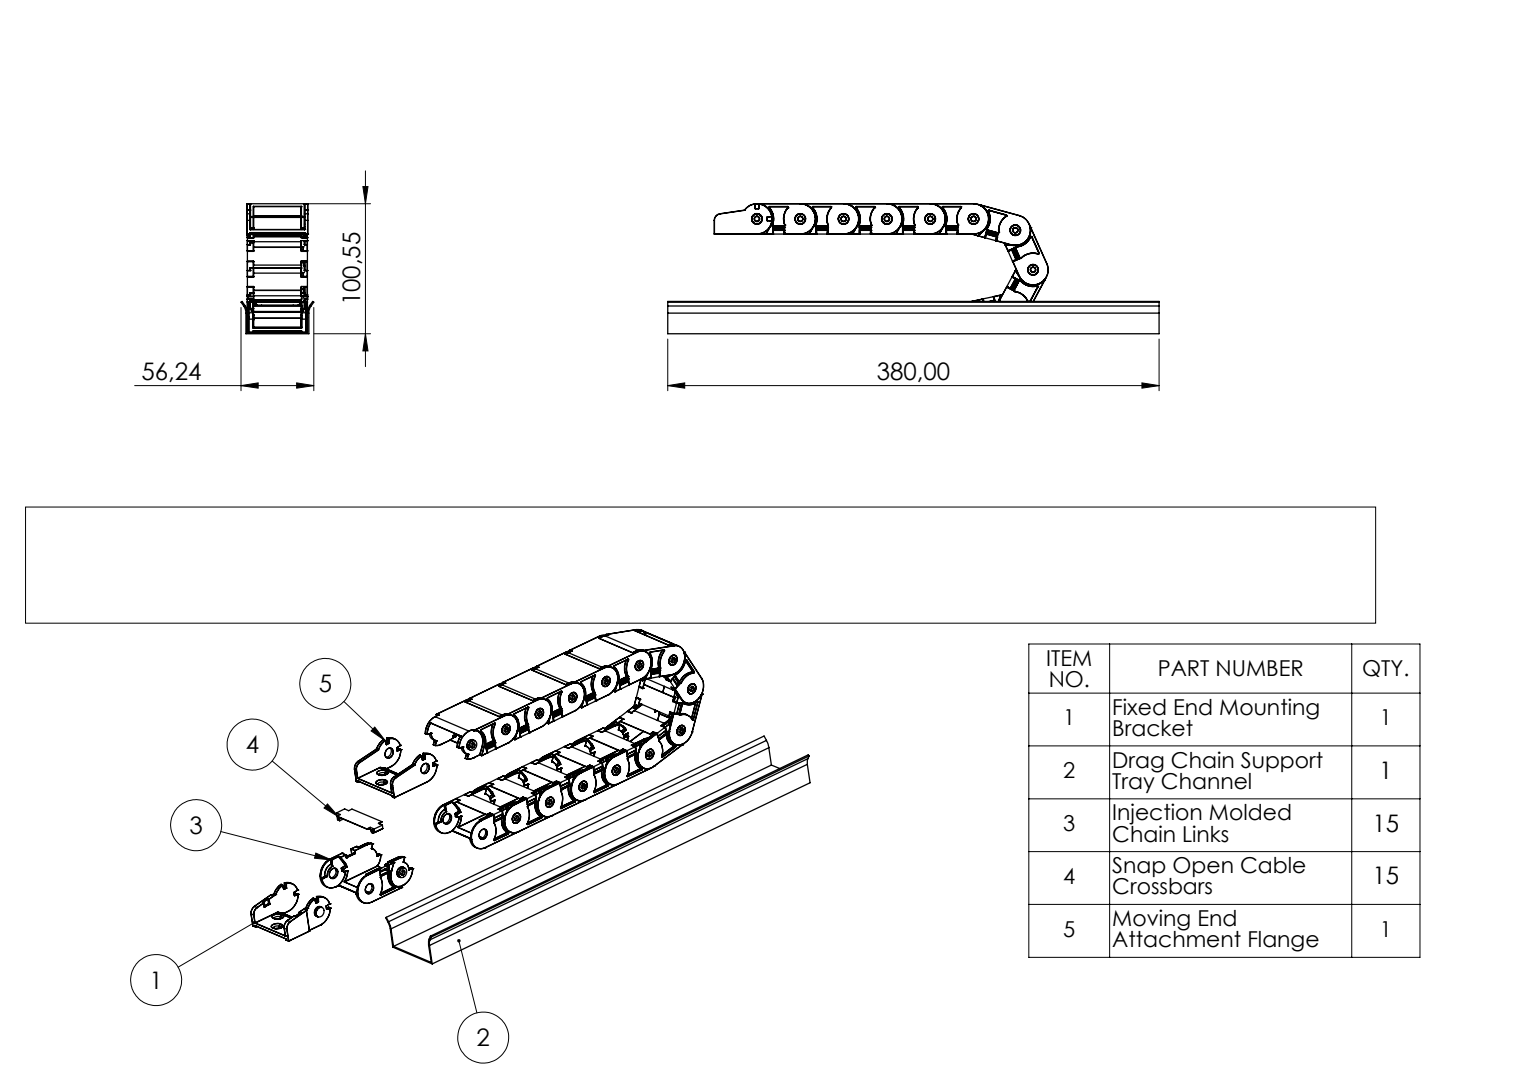
ISO-10303-21;
HEADER;
FILE_DESCRIPTION (('STEP AP214'),
    '1' );
FILE_NAME ('MAS-200',
    '2026-10-08T22:59:04',
    ( '' ),
    ( '' ),
    'SwSTEP 2.0',
    'SolidWorks 2020',
    '' );
FILE_SCHEMA (( 'AUTOMOTIVE_DESIGN' ));
ENDSEC;

DATA;
#1 = CARTESIAN_POINT ( 'NONE',  ( -16.92989143108098204, 9.949999999999981526, -12.88248387475667656 ) ) ;
#2 = ADVANCED_FACE ( 'NONE', ( #179969 ), #178383, .T. ) ;
#4 = DIRECTION ( 'NONE',  ( 0.000000000000000000, 0.000000000000000000, -1.000000000000000000 ) ) ;
#3 = CARTESIAN_POINT ( 'NONE',  ( -23.15000000000000213, 3.470628026992396808, -231.7731008717366876 ) ) ;
#5 = DIRECTION ( 'NONE',  ( 1.000000000000000000, -7.304098846218133681E-16, 0.000000000000000000 ) ) ;
#8 = ORIENTED_EDGE ( 'NONE', *, *, #143500, .T. ) ;
#7 = EDGE_CURVE ( 'NONE', #162791, #50451, #132568, .T. ) ;
#6 = CARTESIAN_POINT ( 'NONE',  ( 20.11144452914042802, 66.06638914889212799, -128.6328140305745933 ) ) ;
#10 = DIRECTION ( 'NONE',  ( 0.000000000000000000, 0.3427706569149662763, -0.9394191166662954062 ) ) ;
#9 = CARTESIAN_POINT ( 'NONE',  ( -18.59999999999999787, 68.22930980752001062, -227.7331931781284879 ) ) ;
#11 = ORIENTED_EDGE ( 'NONE', *, *, #97972, .T. ) ;
#13 = ORIENTED_EDGE ( 'NONE', *, *, #236887, .F. ) ;
#12 = CARTESIAN_POINT ( 'NONE',  ( 20.94999999999999929, 11.65000000001115943, -67.00000000000000000 ) ) ;
#14 = ORIENTED_EDGE ( 'NONE', *, *, #107088, .T. ) ;
#15 = DIRECTION ( 'NONE',  ( 0.000000000000000000, 0.000000000000000000, -1.000000000000000000 ) ) ;
#16 = CARTESIAN_POINT ( 'NONE',  ( -22.47071067811865319, 0.09909245471376178227, -25.77992525550193648 ) ) ;
#17 = CARTESIAN_POINT ( 'NONE',  ( -21.05000000000000071, 11.65000000001115232, -167.5999999999999659 ) ) ;
#18 = CARTESIAN_POINT ( 'NONE',  ( -17.29838795460356593, 22.07107181154411890, -229.9709893146081754 ) ) ;
#19 = ORIENTED_EDGE ( 'NONE', *, *, #38836, .T. ) ;
#20 = LINE ( 'NONE', #198225, #75570 ) ;
#21 = CARTESIAN_POINT ( 'NONE',  ( 20.97462148592267539, 8.874737576461731337, -112.7546443317310434 ) ) ;
#22 = CARTESIAN_POINT ( 'NONE',  ( 21.05000000000000071, 11.75000000001116263, -93.48519422934610645 ) ) ;
#23 = EDGE_CURVE ( 'NONE', #151382, #73251, #20149, .T. ) ;
#24 = ORIENTED_EDGE ( 'NONE', *, *, #246973, .F. ) ;
#25 = ADVANCED_FACE ( 'NONE', ( #203377 ), #234826, .T. ) ;
#26 = TOROIDAL_SURFACE ( 'NONE', #183386, 0.4000000000000009104, 0.1000000000000000056 ) ;
#27 = DIRECTION ( 'NONE',  ( -1.000000000000000000, -2.952720810173289112E-16, 0.000000000000000000 ) ) ;
#28 = CIRCLE ( 'NONE', #245740, 0.1000000000000032113 ) ;
#29 = DIRECTION ( 'NONE',  ( -1.020425574104004196E-15, -6.982962677686266711E-15, 1.000000000000000000 ) ) ;
#30 = EDGE_CURVE ( 'NONE', #21530, #216178, #199211, .T. ) ;
#31 = ORIENTED_EDGE ( 'NONE', *, *, #146192, .F. ) ;
#32 = ORIENTED_EDGE ( 'NONE', *, *, #162707, .T. ) ;
#33 = CARTESIAN_POINT ( 'NONE',  ( 18.39999999999999503, 64.52683809664910086, -56.87310748452440379 ) ) ;
#34 = AXIS2_PLACEMENT_3D ( 'NONE', #189135, #91325, #191735 ) ;
#35 = ORIENTED_EDGE ( 'NONE', *, *, #78924, .T. ) ;
#36 = CARTESIAN_POINT ( 'NONE',  ( -17.29838795458766043, 10.37154985795013218, -11.39525871738185714 ) ) ;
#37 = ORIENTED_EDGE ( 'NONE', *, *, #109345, .T. ) ;
#38 = PLANE ( 'NONE',  #96833 ) ;
#39 = LINE ( 'NONE', #62597, #48246 ) ;
#40 = LINE ( 'NONE', #161717, #239034 ) ;
#41 = ADVANCED_FACE ( 'NONE', ( #121306 ), #43023, .F. ) ;
#42 = CARTESIAN_POINT ( 'NONE',  ( -20.94999999999999929, 0.000000000000000000, -7.900000000000000355 ) ) ;
#43 = TOROIDAL_SURFACE ( 'NONE', #87521, 0.2000000000000000111, 0.1000000000000000056 ) ;
#44 = EDGE_CURVE ( 'NONE', #241330, #245837, #16247, .T. ) ;
#45 = AXIS2_PLACEMENT_3D ( 'NONE', #144433, #222696, #243559 ) ;
#46 = DIRECTION ( 'NONE',  ( 4.408576920032446739E-17, 0.1350103645451945777, -0.9908441862701590219 ) ) ;
#47 = DIRECTION ( 'NONE',  ( -0.000000000000000000, 6.982962677686266711E-15, -1.000000000000000000 ) ) ;
#48 = CARTESIAN_POINT ( 'NONE',  ( 21.05000000000000071, 5.850000000011156942, -56.86750277572208034 ) ) ;
#49 = ORIENTED_EDGE ( 'NONE', *, *, #170481, .T. ) ;
#51 = LINE ( 'NONE', #18341, #77316 ) ;
#50 = DIRECTION ( 'NONE',  ( -0.000000000000000000, -0.000000000000000000, 1.000000000000000000 ) ) ;
#52 = VERTEX_POINT ( 'NONE', #84661 ) ;
#55 = ORIENTED_EDGE ( 'NONE', *, *, #79678, .T. ) ;
#54 = CARTESIAN_POINT ( 'NONE',  ( -21.05000000000000071, 56.01362831242966678, -232.7091905853083347 ) ) ;
#53 = CARTESIAN_POINT ( 'NONE',  ( 21.05000000000000071, 76.00000000001172396, -71.52310748452431710 ) ) ;
#56 = COLOUR_RGB ( '', 0.40784314, 0.44705882, 0.49803922) ;
#57 = ORIENTED_EDGE ( 'NONE', *, *, #255744, .F. ) ;
#58 = DIRECTION ( 'NONE',  ( 1.000000000000000000, 0.000000000000000000, 0.000000000000000000 ) ) ;
#59 = CARTESIAN_POINT ( 'NONE',  ( 21.05000000000000071, -0.08559286335111461475, -60.58633726513042461 ) ) ;
#60 = FACE_OUTER_BOUND ( 'NONE', #199534, .T. ) ;
#61 = CARTESIAN_POINT ( 'NONE',  ( -18.39418127959864790, 64.51609439831406689, -145.7731074845244450 ) ) ;
#62 = VERTEX_POINT ( 'NONE', #243781 ) ;
#63 = LINE ( 'NONE', #3928, #147005 ) ;
#64 = DIRECTION ( 'NONE',  ( 0.000000000000000000, 0.000000000000000000, 1.000000000000000000 ) ) ;
#66 = LINE ( 'NONE', #97860, #134130 ) ;
#65 = DIRECTION ( 'NONE',  ( -1.000000000000000000, 0.000000000000000000, 0.000000000000000000 ) ) ;
#68 = ORIENTED_EDGE ( 'NONE', *, *, #6404, .T. ) ;
#67 = CARTESIAN_POINT ( 'NONE',  ( -23.15000000000000213, 0.000000000000000000, -4.149999999999999467 ) ) ;
#69 = AXIS2_PLACEMENT_3D ( 'NONE', #162469, #21667, #98580 ) ;
#70 = VECTOR ( 'NONE', #89864, 1000.000000000000000 ) ;
#71 = ORIENTED_EDGE ( 'NONE', *, *, #179559, .T. ) ;
#72 = B_SPLINE_CURVE_WITH_KNOTS ( 'NONE', 3,
 ( #139012, #19102, #60787, #178213, #62093, #257652, #41274, #180758, #218573, #162488, #79052, #22993, #39989, #157373, #119506, #236866, #137752, #173434, #141618, #102458, #199035, #795, #182040, #58212, #240730, #42515, #122066, #201587, #20411, #3376 ),
 .UNSPECIFIED., .F., .F.,
 ( 4, 2, 2, 2, 2, 2, 2, 2, 2, 2, 2, 2, 2, 2, 4 ),
 ( 0.000000000000000000, 0.0003422764154113359459, 0.0006845528308226718917, 0.001026829246234007729, 0.001369105661645343783, 0.002053658492468013290, 0.002738211323290682796, 0.003080487738702016899, 0.003422764154113351869, 0.003765040569524686406, 0.004107316984936021376, 0.004449593400347355912, 0.004791869815758691316, 0.005134146231170024985, 0.005476422646581360389 ),
 .UNSPECIFIED. ) ;
#73 = CARTESIAN_POINT ( 'NONE',  ( 33.30000000000001137, 3.332938107839120701, 33.00000000000000000 ) ) ;
#74 = ORIENTED_EDGE ( 'NONE', *, *, #168378, .T. ) ;
#75 = CARTESIAN_POINT ( 'NONE',  ( 20.94999999999999574, 65.57661458509869590, -62.03105556065429482 ) ) ;
#76 = ORIENTED_EDGE ( 'NONE', *, *, #212684, .T. ) ;
#77 = LINE ( 'NONE', #43075, #147484 ) ;
#78 = CARTESIAN_POINT ( 'NONE',  ( 22.59999999999999432, 75.89914163091330579, -114.7726746080137161 ) ) ;
#79 = CARTESIAN_POINT ( 'NONE',  ( -20.54999999999999716, 87.75000000001259082, -191.1731074845242517 ) ) ;
#80 = ORIENTED_EDGE ( 'NONE', *, *, #1653, .T. ) ;
#81 = DIRECTION ( 'NONE',  ( 1.000000000000000000, -7.049440681616511973E-16, 1.911869773728122111E-16 ) ) ;
#82 = VECTOR ( 'NONE', #56443, 999.9999999999998863 ) ;
#83 = AXIS2_PLACEMENT_3D ( 'NONE', #206420, #107313, #246821 ) ;
#84 = EDGE_CURVE ( 'NONE', #177357, #123054, #144663, .T. ) ;
#85 = CIRCLE ( 'NONE', #249894, 12.87500000000000000 ) ;
#86 = AXIS2_PLACEMENT_3D ( 'NONE', #170578, #248783, #191400 ) ;
#87 = CARTESIAN_POINT ( 'NONE',  ( -18.59999999999999787, 61.54970422893871529, -212.2965875311496688 ) ) ;
#88 = ORIENTED_EDGE ( 'NONE', *, *, #100506, .F. ) ;
#89 = CIRCLE ( 'NONE', #91688, 0.2000000000000000944 ) ;
#90 = ORIENTED_EDGE ( 'NONE', *, *, #88866, .F. ) ;
#91 = EDGE_LOOP ( 'NONE', ( #74556, #125437, #66569, #237966 ) ) ;
#92 = CARTESIAN_POINT ( 'NONE',  ( -20.90000000000000213, 6.336640076952988920, 12.03401928653448572 ) ) ;
#94 = EDGE_CURVE ( 'NONE', #19242, #16854, #137031, .T. ) ;
#93 = EDGE_LOOP ( 'NONE', ( #41790, #120721, #253364, #8024, #101724, #76712, #208119, #163090, #81602, #93473, #199890, #120447, #37635, #170547, #25122, #143467, #230838, #110010, #37319, #108527, #200762, #188074, #74749, #27804, #95098, #214920, #223956 ) ) ;
#96 = EDGE_LOOP ( 'NONE', ( #150504, #184348, #87694, #206446 ) ) ;
#95 = CARTESIAN_POINT ( 'NONE',  ( -18.50000000000000000, 76.00000000001244871, -170.0231074845243597 ) ) ;
#97 = ORIENTED_EDGE ( 'NONE', *, *, #227198, .T. ) ;
#98 = ADVANCED_FACE ( 'NONE', ( #186389 ), #170715, .F. ) ;
#100 = EDGE_CURVE ( 'NONE', #48831, #76480, #107799, .T. ) ;
#99 = AXIS2_PLACEMENT_3D ( 'NONE', #76575, #156148, #56984 ) ;
#103 = ORIENTED_EDGE ( 'NONE', *, *, #206571, .T. ) ;
#102 = ORIENTED_EDGE ( 'NONE', *, *, #34870, .F. ) ;
#101 = CARTESIAN_POINT ( 'NONE',  ( -20.54999999999999716, 23.49882452903949925, -253.1653563615082305 ) ) ;
#104 = VECTOR ( 'NONE', #151138, 1000.000000000000000 ) ;
#105 = ORIENTED_EDGE ( 'NONE', *, *, #252643, .T. ) ;
#106 = CARTESIAN_POINT ( 'NONE',  ( 23.14999999999999858, 76.00000000001170974, -69.52310748452431710 ) ) ;
#107 = CARTESIAN_POINT ( 'NONE',  ( -23.15000000000000213, 85.60000000001221565, -146.4170766071767389 ) ) ;
#108 = CARTESIAN_POINT ( 'NONE',  ( -16.82055514392371620, 14.15329893112338588, -219.2288882764422624 ) ) ;
#109 = VERTEX_POINT ( 'NONE', #88531 ) ;
#110 = EDGE_CURVE ( 'NONE', #147343, #202762, #12898, .T. ) ;
#111 = CARTESIAN_POINT ( 'NONE',  ( -20.94999999999999929, 87.48912529308798014, -105.9231074845242091 ) ) ;
#113 = VERTEX_POINT ( 'NONE', #246350 ) ;
#112 = CARTESIAN_POINT ( 'NONE',  ( 21.07928932188134397, 6.328516656404459262, -167.4011048543455615 ) ) ;
#114 = DIRECTION ( 'NONE',  ( 0.000000000000000000, -0.4088369013363280513, 0.9126074666063769270 ) ) ;
#115 = ORIENTED_EDGE ( 'NONE', *, *, #108700, .T. ) ;
#116 = EDGE_LOOP ( 'NONE', ( #122907, #87226, #174706, #3134 ) ) ;
#117 = CARTESIAN_POINT ( 'NONE',  ( -20.94999999999999929, 14.80545736607782814, -235.9842437978701639 ) ) ;
#118 = CARTESIAN_POINT ( 'NONE',  ( 22.88900146558018989, 64.28838232313110268, -213.4537907441674918 ) ) ;
#119 = ORIENTED_EDGE ( 'NONE', *, *, #90031, .T. ) ;
#120 = ORIENTED_EDGE ( 'NONE', *, *, #167346, .T. ) ;
#122 = TOROIDAL_SURFACE ( 'NONE', #25285, 11.65000000000000036, 0.1000000000000000056 ) ;
#121 = DIRECTION ( 'NONE',  ( 1.000000000000000000, 0.000000000000000000, -0.000000000000000000 ) ) ;
#123 = CARTESIAN_POINT ( 'NONE',  ( -23.15000000000000213, 54.26389919992384137, -237.1169412515656632 ) ) ;
#125 = VERTEX_POINT ( 'NONE', #228076 ) ;
#124 = ORIENTED_EDGE ( 'NONE', *, *, #248251, .T. ) ;
#126 = VERTEX_POINT ( 'NONE', #92393 ) ;
#127 = DIRECTION ( 'NONE',  ( 0.000000000000000000, -0.9126074666065964180, -0.4088369013358383874 ) ) ;
#129 = ORIENTED_EDGE ( 'NONE', *, *, #240704, .T. ) ;
#128 = EDGE_CURVE ( 'NONE', #174631, #91171, #224322, .T. ) ;
#130 = ORIENTED_EDGE ( 'NONE', *, *, #78727, .F. ) ;
#131 = DIRECTION ( 'NONE',  ( -0.000000000000000000, -6.982962677686266711E-15, 1.000000000000000000 ) ) ;
#132 = AXIS2_PLACEMENT_3D ( 'NONE', #200037, #1808, #61804 ) ;
#133 = VERTEX_POINT ( 'NONE', #245061 ) ;
#134 = CARTESIAN_POINT ( 'NONE',  ( -16.93909480342660245, 12.44555890197899295, -211.1852061227702109 ) ) ;
#136 = DIRECTION ( 'NONE',  ( 0.000000000000000000, -0.2128009952263678062, 0.9770955615653298398 ) ) ;
#135 = DIRECTION ( 'NONE',  ( 0.000000000000000000, -1.000000000000000000, 0.000000000000000000 ) ) ;
#137 = ORIENTED_EDGE ( 'NONE', *, *, #203695, .F. ) ;
#140 = EDGE_CURVE ( 'NONE', #198947, #93557, #66106, .T. ) ;
#139 = ORIENTED_EDGE ( 'NONE', *, *, #116118, .F. ) ;
#138 = ORIENTED_EDGE ( 'NONE', *, *, #133333, .T. ) ;
#141 = LINE ( 'NONE', #80958, #244386 ) ;
#142 = CARTESIAN_POINT ( 'NONE',  ( 20.12500000000000355, 10.24195072709382970, -175.3602037270860592 ) ) ;
#144 = ORIENTED_EDGE ( 'NONE', *, *, #165937, .T. ) ;
#143 = AXIS2_PLACEMENT_3D ( 'NONE', #77919, #25665, #21818 ) ;
#145 = VECTOR ( 'NONE', #17658, 1000.000000000000000 ) ;
#146 = LINE ( 'NONE', #4012, #142490 ) ;
#147 = ORIENTED_EDGE ( 'NONE', *, *, #183774, .F. ) ;
#148 = ORIENTED_EDGE ( 'NONE', *, *, #102799, .T. ) ;
#149 = AXIS2_PLACEMENT_3D ( 'NONE', #44529, #5360, #61520 ) ;
#150 = DIRECTION ( 'NONE',  ( 0.000000000000000000, 0.8660254037844309360, -0.5000000000000134337 ) ) ;
#151 = ORIENTED_EDGE ( 'NONE', *, *, #31189, .T. ) ;
#152 = DIRECTION ( 'NONE',  ( 1.000000000000000000, 0.000000000000000000, 0.000000000000000000 ) ) ;
#153 = CARTESIAN_POINT ( 'NONE',  ( 18.59999999999999432, 77.13501884592184865, -61.80613060109197932 ) ) ;
#154 = ORIENTED_EDGE ( 'NONE', *, *, #235914, .T. ) ;
#155 = CIRCLE ( 'NONE', #224998, 12.77499999999999503 ) ;
#156 = DIRECTION ( 'NONE',  ( -1.000000000000000000, 0.000000000000000000, 0.000000000000000000 ) ) ;
#158 = AXIS2_PLACEMENT_3D ( 'NONE', #230625, #35020, #51950 ) ;
#157 = CARTESIAN_POINT ( 'NONE',  ( -21.05000000000000071, 0.4879293624014888198, -209.1697915983179428 ) ) ;
#160 = CARTESIAN_POINT ( 'NONE',  ( -16.82055514392394713, 9.950000000011193890, -121.3232019254582497 ) ) ;
#159 = DIRECTION ( 'NONE',  ( -1.000000000000000000, 0.000000000000000000, 0.000000000000000000 ) ) ;
#161 = CARTESIAN_POINT ( 'NONE',  ( 21.15000000000003055, 74.83745509109094485, -44.02310748452479316 ) ) ;
#162 = EDGE_CURVE ( 'NONE', #138584, #10632, #99412, .T. ) ;
#163 = CARTESIAN_POINT ( 'NONE',  ( 21.07928932188134397, 1.148907358139439339E-11, -201.0000000000015064 ) ) ;
#164 = DIRECTION ( 'NONE',  ( 2.952720810173289605E-16, -0.4721928772777346794, -0.8814952561688429444 ) ) ;
#165 = DIRECTION ( 'NONE',  ( -0.000000000000000000, 1.000000000000000000, 0.000000000000000000 ) ) ;
#166 = DIRECTION ( 'NONE',  ( -2.952720810173289112E-16, 1.000000000000000000, 0.000000000000000000 ) ) ;
#167 = CARTESIAN_POINT ( 'NONE',  ( -18.39999999999999858, 11.47316190337362762, -176.8259460668079441 ) ) ;
#168 = VERTEX_POINT ( 'NONE', #130234 ) ;
#169 = VECTOR ( 'NONE', #156157, 1000.000000000000000 ) ;
#170 = VECTOR ( 'NONE', #232496, 1000.000000000000000 ) ;
#171 = CIRCLE ( 'NONE', #95836, 0.9750000000000036415 ) ;
#172 = AXIS2_PLACEMENT_3D ( 'NONE', #68198, #90308, #107312 ) ;
#173 = AXIS2_PLACEMENT_3D ( 'NONE', #207427, #126590, #204823 ) ;
#174 = EDGE_CURVE ( 'NONE', #29202, #220627, #141140, .T. ) ;
#176 = VERTEX_POINT ( 'NONE', #31196 ) ;
#175 = ORIENTED_EDGE ( 'NONE', *, *, #85520, .F. ) ;
#177 = EDGE_LOOP ( 'NONE', ( #39245, #107994, #42022, #72538 ) ) ;
#179 = ORIENTED_EDGE ( 'NONE', *, *, #45901, .T. ) ;
#178 = EDGE_CURVE ( 'NONE', #224075, #38015, #66431, .T. ) ;
#180 = CARTESIAN_POINT ( 'NONE',  ( 21.14999999999999858, 76.10000000001194564, -103.0231074845243171 ) ) ;
#181 = LINE ( 'NONE', #1467, #236049 ) ;
#182 = EDGE_CURVE ( 'NONE', #9569, #208902, #126394, .T. ) ;
#183 = ADVANCED_FACE ( 'NONE', ( #7745 ), #109386, .T. ) ;
#185 = DIRECTION ( 'NONE',  ( -1.000000000000000000, 0.000000000000000000, 0.000000000000000000 ) ) ;
#184 = DIRECTION ( 'NONE',  ( -1.000000000000000000, 2.952720810173289112E-16, 2.061873921506763405E-30 ) ) ;
#186 = DIRECTION ( 'NONE',  ( -0.000000000000000000, 0.1350103645451876666, 0.9908441862701600211 ) ) ;
#187 = EDGE_LOOP ( 'NONE', ( #19437, #210011, #114046, #182505, #122843 ) ) ;
#188 = FACE_OUTER_BOUND ( 'NONE', #64548, .T. ) ;
#189 = CIRCLE ( 'NONE', #183374, 0.1000000000000015044 ) ;
#190 = CARTESIAN_POINT ( 'NONE',  ( 18.39999999999999503, 70.35000000001159037, -56.87310748452436115 ) ) ;
#191 = CARTESIAN_POINT ( 'NONE',  ( 18.49999999999999289, 69.55000000001277272, -215.2731074845244166 ) ) ;
#192 = EDGE_CURVE ( 'NONE', #72719, #31733, #199411, .T. ) ;
#193 = CARTESIAN_POINT ( 'NONE',  ( -18.40000000000000213, 11.47316190337364183, -91.25000000000005684 ) ) ;
#194 = ORIENTED_EDGE ( 'NONE', *, *, #188174, .T. ) ;
#195 = EDGE_CURVE ( 'NONE', #225539, #67597, #120326, .T. ) ;
#197 = EDGE_CURVE ( 'NONE', #86923, #12856, #126876, .T. ) ;
#196 = EDGE_CURVE ( 'NONE', #151569, #28788, #226776, .T. ) ;
#198 = DIRECTION ( 'NONE',  ( 1.000000000000000000, 0.000000000000000000, 0.000000000000000000 ) ) ;
#199 = CARTESIAN_POINT ( 'NONE',  ( -22.50000000000000000, 1.619487989037824871, -230.7814958294534335 ) ) ;
#200 = VERTEX_POINT ( 'NONE', #187678 ) ;
#201 = DIRECTION ( 'NONE',  ( 1.000000000000000000, 1.832422279913646096E-16, 3.990820347355631841E-17 ) ) ;
#202 = CARTESIAN_POINT ( 'NONE',  ( 20.99999999999999645, 9.749999999999982236, -9.250000000000001776 ) ) ;
#203 = FACE_OUTER_BOUND ( 'NONE', #140613, .T. ) ;
#204 = DIRECTION ( 'NONE',  ( -1.000000000000000000, -0.000000000000000000, -0.000000000000000000 ) ) ;
#205 = VERTEX_POINT ( 'NONE', #188945 ) ;
#206 = DIRECTION ( 'NONE',  ( 2.694716079187273439E-16, 1.000000000000000000, 6.467318590049456648E-15 ) ) ;
#207 = CARTESIAN_POINT ( 'NONE',  ( -16.81744102076748959, 66.05000000001182059, -82.17310748452439384 ) ) ;
#208 = CIRCLE ( 'NONE', #96054, 11.75000000000000000 ) ;
#209 = DIRECTION ( 'NONE',  ( -0.7071067811865474617, -0.7071067811865474617, -2.044391222244499837E-16 ) ) ;
#210 = EDGE_CURVE ( 'NONE', #252512, #147282, #169419, .T. ) ;
#212 = DIRECTION ( 'NONE',  ( -0.7070776581708964059, -0.3339045366652730884, -0.6233369439636241571 ) ) ;
#211 = CARTESIAN_POINT ( 'NONE',  ( -23.15000000000000213, 74.00000000001254818, -183.2477294072864709 ) ) ;
#213 = CARTESIAN_POINT ( 'NONE',  ( 18.49999999999998934, 6.550000000011156231, -177.5170271704400022 ) ) ;
#214 = AXIS2_PLACEMENT_3D ( 'NONE', #162739, #3632, #83138 ) ;
#215 = DIRECTION ( 'NONE',  ( -1.000000000000000000, 0.000000000000000000, 0.000000000000000000 ) ) ;
#216 = FACE_OUTER_BOUND ( 'NONE', #240838, .T. ) ;
#217 = CARTESIAN_POINT ( 'NONE',  ( 22.49806830649814060, 75.92253568368651884, -114.6729971393633889 ) ) ;
#218 = EDGE_CURVE ( 'NONE', #140485, #55100, #47742, .T. ) ;
#219 = ADVANCED_FACE ( 'NONE', ( #251471 ), #75440, .T. ) ;
#221 = VERTEX_POINT ( 'NONE', #213632 ) ;
#220 = CIRCLE ( 'NONE', #212623, 0.1000000000000024342 ) ;
#222 = ORIENTED_EDGE ( 'NONE', *, *, #184474, .T. ) ;
#223 = EDGE_CURVE ( 'NONE', #25855, #57391, #222711, .T. ) ;
#224 = AXIS2_PLACEMENT_3D ( 'NONE', #149688, #207076, #227918 ) ;
#225 = ORIENTED_EDGE ( 'NONE', *, *, #31957, .F. ) ;
#226 = LINE ( 'NONE', #155042, #92913 ) ;
#227 = EDGE_CURVE ( 'NONE', #173426, #116632, #172895, .T. ) ;
#228 = DIRECTION ( 'NONE',  ( -1.073024830501117725E-15, 6.982962677686266711E-15, -1.000000000000000000 ) ) ;
#229 = AXIS2_PLACEMENT_3D ( 'NONE', #181398, #200936, #217905 ) ;
#230 = DIRECTION ( 'NONE',  ( 0.000000000000000000, 0.000000000000000000, -1.000000000000000000 ) ) ;
#231 = CARTESIAN_POINT ( 'NONE',  ( 22.47007471830798764, 65.21035539001043446, -243.3066537799435878 ) ) ;
#232 = AXIS2_PLACEMENT_3D ( 'NONE', #173463, #54731, #134253 ) ;
#233 = ORIENTED_EDGE ( 'NONE', *, *, #144291, .F. ) ;
#234 = CIRCLE ( 'NONE', #162756, 0.09999999999998898659 ) ;
#235 = DIRECTION ( 'NONE',  ( 1.000000000000000000, 0.000000000000000000, 0.000000000000000000 ) ) ;
#236 = CARTESIAN_POINT ( 'NONE',  ( 21.00000000000000000, 51.97441255244040548, -232.0063394385699667 ) ) ;
#238 = CARTESIAN_POINT ( 'NONE',  ( 21.97500000000000497, 9.750000000011153745, -112.7500000000000284 ) ) ;
#237 = AXIS2_PLACEMENT_3D ( 'NONE', #83814, #157333, #257616 ) ;
#239 = CARTESIAN_POINT ( 'NONE',  ( -20.64999999999999858, 85.50000000001188027, -93.12913836187179584 ) ) ;
#241 = ORIENTED_EDGE ( 'NONE', *, *, #154688, .T. ) ;
#240 = LINE ( 'NONE', #240155, #250850 ) ;
#243 = DIRECTION ( 'NONE',  ( 0.000000000000000000, -0.9770955615653290627, -0.2128009952263723858 ) ) ;
#242 = DIRECTION ( 'NONE',  ( 0.000000000000000000, 0.1568667991644863147, -0.9876197685951252359 ) ) ;
#244 = DIRECTION ( 'NONE',  ( -1.000000000000000000, 0.000000000000000000, 0.000000000000000000 ) ) ;
#245 = DIRECTION ( 'NONE',  ( -1.000000000000000000, 0.000000000000000000, 0.000000000000000000 ) ) ;
#246 = CARTESIAN_POINT ( 'NONE',  ( 22.39999999999999503, -0.09999999998884338825, -55.35042919245524473 ) ) ;
#247 = VERTEX_POINT ( 'NONE', #134084 ) ;
#248 =( NAMED_UNIT ( * ) SI_UNIT ( $, .STERADIAN. ) SOLID_ANGLE_UNIT ( ) );
#249 = LINE ( 'NONE', #242710, #54314 ) ;
#250 = DIRECTION ( 'NONE',  ( 2.557131231893037478E-16, 0.8660254037844420383, -0.4999999999999942824 ) ) ;
#251 = CIRCLE ( 'NONE', #17030, 0.09999999999998898659 ) ;
#252 = ORIENTED_EDGE ( 'NONE', *, *, #113172, .F. ) ;
#253 = CYLINDRICAL_SURFACE ( 'NONE', #33673, 0.1000000000000000472 ) ;
#254 = CARTESIAN_POINT ( 'NONE',  ( -23.15000000000000213, 2.000000000011154189, -113.7246219227621395 ) ) ;
#255 = ORIENTED_EDGE ( 'NONE', *, *, #208280, .F. ) ;
#256 = CARTESIAN_POINT ( 'NONE',  ( 18.49999999999999289, 55.04793976901535757, -229.8170162380219210 ) ) ;
#257 = CARTESIAN_POINT ( 'NONE',  ( -21.05000000000000071, 0.000000000000000000, -33.50000000000000000 ) ) ;
#258 = DIRECTION ( 'NONE',  ( 0.000000000000000000, -0.2818822000686205809, 0.9594490217226104845 ) ) ;
#259 = ORIENTED_EDGE ( 'NONE', *, *, #102586, .T. ) ;
#260 = VERTEX_POINT ( 'NONE', #174569 ) ;
#261 = CARTESIAN_POINT ( 'NONE',  ( -22.39999999999999858, 11.65000000001115588, -100.5000000000000284 ) ) ;
#262 = CYLINDRICAL_SURFACE ( 'NONE', #140052, 0.09999999999999939493 ) ;
#263 = VECTOR ( 'NONE', #242147, 1000.000000000000000 ) ;
#264 = ADVANCED_FACE ( 'NONE', ( #17990 ), #237050, .T. ) ;
#265 = DIRECTION ( 'NONE',  ( 1.000000000000000000, 1.836970198721029934E-16, 0.000000000000000000 ) ) ;
#267 = DIRECTION ( 'NONE',  ( 0.000000000000000000, -1.000000000000000000, 0.000000000000000000 ) ) ;
#266 = AXIS2_PLACEMENT_3D ( 'NONE', #27213, #123720, #224080 ) ;
#270 = CARTESIAN_POINT ( 'NONE',  ( -21.59142135623730852, 7.850000000011158718, -112.7500000000000284 ) ) ;
#269 = TOROIDAL_SURFACE ( 'NONE', #212681, 0.2000000000000000111, 0.1000000000000000056 ) ;
#268 = CARTESIAN_POINT ( 'NONE',  ( 21.72449340488910252, 43.99894805634765760, -234.9941606142489832 ) ) ;
#271 = DIRECTION ( 'NONE',  ( 3.265361837132813093E-16, 1.000000000000000000, 6.982962677686266711E-15 ) ) ;
#272 = EDGE_CURVE ( 'NONE', #20238, #178566, #58379, .T. ) ;
#273 = DIRECTION ( 'NONE',  ( 1.000000000000000000, 0.000000000000000000, 0.000000000000000000 ) ) ;
#274 = FACE_OUTER_BOUND ( 'NONE', #244850, .T. ) ;
#275 = EDGE_LOOP ( 'NONE', ( #125788, #98661, #200671, #130469 ) ) ;
#276 = CARTESIAN_POINT ( 'NONE',  ( 23.25000000000000000, 85.60000000001159037, -59.62913836187181005 ) ) ;
#278 = VERTEX_POINT ( 'NONE', #173282 ) ;
#277 = DIRECTION ( 'NONE',  ( 1.000000000000000000, 0.000000000000000000, 0.000000000000000000 ) ) ;
#279 = VECTOR ( 'NONE', #178302, 1000.000000000000227 ) ;
#280 = DIRECTION ( 'NONE',  ( 1.000000000000000000, 0.000000000000000000, -0.000000000000000000 ) ) ;
#281 = DIRECTION ( 'NONE',  ( 1.000000000000000000, 0.000000000000000000, 0.000000000000000000 ) ) ;
#283 = DIRECTION ( 'NONE',  ( 1.000000000000000000, -0.000000000000000000, -0.000000000000000000 ) ) ;
#282 = DIRECTION ( 'NONE',  ( 0.000000000000000000, 1.776356839400155604E-15, 1.000000000000000000 ) ) ;
#284 = EDGE_CURVE ( 'NONE', #234077, #216189, #164488, .T. ) ;
#285 = EDGE_CURVE ( 'NONE', #102466, #142934, #55807, .T. ) ;
#286 = VERTEX_POINT ( 'NONE', #33766 ) ;
#287 = CARTESIAN_POINT ( 'NONE',  ( -18.50000000000000000, -1.637172712959223952, -112.0821533654720383 ) ) ;
#288 = FACE_OUTER_BOUND ( 'NONE', #250177, .T. ) ;
#289 = DIRECTION ( 'NONE',  ( 0.000000000000000000, -6.982962677686266711E-15, 1.000000000000000000 ) ) ;
#290 = DIRECTION ( 'NONE',  ( 1.000000000000000000, 0.000000000000000000, 0.000000000000000000 ) ) ;
#291 = CYLINDRICAL_SURFACE ( 'NONE', #124370, 0.1000000000000028644 ) ;
#292 = ORIENTED_EDGE ( 'NONE', *, *, #254482, .F. ) ;
#293 = DIRECTION ( 'NONE',  ( 0.000000000000000000, -1.000000000000000000, 0.000000000000000000 ) ) ;
#295 = VERTEX_POINT ( 'NONE', #252749 ) ;
#294 = AXIS2_PLACEMENT_3D ( 'NONE', #120251, #5368, #35877 ) ;
#296 = CARTESIAN_POINT ( 'NONE',  ( 22.50927854361892244, 76.10085807354055021, -215.2726746105512348 ) ) ;
#297 = VERTEX_POINT ( 'NONE', #114542 ) ;
#298 = DIRECTION ( 'NONE',  ( 0.000000000000000000, -0.9910827722268049644, -0.1332476588733589040 ) ) ;
#299 = ORIENTED_EDGE ( 'NONE', *, *, #10132, .F. ) ;
#300 = EDGE_CURVE ( 'NONE', #67768, #134738, #175812, .T. ) ;
#301 = CARTESIAN_POINT ( 'NONE',  ( -21.59780538579341425, 6.847090529954407145, -167.4010213304019885 ) ) ;
#302 = ADVANCED_FACE ( 'NONE', ( #14182 ), #214528, .T. ) ;
#303 = DIRECTION ( 'NONE',  ( 0.7071067811865462405, 0.6909108974501247946, 0.1504730267678065503 ) ) ;
#304 = ORIENTED_EDGE ( 'NONE', *, *, #196870, .F. ) ;
#305 = AXIS2_PLACEMENT_3D ( 'NONE', #200096, #237928, #219641 ) ;
#306 = CARTESIAN_POINT ( 'NONE',  ( -16.81931177881022421, 9.936996059515065483, -87.77321787861730229 ) ) ;
#307 = FACE_OUTER_BOUND ( 'NONE', #226701, .T. ) ;
#308 = CARTESIAN_POINT ( 'NONE',  ( -23.25000000000000000, 76.00000000001264766, -199.4731074845243484 ) ) ;
#309 = AXIS2_PLACEMENT_3D ( 'NONE', #21762, #240801, #38751 ) ;
#310 = CARTESIAN_POINT ( 'NONE',  ( -18.50000000000000000, 9.350000000000001421, -21.35000000000000142 ) ) ;
#311 = CARTESIAN_POINT ( 'NONE',  ( 23.14999999999998437, 76.00000000001165290, -69.52310748452431710 ) ) ;
#312 = ADVANCED_FACE ( 'NONE', ( #35040 ), #74164, .F. ) ;
#313 = LINE ( 'NONE', #160718, #74675 ) ;
#315 = DIRECTION ( 'NONE',  ( -0.000000000000000000, 1.000000000000000000, -0.000000000000000000 ) ) ;
#314 = AXIS2_PLACEMENT_3D ( 'NONE', #40816, #102008, #159455 ) ;
#317 = ORIENTED_EDGE ( 'NONE', *, *, #114958, .T. ) ;
#316 = EDGE_CURVE ( 'NONE', #120394, #176327, #185325, .T. ) ;
#318 = DIRECTION ( 'NONE',  ( 0.000000000000000000, 0.6728971962616412394, -0.7397360091703134577 ) ) ;
#319 = VERTEX_POINT ( 'NONE', #153722 ) ;
#321 = ORIENTED_EDGE ( 'NONE', *, *, #151126, .F. ) ;
#320 = CARTESIAN_POINT ( 'NONE',  ( 20.94999999999999929, 1.115600667400684642E-11, -134.0000000000000284 ) ) ;
#322 = EDGE_LOOP ( 'NONE', ( #244833, #202567, #58686, #132622 ) ) ;
#323 = DIRECTION ( 'NONE',  ( -0.000000000000000000, -6.982962677686266711E-15, 1.000000000000000000 ) ) ;
#324 = DIRECTION ( 'NONE',  ( 0.000000000000000000, 0.2128009952263601456, -0.9770955615653316162 ) ) ;
#325 = CARTESIAN_POINT ( 'NONE',  ( -18.50000000000000000, -7.631834139421013852, -210.1304494778855769 ) ) ;
#326 = CARTESIAN_POINT ( 'NONE',  ( 21.05000000000000071, 60.06860817181090795, -221.2964476536733684 ) ) ;
#327 = DIRECTION ( 'NONE',  ( -1.000000000000000000, -0.000000000000000000, -0.000000000000000000 ) ) ;
#328 = CIRCLE ( 'NONE', #17110, 0.09999999999998898659 ) ;
#329 = ORIENTED_EDGE ( 'NONE', *, *, #220458, .F. ) ;
#330 = CARTESIAN_POINT ( 'NONE',  ( -20.54999999999999716, -8.999999999988844479, -191.1060308773475356 ) ) ;
#331 = EDGE_CURVE ( 'NONE', #102761, #231063, #231938, .T. ) ;
#334 = ORIENTED_EDGE ( 'NONE', *, *, #211457, .T. ) ;
#333 = B_SPLINE_CURVE_WITH_KNOTS ( 'NONE', 3,
 ( #148170, #229008, #126030, #184720, #50334, #66064, #49068, #145593, #90750, #205561, #47767, #209424, #226401 ),
 .UNSPECIFIED., .F., .F.,
 ( 4, 3, 3, 3, 4 ),
 ( -3.224855718292275407E-06, 0.000000000000000000, 6.199515528651840239E-06, 4.034952380126954614E-05, 7.452715123699161213E-05 ),
 .UNSPECIFIED. ) ;
#332 = CYLINDRICAL_SURFACE ( 'NONE', #17646, 0.1000000000000075273 ) ;
#335 = EDGE_CURVE ( 'NONE', #34147, #83134, #97503, .T. ) ;
#336 = CARTESIAN_POINT ( 'NONE',  ( -20.94999027547553894, 10.29326151434211489, -38.95928225104149334 ) ) ;
#337 = CARTESIAN_POINT ( 'NONE',  ( -23.25000000000000355, 7.488999128699433072, -208.8358083214519070 ) ) ;
#339 = ADVANCED_FACE ( 'NONE', ( #38863 ), #118398, .T. ) ;
#338 = CIRCLE ( 'NONE', #33524, 0.5000000000000004441 ) ;
#340 = ORIENTED_EDGE ( 'NONE', *, *, #133488, .F. ) ;
#341 = AXIS2_PLACEMENT_3D ( 'NONE', #63201, #44950, #142741 ) ;
#342 = EDGE_CURVE ( 'NONE', #84120, #176836, #119484, .T. ) ;
#343 = AXIS2_PLACEMENT_3D ( 'NONE', #231284, #38216, #12243 ) ;
#344 = DIRECTION ( 'NONE',  ( 1.000000000000000000, 0.000000000000000000, 0.000000000000000000 ) ) ;
#345 = ORIENTED_EDGE ( 'NONE', *, *, #216352, .F. ) ;
#346 = DIRECTION ( 'NONE',  ( 0.000000000000000000, -7.272083257015735086E-15, 1.000000000000000000 ) ) ;
#347 = DIRECTION ( 'NONE',  ( 0.000000000000000000, -1.000000000000000000, 0.000000000000000000 ) ) ;
#348 = CARTESIAN_POINT ( 'NONE',  ( 20.95000000000000284, 64.36312671090941251, -176.8448666978491985 ) ) ;
#349 = CIRCLE ( 'NONE', #121198, 0.1000000000000000472 ) ;
#350 = EDGE_CURVE ( 'NONE', #79629, #237280, #201885, .T. ) ;
#351 = AXIS2_PLACEMENT_3D ( 'NONE', #154646, #254933, #132486 ) ;
#352 = CARTESIAN_POINT ( 'NONE',  ( -18.59999999999999787, 10.63601275468165142, -265.6051570720007931 ) ) ;
#353 = ADVANCED_FACE ( 'NONE', ( #239625 ), #221311, .T. ) ;
#354 = CIRCLE ( 'NONE', #158793, 0.09999999999999939493 ) ;
#355 = CIRCLE ( 'NONE', #133630, 0.6000000000000033085 ) ;
#356 = EDGE_LOOP ( 'NONE', ( #15486, #102274, #95283, #141475 ) ) ;
#358 =( LENGTH_UNIT ( ) NAMED_UNIT ( * ) SI_UNIT ( .MILLI., .METRE. ) );
#357 = AXIS2_PLACEMENT_3D ( 'NONE', #213494, #19149, #34902 ) ;
#359 = AXIS2_PLACEMENT_3D ( 'NONE', #100272, #179854, #1176 ) ;
#360 = VERTEX_POINT ( 'NONE', #59665 ) ;
#361 = DIRECTION ( 'NONE',  ( 0.000000000000000000, 0.6728971962617102953, 0.7397360091702507301 ) ) ;
#363 = ADVANCED_FACE ( 'NONE', ( #179658 ), #56124, .T. ) ;
#362 = CARTESIAN_POINT ( 'NONE',  ( -16.92570016628983609, 9.958788957751020021, -79.62065067003905483 ) ) ;
#365 = VERTEX_POINT ( 'NONE', #103924 ) ;
#364 = CARTESIAN_POINT ( 'NONE',  ( 20.94999999999999929, 85.00000000001179501, -79.41707660717668205 ) ) ;
#366 = DIRECTION ( 'NONE',  ( 0.000000000000000000, 0.000000000000000000, -1.000000000000000000 ) ) ;
#367 = FACE_OUTER_BOUND ( 'NONE', #189454, .T. ) ;
#368 = CARTESIAN_POINT ( 'NONE',  ( -23.15000000000000213, 71.75000000001151079, -48.27310748452435263 ) ) ;
#369 = CARTESIAN_POINT ( 'NONE',  ( -20.54999999999999361, 15.92646454033039305, -219.3818586450342707 ) ) ;
#370 = DIRECTION ( 'NONE',  ( 1.836970198721029934E-16, -1.000000000000000000, -0.000000000000000000 ) ) ;
#371 = DIRECTION ( 'NONE',  ( 0.000000000000000000, -0.8814952561688430555, 0.4721928772777346239 ) ) ;
#372 = TOROIDAL_SURFACE ( 'NONE', #246093, 0.9750000000000019762, 0.1000000000000000056 ) ;
#374 = VERTEX_POINT ( 'NONE', #183498 ) ;
#373 = CARTESIAN_POINT ( 'NONE',  ( 20.94999999999999574, 67.23127455305841238, -235.8551265064783991 ) ) ;
#375 = CARTESIAN_POINT ( 'NONE',  ( -23.15000000000000213, 54.09940989982483472, -238.8890605415484174 ) ) ;
#376 = ORIENTED_EDGE ( 'NONE', *, *, #193695, .T. ) ;
#377 = EDGE_LOOP ( 'NONE', ( #153054, #45410, #48839 ) ) ;
#378 = FACE_OUTER_BOUND ( 'NONE', #36021, .T. ) ;
#379 = CARTESIAN_POINT ( 'NONE',  ( 22.47007471830797343, 68.27928934808548433, -103.0231074845243455 ) ) ;
#380 = ORIENTED_EDGE ( 'NONE', *, *, #23400, .F. ) ;
#381 = CARTESIAN_POINT ( 'NONE',  ( -18.59999999999999787, 77.83585931145570669, -125.0186683157258045 ) ) ;
#382 = AXIS2_PLACEMENT_3D ( 'NONE', #149587, #227805, #71331 ) ;
#383 = ORIENTED_EDGE ( 'NONE', *, *, #120416, .F. ) ;
#384 = CIRCLE ( 'NONE', #179491, 0.1000000000000124678 ) ;
#386 = ADVANCED_FACE ( 'NONE', ( #20587 ), #193882, .T. ) ;
#385 = CARTESIAN_POINT ( 'NONE',  ( 23.24999999999999289, 11.65000000001116298, -155.3500000000000227 ) ) ;
#387 = DIRECTION ( 'NONE',  ( 0.000000000000000000, 0.9770955615653551529, 0.2128009952262517601 ) ) ;
#389 = EDGE_LOOP ( 'NONE', ( #34523, #210444, #11516, #231770, #22823, #35860, #120111, #57918, #85074, #11479, #66670, #27843 ) ) ;
#388 = AXIS2_PLACEMENT_3D ( 'NONE', #182068, #137780, #103776 ) ;
#390 = CARTESIAN_POINT ( 'NONE',  ( -18.41431012584568805, 64.51252797080333323, -45.24987147142272903 ) ) ;
#391 = ORIENTED_EDGE ( 'NONE', *, *, #246071, .F. ) ;
#392 = CARTESIAN_POINT ( 'NONE',  ( -22.39999999999999858, 76.00000000001243450, -177.8138870828977360 ) ) ;
#393 = EDGE_CURVE ( 'NONE', #139006, #141665, #163936, .T. ) ;
#395 = ORIENTED_EDGE ( 'NONE', *, *, #245882, .T. ) ;
#394 = CYLINDRICAL_SURFACE ( 'NONE', #26043, 0.09999999999999939493 ) ;
#396 = DIRECTION ( 'NONE',  ( 0.000000000000000000, 1.000000000000000000, 6.982962677686266711E-15 ) ) ;
#397 = ORIENTED_EDGE ( 'NONE', *, *, #191069, .F. ) ;
#398 = EDGE_CURVE ( 'NONE', #14558, #190027, #2320, .T. ) ;
#399 = CARTESIAN_POINT ( 'NONE',  ( 21.05000000000000071, -11.74999999998883560, -97.40000000000004832 ) ) ;
#400 = EDGE_CURVE ( 'NONE', #236903, #41196, #35696, .T. ) ;
#401 = VERTEX_POINT ( 'NONE', #80504 ) ;
#403 = ORIENTED_EDGE ( 'NONE', *, *, #146611, .T. ) ;
#402 = EDGE_LOOP ( 'NONE', ( #242482, #239735, #248991, #84795 ) ) ;
#404 = CARTESIAN_POINT ( 'NONE',  ( -20.94999999999999929, 43.24695311518262031, -245.0026972281755491 ) ) ;
#405 = ORIENTED_EDGE ( 'NONE', *, *, #194450, .F. ) ;
#406 = DIRECTION ( 'NONE',  ( 0.000000000000000000, 0.000000000000000000, -1.000000000000000000 ) ) ;
#407 = VECTOR ( 'NONE', #248788, 1000.000000000000000 ) ;
#408 = ORIENTED_EDGE ( 'NONE', *, *, #58975, .F. ) ;
#409 = AXIS2_PLACEMENT_3D ( 'NONE', #159903, #62072, #196433 ) ;
#410 = CIRCLE ( 'NONE', #104453, 0.09999999999999939493 ) ;
#411 = VERTEX_POINT ( 'NONE', #140497 ) ;
#412 = EDGE_CURVE ( 'NONE', #54594, #188452, #201762, .T. ) ;
#413 = CYLINDRICAL_SURFACE ( 'NONE', #45294, 1.749999999999998002 ) ;
#414 = CARTESIAN_POINT ( 'NONE',  ( -21.05000000000000071, 56.46250644710310951, -240.6794019422471251 ) ) ;
#416 = VERTEX_POINT ( 'NONE', #243460 ) ;
#415 = CARTESIAN_POINT ( 'NONE',  ( -20.94999999999999929, -11.48912529306489994, -130.9000000000000341 ) ) ;
#417 = CARTESIAN_POINT ( 'NONE',  ( -23.15000000000000213, 11.65000000001115588, -88.75000000000004263 ) ) ;
#418 = ORIENTED_EDGE ( 'NONE', *, *, #6305, .F. ) ;
#419 = CARTESIAN_POINT ( 'NONE',  ( -18.40000000000000213, 64.52683809664901560, -45.34905355133235361 ) ) ;
#420 = CARTESIAN_POINT ( 'NONE',  ( -20.64999999999999858, 1.115625160336667635E-11, -169.5000000000000284 ) ) ;
#421 = CARTESIAN_POINT ( 'NONE',  ( -12.25000000000000178, 66.15000000001155911, -52.77310748452439526 ) ) ;
#422 = ORIENTED_EDGE ( 'NONE', *, *, #103927, .F. ) ;
#423 = CARTESIAN_POINT ( 'NONE',  ( 23.50000000000005684, 64.35000000001120668, -36.02310748452479316 ) ) ;
#424 = CARTESIAN_POINT ( 'NONE',  ( 23.14999999999999858, 5.000000000011153745, -146.4052660189131245 ) ) ;
#425 = CARTESIAN_POINT ( 'NONE',  ( 21.05000000000000071, 65.27628289530457550, -128.8581939154367717 ) ) ;
#426 = AXIS2_PLACEMENT_3D ( 'NONE', #170438, #150818, #257245 ) ;
#427 = EDGE_LOOP ( 'NONE', ( #38646, #216992, #230740, #125875 ) ) ;
#428 = CARTESIAN_POINT ( 'NONE',  ( 13.99999999999999822, 47.91805600923871822, -233.7139610577891631 ) ) ;
#429 = VERTEX_POINT ( 'NONE', #64820 ) ;
#430 = EDGE_LOOP ( 'NONE', ( #122674, #216629, #10019, #127244 ) ) ;
#431 = CARTESIAN_POINT ( 'NONE',  ( -18.59999999999999787, 64.25000000001244871, -170.0231074845244166 ) ) ;
#432 = ORIENTED_EDGE ( 'NONE', *, *, #190307, .F. ) ;
#433 = VERTEX_POINT ( 'NONE', #45265 ) ;
#434 = CARTESIAN_POINT ( 'NONE',  ( -16.84421487269769102, 9.950000000011138823, -79.66950212244499596 ) ) ;
#435 = EDGE_CURVE ( 'NONE', #50141, #155954, #166590, .T. ) ;
#436 = CARTESIAN_POINT ( 'NONE',  ( -16.93211319090181988, 9.999986781168624717, -188.4225054992730293 ) ) ;
#437 = ORIENTED_EDGE ( 'NONE', *, *, #217472, .F. ) ;
#438 = ADVANCED_FACE ( 'NONE', ( #220054 ), #102639, .T. ) ;
#439 = ORIENTED_EDGE ( 'NONE', *, *, #203304, .T. ) ;
#440 = CARTESIAN_POINT ( 'NONE',  ( -23.15000000000000213, 11.75000000000000355, -26.65839931010294350 ) ) ;
#441 = LINE ( 'NONE', #175283, #227247 ) ;
#442 = VERTEX_POINT ( 'NONE', #204323 ) ;
#443 = AXIS2_PLACEMENT_3D ( 'NONE', #84004, #106171, #207893 ) ;
#444 = AXIS2_PLACEMENT_3D ( 'NONE', #191508, #53247, #36272 ) ;
#446 = EDGE_CURVE ( 'NONE', #92780, #16498, #242176, .T. ) ;
#445 = EDGE_LOOP ( 'NONE', ( #60488, #4015, #173917, #89051 ) ) ;
#447 = B_SPLINE_CURVE_WITH_KNOTS ( 'NONE', 3,
 ( #104583, #22530, #181601, #82451, #44648, #185439, #202431, #102011 ),
 .UNSPECIFIED., .F., .F.,
 ( 4, 2, 2, 4 ),
 ( 0.000000000000000000, 0.0002114466876441559802, 0.0003171700314662930322, 0.0004228933752884300843 ),
 .UNSPECIFIED. ) ;
#448 = ORIENTED_EDGE ( 'NONE', *, *, #174825, .F. ) ;
#449 = VECTOR ( 'NONE', #150397, 1000.000000000000000 ) ;
#450 = CARTESIAN_POINT ( 'NONE',  ( 21.05000000000000071, 69.74218538953655866, -203.6208977758331855 ) ) ;
#451 = DIRECTION ( 'NONE',  ( 0.000000000000000000, 0.9126074666063545004, 0.4088369013363783999 ) ) ;
#452 = DIRECTION ( 'NONE',  ( 1.000000000000000000, 0.000000000000000000, 0.000000000000000000 ) ) ;
#453 = DIRECTION ( 'NONE',  ( 1.000000000000000000, 0.000000000000000000, -0.000000000000000000 ) ) ;
#454 = DIRECTION ( 'NONE',  ( 0.000000000000000000, 0.000000000000000000, -1.000000000000000000 ) ) ;
#455 = AXIS2_PLACEMENT_3D ( 'NONE', #75670, #54785, #56055 ) ;
#456 = SPHERICAL_SURFACE ( 'NONE', #94402, 0.1000000000000000056 ) ;
#458 = EDGE_CURVE ( 'NONE', #4905, #253894, #120982, .T. ) ;
#457 = DIRECTION ( 'NONE',  ( 1.000000000000000000, 0.000000000000000000, 0.000000000000000000 ) ) ;
#460 = CARTESIAN_POINT ( 'NONE',  ( 21.09813707148777340, 6.385062105747659977, -100.4686485004705219 ) ) ;
#459 = CARTESIAN_POINT ( 'NONE',  ( -16.77779411440718249, 66.05389855290464141, -149.1861649015289402 ) ) ;
#461 = FACE_OUTER_BOUND ( 'NONE', #189351, .T. ) ;
#462 = CARTESIAN_POINT ( 'NONE',  ( -16.77180007708461318, 22.96538637364528412, -230.9282705005597620 ) ) ;
#463 = DIRECTION ( 'NONE',  ( -1.000000000000000000, 0.000000000000000000, -0.000000000000000000 ) ) ;
#464 = CARTESIAN_POINT ( 'NONE',  ( -15.55912972643740488, 29.51733789627897409, -236.0932609367895907 ) ) ;
#465 = ORIENTED_EDGE ( 'NONE', *, *, #48822, .T. ) ;
#466 = EDGE_CURVE ( 'NONE', #193723, #152968, #120794, .T. ) ;
#468 = ORIENTED_EDGE ( 'NONE', *, *, #8297, .T. ) ;
#467 = CARTESIAN_POINT ( 'NONE',  ( -12.25000000000000178, 47.91805600923872532, -233.7139610577891631 ) ) ;
#469 = CARTESIAN_POINT ( 'NONE',  ( 18.59999999999999076, 64.75617845954087670, -200.4736850529726269 ) ) ;
#470 = DIRECTION ( 'NONE',  ( 0.000000000000000000, 0.9998779222360096863, -0.01562500000001061998 ) ) ;
#471 = ADVANCED_FACE ( 'NONE', ( #161377 ), #240905, .T. ) ;
#472 = EDGE_CURVE ( 'NONE', #99142, #37547, #63531, .T. ) ;
#473 = DIRECTION ( 'NONE',  ( -1.000000000000000000, -0.000000000000000000, -0.000000000000000000 ) ) ;
#474 = EDGE_LOOP ( 'NONE', ( #173375, #214797, #80010, #38035 ) ) ;
#475 = AXIS2_PLACEMENT_3D ( 'NONE', #177956, #81371, #38431 ) ;
#476 =( LENGTH_UNIT ( ) NAMED_UNIT ( * ) SI_UNIT ( .MILLI., .METRE. ) );
#477 = CARTESIAN_POINT ( 'NONE',  ( -20.94999999999999929, 44.43513953521873106, -247.3415577889845736 ) ) ;
#478 = VECTOR ( 'NONE', #249908, 1000.000000000000000 ) ;
#479 = CARTESIAN_POINT ( 'NONE',  ( -17.11825945287481687, 9.950000000011138823, -54.25000000000000711 ) ) ;
#480 = ORIENTED_EDGE ( 'NONE', *, *, #233587, .T. ) ;
#481 = EDGE_CURVE ( 'NONE', #3545, #139104, #71272, .T. ) ;
#482 = CARTESIAN_POINT ( 'NONE',  ( -18.52643265882458579, 10.31973158071402530, -206.5505334713354273 ) ) ;
#483 = CYLINDRICAL_SURFACE ( 'NONE', #100617, 0.1000000000000055844 ) ;
#485 = ADVANCED_FACE ( 'NONE', ( #188619 ), #68687, .F. ) ;
#484 = CIRCLE ( 'NONE', #104535, 0.09999999999998898659 ) ;
#486 = DIRECTION ( 'NONE',  ( 1.000000000000000000, -7.304098846218134667E-16, -5.100424963727256530E-30 ) ) ;
#487 = AXIS2_PLACEMENT_3D ( 'NONE', #75647, #218977, #256772 ) ;
#488 = CARTESIAN_POINT ( 'NONE',  ( -20.94999999999999929, 69.15387683765929694, -99.28538121767448388 ) ) ;
#490 = ORIENTED_EDGE ( 'NONE', *, *, #191260, .T. ) ;
#489 = CARTESIAN_POINT ( 'NONE',  ( -20.94999999999999929, 67.49462292596868451, -195.5612049585272700 ) ) ;
#491 = ADVANCED_FACE ( 'NONE', ( #30869 ), #107802, .F. ) ;
#493 = VERTEX_POINT ( 'NONE', #148215 ) ;
#492 = DIRECTION ( 'NONE',  ( 0.000000000000000000, -1.000000000000000000, -2.891205793294679805E-16 ) ) ;
#495 = VECTOR ( 'NONE', #96044, 1000.000000000000000 ) ;
#494 = DIRECTION ( 'NONE',  ( 0.000000000000000000, -1.000000000000000000, -2.891205793294679805E-16 ) ) ;
#496 = FACE_OUTER_BOUND ( 'NONE', #17360, .T. ) ;
#497 = CARTESIAN_POINT ( 'NONE',  ( -22.10000000000000142, -11.65000000000000036, 12.09999999999999609 ) ) ;
#498 = EDGE_CURVE ( 'NONE', #61807, #44661, #190075, .T. ) ;
#500 = DIRECTION ( 'NONE',  ( 1.000000000000000000, 0.000000000000000000, 0.000000000000000000 ) ) ;
#499 = CARTESIAN_POINT ( 'NONE',  ( -16.94132844910802049, 63.05686860792959436, -213.0719227120540609 ) ) ;
#501 = DIRECTION ( 'NONE',  ( 0.000000000000000000, -1.000000000000000000, -6.982962677686266711E-15 ) ) ;
#502 = CARTESIAN_POINT ( 'NONE',  ( 22.39999999999999503, 11.75000000001115552, -67.00000000000004263 ) ) ;
#504 = DIRECTION ( 'NONE',  ( 0.000000000000000000, 1.000000000000000000, 0.000000000000000000 ) ) ;
#503 = AXIS2_PLACEMENT_3D ( 'NONE', #254332, #51308, #249556 ) ;
#505 = CARTESIAN_POINT ( 'NONE',  ( -18.40000000000000213, 85.50000000001242029, -163.4229180933022860 ) ) ;
#506 = CARTESIAN_POINT ( 'NONE',  ( 21.14999999999999858, 10.21728496540352360, -227.9671432372868765 ) ) ;
#507 = EDGE_CURVE ( 'NONE', #246385, #131339, #94376, .T. ) ;
#509 = EDGE_CURVE ( 'NONE', #239043, #160419, #536, .T. ) ;
#508 = AXIS2_PLACEMENT_3D ( 'NONE', #214942, #57126, #117135 ) ;
#510 = ORIENTED_EDGE ( 'NONE', *, *, #73936, .T. ) ;
#511 = CARTESIAN_POINT ( 'NONE',  ( -23.25000000000000000, 2.000000000011154189, -53.77537807723790309 ) ) ;
#512 = EDGE_LOOP ( 'NONE', ( #80460, #76518, #125761, #137091, #11787, #28045, #59353 ) ) ;
#513 = CIRCLE ( 'NONE', #221269, 0.09999999999999939493 ) ;
#514 = VERTEX_POINT ( 'NONE', #110365 ) ;
#515 = EDGE_CURVE ( 'NONE', #206460, #129055, #226257, .T. ) ;
#516 = CARTESIAN_POINT ( 'NONE',  ( 20.97438252431638972, 67.07457649393589350, -94.55073679551357202 ) ) ;
#517 = CARTESIAN_POINT ( 'NONE',  ( 21.05000000000000071, 78.89331866122350334, -228.7665898296168052 ) ) ;
#518 = ORIENTED_EDGE ( 'NONE', *, *, #173023, .F. ) ;
#519 = CIRCLE ( 'NONE', #54870, 0.1000000000000028644 ) ;
#520 = ADVANCED_FACE ( 'NONE', ( #209471 ), #170403, .T. ) ;
#521 = EDGE_CURVE ( 'NONE', #72122, #174796, #227746, .T. ) ;
#522 = EDGE_LOOP ( 'NONE', ( #79861, #184621, #166928, #70389 ) ) ;
#523 = FILL_AREA_STYLE_COLOUR ( '', #40236 ) ;
#524 = EDGE_CURVE ( 'NONE', #89812, #126094, #5508, .T. ) ;
#526 = ORIENTED_EDGE ( 'NONE', *, *, #181331, .T. ) ;
#525 = VECTOR ( 'NONE', #181803, 1000.000000000000000 ) ;
#527 = AXIS2_PLACEMENT_3D ( 'NONE', #46875, #130268, #126427 ) ;
#528 = VECTOR ( 'NONE', #86821, 1000.000000000000000 ) ;
#529 = EDGE_LOOP ( 'NONE', ( #16011, #85095, #85187, #255666 ) ) ;
#530 = AXIS2_PLACEMENT_3D ( 'NONE', #16682, #154923, #256492 ) ;
#531 = CARTESIAN_POINT ( 'NONE',  ( -21.05000000000000071, 40.27305497204160645, -251.4871534980821082 ) ) ;
#532 = LINE ( 'NONE', #140035, #145210 ) ;
#533 = DIRECTION ( 'NONE',  ( 1.000000000000000000, 0.000000000000000000, 0.000000000000000000 ) ) ;
#534 = LINE ( 'NONE', #56632, #244821 ) ;
#536 = CIRCLE ( 'NONE', #105450, 0.09999999999998898659 ) ;
#535 = CARTESIAN_POINT ( 'NONE',  ( -23.25000000000000000, 71.75000000001186606, -90.87310748452432563 ) ) ;
#537 = DIRECTION ( 'NONE',  ( 1.000000000000000000, 0.000000000000000000, -0.000000000000000000 ) ) ;
#538 = DIRECTION ( 'NONE',  ( 1.000000000000000000, 0.000000000000000000, 0.000000000000000000 ) ) ;
#540 = ORIENTED_EDGE ( 'NONE', *, *, #177845, .T. ) ;
#539 = FACE_OUTER_BOUND ( 'NONE', #95996, .T. ) ;
#542 = DIRECTION ( 'NONE',  ( 0.000000000000000000, 0.000000000000000000, 1.000000000000000000 ) ) ;
#541 = CARTESIAN_POINT ( 'NONE',  ( -16.97683809663753962, 66.05000000001226113, -149.7946366524138284 ) ) ;
#543 = EDGE_CURVE ( 'NONE', #117026, #131456, #76254, .T. ) ;
#544 = CARTESIAN_POINT ( 'NONE',  ( -20.64999999999999858, 67.23127455305841238, -235.8551265064783991 ) ) ;
#545 = ORIENTED_EDGE ( 'NONE', *, *, #247092, .F. ) ;
#546 = DIRECTION ( 'NONE',  ( 1.000000000000000000, 0.000000000000000000, 0.000000000000000000 ) ) ;
#547 = FACE_OUTER_BOUND ( 'NONE', #29913, .T. ) ;
#548 = ORIENTED_EDGE ( 'NONE', *, *, #24283, .F. ) ;
#550 = CARTESIAN_POINT ( 'NONE',  ( -20.94999999999999929, 74.25000000001156764, -57.85359592662268824 ) ) ;
#549 = DIRECTION ( 'NONE',  ( 0.000000000000000000, 0.000000000000000000, 1.000000000000000000 ) ) ;
#551 = CARTESIAN_POINT ( 'NONE',  ( 18.39999999999999503, 64.25000000001253397, -179.2731074845244450 ) ) ;
#552 = DIRECTION ( 'NONE',  ( 0.000000000000000000, 0.000000000000000000, -1.000000000000000000 ) ) ;
#553 = ORIENTED_EDGE ( 'NONE', *, *, #95844, .F. ) ;
#554 = FACE_OUTER_BOUND ( 'NONE', #175787, .T. ) ;
#555 = CARTESIAN_POINT ( 'NONE',  ( -18.33682934331559267, -0.6949736787240441416, -242.5041756961801980 ) ) ;
#556 = DIRECTION ( 'NONE',  ( 0.000000000000000000, 6.982962677686267499E-15, -1.000000000000000000 ) ) ;
#557 = CARTESIAN_POINT ( 'NONE',  ( 16.87683809663750267, 9.950000000011138823, -146.6500000000000341 ) ) ;
#558 = ORIENTED_EDGE ( 'NONE', *, *, #48980, .F. ) ;
#559 = CARTESIAN_POINT ( 'NONE',  ( -21.14999999999999858, 64.35000000001262777, -196.7392418215462726 ) ) ;
#560 = CARTESIAN_POINT ( 'NONE',  ( -17.73285935860190676, 10.85798180380700728, -123.7585618097890148 ) ) ;
#561 = EDGE_CURVE ( 'NONE', #167581, #177661, #248601, .T. ) ;
#562 = CARTESIAN_POINT ( 'NONE',  ( -23.25000000000000000, 76.00000000001165290, -61.62310748452430431 ) ) ;
#563 = DIRECTION ( 'NONE',  ( 1.000000000000000000, -7.049440681616512959E-16, 1.911869773728117674E-16 ) ) ;
#564 = DIRECTION ( 'NONE',  ( 0.000000000000000000, 0.9550021345545507412, -0.2965989261549202838 ) ) ;
#565 = EDGE_CURVE ( 'NONE', #186188, #257228, #38296, .T. ) ;
#566 = DIRECTION ( 'NONE',  ( 0.000000000000000000, 0.000000000000000000, -1.000000000000000000 ) ) ;
#567 = AXIS2_PLACEMENT_3D ( 'NONE', #191071, #17524, #234014 ) ;
#569 = ORIENTED_EDGE ( 'NONE', *, *, #82426, .T. ) ;
#568 = CARTESIAN_POINT ( 'NONE',  ( 18.39999999999999503, 32.67104411594546320, -237.4063322638886859 ) ) ;
#570 = CARTESIAN_POINT ( 'NONE',  ( -23.25000000000000000, 23.68770167995059595, -252.8127582590406348 ) ) ;
#571 = CARTESIAN_POINT ( 'NONE',  ( -21.05000000000000071, 1.115649653272650466E-11, -171.5000000000000284 ) ) ;
#572 = DIRECTION ( 'NONE',  ( 0.000000000000000000, -1.000000000000000000, 0.000000000000000000 ) ) ;
#573 = CARTESIAN_POINT ( 'NONE',  ( 21.05000000000000071, 10.68429367439853905, -175.0266739386375150 ) ) ;
#575 = ORIENTED_EDGE ( 'NONE', *, *, #24922, .T. ) ;
#574 = CARTESIAN_POINT ( 'NONE',  ( 20.94999999999999574, 44.06250559941687328, -258.7395785465160429 ) ) ;
#576 = DIRECTION ( 'NONE',  ( 0.000000000000000000, 1.000000000000000000, 0.000000000000000000 ) ) ;
#577 = DIRECTION ( 'NONE',  ( 0.000000000000000000, -7.172728831056617961E-15, 1.000000000000000000 ) ) ;
#578 = ORIENTED_EDGE ( 'NONE', *, *, #68615, .F. ) ;
#579 = DIRECTION ( 'NONE',  ( 1.000000000000000000, 0.000000000000000000, 0.000000000000000000 ) ) ;
#580 = CARTESIAN_POINT ( 'NONE',  ( 21.04999999999999716, 76.01454569058392963, -176.5201252709579194 ) ) ;
#581 = LINE ( 'NONE', #39765, #75360 ) ;
#582 = ADVANCED_FACE ( 'NONE', ( #208207 ), #150784, .T. ) ;
#584 = CIRCLE ( 'NONE', #183777, 0.1000000000000033362 ) ;
#583 = CARTESIAN_POINT ( 'NONE',  ( 22.39999999999999858, 59.68594599439719417, -233.9123800762197902 ) ) ;
#586 = AXIS2_PLACEMENT_3D ( 'NONE', #112751, #253528, #74936 ) ;
#585 = DIRECTION ( 'NONE',  ( 0.000000000000000000, 0.000000000000000000, -1.000000000000000000 ) ) ;
#587 = ORIENTED_EDGE ( 'NONE', *, *, #178313, .F. ) ;
#588 = VERTEX_POINT ( 'NONE', #129920 ) ;
#589 = AXIS2_PLACEMENT_3D ( 'NONE', #105465, #182495, #185039 ) ;
#590 = CARTESIAN_POINT ( 'NONE',  ( -18.40000000000000213, 23.63051550414076729, -229.7170656735756324 ) ) ;
#591 = DIRECTION ( 'NONE',  ( 0.000000000000000000, -0.000000000000000000, 1.000000000000000000 ) ) ;
#592 =( BOUNDED_SURFACE ( )  B_SPLINE_SURFACE ( 3, 2, ( 
 ( #139194, #218736, #199202 ),
 ( #179650, #4506, #84001 ),
 ( #64499, #144017, #44937 ),
 ( #124484, #145299, #244407 ),
 ( #65778, #224842, #130882 ),
 ( #30529, #129613, #87880 ) ),
 .UNSPECIFIED., .F., .F., .F. ) 
 B_SPLINE_SURFACE_WITH_KNOTS ( ( 4, 2, 4 ),
 ( 3, 3 ),
 ( 0.0001342700090130149982, 0.0002909192928057525150, 0.0004475685765984900046 ),
 ( 0.000000000000000000, 1.000000000000000000 ),
 .UNSPECIFIED. ) 
 GEOMETRIC_REPRESENTATION_ITEM ( )  RATIONAL_B_SPLINE_SURFACE ( (
 ( 1.000000000000000000, 0.7250110520819876836, 1.000000000000000000),
 ( 1.000000000000000000, 0.7257599279122789460, 1.000000000000000000),
 ( 1.000000000000000000, 0.7137594617299418687, 1.000000000000000000),
 ( 1.000000000000000000, 0.6959270178795029516, 1.000000000000000000),
 ( 1.000000000000000000, 0.6919879549349066128, 1.000000000000000000),
 ( 1.000000000000000000, 0.7071067811865494601, 1.000000000000000000) ) ) 
 REPRESENTATION_ITEM ( '' )  SURFACE ( )  );
#593 = DIRECTION ( 'NONE',  ( 1.000000000000000000, 0.000000000000000000, 0.000000000000000000 ) ) ;
#594 = DIRECTION ( 'NONE',  ( -1.000000000000000000, 0.000000000000000000, 0.000000000000000000 ) ) ;
#595 = ORIENTED_EDGE ( 'NONE', *, *, #102002, .T. ) ;
#596 = CARTESIAN_POINT ( 'NONE',  ( -21.14999999999999858, -1.427715776309795404, -194.9144328397408401 ) ) ;
#597 = AXIS2_PLACEMENT_3D ( 'NONE', #30263, #69391, #11991 ) ;
#598 = DIRECTION ( 'NONE',  ( -0.7071067811865474617, -0.7071067811865474617, -0.000000000000000000 ) ) ;
#599 = CARTESIAN_POINT ( 'NONE',  ( 20.94999999999999929, 67.22371710471975348, -148.7731074845244166 ) ) ;
#600 = ORIENTED_EDGE ( 'NONE', *, *, #38576, .F. ) ;
#601 = CARTESIAN_POINT ( 'NONE',  ( -16.87331047859649757, 66.05000000001153637, -48.67310748452439384 ) ) ;
#602 = ORIENTED_EDGE ( 'NONE', *, *, #47162, .T. ) ;
#603 = VERTEX_POINT ( 'NONE', #169105 ) ;
#604 = SPHERICAL_SURFACE ( 'NONE', #217070, 0.1000000000000000056 ) ;
#605 = DIRECTION ( 'NONE',  ( 1.000000000000000000, -0.000000000000000000, 0.000000000000000000 ) ) ;
#606 = DIRECTION ( 'NONE',  ( -0.000000000000000000, 0.4721928772777331806, 0.8814952561688438326 ) ) ;
#607 = EDGE_LOOP ( 'NONE', ( #13906, #218176, #236632, #54115 ) ) ;
#608 = DIRECTION ( 'NONE',  ( -1.000000000000000000, 0.000000000000000000, 0.000000000000000000 ) ) ;
#609 = LINE ( 'NONE', #234103, #72056 ) ;
#610 = EDGE_CURVE ( 'NONE', #44096, #9432, #54358, .T. ) ;
#611 = VERTEX_POINT ( 'NONE', #153398 ) ;
#612 = CARTESIAN_POINT ( 'NONE',  ( 22.48660254037843842, 11.75000000001115730, -100.4500000000000313 ) ) ;
#614 = ORIENTED_EDGE ( 'NONE', *, *, #241541, .T. ) ;
#613 = DIRECTION ( 'NONE',  ( 0.000000000000000000, -6.982962677686266711E-15, 1.000000000000000000 ) ) ;
#615 = CIRCLE ( 'NONE', #146367, 2.000000000000005773 ) ;
#616 = VECTOR ( 'NONE', #164742, 1000.000000000000000 ) ;
#618 = ADVANCED_FACE ( 'NONE', ( #152096 ), #136321, .T. ) ;
#617 = DIRECTION ( 'NONE',  ( 2.557131231893037478E-16, 0.8660254037844420383, -0.4999999999999942824 ) ) ;
#619 = DIRECTION ( 'NONE',  ( -2.578261006436899437E-14, -0.1350103645451973811, 0.9908441862701586889 ) ) ;
#620 = CIRCLE ( 'NONE', #221208, 0.2000000000000057288 ) ;
#621 = ORIENTED_EDGE ( 'NONE', *, *, #77674, .T. ) ;
#622 = CARTESIAN_POINT ( 'NONE',  ( -21.05000000000000071, 76.25610579210490414, -203.5580039261966760 ) ) ;
#624 = EDGE_CURVE ( 'NONE', #224260, #121586, #254952, .T. ) ;
#623 = CARTESIAN_POINT ( 'NONE',  ( 21.06490991615909181, 10.72489134759826790, -79.20371135353316561 ) ) ;
#625 = DIRECTION ( 'NONE',  ( 0.000000000000000000, -6.467318590049456648E-15, 1.000000000000000000 ) ) ;
#626 = ORIENTED_EDGE ( 'NONE', *, *, #237164, .T. ) ;
#627 = CARTESIAN_POINT ( 'NONE',  ( 18.49999999999999645, 1.637172712981537659, -45.08215336547201701 ) ) ;
#629 = EDGE_CURVE ( 'NONE', #170828, #113349, #13847, .T. ) ;
#628 = CARTESIAN_POINT ( 'NONE',  ( 20.94999999999999574, 69.65000000001187175, -93.17928539484123007 ) ) ;
#630 = CARTESIAN_POINT ( 'NONE',  ( -18.59999999999999787, 1.115600667400684642E-11, -67.00000000000004263 ) ) ;
#631 = ORIENTED_EDGE ( 'NONE', *, *, #65245, .T. ) ;
#632 = EDGE_CURVE ( 'NONE', #13934, #143709, #236723, .T. ) ;
#633 = VERTEX_POINT ( 'NONE', #171670 ) ;
#634 = ORIENTED_EDGE ( 'NONE', *, *, #116099, .T. ) ;
#635 = ORIENTED_EDGE ( 'NONE', *, *, #34729, .F. ) ;
#636 = DIRECTION ( 'NONE',  ( 1.000000000000000000, 0.000000000000000000, 0.000000000000000000 ) ) ;
#638 = EDGE_CURVE ( 'NONE', #245148, #85564, #76363, .T. ) ;
#637 = CARTESIAN_POINT ( 'NONE',  ( 21.12400222705963060, 8.778511907088196509, -45.75000000000000000 ) ) ;
#639 = VECTOR ( 'NONE', #154118, 1000.000000000000114 ) ;
#641 = EDGE_LOOP ( 'NONE', ( #78881, #244574, #237015, #68225, #250908, #111414, #247052, #30325, #136634, #124686, #247417, #184716 ) ) ;
#640 = CARTESIAN_POINT ( 'NONE',  ( 18.52928932188133970, 10.27928932189250411, -158.6500000000000057 ) ) ;
#642 = FACE_OUTER_BOUND ( 'NONE', #91854, .T. ) ;
#643 = DIRECTION ( 'NONE',  ( -1.000000000000000000, 0.000000000000000000, 0.000000000000000000 ) ) ;
#644 = CARTESIAN_POINT ( 'NONE',  ( 23.15000000000000213, 85.00000000001149658, -45.91707660717670336 ) ) ;
#645 = CARTESIAN_POINT ( 'NONE',  ( 20.94999999999999574, 77.83534155023670564, -158.3679561919613548 ) ) ;
#646 = FACE_OUTER_BOUND ( 'NONE', #203716, .T. ) ;
#647 = CIRCLE ( 'NONE', #158927, 11.80000000000001670 ) ;
#648 = DIRECTION ( 'NONE',  ( 0.000000000000000000, 0.2128009952263604232, -0.9770955615653316162 ) ) ;
#650 = ORIENTED_EDGE ( 'NONE', *, *, #214860, .F. ) ;
#649 = DIRECTION ( 'NONE',  ( 0.000000000000000000, -0.6728971962616965286, 0.7397360091702632756 ) ) ;
#652 = ORIENTED_EDGE ( 'NONE', *, *, #252109, .F. ) ;
#651 = DIRECTION ( 'NONE',  ( 1.000000000000000000, 0.000000000000000000, 0.000000000000000000 ) ) ;
#653 = CARTESIAN_POINT ( 'NONE',  ( -16.85718274719388177, 60.89144504857533491, -221.1185173850411445 ) ) ;
#654 = VERTEX_POINT ( 'NONE', #97177 ) ;
#655 = ORIENTED_EDGE ( 'NONE', *, *, #91877, .T. ) ;
#656 = CARTESIAN_POINT ( 'NONE',  ( -21.44999999999999929, 68.75000000001151079, -48.27310748452437394 ) ) ;
#657 = DIRECTION ( 'NONE',  ( 1.000000000000000000, 0.000000000000000000, 0.000000000000000000 ) ) ;
#658 = CIRCLE ( 'NONE', #225521, 0.1000000000000013933 ) ;
#659 = DIRECTION ( 'NONE',  ( 0.000000000000000000, -0.9876197685951263461, 0.1568667991644794590 ) ) ;
#660 = CIRCLE ( 'NONE', #167314, 0.1000000000000002554 ) ;
#661 = DIRECTION ( 'NONE',  ( 0.000000000000000000, 0.000000000000000000, 1.000000000000000000 ) ) ;
#662 = CARTESIAN_POINT ( 'NONE',  ( -18.40000000000000213, 64.25000000001199396, -112.2731074845243739 ) ) ;
#663 = DIRECTION ( 'NONE',  ( 0.000000000000000000, 0.000000000000000000, -1.000000000000000000 ) ) ;
#664 = AXIS2_PLACEMENT_3D ( 'NONE', #248100, #70784, #68187 ) ;
#665 = FACE_OUTER_BOUND ( 'NONE', #166817, .T. ) ;
#666 = ORIENTED_EDGE ( 'NONE', *, *, #40911, .T. ) ;
#667 = EDGE_LOOP ( 'NONE', ( #215294, #148642, #179262, #17609, #245790 ) ) ;
#668 = SURFACE_STYLE_USAGE ( .BOTH. , #22864 ) ;
#669 = AXIS2_PLACEMENT_3D ( 'NONE', #62579, #85950, #142101 ) ;
#670 = VERTEX_POINT ( 'NONE', #54237 ) ;
#671 = DIRECTION ( 'NONE',  ( 0.000000000000000000, 6.982962677686266711E-15, -1.000000000000000000 ) ) ;
#672 = CARTESIAN_POINT ( 'NONE',  ( -23.15000000000000213, -8.999999999988846255, -176.8939691226524076 ) ) ;
#674 = ADVANCED_FACE ( 'NONE', ( #35989 ), #104880, .F. ) ;
#673 = CARTESIAN_POINT ( 'NONE',  ( 21.46681500597178882, 76.00000000001243450, -176.8806186439590249 ) ) ;
#676 =( BOUNDED_SURFACE ( )  B_SPLINE_SURFACE ( 3, 2, ( 
 ( #42500, #144156, #123339 ),
 ( #141606, #122052, #161182 ),
 ( #201576, #238130, #24253 ),
 ( #39977, #239438, #103734 ),
 ( #45076, #120792, #243261 ),
 ( #223694, #59464, #119492 ) ),
 .UNSPECIFIED., .F., .F., .F. ) 
 B_SPLINE_SURFACE_WITH_KNOTS ( ( 4, 2, 4 ),
 ( 3, 3 ),
 ( 4.712388980384689674, 5.497787143782137953, 6.283185307179586232 ),
 ( 0.000000000000000000, 1.000000000000000000 ),
 .UNSPECIFIED. ) 
 GEOMETRIC_REPRESENTATION_ITEM ( )  RATIONAL_B_SPLINE_SURFACE ( (
 ( 1.000000000000000000, 0.7071067811865536790, 1.000000000000000000),
 ( 1.000000000000000000, 0.7727932973495903468, 1.000000000000000000),
 ( 1.000000000000000000, 0.8282379607643433062, 1.000000000000000000),
 ( 1.000000000000000000, 0.9038128468045532049, 1.000000000000000000),
 ( 1.000000000000000000, 0.9240297172239071433, 1.000000000000000000),
 ( 1.000000000000000000, 0.9238795325112914014, 1.000000000000000000) ) ) 
 REPRESENTATION_ITEM ( '' )  SURFACE ( )  );
#675 = AXIS2_PLACEMENT_3D ( 'NONE', #77860, #154878, #178290 ) ;
#677 = CARTESIAN_POINT ( 'NONE',  ( -21.05000000000000426, 57.84918772656043018, -226.1321410194968280 ) ) ;
#678 = ORIENTED_EDGE ( 'NONE', *, *, #100875, .T. ) ;
#679 = CARTESIAN_POINT ( 'NONE',  ( -23.25000000000000000, -1.835859311432481045, -212.6044391687984785 ) ) ;
#680 = EDGE_LOOP ( 'NONE', ( #34192, #227915, #87333 ) ) ;
#682 = ADVANCED_FACE ( 'NONE', ( #93369 ), #256227, .F. ) ;
#681 = DIRECTION ( 'NONE',  ( 1.000000000000000000, -0.000000000000000000, -0.000000000000000000 ) ) ;
#683 = ORIENTED_EDGE ( 'NONE', *, *, #92102, .F. ) ;
#684 = DIRECTION ( 'NONE',  ( -1.000000000000000000, 0.000000000000000000, 0.000000000000000000 ) ) ;
#685 = EDGE_CURVE ( 'NONE', #12588, #160946, #231620, .T. ) ;
#686 = CARTESIAN_POINT ( 'NONE',  ( -16.89268316805466341, 9.951721813253341153, -113.1442475214544885 ) ) ;
#687 = EDGE_CURVE ( 'NONE', #34471, #187182, #9630, .T. ) ;
#688 = ORIENTED_EDGE ( 'NONE', *, *, #183122, .T. ) ;
#689 = CYLINDRICAL_SURFACE ( 'NONE', #44570, 11.80000000000000426 ) ;
#691 = VERTEX_POINT ( 'NONE', #157234 ) ;
#690 = DIRECTION ( 'NONE',  ( 1.000000000000000000, 0.000000000000000000, -0.000000000000000000 ) ) ;
#692 = VECTOR ( 'NONE', #235400, 1000.000000000000114 ) ;
#693 = LINE ( 'NONE', #254979, #156291 ) ;
#695 = VERTEX_POINT ( 'NONE', #253718 ) ;
#694 = TOROIDAL_SURFACE ( 'NONE', #134002, 0.2000000000000000111, 0.1000000000000000056 ) ;
#696 = VECTOR ( 'NONE', #239567, 1000.000000000000227 ) ;
#697 = AXIS2_PLACEMENT_3D ( 'NONE', #238510, #41624, #258027 ) ;
#698 = DIRECTION ( 'NONE',  ( -1.000000000000000000, 0.000000000000000000, 0.000000000000000000 ) ) ;
#699 = EDGE_LOOP ( 'NONE', ( #15772, #45586, #89651 ) ) ;
#700 = EDGE_CURVE ( 'NONE', #10156, #141625, #51297, .T. ) ;
#701 = CARTESIAN_POINT ( 'NONE',  ( 16.87683809663750267, 22.97806745954241592, -230.9350634111226270 ) ) ;
#702 = CARTESIAN_POINT ( 'NONE',  ( 20.04142135623731136, 64.25000000001250555, -178.8731074845244393 ) ) ;
#703 = CARTESIAN_POINT ( 'NONE',  ( -20.54999999999999716, 1.115625160336667635E-11, -69.00000000000000000 ) ) ;
#704 = CARTESIAN_POINT ( 'NONE',  ( -16.86733706339143524, 9.965990529650820662, -121.4031153019987386 ) ) ;
#705 = EDGE_CURVE ( 'NONE', #15348, #228584, #142870, .T. ) ;
#706 = CARTESIAN_POINT ( 'NONE',  ( -23.15000000000000213, 1.115600667400684642E-11, -167.5000000000000284 ) ) ;
#707 = ORIENTED_EDGE ( 'NONE', *, *, #23388, .F. ) ;
#708 = DIRECTION ( 'NONE',  ( 0.000000000000000000, 1.000000000000000000, -0.000000000000000000 ) ) ;
#709 = CARTESIAN_POINT ( 'NONE',  ( 18.69999999999999929, -11.65000000000000036, -15.00000000000000000 ) ) ;
#710 = DIRECTION ( 'NONE',  ( 1.000000000000000000, 0.000000000000000000, 0.000000000000000000 ) ) ;
#711 = EDGE_LOOP ( 'NONE', ( #221584, #172126, #200683, #173138 ) ) ;
#713 = CARTESIAN_POINT ( 'NONE',  ( -21.14999999999999858, 76.00000000001200817, -109.5637644362255543 ) ) ;
#712 = CIRCLE ( 'NONE', #213125, 0.8750000000000007772 ) ;
#714 = EDGE_LOOP ( 'NONE', ( #126745, #183780, #201751, #236755 ) ) ;
#715 = CARTESIAN_POINT ( 'NONE',  ( -16.87683809663752399, 21.23804903844422043, -146.6500000000000341 ) ) ;
#716 = ORIENTED_EDGE ( 'NONE', *, *, #78279, .T. ) ;
#717 = CARTESIAN_POINT ( 'NONE',  ( 20.94999999999999929, 77.36242903720570041, -162.1342262366031548 ) ) ;
#718 = FACE_OUTER_BOUND ( 'NONE', #166984, .T. ) ;
#719 = EDGE_CURVE ( 'NONE', #17064, #33613, #92090, .T. ) ;
#720 = ORIENTED_EDGE ( 'NONE', *, *, #92942, .T. ) ;
#722 = EDGE_LOOP ( 'NONE', ( #109350, #213225, #212878, #122895 ) ) ;
#721 = LINE ( 'NONE', #159848, #119717 ) ;
#723 = ADVANCED_FACE ( 'NONE', ( #191226 ), #255273, .F. ) ;
#724 = CARTESIAN_POINT ( 'NONE',  ( -18.52186455168981638, 8.844482643606943029, -245.4073368711099477 ) ) ;
#725 = EDGE_LOOP ( 'NONE', ( #93746, #200882, #21273 ) ) ;
#726 = EDGE_CURVE ( 'NONE', #253511, #179129, #72550, .T. ) ;
#727 = DIRECTION ( 'NONE',  ( 0.000000000000000000, 0.9770955615653316162, 0.2128009952263604232 ) ) ;
#728 = DIRECTION ( 'NONE',  ( 0.000000000000000000, 0.9908441862701600211, -0.1350103645451876666 ) ) ;
#729 = VERTEX_POINT ( 'NONE', #162357 ) ;
#730 = ORIENTED_EDGE ( 'NONE', *, *, #103764, .F. ) ;
#731 = FACE_BOUND ( 'NONE', #81297, .T. ) ;
#732 = CARTESIAN_POINT ( 'NONE',  ( -18.40000000000000213, 70.35000000001187459, -90.37310748452433984 ) ) ;
#733 = EDGE_LOOP ( 'NONE', ( #232923, #215789, #253052, #35694 ) ) ;
#734 = DIRECTION ( 'NONE',  ( 0.000000000000000000, -0.9998779222360097974, 0.01562500000000363945 ) ) ;
#735 = ORIENTED_EDGE ( 'NONE', *, *, #173041, .F. ) ;
#736 = ORIENTED_EDGE ( 'NONE', *, *, #51566, .T. ) ;
#737 = AXIS2_PLACEMENT_3D ( 'NONE', #87488, #126631, #168379 ) ;
#738 = FACE_OUTER_BOUND ( 'NONE', #224116, .T. ) ;
#740 = ORIENTED_EDGE ( 'NONE', *, *, #146274, .F. ) ;
#739 = CARTESIAN_POINT ( 'NONE',  ( 21.10000000000000142, 6.223900101154156594, 12.09999999999999964 ) ) ;
#741 = CYLINDRICAL_SURFACE ( 'NONE', #86628, 0.1999999999999987899 ) ;
#742 = DIRECTION ( 'NONE',  ( -1.000000000000000000, -0.000000000000000000, 0.000000000000000000 ) ) ;
#744 = ADVANCED_FACE ( 'NONE', ( #222276 ), #93020, .T. ) ;
#743 = CARTESIAN_POINT ( 'NONE',  ( -16.80469485234341320, 63.08282825821666506, -213.1683133085603856 ) ) ;
#746 = CARTESIAN_POINT ( 'NONE',  ( 20.94999999999999574, -11.64999999998883595, -36.60000000000000853 ) ) ;
#745 = FACE_OUTER_BOUND ( 'NONE', #98219, .T. ) ;
#747 = CYLINDRICAL_SURFACE ( 'NONE', #257067, 0.5000000000000004441 ) ;
#748 = DIRECTION ( 'NONE',  ( 1.000000000000000000, 0.000000000000000000, 0.000000000000000000 ) ) ;
#749 = VECTOR ( 'NONE', #230866, 1000.000000000000000 ) ;
#750 = CARTESIAN_POINT ( 'NONE',  ( 18.41356215285961895, -9.499999999988869348, -40.53206939669960462 ) ) ;
#751 = CIRCLE ( 'NONE', #108925, 0.09999999999998898659 ) ;
#752 = DIRECTION ( 'NONE',  ( 0.000000000000000000, 0.000000000000000000, 1.000000000000000000 ) ) ;
#753 = AXIS2_PLACEMENT_3D ( 'NONE', #237667, #179014, #176429 ) ;
#754 = EDGE_LOOP ( 'NONE', ( #252584, #112082, #982, #102048 ) ) ;
#755 = EDGE_LOOP ( 'NONE', ( #182777, #183423, #9876, #121194 ) ) ;
#756 = ORIENTED_EDGE ( 'NONE', *, *, #206141, .F. ) ;
#757 = EDGE_CURVE ( 'NONE', #213598, #47066, #138218, .T. ) ;
#758 = DIRECTION ( 'NONE',  ( 0.000000000000000000, 0.000000000000000000, -1.000000000000000000 ) ) ;
#759 = ORIENTED_EDGE ( 'NONE', *, *, #133909, .T. ) ;
#760 = LINE ( 'NONE', #80294, #188466 ) ;
#761 = DIRECTION ( 'NONE',  ( 1.224646799147353207E-16, -1.000000000000000000, -6.982962677686266711E-15 ) ) ;
#762 = EDGE_CURVE ( 'NONE', #110751, #214790, #59667, .T. ) ;
#763 = ORIENTED_EDGE ( 'NONE', *, *, #124966, .T. ) ;
#764 = CIRCLE ( 'NONE', #146531, 0.09999999999999949207 ) ;
#766 = EDGE_CURVE ( 'NONE', #120723, #201736, #30504, .T. ) ;
#765 = CARTESIAN_POINT ( 'NONE',  ( -18.39999999999999858, 64.52683809664941350, -93.69716141771641560 ) ) ;
#768 = ORIENTED_EDGE ( 'NONE', *, *, #108329, .T. ) ;
#767 = ORIENTED_EDGE ( 'NONE', *, *, #253164, .T. ) ;
#769 = ORIENTED_EDGE ( 'NONE', *, *, #44737, .T. ) ;
#770 = ORIENTED_EDGE ( 'NONE', *, *, #240435, .F. ) ;
#771 = EDGE_CURVE ( 'NONE', #146335, #61093, #246950, .T. ) ;
#772 = CARTESIAN_POINT ( 'NONE',  ( 18.59999999999999076, 62.49201502323811752, -208.8221019049098857 ) ) ;
#773 = CARTESIAN_POINT ( 'NONE',  ( 20.94999999999999929, 71.00000000001151079, -48.42837350343745584 ) ) ;
#776 = ADVANCED_FACE ( 'NONE', ( #218436 ), #241868, .T. ) ;
#775 = ORIENTED_EDGE ( 'NONE', *, *, #51382, .T. ) ;
#774 = CARTESIAN_POINT ( 'NONE',  ( 20.12500000000000000, 66.25000000001223555, -148.7731074845244450 ) ) ;
#777 = DIRECTION ( 'NONE',  ( 0.000000000000000000, -6.982962677686266711E-15, 1.000000000000000000 ) ) ;
#778 = DIRECTION ( 'NONE',  ( -2.342056488767301376E-15, 0.1350103645451974088, -0.9908441862701587999 ) ) ;
#780 = ORIENTED_EDGE ( 'NONE', *, *, #246088, .F. ) ;
#779 = CARTESIAN_POINT ( 'NONE',  ( 20.95520789717937404, 10.57693059939611224, -141.5802329738748710 ) ) ;
#781 = CARTESIAN_POINT ( 'NONE',  ( 21.05000000000003979, 77.26165318615413469, -44.00978271863746016 ) ) ;
#782 = VERTEX_POINT ( 'NONE', #38545 ) ;
#783 = LINE ( 'NONE', #80319, #8482 ) ;
#785 = VERTEX_POINT ( 'NONE', #120670 ) ;
#784 = CARTESIAN_POINT ( 'NONE',  ( 21.15000000000005187, 82.72707916847673459, -26.51159310135756897 ) ) ;
#786 = DIRECTION ( 'NONE',  ( 0.000000000000000000, 0.9424537609900496271, 0.3343365196859450217 ) ) ;
#787 = CARTESIAN_POINT ( 'NONE',  ( -14.56336952470179824, 27.81851053932208728, -234.0989799278904115 ) ) ;
#788 = VECTOR ( 'NONE', #158193, 1000.000000000000000 ) ;
#789 = CIRCLE ( 'NONE', #92397, 0.09999999999999939493 ) ;
#790 = CARTESIAN_POINT ( 'NONE',  ( 20.85000000106584750, 11.75000000001115907, -60.15550465647353207 ) ) ;
#791 = TOROIDAL_SURFACE ( 'NONE', #108965, 0.4000000000000003553, 0.1000000000000000056 ) ;
#792 = ORIENTED_EDGE ( 'NONE', *, *, #7077, .F. ) ;
#794 = CARTESIAN_POINT ( 'NONE',  ( -18.59999999999999787, 9.350000000011156942, -45.65000000000000568 ) ) ;
#793 = CARTESIAN_POINT ( 'NONE',  ( -16.80070461187922959, 9.950000000011137047, -46.14696382916198303 ) ) ;
#795 = CARTESIAN_POINT ( 'NONE',  ( -15.31895204843005054, 66.60346600605788581, -85.11716770535106491 ) ) ;
#796 = CARTESIAN_POINT ( 'NONE',  ( 18.48413544395647534, 85.66430403364030610, -163.3400024914861888 ) ) ;
#797 = EDGE_CURVE ( 'NONE', #139213, #218531, #126331, .T. ) ;
#798 = CARTESIAN_POINT ( 'NONE',  ( 20.94999999999999929, 67.12338541492522381, -161.6380270056797599 ) ) ;
#799 = CARTESIAN_POINT ( 'NONE',  ( 23.14999999999999858, 71.18691588786234092, -91.08158972800052311 ) ) ;
#800 = ADVANCED_FACE ( 'NONE', ( #141486 ), #137617, .F. ) ;
#801 = ORIENTED_EDGE ( 'NONE', *, *, #154892, .F. ) ;
#802 = ORIENTED_EDGE ( 'NONE', *, *, #150859, .T. ) ;
#803 = EDGE_LOOP ( 'NONE', ( #185870, #252756, #109743, #49629 ) ) ;
#804 = DIRECTION ( 'NONE',  ( -3.265361837132812600E-16, 0.4721928772777346239, 0.8814952561688430555 ) ) ;
#805 = ORIENTED_EDGE ( 'NONE', *, *, #207373, .F. ) ;
#806 = FACE_OUTER_BOUND ( 'NONE', #236236, .T. ) ;
#807 = ORIENTED_EDGE ( 'NONE', *, *, #217651, .F. ) ;
#808 = EDGE_CURVE ( 'NONE', #17724, #122594, #59345, .T. ) ;
#809 = DIRECTION ( 'NONE',  ( -1.000000000000000000, -2.885090398161910739E-16, -6.283419270304611573E-17 ) ) ;
#810 = LINE ( 'NONE', #257668, #225073 ) ;
#811 = AXIS2_PLACEMENT_3D ( 'NONE', #209395, #174172, #150714 ) ;
#812 = EDGE_CURVE ( 'NONE', #61221, #186482, #97065, .T. ) ;
#813 = ORIENTED_EDGE ( 'NONE', *, *, #63724, .F. ) ;
#814 = DIRECTION ( 'NONE',  ( 0.000000000000000000, 0.000000000000000000, -1.000000000000000000 ) ) ;
#815 = EDGE_CURVE ( 'NONE', #144454, #50955, #20274, .T. ) ;
#816 = VERTEX_POINT ( 'NONE', #22856 ) ;
#817 = ORIENTED_EDGE ( 'NONE', *, *, #80729, .T. ) ;
#818 = ORIENTED_EDGE ( 'NONE', *, *, #85034, .T. ) ;
#819 = ADVANCED_FACE ( 'NONE', ( #178071 ), #102324, .T. ) ;
#820 = DIRECTION ( 'NONE',  ( 1.000000000000000000, 0.000000000000000000, 0.000000000000000000 ) ) ;
#821 = CARTESIAN_POINT ( 'NONE',  ( 22.42196299218230493, 75.99755832602546946, -215.1727191871738398 ) ) ;
#822 = FACE_OUTER_BOUND ( 'NONE', #16958, .T. ) ;
#823 = CARTESIAN_POINT ( 'NONE',  ( -22.59080734064478335, 11.75000000001115907, -167.4692502919029380 ) ) ;
#824 = CARTESIAN_POINT ( 'NONE',  ( 21.30000000000002558, 76.00000000001237765, -170.0231074845243597 ) ) ;
#825 = CARTESIAN_POINT ( 'NONE',  ( -21.00000000000000000, 7.800000000000000711, -1.212568896937008089 ) ) ;
#826 = AXIS2_PLACEMENT_3D ( 'NONE', #121089, #76785, #174665 ) ;
#828 = FACE_OUTER_BOUND ( 'NONE', #254581, .T. ) ;
#827 = FACE_OUTER_BOUND ( 'NONE', #190311, .T. ) ;
#829 = FACE_OUTER_BOUND ( 'NONE', #191459, .T. ) ;
#831 = ORIENTED_EDGE ( 'NONE', *, *, #64309, .T. ) ;
#830 = CARTESIAN_POINT ( 'NONE',  ( 22.37643362114956247, 68.37421000605357335, -103.1221888582057460 ) ) ;
#832 = DIRECTION ( 'NONE',  ( 1.000000000000000000, -7.304098846218134667E-16, -5.100424963727256530E-30 ) ) ;
#833 = EDGE_LOOP ( 'NONE', ( #155225, #94012, #29102, #142462, #244770 ) ) ;
#834 = CARTESIAN_POINT ( 'NONE',  ( -18.40000000000000213, -9.519327731081286714, -140.9729763765593304 ) ) ;
#835 = EDGE_CURVE ( 'NONE', #115342, #123667, #138878, .T. ) ;
#836 = ORIENTED_EDGE ( 'NONE', *, *, #101044, .T. ) ;
#837 = ORIENTED_EDGE ( 'NONE', *, *, #33805, .F. ) ;
#838 = DIRECTION ( 'NONE',  ( 1.000000000000000000, 0.000000000000000000, 0.000000000000000000 ) ) ;
#839 = CIRCLE ( 'NONE', #250650, 2.000000000000001776 ) ;
#840 = FACE_OUTER_BOUND ( 'NONE', #86890, .T. ) ;
#841 = CARTESIAN_POINT ( 'NONE',  ( 23.14999999999999858, 76.00000000001169553, -67.52310748452430289 ) ) ;
#842 = ORIENTED_EDGE ( 'NONE', *, *, #95761, .F. ) ;
#843 = CIRCLE ( 'NONE', #192410, 2.000000000000003109 ) ;
#844 = AXIS2_PLACEMENT_3D ( 'NONE', #116240, #210200, #54935 ) ;
#845 = AXIS2_PLACEMENT_3D ( 'NONE', #148975, #12035, #206367 ) ;
#846 = DIRECTION ( 'NONE',  ( 0.000000000000000000, 0.000000000000000000, 1.000000000000000000 ) ) ;
#847 = TOROIDAL_SURFACE ( 'NONE', #100785, 4.099999999999999645, 0.1000000000000000056 ) ;
#848 = ORIENTED_EDGE ( 'NONE', *, *, #73889, .F. ) ;
#849 = EDGE_LOOP ( 'NONE', ( #140911, #103088, #131923, #146660 ) ) ;
#850 = CARTESIAN_POINT ( 'NONE',  ( -16.89797118371581419, 9.976380722644179855, -12.56270663244076857 ) ) ;
#851 = EDGE_LOOP ( 'NONE', ( #102145, #160499, #222247 ) ) ;
#852 = CARTESIAN_POINT ( 'NONE',  ( 21.30000000000002558, 76.00000000001213607, -136.5231074845242745 ) ) ;
#853 = DIRECTION ( 'NONE',  ( -1.000000000000000000, 0.000000000000000000, -0.000000000000000000 ) ) ;
#854 = ORIENTED_EDGE ( 'NONE', *, *, #85923, .F. ) ;
#855 = CARTESIAN_POINT ( 'NONE',  ( 21.05000000000000071, 69.74218538953603286, -136.6208977758331287 ) ) ;
#856 = DIRECTION ( 'NONE',  ( 2.465190328815662439E-32, -0.9126074666063770380, -0.4088369013363282178 ) ) ;
#857 = CARTESIAN_POINT ( 'NONE',  ( 18.59999999999999076, 10.99842653345846699, -220.2504445088529792 ) ) ;
#858 = ORIENTED_EDGE ( 'NONE', *, *, #21750, .T. ) ;
#859 = AXIS2_PLACEMENT_3D ( 'NONE', #123694, #27188, #143234 ) ;
#860 = CARTESIAN_POINT ( 'NONE',  ( -21.05000000000000071, 74.14897176987119565, -124.8691942151018139 ) ) ;
#861 = DIRECTION ( 'NONE',  ( 0.000000000000000000, 0.3738317757009942399, -0.9274965247785252886 ) ) ;
#862 = AXIS2_PLACEMENT_3D ( 'NONE', #221308, #2266, #162654 ) ;
#863 = CARTESIAN_POINT ( 'NONE',  ( 21.05000000000000071, 70.50000000001205080, -124.1178414656112352 ) ) ;
#864 = CIRCLE ( 'NONE', #179979, 6.258578643762696458 ) ;
#865 = ORIENTED_EDGE ( 'NONE', *, *, #57052, .T. ) ;
#866 = AXIS2_PLACEMENT_3D ( 'NONE', #49325, #89726, #93591 ) ;
#869 = ORIENTED_EDGE ( 'NONE', *, *, #89409, .F. ) ;
#868 = EDGE_CURVE ( 'NONE', #145080, #106770, #13915, .T. ) ;
#867 = CARTESIAN_POINT ( 'NONE',  ( -18.50000000000000000, 16.56538529403860238, -240.6448716151659823 ) ) ;
#870 = FACE_OUTER_BOUND ( 'NONE', #12758, .T. ) ;
#871 = AXIS2_PLACEMENT_3D ( 'NONE', #98806, #217487, #221333 ) ;
#872 = CARTESIAN_POINT ( 'NONE',  ( 23.15000000000000213, -12.41227409413852811, -97.50000000000004263 ) ) ;
#873 = CARTESIAN_POINT ( 'NONE',  ( -18.59999999999999787, 7.021664781900089913, -37.13356540189729316 ) ) ;
#874 = DIRECTION ( 'NONE',  ( 0.000000000000000000, -1.000000000000000000, 0.000000000000000000 ) ) ;
#875 = CARTESIAN_POINT ( 'NONE',  ( -16.88219499860498374, 66.04979357458446998, -123.8737977944170581 ) ) ;
#876 = EDGE_LOOP ( 'NONE', ( #135196, #248914, #189669, #154039 ) ) ;
#877 = FACE_OUTER_BOUND ( 'NONE', #241147, .T. ) ;
#878 = DIRECTION ( 'NONE',  ( 0.000000000000000000, 0.000000000000000000, -1.000000000000000000 ) ) ;
#879 = CARTESIAN_POINT ( 'NONE',  ( -18.59999999999999787, 77.44184265367995579, -241.6694879557322508 ) ) ;
#880 = FACE_OUTER_BOUND ( 'NONE', #179454, .T. ) ;
#881 = EDGE_CURVE ( 'NONE', #38302, #220817, #47206, .T. ) ;
#882 = AXIS2_PLACEMENT_3D ( 'NONE', #20233, #158478, #21524 ) ;
#883 = AXIS2_PLACEMENT_3D ( 'NONE', #48065, #246277, #168062 ) ;
#884 = CARTESIAN_POINT ( 'NONE',  ( 20.22516295850462598, 66.10063570456274817, -61.61304177243275149 ) ) ;
#885 = AXIS2_PLACEMENT_3D ( 'NONE', #13789, #95876, #252376 ) ;
#886 = CIRCLE ( 'NONE', #254924, 0.09999999999998898659 ) ;
#887 = ORIENTED_EDGE ( 'NONE', *, *, #95778, .T. ) ;
#888 = ORIENTED_EDGE ( 'NONE', *, *, #177250, .T. ) ;
#889 = FACE_OUTER_BOUND ( 'NONE', #237114, .T. ) ;
#890 = DIRECTION ( 'NONE',  ( -1.476360405086644309E-16, -1.000000000000000000, -0.000000000000000000 ) ) ;
#891 = DIRECTION ( 'NONE',  ( 0.000000000000000000, -1.000000000000000000, -6.860497997771532351E-15 ) ) ;
#892 = ORIENTED_EDGE ( 'NONE', *, *, #60521, .F. ) ;
#893 = LINE ( 'NONE', #202972, #43304 ) ;
#894 = FACE_OUTER_BOUND ( 'NONE', #91992, .T. ) ;
#895 = CARTESIAN_POINT ( 'NONE',  ( 18.54999999999999716, 9.950000000011153034, -46.14999999999994884 ) ) ;
#896 = CARTESIAN_POINT ( 'NONE',  ( 23.24999999999999289, 57.93055674131822741, -245.5071546967800771 ) ) ;
#897 = AXIS2_PLACEMENT_3D ( 'NONE', #252922, #212543, #254198 ) ;
#898 = ORIENTED_EDGE ( 'NONE', *, *, #17139, .F. ) ;
#899 = CARTESIAN_POINT ( 'NONE',  ( -23.49999999999994316, 74.83745509109094485, -44.02310748452479316 ) ) ;
#900 = ORIENTED_EDGE ( 'NONE', *, *, #233229, .T. ) ;
#901 = DIRECTION ( 'NONE',  ( 1.000000000000000000, -2.952720810173289112E-16, -2.061873921506763405E-30 ) ) ;
#902 = FACE_OUTER_BOUND ( 'NONE', #56191, .T. ) ;
#903 = CARTESIAN_POINT ( 'NONE',  ( 20.94999999999999929, 1.115600667400684642E-11, -134.0000000000000284 ) ) ;
#904 = CARTESIAN_POINT ( 'NONE',  ( 18.54148534481893762, 65.67467670974396299, -63.95317318268842399 ) ) ;
#905 = CARTESIAN_POINT ( 'NONE',  ( -23.15000000000000213, 1.925233644870972816, -79.73024353312617052 ) ) ;
#906 = CARTESIAN_POINT ( 'NONE',  ( -20.85000000000000142, -1.835859311432481045, -212.5044391687984842 ) ) ;
#907 = LINE ( 'NONE', #247242, #149676 ) ;
#908 = CARTESIAN_POINT ( 'NONE',  ( -23.15000000000000213, 84.66355140188136374, -146.0472086025916099 ) ) ;
#909 = CARTESIAN_POINT ( 'NONE',  ( -23.15000000000000213, 4.250000000011156409, -88.25000000000005684 ) ) ;
#910 = DIRECTION ( 'NONE',  ( 0.000000000000000000, 0.000000000000000000, -1.000000000000000000 ) ) ;
#912 = EDGE_CURVE ( 'NONE', #150586, #28814, #180624, .T. ) ;
#911 = CARTESIAN_POINT ( 'NONE',  ( -23.39999999999994529, 84.00000000001119815, -37.18565239344504647 ) ) ;
#913 = LINE ( 'NONE', #177050, #202210 ) ;
#914 = B_SPLINE_CURVE_WITH_KNOTS ( 'NONE', 3,
 ( #31194, #50679, #228074, #166844 ),
 .UNSPECIFIED., .F., .F.,
 ( 4, 4 ),
 ( 0.000000000000000000, 0.0001048066582182268164 ),
 .UNSPECIFIED. ) ;
#915 = DIRECTION ( 'NONE',  ( 2.952720810173289112E-16, 1.000000000000000000, 6.467318590049456648E-15 ) ) ;
#916 = DIRECTION ( 'NONE',  ( -0.000000000000000000, 0.5474227397873200340, -0.8368562265788217491 ) ) ;
#917 = ORIENTED_EDGE ( 'NONE', *, *, #4878, .T. ) ;
#918 = DIRECTION ( 'NONE',  ( -1.000000000000000000, 7.304098846218134667E-16, 5.100424963727256530E-30 ) ) ;
#920 = EDGE_CURVE ( 'NONE', #170466, #191384, #225694, .T. ) ;
#919 = CARTESIAN_POINT ( 'NONE',  ( -23.25000000000000000, 76.00000000001172396, -71.62310748452431142 ) ) ;
#921 = CARTESIAN_POINT ( 'NONE',  ( 23.25000000000000000, -8.999999999988842703, -191.1060308773475072 ) ) ;
#922 = APPLICATION_CONTEXT ( 'automotive_design' ) ;
#923 = ORIENTED_EDGE ( 'NONE', *, *, #9294, .F. ) ;
#925 = ADVANCED_FACE ( 'NONE', ( #171064 ), #228436, .T. ) ;
#924 = CARTESIAN_POINT ( 'NONE',  ( -22.49510344025093644, 0.06712767820541534758, -55.35002989488578606 ) ) ;
#926 = CARTESIAN_POINT ( 'NONE',  ( 21.14999999999999503, 1.115600667400684642E-11, -134.0000000000000000 ) ) ;
#927 = EDGE_LOOP ( 'NONE', ( #85776, #236101, #50558, #161418 ) ) ;
#928 = CARTESIAN_POINT ( 'NONE',  ( -16.87304349924914604, 9.961745077968330975, -188.3890666750451999 ) ) ;
#929 = CARTESIAN_POINT ( 'NONE',  ( 22.59999999999999432, 31.76322370622491320, -238.8696546380523671 ) ) ;
#930 = VECTOR ( 'NONE', #157455, 1000.000000000000000 ) ;
#931 = ADVANCED_FACE ( 'NONE', ( #208858 ), #144935, .T. ) ;
#932 = VERTEX_POINT ( 'NONE', #64520 ) ;
#933 = CIRCLE ( 'NONE', #167593, 0.1000000000000028644 ) ;
#934 = ORIENTED_EDGE ( 'NONE', *, *, #121343, .F. ) ;
#935 = DIRECTION ( 'NONE',  ( -0.000000000000000000, 1.000000000000000000, 6.982962677686267499E-15 ) ) ;
#936 = VERTEX_POINT ( 'NONE', #30232 ) ;
#937 = B_SPLINE_CURVE_WITH_KNOTS ( 'NONE', 3,
 ( #16436, #256229, #95929, #254954, #76368, #56786, #112952, #37281, #77643, #73851 ),
 .UNSPECIFIED., .F., .F.,
 ( 4, 2, 2, 2, 4 ),
 ( 5.329075035707888194E-16, 9.930191194499807640E-05, 0.0001986038238894632403, 0.0003972076477784337650, 0.0007944152955563318257 ),
 .UNSPECIFIED. ) ;
#938 = EDGE_CURVE ( 'NONE', #254106, #142564, #184202, .T. ) ;
#939 = CARTESIAN_POINT ( 'NONE',  ( 21.05000000000000071, -0.08559286336224566916, 6.413662734869540749 ) ) ;
#940 = CARTESIAN_POINT ( 'NONE',  ( 21.05000000000000071, -8.999999999988842703, -57.10603087734755690 ) ) ;
#942 = CARTESIAN_POINT ( 'NONE',  ( 21.13498764882293557, 34.00176438950338564, -243.6238902785767095 ) ) ;
#941 = UNCERTAINTY_MEASURE_WITH_UNIT (LENGTH_MEASURE( 1.000000000000000082E-05 ), #199056, 'distance_accuracy_value', 'NONE');
#943 = CARTESIAN_POINT ( 'NONE',  ( 23.14999999999999503, 64.35000000001173248, -81.27310748452440237 ) ) ;
#944 = CARTESIAN_POINT ( 'NONE',  ( -20.94999999999999929, 76.25610579210490414, -203.5580039261966760 ) ) ;
#945 = CARTESIAN_POINT ( 'NONE',  ( 20.94999999999999574, 1.115600667400684642E-11, -100.5000000000000284 ) ) ;
#946 = CIRCLE ( 'NONE', #104987, 0.1999999999999987899 ) ;
#947 = DIRECTION ( 'NONE',  ( -1.000000000000000000, 6.938893903907270030E-14, 0.000000000000000000 ) ) ;
#949 = DIRECTION ( 'NONE',  ( 1.000000000000000000, 0.000000000000000000, 0.000000000000000000 ) ) ;
#948 = AXIS2_PLACEMENT_3D ( 'NONE', #31250, #130291, #251525 ) ;
#951 = ORIENTED_EDGE ( 'NONE', *, *, #5769, .F. ) ;
#950 = CARTESIAN_POINT ( 'NONE',  ( 18.44206774312969443, 86.89455662089525845, -199.6122089586171739 ) ) ;
#952 = VERTEX_POINT ( 'NONE', #168495 ) ;
#954 = DIRECTION ( 'NONE',  ( -1.000000000000000000, 0.000000000000000000, 0.000000000000000000 ) ) ;
#953 = CARTESIAN_POINT ( 'NONE',  ( 22.40000000000010516, -9.465541304798784944E-13, 11.75043289245892808 ) ) ;
#956 = ORIENTED_EDGE ( 'NONE', *, *, #204565, .T. ) ;
#955 = CARTESIAN_POINT ( 'NONE',  ( -16.84793658983402764, 60.96125253478340511, -220.9609974078819903 ) ) ;
#957 = EDGE_LOOP ( 'NONE', ( #50520, #79684, #17049, #193542 ) ) ;
#958 = CARTESIAN_POINT ( 'NONE',  ( -16.94052228080552425, 66.01372026691339556, -149.1327319818550450 ) ) ;
#959 = CARTESIAN_POINT ( 'NONE',  ( 13.40000000000000036, -11.65000000000000036, 17.70000000000000284 ) ) ;
#960 = CARTESIAN_POINT ( 'NONE',  ( -20.85000000000000142, 7.021664781900089913, -37.33356540189728889 ) ) ;
#961 = FACE_OUTER_BOUND ( 'NONE', #150516, .T. ) ;
#962 = DIRECTION ( 'NONE',  ( 1.000000000000000000, -0.000000000000000000, -0.000000000000000000 ) ) ;
#963 = DIRECTION ( 'NONE',  ( 0.000000000000000000, -1.734723475976997999E-14, 1.000000000000000000 ) ) ;
#964 = CARTESIAN_POINT ( 'NONE',  ( 18.59999999999999076, 69.45000000001252261, -182.2731074845244166 ) ) ;
#965 = EDGE_CURVE ( 'NONE', #227768, #157652, #25810, .T. ) ;
#966 = AXIS2_PLACEMENT_3D ( 'NONE', #7756, #245072, #225483 ) ;
#967 = VECTOR ( 'NONE', #117987, 1000.000000000000114 ) ;
#969 = VECTOR ( 'NONE', #242743, 1000.000000000000000 ) ;
#968 = CARTESIAN_POINT ( 'NONE',  ( -21.05000000000000071, 87.65000000001192859, -106.1231074845242262 ) ) ;
#970 = EDGE_LOOP ( 'NONE', ( #120414, #176231, #21740, #124725 ) ) ;
#971 = VERTEX_POINT ( 'NONE', #210151 ) ;
#972 = DIRECTION ( 'NONE',  ( 6.938893903907991995E-14, 0.000000000000000000, 1.000000000000000000 ) ) ;
#973 = VERTEX_POINT ( 'NONE', #10661 ) ;
#974 = LINE ( 'NONE', #144343, #138543 ) ;
#975 = VERTEX_POINT ( 'NONE', #144040 ) ;
#976 = CARTESIAN_POINT ( 'NONE',  ( -16.97683809663753962, 14.02673956256705523, -218.6477791648082700 ) ) ;
#977 = ADVANCED_FACE ( 'NONE', ( #13240 ), #152767, .T. ) ;
#978 = CARTESIAN_POINT ( 'NONE',  ( -15.69373346032659100, 48.53477651487867206, -233.9781183031096816 ) ) ;
#979 = CARTESIAN_POINT ( 'NONE',  ( -20.54999999999999716, 50.16665896658852120, -238.7333021241242079 ) ) ;
#980 = CARTESIAN_POINT ( 'NONE',  ( 18.52928932188133970, 65.72071067813013201, -44.87310748452439668 ) ) ;
#981 = CARTESIAN_POINT ( 'NONE',  ( 20.94999999999999929, 1.115600667400684642E-11, -100.5000000000000426 ) ) ;
#982 = ORIENTED_EDGE ( 'NONE', *, *, #230832, .F. ) ;
#984 = ADVANCED_FACE ( 'NONE', ( #247971 ), #13226, .T. ) ;
#983 = CARTESIAN_POINT ( 'NONE',  ( -23.25000000000000000, 2.000000000011154189, -87.87537807723795424 ) ) ;
#985 = ORIENTED_EDGE ( 'NONE', *, *, #144619, .F. ) ;
#986 = CARTESIAN_POINT ( 'NONE',  ( 21.05000000000000071, 0.09779029131994770863, -27.24218538952387547 ) ) ;
#987 = SPHERICAL_SURFACE ( 'NONE', #235532, 0.1000000000000000056 ) ;
#988 = CARTESIAN_POINT ( 'NONE',  ( -1.739115166359751170E-14, 11.65000000001114699, -146.2500000000000284 ) ) ;
#989 = CARTESIAN_POINT ( 'NONE',  ( -20.65000000000000568, 68.75000000001153921, -48.67310748452437252 ) ) ;
#990 = EDGE_CURVE ( 'NONE', #220874, #195448, #229707, .T. ) ;
#991 = VERTEX_POINT ( 'NONE', #173638 ) ;
#992 = CIRCLE ( 'NONE', #105215, 12.97499999999999964 ) ;
#993 = CARTESIAN_POINT ( 'NONE',  ( -18.52309608778508476, 85.64247632006660638, -29.30851114335468921 ) ) ;
#994 = VERTEX_POINT ( 'NONE', #31540 ) ;
#997 = VERTEX_POINT ( 'NONE', #190596 ) ;
#996 = DIRECTION ( 'NONE',  ( -1.000000000000000000, 2.952720810173289112E-16, 2.061873921506763405E-30 ) ) ;
#995 = CARTESIAN_POINT ( 'NONE',  ( -22.59999999999999787, 64.25043287652329127, -203.6239658536231616 ) ) ;
#998 = VECTOR ( 'NONE', #226913, 1000.000000000000000 ) ;
#999 = CARTESIAN_POINT ( 'NONE',  ( -20.94999999999999929, 1.115600667400684642E-11, -100.5000000000000426 ) ) ;
#1000 = CARTESIAN_POINT ( 'NONE',  ( -23.15000000000000213, 1.115651490242849210E-11, -96.35000000000003695 ) ) ;
#1001 = ORIENTED_EDGE ( 'NONE', *, *, #105577, .T. ) ;
#1002 = CARTESIAN_POINT ( 'NONE',  ( -20.85000000000000142, 7.120270961708750512, -137.6595630418393625 ) ) ;
#1003 = AXIS2_PLACEMENT_3D ( 'NONE', #134817, #155729, #193549 ) ;
#1005 = EDGE_CURVE ( 'NONE', #205753, #123238, #843, .T. ) ;
#1004 = CARTESIAN_POINT ( 'NONE',  ( 21.05000000000000071, 1.115650877919449575E-11, -196.8999999999999773 ) ) ;
#1006 = DIRECTION ( 'NONE',  ( 1.000000000000000000, 0.000000000000000000, 0.000000000000000000 ) ) ;
#1007 = ORIENTED_EDGE ( 'NONE', *, *, #156845, .F. ) ;
#1008 = AXIS2_PLACEMENT_3D ( 'NONE', #183384, #165097, #242056 ) ;
#1009 = EDGE_CURVE ( 'NONE', #228001, #178016, #16977, .T. ) ;
#1010 = EDGE_CURVE ( 'NONE', #27613, #234902, #105062, .T. ) ;
#1011 = CYLINDRICAL_SURFACE ( 'NONE', #164253, 0.1000000000000001443 ) ;
#1012 = AXIS2_PLACEMENT_3D ( 'NONE', #50416, #71315, #248640 ) ;
#1013 = ORIENTED_EDGE ( 'NONE', *, *, #141561, .F. ) ;
#1014 = VECTOR ( 'NONE', #215002, 1000.000000000000000 ) ;
#1015 = CIRCLE ( 'NONE', #130218, 0.09999999999999907574 ) ;
#1016 = FACE_OUTER_BOUND ( 'NONE', #23267, .T. ) ;
#1017 = CARTESIAN_POINT ( 'NONE',  ( 21.07016717456946608, 61.13071397353302672, -234.2006012892922797 ) ) ;
#1018 = CARTESIAN_POINT ( 'NONE',  ( -18.40000000000000213, 67.17743825834537574, -78.77310748452437394 ) ) ;
#1019 = ORIENTED_EDGE ( 'NONE', *, *, #12800, .T. ) ;
#1020 = DIRECTION ( 'NONE',  ( 0.000000000000000000, 0.000000000000000000, -1.000000000000000000 ) ) ;
#1022 = ORIENTED_EDGE ( 'NONE', *, *, #256802, .T. ) ;
#1021 = AXIS2_PLACEMENT_3D ( 'NONE', #24358, #201685, #107719 ) ;
#1023 = DIRECTION ( 'NONE',  ( 0.000000000000000000, 0.000000000000000000, 1.000000000000000000 ) ) ;
#1024 = AXIS2_PLACEMENT_3D ( 'NONE', #181277, #82122, #221642 ) ;
#1025 = EDGE_CURVE ( 'NONE', #149860, #28751, #199594, .T. ) ;
#1026 = DIRECTION ( 'NONE',  ( -1.000000000000000000, -9.012599976027990443E-15, -6.882867235861669241E-14 ) ) ;
#1027 = DIRECTION ( 'NONE',  ( 0.000000000000000000, 0.9654727137038715545, 0.2605042016806676242 ) ) ;
#1028 = VERTEX_POINT ( 'NONE', #117468 ) ;
#1029 = EDGE_CURVE ( 'NONE', #88325, #70494, #117580, .T. ) ;
#1030 = CARTESIAN_POINT ( 'NONE',  ( 21.10642757222115407, 22.98234816118409185, -230.0602600960314419 ) ) ;
#1031 = EDGE_CURVE ( 'NONE', #108484, #237026, #66, .T. ) ;
#1032 = VECTOR ( 'NONE', #248459, 999.9999999999998863 ) ;
#1033 = CARTESIAN_POINT ( 'NONE',  ( 21.05000000000000071, 1.115600667400684642E-11, -200.9999999999999432 ) ) ;
#1034 = TOROIDAL_SURFACE ( 'NONE', #80138, 7.800000000000000711, 0.1000000000000000056 ) ;
#1035 = CARTESIAN_POINT ( 'NONE',  ( -20.54999999999999716, 76.00000000001244871, -170.0231074845243597 ) ) ;
#1036 = ORIENTED_EDGE ( 'NONE', *, *, #252988, .T. ) ;
#1037 = TOROIDAL_SURFACE ( 'NONE', #71828, 0.2000000000000000111, 0.1000000000000000056 ) ;
#1038 = VECTOR ( 'NONE', #250333, 1000.000000000000000 ) ;
#1039 = CARTESIAN_POINT ( 'NONE',  ( -20.85000000000000142, 77.25000000001239187, -162.2226267301092548 ) ) ;
#1040 = LINE ( 'NONE', #115896, #206521 ) ;
#1041 = ORIENTED_EDGE ( 'NONE', *, *, #205494, .F. ) ;
#1042 = CARTESIAN_POINT ( 'NONE',  ( 19.99999999999998934, 64.25000000001151079, -48.17310748452440805 ) ) ;
#1043 = ORIENTED_EDGE ( 'NONE', *, *, #128497, .F. ) ;
#1044 = ORIENTED_EDGE ( 'NONE', *, *, #191598, .F. ) ;
#1045 = TOROIDAL_SURFACE ( 'NONE', #30150, 11.65000000000000036, 0.1000000000000000056 ) ;
#1046 = DIRECTION ( 'NONE',  ( -1.000000000000000000, 2.952720810173289112E-16, 2.061873921506763405E-30 ) ) ;
#1047 = ORIENTED_EDGE ( 'NONE', *, *, #175147, .T. ) ;
#1049 = ORIENTED_EDGE ( 'NONE', *, *, #19953, .F. ) ;
#1048 = FACE_OUTER_BOUND ( 'NONE', #196732, .T. ) ;
#1050 = ADVANCED_FACE ( 'NONE', ( #118760 ), #42562, .F. ) ;
#1051 = ADVANCED_FACE ( 'NONE', ( #15824 ), #217817, .T. ) ;
#1052 = CIRCLE ( 'NONE', #79612, 0.09999999999999935330 ) ;
#1055 = ORIENTED_EDGE ( 'NONE', *, *, #23889, .F. ) ;
#1054 = ORIENTED_EDGE ( 'NONE', *, *, #171013, .T. ) ;
#1053 = CARTESIAN_POINT ( 'NONE',  ( -16.94107738177414291, 14.24304960796391306, -219.3391119284832484 ) ) ;
#1056 = B_SPLINE_CURVE_WITH_KNOTS ( 'NONE', 3,
 ( #24582, #242312, #4960, #182362, #88352, #44128 ),
 .UNSPECIFIED., .F., .F.,
 ( 4, 2, 4 ),
 ( 0.000000000000000000, 0.0002113392456166024729, 0.0004226784912332049457 ),
 .UNSPECIFIED. ) ;
#1057 = CARTESIAN_POINT ( 'NONE',  ( 21.05000000000000071, 65.52661458509899717, -95.44445302027585853 ) ) ;
#1058 = PLANE ( 'NONE',  #110612 ) ;
#1060 = EDGE_CURVE ( 'NONE', #31696, #10002, #250840, .T. ) ;
#1059 = CARTESIAN_POINT ( 'NONE',  ( -21.65000000000000213, 68.29142135624935861, -124.2731074845243597 ) ) ;
#1061 = LINE ( 'NONE', #25789, #119140 ) ;
#1062 = CARTESIAN_POINT ( 'NONE',  ( 23.14999999999998437, 0.8618440306782493288, -204.9572370243411115 ) ) ;
#1063 = AXIS2_PLACEMENT_3D ( 'NONE', #82994, #24366, #21792 ) ;
#1064 = CARTESIAN_POINT ( 'NONE',  ( -23.49999999999994316, 83.80000000001119531, -34.86056257560453986 ) ) ;
#1065 = AXIS2_PLACEMENT_3D ( 'NONE', #149817, #229347, #50668 ) ;
#1066 = DIRECTION ( 'NONE',  ( -1.000000000000000000, -0.000000000000000000, -0.000000000000000000 ) ) ;
#1069 = DIRECTION ( 'NONE',  ( 1.000000000000000000, 0.000000000000000000, 0.000000000000000000 ) ) ;
#1068 = CARTESIAN_POINT ( 'NONE',  ( 18.59999999999999076, 68.92903212821357783, -166.2765432626560766 ) ) ;
#1067 = VECTOR ( 'NONE', #103802, 1000.000000000000000 ) ;
#1070 = ORIENTED_EDGE ( 'NONE', *, *, #6774, .F. ) ;
#1071 = ORIENTED_EDGE ( 'NONE', *, *, #163341, .T. ) ;
#1072 = CARTESIAN_POINT ( 'NONE',  ( 18.79999999999999716, 6.841561409100513025, 9.675512259591560138 ) ) ;
#1074 = VERTEX_POINT ( 'NONE', #134427 ) ;
#1073 = CARTESIAN_POINT ( 'NONE',  ( -23.15000000000000213, 1.115600667400684642E-11, -65.00000000000000000 ) ) ;
#1075 = CARTESIAN_POINT ( 'NONE',  ( 22.39999999999999503, 0.1000000000111554016, -126.2092204016266379 ) ) ;
#1076 = ORIENTED_EDGE ( 'NONE', *, *, #254807, .T. ) ;
#1077 = DIRECTION ( 'NONE',  ( -0.000000000000000000, -0.1350103645451876666, 0.9908441862701600211 ) ) ;
#1078 = EDGE_LOOP ( 'NONE', ( #153899, #117454, #241349, #25597 ) ) ;
#1079 = CARTESIAN_POINT ( 'NONE',  ( 23.14999999999999503, 11.65000000001116298, -179.7499999999999716 ) ) ;
#1080 = ADVANCED_FACE ( 'NONE', ( #36672 ), #154068, .F. ) ;
#1081 = ORIENTED_EDGE ( 'NONE', *, *, #230083, .T. ) ;
#1082 = CARTESIAN_POINT ( 'NONE',  ( -16.92563707711778775, 66.03100930561501514, -82.14234918500042681 ) ) ;
#1084 = EDGE_CURVE ( 'NONE', #166202, #45065, #38658, .T. ) ;
#1083 = CYLINDRICAL_SURFACE ( 'NONE', #136111, 0.09999999999999438505 ) ;
#1085 = AXIS2_PLACEMENT_3D ( 'NONE', #149356, #48937, #73678 ) ;
#1087 = EDGE_LOOP ( 'NONE', ( #140736, #240001, #225855, #36280 ) ) ;
#1086 = ORIENTED_EDGE ( 'NONE', *, *, #86462, .F. ) ;
#1088 = ORIENTED_EDGE ( 'NONE', *, *, #35954, .T. ) ;
#1089 = CARTESIAN_POINT ( 'NONE',  ( -20.54999999999999716, 1.115625160336667635E-11, -136.0000000000000284 ) ) ;
#1090 = ORIENTED_EDGE ( 'NONE', *, *, #72256, .T. ) ;
#1091 = VERTEX_POINT ( 'NONE', #138280 ) ;
#1092 = CARTESIAN_POINT ( 'NONE',  ( 20.94999999999999929, -8.730841121484166578, -90.90192528101570701 ) ) ;
#1093 = CIRCLE ( 'NONE', #167741, 0.1000000000000028644 ) ;
#1096 = EDGE_CURVE ( 'NONE', #181952, #210604, #195739, .T. ) ;
#1095 = VERTEX_POINT ( 'NONE', #78315 ) ;
#1094 = FACE_OUTER_BOUND ( 'NONE', #108621, .T. ) ;
#1098 = CARTESIAN_POINT ( 'NONE',  ( 23.14999999999999858, 5.500000000011153745, -146.4052660189131245 ) ) ;
#1097 = DIRECTION ( 'NONE',  ( -1.000000000000000000, 0.000000000000000000, -0.000000000000000000 ) ) ;
#1099 = DIRECTION ( 'NONE',  ( 0.000000000000000000, 0.000000000000000000, -1.000000000000000000 ) ) ;
#1100 = FACE_OUTER_BOUND ( 'NONE', #4489, .T. ) ;
#1101 = DIRECTION ( 'NONE',  ( 0.000000000000000000, -0.9910827722268055195, 0.1332476588733540468 ) ) ;
#1102 = EDGE_LOOP ( 'NONE', ( #9288, #170503 ) ) ;
#1103 = EDGE_CURVE ( 'NONE', #196419, #152244, #238187, .T. ) ;
#1104 = VERTEX_POINT ( 'NONE', #27388 ) ;
#1105 = FACE_OUTER_BOUND ( 'NONE', #33158, .T. ) ;
#1106 = CARTESIAN_POINT ( 'NONE',  ( 20.94999999999999929, -9.399999999988844834, -57.10603087734755690 ) ) ;
#1107 = DIRECTION ( 'NONE',  ( -0.000000000000000000, 0.000000000000000000, 1.000000000000000000 ) ) ;
#1108 = EDGE_CURVE ( 'NONE', #224475, #57327, #209152, .T. ) ;
#1109 = ORIENTED_EDGE ( 'NONE', *, *, #21363, .F. ) ;
#1110 = FACE_OUTER_BOUND ( 'NONE', #233161, .T. ) ;
#1111 = EDGE_CURVE ( 'NONE', #101652, #9861, #66472, .T. ) ;
#1112 = CIRCLE ( 'NONE', #151177, 0.2000000000000057288 ) ;
#1113 = CARTESIAN_POINT ( 'NONE',  ( -23.25000000000000000, 61.54970422893871529, -212.2965875311496688 ) ) ;
#1114 = CARTESIAN_POINT ( 'NONE',  ( -15.52965525596988527, 12.53792204840291369, -214.5112614470118615 ) ) ;
#1116 = ADVANCED_FACE ( 'NONE', ( #84706 ), #204865, .T. ) ;
#1115 = ADVANCED_FACE ( 'NONE', ( #182586 ), #85999, .T. ) ;
#1117 = ORIENTED_EDGE ( 'NONE', *, *, #211260, .F. ) ;
#1118 = ORIENTED_EDGE ( 'NONE', *, *, #258057, .F. ) ;
#1119 = DIRECTION ( 'NONE',  ( 1.000000000000000000, -0.000000000000000000, -0.000000000000000000 ) ) ;
#1120 = DIRECTION ( 'NONE',  ( 0.000000000000000000, 1.000000000000000000, 6.982962677686266711E-15 ) ) ;
#1121 = EDGE_LOOP ( 'NONE', ( #113054, #182674, #33801, #198627 ) ) ;
#1122 = SPHERICAL_SURFACE ( 'NONE', #193152, 0.1000000000000000056 ) ;
#1123 = ORIENTED_EDGE ( 'NONE', *, *, #146803, .T. ) ;
#1124 = CARTESIAN_POINT ( 'NONE',  ( 21.05000000000000071, 72.06688615501691686, -225.0895073929160048 ) ) ;
#1125 = DIRECTION ( 'NONE',  ( 0.000000000000000000, 6.982962677686266711E-15, -1.000000000000000000 ) ) ;
#1127 = CARTESIAN_POINT ( 'NONE',  ( -20.94999999999999929, 76.00000000001237765, -170.0231074845243597 ) ) ;
#1126 = CARTESIAN_POINT ( 'NONE',  ( -22.39999999999999858, 10.80758397488570743, -226.8651660546161111 ) ) ;
#1128 = CARTESIAN_POINT ( 'NONE',  ( -18.39999999999999858, 85.60000000001241460, -163.4229180933022576 ) ) ;
#1129 = FACE_OUTER_BOUND ( 'NONE', #213578, .T. ) ;
#1130 = VERTEX_POINT ( 'NONE', #101710 ) ;
#1131 = AXIS2_PLACEMENT_3D ( 'NONE', #155849, #153298, #136228 ) ;
#1132 = CARTESIAN_POINT ( 'NONE',  ( -23.15000000000000213, 61.88149656937975607, -248.1136133839584090 ) ) ;
#1133 = EDGE_CURVE ( 'NONE', #226006, #125569, #21733, .T. ) ;
#1134 = EDGE_CURVE ( 'NONE', #176594, #123224, #5180, .T. ) ;
#1135 = CIRCLE ( 'NONE', #230280, 0.1000000000000028644 ) ;
#1137 = ORIENTED_EDGE ( 'NONE', *, *, #13931, .T. ) ;
#1136 = EDGE_LOOP ( 'NONE', ( #176857, #128273, #32056, #181394 ) ) ;
#1138 = ORIENTED_EDGE ( 'NONE', *, *, #55559, .F. ) ;
#1139 = VERTEX_POINT ( 'NONE', #3933 ) ;
#1140 = AXIS2_PLACEMENT_3D ( 'NONE', #231171, #127229, #167657 ) ;
#1141 = EDGE_CURVE ( 'NONE', #118769, #81824, #59092, .T. ) ;
#1142 = CARTESIAN_POINT ( 'NONE',  ( -16.94445028196808778, 66.00793639031455484, -157.4157773061059800 ) ) ;
#1143 = CARTESIAN_POINT ( 'NONE',  ( -22.57848426163147693, 76.00426432929484122, -81.27316579141465525 ) ) ;
#1144 = LINE ( 'NONE', #173765, #92456 ) ;
#1145 = DIRECTION ( 'NONE',  ( -1.000000000000000000, -3.265361837132813093E-16, 0.000000000000000000 ) ) ;
#1146 = FACE_OUTER_BOUND ( 'NONE', #164575, .T. ) ;
#1148 = DIRECTION ( 'NONE',  ( 0.000000000000000000, -0.1335171055202864221, 0.9910465087640865089 ) ) ;
#1147 = CARTESIAN_POINT ( 'NONE',  ( 20.96937028524355640, 10.62446937162667737, -7.491426101169610163 ) ) ;
#1149 = EDGE_CURVE ( 'NONE', #115956, #185096, #224248, .T. ) ;
#1150 = ORIENTED_EDGE ( 'NONE', *, *, #62827, .T. ) ;
#1151 = CARTESIAN_POINT ( 'NONE',  ( -16.83199318825828072, 66.06935387203033372, -48.79552229631519111 ) ) ;
#1152 = EDGE_LOOP ( 'NONE', ( #213535, #112196, #56971, #205951 ) ) ;
#1153 = CARTESIAN_POINT ( 'NONE',  ( -23.24999999999999645, 85.60000000001137721, -29.32291809330221355 ) ) ;
#1154 = ADVANCED_FACE ( 'NONE', ( #82149 ), #61338, .F. ) ;
#1155 = VERTEX_POINT ( 'NONE', #161747 ) ;
#1156 = ORIENTED_EDGE ( 'NONE', *, *, #29802, .T. ) ;
#1157 = CARTESIAN_POINT ( 'NONE',  ( 23.14999999999999858, 0.000000000000000000, -33.50000000000000000 ) ) ;
#1159 = CIRCLE ( 'NONE', #221721, 0.09999999999998898659 ) ;
#1158 = LINE ( 'NONE', #121168, #231032 ) ;
#1160 = CARTESIAN_POINT ( 'NONE',  ( 20.94999999999999929, 0.000000000000000000, -12.87500000000000000 ) ) ;
#1161 = AXIS2_PLACEMENT_3D ( 'NONE', #77695, #114274, #157280 ) ;
#1162 = DIRECTION ( 'NONE',  ( 0.000000000000000000, 0.2128009952264768301, -0.9770955615653060811 ) ) ;
#1163 = DIRECTION ( 'NONE',  ( 1.000000000000000000, 0.000000000000000000, 0.000000000000000000 ) ) ;
#1164 = ORIENTED_EDGE ( 'NONE', *, *, #177190, .F. ) ;
#1165 = ORIENTED_EDGE ( 'NONE', *, *, #245877, .T. ) ;
#1166 = AXIS2_PLACEMENT_3D ( 'NONE', #61305, #43035, #117434 ) ;
#1167 = DIRECTION ( 'NONE',  ( -0.000000000000000000, 0.000000000000000000, 1.000000000000000000 ) ) ;
#1169 = EDGE_CURVE ( 'NONE', #149634, #78058, #175861, .T. ) ;
#1168 = ORIENTED_EDGE ( 'NONE', *, *, #66721, .F. ) ;
#1170 = FACE_OUTER_BOUND ( 'NONE', #239611, .T. ) ;
#1171 = DIRECTION ( 'NONE',  ( 0.000000000000000000, 0.000000000000000000, -1.000000000000000000 ) ) ;
#1172 = ADVANCED_FACE ( 'NONE', ( #241277 ), #63904, .F. ) ;
#1173 = DIRECTION ( 'NONE',  ( 1.000000000000000000, 0.000000000000000000, 0.000000000000000000 ) ) ;
#1174 = CARTESIAN_POINT ( 'NONE',  ( -22.47071067811865319, 75.90090754530959316, -144.2431822290223522 ) ) ;
#1175 = CARTESIAN_POINT ( 'NONE',  ( -23.25000000000000000, -11.75000000000000000, 3.469446951953614189E-15 ) ) ;
#1176 = DIRECTION ( 'NONE',  ( -3.265361837132813093E-16, 1.000000000000000000, 0.000000000000000000 ) ) ;
#1177 = CIRCLE ( 'NONE', #121826, 0.6000000000000081934 ) ;
#1180 = DIRECTION ( 'NONE',  ( 0.000000000000000000, 0.000000000000000000, 1.000000000000000000 ) ) ;
#1179 = AXIS2_PLACEMENT_3D ( 'NONE', #169114, #67404, #208218 ) ;
#1178 = CARTESIAN_POINT ( 'NONE',  ( -16.94333152882355975, 30.26242836586778040, -234.7913307026829841 ) ) ;
#1182 = DIRECTION ( 'NONE',  ( -1.000000000000000000, -0.000000000000000000, -0.000000000000000000 ) ) ;
#1181 = VECTOR ( 'NONE', #107103, 1000.000000000000000 ) ;
#1183 = AXIS2_PLACEMENT_3D ( 'NONE', #208111, #209369, #67292 ) ;
#1185 = EDGE_CURVE ( 'NONE', #42318, #28415, #156424, .T. ) ;
#1184 = CARTESIAN_POINT ( 'NONE',  ( -21.05000000000000071, 6.350981563072554792, -199.7191680003453769 ) ) ;
#1186 = CARTESIAN_POINT ( 'NONE',  ( -23.15000000000000213, 0.000000000000000000, 0.000000000000000000 ) ) ;
#1187 = ORIENTED_EDGE ( 'NONE', *, *, #165921, .F. ) ;
#1189 = ADVANCED_FACE ( 'NONE', ( #122614 ), #9245, .F. ) ;
#1188 = CARTESIAN_POINT ( 'NONE',  ( -16.87665923198281348, 30.20632856012693424, -234.8070450048000737 ) ) ;
#1190 = ORIENTED_EDGE ( 'NONE', *, *, #142213, .T. ) ;
#1191 = CARTESIAN_POINT ( 'NONE',  ( -18.59999999999999787, 7.250000000011155521, -155.3500000000000227 ) ) ;
#1192 = CARTESIAN_POINT ( 'NONE',  ( 13.40000000000005898, 67.72071067812984779, -17.05239680640613997 ) ) ;
#1193 = ORIENTED_EDGE ( 'NONE', *, *, #64693, .T. ) ;
#1194 = DIRECTION ( 'NONE',  ( 0.000000000000000000, 0.000000000000000000, 1.000000000000000000 ) ) ;
#1195 = LINE ( 'NONE', #182443, #193762 ) ;
#1197 = AXIS2_PLACEMENT_3D ( 'NONE', #36958, #101994, #116467 ) ;
#1196 = CARTESIAN_POINT ( 'NONE',  ( -18.50000000000000000, 51.33926024308902925, -230.0993571250899379 ) ) ;
#1198 = ADVANCED_FACE ( 'NONE', ( #80877 ), #126440, .F. ) ;
#1199 = CARTESIAN_POINT ( 'NONE',  ( -20.94999999999994600, 65.25000000001119815, -51.02310748452479316 ) ) ;
#1200 = CARTESIAN_POINT ( 'NONE',  ( -20.85000000000000142, 6.846123162363745074, -171.2377262668498759 ) ) ;
#1201 = FACE_OUTER_BOUND ( 'NONE', #201757, .T. ) ;
#1202 = ORIENTED_EDGE ( 'NONE', *, *, #70596, .F. ) ;
#1203 = LINE ( 'NONE', #44221, #137456 ) ;
#1205 = ORIENTED_EDGE ( 'NONE', *, *, #153700, .T. ) ;
#1204 = DIRECTION ( 'NONE',  ( 0.000000000000000000, 0.4999999999999689138, 0.8660254037844565822 ) ) ;
#1206 = VECTOR ( 'NONE', #217210, 1000.000000000000000 ) ;
#1207 = DIRECTION ( 'NONE',  ( 1.000000000000000000, 0.000000000000000000, 0.000000000000000000 ) ) ;
#1208 = CIRCLE ( 'NONE', #117918, 0.1999999999999987899 ) ;
#1209 = LINE ( 'NONE', #44225, #82841 ) ;
#1210 = CARTESIAN_POINT ( 'NONE',  ( 20.99999999999997868, 76.00000000001237765, -170.0231074845243597 ) ) ;
#1211 = ORIENTED_EDGE ( 'NONE', *, *, #25154, .T. ) ;
#1212 = CARTESIAN_POINT ( 'NONE',  ( -22.49510344025093644, 75.93287232181796753, -148.1730775896385808 ) ) ;
#1213 = AXIS2_PLACEMENT_3D ( 'NONE', #17555, #99643, #159659 ) ;
#1214 = APPLICATION_PROTOCOL_DEFINITION ( 'draft international standard', 'automotive_design', 1998, #139160 ) ;
#1216 = CIRCLE ( 'NONE', #126111, 0.09999999999999939493 ) ;
#1215 = FACE_OUTER_BOUND ( 'NONE', #255672, .T. ) ;
#1217 = EDGE_LOOP ( 'NONE', ( #94303, #5481, #138383, #26896, #232197 ) ) ;
#1218 = AXIS2_PLACEMENT_3D ( 'NONE', #140597, #156355, #178481 ) ;
#1219 = DIRECTION ( 'NONE',  ( 1.000000000000000000, -0.000000000000000000, -0.000000000000000000 ) ) ;
#1220 = FACE_OUTER_BOUND ( 'NONE', #156586, .T. ) ;
#1221 = AXIS2_PLACEMENT_3D ( 'NONE', #83190, #118526, #58505 ) ;
#1222 = VECTOR ( 'NONE', #70005, 1000.000000000000000 ) ;
#1223 = CARTESIAN_POINT ( 'NONE',  ( -18.59999999999999787, 64.25000000001190870, -96.00830171387039513 ) ) ;
#1224 = VERTEX_POINT ( 'NONE', #31242 ) ;
#1225 = ORIENTED_EDGE ( 'NONE', *, *, #153604, .F. ) ;
#1226 = CARTESIAN_POINT ( 'NONE',  ( -23.25000000000000000, 76.00000000001244871, -170.0231074845243597 ) ) ;
#1228 = AXIS2_PLACEMENT_3D ( 'NONE', #234016, #55344, #254814 ) ;
#1227 = CARTESIAN_POINT ( 'NONE',  ( -23.25000000000000000, -1.835859311432481045, -212.5044391687984842 ) ) ;
#1230 = CIRCLE ( 'NONE', #21927, 11.80000000000000426 ) ;
#1229 = FACE_OUTER_BOUND ( 'NONE', #124610, .T. ) ;
#1231 = CYLINDRICAL_SURFACE ( 'NONE', #44591, 0.09999999999998898659 ) ;
#1232 = CARTESIAN_POINT ( 'NONE',  ( 21.05000000000000071, 85.50000000001251976, -179.9170766071767389 ) ) ;
#1233 = ADVANCED_FACE ( 'NONE', ( #109429 ), #132875, .F. ) ;
#1234 = CARTESIAN_POINT ( 'NONE',  ( -18.59999999999999787, -11.75000000000000000, 29.89999999999999858 ) ) ;
#1236 = CARTESIAN_POINT ( 'NONE',  ( -18.59999999999999787, 11.75000000000000000, 30.09999999999999787 ) ) ;
#1235 = CARTESIAN_POINT ( 'NONE',  ( 20.95035502843362707, 65.52236167323542304, -95.44680777578801667 ) ) ;
#1237 = CIRCLE ( 'NONE', #88726, 0.5000000000000004441 ) ;
#1238 = CARTESIAN_POINT ( 'NONE',  ( -20.94999999999999929, 76.00000000001195133, -103.0231074845243171 ) ) ;
#1239 = FACE_OUTER_BOUND ( 'NONE', #129427, .T. ) ;
#1240 = DIRECTION ( 'NONE',  ( 1.000000000000000000, 0.000000000000000000, 0.000000000000000000 ) ) ;
#1241 = CARTESIAN_POINT ( 'NONE',  ( -16.88495309932523369, 9.954627058484017965, -146.6345486738119348 ) ) ;
#1242 = ORIENTED_EDGE ( 'NONE', *, *, #189634, .F. ) ;
#1243 = ORIENTED_EDGE ( 'NONE', *, *, #90316, .T. ) ;
#1244 = AXIS2_PLACEMENT_3D ( 'NONE', #170789, #254105, #134165 ) ;
#1245 = CARTESIAN_POINT ( 'NONE',  ( -18.41431012584568805, 64.51252797080402956, -145.7498714714227788 ) ) ;
#1247 = CARTESIAN_POINT ( 'NONE',  ( 21.05000000000000071, 67.22371710472012296, -191.3731074845244109 ) ) ;
#1246 = CARTESIAN_POINT ( 'NONE',  ( -21.05000000000000071, 69.58624026620167058, -102.9374944237203948 ) ) ;
#1248 = AXIS2_PLACEMENT_3D ( 'NONE', #185662, #63124, #162264 ) ;
#1249 = VECTOR ( 'NONE', #185443, 1000.000000000000000 ) ;
#1250 = CIRCLE ( 'NONE', #209554, 0.2000000000000057288 ) ;
#1251 = DIRECTION ( 'NONE',  ( -0.7071067811864931718, -0.2890913453341744099, 0.6453109281989217738 ) ) ;
#1253 = ADVANCED_FACE ( 'NONE', ( #12943 ), #10365, .F. ) ;
#1252 = DIRECTION ( 'NONE',  ( 0.000000000000000000, -0.4721928772777346239, -0.8814952561688430555 ) ) ;
#1254 = FACE_BOUND ( 'NONE', #25184, .T. ) ;
#1255 = VERTEX_POINT ( 'NONE', #130282 ) ;
#1256 = CARTESIAN_POINT ( 'NONE',  ( 21.14999999999999503, 76.10000000001203091, -114.6726782920691079 ) ) ;
#1257 = ORIENTED_EDGE ( 'NONE', *, *, #10705, .T. ) ;
#1258 = EDGE_CURVE ( 'NONE', #252901, #127123, #130020, .T. ) ;
#1259 = CARTESIAN_POINT ( 'NONE',  ( -12.33960340485503515, 9.360749169915104417, -17.31457014060726962 ) ) ;
#1260 = ORIENTED_EDGE ( 'NONE', *, *, #116402, .F. ) ;
#1262 = EDGE_CURVE ( 'NONE', #252143, #114575, #242463, .T. ) ;
#1261 = CIRCLE ( 'NONE', #80352, 0.09999999999999883982 ) ;
#1263 = AXIS2_PLACEMENT_3D ( 'NONE', #235738, #57082, #136631 ) ;
#1264 = CIRCLE ( 'NONE', #80355, 11.75000000000001066 ) ;
#1265 = VECTOR ( 'NONE', #67470, 1000.000000000000000 ) ;
#1266 = CARTESIAN_POINT ( 'NONE',  ( 18.44206774312972996, 85.49102735755145943, -29.39687997982606404 ) ) ;
#1267 = EDGE_CURVE ( 'NONE', #34286, #18345, #17600, .T. ) ;
#1268 = EDGE_CURVE ( 'NONE', #177395, #152802, #103725, .T. ) ;
#1269 = ORIENTED_EDGE ( 'NONE', *, *, #30961, .F. ) ;
#1270 = CARTESIAN_POINT ( 'NONE',  ( -17.01764560440403784, 66.05000000001263061, -190.7731074853133180 ) ) ;
#1271 = ORIENTED_EDGE ( 'NONE', *, *, #247386, .F. ) ;
#1272 = EDGE_CURVE ( 'NONE', #91651, #218145, #55012, .T. ) ;
#1273 = DIRECTION ( 'NONE',  ( 0.000000000000000000, -1.000000000000000000, -6.789366196018718420E-15 ) ) ;
#1274 = CARTESIAN_POINT ( 'NONE',  ( -23.15000000000000213, 7.128833340094563376, -233.7327013124401276 ) ) ;
#1275 = DIRECTION ( 'NONE',  ( 1.000000000000000000, 0.000000000000000000, 0.000000000000000000 ) ) ;
#1276 = CARTESIAN_POINT ( 'NONE',  ( 21.05000000000000071, 61.95000000001175522, -75.03680255528533394 ) ) ;
#1277 = DIRECTION ( 'NONE',  ( 1.000000000000000000, 0.000000000000000000, 0.000000000000000000 ) ) ;
#1279 = DIRECTION ( 'NONE',  ( -0.000000000000000000, 1.000000000000000000, -0.000000000000000000 ) ) ;
#1278 = PLANE ( 'NONE',  #112418 ) ;
#1280 = EDGE_CURVE ( 'NONE', #250524, #245594, #200785, .T. ) ;
#1281 = CARTESIAN_POINT ( 'NONE',  ( 16.87683809663749557, 9.950000000011131718, -54.35000000000000142 ) ) ;
#1283 = EDGE_LOOP ( 'NONE', ( #201603, #71956, #89397 ) ) ;
#1282 = CARTESIAN_POINT ( 'NONE',  ( 20.74625933824082580, 67.11708647892778856, -127.9679364604012477 ) ) ;
#1285 = CARTESIAN_POINT ( 'NONE',  ( -16.81453563122427752, 66.06089979457505024, -115.7348488238790338 ) ) ;
#1284 = CARTESIAN_POINT ( 'NONE',  ( -18.47140463609786210, 37.97412965213577962, -261.2273517166002534 ) ) ;
#1286 = VERTEX_POINT ( 'NONE', #149882 ) ;
#1288 = EDGE_LOOP ( 'NONE', ( #222345, #60721, #222413, #103347 ) ) ;
#1287 = DIRECTION ( 'NONE',  ( -1.000000000000000000, 0.000000000000000000, 0.000000000000000000 ) ) ;
#1289 = VERTEX_POINT ( 'NONE', #29937 ) ;
#1290 = FACE_OUTER_BOUND ( 'NONE', #252660, .T. ) ;
#1291 = DIRECTION ( 'NONE',  ( 0.000000000000000000, 0.000000000000000000, -1.000000000000000000 ) ) ;
#1292 = CYLINDRICAL_SURFACE ( 'NONE', #68375, 12.87499999999999822 ) ;
#1293 = CIRCLE ( 'NONE', #172041, 0.1000000000000053346 ) ;
#1294 = VERTEX_POINT ( 'NONE', #91167 ) ;
#1295 = DIRECTION ( 'NONE',  ( 0.000000000000000000, 7.086529944415894657E-15, -1.000000000000000000 ) ) ;
#1296 = LINE ( 'NONE', #62581, #184822 ) ;
#1297 = DIRECTION ( 'NONE',  ( 0.000000000000000000, -6.982962677686266711E-15, 1.000000000000000000 ) ) ;
#1298 = EDGE_LOOP ( 'NONE', ( #189655, #86851, #167928, #233536 ) ) ;
#1300 = ADVANCED_FACE ( 'NONE', ( #170762 ), #69060, .F. ) ;
#1299 = CARTESIAN_POINT ( 'NONE',  ( -18.54148534481894472, 46.44433919924418319, -243.0795225066946159 ) ) ;
#1301 = B_SPLINE_CURVE_WITH_KNOTS ( 'NONE', 3,
 ( #78150, #179853, #222794, #162864, #237246, #44192, #98978, #200690, #58583, #161581, #61170, #42898, #178584 ),
 .UNSPECIFIED., .F., .F.,
 ( 4, 3, 3, 3, 4 ),
 ( 1.084445006577768341E-16, 1.946463881814499081E-05, 3.922356109944648083E-05, 4.215060953239448225E-05, 4.415117091092920593E-05 ),
 .UNSPECIFIED. ) ;
#1302 = CARTESIAN_POINT ( 'NONE',  ( 21.07971444708685738, 69.67020791838558580, -136.6109309208422644 ) ) ;
#1303 = EDGE_LOOP ( 'NONE', ( #252309, #196137, #144068, #151074 ) ) ;
#1304 = ORIENTED_EDGE ( 'NONE', *, *, #48349, .T. ) ;
#1305 = CARTESIAN_POINT ( 'NONE',  ( -23.25000000000000000, 68.76258920191057200, -222.5680764032308048 ) ) ;
#1306 = AXIS2_PLACEMENT_3D ( 'NONE', #80522, #239639, #121000 ) ;
#1307 = CIRCLE ( 'NONE', #167950, 0.09999999999998898659 ) ;
#1308 = ORIENTED_EDGE ( 'NONE', *, *, #192763, .F. ) ;
#1309 = CARTESIAN_POINT ( 'NONE',  ( 18.49999999999999289, 65.50857864377491069, -145.1731074845244507 ) ) ;
#1310 = ORIENTED_EDGE ( 'NONE', *, *, #34015, .F. ) ;
#1311 = DIRECTION ( 'NONE',  ( 1.000000000000000000, 0.000000000000000000, 0.000000000000000000 ) ) ;
#1312 = EDGE_CURVE ( 'NONE', #167415, #254024, #125760, .T. ) ;
#1313 = DIRECTION ( 'NONE',  ( 0.000000000000000000, 0.9126074666064236673, 0.4088369013362239679 ) ) ;
#1314 = DIRECTION ( 'NONE',  ( -0.000000000000000000, -0.8814952561688430555, 0.4721928772777346239 ) ) ;
#1315 = DIRECTION ( 'NONE',  ( -1.000000000000000000, -0.000000000000000000, -0.000000000000000000 ) ) ;
#1316 = CARTESIAN_POINT ( 'NONE',  ( 20.95346350065193519, 60.88192102021747587, -225.3139116850534833 ) ) ;
#1317 = ORIENTED_EDGE ( 'NONE', *, *, #97114, .T. ) ;
#1319 = CIRCLE ( 'NONE', #118039, 0.1000000000000055844 ) ;
#1318 = DIRECTION ( 'NONE',  ( 1.000000000000000000, 0.000000000000000000, 0.000000000000000000 ) ) ;
#1320 = CARTESIAN_POINT ( 'NONE',  ( 20.73486653747088226, 7.250000000011182166, -46.15000000000000568 ) ) ;
#1321 = LINE ( 'NONE', #118740, #239105 ) ;
#1322 = ORIENTED_EDGE ( 'NONE', *, *, #36825, .T. ) ;
#1324 = DIRECTION ( 'NONE',  ( 1.000000000000000000, 0.000000000000000000, 0.000000000000000000 ) ) ;
#1323 = CARTESIAN_POINT ( 'NONE',  ( -22.42357213249529480, 75.90091303601087702, -177.6960398708842774 ) ) ;
#1326 = ORIENTED_EDGE ( 'NONE', *, *, #86425, .F. ) ;
#1325 = CIRCLE ( 'NONE', #163847, 0.09999999999999564793 ) ;
#1328 = ORIENTED_EDGE ( 'NONE', *, *, #26805, .F. ) ;
#1327 = DIRECTION ( 'NONE',  ( 1.000000000000000000, 0.000000000000000000, 0.000000000000000000 ) ) ;
#1329 = EDGE_CURVE ( 'NONE', #121951, #79366, #159296, .T. ) ;
#1330 = ORIENTED_EDGE ( 'NONE', *, *, #171509, .T. ) ;
#1331 = DIRECTION ( 'NONE',  ( 0.000000000000000000, -7.086529944415886769E-15, 1.000000000000000000 ) ) ;
#1333 = DIRECTION ( 'NONE',  ( 0.000000000000000000, 0.000000000000000000, 1.000000000000000000 ) ) ;
#1332 = AXIS2_PLACEMENT_3D ( 'NONE', #140565, #62330, #242231 ) ;
#1334 = CARTESIAN_POINT ( 'NONE',  ( -18.40000000000000213, 64.52683809664951298, -115.5731074845243853 ) ) ;
#1336 = ORIENTED_EDGE ( 'NONE', *, *, #63720, .F. ) ;
#1335 =( BOUNDED_CURVE ( )  B_SPLINE_CURVE ( 3, ( #84635, #62558, #164232, #200777 ),
 .UNSPECIFIED., .F., .F. ) 
 B_SPLINE_CURVE_WITH_KNOTS ( ( 4, 4 ),
 ( 1.570796326794885012, 3.141592653589794448 ),
 .UNSPECIFIED. ) 
 CURVE ( )  GEOMETRIC_REPRESENTATION_ITEM ( )  RATIONAL_B_SPLINE_CURVE ( ( 1.000000000000000000, 0.8047378541243619399, 0.8047378541243619399, 1.000000000000000000 ) ) 
 REPRESENTATION_ITEM ( '' )  );
#1338 = EDGE_CURVE ( 'NONE', #144177, #154033, #211118, .T. ) ;
#1337 = DIRECTION ( 'NONE',  ( 0.000000000000000000, 0.2617529984165152257, 0.9651348961777124202 ) ) ;
#1340 = DIRECTION ( 'NONE',  ( 1.000000000000000000, 0.000000000000000000, 0.000000000000000000 ) ) ;
#1339 = FACE_BOUND ( 'NONE', #186909, .T. ) ;
#1342 = ORIENTED_EDGE ( 'NONE', *, *, #193622, .T. ) ;
#1341 = DIRECTION ( 'NONE',  ( -0.000000000000000000, -6.982962677686266711E-15, 1.000000000000000000 ) ) ;
#1343 = AXIS2_PLACEMENT_3D ( 'NONE', #63673, #119830, #138067 ) ;
#1344 = EDGE_CURVE ( 'NONE', #95913, #198456, #59265, .T. ) ;
#1345 = TOROIDAL_SURFACE ( 'NONE', #51387, 0.2000000000000000111, 0.1000000000000000056 ) ;
#1346 = ADVANCED_FACE ( 'NONE', ( #229406 ), #188493, .T. ) ;
#1347 = AXIS2_PLACEMENT_3D ( 'NONE', #224806, #43623, #241811 ) ;
#1348 = VERTEX_POINT ( 'NONE', #209839 ) ;
#1349 = ADVANCED_FACE ( 'NONE', ( #250241 ), #148585, .T. ) ;
#1350 = DIRECTION ( 'NONE',  ( 1.186688945009010077E-16, 1.000000000000000000, 6.982962677686266711E-15 ) ) ;
#1351 = EDGE_LOOP ( 'NONE', ( #149134, #36739, #59727, #188975 ) ) ;
#1352 = CARTESIAN_POINT ( 'NONE',  ( 13.40000000000000036, -8.350000000000004974, 19.04142135623731136 ) ) ;
#1353 = ORIENTED_EDGE ( 'NONE', *, *, #85308, .T. ) ;
#1354 = ADVANCED_FACE ( 'NONE', ( #88580 ), #208179, .T. ) ;
#1355 = DIRECTION ( 'NONE',  ( 1.000000000000000000, -3.965082230804126670E-15, 0.000000000000000000 ) ) ;
#1356 = DIRECTION ( 'NONE',  ( 1.000000000000000000, 3.265361837132813093E-16, -0.000000000000000000 ) ) ;
#1357 = DIRECTION ( 'NONE',  ( 1.000000000000000000, -7.304098846218135653E-16, -2.111765289898286048E-31 ) ) ;
#1358 = EDGE_LOOP ( 'NONE', ( #114954, #154136, #45014 ) ) ;
#1359 = FACE_OUTER_BOUND ( 'NONE', #222216, .T. ) ;
#1360 = CIRCLE ( 'NONE', #163695, 0.1000000000000028644 ) ;
#1361 = AXIS2_PLACEMENT_3D ( 'NONE', #98472, #112958, #18973 ) ;
#1362 = CIRCLE ( 'NONE', #196999, 0.1999999999999987899 ) ;
#1363 = CARTESIAN_POINT ( 'NONE',  ( 21.05000000000005400, 76.00000000001119815, -36.02310748452479316 ) ) ;
#1364 = EDGE_CURVE ( 'NONE', #205644, #71110, #67688, .T. ) ;
#1365 = ORIENTED_EDGE ( 'NONE', *, *, #203704, .F. ) ;
#1366 = VERTEX_POINT ( 'NONE', #174615 ) ;
#1367 = ORIENTED_EDGE ( 'NONE', *, *, #19245, .F. ) ;
#1368 = DIRECTION ( 'NONE',  ( 0.000000000000000000, 0.000000000000000000, -1.000000000000000000 ) ) ;
#1369 = ORIENTED_EDGE ( 'NONE', *, *, #215843, .F. ) ;
#1371 = ORIENTED_EDGE ( 'NONE', *, *, #163107, .F. ) ;
#1370 = DIRECTION ( 'NONE',  ( -1.000000000000000000, 7.304098846218135653E-16, 0.000000000000000000 ) ) ;
#1372 = ADVANCED_FACE ( 'NONE', ( #75483 ), #194142, .F. ) ;
#1373 = EDGE_CURVE ( 'NONE', #62686, #5270, #114584, .T. ) ;
#1374 = ORIENTED_EDGE ( 'NONE', *, *, #27708, .F. ) ;
#1377 = ORIENTED_EDGE ( 'NONE', *, *, #102892, .F. ) ;
#1376 = ORIENTED_EDGE ( 'NONE', *, *, #1643, .T. ) ;
#1375 = DIRECTION ( 'NONE',  ( -1.000000000000000000, 2.952720810173289112E-16, 2.061873921506763405E-30 ) ) ;
#1378 = AXIS2_PLACEMENT_3D ( 'NONE', #246617, #163255, #23761 ) ;
#1379 = AXIS2_PLACEMENT_3D ( 'NONE', #104414, #182715, #83561 ) ;
#1380 = ADVANCED_FACE ( 'NONE', ( #14222 ), #167674, .T. ) ;
#1381 = ORIENTED_EDGE ( 'NONE', *, *, #10400, .F. ) ;
#1382 = SPHERICAL_SURFACE ( 'NONE', #206436, 0.1000000000000000056 ) ;
#1383 = CIRCLE ( 'NONE', #155572, 0.1000000000000050987 ) ;
#1384 = LINE ( 'NONE', #163073, #68078 ) ;
#1385 = CARTESIAN_POINT ( 'NONE',  ( -16.97683809663752186, 13.99889777621145903, -218.5199410132753428 ) ) ;
#1386 = ORIENTED_EDGE ( 'NONE', *, *, #239545, .T. ) ;
#1387 = TOROIDAL_SURFACE ( 'NONE', #163725, 12.77500000000000036, 0.1000000000000000056 ) ;
#1388 = CARTESIAN_POINT ( 'NONE',  ( -18.59999999999999787, 5.341242990002807112, -23.69334979351197745 ) ) ;
#1389 = TOROIDAL_SURFACE ( 'NONE', #39030, 0.2000000000000000111, 0.1000000000000000056 ) ;
#1391 = EDGE_LOOP ( 'NONE', ( #245342, #198224, #7987, #176680 ) ) ;
#1390 = DIRECTION ( 'NONE',  ( -1.070660780358590712E-14, 0.9875102702516478370, -0.1575546449569727447 ) ) ;
#1392 = CARTESIAN_POINT ( 'NONE',  ( -21.14999999999999858, 30.94729882110367569, -252.1099006007311232 ) ) ;
#1394 = EDGE_LOOP ( 'NONE', ( #63811, #237664, #26093, #226339 ) ) ;
#1393 = CARTESIAN_POINT ( 'NONE',  ( 19.97071067811864609, 11.72071067812981404, -125.1500000000000341 ) ) ;
#1395 =( BOUNDED_SURFACE ( )  B_SPLINE_SURFACE ( 3, 2, ( 
 ( #95052, #196717, #256638 ),
 ( #59750, #15551, #178476 ),
 ( #54636, #115915, #134173 ),
 ( #179742, #114620, #156350 ),
 ( #254115, #75520, #155065 ),
 ( #234564, #74250, #117193 ),
 ( #199305, #55900, #237139 ),
 ( #177196, #135452, #20676 ),
 ( #217549, #37676, #98873 ),
 ( #235840, #38951, #214996 ) ),
 .UNSPECIFIED., .F., .F., .F. ) 
 B_SPLINE_SURFACE_WITH_KNOTS ( ( 4, 2, 2, 2, 4 ),
 ( 3, 3 ),
 ( 0.002161241639767768653, 0.002579950749617439427, 0.002789305304542274815, 0.002893982582004692508, 0.002998659859467110202 ),
 ( 0.000000000000000000, 1.000000000000000000 ),
 .UNSPECIFIED. ) 
 GEOMETRIC_REPRESENTATION_ITEM ( )  RATIONAL_B_SPLINE_SURFACE ( (
 ( 1.000000000000000000, 0.7071067811864816255, 1.000000000000000000),
 ( 1.000000000000000000, 0.7632447400665326454, 1.000000000000000000),
 ( 1.000000000000000000, 0.8158073005107645548, 1.000000000000000000),
 ( 1.000000000000000000, 0.8906973462396717833, 1.000000000000000000),
 ( 1.000000000000000000, 0.9149408947796511260, 1.000000000000000000),
 ( 1.000000000000000000, 0.9493368785277698230, 1.000000000000000000),
 ( 1.000000000000000000, 0.9605194247158244103, 1.000000000000000000),
 ( 1.000000000000000000, 0.9803630264779819026, 1.000000000000000000),
 ( 1.000000000000000000, 0.9900844824272359013, 1.000000000000000000),
 ( 1.000000000000000000, 0.9894588281429361754, 1.000000000000000000) ) ) 
 REPRESENTATION_ITEM ( '' )  SURFACE ( )  );
#1396 = ORIENTED_EDGE ( 'NONE', *, *, #10929, .T. ) ;
#1397 = VECTOR ( 'NONE', #170639, 1000.000000000000227 ) ;
#1398 = CARTESIAN_POINT ( 'NONE',  ( 18.49999999999999645, 1.148907358139439339E-11, -201.0000000000015064 ) ) ;
#1400 = EDGE_CURVE ( 'NONE', #241874, #133509, #242653, .T. ) ;
#1399 =( LENGTH_UNIT ( ) NAMED_UNIT ( * ) SI_UNIT ( .MILLI., .METRE. ) );
#1401 = AXIS2_PLACEMENT_3D ( 'NONE', #177812, #119103, #201198 ) ;
#1402 = ORIENTED_EDGE ( 'NONE', *, *, #146572, .F. ) ;
#1403 = ORIENTED_EDGE ( 'NONE', *, *, #157105, .F. ) ;
#1404 = AXIS2_PLACEMENT_3D ( 'NONE', #179154, #203814, #100818 ) ;
#1405 = DIRECTION ( 'NONE',  ( 3.616040088954490704E-32, 7.105427357601001859E-15, -1.000000000000000000 ) ) ;
#1407 = ADVANCED_FACE ( 'NONE', ( #79280 ), #5302, .F. ) ;
#1406 = DIRECTION ( 'NONE',  ( 0.000000000000000000, -1.000000000000000000, -7.272083257015735086E-15 ) ) ;
#1408 = AXIS2_PLACEMENT_3D ( 'NONE', #143754, #31253, #208582 ) ;
#1410 = ORIENTED_EDGE ( 'NONE', *, *, #124135, .T. ) ;
#1409 = VERTEX_POINT ( 'NONE', #197953 ) ;
#1411 = ORIENTED_EDGE ( 'NONE', *, *, #194967, .F. ) ;
#1412 = CARTESIAN_POINT ( 'NONE',  ( -21.05000000000000071, 74.83729825007360148, -61.52310748452433131 ) ) ;
#1413 = ORIENTED_EDGE ( 'NONE', *, *, #158241, .F. ) ;
#1414 = EDGE_LOOP ( 'NONE', ( #203161, #178221, #177205, #167831 ) ) ;
#1416 = EDGE_CURVE ( 'NONE', #106998, #147671, #205037, .T. ) ;
#1415 = ORIENTED_EDGE ( 'NONE', *, *, #119535, .T. ) ;
#1417 = CARTESIAN_POINT ( 'NONE',  ( -20.64999999999999858, 71.65000000001253966, -182.3731074845244109 ) ) ;
#1418 = AXIS2_PLACEMENT_3D ( 'NONE', #15989, #95484, #255802 ) ;
#1420 = CARTESIAN_POINT ( 'NONE',  ( -18.59999999999999787, 11.65000000001115232, -74.01480577065404987 ) ) ;
#1419 = DIRECTION ( 'NONE',  ( 0.000000000000000000, 0.000000000000000000, -1.000000000000000000 ) ) ;
#1421 = ORIENTED_EDGE ( 'NONE', *, *, #65537, .F. ) ;
#1422 = ADVANCED_FACE ( 'NONE', ( #139245 ), #255316, .F. ) ;
#1424 = ORIENTED_EDGE ( 'NONE', *, *, #36460, .F. ) ;
#1423 = ORIENTED_EDGE ( 'NONE', *, *, #186682, .F. ) ;
#1425 = AXIS2_PLACEMENT_3D ( 'NONE', #107, #79635, #159217 ) ;
#1426 = DIRECTION ( 'NONE',  ( -4.408576920032448588E-17, 0.1350103645451876944, -0.9908441862701601321 ) ) ;
#1427 = LINE ( 'NONE', #80959, #99390 ) ;
#1428 = ADVANCED_FACE ( 'NONE', ( #156308 ), #251014, .T. ) ;
#1429 = EDGE_LOOP ( 'NONE', ( #115752, #177221, #179062, #191512 ) ) ;
#1430 = CIRCLE ( 'NONE', #180516, 11.74999999999999645 ) ;
#1432 =( BOUNDED_SURFACE ( )  B_SPLINE_SURFACE ( 3, 2, ( 
 ( #219285, #241437, #40702 ),
 ( #118927, #101883, #139735 ),
 ( #120236, #257085, #62791 ),
 ( #142312, #181469, #221830 ) ),
 .UNSPECIFIED., .F., .F., .F. ) 
 B_SPLINE_SURFACE_WITH_KNOTS ( ( 4, 4 ),
 ( 3, 3 ),
 ( 0.000000000000000000, 0.001979672783031562362 ),
 ( 0.000000000000000000, 1.000000000000000000 ),
 .UNSPECIFIED. ) 
 GEOMETRIC_REPRESENTATION_ITEM ( )  RATIONAL_B_SPLINE_SURFACE ( (
 ( 1.000000000000000000, 0.7103081912008041288, 1.000000000000000000),
 ( 1.000000000000000000, 0.7104998333558241175, 1.000000000000000000),
 ( 1.000000000000000000, 0.7107238315755781688, 1.000000000000000000),
 ( 1.000000000000000000, 0.7110073749538949883, 1.000000000000000000) ) ) 
 REPRESENTATION_ITEM ( '' )  SURFACE ( )  );
#1431 = CIRCLE ( 'NONE', #64472, 11.79999999999999538 ) ;
#1433 = VECTOR ( 'NONE', #43701, 1000.000000000000114 ) ;
#1434 = EDGE_CURVE ( 'NONE', #127173, #23304, #130213, .T. ) ;
#1435 = AXIS2_PLACEMENT_3D ( 'NONE', #47076, #126633, #27576 ) ;
#1436 = CARTESIAN_POINT ( 'NONE',  ( -21.14999999999999858, 12.92448621296781930, -205.1280733356431938 ) ) ;
#1437 = EDGE_CURVE ( 'NONE', #26265, #126765, #32201, .T. ) ;
#1438 = EDGE_LOOP ( 'NONE', ( #59081, #252539, #235616, #116783 ) ) ;
#1439 = ORIENTED_EDGE ( 'NONE', *, *, #171966, .F. ) ;
#1440 = CARTESIAN_POINT ( 'NONE',  ( -20.85000000000000142, 67.67657779757796277, -227.9615671787948372 ) ) ;
#1441 = EDGE_LOOP ( 'NONE', ( #100065, #27139, #58016, #75040 ) ) ;
#1442 = DIRECTION ( 'NONE',  ( -1.000000000000000000, 0.000000000000000000, -0.000000000000000000 ) ) ;
#1443 = DIRECTION ( 'NONE',  ( 1.000000000000000000, 0.000000000000000000, 0.000000000000000000 ) ) ;
#1444 = EDGE_LOOP ( 'NONE', ( #137862, #189832, #184078, #139307 ) ) ;
#1445 = CYLINDRICAL_SURFACE ( 'NONE', #110321, 0.5000000000000004441 ) ;
#1446 = DIRECTION ( 'NONE',  ( 1.000000000000000000, 0.000000000000000000, 0.000000000000000000 ) ) ;
#1448 = CARTESIAN_POINT ( 'NONE',  ( -16.85722902420154767, 9.950000000011135270, -121.2344525262295463 ) ) ;
#1447 = DIRECTION ( 'NONE',  ( 1.652117596168391700E-15, 1.000000000000000000, -0.000000000000000000 ) ) ;
#1449 = DIRECTION ( 'NONE',  ( -1.000000000000000000, 1.836970198721029934E-16, 1.282749433769087757E-30 ) ) ;
#1450 = CARTESIAN_POINT ( 'NONE',  ( -23.25000000000000000, 76.00000000001165290, -61.62310748452430431 ) ) ;
#1451 = DIRECTION ( 'NONE',  ( 0.000000000000000000, -1.000000000000000000, 0.000000000000000000 ) ) ;
#1452 = DIRECTION ( 'NONE',  ( 1.000000000000000000, 0.000000000000000000, -0.000000000000000000 ) ) ;
#1453 = CARTESIAN_POINT ( 'NONE',  ( 21.14999999999999858, 76.00000000001200817, -109.5637644362255685 ) ) ;
#1454 = FACE_OUTER_BOUND ( 'NONE', #199672, .T. ) ;
#1455 = AXIS2_PLACEMENT_3D ( 'NONE', #14863, #232629, #76091 ) ;
#1457 = ORIENTED_EDGE ( 'NONE', *, *, #165449, .F. ) ;
#1456 = AXIS2_PLACEMENT_3D ( 'NONE', #81465, #648, #179341 ) ;
#1459 = EDGE_CURVE ( 'NONE', #21234, #49859, #17775, .T. ) ;
#1458 = TOROIDAL_SURFACE ( 'NONE', #201375, 0.2000000000000000111, 0.1000000000000000056 ) ;
#1460 = VECTOR ( 'NONE', #174331, 1000.000000000000000 ) ;
#1461 = ADVANCED_FACE ( 'NONE', ( #80550 ), #121028, .T. ) ;
#1463 = VERTEX_POINT ( 'NONE', #200529 ) ;
#1462 = ORIENTED_EDGE ( 'NONE', *, *, #232577, .T. ) ;
#1464 = ORIENTED_EDGE ( 'NONE', *, *, #230041, .F. ) ;
#1465 = ORIENTED_EDGE ( 'NONE', *, *, #68076, .T. ) ;
#1466 = CARTESIAN_POINT ( 'NONE',  ( -16.98495255085919098, 10.00556436600592924, -79.63461720622055395 ) ) ;
#1467 = CARTESIAN_POINT ( 'NONE',  ( 20.94999999999999929, 77.34915357198845243, -162.2356101489344837 ) ) ;
#1469 = CYLINDRICAL_SURFACE ( 'NONE', #111460, 0.1000000000000028644 ) ;
#1468 = CARTESIAN_POINT ( 'NONE',  ( -23.15000000000000213, 64.35000000001258513, -191.3731074845244393 ) ) ;
#1470 = DIRECTION ( 'NONE',  ( 0.000000000000000000, 0.000000000000000000, -1.000000000000000000 ) ) ;
#1471 = ORIENTED_EDGE ( 'NONE', *, *, #52588, .F. ) ;
#1472 = LINE ( 'NONE', #118882, #221495 ) ;
#1473 = EDGE_CURVE ( 'NONE', #233248, #67516, #20631, .T. ) ;
#1474 = FACE_OUTER_BOUND ( 'NONE', #212469, .T. ) ;
#1475 = CARTESIAN_POINT ( 'NONE',  ( 18.59999999999997655, 77.16412189325360771, -162.1082593989527254 ) ) ;
#1476 = B_SPLINE_CURVE_WITH_KNOTS ( 'NONE', 3,
 ( #18926, #174203, #254914, #149808, #215829, #236684, #75090, #154627, #115458, #169391, #195025, #257485, #214557, #248892, #97141, #234121, #196285, #98425, #176743 ),
 .UNSPECIFIED., .F., .F.,
 ( 4, 3, 3, 3, 3, 3, 4 ),
 ( 0.000000000000000000, 7.110282409889811541E-05, 0.0001508797727291456749, 0.0002027344179858454128, 0.0002343294522348951471, 0.0002454816334821100063, 0.0002619873080085602097 ),
 .UNSPECIFIED. ) ;
#1477 = EDGE_CURVE ( 'NONE', #5738, #125216, #26199, .T. ) ;
#1478 = CARTESIAN_POINT ( 'NONE',  ( -17.04761207306819060, 65.97354912661452886, -157.3731074845244109 ) ) ;
#1479 = VERTEX_POINT ( 'NONE', #244777 ) ;
#1480 = DIRECTION ( 'NONE',  ( 1.000000000000000000, 0.000000000000000000, 0.000000000000000000 ) ) ;
#1481 = CARTESIAN_POINT ( 'NONE',  ( -18.59999999999999787, 79.19526988099229925, -196.1889237952725296 ) ) ;
#1482 = VERTEX_POINT ( 'NONE', #62306 ) ;
#1483 = DIRECTION ( 'NONE',  ( -0.000000000000000000, 1.000000000000000000, -0.000000000000000000 ) ) ;
#1484 = DIRECTION ( 'NONE',  ( 1.000000000000000000, 0.000000000000000000, 0.000000000000000000 ) ) ;
#1485 = ADVANCED_FACE ( 'NONE', ( #218794 ), #100951, .F. ) ;
#1486 = CARTESIAN_POINT ( 'NONE',  ( -20.94999999999999929, 7.675662554762638479, -241.7139905447625381 ) ) ;
#1487 = DIRECTION ( 'NONE',  ( 1.000000000000000000, 0.000000000000000000, 0.000000000000000000 ) ) ;
#1488 = CARTESIAN_POINT ( 'NONE',  ( -18.40000000000000213, 43.39957528361355799, -233.6562381667159798 ) ) ;
#1489 = ORIENTED_EDGE ( 'NONE', *, *, #175669, .F. ) ;
#1490 = DIRECTION ( 'NONE',  ( 0.000000000000000000, 0.000000000000000000, 1.000000000000000000 ) ) ;
#1491 = DIRECTION ( 'NONE',  ( 0.000000000000000000, -0.8164989248600462712, 0.5773469543544753613 ) ) ;
#1492 = CYLINDRICAL_SURFACE ( 'NONE', #191762, 0.09999999999999892308 ) ;
#1494 = LINE ( 'NONE', #24948, #45413 ) ;
#1493 = DIRECTION ( 'NONE',  ( -1.000000000000000000, 7.304098846218134667E-16, 2.111765289898285610E-31 ) ) ;
#1495 = CARTESIAN_POINT ( 'NONE',  ( -20.94999999999994600, 66.25000000001114131, -51.02310748452476474 ) ) ;
#1497 = EDGE_CURVE ( 'NONE', #177351, #201736, #196861, .T. ) ;
#1496 = CARTESIAN_POINT ( 'NONE',  ( -23.15000000000000213, 73.50000000001254818, -183.2477294072864709 ) ) ;
#1498 = DIRECTION ( 'NONE',  ( 1.000000000000000000, 0.000000000000000000, 0.000000000000000000 ) ) ;
#1499 = CARTESIAN_POINT ( 'NONE',  ( -20.94999999999999929, 1.115600667400684642E-11, -96.40000000000003411 ) ) ;
#1501 = EDGE_LOOP ( 'NONE', ( #80472, #68584, #253815, #52085 ) ) ;
#1500 = CARTESIAN_POINT ( 'NONE',  ( -21.14999999999999858, 87.75000000001192291, -100.1231074845242262 ) ) ;
#1502 = TOROIDAL_SURFACE ( 'NONE', #14190, 0.2000000000000000111, 0.1000000000000000056 ) ;
#1503 = ORIENTED_EDGE ( 'NONE', *, *, #31993, .T. ) ;
#1504 = ORIENTED_EDGE ( 'NONE', *, *, #198365, .F. ) ;
#1505 = EDGE_CURVE ( 'NONE', #78857, #197503, #63577, .T. ) ;
#1506 = CARTESIAN_POINT ( 'NONE',  ( 20.94999999999999929, 14.61354176542825201, -235.9279552357344016 ) ) ;
#1507 = CARTESIAN_POINT ( 'NONE',  ( -23.25000000000000000, 1.115600667400684642E-11, -33.50000000000000000 ) ) ;
#1509 = LINE ( 'NONE', #6648, #175588 ) ;
#1508 = AXIS2_PLACEMENT_3D ( 'NONE', #56459, #216827, #96854 ) ;
#1510 = CARTESIAN_POINT ( 'NONE',  ( 21.53699400383268170, 65.45457063879538850, -242.4061840233472083 ) ) ;
#1511 = ORIENTED_EDGE ( 'NONE', *, *, #236939, .T. ) ;
#1512 = CIRCLE ( 'NONE', #51558, 0.1000000000000013933 ) ;
#1513 = DIRECTION ( 'NONE',  ( 0.000000000000000000, 0.000000000000000000, -1.000000000000000000 ) ) ;
#1514 = AXIS2_PLACEMENT_3D ( 'NONE', #216703, #117607, #38090 ) ;
#1515 = CARTESIAN_POINT ( 'NONE',  ( 18.59999999999999076, 65.79142135624984178, -182.2731074845244450 ) ) ;
#1516 = DIRECTION ( 'NONE',  ( 1.000000000000000000, -0.000000000000000000, -0.000000000000000000 ) ) ;
#1517 = AXIS2_PLACEMENT_3D ( 'NONE', #15530, #95033, #174632 ) ;
#1518 = CARTESIAN_POINT ( 'NONE',  ( 20.94999999999999929, -8.999999999988844479, -43.39396912265245021 ) ) ;
#1520 = ORIENTED_EDGE ( 'NONE', *, *, #63237, .F. ) ;
#1519 = CARTESIAN_POINT ( 'NONE',  ( -18.59999999999999787, 13.71992543034163958, -238.5823796952984992 ) ) ;
#1522 = CARTESIAN_POINT ( 'NONE',  ( -17.80356949363962826, 10.87673139701326441, -157.2130730242256220 ) ) ;
#1521 = CARTESIAN_POINT ( 'NONE',  ( -17.04761207306821191, 10.02645087340893326, -146.6500000000000341 ) ) ;
#1523 = DIRECTION ( 'NONE',  ( 0.000000000000000000, 0.8700118002898321601, -0.4930308989875230585 ) ) ;
#1524 = FACE_OUTER_BOUND ( 'NONE', #20858, .T. ) ;
#1525 = ORIENTED_EDGE ( 'NONE', *, *, #153889, .T. ) ;
#1526 = VECTOR ( 'NONE', #257656, 1000.000000000000000 ) ;
#1527 = DIRECTION ( 'NONE',  ( 0.000000000000000000, 0.000000000000000000, 1.000000000000000000 ) ) ;
#1529 = DIRECTION ( 'NONE',  ( 0.000000000000000000, 0.9915357197604892647, -0.1298341882519715440 ) ) ;
#1528 = AXIS2_PLACEMENT_3D ( 'NONE', #7515, #141884, #87026 ) ;
#1531 = AXIS2_PLACEMENT_3D ( 'NONE', #39502, #197251, #58994 ) ;
#1530 = CARTESIAN_POINT ( 'NONE',  ( -21.05000000000000071, 1.115600667400684642E-11, -67.00000000000000000 ) ) ;
#1532 = ORIENTED_EDGE ( 'NONE', *, *, #65148, .F. ) ;
#1533 = FACE_OUTER_BOUND ( 'NONE', #81379, .T. ) ;
#1534 = DIRECTION ( 'NONE',  ( 0.000000000000000000, 0.9651348961777157509, -0.2617529984165031243 ) ) ;
#1535 = ORIENTED_EDGE ( 'NONE', *, *, #187968, .T. ) ;
#1536 = DIRECTION ( 'NONE',  ( -1.000000000000000000, 3.151514657663852580E-16, -8.547182517843351137E-17 ) ) ;
#1537 = DIRECTION ( 'NONE',  ( 0.000000000000000000, -0.9770955615653315052, -0.2128009952263603954 ) ) ;
#1538 = CARTESIAN_POINT ( 'NONE',  ( 18.59999999999999787, 45.99141771592758943, -256.5205054824189119 ) ) ;
#1539 = ORIENTED_EDGE ( 'NONE', *, *, #4821, .T. ) ;
#1540 = ORIENTED_EDGE ( 'NONE', *, *, #8391, .F. ) ;
#1541 = AXIS2_PLACEMENT_3D ( 'NONE', #159374, #156826, #236325 ) ;
#1542 = AXIS2_PLACEMENT_3D ( 'NONE', #201731, #59621, #160067 ) ;
#1543 = CIRCLE ( 'NONE', #155719, 11.89999999999999858 ) ;
#1544 = CARTESIAN_POINT ( 'NONE',  ( -23.25000000000000000, 87.75000000001237765, -170.0231074845242745 ) ) ;
#1545 = DIRECTION ( 'NONE',  ( -1.000000000000000000, -0.000000000000000000, -0.000000000000000000 ) ) ;
#1546 = CARTESIAN_POINT ( 'NONE',  ( 21.10642757222115407, 13.08238103144605979, -210.6784328906550172 ) ) ;
#1547 = DIRECTION ( 'NONE',  ( -1.000000000000000000, 0.000000000000000000, 0.000000000000000000 ) ) ;
#1548 = EDGE_CURVE ( 'NONE', #58178, #63249, #2309, .T. ) ;
#1550 = CARTESIAN_POINT ( 'NONE',  ( 22.88900146558018989, 8.703904791123973084, -46.15000000000001279 ) ) ;
#1549 = CYLINDRICAL_SURFACE ( 'NONE', #157506, 0.09999999999999939493 ) ;
#1551 = FACE_OUTER_BOUND ( 'NONE', #194817, .T. ) ;
#1552 = DIRECTION ( 'NONE',  ( 0.000000000000000000, 0.000000000000000000, -1.000000000000000000 ) ) ;
#1553 = CARTESIAN_POINT ( 'NONE',  ( 22.40000000000010516, 76.00000000001315925, -148.2735403769831919 ) ) ;
#1554 = ORIENTED_EDGE ( 'NONE', *, *, #6296, .T. ) ;
#1555 = DIRECTION ( 'NONE',  ( 0.000000000000000000, 0.000000000000000000, -1.000000000000000000 ) ) ;
#1557 = EDGE_LOOP ( 'NONE', ( #199268, #132770, #118113, #188463 ) ) ;
#1556 = DIRECTION ( 'NONE',  ( 1.000000000000000000, 0.000000000000000000, 0.000000000000000000 ) ) ;
#1558 = CARTESIAN_POINT ( 'NONE',  ( 20.95575313997065336, 65.38544669673778742, -195.9018167825796013 ) ) ;
#1559 = CARTESIAN_POINT ( 'NONE',  ( 23.14999999999999858, 2.000000000011158630, -100.5000000000000426 ) ) ;
#1561 = CARTESIAN_POINT ( 'NONE',  ( 18.49999999999999289, 64.25000000001220712, -148.2731074845243882 ) ) ;
#1560 = CARTESIAN_POINT ( 'NONE',  ( 21.93340585898353723, 76.00000000001200817, -110.3472545066553181 ) ) ;
#1562 = EDGE_LOOP ( 'NONE', ( #208368, #145962, #52787, #187592 ) ) ;
#1564 = DIRECTION ( 'NONE',  ( 0.000000000000000000, -2.664535259100430523E-15, -1.000000000000000000 ) ) ;
#1563 = CARTESIAN_POINT ( 'NONE',  ( -16.88705144915421030, 66.05000000001159322, -56.59212888981229383 ) ) ;
#1565 = CARTESIAN_POINT ( 'NONE',  ( -18.59999999999999787, 70.15623657602074559, -198.0563205710787713 ) ) ;
#1566 = LINE ( 'NONE', #83645, #180517 ) ;
#1567 = PLANE ( 'NONE',  #132508 ) ;
#1568 = CARTESIAN_POINT ( 'NONE',  ( -14.22969084473440304, 66.54399267394325079, -185.0344739903777054 ) ) ;
#1569 = VERTEX_POINT ( 'NONE', #161428 ) ;
#1570 = DIRECTION ( 'NONE',  ( 1.000000000000000000, 0.000000000000000000, 0.000000000000000000 ) ) ;
#1572 = ADVANCED_FACE ( 'NONE', ( #45310 ), #171968, .T. ) ;
#1571 = ORIENTED_EDGE ( 'NONE', *, *, #45184, .F. ) ;
#1573 = VECTOR ( 'NONE', #176745, 1000.000000000000000 ) ;
#1574 = CIRCLE ( 'NONE', #63947, 11.89999999999999325 ) ;
#1575 = CARTESIAN_POINT ( 'NONE',  ( -16.78270389226384296, 9.947372616628161524, -54.34120703691146304 ) ) ;
#1576 = ORIENTED_EDGE ( 'NONE', *, *, #142962, .T. ) ;
#1577 = CARTESIAN_POINT ( 'NONE',  ( -17.11825945287482753, 66.05000000001157900, -56.77310748452439526 ) ) ;
#1578 = CIRCLE ( 'NONE', #80675, 0.1999999999999987899 ) ;
#1579 = ORIENTED_EDGE ( 'NONE', *, *, #24060, .T. ) ;
#1580 = CARTESIAN_POINT ( 'NONE',  ( 20.95512820512820440, 67.12384868372369340, -81.77310748452437394 ) ) ;
#1581 = EDGE_CURVE ( 'NONE', #109416, #94890, #71982, .T. ) ;
#1582 = TOROIDAL_SURFACE ( 'NONE', #180657, 0.2000000000000000111, 0.1000000000000000056 ) ;
#1584 = EDGE_CURVE ( 'NONE', #45271, #124804, #88508, .T. ) ;
#1583 = CARTESIAN_POINT ( 'NONE',  ( 15.48841904831874849, 12.80238349835111755, -219.5505295114098772 ) ) ;
#1585 = EDGE_LOOP ( 'NONE', ( #206508, #204425, #175251, #229716 ) ) ;
#1586 = AXIS2_PLACEMENT_3D ( 'NONE', #32071, #191144, #254875 ) ;
#1587 = EDGE_CURVE ( 'NONE', #218579, #256518, #102684, .T. ) ;
#1588 = LINE ( 'NONE', #141126, #111848 ) ;
#1589 = CARTESIAN_POINT ( 'NONE',  ( -18.50000000000000000, 79.14291928130900544, -196.3819507745080557 ) ) ;
#1591 = VECTOR ( 'NONE', #148746, 1000.000000000000000 ) ;
#1590 = CARTESIAN_POINT ( 'NONE',  ( 18.59999999999999432, 43.52285900727589762, -245.0935880436369985 ) ) ;
#1593 = AXIS2_PLACEMENT_3D ( 'NONE', #253971, #134029, #57037 ) ;
#1592 = DIRECTION ( 'NONE',  ( 0.000000000000000000, 0.000000000000000000, 1.000000000000000000 ) ) ;
#1594 = CARTESIAN_POINT ( 'NONE',  ( -23.15000000000000213, 28.42524210734032053, -258.3567845160494585 ) ) ;
#1595 = EDGE_CURVE ( 'NONE', #206343, #132612, #121869, .T. ) ;
#1596 = AXIS2_PLACEMENT_3D ( 'NONE', #245526, #66878, #107284 ) ;
#1597 = CARTESIAN_POINT ( 'NONE',  ( 12.29592348164039528, 62.46590406472955692, -217.6831045281099932 ) ) ;
#1598 = ORIENTED_EDGE ( 'NONE', *, *, #104966, .F. ) ;
#1599 = CARTESIAN_POINT ( 'NONE',  ( -20.64999999999999858, 36.65892442174472876, -249.5511627012454596 ) ) ;
#1600 = ORIENTED_EDGE ( 'NONE', *, *, #123794, .F. ) ;
#1602 = ORIENTED_EDGE ( 'NONE', *, *, #31508, .T. ) ;
#1601 = DIRECTION ( 'NONE',  ( 0.000000000000000000, -1.000000000000000000, -6.982962677686265922E-15 ) ) ;
#1603 = VECTOR ( 'NONE', #33822, 1000.000000000000227 ) ;
#1604 = EDGE_LOOP ( 'NONE', ( #60654, #74965, #96659, #87879 ) ) ;
#1605 = DIRECTION ( 'NONE',  ( 1.000000000000000000, -0.000000000000000000, -0.000000000000000000 ) ) ;
#1607 = EDGE_CURVE ( 'NONE', #216121, #231120, #9420, .T. ) ;
#1606 = DIRECTION ( 'NONE',  ( 1.000000000000000000, 7.304098846218134667E-16, -0.000000000000000000 ) ) ;
#1608 = CARTESIAN_POINT ( 'NONE',  ( 14.45204356427542258, 66.54933111084504560, -188.4675609943170400 ) ) ;
#1609 = CARTESIAN_POINT ( 'NONE',  ( -21.44999999999999929, 63.46669608621377279, -222.0380013001639270 ) ) ;
#1610 = LINE ( 'NONE', #81141, #79369 ) ;
#1611 = ORIENTED_EDGE ( 'NONE', *, *, #235679, .F. ) ;
#1612 = FACE_OUTER_BOUND ( 'NONE', #57645, .T. ) ;
#1614 = DIRECTION ( 'NONE',  ( 1.000000000000000000, 0.000000000000000000, 0.000000000000000000 ) ) ;
#1613 = AXIS2_PLACEMENT_3D ( 'NONE', #48354, #105731, #87466 ) ;
#1615 = VERTEX_POINT ( 'NONE', #163984 ) ;
#1617 = EDGE_CURVE ( 'NONE', #140162, #6455, #59446, .T. ) ;
#1616 = CARTESIAN_POINT ( 'NONE',  ( 18.59999999999999076, 51.87818942736608818, -231.5469534541122414 ) ) ;
#1618 = AXIS2_PLACEMENT_3D ( 'NONE', #201862, #105290, #104016 ) ;
#1619 = CARTESIAN_POINT ( 'NONE',  ( 23.14999999999999858, 11.65000000000000746, -26.48519422934606027 ) ) ;
#1620 = VERTEX_POINT ( 'NONE', #165255 ) ;
#1621 = CIRCLE ( 'NONE', #101554, 0.1000000000000000472 ) ;
#1622 = AXIS2_PLACEMENT_3D ( 'NONE', #232633, #14868, #177796 ) ;
#1623 = EDGE_LOOP ( 'NONE', ( #42024, #102009, #184230, #237736 ) ) ;
#1624 = DIRECTION ( 'NONE',  ( 0.000000000000000000, 0.000000000000000000, -1.000000000000000000 ) ) ;
#1625 = CARTESIAN_POINT ( 'NONE',  ( -18.59999999999999787, 64.02438395623025258, -266.2629958759080182 ) ) ;
#1626 = CARTESIAN_POINT ( 'NONE',  ( 20.99999999999999645, 66.25000000001162448, -60.27310748452439526 ) ) ;
#1627 = CARTESIAN_POINT ( 'NONE',  ( 21.14999999999999503, 76.00000000001165290, -69.52310748452431710 ) ) ;
#1628 = AXIS2_PLACEMENT_3D ( 'NONE', #235147, #253414, #214301 ) ;
#1629 = DIRECTION ( 'NONE',  ( 0.000000000000000000, -0.9908441862701596881, 0.1350103645451904977 ) ) ;
#1630 = CIRCLE ( 'NONE', #89135, 0.1000000000000000888 ) ;
#1631 = CIRCLE ( 'NONE', #143297, 11.74999999999999289 ) ;
#1632 = EDGE_LOOP ( 'NONE', ( #167534, #95771, #153789, #255852, #194006, #42861, #88956, #101450, #103179, #1381, #99248, #94098, #160662, #52035, #31709, #102029, #113560, #203152 ) ) ;
#1633 = ADVANCED_BREP_SHAPE_REPRESENTATION ( '', ( #20540, #2425 ), #56573 ) ;
#1634 = ADVANCED_FACE ( 'NONE', ( #186106 ), #7459, .T. ) ;
#1635 = ADVANCED_FACE ( 'NONE', ( #131258 ), #46572, .T. ) ;
#1636 = ORIENTED_EDGE ( 'NONE', *, *, #63940, .T. ) ;
#1637 = LINE ( 'NONE', #201135, #51954 ) ;
#1638 = FACE_OUTER_BOUND ( 'NONE', #117688, .T. ) ;
#1640 = VERTEX_POINT ( 'NONE', #167851 ) ;
#1639 = DIRECTION ( 'NONE',  ( 0.000000000000000000, 0.000000000000000000, -1.000000000000000000 ) ) ;
#1641 = CYLINDRICAL_SURFACE ( 'NONE', #28968, 11.80000000000000604 ) ;
#1643 = EDGE_CURVE ( 'NONE', #257362, #43709, #111700, .T. ) ;
#1642 = DIRECTION ( 'NONE',  ( 0.000000000000000000, -0.2128009952263982818, 0.9770955615653232895 ) ) ;
#1645 = EDGE_CURVE ( 'NONE', #160984, #20407, #109363, .T. ) ;
#1644 = CARTESIAN_POINT ( 'NONE',  ( 21.13614978966381841, 76.00000000001197975, -109.5222121863580895 ) ) ;
#1646 = DIRECTION ( 'NONE',  ( 0.000000000000000000, 1.000000000000000000, 0.000000000000000000 ) ) ;
#1647 = DIRECTION ( 'NONE',  ( -0.000000000000000000, 1.000000000000000000, -0.000000000000000000 ) ) ;
#1648 = CARTESIAN_POINT ( 'NONE',  ( -18.43599941264928077, 85.51932742860607561, -129.5501306950018261 ) ) ;
#1650 = ORIENTED_EDGE ( 'NONE', *, *, #170622, .T. ) ;
#1649 = CARTESIAN_POINT ( 'NONE',  ( -18.59999999999999787, 9.350000000011156942, -88.25000000000005684 ) ) ;
#1651 = EDGE_CURVE ( 'NONE', #102497, #9837, #51694, .T. ) ;
#1652 = ADVANCED_FACE ( 'NONE', ( #68726 ), #166568, .T. ) ;
#1654 = ADVANCED_FACE ( 'NONE', ( #246089 ), #129957, .F. ) ;
#1653 = EDGE_CURVE ( 'NONE', #132176, #230733, #76236, .T. ) ;
#1655 = AXIS2_PLACEMENT_3D ( 'NONE', #121304, #200804, #23483 ) ;
#1656 = ORIENTED_EDGE ( 'NONE', *, *, #16266, .F. ) ;
#1657 = VERTEX_POINT ( 'NONE', #70031 ) ;
#1658 = EDGE_CURVE ( 'NONE', #80403, #225274, #159467, .T. ) ;
#1659 = DIRECTION ( 'NONE',  ( 0.000000000000000000, 0.2617529984165152257, 0.9651348961777124202 ) ) ;
#1660 = CARTESIAN_POINT ( 'NONE',  ( -18.58693740092131108, 85.40643215026551616, -196.3982910280228111 ) ) ;
#1661 = ORIENTED_EDGE ( 'NONE', *, *, #105338, .F. ) ;
#1662 = DIRECTION ( 'NONE',  ( 1.000000000000000000, 0.000000000000000000, 0.000000000000000000 ) ) ;
#1663 = ADVANCED_FACE ( 'NONE', ( #109114 ), #146954, .F. ) ;
#1664 = SURFACE_SIDE_STYLE ('',( #16137 ) ) ;
#1665 = ORIENTED_EDGE ( 'NONE', *, *, #203874, .F. ) ;
#1666 = EDGE_CURVE ( 'NONE', #136766, #153767, #80300, .T. ) ;
#1668 = ADVANCED_FACE ( 'NONE', ( #191265 ), #92132, .T. ) ;
#1667 = AXIS2_PLACEMENT_3D ( 'NONE', #224564, #87615, #44664 ) ;
#1669 = CYLINDRICAL_SURFACE ( 'NONE', #106167, 0.5000000000000007772 ) ;
#1670 = CIRCLE ( 'NONE', #80777, 0.09999999999999868716 ) ;
#1671 = TOROIDAL_SURFACE ( 'NONE', #18441, 11.90000000000000391, 0.1000000000000000056 ) ;
#1672 = CARTESIAN_POINT ( 'NONE',  ( 23.24999999999999289, 11.40444339177024524, -198.6185779617709670 ) ) ;
#1673 = EDGE_CURVE ( 'NONE', #28383, #222419, #249930, .T. ) ;
#1674 = VERTEX_POINT ( 'NONE', #171707 ) ;
#1675 = EDGE_LOOP ( 'NONE', ( #32442, #157357, #48251, #91290 ) ) ;
#1676 = DIRECTION ( 'NONE',  ( 0.000000000000000000, 0.9770955615653550419, 0.2128009952262526761 ) ) ;
#1677 = ORIENTED_EDGE ( 'NONE', *, *, #116347, .F. ) ;
#1678 = CARTESIAN_POINT ( 'NONE',  ( 23.24999999999999645, 36.65892442174472876, -249.5511627012454596 ) ) ;
#1679 = ORIENTED_EDGE ( 'NONE', *, *, #204174, .F. ) ;
#1681 = ORIENTED_EDGE ( 'NONE', *, *, #32691, .T. ) ;
#1680 = FACE_OUTER_BOUND ( 'NONE', #211007, .T. ) ;
#1682 = EDGE_CURVE ( 'NONE', #64185, #88756, #170443, .T. ) ;
#1683 = ADVANCED_FACE ( 'NONE', ( #8753 ), #89553, .F. ) ;
#1684 = DIRECTION ( 'NONE',  ( 0.000000000000000000, -8.717686153663073805E-15, 1.000000000000000000 ) ) ;
#1685 = ORIENTED_EDGE ( 'NONE', *, *, #121618, .F. ) ;
#1686 = DIRECTION ( 'NONE',  ( 0.000000000000000000, 0.4999999999999413247, -0.8660254037844724584 ) ) ;
#1687 = ORIENTED_EDGE ( 'NONE', *, *, #137543, .F. ) ;
#1689 = VERTEX_POINT ( 'NONE', #90840 ) ;
#1688 = ORIENTED_EDGE ( 'NONE', *, *, #170645, .T. ) ;
#1691 = CARTESIAN_POINT ( 'NONE',  ( 18.59999999999999076, 14.51805813080544638, -219.6885945441820809 ) ) ;
#1690 = AXIS2_PLACEMENT_3D ( 'NONE', #73203, #246661, #92719 ) ;
#1692 = CARTESIAN_POINT ( 'NONE',  ( -20.64999999999999858, 2.000000000011154189, -87.27537807723794572 ) ) ;
#1693 = ORIENTED_EDGE ( 'NONE', *, *, #85923, .T. ) ;
#1694 = CIRCLE ( 'NONE', #255745, 0.2000000000000057288 ) ;
#1695 = CIRCLE ( 'NONE', #26674, 0.5000000000000013323 ) ;
#1696 = AXIS2_PLACEMENT_3D ( 'NONE', #2027, #103687, #241933 ) ;
#1697 = CIRCLE ( 'NONE', #193452, 11.90000000000000213 ) ;
#1698 = ORIENTED_EDGE ( 'NONE', *, *, #98166, .F. ) ;
#1699 = DIRECTION ( 'NONE',  ( 0.000000000000000000, 0.5000000000000004441, 0.8660254037844384856 ) ) ;
#1700 = DIRECTION ( 'NONE',  ( 0.000000000000000000, 0.000000000000000000, -1.000000000000000000 ) ) ;
#1702 = ORIENTED_EDGE ( 'NONE', *, *, #11566, .F. ) ;
#1701 = CARTESIAN_POINT ( 'NONE',  ( 23.14999999999999858, 1.115600667400684642E-11, -138.0000000000000284 ) ) ;
#1703 = CARTESIAN_POINT ( 'NONE',  ( -21.59142135623730852, 68.15000000001259650, -191.2731074845244166 ) ) ;
#1704 = ORIENTED_EDGE ( 'NONE', *, *, #47457, .F. ) ;
#1705 = CARTESIAN_POINT ( 'NONE',  ( 22.39999999999999503, 75.90000000001170122, -75.77310748452431710 ) ) ;
#1706 = DIRECTION ( 'NONE',  ( 0.000000000000000000, 0.000000000000000000, -1.000000000000000000 ) ) ;
#1707 = CIRCLE ( 'NONE', #247410, 0.09999999999998898659 ) ;
#1708 = ORIENTED_EDGE ( 'NONE', *, *, #138001, .F. ) ;
#1709 = AXIS2_PLACEMENT_3D ( 'NONE', #219039, #76967, #142072 ) ;
#1710 = DIRECTION ( 'NONE',  ( 1.000000000000000000, -0.000000000000000000, 0.000000000000000000 ) ) ;
#1711 = DIRECTION ( 'NONE',  ( 0.000000000000000000, 0.000000000000000000, 1.000000000000000000 ) ) ;
#1712 = CARTESIAN_POINT ( 'NONE',  ( 21.14999999999999858, 76.00000000001173817, -81.17267829206912211 ) ) ;
#1713 = CIRCLE ( 'NONE', #93299, 0.09999999999999781286 ) ;
#1714 = VERTEX_POINT ( 'NONE', #189958 ) ;
#1715 = LINE ( 'NONE', #186804, #167998 ) ;
#1716 = ORIENTED_EDGE ( 'NONE', *, *, #59055, .F. ) ;
#1717 = AXIS2_PLACEMENT_3D ( 'NONE', #156925, #76069, #154373 ) ;
#1718 = ORIENTED_EDGE ( 'NONE', *, *, #113383, .T. ) ;
#1720 = ORIENTED_EDGE ( 'NONE', *, *, #76106, .T. ) ;
#1719 = VECTOR ( 'NONE', #30914, 1000.000000000000000 ) ;
#1721 = ORIENTED_EDGE ( 'NONE', *, *, #167214, .T. ) ;
#1722 = CARTESIAN_POINT ( 'NONE',  ( 20.94999999999999929, 76.00000000001244871, -170.0231074845243597 ) ) ;
#1723 = ORIENTED_EDGE ( 'NONE', *, *, #2166, .F. ) ;
#1724 = ORIENTED_EDGE ( 'NONE', *, *, #184061, .F. ) ;
#1725 = DIRECTION ( 'NONE',  ( 0.7071359030027705161, -0.6908824414807910319, -0.1504668293611502450 ) ) ;
#1726 = AXIS2_PLACEMENT_3D ( 'NONE', #171029, #167159, #68024 ) ;
#1727 = CARTESIAN_POINT ( 'NONE',  ( 22.45305468355010703, 76.10085836911248691, -215.2726746080140856 ) ) ;
#1728 = AXIS2_PLACEMENT_3D ( 'NONE', #100004, #115753, #236991 ) ;
#1729 = VERTEX_POINT ( 'NONE', #175549 ) ;
#1730 = ADVANCED_FACE ( 'NONE', ( #97219 ), #221967, .F. ) ;
#1731 = VERTEX_POINT ( 'NONE', #253758 ) ;
#1732 = ADVANCED_FACE ( 'NONE', ( #95967 ), #218051, .T. ) ;
#1733 = ORIENTED_EDGE ( 'NONE', *, *, #62158, .F. ) ;
#1734 = EDGE_CURVE ( 'NONE', #111659, #234461, #34758, .T. ) ;
#1735 = CARTESIAN_POINT ( 'NONE',  ( 21.11833042828125429, 69.55435530615748974, -203.5302079935838151 ) ) ;
#1736 = ADVANCED_FACE ( 'NONE', ( #231663 ), #13887, .T. ) ;
#1737 = DIRECTION ( 'NONE',  ( -1.000000000000000000, -0.000000000000000000, -0.000000000000000000 ) ) ;
#1738 = CARTESIAN_POINT ( 'NONE',  ( -16.81744102076748959, 14.15900158805613884, -219.2550725561364118 ) ) ;
#1739 = CARTESIAN_POINT ( 'NONE',  ( -21.14999999999999858, 1.115600667400684642E-11, -33.50000000000000000 ) ) ;
#1740 = DIRECTION ( 'NONE',  ( 0.000000000000000000, -0.4999999999999478195, -0.8660254037844686836 ) ) ;
#1741 = CARTESIAN_POINT ( 'NONE',  ( 21.05000000000000071, -0.09999999998884338825, -127.4593430482987912 ) ) ;
#1742 = CARTESIAN_POINT ( 'NONE',  ( -17.04761207306819060, 65.97354912661484150, -190.8731074845244109 ) ) ;
#1744 = CARTESIAN_POINT ( 'NONE',  ( 21.11833042828143192, 34.01722704040963663, -243.6717221766632804 ) ) ;
#1743 = DIRECTION ( 'NONE',  ( -1.000000000000000000, 0.000000000000000000, 0.000000000000000000 ) ) ;
#1745 = DIRECTION ( 'NONE',  ( 1.000000000000000000, 0.000000000000000000, 0.000000000000000000 ) ) ;
#1746 = CARTESIAN_POINT ( 'NONE',  ( -16.87683809663752399, 52.34166666667822199, -52.77310748452448763 ) ) ;
#1747 = AXIS2_PLACEMENT_3D ( 'NONE', #232911, #148207, #227739 ) ;
#1748 = DIRECTION ( 'NONE',  ( 0.000000000000000000, 0.2128009952263588966, -0.9770955615653318382 ) ) ;
#1750 = CARTESIAN_POINT ( 'NONE',  ( -23.15000000000000213, -8.999999999988844479, -57.10603087734755690 ) ) ;
#1749 = AXIS2_PLACEMENT_3D ( 'NONE', #28287, #25688, #229029 ) ;
#1751 =( BOUNDED_CURVE ( )  B_SPLINE_CURVE ( 3, ( #102851, #178596, #160316, #198125 ),
 .UNSPECIFIED., .F., .T. ) 
 B_SPLINE_CURVE_WITH_KNOTS ( ( 4, 4 ),
 ( 1.570796326794904108, 3.141592653589698969 ),
 .UNSPECIFIED. ) 
 CURVE ( )  GEOMETRIC_REPRESENTATION_ITEM ( )  RATIONAL_B_SPLINE_CURVE ( ( 1.000000000000000000, 0.8047378541243889183, 0.8047378541243889183, 1.000000000000000000 ) ) 
 REPRESENTATION_ITEM ( '' )  );
#1752 = ORIENTED_EDGE ( 'NONE', *, *, #166734, .T. ) ;
#1753 = EDGE_CURVE ( 'NONE', #216962, #117682, #84575, .T. ) ;
#1754 = EDGE_CURVE ( 'NONE', #185637, #6907, #16291, .T. ) ;
#1755 = TOROIDAL_SURFACE ( 'NONE', #214163, 0.4000000000000009104, 0.1000000000000000056 ) ;
#1756 = AXIS2_PLACEMENT_3D ( 'NONE', #224993, #141630, #165050 ) ;
#1758 = ORIENTED_EDGE ( 'NONE', *, *, #83281, .T. ) ;
#1757 = LINE ( 'NONE', #203820, #24029 ) ;
#1759 = DIRECTION ( 'NONE',  ( 0.000000000000000000, 0.000000000000000000, -1.000000000000000000 ) ) ;
#1760 = DIRECTION ( 'NONE',  ( -1.000000000000000000, 0.000000000000000000, 0.000000000000000000 ) ) ;
#1761 = AXIS2_PLACEMENT_3D ( 'NONE', #217075, #1877, #162281 ) ;
#1762 = FACE_OUTER_BOUND ( 'NONE', #190353, .T. ) ;
#1763 = ORIENTED_EDGE ( 'NONE', *, *, #132664, .T. ) ;
#1764 = AXIS2_PLACEMENT_3D ( 'NONE', #228855, #129746, #163748 ) ;
#1765 = AXIS2_PLACEMENT_3D ( 'NONE', #100012, #208153, #186003 ) ;
#1766 = ADVANCED_FACE ( 'NONE', ( #197641 ), #77681, .F. ) ;
#1767 = DIRECTION ( 'NONE',  ( 0.000000000000000000, 0.2617529984165031243, 0.9651348961777157509 ) ) ;
#1768 = AXIS2_PLACEMENT_3D ( 'NONE', #114364, #193911, #170543 ) ;
#1769 = EDGE_CURVE ( 'NONE', #179303, #61312, #15179, .T. ) ;
#1770 = DIRECTION ( 'NONE',  ( 0.000000000000000000, 0.000000000000000000, -1.000000000000000000 ) ) ;
#1771 = ORIENTED_EDGE ( 'NONE', *, *, #204835, .F. ) ;
#1772 = AXIS2_PLACEMENT_3D ( 'NONE', #171722, #253772, #95982 ) ;
#1773 = CARTESIAN_POINT ( 'NONE',  ( -18.55121869061588669, 10.32747123227773045, -206.5774032850249000 ) ) ;
#1774 = LINE ( 'NONE', #179174, #234436 ) ;
#1775 = DIRECTION ( 'NONE',  ( 1.000000000000000000, 0.000000000000000000, 0.000000000000000000 ) ) ;
#1777 = ORIENTED_EDGE ( 'NONE', *, *, #186905, .F. ) ;
#1776 = CARTESIAN_POINT ( 'NONE',  ( -23.15000000000000213, 6.300962096140152013, -220.8843452229073705 ) ) ;
#1778 = ADVANCED_FACE ( 'NONE', ( #195115 ), #16473, .T. ) ;
#1780 = ORIENTED_EDGE ( 'NONE', *, *, #72524, .T. ) ;
#1779 = CARTESIAN_POINT ( 'NONE',  ( 21.05000000000000071, 40.72908339264471067, -238.0561209609712705 ) ) ;
#1781 = DIRECTION ( 'NONE',  ( 0.000000000000000000, 0.9333616406058473647, 0.3589373870824282275 ) ) ;
#1782 = CARTESIAN_POINT ( 'NONE',  ( -18.50000000000000000, 52.17883100310857003, -232.4626431718731396 ) ) ;
#1783 = EDGE_CURVE ( 'NONE', #88936, #209005, #230361, .T. ) ;
#1784 = CARTESIAN_POINT ( 'NONE',  ( 20.94999999999999574, 68.17695920783671681, -227.9262201573640141 ) ) ;
#1785 = CIRCLE ( 'NONE', #147559, 0.09999999999999939493 ) ;
#1787 = CARTESIAN_POINT ( 'NONE',  ( 23.14999999999999858, 1.115600667400684642E-11, -100.5000000000000426 ) ) ;
#1786 = CARTESIAN_POINT ( 'NONE',  ( -20.54999999999999716, 71.65000000001259650, -191.1731074845243654 ) ) ;
#1788 = CARTESIAN_POINT ( 'NONE',  ( -21.05000000000000782, 34.10431353847246072, -243.7569376156651515 ) ) ;
#1790 = EDGE_CURVE ( 'NONE', #60110, #211620, #42940, .T. ) ;
#1789 = CARTESIAN_POINT ( 'NONE',  ( -18.51697539158856998, 10.31565961586830227, -39.03641941191784070 ) ) ;
#1791 = DIRECTION ( 'NONE',  ( 0.000000000000000000, 0.8660254037844420383, -0.4999999999999943379 ) ) ;
#1792 = LINE ( 'NONE', #116623, #180804 ) ;
#1793 = AXIS2_PLACEMENT_3D ( 'NONE', #96958, #176557, #156997 ) ;
#1795 = ORIENTED_EDGE ( 'NONE', *, *, #173721, .T. ) ;
#1794 = AXIS2_PLACEMENT_3D ( 'NONE', #171098, #206329, #165938 ) ;
#1796 = DIRECTION ( 'NONE',  ( 0.000000000000000000, 0.000000000000000000, -1.000000000000000000 ) ) ;
#1797 = CIRCLE ( 'NONE', #243412, 0.1000000000000002554 ) ;
#1798 = VERTEX_POINT ( 'NONE', #64553 ) ;
#1799 = EDGE_LOOP ( 'NONE', ( #72271, #44085, #66351, #123931 ) ) ;
#1800 = DIRECTION ( 'NONE',  ( 1.000000000000000000, 0.000000000000000000, 0.000000000000000000 ) ) ;
#1801 = CARTESIAN_POINT ( 'NONE',  ( -23.25000000000000000, 74.08971962618045382, -149.1544753397233194 ) ) ;
#1802 = ORIENTED_EDGE ( 'NONE', *, *, #250928, .T. ) ;
#1803 = EDGE_CURVE ( 'NONE', #177022, #204435, #138747, .T. ) ;
#1804 = SHAPE_REPRESENTATION ( 'Snap Open Cable Crossbars 8', ( #2425 ), #56573 ) ;
#1805 = VERTEX_POINT ( 'NONE', #42428 ) ;
#1806 = ADVANCED_FACE ( 'NONE', ( #218474 ), #129726, .T. ) ;
#1807 = ORIENTED_EDGE ( 'NONE', *, *, #101523, .T. ) ;
#1808 = DIRECTION ( 'NONE',  ( 1.836970198721029934E-16, 1.000000000000000000, 6.982962677686266711E-15 ) ) ;
#1809 = AXIS2_PLACEMENT_3D ( 'NONE', #153171, #240376, #125555 ) ;
#1810 = ORIENTED_EDGE ( 'NONE', *, *, #7566, .F. ) ;
#1811 = CARTESIAN_POINT ( 'NONE',  ( -16.87036670365549895, 9.989418819312803066, -180.0204398826979286 ) ) ;
#1812 = DIRECTION ( 'NONE',  ( 0.000000000000000000, -0.9654727137038715545, 0.2605042016806676242 ) ) ;
#1813 = DIRECTION ( 'NONE',  ( 0.000000000000000000, 0.000000000000000000, -1.000000000000000000 ) ) ;
#1814 = CARTESIAN_POINT ( 'NONE',  ( -21.05000000000000071, 10.71906255309368383, -222.4921384173655383 ) ) ;
#1815 = CARTESIAN_POINT ( 'NONE',  ( -18.59999999999999787, 11.75000000001115197, -122.2500000000000284 ) ) ;
#1816 = AXIS2_PLACEMENT_3D ( 'NONE', #183721, #5041, #10225 ) ;
#1817 = CYLINDRICAL_SURFACE ( 'NONE', #87465, 0.1000000000000028644 ) ;
#1818 = DIRECTION ( 'NONE',  ( 1.000000000000000000, 0.000000000000000000, 0.000000000000000000 ) ) ;
#1820 = VERTEX_POINT ( 'NONE', #104926 ) ;
#1819 = DIRECTION ( 'NONE',  ( 1.000000000000000000, 0.000000000000000000, 0.000000000000000000 ) ) ;
#1822 = DIRECTION ( 'NONE',  ( -1.000000000000000000, 0.000000000000000000, 0.000000000000000000 ) ) ;
#1821 = CARTESIAN_POINT ( 'NONE',  ( 21.97500000000000497, 9.750000000011153745, -155.1500000000000057 ) ) ;
#1823 = CARTESIAN_POINT ( 'NONE',  ( 21.05000000000000071, 11.60000000000000675, -26.57179676972450011 ) ) ;
#1824 = ORIENTED_EDGE ( 'NONE', *, *, #118042, .T. ) ;
#1825 = CARTESIAN_POINT ( 'NONE',  ( 20.94999999999999929, 84.66355140188167638, -179.5472086025916099 ) ) ;
#1826 = FILL_AREA_STYLE ('',( #224731 ) ) ;
#1827 = VERTEX_POINT ( 'NONE', #123248 ) ;
#1829 = LINE ( 'NONE', #244301, #75036 ) ;
#1828 = CARTESIAN_POINT ( 'NONE',  ( 21.05000000000000071, 65.57661458509942065, -162.5310555606543232 ) ) ;
#1830 = CARTESIAN_POINT ( 'NONE',  ( 20.94999999999999929, 1.115600667400684642E-11, -135.9000000000000625 ) ) ;
#1831 = ORIENTED_EDGE ( 'NONE', *, *, #22736, .F. ) ;
#1832 = AXIS2_PLACEMENT_3D ( 'NONE', #135364, #212370, #33764 ) ;
#1833 = CARTESIAN_POINT ( 'NONE',  ( 18.49999999999999645, -1.164121893230052995, -74.91484808557160591 ) ) ;
#1834 = CARTESIAN_POINT ( 'NONE',  ( -22.50000000000088463, 0.04536165659890484952, -21.84949116579043604 ) ) ;
#1835 = DIRECTION ( 'NONE',  ( 2.952720810173289112E-16, -1.000000000000000000, -0.000000000000000000 ) ) ;
#1836 = ORIENTED_EDGE ( 'NONE', *, *, #22910, .F. ) ;
#1837 = CARTESIAN_POINT ( 'NONE',  ( -17.01764560440408047, 66.05000000001255955, -182.7731074837355436 ) ) ;
#1838 = FACE_OUTER_BOUND ( 'NONE', #225196, .T. ) ;
#1839 = CARTESIAN_POINT ( 'NONE',  ( 20.94999999999999929, 76.00000000001126921, -203.5231074845248997 ) ) ;
#1840 = CIRCLE ( 'NONE', #255900, 0.09999999999999939493 ) ;
#1841 = DIRECTION ( 'NONE',  ( -0.000000000000000000, -1.000000000000000000, -8.609265936414532828E-15 ) ) ;
#1842 = AXIS2_PLACEMENT_3D ( 'NONE', #100695, #94617, #171631 ) ;
#1843 = CARTESIAN_POINT ( 'NONE',  ( -6.000000000000003553, -11.65000000000000036, 10.00000000000000178 ) ) ;
#1844 = CIRCLE ( 'NONE', #147615, 0.09999999999998898659 ) ;
#1845 = AXIS2_PLACEMENT_3D ( 'NONE', #174388, #171808, #248747 ) ;
#1847 = VERTEX_POINT ( 'NONE', #201490 ) ;
#1846 = CARTESIAN_POINT ( 'NONE',  ( 21.06600267594171783, 8.775166069211060460, -179.7042627823747125 ) ) ;
#1848 = LINE ( 'NONE', #43576, #118337 ) ;
#1849 = FACE_OUTER_BOUND ( 'NONE', #29017, .T. ) ;
#1850 = CARTESIAN_POINT ( 'NONE',  ( -23.15000000000000213, 11.65000000001115588, -179.6499999999999773 ) ) ;
#1852 = SPHERICAL_SURFACE ( 'NONE', #180446, 0.1000000000000000056 ) ;
#1851 = STYLED_ITEM ( 'NONE', ( #65603 ), #63721 ) ;
#1853 = EDGE_CURVE ( 'NONE', #237782, #214060, #30480, .T. ) ;
#1854 = PLANE ( 'NONE',  #71495 ) ;
#1856 = ORIENTED_EDGE ( 'NONE', *, *, #244760, .T. ) ;
#1855 = CYLINDRICAL_SURFACE ( 'NONE', #177529, 0.1000000000000001443 ) ;
#1857 = DIRECTION ( 'NONE',  ( -1.000000000000000000, -0.000000000000000000, -0.000000000000000000 ) ) ;
#1858 = CARTESIAN_POINT ( 'NONE',  ( -16.97092634996758775, 63.04181532628136608, -213.0951363382118018 ) ) ;
#1859 = DIRECTION ( 'NONE',  ( 0.000000000000000000, -0.2128009952263403282, 0.9770955615653358350 ) ) ;
#1860 = ORIENTED_EDGE ( 'NONE', *, *, #103698, .T. ) ;
#1861 = CARTESIAN_POINT ( 'NONE',  ( -23.25000000000000000, 1.115600667400684642E-11, -200.9999999999999432 ) ) ;
#1862 = EDGE_CURVE ( 'NONE', #182190, #197418, #184379, .T. ) ;
#1863 = EDGE_CURVE ( 'NONE', #84975, #128539, #78956, .T. ) ;
#1864 = CARTESIAN_POINT ( 'NONE',  ( -18.59999999999999787, -1.249999999988843369, -75.00000000000004263 ) ) ;
#1865 = CARTESIAN_POINT ( 'NONE',  ( -18.40000000000000924, 78.23216008268646249, -231.5864513804630178 ) ) ;
#1866 = VECTOR ( 'NONE', #230453, 1000.000000000000000 ) ;
#1867 = DIRECTION ( 'NONE',  ( 1.000000000000000000, 0.000000000000000000, 0.000000000000000000 ) ) ;
#1869 = ORIENTED_EDGE ( 'NONE', *, *, #233397, .T. ) ;
#1868 = CIRCLE ( 'NONE', #135143, 3.899999999999999467 ) ;
#1870 = ORIENTED_EDGE ( 'NONE', *, *, #1459, .F. ) ;
#1871 = CIRCLE ( 'NONE', #14577, 4.049999999999998046 ) ;
#1872 = CARTESIAN_POINT ( 'NONE',  ( -21.64999999999999858, 10.05000000001113847, -54.25000000000000711 ) ) ;
#1874 = CARTESIAN_POINT ( 'NONE',  ( -21.08479644141222664, 34.01140125657141766, -243.7845722631506646 ) ) ;
#1873 = CIRCLE ( 'NONE', #172642, 7.800000000000001599 ) ;
#1875 = EDGE_CURVE ( 'NONE', #220791, #75515, #120709, .T. ) ;
#1876 = CARTESIAN_POINT ( 'NONE',  ( -18.50000000000000000, -4.375386779258390924, -188.8379487402709742 ) ) ;
#1877 = DIRECTION ( 'NONE',  ( -1.000000000000000000, -0.000000000000000000, 0.000000000000000000 ) ) ;
#1878 = ORIENTED_EDGE ( 'NONE', *, *, #194972, .T. ) ;
#1879 = CARTESIAN_POINT ( 'NONE',  ( -23.15000000000000213, 11.75000000001115552, -63.89999999999999858 ) ) ;
#1880 = AXIS2_PLACEMENT_3D ( 'NONE', #236031, #155251, #232209 ) ;
#1881 = CIRCLE ( 'NONE', #139248, 11.74999999999999645 ) ;
#1882 = AXIS2_PLACEMENT_3D ( 'NONE', #230618, #135336, #213596 ) ;
#1883 = CARTESIAN_POINT ( 'NONE',  ( 20.51284917709620359, 11.70743148473744988, -206.3025725608655421 ) ) ;
#1884 = AXIS2_PLACEMENT_3D ( 'NONE', #26679, #106170, #245708 ) ;
#1885 = LINE ( 'NONE', #158448, #203915 ) ;
#1886 = CARTESIAN_POINT ( 'NONE',  ( 20.95556889135987788, 10.62194358774625336, -108.1423942218575434 ) ) ;
#1887 = AXIS2_PLACEMENT_3D ( 'NONE', #55717, #36223, #236970 ) ;
#1888 = DIRECTION ( 'NONE',  ( -1.000000000000000000, -0.000000000000000000, 0.000000000000000000 ) ) ;
#1889 = ORIENTED_EDGE ( 'NONE', *, *, #90325, .F. ) ;
#1891 = ORIENTED_EDGE ( 'NONE', *, *, #139422, .T. ) ;
#1890 = CARTESIAN_POINT ( 'NONE',  ( -23.15000000000000213, 74.00000000001180922, -82.74772940728641402 ) ) ;
#1892 = CIRCLE ( 'NONE', #81008, 0.4999999999999944489 ) ;
#1893 = ORIENTED_EDGE ( 'NONE', *, *, #250623, .T. ) ;
#1894 = DIRECTION ( 'NONE',  ( -0.000000000000000000, 0.1298341882520054891, 0.9915357197604850459 ) ) ;
#1895 = ORIENTED_EDGE ( 'NONE', *, *, #207763, .F. ) ;
#1896 = EDGE_CURVE ( 'NONE', #52627, #85480, #251193, .T. ) ;
#1897 = LINE ( 'NONE', #98400, #254811 ) ;
#1898 = CARTESIAN_POINT ( 'NONE',  ( -21.04999999999999716, 6.300179817925787518, -100.4485171181182039 ) ) ;
#1899 = ADVANCED_FACE ( 'NONE', ( #67126 ), #109557, .T. ) ;
#1900 = CYLINDRICAL_SURFACE ( 'NONE', #133191, 0.1000000000000028644 ) ;
#1901 = VERTEX_POINT ( 'NONE', #150527 ) ;
#1903 = AXIS2_PLACEMENT_3D ( 'NONE', #254078, #75484, #96279 ) ;
#1902 = CARTESIAN_POINT ( 'NONE',  ( 20.94999999999999574, 67.07338541492499928, -128.0514244653012383 ) ) ;
#1904 = DIRECTION ( 'NONE',  ( 0.000000000000000000, 0.000000000000000000, -1.000000000000000000 ) ) ;
#1905 = TOROIDAL_SURFACE ( 'NONE', #255779, 0.2000000000000000111, 0.1000000000000000056 ) ;
#1906 = ORIENTED_EDGE ( 'NONE', *, *, #23559, .F. ) ;
#1907 = CARTESIAN_POINT ( 'NONE',  ( -23.25000000000000000, 71.65000000001259650, -191.1731074845243654 ) ) ;
#1909 = ORIENTED_EDGE ( 'NONE', *, *, #95376, .F. ) ;
#1908 = DIRECTION ( 'NONE',  ( -1.000000000000000000, 0.000000000000000000, 0.000000000000000000 ) ) ;
#1910 = FACE_OUTER_BOUND ( 'NONE', #11950, .T. ) ;
#1912 = ADVANCED_FACE ( 'NONE', ( #228786 ), #185790, .F. ) ;
#1911 = DIRECTION ( 'NONE',  ( 0.000000000000000000, -1.000000000000000000, -6.982962677686265922E-15 ) ) ;
#1913 = ORIENTED_EDGE ( 'NONE', *, *, #102055, .F. ) ;
#1914 = CARTESIAN_POINT ( 'NONE',  ( 20.95512820512820440, 65.37615131630072085, -191.3229454651000481 ) ) ;
#1915 = CARTESIAN_POINT ( 'NONE',  ( -22.39999999999999858, 11.75000000001115552, -100.6000000000000369 ) ) ;
#1916 = DIRECTION ( 'NONE',  ( 0.000000000000000000, 0.000000000000000000, -1.000000000000000000 ) ) ;
#1917 = EDGE_LOOP ( 'NONE', ( #93620, #204400, #64244, #37138, #52393, #59076 ) ) ;
#1918 = DIRECTION ( 'NONE',  ( -0.000000000000000000, 0.8814952561688430555, -0.4721928772777346239 ) ) ;
#1919 = CARTESIAN_POINT ( 'NONE',  ( 12.42718393586866021, 48.82205200898362563, -233.8342296612539997 ) ) ;
#1920 = FACE_OUTER_BOUND ( 'NONE', #225522, .T. ) ;
#1921 = ADVANCED_FACE ( 'NONE', ( #168844 ), #207948, .T. ) ;
#1922 = CIRCLE ( 'NONE', #18693, 4.900000000000003020 ) ;
#1923 = ORIENTED_EDGE ( 'NONE', *, *, #127687, .F. ) ;
#1924 = TOROIDAL_SURFACE ( 'NONE', #35315, 0.2000000000000000111, 0.1000000000000000056 ) ;
#1925 = AXIS2_PLACEMENT_3D ( 'NONE', #240575, #78902, #99751 ) ;
#1926 = VERTEX_POINT ( 'NONE', #147952 ) ;
#1927 = VECTOR ( 'NONE', #206610, 1000.000000000000000 ) ;
#1928 = EDGE_CURVE ( 'NONE', #155405, #122855, #1216, .T. ) ;
#1929 = VECTOR ( 'NONE', #139704, 1000.000000000000000 ) ;
#1930 = EDGE_CURVE ( 'NONE', #157880, #236445, #248331, .T. ) ;
#1931 = ORIENTED_EDGE ( 'NONE', *, *, #44090, .T. ) ;
#1932 = CARTESIAN_POINT ( 'NONE',  ( 18.50000972452444969, 10.29326151434227121, -38.95928225104144360 ) ) ;
#1933 = DIRECTION ( 'NONE',  ( 0.000000000000000000, -6.982962677686266711E-15, 1.000000000000000000 ) ) ;
#1935 = ORIENTED_EDGE ( 'NONE', *, *, #53136, .T. ) ;
#1934 = CARTESIAN_POINT ( 'NONE',  ( 18.59999999999999787, -1.835859311443637010, -45.00443916879852679 ) ) ;
#1936 = CARTESIAN_POINT ( 'NONE',  ( 21.05315837450969596, 11.75000000001116085, -127.1583560044167029 ) ) ;
#1937 = DIRECTION ( 'NONE',  ( 0.000000000000000000, -0.5000000000000275335, -0.8660254037844228314 ) ) ;
#1938 = EDGE_CURVE ( 'NONE', #192475, #210448, #69715, .T. ) ;
#1940 = ADVANCED_FACE ( 'NONE', ( #127099 ), #187100, .F. ) ;
#1939 = FACE_BOUND ( 'NONE', #159620, .T. ) ;
#1941 = DIRECTION ( 'NONE',  ( -1.000000000000000000, -2.952720810173289112E-16, 0.000000000000000000 ) ) ;
#1942 = CARTESIAN_POINT ( 'NONE',  ( -18.50000000000001066, 85.41920341803874805, -129.2753216740955509 ) ) ;
#1943 = VECTOR ( 'NONE', #227255, 1000.000000000000000 ) ;
#1944 = LINE ( 'NONE', #161050, #230414 ) ;
#1945 = CIRCLE ( 'NONE', #113834, 0.9750000000000036415 ) ;
#1947 = ORIENTED_EDGE ( 'NONE', *, *, #71541, .T. ) ;
#1946 = CARTESIAN_POINT ( 'NONE',  ( 21.05000000000000071, 76.00000000001267608, -203.5231074845243597 ) ) ;
#1949 = ORIENTED_EDGE ( 'NONE', *, *, #196865, .F. ) ;
#1948 = CYLINDRICAL_SURFACE ( 'NONE', #15214, 0.1000000000000046685 ) ;
#1950 = AXIS2_PLACEMENT_3D ( 'NONE', #25247, #61782, #125604 ) ;
#1951 = ORIENTED_EDGE ( 'NONE', *, *, #237695, .T. ) ;
#1952 = ORIENTED_EDGE ( 'NONE', *, *, #205499, .F. ) ;
#1953 = CARTESIAN_POINT ( 'NONE',  ( 21.05000000000000071, 7.128833340094563376, -233.7327013124401276 ) ) ;
#1954 = CARTESIAN_POINT ( 'NONE',  ( -18.59999999999999787, 11.75000000001115197, -121.8500000000000369 ) ) ;
#1955 = ADVANCED_FACE ( 'NONE', ( #65835 ), #8446, .F. ) ;
#1956 = EDGE_CURVE ( 'NONE', #221156, #137732, #149255, .T. ) ;
#1957 = DIRECTION ( 'NONE',  ( 0.000000000000000000, 0.4999999999999088507, -0.8660254037844913322 ) ) ;
#1958 = DIRECTION ( 'NONE',  ( -3.469446951953614189E-14, 0.000000000000000000, 1.000000000000000000 ) ) ;
#1960 = EDGE_CURVE ( 'NONE', #37312, #186227, #89247, .T. ) ;
#1959 = AXIS2_PLACEMENT_3D ( 'NONE', #29194, #149112, #90393 ) ;
#1961 = CARTESIAN_POINT ( 'NONE',  ( 20.52683494730046476, 67.01946918171127265, -195.0178547619902076 ) ) ;
#1962 = CARTESIAN_POINT ( 'NONE',  ( 20.95429402530587737, 10.48661124036732240, -207.4390072342162910 ) ) ;
#1963 = AXIS2_PLACEMENT_3D ( 'NONE', #187153, #72336, #107582 ) ;
#1965 = ORIENTED_EDGE ( 'NONE', *, *, #65276, .T. ) ;
#1964 = EDGE_CURVE ( 'NONE', #195562, #196915, #50122, .T. ) ;
#1966 = ORIENTED_EDGE ( 'NONE', *, *, #252403, .T. ) ;
#1967 = ORIENTED_EDGE ( 'NONE', *, *, #232485, .F. ) ;
#1968 = EDGE_CURVE ( 'NONE', #143912, #15448, #101125, .T. ) ;
#1969 = DIRECTION ( 'NONE',  ( 0.000000000000000000, -0.008583690987162452199, -0.9999631594459053030 ) ) ;
#1970 = EDGE_CURVE ( 'NONE', #257729, #70270, #134489, .T. ) ;
#1972 = CIRCLE ( 'NONE', #147752, 0.4999999999999944489 ) ;
#1971 = FACE_OUTER_BOUND ( 'NONE', #116172, .T. ) ;
#1973 = CIRCLE ( 'NONE', #35361, 0.09999999999999939493 ) ;
#1974 = CARTESIAN_POINT ( 'NONE',  ( 21.53752568622141439, 75.90102553874177715, -176.8099153590729884 ) ) ;
#1975 = CIRCLE ( 'NONE', #47763, 7.800000000000001599 ) ;
#1976 = CARTESIAN_POINT ( 'NONE',  ( 20.09999999999999787, 9.750000000011137757, -109.7500000000000426 ) ) ;
#1977 = ADVANCED_FACE ( 'NONE', ( #106229 ), #130955, .F. ) ;
#1978 = ORIENTED_EDGE ( 'NONE', *, *, #138333, .F. ) ;
#1979 = CARTESIAN_POINT ( 'NONE',  ( -16.93262454970419384, 65.99797953208187096, -149.0960312582870984 ) ) ;
#1980 = ORIENTED_EDGE ( 'NONE', *, *, #49123, .T. ) ;
#1981 = CYLINDRICAL_SURFACE ( 'NONE', #179592, 11.75000000000001066 ) ;
#1982 = ORIENTED_EDGE ( 'NONE', *, *, #257181, .F. ) ;
#1983 = EDGE_CURVE ( 'NONE', #206700, #26858, #206638, .T. ) ;
#1984 = DIRECTION ( 'NONE',  ( 0.000000000000000000, 0.000000000000000000, -1.000000000000000000 ) ) ;
#1985 = EDGE_CURVE ( 'NONE', #54629, #150801, #167541, .T. ) ;
#1986 = DIRECTION ( 'NONE',  ( 0.000000000000000000, -1.000000000000000000, -6.982962677686265922E-15 ) ) ;
#1988 = ORIENTED_EDGE ( 'NONE', *, *, #170106, .F. ) ;
#1987 = ADVANCED_FACE ( 'NONE', ( #31882 ), #172701, .T. ) ;
#1989 = CARTESIAN_POINT ( 'NONE',  ( -20.54999999999999716, 1.115600667400684642E-11, -67.00000000000000000 ) ) ;
#1991 = VERTEX_POINT ( 'NONE', #196074 ) ;
#1990 = CARTESIAN_POINT ( 'NONE',  ( -20.64999999999999858, 85.50000000001207923, -126.6291383618717816 ) ) ;
#1992 = CARTESIAN_POINT ( 'NONE',  ( -20.99749315643149217, 64.25000000001148237, -43.03791325328343476 ) ) ;
#1993 = AXIS2_PLACEMENT_3D ( 'NONE', #142244, #183945, #61432 ) ;
#1994 = EDGE_LOOP ( 'NONE', ( #202796, #207521, #200932, #192769 ) ) ;
#1995 = CIRCLE ( 'NONE', #68659, 0.09999999999998898659 ) ;
#1996 = FACE_OUTER_BOUND ( 'NONE', #62739, .T. ) ;
#1997 = ORIENTED_EDGE ( 'NONE', *, *, #246276, .F. ) ;
#1998 = EDGE_CURVE ( 'NONE', #121258, #56183, #59641, .T. ) ;
#1999 = DIRECTION ( 'NONE',  ( 0.000000000000000000, -1.000000000000000000, 0.000000000000000000 ) ) ;
#2000 = CARTESIAN_POINT ( 'NONE',  ( 19.96984138294296329, 64.25000000001250555, -178.7985354133239753 ) ) ;
#2001 = CYLINDRICAL_SURFACE ( 'NONE', #44834, 0.1000000000000000611 ) ;
#2002 = DIRECTION ( 'NONE',  ( 0.000000000000000000, -0.9908441862701791170, 0.1350103645450472789 ) ) ;
#2003 = CARTESIAN_POINT ( 'NONE',  ( -23.49999999999994316, 64.35000000001120668, -29.92310748452479174 ) ) ;
#2004 = VERTEX_POINT ( 'NONE', #113950 ) ;
#2005 = DIRECTION ( 'NONE',  ( 1.000000000000000000, 0.000000000000000000, 0.000000000000000000 ) ) ;
#2006 = DIRECTION ( 'NONE',  ( -1.836970198721029934E-16, -1.000000000000000000, -6.982962677686266711E-15 ) ) ;
#2007 = PLANE ( 'NONE',  #146979 ) ;
#2008 = VERTEX_POINT ( 'NONE', #231357 ) ;
#2009 = CARTESIAN_POINT ( 'NONE',  ( -21.05000000000000071, 76.02110330807114735, -109.3276238137883354 ) ) ;
#2010 = ORIENTED_EDGE ( 'NONE', *, *, #13983, .T. ) ;
#2011 = DIRECTION ( 'NONE',  ( -1.000000000000000000, -0.000000000000000000, 0.000000000000000000 ) ) ;
#2012 = ORIENTED_EDGE ( 'NONE', *, *, #116816, .T. ) ;
#2013 = AXIS2_PLACEMENT_3D ( 'NONE', #234226, #54301, #34786 ) ;
#2014 = AXIS2_PLACEMENT_3D ( 'NONE', #80731, #238540, #218968 ) ;
#2015 = CARTESIAN_POINT ( 'NONE',  ( -23.15000000000000213, 59.16775194334852728, -221.0793150863668473 ) ) ;
#2016 = CARTESIAN_POINT ( 'NONE',  ( -20.93975676684922504, 10.31104185824063180, -72.52045169831058047 ) ) ;
#2017 = ORIENTED_EDGE ( 'NONE', *, *, #164449, .T. ) ;
#2019 = ORIENTED_EDGE ( 'NONE', *, *, #17909, .T. ) ;
#2018 = FACE_OUTER_BOUND ( 'NONE', #178784, .T. ) ;
#2020 = CARTESIAN_POINT ( 'NONE',  ( 21.05000000000000071, 76.00000000001170974, -69.52310748452431710 ) ) ;
#2021 = ORIENTED_EDGE ( 'NONE', *, *, #250072, .F. ) ;
#2022 = CARTESIAN_POINT ( 'NONE',  ( -20.94999999999999929, -12.41227409413852811, -197.9999999999999432 ) ) ;
#2023 = DIRECTION ( 'NONE',  ( -0.000000000000000000, 1.000000000000000000, -0.000000000000000000 ) ) ;
#2024 = VERTEX_POINT ( 'NONE', #17423 ) ;
#2025 = ORIENTED_EDGE ( 'NONE', *, *, #124889, .F. ) ;
#2026 = EDGE_CURVE ( 'NONE', #49183, #47477, #35737, .T. ) ;
#2027 = CARTESIAN_POINT ( 'NONE',  ( 20.04999999999999716, 8.750000000011173285, -143.2500000000000284 ) ) ;
#2028 = FACE_OUTER_BOUND ( 'NONE', #209242, .T. ) ;
#2030 = DIRECTION ( 'NONE',  ( -0.000000000000000000, 0.000000000000000000, 1.000000000000000000 ) ) ;
#2029 = AXIS2_PLACEMENT_3D ( 'NONE', #26764, #47564, #67147 ) ;
#2031 = EDGE_CURVE ( 'NONE', #227184, #229125, #238749, .T. ) ;
#2032 = AXIS2_PLACEMENT_3D ( 'NONE', #32480, #72887, #152417 ) ;
#2033 = EDGE_LOOP ( 'NONE', ( #233919, #3187, #70039, #165221 ) ) ;
#2034 = ORIENTED_EDGE ( 'NONE', *, *, #224184, .F. ) ;
#2035 = CIRCLE ( 'NONE', #168706, 0.1000000000000043771 ) ;
#2036 = AXIS2_PLACEMENT_3D ( 'NONE', #33109, #70936, #89171 ) ;
#2037 = DIRECTION ( 'NONE',  ( 1.000000000000000000, -0.000000000000000000, -0.000000000000000000 ) ) ;
#2038 = COLOUR_RGB ( '', 0.72549020, 0.75294118, 0.79215686) ;
#2039 = EDGE_CURVE ( 'NONE', #83610, #99200, #209715, .T. ) ;
#2040 = EDGE_CURVE ( 'NONE', #95482, #64016, #240281, .T. ) ;
#2042 = ORIENTED_EDGE ( 'NONE', *, *, #74139, .F. ) ;
#2041 = CARTESIAN_POINT ( 'NONE',  ( -16.87372386987899020, 9.880600233647912845, -46.64926987186640162 ) ) ;
#2043 = DIRECTION ( 'NONE',  ( 1.000000000000000000, -1.186688945009010077E-16, -8.286604613020808509E-31 ) ) ;
#2044 = CARTESIAN_POINT ( 'NONE',  ( 20.94999999999999929, 14.05000000001115623, -61.48630492923908974 ) ) ;
#2045 = CARTESIAN_POINT ( 'NONE',  ( -16.79140778683509438, 63.08531055272182186, -213.1485019413766508 ) ) ;
#2047 = DIRECTION ( 'NONE',  ( 0.000000000000000000, -0.8814952561688476074, 0.4721928772777262417 ) ) ;
#2046 = CARTESIAN_POINT ( 'NONE',  ( -16.91256925476571382, 66.01426884188386168, -123.9907499735296454 ) ) ;
#2048 = CARTESIAN_POINT ( 'NONE',  ( -21.05000000000000071, 76.10000000001220144, -143.0637644362255401 ) ) ;
#2049 = CYLINDRICAL_SURFACE ( 'NONE', #165163, 0.09999999999999976963 ) ;
#2050 = CARTESIAN_POINT ( 'NONE',  ( -0.8999999999999994671, -8.350000000000003197, 21.95857864376269220 ) ) ;
#2051 = DIRECTION ( 'NONE',  ( 0.000000000000000000, 0.000000000000000000, -1.000000000000000000 ) ) ;
#2052 = AXIS2_PLACEMENT_3D ( 'NONE', #79603, #220433, #200858 ) ;
#2053 = ORIENTED_EDGE ( 'NONE', *, *, #23400, .T. ) ;
#2054 = AXIS2_PLACEMENT_3D ( 'NONE', #62377, #203158, #164046 ) ;
#2055 = AXIS2_PLACEMENT_3D ( 'NONE', #151383, #191803, #135636 ) ;
#2056 = ORIENTED_EDGE ( 'NONE', *, *, #230473, .T. ) ;
#2057 = DIRECTION ( 'NONE',  ( 0.000000000000000000, 0.000000000000000000, 1.000000000000000000 ) ) ;
#2058 = ORIENTED_EDGE ( 'NONE', *, *, #174890, .F. ) ;
#2059 = CARTESIAN_POINT ( 'NONE',  ( -20.94999999999999929, 64.35000000001176090, -76.30697314750248950 ) ) ;
#2060 = AXIS2_PLACEMENT_3D ( 'NONE', #76641, #152367, #231897 ) ;
#2061 = AXIS2_PLACEMENT_3D ( 'NONE', #88179, #246008, #206879 ) ;
#2062 = ORIENTED_EDGE ( 'NONE', *, *, #106889, .T. ) ;
#2063 = AXIS2_PLACEMENT_3D ( 'NONE', #208848, #48479, #11955 ) ;
#2064 = SURFACE_STYLE_FILL_AREA ( #162459 ) ;
#2065 = CARTESIAN_POINT ( 'NONE',  ( -21.05000000000000071, 64.35000000001214460, -136.4231074845243938 ) ) ;
#2067 = ORIENTED_EDGE ( 'NONE', *, *, #86124, .F. ) ;
#2066 = EDGE_LOOP ( 'NONE', ( #121633, #228771, #100380, #90357 ) ) ;
#2068 = ADVANCED_FACE ( 'NONE', ( #53983 ), #194808, .T. ) ;
#2069 = ORIENTED_EDGE ( 'NONE', *, *, #253484, .F. ) ;
#2070 = EDGE_LOOP ( 'NONE', ( #17337, #64326, #202230, #204771 ) ) ;
#2072 = CARTESIAN_POINT ( 'NONE',  ( -23.25000000000000355, 65.95000000001201101, -115.7731074845243597 ) ) ;
#2071 = AXIS2_PLACEMENT_3D ( 'NONE', #163669, #185794, #86661 ) ;
#2073 = CARTESIAN_POINT ( 'NONE',  ( -16.77683809663752257, 23.65833333334447985, -117.2500000000000284 ) ) ;
#2075 = VERTEX_POINT ( 'NONE', #235196 ) ;
#2074 = DIRECTION ( 'NONE',  ( -1.000000000000000000, 0.000000000000000000, 0.000000000000000000 ) ) ;
#2076 = AXIS2_PLACEMENT_3D ( 'NONE', #145577, #223822, #26957 ) ;
#2077 = CARTESIAN_POINT ( 'NONE',  ( 20.84451136049691655, 39.15603001675818007, -236.7953489976115407 ) ) ;
#2078 = FACE_OUTER_BOUND ( 'NONE', #151851, .T. ) ;
#2080 = ORIENTED_EDGE ( 'NONE', *, *, #256043, .T. ) ;
#2079 = LINE ( 'NONE', #161180, #97613 ) ;
#2081 = CARTESIAN_POINT ( 'NONE',  ( 15.74999999999999645, 9.850000000011137402, -50.24999999999999289 ) ) ;
#2082 = ORIENTED_EDGE ( 'NONE', *, *, #111279, .F. ) ;
#2083 = CIRCLE ( 'NONE', #185278, 0.1000000000000033362 ) ;
#2084 = CARTESIAN_POINT ( 'NONE',  ( -21.64999999999999858, 7.350000000011155166, -54.65000000000000568 ) ) ;
#2085 = AXIS2_PLACEMENT_3D ( 'NONE', #968, #120985, #200495 ) ;
#2086 = EDGE_CURVE ( 'NONE', #146851, #82665, #184745, .T. ) ;
#2088 = ORIENTED_EDGE ( 'NONE', *, *, #219268, .F. ) ;
#2087 = DIRECTION ( 'NONE',  ( 1.000000000000000000, 2.952720810173289112E-16, -0.000000000000000000 ) ) ;
#2089 = CARTESIAN_POINT ( 'NONE',  ( -22.50000000000000000, 76.00000000001213607, -136.5231074845242745 ) ) ;
#2090 = CYLINDRICAL_SURFACE ( 'NONE', #228963, 0.1000000000000028644 ) ;
#2091 = EDGE_CURVE ( 'NONE', #32455, #139213, #97225, .T. ) ;
#2092 = CARTESIAN_POINT ( 'NONE',  ( 20.99749315643149217, 11.75000000001115907, -59.98519423124097472 ) ) ;
#2093 = ORIENTED_EDGE ( 'NONE', *, *, #228679, .T. ) ;
#2094 = CARTESIAN_POINT ( 'NONE',  ( -23.25000000000000355, 60.86901957628278836, -220.9190389461266477 ) ) ;
#2095 = FACE_OUTER_BOUND ( 'NONE', #88596, .T. ) ;
#2096 = CARTESIAN_POINT ( 'NONE',  ( 18.37172112093829668, 85.57096165225587470, -163.2063730310406697 ) ) ;
#2097 = DIRECTION ( 'NONE',  ( 1.000000000000000000, -0.000000000000000000, -0.000000000000000000 ) ) ;
#2098 = CARTESIAN_POINT ( 'NONE',  ( 18.59999999999999432, 77.86671491006917734, -91.27043223824227880 ) ) ;
#2099 = ORIENTED_EDGE ( 'NONE', *, *, #22221, .T. ) ;
#2100 = ORIENTED_EDGE ( 'NONE', *, *, #71790, .T. ) ;
#2101 = ORIENTED_EDGE ( 'NONE', *, *, #6458, .F. ) ;
#2102 = ADVANCED_FACE ( 'NONE', ( #74872 ), #243018, .F. ) ;
#2103 = CARTESIAN_POINT ( 'NONE',  ( -16.98495255085921229, 10.00556436600593280, -180.1346172062204687 ) ) ;
#2104 = ORIENTED_EDGE ( 'NONE', *, *, #158035, .T. ) ;
#2105 = CARTESIAN_POINT ( 'NONE',  ( 21.04999999999998650, 69.35000000001186038, -90.77310748452435973 ) ) ;
#2106 = ORIENTED_EDGE ( 'NONE', *, *, #177693, .F. ) ;
#2107 = LINE ( 'NONE', #102472, #215120 ) ;
#2108 = CARTESIAN_POINT ( 'NONE',  ( -21.14999999999999858, 1.572268701310051586, -230.8696453550703325 ) ) ;
#2109 = EDGE_CURVE ( 'NONE', #23713, #81104, #130594, .T. ) ;
#2110 = EDGE_CURVE ( 'NONE', #153327, #225893, #171407, .T. ) ;
#2111 = CIRCLE ( 'NONE', #114562, 0.09999999999999939493 ) ;
#2112 = CIRCLE ( 'NONE', #185298, 0.09999999999999892308 ) ;
#2113 = ORIENTED_EDGE ( 'NONE', *, *, #171486, .F. ) ;
#2114 = ADVANCED_FACE ( 'NONE', ( #116537 ), #211788, .T. ) ;
#2115 = DIRECTION ( 'NONE',  ( 0.000000000000000000, 0.000000000000000000, -1.000000000000000000 ) ) ;
#2116 = AXIS2_PLACEMENT_3D ( 'NONE', #124197, #208546, #145011 ) ;
#2117 = ORIENTED_EDGE ( 'NONE', *, *, #77030, .F. ) ;
#2118 = ORIENTED_EDGE ( 'NONE', *, *, #171993, .F. ) ;
#2119 = ORIENTED_EDGE ( 'NONE', *, *, #28206, .T. ) ;
#2120 = DIRECTION ( 'NONE',  ( 0.000000000000000000, 0.9908441862701782288, -0.1350103645450542456 ) ) ;
#2121 = DIRECTION ( 'NONE',  ( 0.000000000000000000, -6.982962677686266711E-15, 1.000000000000000000 ) ) ;
#2122 = TOROIDAL_SURFACE ( 'NONE', #6414, 0.2000000000000000111, 0.1000000000000000056 ) ;
#2123 = DIRECTION ( 'NONE',  ( 0.000000000000000000, 0.000000000000000000, 1.000000000000000000 ) ) ;
#2124 = CARTESIAN_POINT ( 'NONE',  ( -21.55000000000000071, 7.350000000011155166, -179.8499999999999943 ) ) ;
#2125 = DIRECTION ( 'NONE',  ( 0.000000000000000000, 6.982962677686266711E-15, -1.000000000000000000 ) ) ;
#2126 = DIRECTION ( 'NONE',  ( 0.000000000000000000, 6.982962677686266711E-15, -1.000000000000000000 ) ) ;
#2127 = ADVANCED_FACE ( 'NONE', ( #137357 ), #72278, .F. ) ;
#2128 =( BOUNDED_CURVE ( )  B_SPLINE_CURVE ( 3, ( #228953, #211966, #188532, #33357 ),
 .UNSPECIFIED., .F., .F. ) 
 B_SPLINE_CURVE_WITH_KNOTS ( ( 4, 4 ),
 ( 0.000000000000000000, 1.570796326794908992 ),
 .UNSPECIFIED. ) 
 CURVE ( )  GEOMETRIC_REPRESENTATION_ITEM ( )  RATIONAL_B_SPLINE_CURVE ( ( 1.000000000000000000, 0.8047378541243619399, 0.8047378541243619399, 1.000000000000000000 ) ) 
 REPRESENTATION_ITEM ( '' )  );
#2130 = CARTESIAN_POINT ( 'NONE',  ( 18.59999999999999076, 1.835341550235567887, -145.5551512925629822 ) ) ;
#2129 = DIRECTION ( 'NONE',  ( 0.000000000000000000, 0.000000000000000000, -1.000000000000000000 ) ) ;
#2131 = CYLINDRICAL_SURFACE ( 'NONE', #62295, 0.1000000000000028644 ) ;
#2133 = ORIENTED_EDGE ( 'NONE', *, *, #155455, .T. ) ;
#2132 = CARTESIAN_POINT ( 'NONE',  ( 21.14999999999999858, 87.75000000001259082, -191.2731074845242745 ) ) ;
#2134 = DIRECTION ( 'NONE',  ( 0.7071067811865474617, 0.6909108974501236844, 0.1504730267678057731 ) ) ;
#2135 = LINE ( 'NONE', #137792, #19751 ) ;
#2136 = ORIENTED_EDGE ( 'NONE', *, *, #172077, .F. ) ;
#2137 = ORIENTED_EDGE ( 'NONE', *, *, #120516, .T. ) ;
#2138 = FACE_OUTER_BOUND ( 'NONE', #13583, .T. ) ;
#2139 = CIRCLE ( 'NONE', #214521, 0.1000000000000017680 ) ;
#2140 = DIRECTION ( 'NONE',  ( 0.000000000000000000, -7.056502275159894776E-15, 1.000000000000000000 ) ) ;
#2141 = CARTESIAN_POINT ( 'NONE',  ( 19.75857864376268935, 64.25000000001148237, -44.77310748452440237 ) ) ;
#2142 = ORIENTED_EDGE ( 'NONE', *, *, #212820, .F. ) ;
#2143 = AXIS2_PLACEMENT_3D ( 'NONE', #50735, #208578, #170767 ) ;
#2144 = AXIS2_PLACEMENT_3D ( 'NONE', #156264, #93689, #76680 ) ;
#2145 = DIRECTION ( 'NONE',  ( 0.000000000000000000, 0.000000000000000000, 1.000000000000000000 ) ) ;
#2146 = ORIENTED_EDGE ( 'NONE', *, *, #84330, .T. ) ;
#2147 = VERTEX_POINT ( 'NONE', #216897 ) ;
#2148 = DIRECTION ( 'NONE',  ( 0.000000000000000000, 0.000000000000000000, 1.000000000000000000 ) ) ;
#2149 = ORIENTED_EDGE ( 'NONE', *, *, #223484, .T. ) ;
#2150 = CARTESIAN_POINT ( 'NONE',  ( 20.09999999673965121, 5.571292164246353984, 16.50791943615039514 ) ) ;
#2151 = DIRECTION ( 'NONE',  ( 1.000000000000000000, 0.000000000000000000, -0.000000000000000000 ) ) ;
#2152 = CIRCLE ( 'NONE', #110487, 0.1000000000000028644 ) ;
#2153 = CARTESIAN_POINT ( 'NONE',  ( -16.80469485234341320, 9.942151663152195340, -121.3099668439312495 ) ) ;
#2154 = CARTESIAN_POINT ( 'NONE',  ( 22.57320508075688892, 11.75000000001115552, -134.0000000000000000 ) ) ;
#2155 = ORIENTED_EDGE ( 'NONE', *, *, #13809, .F. ) ;
#2156 = FACE_OUTER_BOUND ( 'NONE', #67120, .T. ) ;
#2157 = DIRECTION ( 'NONE',  ( 0.000000000000000000, -0.4930308989875248349, -0.8700118002898312719 ) ) ;
#2158 = DIRECTION ( 'NONE',  ( -1.000000000000000000, -0.000000000000000000, -0.000000000000000000 ) ) ;
#2159 = TOROIDAL_SURFACE ( 'NONE', #222737, 0.4000000000000003553, 0.1000000000000000056 ) ;
#2160 = ADVANCED_FACE ( 'NONE', ( #220767 ), #22578, .F. ) ;
#2161 = ORIENTED_EDGE ( 'NONE', *, *, #100078, .F. ) ;
#2162 = CIRCLE ( 'NONE', #181272, 2.000000000000006661 ) ;
#2163 = EDGE_LOOP ( 'NONE', ( #167237, #72428, #10118, #32795 ) ) ;
#2164 = CARTESIAN_POINT ( 'NONE',  ( 23.14999999999998437, 71.95000000001165574, -69.52310748452434552 ) ) ;
#2165 = DIRECTION ( 'NONE',  ( 0.000000000000000000, -0.8660254037844419273, 0.4999999999999942824 ) ) ;
#2166 = EDGE_CURVE ( 'NONE', #91133, #131663, #9782, .T. ) ;
#2167 = DIRECTION ( 'NONE',  ( 1.000000000000000000, 0.000000000000000000, -0.000000000000000000 ) ) ;
#2168 = CARTESIAN_POINT ( 'NONE',  ( -21.45000000000000284, 65.35370752038342346, -213.3282663891675952 ) ) ;
#2169 = CARTESIAN_POINT ( 'NONE',  ( 20.94999999999999574, -11.48912529306490349, -170.5999999999999659 ) ) ;
#2170 = CARTESIAN_POINT ( 'NONE',  ( 21.05000000000000071, 87.48912529308749697, -39.02310748452423894 ) ) ;
#2171 = ORIENTED_EDGE ( 'NONE', *, *, #219471, .F. ) ;
#2172 = DIRECTION ( 'NONE',  ( 0.000000000000000000, 1.000000000000000000, 2.891205793294679805E-16 ) ) ;
#2173 = DIRECTION ( 'NONE',  ( 0.000000000000000000, 0.000000000000000000, -1.000000000000000000 ) ) ;
#2174 = EDGE_CURVE ( 'NONE', #28041, #167915, #76409, .T. ) ;
#2175 = EDGE_CURVE ( 'NONE', #61516, #42744, #101312, .T. ) ;
#2176 = CARTESIAN_POINT ( 'NONE',  ( -18.48179518609297389, 77.41031392689789925, -241.7248553661750918 ) ) ;
#2177 = CARTESIAN_POINT ( 'NONE',  ( 21.53699400381585249, 6.787711793193205168, -134.0000000000000000 ) ) ;
#2178 = AXIS2_PLACEMENT_3D ( 'NONE', #78745, #134856, #20087 ) ;
#2179 = CARTESIAN_POINT ( 'NONE',  ( -21.33487959338958362, 69.27444184810150318, -203.5231074845243882 ) ) ;
#2180 = CARTESIAN_POINT ( 'NONE',  ( 20.41140022480506389, 65.58956915760997219, -61.90810618088980277 ) ) ;
#2181 = ORIENTED_EDGE ( 'NONE', *, *, #224044, .T. ) ;
#2182 = ORIENTED_EDGE ( 'NONE', *, *, #222072, .F. ) ;
#2183 = CARTESIAN_POINT ( 'NONE',  ( 18.49999999999999289, 6.450000000011156587, -77.01702717044007329 ) ) ;
#2184 = CARTESIAN_POINT ( 'NONE',  ( 21.05000000000000071, 76.00000000001242029, -165.9231074845243654 ) ) ;
#2186 = CYLINDRICAL_SURFACE ( 'NONE', #18211, 0.09999999999999939493 ) ;
#2185 = CIRCLE ( 'NONE', #147950, 0.5000000000000022204 ) ;
#2187 = CARTESIAN_POINT ( 'NONE',  ( 20.96428641294528106, 17.15731666422714241, -224.5635080354869046 ) ) ;
#2188 = EDGE_CURVE ( 'NONE', #56118, #23218, #180492, .T. ) ;
#2189 = ORIENTED_EDGE ( 'NONE', *, *, #193610, .F. ) ;
#2190 = CARTESIAN_POINT ( 'NONE',  ( -18.34374000495059676, 64.52683809664972614, -145.7731074845244450 ) ) ;
#2191 = EDGE_CURVE ( 'NONE', #47266, #177428, #26568, .T. ) ;
#2192 = DIRECTION ( 'NONE',  ( 0.000000000000000000, 0.9126074666063660468, 0.4088369013363524762 ) ) ;
#2193 = DIRECTION ( 'NONE',  ( 1.000000000000000000, 0.000000000000000000, 0.000000000000000000 ) ) ;
#2194 = PRODUCT_DEFINITION ( 'UNKNOWN', '', #98794, #60944 ) ;
#2195 = DIRECTION ( 'NONE',  ( -1.000000000000000000, -2.952720810173289112E-16, 0.000000000000000000 ) ) ;
#2196 = TOROIDAL_SURFACE ( 'NONE', #168860, 0.2000000000000000111, 0.1000000000000000056 ) ;
#2197 = VERTEX_POINT ( 'NONE', #141229 ) ;
#2198 = CARTESIAN_POINT ( 'NONE',  ( -20.85000000000000142, 76.00000000001126921, -203.5231074845248997 ) ) ;
#2199 = EDGE_CURVE ( 'NONE', #166220, #129337, #219461, .T. ) ;
#2200 = ORIENTED_EDGE ( 'NONE', *, *, #62626, .F. ) ;
#2201 = ADVANCED_FACE ( 'NONE', ( #60393 ), #162094, .F. ) ;
#2202 = CARTESIAN_POINT ( 'NONE',  ( -21.04999999999999716, 76.01771943332057901, -75.96419217299552429 ) ) ;
#2203 = ADVANCED_FACE ( 'NONE', ( #120419 ), #199938, .T. ) ;
#2204 = DIRECTION ( 'NONE',  ( 0.000000000000000000, 0.000000000000000000, -1.000000000000000000 ) ) ;
#2205 = CARTESIAN_POINT ( 'NONE',  ( -21.05000000000000782, 10.01651311888701201, -228.1334776613236386 ) ) ;
#2206 = DIRECTION ( 'NONE',  ( 0.000000000000000000, 0.8814952561688430555, -0.4721928772777346239 ) ) ;
#2207 = CARTESIAN_POINT ( 'NONE',  ( -16.77977881697927032, 9.946601933544062746, -46.16137857311505854 ) ) ;
#2208 = DIRECTION ( 'NONE',  ( -1.000000000000000000, 0.000000000000000000, 0.000000000000000000 ) ) ;
#2209 = B_SPLINE_CURVE_WITH_KNOTS ( 'NONE', 3,
 ( #113554, #173585, #210106, #212668 ),
 .UNSPECIFIED., .F., .F.,
 ( 4, 4 ),
 ( 6.254634441385501517E-18, 0.0001058379652594648159 ),
 .UNSPECIFIED. ) ;
#2210 = CARTESIAN_POINT ( 'NONE',  ( 21.05000000000000071, 87.65000000001163016, -66.62310748452424036 ) ) ;
#2211 = CARTESIAN_POINT ( 'NONE',  ( -21.05000000000000071, 43.57281345108133053, -239.9888335660389487 ) ) ;
#2212 = DIRECTION ( 'NONE',  ( -0.000000000000000000, -0.9126074666063770380, -0.4088369013363281068 ) ) ;
#2213 = CARTESIAN_POINT ( 'NONE',  ( -23.15000000000000213, 54.12082040172526831, -247.0224274369251134 ) ) ;
#2214 = CARTESIAN_POINT ( 'NONE',  ( -21.55000000000000426, 68.29142135624952914, -148.8731074845244109 ) ) ;
#2216 = EDGE_CURVE ( 'NONE', #139066, #12375, #192974, .T. ) ;
#2215 = FACE_BOUND ( 'NONE', #82865, .T. ) ;
#2217 = VECTOR ( 'NONE', #218757, 1000.000000000000000 ) ;
#2218 = CYLINDRICAL_SURFACE ( 'NONE', #153849, 0.09999999999999609201 ) ;
#2220 = CARTESIAN_POINT ( 'NONE',  ( -23.15000000000000213, 84.59626168225520360, -145.9732350016745954 ) ) ;
#2219 = VECTOR ( 'NONE', #3106, 1000.000000000000000 ) ;
#2221 = CIRCLE ( 'NONE', #214611, 0.5000000000000004441 ) ;
#2222 = ORIENTED_EDGE ( 'NONE', *, *, #28885, .T. ) ;
#2223 =( BOUNDED_SURFACE ( )  B_SPLINE_SURFACE ( 3, 2, ( 
 ( #73787, #72490, #30806 ),
 ( #54182, #169044, #89454 ),
 ( #133722, #193714, #189852 ),
 ( #129863, #248538, #15076 ),
 ( #52900, #214544, #134989 ),
 ( #213255, #191160, #152035 ),
 ( #75073, #170339, #69929 ),
 ( #34656, #94593, #132446 ),
 ( #33385, #174188, #230253 ),
 ( #154612, #234105, #112885 ) ),
 .UNSPECIFIED., .F., .F., .T. ) 
 B_SPLINE_SURFACE_WITH_KNOTS ( ( 4, 2, 2, 2, 4 ),
 ( 3, 3 ),
 ( 0.0001701955120502373817, 0.0002247052511886151935, 0.0002792149903269930053, 0.0003882344686037486831, 0.0006062734251572600387 ),
 ( 0.000000000000000000, 1.000000000000000000 ),
 .UNSPECIFIED. ) 
 GEOMETRIC_REPRESENTATION_ITEM ( )  RATIONAL_B_SPLINE_SURFACE ( (
 ( 1.000000000000000000, 0.2966190024560606542, 1.000000000000000000),
 ( 1.000000000000000000, 0.2964522492712500235, 1.000000000000000000),
 ( 1.000000000000000000, 0.3059923531882490222, 1.000000000000000000),
 ( 1.000000000000000000, 0.3355751146946277519, 1.000000000000000000),
 ( 1.000000000000000000, 0.3550672384962930139, 1.000000000000000000),
 ( 1.000000000000000000, 0.4157034672182384760, 1.000000000000000000),
 ( 1.000000000000000000, 0.4588031877647695822, 1.000000000000000000),
 ( 1.000000000000000000, 0.5771441759674355021, 1.000000000000000000),
 ( 1.000000000000000000, 0.6469377121761927807, 1.000000000000000000),
 ( 1.000000000000000000, 0.7071067811865870967, 1.000000000000000000) ) ) 
 REPRESENTATION_ITEM ( '' )  SURFACE ( )  );
#2224 = CYLINDRICAL_SURFACE ( 'NONE', #27248, 0.09999999999999983902 ) ;
#2225 = CARTESIAN_POINT ( 'NONE',  ( -21.14999999999999858, 64.25000000001232081, -163.2969768484652491 ) ) ;
#2226 = ORIENTED_EDGE ( 'NONE', *, *, #96808, .F. ) ;
#2227 = CARTESIAN_POINT ( 'NONE',  ( 21.05000000000000071, -11.64999999999999147, -30.50000000000000000 ) ) ;
#2228 = EDGE_CURVE ( 'NONE', #64408, #27378, #122959, .T. ) ;
#2229 = DIRECTION ( 'NONE',  ( 1.000000000000000000, 0.000000000000000000, 0.000000000000000000 ) ) ;
#2230 = ORIENTED_EDGE ( 'NONE', *, *, #52736, .T. ) ;
#2231 = CARTESIAN_POINT ( 'NONE',  ( -23.25000000000000000, 76.00000000001195133, -103.0231074845243171 ) ) ;
#2232 = CARTESIAN_POINT ( 'NONE',  ( 23.14999999999999503, 19.71413185295147485, -225.2601813404592406 ) ) ;
#2233 = ORIENTED_EDGE ( 'NONE', *, *, #117676, .T. ) ;
#2234 = VECTOR ( 'NONE', #4879, 1000.000000000000000 ) ;
#2235 = CIRCLE ( 'NONE', #43948, 0.1000000000000028644 ) ;
#2236 = TOROIDAL_SURFACE ( 'NONE', #114696, 0.4000000000000015210, 0.1000000000000000056 ) ;
#2237 = EDGE_LOOP ( 'NONE', ( #95473, #164357, #65139, #155619 ) ) ;
#2238 = CARTESIAN_POINT ( 'NONE',  ( 21.14999999999999858, 64.25000000001213607, -136.4231074845243938 ) ) ;
#2239 = EDGE_CURVE ( 'NONE', #9664, #124376, #197236, .T. ) ;
#2240 = VERTEX_POINT ( 'NONE', #179108 ) ;
#2241 = CARTESIAN_POINT ( 'NONE',  ( 20.94999999999999574, 44.06843597547144498, -258.9974126733343951 ) ) ;
#2242 = FACE_OUTER_BOUND ( 'NONE', #130637, .T. ) ;
#2244 = VECTOR ( 'NONE', #91441, 1000.000000000000227 ) ;
#2243 = DIRECTION ( 'NONE',  ( 0.000000000000000000, 0.9770955615653255100, 0.2128009952263878735 ) ) ;
#2245 = EDGE_CURVE ( 'NONE', #48124, #203548, #241611, .T. ) ;
#2247 = CYLINDRICAL_SURFACE ( 'NONE', #187824, 7.900000000000003908 ) ;
#2246 = AXIS2_PLACEMENT_3D ( 'NONE', #173608, #52297, #17068 ) ;
#2248 = CARTESIAN_POINT ( 'NONE',  ( -21.65000000000000213, 7.708578643773852157, -88.15000000000004832 ) ) ;
#2249 = DIRECTION ( 'NONE',  ( 0.000000000000000000, -1.000000000000000000, -6.860497997771531562E-15 ) ) ;
#2250 = DIRECTION ( 'NONE',  ( -0.000000000000000000, -0.000000000000000000, 1.000000000000000000 ) ) ;
#2251 = DIRECTION ( 'NONE',  ( 0.000000000000000000, 0.9126074666063660468, 0.4088369013363524762 ) ) ;
#2253 = VERTEX_POINT ( 'NONE', #414 ) ;
#2252 = DIRECTION ( 'NONE',  ( -1.000000000000000000, 0.000000000000000000, 0.000000000000000000 ) ) ;
#2254 = EDGE_LOOP ( 'NONE', ( #136794, #52446, #245311, #24312 ) ) ;
#2256 = DIRECTION ( 'NONE',  ( 0.000000000000000000, 0.9126074666063660468, 0.4088369013363524762 ) ) ;
#2255 = LINE ( 'NONE', #41426, #216030 ) ;
#2258 = ORIENTED_EDGE ( 'NONE', *, *, #68816, .T. ) ;
#2257 = CARTESIAN_POINT ( 'NONE',  ( 20.95224633520496127, 8.900522166568386240, -108.9932764479213034 ) ) ;
#2259 = ORIENTED_EDGE ( 'NONE', *, *, #44511, .F. ) ;
#2260 = DIRECTION ( 'NONE',  ( 0.000000000000000000, 0.2128009952263604232, -0.9770955615653316162 ) ) ;
#2261 = CARTESIAN_POINT ( 'NONE',  ( 22.39999999999999503, 76.10085836911093793, -148.2726746080136877 ) ) ;
#2262 = ADVANCED_FACE ( 'NONE', ( #4266 ), #59079, .F. ) ;
#2263 = AXIS2_PLACEMENT_3D ( 'NONE', #76115, #20022, #117812 ) ;
#2264 = EDGE_CURVE ( 'NONE', #74308, #96338, #84766, .T. ) ;
#2265 = VECTOR ( 'NONE', #40878, 1000.000000000000000 ) ;
#2266 = DIRECTION ( 'NONE',  ( 0.000000000000000000, -0.000000000000000000, -1.000000000000000000 ) ) ;
#2267 = DIRECTION ( 'NONE',  ( 0.000000000000000000, -0.1455152366551721865, -0.9893560106964475187 ) ) ;
#2268 = TOROIDAL_SURFACE ( 'NONE', #247986, 2.100000000000002309, 0.1000000000000000056 ) ;
#2269 = DIRECTION ( 'NONE',  ( 0.000000000000000000, -8.267618268485201230E-15, 1.000000000000000000 ) ) ;
#2270 = FACE_OUTER_BOUND ( 'NONE', #139592, .T. ) ;
#2271 = PLANE ( 'NONE',  #131101 ) ;
#2272 = ORIENTED_EDGE ( 'NONE', *, *, #247706, .T. ) ;
#2273 = ORIENTED_EDGE ( 'NONE', *, *, #239821, .F. ) ;
#2274 = ORIENTED_EDGE ( 'NONE', *, *, #41752, .T. ) ;
#2275 = DIRECTION ( 'NONE',  ( -0.000000000000000000, -0.000000000000000000, 1.000000000000000000 ) ) ;
#2277 = EDGE_CURVE ( 'NONE', #149628, #150106, #83774, .T. ) ;
#2276 = ORIENTED_EDGE ( 'NONE', *, *, #136399, .F. ) ;
#2278 = DIRECTION ( 'NONE',  ( -1.000000000000000000, -0.000000000000000000, -0.000000000000000000 ) ) ;
#2279 = DIRECTION ( 'NONE',  ( -1.020425574104004394E-15, 0.9126074666063769270, 0.4088369013363280513 ) ) ;
#2280 = EDGE_CURVE ( 'NONE', #246278, #91774, #81227, .T. ) ;
#2281 = CARTESIAN_POINT ( 'NONE',  ( -23.15000000000000213, 76.00000000001142553, -36.02310748452432421 ) ) ;
#2282 = CARTESIAN_POINT ( 'NONE',  ( -21.44999999999999929, 68.65000000001229807, -157.7731074845244166 ) ) ;
#2283 = ORIENTED_EDGE ( 'NONE', *, *, #158672, .T. ) ;
#2284 = CYLINDRICAL_SURFACE ( 'NONE', #233573, 0.1000000000000028644 ) ;
#2285 = VERTEX_POINT ( 'NONE', #107231 ) ;
#2286 = AXIS2_PLACEMENT_3D ( 'NONE', #49761, #73209, #129304 ) ;
#2287 = CARTESIAN_POINT ( 'NONE',  ( -18.40000000000000213, 64.52683809664972614, -145.7731074845244450 ) ) ;
#2288 = DIRECTION ( 'NONE',  ( 0.000000000000000000, 0.000000000000000000, -1.000000000000000000 ) ) ;
#2289 = EDGE_CURVE ( 'NONE', #178217, #49193, #223313, .T. ) ;
#2290 = CIRCLE ( 'NONE', #168784, 0.1000000000000106498 ) ;
#2291 = DIRECTION ( 'NONE',  ( 0.000000000000000000, -0.4791956752371546169, -0.8777080977375152360 ) ) ;
#2292 = CARTESIAN_POINT ( 'NONE',  ( -22.39999999999999858, 65.09550114356427741, -243.3481044654562879 ) ) ;
#2293 = AXIS2_PLACEMENT_3D ( 'NONE', #61986, #161089, #24153 ) ;
#2295 = ORIENTED_EDGE ( 'NONE', *, *, #162133, .F. ) ;
#2294 = EDGE_CURVE ( 'NONE', #210604, #245137, #5670, .T. ) ;
#2296 = CARTESIAN_POINT ( 'NONE',  ( -21.05439746398122836, 64.25000000001189449, -96.03319099703979589 ) ) ;
#2297 = ORIENTED_EDGE ( 'NONE', *, *, #84952, .T. ) ;
#2300 = ORIENTED_EDGE ( 'NONE', *, *, #78334, .T. ) ;
#2299 = DIRECTION ( 'NONE',  ( 0.000000000000000000, -0.9126074666063773710, -0.4088369013363274962 ) ) ;
#2298 = CYLINDRICAL_SURFACE ( 'NONE', #45055, 1.749999999999999778 ) ;
#2301 = CARTESIAN_POINT ( 'NONE',  ( -21.76363531954647357, 0.09900187431060442078, -160.4870634521282398 ) ) ;
#2302 = ORIENTED_EDGE ( 'NONE', *, *, #37868, .T. ) ;
#2303 = AXIS2_PLACEMENT_3D ( 'NONE', #215291, #116217, #17118 ) ;
#2304 = CARTESIAN_POINT ( 'NONE',  ( -6.000000000000002665, -11.25000000000000000, 14.00000000000000178 ) ) ;
#2305 = ORIENTED_EDGE ( 'NONE', *, *, #186067, .F. ) ;
#2306 = CARTESIAN_POINT ( 'NONE',  ( 18.49999999999999645, 5.699452464332751767, -121.4577260434301991 ) ) ;
#2307 = DIRECTION ( 'NONE',  ( 4.336808689942017736E-16, 0.000000000000000000, 1.000000000000000000 ) ) ;
#2308 = ADVANCED_FACE ( 'NONE', ( #245479 ), #47239, .T. ) ;
#2309 = LINE ( 'NONE', #81826, #246743 ) ;
#2310 = UNCERTAINTY_MEASURE_WITH_UNIT (LENGTH_MEASURE( 1.000000000000000082E-05 ), #192241, 'distance_accuracy_value', 'NONE');
#2311 = ADVANCED_FACE ( 'NONE', ( #25157 ), #227174, .T. ) ;
#2313 = VERTEX_POINT ( 'NONE', #8145 ) ;
#2312 = DIRECTION ( 'NONE',  ( 0.000000000000000000, -0.8700118002898321601, 0.4930308989875230030 ) ) ;
#2314 = CARTESIAN_POINT ( 'NONE',  ( -20.64999999999999858, 61.88149656937975607, -248.1136133839584090 ) ) ;
#2315 = VECTOR ( 'NONE', #168034, 999.9999999999998863 ) ;
#2316 = ORIENTED_EDGE ( 'NONE', *, *, #26990, .T. ) ;
#2317 = DIRECTION ( 'NONE',  ( 0.000000000000000000, 0.4646089985449745052, 0.8855159391400224678 ) ) ;
#2318 = CARTESIAN_POINT ( 'NONE',  ( -22.10000000000000497, 6.223900101154156594, 12.09999999999999964 ) ) ;
#2319 = LINE ( 'NONE', #1018, #54592 ) ;
#2320 = CIRCLE ( 'NONE', #148096, 0.09999999999998898659 ) ;
#2321 = B_SPLINE_CURVE_WITH_KNOTS ( 'NONE', 3,
 ( #18012, #135383, #35060, #114557, #256573, #194114, #115837, #15475, #255290, #157576 ),
 .UNSPECIFIED., .F., .F.,
 ( 4, 3, 3, 4 ),
 ( 0.000000000000000000, 0.0002000000000008585893, 0.001000000000082977483, 0.001967863649483336721 ),
 .UNSPECIFIED. ) ;
#2322 = VERTEX_POINT ( 'NONE', #164653 ) ;
#2323 = FACE_OUTER_BOUND ( 'NONE', #221063, .T. ) ;
#2324 = ORIENTED_EDGE ( 'NONE', *, *, #82387, .T. ) ;
#2325 = CARTESIAN_POINT ( 'NONE',  ( -20.54999999999999716, 76.00000000001244871, -170.0231074845243597 ) ) ;
#2326 = CARTESIAN_POINT ( 'NONE',  ( 23.25000000000000000, 82.67551891922275331, -215.5849511313000164 ) ) ;
#2327 = DIRECTION ( 'NONE',  ( 0.000000000000000000, 0.2605042016806672911, -0.9654727137038716656 ) ) ;
#2328 = AXIS2_PLACEMENT_3D ( 'NONE', #70395, #7830, #149920 ) ;
#2330 = VERTEX_POINT ( 'NONE', #188063 ) ;
#2329 = PLANE ( 'NONE',  #252783 ) ;
#2331 = CARTESIAN_POINT ( 'NONE',  ( 21.08750232978087880, 22.97271790860457230, -230.0531648411424044 ) ) ;
#2332 = CYLINDRICAL_SURFACE ( 'NONE', #72274, 0.09999999999999867328 ) ;
#2333 = CARTESIAN_POINT ( 'NONE',  ( 21.05000000000000071, 28.15345123516638282, -259.0759448016705733 ) ) ;
#2334 = ORIENTED_EDGE ( 'NONE', *, *, #214841, .T. ) ;
#2335 = DIRECTION ( 'NONE',  ( 0.000000000000000000, 0.5859227990963212784, 0.8103668758649578141 ) ) ;
#2336 = CARTESIAN_POINT ( 'NONE',  ( -23.25000000000000000, 7.128833340093095217, -233.7327013124392749 ) ) ;
#2337 = ORIENTED_EDGE ( 'NONE', *, *, #212153, .F. ) ;
#2338 = SPHERICAL_SURFACE ( 'NONE', #28389, 0.1000000000000000056 ) ;
#2339 = AXIS2_PLACEMENT_3D ( 'NONE', #85200, #109930, #4409 ) ;
#2340 = AXIS2_PLACEMENT_3D ( 'NONE', #135814, #217910, #198371 ) ;
#2341 = EDGE_CURVE ( 'NONE', #80343, #8664, #126314, .T. ) ;
#2342 = AXIS2_PLACEMENT_3D ( 'NONE', #87864, #249549, #187018 ) ;
#2343 = ORIENTED_EDGE ( 'NONE', *, *, #155700, .F. ) ;
#2344 = ORIENTED_EDGE ( 'NONE', *, *, #168711, .T. ) ;
#2345 = DIRECTION ( 'NONE',  ( -0.000000000000000000, 0.1350103645451649625, -0.9908441862701631297 ) ) ;
#2346 = ORIENTED_EDGE ( 'NONE', *, *, #179917, .F. ) ;
#2348 = ORIENTED_EDGE ( 'NONE', *, *, #74702, .T. ) ;
#2347 = CARTESIAN_POINT ( 'NONE',  ( 18.59999999999999076, 64.25000000001246292, -181.7731074845244450 ) ) ;
#2351 = VERTEX_POINT ( 'NONE', #66830 ) ;
#2350 = EDGE_LOOP ( 'NONE', ( #67786, #198931, #110375, #253215 ) ) ;
#2349 = DIRECTION ( 'NONE',  ( 0.000000000000000000, -0.000000000000000000, 1.000000000000000000 ) ) ;
#2352 = DIRECTION ( 'NONE',  ( -1.000000000000000000, -0.000000000000000000, -0.000000000000000000 ) ) ;
#2353 = CARTESIAN_POINT ( 'NONE',  ( -20.92356734117541706, 65.68026841930851845, -30.47257401318895376 ) ) ;
#2354 = CARTESIAN_POINT ( 'NONE',  ( -20.85000000000000142, 64.25000000001220712, -143.3069731475025321 ) ) ;
#2356 = CARTESIAN_POINT ( 'NONE',  ( 18.59999999999999076, 11.75000000000000355, -8.099999999999999645 ) ) ;
#2355 = FACE_OUTER_BOUND ( 'NONE', #256850, .T. ) ;
#2358 = EDGE_CURVE ( 'NONE', #239783, #205125, #234657, .T. ) ;
#2357 = DIRECTION ( 'NONE',  ( 0.000000000000000000, -0.9770955615653313941, -0.2128009952263603677 ) ) ;
#2359 = CIRCLE ( 'NONE', #10762, 3.900000000000000799 ) ;
#2360 = CARTESIAN_POINT ( 'NONE',  ( -16.94275863009466576, 44.08128092168011136, -235.2799346461642358 ) ) ;
#2362 = FACE_OUTER_BOUND ( 'NONE', #103503, .T. ) ;
#2361 = DIRECTION ( 'NONE',  ( -1.000000000000000000, -0.000000000000000000, 0.000000000000000000 ) ) ;
#2363 = ORIENTED_EDGE ( 'NONE', *, *, #1548, .T. ) ;
#2364 = VERTEX_POINT ( 'NONE', #68113 ) ;
#2365 = CARTESIAN_POINT ( 'NONE',  ( -22.39999999999999858, 0.1000000000111554016, -25.70922040162659883 ) ) ;
#2366 = CIRCLE ( 'NONE', #135647, 11.70000000000001528 ) ;
#2368 = VERTEX_POINT ( 'NONE', #147646 ) ;
#2367 = DIRECTION ( 'NONE',  ( 0.000000000000000000, -1.000000000000000000, 0.000000000000000000 ) ) ;
#2369 = EDGE_LOOP ( 'NONE', ( #246721, #113564, #221007, #28489 ) ) ;
#2370 = CYLINDRICAL_SURFACE ( 'NONE', #81088, 1.749999999999998002 ) ;
#2371 = EDGE_LOOP ( 'NONE', ( #248798, #144734, #105475 ) ) ;
#2372 = CARTESIAN_POINT ( 'NONE',  ( 23.14999999999998437, 1.115650265596050101E-11, -163.4499999999999886 ) ) ;
#2373 = ORIENTED_EDGE ( 'NONE', *, *, #116759, .T. ) ;
#2374 = DIRECTION ( 'NONE',  ( 1.000000000000000000, 0.000000000000000000, 0.000000000000000000 ) ) ;
#2375 = CARTESIAN_POINT ( 'NONE',  ( -18.59999999999999787, 7.476371755685454090, -241.7308184205399471 ) ) ;
#2378 = ORIENTED_EDGE ( 'NONE', *, *, #233140, .F. ) ;
#2377 = VERTEX_POINT ( 'NONE', #5543 ) ;
#2376 = AXIS2_PLACEMENT_3D ( 'NONE', #62994, #87679, #163395 ) ;
#2379 = CIRCLE ( 'NONE', #148144, 11.70000000000000284 ) ;
#2380 = ORIENTED_EDGE ( 'NONE', *, *, #183415, .F. ) ;
#2381 = LINE ( 'NONE', #20704, #57114 ) ;
#2382 = ORIENTED_EDGE ( 'NONE', *, *, #5338, .F. ) ;
#2383 = VERTEX_POINT ( 'NONE', #205023 ) ;
#2384 = CARTESIAN_POINT ( 'NONE',  ( 23.15000000000000213, -9.599999999988842347, -191.1060308773475072 ) ) ;
#2386 = ORIENTED_EDGE ( 'NONE', *, *, #191303, .F. ) ;
#2385 = CYLINDRICAL_SURFACE ( 'NONE', #18571, 0.1000000000000028644 ) ;
#2388 = DIRECTION ( 'NONE',  ( 1.000000000000000000, 0.000000000000000000, 0.000000000000000000 ) ) ;
#2387 = CARTESIAN_POINT ( 'NONE',  ( 23.24999999999999289, 11.75000000001116263, -55.25000000000004974 ) ) ;
#2389 = CARTESIAN_POINT ( 'NONE',  ( -20.94999999999999929, 11.65000000001115232, -93.71613433702194129 ) ) ;
#2390 = DIRECTION ( 'NONE',  ( 0.000000000000000000, -1.000000000000000000, -2.891205793294679805E-16 ) ) ;
#2391 = DIRECTION ( 'NONE',  ( 0.000000000000000000, -1.000000000000000000, 0.000000000000000000 ) ) ;
#2392 = ORIENTED_EDGE ( 'NONE', *, *, #12032, .T. ) ;
#2393 = ORIENTED_EDGE ( 'NONE', *, *, #26086, .F. ) ;
#2394 = DIRECTION ( 'NONE',  ( 0.000000000000000000, 0.4721928772778128947, 0.8814952561688012000 ) ) ;
#2395 = CARTESIAN_POINT ( 'NONE',  ( -16.86733706339143879, 66.03400947037258106, -149.1199921825257206 ) ) ;
#2396 = CYLINDRICAL_SURFACE ( 'NONE', #158089, 0.09999999999999939493 ) ;
#2397 = EDGE_CURVE ( 'NONE', #177487, #11610, #128089, .T. ) ;
#2398 = AXIS2_PLACEMENT_3D ( 'NONE', #88626, #53379, #250294 ) ;
#2399 = ORIENTED_EDGE ( 'NONE', *, *, #105194, .T. ) ;
#2400 = DIRECTION ( 'NONE',  ( 0.000000000000000000, 1.483188571960168804E-13, -1.000000000000000000 ) ) ;
#2401 = AXIS2_PLACEMENT_3D ( 'NONE', #20596, #4830, #81791 ) ;
#2403 = B_SPLINE_CURVE_WITH_KNOTS ( 'NONE', 3,
 ( #238427, #53691, #151540, #172404 ),
 .UNSPECIFIED., .F., .F.,
 ( 4, 4 ),
 ( 0.000000000000000000, 0.0002118541922231967595 ),
 .UNSPECIFIED. ) ;
#2402 = CIRCLE ( 'NONE', #177245, 11.69999999999998863 ) ;
#2404 = CARTESIAN_POINT ( 'NONE',  ( 23.24999999999999645, -3.899999999988843502, -167.5000000000000284 ) ) ;
#2405 = DIRECTION ( 'NONE',  ( 0.000000000000000000, -0.1455152366551721865, -0.9893560106964475187 ) ) ;
#2406 = ORIENTED_EDGE ( 'NONE', *, *, #176143, .F. ) ;
#2407 = ORIENTED_EDGE ( 'NONE', *, *, #217591, .F. ) ;
#2408 = EDGE_CURVE ( 'NONE', #164486, #101793, #222148, .T. ) ;
#2409 = DIRECTION ( 'NONE',  ( -3.035766082959430717E-14, -6.982962677686266711E-15, 1.000000000000000000 ) ) ;
#2410 = CARTESIAN_POINT ( 'NONE',  ( -20.05000000000000426, 63.86602797976523505, -212.9247947273492514 ) ) ;
#2411 = ORIENTED_EDGE ( 'NONE', *, *, #20635, .F. ) ;
#2412 = CARTESIAN_POINT ( 'NONE',  ( -20.94999999999999929, 77.83534155023701828, -191.9679561919613491 ) ) ;
#2413 = EDGE_LOOP ( 'NONE', ( #46517, #136076 ) ) ;
#2414 = CARTESIAN_POINT ( 'NONE',  ( -20.85000000000000142, 42.15997144203495139, -239.2817429668763793 ) ) ;
#2415 = DIRECTION ( 'NONE',  ( 1.000000000000000000, 1.836970198721029934E-16, 3.186635328391151676E-31 ) ) ;
#2417 = CARTESIAN_POINT ( 'NONE',  ( -20.91682497891423154, 68.08564185115264422, -224.1612363371343122 ) ) ;
#2416 = CARTESIAN_POINT ( 'NONE',  ( -20.05000000000000426, 9.250000000011157297, -54.65000000000000568 ) ) ;
#2418 = ADVANCED_FACE ( 'NONE', ( #108518 ), #228484, .T. ) ;
#2419 = CARTESIAN_POINT ( 'NONE',  ( 22.42196299218230493, 0.002441673998456600492, -55.35038829735057675 ) ) ;
#2420 = FACE_OUTER_BOUND ( 'NONE', #249983, .T. ) ;
#2421 = VERTEX_POINT ( 'NONE', #86353 ) ;
#2422 = EDGE_CURVE ( 'NONE', #75669, #50778, #138924, .T. ) ;
#2423 = CARTESIAN_POINT ( 'NONE',  ( -20.94999999999999929, 74.92681270650359693, -207.4801605588535551 ) ) ;
#2424 = AXIS2_PLACEMENT_3D ( 'NONE', #164957, #146654, #103671 ) ;
#2425 = AXIS2_PLACEMENT_3D ( 'NONE', #153513, #135160, #16531 ) ;
#2427 = ORIENTED_EDGE ( 'NONE', *, *, #164308, .F. ) ;
#2426 = ORIENTED_EDGE ( 'NONE', *, *, #77999, .F. ) ;
#2428 = ORIENTED_EDGE ( 'NONE', *, *, #175814, .F. ) ;
#2429 = AXIS2_PLACEMENT_3D ( 'NONE', #151127, #230663, #191554 ) ;
#2430 = VERTEX_POINT ( 'NONE', #45974 ) ;
#2431 = CARTESIAN_POINT ( 'NONE',  ( 21.05000000000000071, 71.00000000001151079, -48.42837350343745584 ) ) ;
#2432 = CARTESIAN_POINT ( 'NONE',  ( -20.94999999999994600, 64.35000000001120668, -30.12310748452479103 ) ) ;
#2433 = CARTESIAN_POINT ( 'NONE',  ( -20.64999999999999858, 71.65000000001259650, -191.1731074845243654 ) ) ;
#2434 = CARTESIAN_POINT ( 'NONE',  ( -16.94445028196807002, 9.992063609697737547, -20.89266982158155628 ) ) ;
#2435 = VECTOR ( 'NONE', #158170, 1000.000000000000000 ) ;
#2436 = DIRECTION ( 'NONE',  ( 0.000000000000000000, -0.6728388485993177515, 0.7397890806274072251 ) ) ;
#2437 = EDGE_CURVE ( 'NONE', #105984, #249805, #159645, .T. ) ;
#2439 = LINE ( 'NONE', #241092, #53387 ) ;
#2438 = CARTESIAN_POINT ( 'NONE',  ( 20.41140022480491467, 10.41043084240188854, -7.615001303634437058 ) ) ;
#2441 = ORIENTED_EDGE ( 'NONE', *, *, #117503, .T. ) ;
#2440 = FACE_BOUND ( 'NONE', #136830, .T. ) ;
#2442 = DIRECTION ( 'NONE',  ( 0.000000000000000000, 0.000000000000000000, 1.000000000000000000 ) ) ;
#2443 = VERTEX_POINT ( 'NONE', #185492 ) ;
#2444 = AXIS2_PLACEMENT_3D ( 'NONE', #49428, #91120, #185088 ) ;
#2445 = DIRECTION ( 'NONE',  ( 1.000000000000000000, 0.000000000000000000, 0.000000000000000000 ) ) ;
#2446 = CIRCLE ( 'NONE', #148194, 11.65000000000000746 ) ;
#2447 = ORIENTED_EDGE ( 'NONE', *, *, #86991, .F. ) ;
#2448 = ORIENTED_EDGE ( 'NONE', *, *, #19922, .T. ) ;
#2449 = DIRECTION ( 'NONE',  ( 0.000000000000000000, -1.000000000000000000, 0.000000000000000000 ) ) ;
#2450 = DIRECTION ( 'NONE',  ( 1.000000000000000000, 0.000000000000000000, 0.000000000000000000 ) ) ;
#2451 = CARTESIAN_POINT ( 'NONE',  ( -16.92280123533709713, 66.05000000001153637, -48.87373979860947060 ) ) ;
#2452 = CARTESIAN_POINT ( 'NONE',  ( -18.34374000495060386, 11.47316190337362585, -109.7500000000000284 ) ) ;
#2453 = AXIS2_PLACEMENT_3D ( 'NONE', #52385, #167250, #207647 ) ;
#2454 = FACE_OUTER_BOUND ( 'NONE', #90440, .T. ) ;
#2455 = ORIENTED_EDGE ( 'NONE', *, *, #81482, .T. ) ;
#2456 = EDGE_LOOP ( 'NONE', ( #42361, #162104, #147373, #116502 ) ) ;
#2457 = AXIS2_PLACEMENT_3D ( 'NONE', #232503, #133388, #212919 ) ;
#2458 = DIRECTION ( 'NONE',  ( 0.000000000000000000, -7.026728003956695223E-15, 1.000000000000000000 ) ) ;
#2459 = EDGE_LOOP ( 'NONE', ( #84036, #123017, #84651, #33522 ) ) ;
#2460 = DIRECTION ( 'NONE',  ( 1.000000000000000000, 0.000000000000000000, 0.000000000000000000 ) ) ;
#2461 = DIRECTION ( 'NONE',  ( 1.000000000000000000, 0.000000000000000000, 0.000000000000000000 ) ) ;
#2462 = VECTOR ( 'NONE', #109339, 999.9999999999998863 ) ;
#2463 = DIRECTION ( 'NONE',  ( 1.000000000000000000, -0.000000000000000000, -0.000000000000000000 ) ) ;
#2464 = CIRCLE ( 'NONE', #48263, 0.1000000000000006578 ) ;
#2465 = DIRECTION ( 'NONE',  ( -1.000000000000000000, 0.000000000000000000, 0.000000000000000000 ) ) ;
#2466 = CARTESIAN_POINT ( 'NONE',  ( -18.59999999999999787, 77.83585931145546510, -91.51866831572576189 ) ) ;
#2467 = FACE_OUTER_BOUND ( 'NONE', #246611, .T. ) ;
#2468 = DIRECTION ( 'NONE',  ( 1.000000000000000000, 0.000000000000000000, -0.000000000000000000 ) ) ;
#2469 = DIRECTION ( 'NONE',  ( 0.000000000000000000, 0.000000000000000000, 1.000000000000000000 ) ) ;
#2470 = DIRECTION ( 'NONE',  ( 1.000000000000000000, 0.000000000000000000, -0.000000000000000000 ) ) ;
#2471 = CARTESIAN_POINT ( 'NONE',  ( 23.14999999999999858, 5.599999999999996980, -21.09473398108690390 ) ) ;
#2472 = LINE ( 'NONE', #198121, #128010 ) ;
#2473 = EDGE_CURVE ( 'NONE', #192876, #25429, #206345, .T. ) ;
#2474 = ORIENTED_EDGE ( 'NONE', *, *, #183247, .F. ) ;
#2475 = ORIENTED_EDGE ( 'NONE', *, *, #234542, .T. ) ;
#2476 = APPLICATION_CONTEXT ( 'automotive_design' ) ;
#2477 = ADVANCED_FACE ( 'NONE', ( #140792 ), #198191, .F. ) ;
#2478 = CARTESIAN_POINT ( 'NONE',  ( -17.11825945287481332, 14.13772148853350252, -219.1573629999798811 ) ) ;
#2480 = CIRCLE ( 'NONE', #98309, 11.80000000000000426 ) ;
#2479 = LINE ( 'NONE', #242382, #193880 ) ;
#2481 = CARTESIAN_POINT ( 'NONE',  ( -23.25000000000000000, 6.933893972126341509, -37.28564583437357527 ) ) ;
#2483 = ORIENTED_EDGE ( 'NONE', *, *, #71657, .T. ) ;
#2482 = VECTOR ( 'NONE', #191935, 1000.000000000000000 ) ;
#2484 = CARTESIAN_POINT ( 'NONE',  ( -20.94999999999999929, 87.48912529308749697, -39.12310748452424747 ) ) ;
#2486 = EDGE_CURVE ( 'NONE', #219374, #227995, #238605, .T. ) ;
#2485 = AXIS2_PLACEMENT_3D ( 'NONE', #224032, #44134, #123671 ) ;
#2487 = DIRECTION ( 'NONE',  ( 0.000000000000000000, -0.1350103645451904977, 0.9908441862701596881 ) ) ;
#2488 = CYLINDRICAL_SURFACE ( 'NONE', #129690, 0.1000000000000013933 ) ;
#2489 = DIRECTION ( 'NONE',  ( 0.000000000000000000, -0.4721928772777347350, -0.8814952561688431665 ) ) ;
#2490 = CARTESIAN_POINT ( 'NONE',  ( -16.94107738177414291, 10.01423928514777373, -121.4500000000000313 ) ) ;
#2491 = DIRECTION ( 'NONE',  ( -1.000000000000000000, 0.000000000000000000, -0.000000000000000000 ) ) ;
#2492 = TOROIDAL_SURFACE ( 'NONE', #52568, 0.2000000000000000111, 0.1000000000000000056 ) ;
#2493 = VERTEX_POINT ( 'NONE', #41706 ) ;
#2494 = DIRECTION ( 'NONE',  ( 0.000000000000000000, 0.000000000000000000, 1.000000000000000000 ) ) ;
#2496 = ORIENTED_EDGE ( 'NONE', *, *, #130595, .F. ) ;
#2495 = CARTESIAN_POINT ( 'NONE',  ( 22.48660254037844197, 11.65000000001116298, -167.4499999999999602 ) ) ;
#2497 = DIRECTION ( 'NONE',  ( 1.000000000000000000, 0.000000000000000000, 0.000000000000000000 ) ) ;
#2498 = EDGE_CURVE ( 'NONE', #84368, #168899, #30849, .T. ) ;
#2499 = DIRECTION ( 'NONE',  ( -1.000000000000000000, 0.000000000000000000, 0.000000000000000000 ) ) ;
#2500 = DIRECTION ( 'NONE',  ( 1.000000000000000000, 0.000000000000000000, 0.000000000000000000 ) ) ;
#2501 = AXIS2_PLACEMENT_3D ( 'NONE', #233664, #34202, #113703 ) ;
#2502 = ORIENTED_EDGE ( 'NONE', *, *, #189485, .F. ) ;
#2503 = DIRECTION ( 'NONE',  ( 0.000000000000000000, 0.000000000000000000, -1.000000000000000000 ) ) ;
#2504 = EDGE_CURVE ( 'NONE', #75643, #187772, #112330, .T. ) ;
#2505 = APPLICATION_PROTOCOL_DEFINITION ( 'draft international standard', 'automotive_design', 1998, #97263 ) ;
#2506 = ADVANCED_FACE ( 'NONE', ( #178670 ), #80787, .T. ) ;
#2507 = CARTESIAN_POINT ( 'NONE',  ( -20.85000000000000142, -1.835859311443637010, -45.00443916879852679 ) ) ;
#2508 = VERTEX_POINT ( 'NONE', #182504 ) ;
#2509 = DIRECTION ( 'NONE',  ( 0.000000000000000000, 0.000000000000000000, 1.000000000000000000 ) ) ;
#2510 = CARTESIAN_POINT ( 'NONE',  ( -21.04999999999994387, 67.75000000001118394, -51.02310748452479316 ) ) ;
#2511 = ADVANCED_FACE ( 'NONE', ( #122524 ), #134841, .F. ) ;
#2512 = CARTESIAN_POINT ( 'NONE',  ( -16.97683809663752186, 66.15000000001158753, -56.87310748452438958 ) ) ;
#2513 = ORIENTED_EDGE ( 'NONE', *, *, #212335, .F. ) ;
#2514 = AXIS2_PLACEMENT_3D ( 'NONE', #52057, #252836, #131610 ) ;
#2515 = ORIENTED_EDGE ( 'NONE', *, *, #16126, .T. ) ;
#2516 = EDGE_CURVE ( 'NONE', #85055, #23218, #43308, .T. ) ;
#2517 = FACE_OUTER_BOUND ( 'NONE', #218625, .T. ) ;
#2518 = ADVANCED_FACE ( 'NONE', ( #22149 ), #239113, .F. ) ;
#2519 = DIRECTION ( 'NONE',  ( -0.7071067811865456854, 0.7071067811865493491, 0.000000000000000000 ) ) ;
#2520 = CARTESIAN_POINT ( 'NONE',  ( 18.49999999999999289, 11.65000000001115943, -21.75000000000000355 ) ) ;
#2521 = FACE_OUTER_BOUND ( 'NONE', #50200, .T. ) ;
#2522 = DIRECTION ( 'NONE',  ( 2.952720810173289112E-16, -1.000000000000000000, -0.000000000000000000 ) ) ;
#2523 = DIRECTION ( 'NONE',  ( 0.000000000000000000, 0.9908441862701605762, -0.1350103645451835310 ) ) ;
#2525 = DIRECTION ( 'NONE',  ( 1.000000000000000000, 0.000000000000000000, 0.000000000000000000 ) ) ;
#2524 = CARTESIAN_POINT ( 'NONE',  ( 22.00356870141732912, 7.254242362486300166, -3.773983934443023074E-12 ) ) ;
#2526 = CARTESIAN_POINT ( 'NONE',  ( 20.46382478191414833, 40.81860725232441922, -237.9338882589013053 ) ) ;
#2527 = CARTESIAN_POINT ( 'NONE',  ( -23.25000000000000000, 1.115600667400684642E-11, -67.00000000000000000 ) ) ;
#2528 = CARTESIAN_POINT ( 'NONE',  ( 22.47809213839789066, 0.03753706763967752658, -155.8500266652121695 ) ) ;
#2529 = DIRECTION ( 'NONE',  ( 1.000000000000000000, -0.000000000000000000, -0.000000000000000000 ) ) ;
#2530 = TOROIDAL_SURFACE ( 'NONE', #143999, 0.4000000000000009104, 0.1000000000000000056 ) ;
#2531 = EDGE_LOOP ( 'NONE', ( #116566, #111181, #239458, #229281, #15993, #112213, #10452, #49800, #222333, #180469 ) ) ;
#2532 = AXIS2_PLACEMENT_3D ( 'NONE', #196465, #218584, #174399 ) ;
#2533 = ORIENTED_EDGE ( 'NONE', *, *, #140585, .F. ) ;
#2534 = AXIS2_PLACEMENT_3D ( 'NONE', #101667, #222921, #181265 ) ;
#2535 = CIRCLE ( 'NONE', #81614, 0.09999999999999534261 ) ;
#2536 = CARTESIAN_POINT ( 'NONE',  ( -18.59999999999999787, 9.350000000000001421, -21.25000000000000000 ) ) ;
#2538 = CARTESIAN_POINT ( 'NONE',  ( 21.12802099929860944, 67.21944740979039068, -191.2749174995927888 ) ) ;
#2537 = DIRECTION ( 'NONE',  ( 1.000000000000000000, 0.000000000000000000, 0.000000000000000000 ) ) ;
#2539 = ADVANCED_FACE ( 'NONE', ( #24724 ), #47377, .T. ) ;
#2540 = CARTESIAN_POINT ( 'NONE',  ( 21.05000000000000071, -8.999999999988842703, -57.50603087734755547 ) ) ;
#2542 = EDGE_CURVE ( 'NONE', #72588, #174999, #143249, .T. ) ;
#2541 = DIRECTION ( 'NONE',  ( 1.000000000000000000, 0.000000000000000000, 0.000000000000000000 ) ) ;
#2543 = DIRECTION ( 'NONE',  ( -1.000000000000000000, -0.000000000000000000, -0.000000000000000000 ) ) ;
#2544 = ORIENTED_EDGE ( 'NONE', *, *, #30633, .F. ) ;
#2545 = DIRECTION ( 'NONE',  ( -1.000000000000000000, 0.000000000000000000, 0.000000000000000000 ) ) ;
#2546 = EDGE_LOOP ( 'NONE', ( #121682, #240910, #99758, #98790 ) ) ;
#2548 = ADVANCED_FACE ( 'NONE', ( #119975 ), #159831, .T. ) ;
#2547 = B_SPLINE_CURVE_WITH_KNOTS ( 'NONE', 3,
 ( #96098, #113115, #135226, #115685, #231794, #195248, #14028, #92254, #32325, #250060, #133949, #71442, #51832, #111841, #233089, #175670, #212235, #230501, #251326, #131387, #153577, #191402, #173141, #213490, #36162, #54419 ),
 .UNSPECIFIED., .F., .F.,
 ( 4, 2, 2, 2, 2, 2, 2, 2, 2, 2, 2, 2, 4 ),
 ( 0.005476422646581349113, 0.006160811967703589548, 0.006845201288825829983, 0.007187395949386920710, 0.007529590609948011437, 0.007871785270509102164, 0.008213979931070192891, 0.008556174591631285353, 0.008898369252192376080, 0.009240563912753466808, 0.009582758573314557535, 0.01026714789443679797, 0.01095153721555903840 ),
 .UNSPECIFIED. ) ;
#2549 = DIRECTION ( 'NONE',  ( 1.000000000000000000, 0.000000000000000000, 0.000000000000000000 ) ) ;
#2550 = AXIS2_PLACEMENT_3D ( 'NONE', #27538, #164451, #167043 ) ;
#2551 = ORIENTED_EDGE ( 'NONE', *, *, #36169, .F. ) ;
#2552 = DIRECTION ( 'NONE',  ( -1.000000000000000000, 0.000000000000000000, 0.000000000000000000 ) ) ;
#2553 = AXIS2_PLACEMENT_3D ( 'NONE', #217952, #178894, #254505 ) ;
#2554 = CARTESIAN_POINT ( 'NONE',  ( -23.25000000000000000, 67.23127455305841238, -235.8551265064783991 ) ) ;
#2555 = AXIS2_PLACEMENT_3D ( 'NONE', #240546, #38496, #121896 ) ;
#2556 = ORIENTED_EDGE ( 'NONE', *, *, #177322, .F. ) ;
#2557 = CARTESIAN_POINT ( 'NONE',  ( 21.05000000000000071, 69.35000000001159037, -59.67928539484125139 ) ) ;
#2558 = ORIENTED_EDGE ( 'NONE', *, *, #78435, .T. ) ;
#2559 = CARTESIAN_POINT ( 'NONE',  ( 18.52928932188133970, 10.27928932189250411, -192.1499999999999488 ) ) ;
#2560 = CARTESIAN_POINT ( 'NONE',  ( -22.00411653962182967, 68.74655713164163728, -69.62214559032503303 ) ) ;
#2561 = CARTESIAN_POINT ( 'NONE',  ( -22.10000000000000142, -11.64999999999999858, 12.09999999999999609 ) ) ;
#2562 = EDGE_CURVE ( 'NONE', #68348, #25415, #220338, .T. ) ;
#2563 = CARTESIAN_POINT ( 'NONE',  ( 20.95512820512820440, 67.12384868372420499, -161.4644784893834810 ) ) ;
#2564 = DIRECTION ( 'NONE',  ( 1.000000000000000000, 5.204170427930452838E-14, 0.000000000000000000 ) ) ;
#2566 = FACE_OUTER_BOUND ( 'NONE', #144052, .T. ) ;
#2565 = CARTESIAN_POINT ( 'NONE',  ( 18.59999999999999076, 1.115600667400684642E-11, -134.0000000000000284 ) ) ;
#2567 = CARTESIAN_POINT ( 'NONE',  ( -21.05000000000000071, 76.00000000001192291, -98.72310748452436258 ) ) ;
#2568 = ADVANCED_FACE ( 'NONE', ( #222880 ), #65099, .F. ) ;
#2570 = ORIENTED_EDGE ( 'NONE', *, *, #217766, .T. ) ;
#2569 = CARTESIAN_POINT ( 'NONE',  ( 21.06490991615909891, 65.27510865242548732, -191.3193961309912936 ) ) ;
#2572 = CARTESIAN_POINT ( 'NONE',  ( 20.94999999999999929, 4.813084112160680661, -145.9415177565238366 ) ) ;
#2571 = DIRECTION ( 'NONE',  ( 0.000000000000000000, -1.000000000000000000, 0.000000000000000000 ) ) ;
#2573 = ORIENTED_EDGE ( 'NONE', *, *, #145484, .F. ) ;
#2575 = ORIENTED_EDGE ( 'NONE', *, *, #27769, .F. ) ;
#2574 = LINE ( 'NONE', #182534, #181703 ) ;
#2576 = CIRCLE ( 'NONE', #152651, 0.1000000000000028644 ) ;
#2577 = VERTEX_POINT ( 'NONE', #79510 ) ;
#2578 = CYLINDRICAL_SURFACE ( 'NONE', #140824, 0.1000000000000028644 ) ;
#2579 = CARTESIAN_POINT ( 'NONE',  ( 21.05000000000000071, 64.35000000001204512, -124.3731074845243825 ) ) ;
#2580 = CARTESIAN_POINT ( 'NONE',  ( -18.59999999999999787, 85.32100840337290037, -62.28716923544637751 ) ) ;
#2581 = ADVANCED_FACE ( 'NONE', ( #59942 ), #102922, .T. ) ;
#2582 = ORIENTED_EDGE ( 'NONE', *, *, #162361, .T. ) ;
#2583 = EDGE_CURVE ( 'NONE', #117760, #218080, #180668, .T. ) ;
#2584 = DIRECTION ( 'NONE',  ( 0.000000000000000000, -0.4721928772777346794, -0.8814952561688431665 ) ) ;
#2585 = DIRECTION ( 'NONE',  ( 7.304098846218134667E-16, 1.000000000000000000, 6.982962677686266711E-15 ) ) ;
#2586 = DIRECTION ( 'NONE',  ( 0.000000000000000000, 1.000000000000000000, 0.000000000000000000 ) ) ;
#2587 = ADVANCED_FACE ( 'NONE', ( #7543 ), #6245, .F. ) ;
#2588 = CARTESIAN_POINT ( 'NONE',  ( -37.88850191057539973, 11.75000000000000000, 6.000000000000001776 ) ) ;
#2589 = CARTESIAN_POINT ( 'NONE',  ( -18.51697539158857353, 46.41023286455060060, -243.0722154975327385 ) ) ;
#2591 = AXIS2_PLACEMENT_3D ( 'NONE', #61545, #237618, #58937 ) ;
#2590 = CARTESIAN_POINT ( 'NONE',  ( 21.08621493067296271, 69.65070570884047640, -136.5793023240004516 ) ) ;
#2592 = ORIENTED_EDGE ( 'NONE', *, *, #199882, .F. ) ;
#2593 = ORIENTED_EDGE ( 'NONE', *, *, #35173, .F. ) ;
#2594 = CARTESIAN_POINT ( 'NONE',  ( -20.85000000000000142, 1.115600667400684642E-11, -200.9999999999999432 ) ) ;
#2595 = AXIS2_PLACEMENT_3D ( 'NONE', #95829, #133693, #234071 ) ;
#2596 = CIRCLE ( 'NONE', #148357, 0.09999999999999939493 ) ;
#2597 = EDGE_CURVE ( 'NONE', #123515, #187371, #193161, .T. ) ;
#2598 = VERTEX_POINT ( 'NONE', #11410 ) ;
#2599 = DIRECTION ( 'NONE',  ( 1.000000000000000000, 0.000000000000000000, -0.000000000000000000 ) ) ;
#2601 = ADVANCED_FACE ( 'NONE', ( #107928 ), #145756, .F. ) ;
#2600 = ORIENTED_EDGE ( 'NONE', *, *, #135602, .T. ) ;
#2602 = CARTESIAN_POINT ( 'NONE',  ( 20.94403535211772294, 10.30632246271647467, -173.0041836778896140 ) ) ;
#2603 = DIRECTION ( 'NONE',  ( 0.000000000000000000, -1.000000000000000000, 0.000000000000000000 ) ) ;
#2604 = CARTESIAN_POINT ( 'NONE',  ( -20.94999999999999929, 76.00000000001142553, -36.02310748452432421 ) ) ;
#2605 = EDGE_CURVE ( 'NONE', #26511, #77835, #89078, .T. ) ;
#2606 = FACE_OUTER_BOUND ( 'NONE', #58765, .T. ) ;
#2607 = LINE ( 'NONE', #161720, #199608 ) ;
#2608 = EDGE_LOOP ( 'NONE', ( #130509, #146115, #19721, #209502 ) ) ;
#2609 = DIRECTION ( 'NONE',  ( 0.000000000000000000, -1.000000000000000000, 0.000000000000000000 ) ) ;
#2610 = DIRECTION ( 'NONE',  ( -7.304098846218134667E-16, 1.000000000000000000, 6.982962677686266711E-15 ) ) ;
#2611 = DIRECTION ( 'NONE',  ( 1.000000000000000000, 0.000000000000000000, 0.000000000000000000 ) ) ;
#2613 = ORIENTED_EDGE ( 'NONE', *, *, #204326, .F. ) ;
#2612 = ADVANCED_FACE ( 'NONE', ( #165342 ), #167937, .F. ) ;
#2615 = CARTESIAN_POINT ( 'NONE',  ( 21.14999999999999858, 60.94483358488582070, -234.0465764481390636 ) ) ;
#2614 = DIRECTION ( 'NONE',  ( 0.000000000000000000, -7.109473446599835262E-15, 1.000000000000000000 ) ) ;
#2616 = AXIS2_PLACEMENT_3D ( 'NONE', #17562, #59224, #140067 ) ;
#2617 = VERTEX_POINT ( 'NONE', #67513 ) ;
#2619 = VERTEX_POINT ( 'NONE', #204448 ) ;
#2618 = DIRECTION ( 'NONE',  ( -1.000000000000000000, -0.000000000000000000, -0.000000000000000000 ) ) ;
#2620 = ORIENTED_EDGE ( 'NONE', *, *, #144929, .T. ) ;
#2621 = CARTESIAN_POINT ( 'NONE',  ( -21.05000000000000071, 11.65000000001115588, -59.98519422934605672 ) ) ;
#2622 = CARTESIAN_POINT ( 'NONE',  ( -18.59999999999999787, -1.164121893241208960, -41.41484808557160591 ) ) ;
#2623 = EDGE_CURVE ( 'NONE', #8256, #229929, #114010, .T. ) ;
#2624 = CYLINDRICAL_SURFACE ( 'NONE', #233334, 0.09999999999999990841 ) ;
#2625 = VERTEX_POINT ( 'NONE', #229171 ) ;
#2626 = DIRECTION ( 'NONE',  ( 1.000000000000000000, -0.000000000000000000, 0.000000000000000000 ) ) ;
#2627 = CARTESIAN_POINT ( 'NONE',  ( -20.94999999999999929, 72.02722222756958104, -225.1832529173024398 ) ) ;
#2628 = ADVANCED_FACE ( 'NONE', ( #243589 ), #18362, .F. ) ;
#2629 = CIRCLE ( 'NONE', #44168, 0.1000000000000133560 ) ;
#2631 = DIRECTION ( 'NONE',  ( 0.000000000000000000, 0.2617529984165152257, 0.9651348961777124202 ) ) ;
#2630 = DIRECTION ( 'NONE',  ( 0.000000000000000000, 0.000000000000000000, 1.000000000000000000 ) ) ;
#2632 = CIRCLE ( 'NONE', #239986, 0.1000000000000046685 ) ;
#2633 = EDGE_CURVE ( 'NONE', #164361, #241144, #126198, .T. ) ;
#2635 = ORIENTED_EDGE ( 'NONE', *, *, #233065, .T. ) ;
#2634 = CARTESIAN_POINT ( 'NONE',  ( -16.97683809663752186, 9.949999999999983302, -9.250000000000001776 ) ) ;
#2636 = VERTEX_POINT ( 'NONE', #186191 ) ;
#2637 = CARTESIAN_POINT ( 'NONE',  ( 22.60000000000000142, -2.401771312552908544, -189.4980873520049727 ) ) ;
#2638 = AXIS2_PLACEMENT_3D ( 'NONE', #39934, #217235, #235526 ) ;
#2639 = DIRECTION ( 'NONE',  ( 1.000000000000000000, -7.304098846218133681E-16, 4.217023435051677994E-16 ) ) ;
#2640 = ORIENTED_EDGE ( 'NONE', *, *, #159471, .F. ) ;
#2642 = TOROIDAL_SURFACE ( 'NONE', #31902, 4.149999999999999467, 0.1000000000000000056 ) ;
#2641 = DIRECTION ( 'NONE',  ( 0.000000000000000000, -1.000000000000000000, -6.982962677686265922E-15 ) ) ;
#2643 = ORIENTED_EDGE ( 'NONE', *, *, #100367, .F. ) ;
#2644 = CIRCLE ( 'NONE', #144266, 7.900000000000003908 ) ;
#2645 = CARTESIAN_POINT ( 'NONE',  ( -23.25000000000000000, 74.00000000001223555, -149.1477294072864765 ) ) ;
#2647 = EDGE_CURVE ( 'NONE', #234687, #108265, #87058, .T. ) ;
#2646 = CARTESIAN_POINT ( 'NONE',  ( 22.40000000000020819, 76.10085836911169110, -114.7726746080140146 ) ) ;
#2648 = FACE_OUTER_BOUND ( 'NONE', #40487, .T. ) ;
#2650 = ORIENTED_EDGE ( 'NONE', *, *, #214883, .T. ) ;
#2649 = VECTOR ( 'NONE', #232974, 1000.000000000000000 ) ;
#2651 = CARTESIAN_POINT ( 'NONE',  ( -23.15000000000000213, 36.65892442174472876, -249.5511627012454596 ) ) ;
#2652 = ADVANCED_FACE ( 'NONE', ( #85757 ), #246160, .T. ) ;
#2653 = VECTOR ( 'NONE', #183279, 1000.000000000000227 ) ;
#2654 = CARTESIAN_POINT ( 'NONE',  ( 18.49999999999999289, 65.79142135624952914, -148.2731074845243882 ) ) ;
#2655 = ORIENTED_EDGE ( 'NONE', *, *, #161876, .T. ) ;
#2656 = ORIENTED_EDGE ( 'NONE', *, *, #25519, .F. ) ;
#2657 = ORIENTED_EDGE ( 'NONE', *, *, #53200, .F. ) ;
#2658 = CARTESIAN_POINT ( 'NONE',  ( -18.50000000000000711, 38.29773864426884700, -236.0513742605307925 ) ) ;
#2659 = EDGE_CURVE ( 'NONE', #97694, #95409, #97427, .T. ) ;
#2660 = ORIENTED_EDGE ( 'NONE', *, *, #171683, .T. ) ;
#2662 = EDGE_LOOP ( 'NONE', ( #255372, #111312, #30213, #95104, #189538, #13881, #156912, #145096 ) ) ;
#2661 = LINE ( 'NONE', #164332, #59484 ) ;
#2663 = ORIENTED_EDGE ( 'NONE', *, *, #228153, .T. ) ;
#2664 = VECTOR ( 'NONE', #201479, 1000.000000000000000 ) ;
#2665 = CIRCLE ( 'NONE', #36012, 6.258578643762701788 ) ;
#2668 = ORIENTED_EDGE ( 'NONE', *, *, #5102, .F. ) ;
#2667 = ORIENTED_EDGE ( 'NONE', *, *, #152205, .F. ) ;
#2666 = CARTESIAN_POINT ( 'NONE',  ( 18.52130828395272033, 78.22078591447844076, -231.5573136408083030 ) ) ;
#2669 = CIRCLE ( 'NONE', #19250, 0.1000000000000028644 ) ;
#2670 = AXIS2_PLACEMENT_3D ( 'NONE', #120402, #242876, #241594 ) ;
#2671 = ORIENTED_EDGE ( 'NONE', *, *, #59711, .T. ) ;
#2672 = LINE ( 'NONE', #84747, #218888 ) ;
#2673 = EDGE_CURVE ( 'NONE', #1805, #203569, #247284, .T. ) ;
#2674 = CARTESIAN_POINT ( 'NONE',  ( 20.94999999999999929, 64.35000000001176090, -76.30697314750248950 ) ) ;
#2675 = AXIS2_PLACEMENT_3D ( 'NONE', #151542, #152833, #15885 ) ;
#2676 = CARTESIAN_POINT ( 'NONE',  ( -16.87683809663752399, 13.90118822005493016, -218.5412211127979845 ) ) ;
#2677 = ORIENTED_EDGE ( 'NONE', *, *, #225088, .T. ) ;
#2678 = DIRECTION ( 'NONE',  ( 0.000000000000000000, 1.224646799142185182E-16, 1.000000000000000000 ) ) ;
#2680 = ORIENTED_EDGE ( 'NONE', *, *, #249182, .F. ) ;
#2679 = CARTESIAN_POINT ( 'NONE',  ( 20.95512820512820440, 10.62384868372303615, -108.1649135690876449 ) ) ;
#2681 = CARTESIAN_POINT ( 'NONE',  ( -23.15000000000000213, -8.999999999988844479, -91.10603087734760663 ) ) ;
#2683 = ORIENTED_EDGE ( 'NONE', *, *, #33531, .T. ) ;
#2682 = DIRECTION ( 'NONE',  ( 0.000000000000000000, 6.938893903907222067E-15, -1.000000000000000000 ) ) ;
#2684 = CIRCLE ( 'NONE', #215083, 0.1000000000000028644 ) ;
#2685 = EDGE_LOOP ( 'NONE', ( #83981, #123688, #240456, #190334 ) ) ;
#2686 = AXIS2_PLACEMENT_3D ( 'NONE', #214499, #68931, #227984 ) ;
#2687 = CARTESIAN_POINT ( 'NONE',  ( -20.85000000000000142, -1.835859311443637010, -45.00443916879852679 ) ) ;
#2688 = CIRCLE ( 'NONE', #231670, 0.1999999999999987899 ) ;
#2689 = ORIENTED_EDGE ( 'NONE', *, *, #84996, .T. ) ;
#2690 = VERTEX_POINT ( 'NONE', #49234 ) ;
#2691 = CARTESIAN_POINT ( 'NONE',  ( -16.92280123533699054, 9.950000000011137047, -180.3506323140850611 ) ) ;
#2692 = DIRECTION ( 'NONE',  ( 0.000000000000000000, -7.272083257015735086E-15, 1.000000000000000000 ) ) ;
#2694 = VERTEX_POINT ( 'NONE', #64942 ) ;
#2693 = ORIENTED_EDGE ( 'NONE', *, *, #252232, .F. ) ;
#2695 = ORIENTED_EDGE ( 'NONE', *, *, #60445, .F. ) ;
#2696 = DIRECTION ( 'NONE',  ( -1.000000000000000000, 0.000000000000000000, 0.000000000000000000 ) ) ;
#2697 = VERTEX_POINT ( 'NONE', #109196 ) ;
#2698 = ORIENTED_EDGE ( 'NONE', *, *, #100935, .F. ) ;
#2699 = DIRECTION ( 'NONE',  ( -1.000000000000000000, -0.000000000000000000, -0.000000000000000000 ) ) ;
#2700 = AXIS2_PLACEMENT_3D ( 'NONE', #38627, #98548, #19057 ) ;
#2702 = ORIENTED_EDGE ( 'NONE', *, *, #97833, .T. ) ;
#2701 = CARTESIAN_POINT ( 'NONE',  ( -18.59999999999999787, 64.35000000001150511, -48.17310748452440095 ) ) ;
#2703 = CARTESIAN_POINT ( 'NONE',  ( -20.54999999999999716, 74.00000000001180922, -82.34772940728642254 ) ) ;
#2704 = CARTESIAN_POINT ( 'NONE',  ( 18.59999999999999076, 16.64998792410002793, -222.7039835543563981 ) ) ;
#2705 = VERTEX_POINT ( 'NONE', #188744 ) ;
#2706 = EDGE_CURVE ( 'NONE', #12615, #103845, #230754, .T. ) ;
#2708 = VERTEX_POINT ( 'NONE', #45387 ) ;
#2707 = ORIENTED_EDGE ( 'NONE', *, *, #230430, .F. ) ;
#2709 = CARTESIAN_POINT ( 'NONE',  ( -18.59999999999999787, 66.85000000001186038, -90.67310748452436542 ) ) ;
#2710 = EDGE_LOOP ( 'NONE', ( #128396, #175451, #183466, #19069 ) ) ;
#2711 = AXIS2_PLACEMENT_3D ( 'NONE', #47359, #90346, #129493 ) ;
#2712 = AXIS2_PLACEMENT_3D ( 'NONE', #235282, #39692, #98306 ) ;
#2713 = CIRCLE ( 'NONE', #152790, 0.4000000000000114575 ) ;
#2714 = AXIS2_PLACEMENT_3D ( 'NONE', #96080, #238160, #814 ) ;
#2715 = CARTESIAN_POINT ( 'NONE',  ( -18.49499033040906326, 85.43814877175658751, -95.82495425860084026 ) ) ;
#2716 = ORIENTED_EDGE ( 'NONE', *, *, #55006, .T. ) ;
#2717 = ORIENTED_EDGE ( 'NONE', *, *, #109385, .T. ) ;
#2718 = ADVANCED_FACE ( 'NONE', ( #169225 ), #124935, .F. ) ;
#2719 = CARTESIAN_POINT ( 'NONE',  ( -23.15000000000000213, 2.000000000011154189, -187.7753780772378889 ) ) ;
#2720 = ORIENTED_EDGE ( 'NONE', *, *, #35424, .T. ) ;
#2721 = CARTESIAN_POINT ( 'NONE',  ( -20.54999999999999716, 2.500000000011154633, -154.2753780772379173 ) ) ;
#2722 = ORIENTED_EDGE ( 'NONE', *, *, #35767, .T. ) ;
#2723 = LINE ( 'NONE', #255733, #156151 ) ;
#2724 = CARTESIAN_POINT ( 'NONE',  ( -17.73285935861207818, 10.85798180380284528, -43.74143819021772828 ) ) ;
#2725 = FACE_OUTER_BOUND ( 'NONE', #118331, .T. ) ;
#2726 = EDGE_CURVE ( 'NONE', #168716, #81862, #139119, .T. ) ;
#2727 = CARTESIAN_POINT ( 'NONE',  ( 18.59999999999999432, -1.299733671219632791, -57.02812952286944892 ) ) ;
#2728 = CARTESIAN_POINT ( 'NONE',  ( 21.05000000000000071, 67.23127455305835554, -235.8551265064784559 ) ) ;
#2729 = CARTESIAN_POINT ( 'NONE',  ( -21.59142135623730852, 68.15000000001259650, -191.1731074845243938 ) ) ;
#2730 = DIRECTION ( 'NONE',  ( -0.7071067811865475727, -0.7071067811865475727, 0.000000000000000000 ) ) ;
#2731 = CARTESIAN_POINT ( 'NONE',  ( -22.50000000000000000, 76.00000000001169553, -75.77310748452431710 ) ) ;
#2732 = AXIS2_PLACEMENT_3D ( 'NONE', #99635, #38413, #241744 ) ;
#2733 = VECTOR ( 'NONE', #35224, 1000.000000000000000 ) ;
#2734 = CIRCLE ( 'NONE', #31990, 11.75000000000000000 ) ;
#2735 = ADVANCED_FACE ( 'NONE', ( #94776 ), #154785, .F. ) ;
#2736 = ORIENTED_EDGE ( 'NONE', *, *, #106681, .F. ) ;
#2737 = EDGE_CURVE ( 'NONE', #240443, #222464, #47177, .T. ) ;
#2739 = ORIENTED_EDGE ( 'NONE', *, *, #38621, .F. ) ;
#2738 = ORIENTED_EDGE ( 'NONE', *, *, #83930, .T. ) ;
#2740 = AXIS2_PLACEMENT_3D ( 'NONE', #72863, #152397, #35025 ) ;
#2741 = ORIENTED_EDGE ( 'NONE', *, *, #20241, .F. ) ;
#2742 = ADVANCED_FACE ( 'NONE', ( #55617 ), #76610, .T. ) ;
#2743 = CARTESIAN_POINT ( 'NONE',  ( -18.70000000000000284, 7.900000000000000355, 1.212568896937007867 ) ) ;
#2744 = CARTESIAN_POINT ( 'NONE',  ( -16.87036670365548474, 66.01058118071016168, -82.04354736722233099 ) ) ;
#2745 = EDGE_CURVE ( 'NONE', #179633, #22197, #6536, .T. ) ;
#2747 = DIRECTION ( 'NONE',  ( 1.000000000000000000, 0.000000000000000000, 0.000000000000000000 ) ) ;
#2746 = DIRECTION ( 'NONE',  ( 0.000000000000000000, 0.1575844902526727098, 0.9875055080513754913 ) ) ;
#2748 = FACE_OUTER_BOUND ( 'NONE', #33714, .T. ) ;
#2749 = ORIENTED_EDGE ( 'NONE', *, *, #142897, .T. ) ;
#2750 = CARTESIAN_POINT ( 'NONE',  ( -20.93302460841142931, 10.31565961587945424, -106.0364194119178620 ) ) ;
#2751 = PLANE ( 'NONE',  #12742 ) ;
#2752 = EDGE_CURVE ( 'NONE', #2577, #216685, #164118, .T. ) ;
#2753 = CARTESIAN_POINT ( 'NONE',  ( 20.85000000000000142, 43.00579525902548994, -254.2551217332645876 ) ) ;
#2754 = DIRECTION ( 'NONE',  ( 0.000000000000000000, 0.000000000000000000, 1.000000000000000000 ) ) ;
#2755 = ORIENTED_EDGE ( 'NONE', *, *, #163487, .F. ) ;
#2756 = CIRCLE ( 'NONE', #211066, 4.049999999999999822 ) ;
#2757 = CARTESIAN_POINT ( 'NONE',  ( -18.59999999999999787, 9.350000000011156942, -188.6499999999999488 ) ) ;
#2758 = CARTESIAN_POINT ( 'NONE',  ( -21.11833042828134310, 0.007100509070570094547, -94.05435530614481365 ) ) ;
#2759 = ORIENTED_EDGE ( 'NONE', *, *, #250214, .T. ) ;
#2760 = CARTESIAN_POINT ( 'NONE',  ( 21.05000000000000071, -8.999999999988842703, -91.10603087734760663 ) ) ;
#2761 = LINE ( 'NONE', #241405, #44575 ) ;
#2762 = CARTESIAN_POINT ( 'NONE',  ( -18.59999999999999787, 9.350000000011156942, -112.7500000000000284 ) ) ;
#2763 = FACE_OUTER_BOUND ( 'NONE', #129096, .T. ) ;
#2764 = CIRCLE ( 'NONE', #86316, 0.1000000000000028644 ) ;
#2765 = CARTESIAN_POINT ( 'NONE',  ( -17.78241384942186087, 10.85557575278904352, -23.25096232753543646 ) ) ;
#2766 = VERTEX_POINT ( 'NONE', #37396 ) ;
#2767 = LINE ( 'NONE', #5320, #211110 ) ;
#2768 = CARTESIAN_POINT ( 'NONE',  ( 20.94999999999999929, 77.13501884592184865, -61.80613060109197932 ) ) ;
#2770 = ADVANCED_FACE ( 'NONE', ( #12709, #51783 ), #92205, .T. ) ;
#2769 = CARTESIAN_POINT ( 'NONE',  ( -21.05000000000000071, -0.01771943329742826576, -60.55891531152861518 ) ) ;
#2772 = DIRECTION ( 'NONE',  ( 4.239556034732056743E-17, -0.1298341882520022972, -0.9915357197604853789 ) ) ;
#2771 = DIRECTION ( 'NONE',  ( 1.000000000000000000, 0.000000000000000000, 0.000000000000000000 ) ) ;
#2773 = CARTESIAN_POINT ( 'NONE',  ( -18.59999999999999787, 85.52395432076518489, -163.1410904276970086 ) ) ;
#2774 = CIRCLE ( 'NONE', #236010, 0.09999999999999990841 ) ;
#2775 = CYLINDRICAL_SURFACE ( 'NONE', #125101, 0.1000000000000075273 ) ;
#2776 = CARTESIAN_POINT ( 'NONE',  ( -21.05000000000000071, 1.261786168565025568, -8.086498963545480478 ) ) ;
#2777 = PLANE ( 'NONE',  #123368 ) ;
#2778 = CIRCLE ( 'NONE', #52842, 11.80000000000000959 ) ;
#2779 = ORIENTED_EDGE ( 'NONE', *, *, #64412, .F. ) ;
#2780 = AXIS2_PLACEMENT_3D ( 'NONE', #255033, #59429, #56866 ) ;
#2782 = ORIENTED_EDGE ( 'NONE', *, *, #180395, .F. ) ;
#2781 = AXIS2_PLACEMENT_3D ( 'NONE', #163197, #124074, #207464 ) ;
#2783 = EDGE_CURVE ( 'NONE', #47266, #80413, #231741, .T. ) ;
#2784 = PLANE ( 'NONE',  #133343 ) ;
#2785 = CARTESIAN_POINT ( 'NONE',  ( -18.52643265882458579, 65.68026841930851845, -30.47257401318894310 ) ) ;
#2786 = ADVANCED_FACE ( 'NONE', ( #171790 ), #135175, .T. ) ;
#2787 = CARTESIAN_POINT ( 'NONE',  ( -12.25000000000000178, 9.850000000011133849, -83.75000000000004263 ) ) ;
#2788 = CIRCLE ( 'NONE', #27787, 0.6000000000000005329 ) ;
#2789 = VERTEX_POINT ( 'NONE', #15265 ) ;
#2790 = EDGE_CURVE ( 'NONE', #26749, #121900, #118323, .T. ) ;
#2791 = CARTESIAN_POINT ( 'NONE',  ( -23.15000000000000213, 64.35000000001254250, -182.1731074845244507 ) ) ;
#2792 = CIRCLE ( 'NONE', #210918, 11.70000000000000284 ) ;
#2793 = DIRECTION ( 'NONE',  ( -1.000000000000000000, 0.000000000000000000, 0.000000000000000000 ) ) ;
#2794 = CARTESIAN_POINT ( 'NONE',  ( -23.25000000000000000, 25.97741635855165754, -254.4468634167653249 ) ) ;
#2795 = VECTOR ( 'NONE', #83860, 1000.000000000000000 ) ;
#2796 = ORIENTED_EDGE ( 'NONE', *, *, #159102, .F. ) ;
#2797 = LINE ( 'NONE', #40703, #158002 ) ;
#2800 = VERTEX_POINT ( 'NONE', #16546 ) ;
#2799 = DIRECTION ( 'NONE',  ( 1.000000000000000000, 3.265361837132813093E-16, -0.000000000000000000 ) ) ;
#2798 = VECTOR ( 'NONE', #76671, 1000.000000000000000 ) ;
#2802 = DIRECTION ( 'NONE',  ( 0.000000000000000000, -0.9908441862701605762, -0.1350103645451835310 ) ) ;
#2801 = CARTESIAN_POINT ( 'NONE',  ( 20.27550659511088682, 9.216043722520002035, -143.2500000000000284 ) ) ;
#2803 = CARTESIAN_POINT ( 'NONE',  ( 20.30531438145591139, 65.90309893892226967, -162.2270896772506035 ) ) ;
#2804 = EDGE_CURVE ( 'NONE', #58858, #117566, #146462, .T. ) ;
#2805 = VECTOR ( 'NONE', #224862, 1000.000000000000000 ) ;
#2806 = PLANE ( 'NONE',  #25318 ) ;
#2808 = ORIENTED_EDGE ( 'NONE', *, *, #180461, .F. ) ;
#2807 = AXIS2_PLACEMENT_3D ( 'NONE', #76164, #209263, #13640 ) ;
#2809 = EDGE_CURVE ( 'NONE', #248652, #118509, #193150, .T. ) ;
#2810 = CARTESIAN_POINT ( 'NONE',  ( 0.000000000000000000, 0.000000000000000000, 0.000000000000000000 ) ) ;
#2811 = CARTESIAN_POINT ( 'NONE',  ( 18.59999999999999076, 34.53503747617446606, -235.1972745784239578 ) ) ;
#2812 = EDGE_CURVE ( 'NONE', #113855, #9346, #20397, .T. ) ;
#2813 = EDGE_LOOP ( 'NONE', ( #157991, #36685, #88276, #78622 ) ) ;
#2814 = DIRECTION ( 'NONE',  ( 0.000000000000000000, 0.4721928772777346239, 0.8814952561688430555 ) ) ;
#2815 = AXIS2_PLACEMENT_3D ( 'NONE', #94429, #119149, #18750 ) ;
#2816 = DIRECTION ( 'NONE',  ( 1.000000000000000000, -1.207181226542539700E-16, 2.694675058168174199E-16 ) ) ;
#2817 = VECTOR ( 'NONE', #17607, 1000.000000000000000 ) ;
#2818 = ADVANCED_FACE ( 'NONE', ( #179474 ), #193519, .T. ) ;
#2819 = FACE_OUTER_BOUND ( 'NONE', #252833, .T. ) ;
#2820 = DIRECTION ( 'NONE',  ( 1.000000000000000000, 0.000000000000000000, 0.000000000000000000 ) ) ;
#2821 = VERTEX_POINT ( 'NONE', #200302 ) ;
#2822 = VERTEX_POINT ( 'NONE', #38663 ) ;
#2823 = CYLINDRICAL_SURFACE ( 'NONE', #111142, 0.09999999999999939493 ) ;
#2824 = DIRECTION ( 'NONE',  ( 1.000000000000000000, 0.000000000000000000, -0.000000000000000000 ) ) ;
#2825 = CARTESIAN_POINT ( 'NONE',  ( 20.95595012432478654, 10.60417921308711975, -141.5957693302180473 ) ) ;
#2826 = DIRECTION ( 'NONE',  ( 1.000000000000000000, 0.000000000000000000, 0.000000000000000000 ) ) ;
#2828 = CARTESIAN_POINT ( 'NONE',  ( -21.05000000000000071, 74.26374286841446803, -91.45445515550682103 ) ) ;
#2827 = LINE ( 'NONE', #185339, #124169 ) ;
#2829 = CARTESIAN_POINT ( 'NONE',  ( -20.54999999999999716, 19.28991295610541812, -237.9781866380819793 ) ) ;
#2830 = LINE ( 'NONE', #21162, #251822 ) ;
#2831 = CARTESIAN_POINT ( 'NONE',  ( 18.44444291854882678, -9.490101180932068559, -107.1289039648910233 ) ) ;
#2832 = ORIENTED_EDGE ( 'NONE', *, *, #141858, .F. ) ;
#2833 = CARTESIAN_POINT ( 'NONE',  ( 18.59999999999999432, -1.299733671219632791, -157.5281295228693637 ) ) ;
#2835 = ORIENTED_EDGE ( 'NONE', *, *, #26231, .T. ) ;
#2834 = DIRECTION ( 'NONE',  ( 0.000000000000000000, -0.8814952561689786137, 0.4721928772774816596 ) ) ;
#2836 = CARTESIAN_POINT ( 'NONE',  ( 23.14999999999999858, 3.900000000011155432, -67.00000000000000000 ) ) ;
#2837 = DIRECTION ( 'NONE',  ( -1.000000000000000000, 0.000000000000000000, 0.000000000000000000 ) ) ;
#2839 = CARTESIAN_POINT ( 'NONE',  ( -18.59999999999999787, 11.75000000001115552, -88.25000000000005684 ) ) ;
#2838 = CARTESIAN_POINT ( 'NONE',  ( -17.11825945287481332, 14.25671114421267127, -219.2337924566137701 ) ) ;
#2840 = EDGE_CURVE ( 'NONE', #128673, #153546, #241988, .T. ) ;
#2841 = ORIENTED_EDGE ( 'NONE', *, *, #163022, .F. ) ;
#2843 = CARTESIAN_POINT ( 'NONE',  ( 18.79999999999999716, 6.783826713665066066, 9.593862367105556288 ) ) ;
#2842 = CARTESIAN_POINT ( 'NONE',  ( -16.92280123533699410, 66.05000000001157900, -56.67247517043902860 ) ) ;
#2845 = ADVANCED_FACE ( 'NONE', ( #118198 ), #157359, .F. ) ;
#2844 = DIRECTION ( 'NONE',  ( 6.938893903907222067E-15, 1.000000000000000000, 6.982962677686266711E-15 ) ) ;
#2846 = CARTESIAN_POINT ( 'NONE',  ( 13.99999999999999822, 66.15000000001258229, -186.7731074845244450 ) ) ;
#2847 = DIRECTION ( 'NONE',  ( -1.000000000000000000, -3.190570557967288949E-16, -6.948722487160392945E-17 ) ) ;
#2848 = CARTESIAN_POINT ( 'NONE',  ( -12.60829076262180415, 66.61047060254583130, -185.7059995716306844 ) ) ;
#2849 = ORIENTED_EDGE ( 'NONE', *, *, #229122, .T. ) ;
#2850 = CIRCLE ( 'NONE', #236092, 0.09999999999999939493 ) ;
#2851 = ORIENTED_EDGE ( 'NONE', *, *, #53293, .F. ) ;
#2852 = AXIS2_PLACEMENT_3D ( 'NONE', #112691, #13597, #31893 ) ;
#2853 = VECTOR ( 'NONE', #232428, 1000.000000000000114 ) ;
#2854 = AXIS2_PLACEMENT_3D ( 'NONE', #174416, #153568, #135216 ) ;
#2855 = EDGE_CURVE ( 'NONE', #38011, #172986, #255817, .T. ) ;
#2856 = DIRECTION ( 'NONE',  ( 0.000000000000000000, 0.9908441862701596881, 0.1350103645451904977 ) ) ;
#2857 = ORIENTED_EDGE ( 'NONE', *, *, #93165, .F. ) ;
#2858 = CARTESIAN_POINT ( 'NONE',  ( -20.94999999999999929, 77.85102823015273543, -91.36919421510179973 ) ) ;
#2859 = ORIENTED_EDGE ( 'NONE', *, *, #236922, .T. ) ;
#2860 = CIRCLE ( 'NONE', #256905, 0.09999999999999939493 ) ;
#2861 = LINE ( 'NONE', #82383, #110139 ) ;
#2862 =( BOUNDED_CURVE ( )  B_SPLINE_CURVE ( 3, ( #150191, #245435, #48500, #189310 ),
 .UNSPECIFIED., .F., .F. ) 
 B_SPLINE_CURVE_WITH_KNOTS ( ( 4, 4 ),
 ( 5.733388419619901200, 5.983100554402348337 ),
 .UNSPECIFIED. ) 
 CURVE ( )  GEOMETRIC_REPRESENTATION_ITEM ( )  RATIONAL_B_SPLINE_CURVE ( ( 1.000000000000000000, 0.9948104011409416580, 0.9948104011409416580, 1.000000000000000000 ) ) 
 REPRESENTATION_ITEM ( '' )  );
#2863 = CARTESIAN_POINT ( 'NONE',  ( -20.95000000000000284, 62.98323157773609893, -207.0610388790104821 ) ) ;
#2864 = ORIENTED_EDGE ( 'NONE', *, *, #151015, .F. ) ;
#2865 = CIRCLE ( 'NONE', #215273, 0.1000000000000045158 ) ;
#2866 = CARTESIAN_POINT ( 'NONE',  ( -16.87372397896795562, 9.880599536652887593, -87.35072451003577498 ) ) ;
#2868 = AXIS2_PLACEMENT_3D ( 'NONE', #237182, #175947, #32601 ) ;
#2867 = DIRECTION ( 'NONE',  ( 0.000000000000000000, -0.8814952561688440547, 0.4721928772777328476 ) ) ;
#2869 = VECTOR ( 'NONE', #140765, 1000.000000000000000 ) ;
#2870 = CARTESIAN_POINT ( 'NONE',  ( -16.77779411440718249, 30.19297764007214724, -234.8043159413754211 ) ) ;
#2871 = CARTESIAN_POINT ( 'NONE',  ( 21.05000000000005400, 74.16448838626246243, -47.52760213295649550 ) ) ;
#2872 = CARTESIAN_POINT ( 'NONE',  ( 21.05000000000000071, -1.360870587180885716, -75.07299792709100927 ) ) ;
#2873 = CARTESIAN_POINT ( 'NONE',  ( 14.11444803880198151, 62.02985059084867459, -218.9026721699492839 ) ) ;
#2874 = EDGE_CURVE ( 'NONE', #24275, #199005, #159911, .T. ) ;
#2875 = ORIENTED_EDGE ( 'NONE', *, *, #17361, .T. ) ;
#2877 = CARTESIAN_POINT ( 'NONE',  ( -18.34374000495060386, 11.47316190337362585, -42.74999999999999289 ) ) ;
#2876 = DIRECTION ( 'NONE',  ( 0.000000000000000000, 0.9126074666063561658, 0.4088369013363748472 ) ) ;
#2878 = VERTEX_POINT ( 'NONE', #41258 ) ;
#2880 = ORIENTED_EDGE ( 'NONE', *, *, #167770, .T. ) ;
#2879 = DIRECTION ( 'NONE',  ( -1.000000000000000000, -0.000000000000000000, -0.000000000000000000 ) ) ;
#2881 = AXIS2_PLACEMENT_3D ( 'NONE', #18555, #237603, #39428 ) ;
#2882 = ORIENTED_EDGE ( 'NONE', *, *, #241618, .T. ) ;
#2883 = CARTESIAN_POINT ( 'NONE',  ( 20.94999999999999929, 1.115600667400684642E-11, -33.50000000000000000 ) ) ;
#2884 = DIRECTION ( 'NONE',  ( -1.040834085586054343E-13, 0.9999176327611370985, 0.01283462868040226822 ) ) ;
#2885 = CARTESIAN_POINT ( 'NONE',  ( 21.13461538461538680, 60.19324435863628509, -221.2538251110503893 ) ) ;
#2886 = CARTESIAN_POINT ( 'NONE',  ( -21.59780538579341069, 60.59700058177565296, -234.1584077978427558 ) ) ;
#2887 = VERTEX_POINT ( 'NONE', #256355 ) ;
#2888 = EDGE_CURVE ( 'NONE', #207855, #252068, #18546, .T. ) ;
#2889 = CARTESIAN_POINT ( 'NONE',  ( -21.05000000000000071, 1.835341550235569663, -78.55515129256303908 ) ) ;
#2890 = CARTESIAN_POINT ( 'NONE',  ( -16.87683809663752399, 66.15000000001229807, -156.6207434663281219 ) ) ;
#2891 = ADVANCED_FACE ( 'NONE', ( #236850 ), #77763, .F. ) ;
#2892 = ORIENTED_EDGE ( 'NONE', *, *, #191215, .F. ) ;
#2893 = DIRECTION ( 'NONE',  ( 0.000000000000000000, 0.000000000000000000, -1.000000000000000000 ) ) ;
#2894 = EDGE_CURVE ( 'NONE', #117327, #96622, #2079, .T. ) ;
#2895 = DIRECTION ( 'NONE',  ( 1.000000000000000000, -0.000000000000000000, -0.000000000000000000 ) ) ;
#2896 = CIRCLE ( 'NONE', #248607, 0.09999999999999939493 ) ;
#2897 = ORIENTED_EDGE ( 'NONE', *, *, #128023, .F. ) ;
#2898 = AXIS2_PLACEMENT_3D ( 'NONE', #38094, #215425, #113750 ) ;
#2899 = DIRECTION ( 'NONE',  ( -6.938893903907220489E-15, 0.9770955615653313941, 0.2128009952263603677 ) ) ;
#2900 = AXIS2_PLACEMENT_3D ( 'NONE', #201147, #143739, #240291 ) ;
#2901 = AXIS2_PLACEMENT_3D ( 'NONE', #193611, #108922, #89350 ) ;
#2902 = EDGE_CURVE ( 'NONE', #5347, #22332, #68424, .T. ) ;
#2903 = CARTESIAN_POINT ( 'NONE',  ( -18.40000000000000213, 64.52683809664972614, -145.8490535513323891 ) ) ;
#2906 = EDGE_CURVE ( 'NONE', #9660, #85698, #238128, .T. ) ;
#2905 = EDGE_CURVE ( 'NONE', #9452, #52291, #137738, .T. ) ;
#2904 = ORIENTED_EDGE ( 'NONE', *, *, #157741, .T. ) ;
#2907 = DIRECTION ( 'NONE',  ( 0.000000000000000000, 0.000000000000000000, 1.000000000000000000 ) ) ;
#2908 = CARTESIAN_POINT ( 'NONE',  ( -12.25000000000000178, 9.850000000011133849, -50.25000000000000711 ) ) ;
#2909 = FACE_OUTER_BOUND ( 'NONE', #250237, .T. ) ;
#2910 = DIRECTION ( 'NONE',  ( 0.000000000000000000, -0.7397360091702802620, 0.6728971962616779878 ) ) ;
#2911 = AXIS2_PLACEMENT_3D ( 'NONE', #169962, #13421, #155523 ) ;
#2912 = CIRCLE ( 'NONE', #161154, 0.1000000000000106498 ) ;
#2913 = VECTOR ( 'NONE', #172553, 1000.000000000000000 ) ;
#2914 = FACE_OUTER_BOUND ( 'NONE', #183063, .T. ) ;
#2915 = CYLINDRICAL_SURFACE ( 'NONE', #193148, 11.74999999999999645 ) ;
#2916 = ADVANCED_FACE ( 'NONE', ( #218557 ), #26941, .F. ) ;
#2918 = EDGE_CURVE ( 'NONE', #39036, #129497, #151836, .T. ) ;
#2917 = DIRECTION ( 'NONE',  ( 2.952720810173289112E-16, 0.9651348961777157509, -0.2617529984165031243 ) ) ;
#2919 = VERTEX_POINT ( 'NONE', #7216 ) ;
#2920 = SPHERICAL_SURFACE ( 'NONE', #104217, 0.1000000000000000056 ) ;
#2921 = AXIS2_PLACEMENT_3D ( 'NONE', #248585, #85619, #146893 ) ;
#2922 = ORIENTED_EDGE ( 'NONE', *, *, #127069, .F. ) ;
#2923 = DIRECTION ( 'NONE',  ( 0.000000000000000000, -1.000000000000000000, -6.860497997771532351E-15 ) ) ;
#2924 = EDGE_CURVE ( 'NONE', #166883, #29111, #110106, .T. ) ;
#2925 = DIRECTION ( 'NONE',  ( 0.000000000000000000, 1.000000000000000000, 0.000000000000000000 ) ) ;
#2927 = ORIENTED_EDGE ( 'NONE', *, *, #160399, .F. ) ;
#2926 = CARTESIAN_POINT ( 'NONE',  ( -23.25000000000000000, 76.00000000001213607, -136.5231074845242745 ) ) ;
#2929 = EDGE_LOOP ( 'NONE', ( #211555, #73148, #61901, #229163 ) ) ;
#2928 = CARTESIAN_POINT ( 'NONE',  ( -18.50000000000000355, 85.41908450282542731, -129.6931996774989102 ) ) ;
#2930 = DIRECTION ( 'NONE',  ( -1.000000000000000000, 0.000000000000000000, 0.000000000000000000 ) ) ;
#2932 = DIRECTION ( 'NONE',  ( 0.000000000000000000, 0.2617529984165030688, 0.9651348961777157509 ) ) ;
#2931 =( BOUNDED_CURVE ( )  B_SPLINE_CURVE ( 3, ( #2903, #124168, #27659, #186710 ),
 .UNSPECIFIED., .F., .F. ) 
 B_SPLINE_CURVE_WITH_KNOTS ( ( 4, 4 ),
 ( 5.733388419619902088, 5.983100554402347449 ),
 .UNSPECIFIED. ) 
 CURVE ( )  GEOMETRIC_REPRESENTATION_ITEM ( )  RATIONAL_B_SPLINE_CURVE ( ( 1.000000000000000000, 0.9948104011409417691, 0.9948104011409417691, 1.000000000000000000 ) ) 
 REPRESENTATION_ITEM ( '' )  );
#2933 = CYLINDRICAL_SURFACE ( 'NONE', #81036, 0.09999999999999939493 ) ;
#2934 = DIRECTION ( 'NONE',  ( 0.000000000000000000, 0.000000000000000000, -1.000000000000000000 ) ) ;
#2935 = EDGE_CURVE ( 'NONE', #77148, #24665, #143437, .T. ) ;
#2937 = ORIENTED_EDGE ( 'NONE', *, *, #140716, .F. ) ;
#2936 = DIRECTION ( 'NONE',  ( 1.000000000000000000, 0.000000000000000000, -0.000000000000000000 ) ) ;
#2938 = ADVANCED_FACE ( 'NONE', ( #183308 ), #166343, .F. ) ;
#2939 = TOROIDAL_SURFACE ( 'NONE', #182013, 0.2000000000000000111, 0.1000000000000000056 ) ;
#2940 = LINE ( 'NONE', #201153, #143563 ) ;
#2941 = ORIENTED_EDGE ( 'NONE', *, *, #60875, .T. ) ;
#2942 = ORIENTED_EDGE ( 'NONE', *, *, #81627, .F. ) ;
#2944 = ADVANCED_FACE ( 'NONE', ( #206717 ), #245848, .T. ) ;
#2943 = CARTESIAN_POINT ( 'NONE',  ( 23.14999999999999858, 1.115600667400684642E-11, -202.9999999999999716 ) ) ;
#2945 = CARTESIAN_POINT ( 'NONE',  ( 20.01093837587850288, 34.49798355602222699, -235.0639822023744614 ) ) ;
#2946 = AXIS2_PLACEMENT_3D ( 'NONE', #28210, #169012, #208117 ) ;
#2947 = ORIENTED_EDGE ( 'NONE', *, *, #170366, .F. ) ;
#2948 = CARTESIAN_POINT ( 'NONE',  ( -20.85000000000000142, 7.128833340094563376, -233.7327013124401276 ) ) ;
#2949 = CARTESIAN_POINT ( 'NONE',  ( 20.94999999999999929, -8.999999999988842703, -191.1060308773475072 ) ) ;
#2950 = TOROIDAL_SURFACE ( 'NONE', #107193, 12.97499999999999609, 0.1000000000000000056 ) ;
#2951 = ADVANCED_FACE ( 'NONE', ( #48917 ), #176768, .T. ) ;
#2952 = ORIENTED_EDGE ( 'NONE', *, *, #40598, .F. ) ;
#2953 = CIRCLE ( 'NONE', #240477, 0.9750000000000036415 ) ;
#2954 = AXIS2_PLACEMENT_3D ( 'NONE', #224651, #164695, #167289 ) ;
#2955 = CARTESIAN_POINT ( 'NONE',  ( -20.64999999999999858, 70.62751970751253339, -223.3325012285725393 ) ) ;
#2956 =( BOUNDED_CURVE ( )  B_SPLINE_CURVE ( 3, ( #125601, #225954, #47333, #82588 ),
 .UNSPECIFIED., .F., .F. ) 
 B_SPLINE_CURVE_WITH_KNOTS ( ( 4, 4 ),
 ( 2.589852378279005940, 2.850972632318389710 ),
 .UNSPECIFIED. ) 
 CURVE ( )  GEOMETRIC_REPRESENTATION_ITEM ( )  RATIONAL_B_SPLINE_CURVE ( ( 1.000000000000000000, 0.9943260843901262636, 0.9943260843901262636, 1.000000000000000000 ) ) 
 REPRESENTATION_ITEM ( '' )  );
#2957 = FACE_OUTER_BOUND ( 'NONE', #112372, .T. ) ;
#2958 = DIRECTION ( 'NONE',  ( 0.000000000000000000, -0.1298341882520022694, -0.9915357197604853789 ) ) ;
#2959 = EDGE_LOOP ( 'NONE', ( #24213, #221751, #38225, #124983 ) ) ;
#2960 = VERTEX_POINT ( 'NONE', #205416 ) ;
#2962 = DIRECTION ( 'NONE',  ( 0.000000000000000000, -0.000000000000000000, 1.000000000000000000 ) ) ;
#2961 = AXIS2_PLACEMENT_3D ( 'NONE', #160224, #221422, #201889 ) ;
#2963 = ORIENTED_EDGE ( 'NONE', *, *, #151337, .F. ) ;
#2964 = EDGE_CURVE ( 'NONE', #32681, #8019, #244549, .T. ) ;
#2965 = CIRCLE ( 'NONE', #202889, 0.1000000000000013933 ) ;
#2966 = VERTEX_POINT ( 'NONE', #188430 ) ;
#2968 = EDGE_LOOP ( 'NONE', ( #53161, #30718, #250507, #106077 ) ) ;
#2967 = CARTESIAN_POINT ( 'NONE',  ( -20.85000000000000142, 7.021664781911246322, -104.3335654018973315 ) ) ;
#2969 = CARTESIAN_POINT ( 'NONE',  ( -22.48660254037843487, 64.35000000001195986, -103.0731074845243711 ) ) ;
#2970 = ORIENTED_EDGE ( 'NONE', *, *, #184693, .F. ) ;
#2971 = FACE_OUTER_BOUND ( 'NONE', #130807, .T. ) ;
#2972 = ORIENTED_EDGE ( 'NONE', *, *, #78032, .F. ) ;
#2974 = ORIENTED_EDGE ( 'NONE', *, *, #137648, .T. ) ;
#2973 = VERTEX_POINT ( 'NONE', #204134 ) ;
#2975 = FACE_OUTER_BOUND ( 'NONE', #65005, .T. ) ;
#2976 = CARTESIAN_POINT ( 'NONE',  ( 18.59999999999999076, 64.35000000001147669, -44.67310748452440095 ) ) ;
#2978 = VERTEX_POINT ( 'NONE', #243259 ) ;
#2977 = AXIS2_PLACEMENT_3D ( 'NONE', #253000, #74412, #122498 ) ;
#2979 = CIRCLE ( 'NONE', #15496, 0.09999999999998898659 ) ;
#2980 = CIRCLE ( 'NONE', #252784, 0.09999999999999949207 ) ;
#2981 = VERTEX_POINT ( 'NONE', #187177 ) ;
#2982 = AXIS2_PLACEMENT_3D ( 'NONE', #19948, #124184, #142441 ) ;
#2983 = CARTESIAN_POINT ( 'NONE',  ( -20.54999999999999716, -11.74999999998884626, -146.3500000000000227 ) ) ;
#2984 = DIRECTION ( 'NONE',  ( 0.000000000000000000, 0.8700118002898321601, -0.4930308989875230585 ) ) ;
#2985 = ORIENTED_EDGE ( 'NONE', *, *, #132465, .F. ) ;
#2986 = CARTESIAN_POINT ( 'NONE',  ( -2.995603634470891112E-16, 87.75000000001148237, -44.77310748452423894 ) ) ;
#2987 = VERTEX_POINT ( 'NONE', #146714 ) ;
#2988 = AXIS2_PLACEMENT_3D ( 'NONE', #69678, #65800, #146600 ) ;
#2989 = CARTESIAN_POINT ( 'NONE',  ( -18.51697539158857353, 65.68434038414380893, -130.9866880726065972 ) ) ;
#2990 = AXIS2_PLACEMENT_3D ( 'NONE', #190719, #10773, #149015 ) ;
#2991 = DIRECTION ( 'NONE',  ( -0.7071067811865456854, -0.7071067811865493491, -4.937700262164544098E-15 ) ) ;
#2992 = ORIENTED_EDGE ( 'NONE', *, *, #209729, .T. ) ;
#2993 = DIRECTION ( 'NONE',  ( 0.000000000000000000, 0.000000000000000000, -1.000000000000000000 ) ) ;
#2994 = ORIENTED_EDGE ( 'NONE', *, *, #42913, .T. ) ;
#2995 = CARTESIAN_POINT ( 'NONE',  ( 21.05000000000000071, 11.65000000001115943, -134.1000000000000227 ) ) ;
#2996 = ORIENTED_EDGE ( 'NONE', *, *, #173000, .F. ) ;
#2997 = VECTOR ( 'NONE', #114422, 1000.000000000000000 ) ;
#2999 = ORIENTED_EDGE ( 'NONE', *, *, #81708, .T. ) ;
#2998 = ORIENTED_EDGE ( 'NONE', *, *, #111549, .F. ) ;
#3000 = ORIENTED_EDGE ( 'NONE', *, *, #195095, .F. ) ;
#3001 = CARTESIAN_POINT ( 'NONE',  ( 20.94999999999999929, -1.362429037182151470, -74.88888124792120493 ) ) ;
#3002 = ORIENTED_EDGE ( 'NONE', *, *, #22460, .F. ) ;
#3003 = CARTESIAN_POINT ( 'NONE',  ( -21.05000000000000071, 77.25000000001189449, -95.02310748452430289 ) ) ;
#3004 = ORIENTED_EDGE ( 'NONE', *, *, #222378, .T. ) ;
#3005 = CARTESIAN_POINT ( 'NONE',  ( -23.24999999999999645, 85.60000000001137721, -29.42291809330221142 ) ) ;
#3006 = CARTESIAN_POINT ( 'NONE',  ( -20.00857864376270001, 61.60676448363446411, -221.6371840927903349 ) ) ;
#3007 = ORIENTED_EDGE ( 'NONE', *, *, #246684, .F. ) ;
#3008 = AXIS2_PLACEMENT_3D ( 'NONE', #180, #202250, #217933 ) ;
#3009 = ADVANCED_FACE ( 'NONE', ( #29405 ), #144154, .T. ) ;
#3010 = AXIS2_PLACEMENT_3D ( 'NONE', #99260, #165, #232397 ) ;
#3011 = ORIENTED_EDGE ( 'NONE', *, *, #90341, .F. ) ;
#3012 = ORIENTED_EDGE ( 'NONE', *, *, #238285, .F. ) ;
#3013 = AXIS2_PLACEMENT_3D ( 'NONE', #51744, #214687, #96017 ) ;
#3014 = CARTESIAN_POINT ( 'NONE',  ( -22.84999999999999787, 0.000000000000000000, 0.000000000000000000 ) ) ;
#3015 = ORIENTED_EDGE ( 'NONE', *, *, #62731, .F. ) ;
#3016 = EDGE_CURVE ( 'NONE', #148732, #119515, #66522, .T. ) ;
#3017 = CARTESIAN_POINT ( 'NONE',  ( -21.10000000000000142, -11.64999999999999858, 11.99999999999999645 ) ) ;
#3018 = CARTESIAN_POINT ( 'NONE',  ( -16.80117486205003630, 14.15842302226418958, -219.2540265911986808 ) ) ;
#3019 = CARTESIAN_POINT ( 'NONE',  ( -21.05000000000000071, 11.75000000001115197, -126.9851942293460922 ) ) ;
#3020 = AXIS2_PLACEMENT_3D ( 'NONE', #75505, #59735, #136722 ) ;
#3021 = CARTESIAN_POINT ( 'NONE',  ( 20.95429693346638800, 65.45669512011676261, -162.4622249462115064 ) ) ;
#3022 = DIRECTION ( 'NONE',  ( 0.000000000000000000, -6.982962677686266711E-15, 1.000000000000000000 ) ) ;
#3023 = EDGE_CURVE ( 'NONE', #205304, #197965, #251765, .T. ) ;
#3024 = AXIS2_PLACEMENT_3D ( 'NONE', #201207, #85076, #120429 ) ;
#3025 = DIRECTION ( 'NONE',  ( 0.000000000000000000, -6.982962677686266711E-15, 1.000000000000000000 ) ) ;
#3027 = CARTESIAN_POINT ( 'NONE',  ( 21.08198257630413508, 6.336596734026219480, -100.4273566762154246 ) ) ;
#3026 = FACE_OUTER_BOUND ( 'NONE', #56842, .T. ) ;
#3028 = DIRECTION ( 'NONE',  ( 0.000000000000000000, 6.982962677686266711E-15, -1.000000000000000000 ) ) ;
#3029 = VECTOR ( 'NONE', #222440, 1000.000000000000000 ) ;
#3030 = CARTESIAN_POINT ( 'NONE',  ( 20.10000000000000853, 4.645987002755569861, 21.91686199900910736 ) ) ;
#3031 = DIRECTION ( 'NONE',  ( 0.000000000000000000, 0.2617529984165083423, 0.9651348961777143076 ) ) ;
#3032 = CARTESIAN_POINT ( 'NONE',  ( 21.12802099929860944, 44.24690014139965655, -236.5304528060606231 ) ) ;
#3034 = ORIENTED_EDGE ( 'NONE', *, *, #39800, .T. ) ;
#3033 = CIRCLE ( 'NONE', #61328, 0.1000000000000028644 ) ;
#3035 = ADVANCED_FACE ( 'NONE', ( #127187 ), #85445, .T. ) ;
#3037 = EDGE_LOOP ( 'NONE', ( #253687, #57875, #12705 ) ) ;
#3036 = CARTESIAN_POINT ( 'NONE',  ( 21.05000000000000071, -4.259020970815407203, -226.0869574510824123 ) ) ;
#3038 = EDGE_CURVE ( 'NONE', #49355, #114960, #205984, .T. ) ;
#3039 = ORIENTED_EDGE ( 'NONE', *, *, #78493, .T. ) ;
#3040 = CARTESIAN_POINT ( 'NONE',  ( -22.39999999999999858, 7.790779598373403836, 0.09999999999999939493 ) ) ;
#3041 = FACE_OUTER_BOUND ( 'NONE', #99103, .T. ) ;
#3042 = EDGE_CURVE ( 'NONE', #15820, #122934, #14467, .T. ) ;
#3043 = CARTESIAN_POINT ( 'NONE',  ( 23.14999999999998437, 0.000000000000000000, 0.000000000000000000 ) ) ;
#3044 = VERTEX_POINT ( 'NONE', #124619 ) ;
#3045 =( LENGTH_UNIT ( ) NAMED_UNIT ( * ) SI_UNIT ( .MILLI., .METRE. ) );
#3046 = CYLINDRICAL_SURFACE ( 'NONE', #158314, 0.09999999999999892308 ) ;
#3047 = EDGE_CURVE ( 'NONE', #223147, #5558, #55921, .T. ) ;
#3048 = CARTESIAN_POINT ( 'NONE',  ( 20.94999999999999929, 1.115600667400684642E-11, -164.6000000000000227 ) ) ;
#3049 = VERTEX_POINT ( 'NONE', #26828 ) ;
#3050 = CIRCLE ( 'NONE', #148844, 0.09999999999999108213 ) ;
#3051 = DIRECTION ( 'NONE',  ( -1.000000000000000000, -2.952720810173289112E-16, 0.000000000000000000 ) ) ;
#3052 = DIRECTION ( 'NONE',  ( 0.000000000000000000, 0.000000000000000000, 1.000000000000000000 ) ) ;
#3053 = EDGE_CURVE ( 'NONE', #170483, #36666, #227559, .T. ) ;
#3054 = DIRECTION ( 'NONE',  ( -4.408576920032447355E-17, -0.07893460099012301889, 0.9968797965484755830 ) ) ;
#3055 = CARTESIAN_POINT ( 'NONE',  ( -16.87683809663752399, 66.15000000001207070, -123.8731074845243683 ) ) ;
#3057 = ORIENTED_EDGE ( 'NONE', *, *, #241751, .T. ) ;
#3056 = LINE ( 'NONE', #158337, #235204 ) ;
#3058 = DIRECTION ( 'NONE',  ( 1.000000000000000000, 0.000000000000000000, 0.000000000000000000 ) ) ;
#3060 = ORIENTED_EDGE ( 'NONE', *, *, #212807, .F. ) ;
#3059 = CARTESIAN_POINT ( 'NONE',  ( -18.40000000000000213, 85.50000000001192291, -96.10095763519393586 ) ) ;
#3061 = CARTESIAN_POINT ( 'NONE',  ( -18.59999999999999787, 64.35000000001259934, -191.3731074845244393 ) ) ;
#3062 = FACE_OUTER_BOUND ( 'NONE', #169130, .T. ) ;
#3063 = DIRECTION ( 'NONE',  ( -1.000000000000000000, 0.000000000000000000, -0.000000000000000000 ) ) ;
#3065 = EDGE_CURVE ( 'NONE', #179449, #121302, #233975, .T. ) ;
#3064 = CARTESIAN_POINT ( 'NONE',  ( -12.29659703204452192, 9.355888454513703323, -183.7886428967780148 ) ) ;
#3067 = CARTESIAN_POINT ( 'NONE',  ( 23.15000000000000213, -11.48912529307605546, -30.39999999999999503 ) ) ;
#3066 = DIRECTION ( 'NONE',  ( 1.000000000000000000, 0.000000000000000000, 0.000000000000000000 ) ) ;
#3068 = LINE ( 'NONE', #63050, #182868 ) ;
#3069 = CARTESIAN_POINT ( 'NONE',  ( 23.25000000000000000, -6.388372595096674544, -212.0629706944429813 ) ) ;
#3070 = PRESENTATION_STYLE_ASSIGNMENT (( #124332 ) ) ;
#3071 = CARTESIAN_POINT ( 'NONE',  ( 20.89999999999999858, -11.75000000000000000, 11.89999999999999680 ) ) ;
#3072 = CIRCLE ( 'NONE', #36444, 0.09999999999998898659 ) ;
#3073 = AXIS2_PLACEMENT_3D ( 'NONE', #51849, #131403, #210956 ) ;
#3074 = VECTOR ( 'NONE', #190597, 1000.000000000000000 ) ;
#3075 = VECTOR ( 'NONE', #31390, 1000.000000000000000 ) ;
#3076 = ORIENTED_EDGE ( 'NONE', *, *, #118391, .F. ) ;
#3077 = FACE_OUTER_BOUND ( 'NONE', #184933, .T. ) ;
#3078 = ORIENTED_EDGE ( 'NONE', *, *, #117560, .T. ) ;
#3079 = ORIENTED_EDGE ( 'NONE', *, *, #16516, .T. ) ;
#3080 = DIRECTION ( 'NONE',  ( 0.000000000000000000, 1.000000000000000000, -6.308085367188393199E-16 ) ) ;
#3081 = EDGE_LOOP ( 'NONE', ( #130287, #144768, #249114, #198906 ) ) ;
#3082 = VERTEX_POINT ( 'NONE', #153200 ) ;
#3084 = VECTOR ( 'NONE', #229687, 1000.000000000000000 ) ;
#3083 = SHAPE_REPRESENTATION_RELATIONSHIP ( 'NONE' , 'NONE' ,  #73451, #119926 ) ;
#3085 = AXIS2_PLACEMENT_3D ( 'NONE', #145893, #127634, #7698 ) ;
#3086 = ORIENTED_EDGE ( 'NONE', *, *, #200979, .F. ) ;
#3087 = DIRECTION ( 'NONE',  ( -0.000000000000000000, -6.982962677686266711E-15, 1.000000000000000000 ) ) ;
#3088 = ORIENTED_EDGE ( 'NONE', *, *, #13395, .T. ) ;
#3089 = EDGE_CURVE ( 'NONE', #24547, #60636, #101713, .T. ) ;
#3090 = CYLINDRICAL_SURFACE ( 'NONE', #242187, 0.1000000000000000472 ) ;
#3091 = PLANE ( 'NONE',  #149343 ) ;
#3092 = AXIS2_PLACEMENT_3D ( 'NONE', #188305, #125756, #9671 ) ;
#3093 = CARTESIAN_POINT ( 'NONE',  ( -18.59999999999999787, 46.62132166459547733, -243.0426574061995950 ) ) ;
#3094 = CARTESIAN_POINT ( 'NONE',  ( -16.87683809663752754, 29.61458345175765317, -234.5865886027308136 ) ) ;
#3095 = FACE_OUTER_BOUND ( 'NONE', #60148, .T. ) ;
#3096 = CYLINDRICAL_SURFACE ( 'NONE', #111320, 0.09999999999999939493 ) ;
#3097 = LINE ( 'NONE', #184314, #70327 ) ;
#3099 = ORIENTED_EDGE ( 'NONE', *, *, #152190, .T. ) ;
#3098 = CARTESIAN_POINT ( 'NONE',  ( 18.59999999999999787, -9.849999999999994316, 30.09999999999999787 ) ) ;
#3101 = DIRECTION ( 'NONE',  ( 1.000000000000000000, 0.000000000000000000, 0.000000000000000000 ) ) ;
#3100 = CARTESIAN_POINT ( 'NONE',  ( 20.95420533658165141, 65.45413552525202761, -61.95560146383115807 ) ) ;
#3102 = EDGE_CURVE ( 'NONE', #44054, #24915, #254779, .T. ) ;
#3103 = DIRECTION ( 'NONE',  ( -1.000000000000000000, -2.885090398161910246E-16, -6.283419270304610340E-17 ) ) ;
#3104 = ADVANCED_FACE ( 'NONE', ( #191034 ), #175327, .F. ) ;
#3105 = ORIENTED_EDGE ( 'NONE', *, *, #155947, .T. ) ;
#3106 = DIRECTION ( 'NONE',  ( -0.000000000000000000, -6.982962677686266711E-15, 1.000000000000000000 ) ) ;
#3107 = CARTESIAN_POINT ( 'NONE',  ( -20.05000000000000426, 66.75000000001230660, -157.6731074845244223 ) ) ;
#3108 = EDGE_LOOP ( 'NONE', ( #251915, #214247, #181986, #186028 ) ) ;
#3109 = EDGE_CURVE ( 'NONE', #17147, #94857, #235029, .T. ) ;
#3111 = CARTESIAN_POINT ( 'NONE',  ( 22.47071067811864964, 75.90090754530910999, -77.24318222902236641 ) ) ;
#3110 = LINE ( 'NONE', #183067, #153785 ) ;
#3112 = EDGE_CURVE ( 'NONE', #172515, #48110, #11692, .T. ) ;
#3113 = CIRCLE ( 'NONE', #182211, 12.97499999999999787 ) ;
#3114 = CARTESIAN_POINT ( 'NONE',  ( -23.15000000000000213, 76.00000000001195133, -103.0231074845243171 ) ) ;
#3115 = EDGE_CURVE ( 'NONE', #255583, #220964, #130962, .T. ) ;
#3116 = ORIENTED_EDGE ( 'NONE', *, *, #57374, .F. ) ;
#3117 = CARTESIAN_POINT ( 'NONE',  ( 21.05000000000000071, 6.413978881499641460, -67.08579911627448666 ) ) ;
#3118 = CARTESIAN_POINT ( 'NONE',  ( 18.54999999999999716, 23.65833333334447985, -150.7500000000000284 ) ) ;
#3119 = EDGE_CURVE ( 'NONE', #253291, #144360, #147534, .T. ) ;
#3120 = CARTESIAN_POINT ( 'NONE',  ( -22.50000000000094147, 0.1000000000110504439, -21.85042919245518434 ) ) ;
#3121 = CARTESIAN_POINT ( 'NONE',  ( -22.50000000000094147, 0.1000000000110504439, -122.3504291924551950 ) ) ;
#3122 = ORIENTED_EDGE ( 'NONE', *, *, #54019, .T. ) ;
#3123 = CIRCLE ( 'NONE', #11545, 0.09999999999998898659 ) ;
#3124 = CARTESIAN_POINT ( 'NONE',  ( 21.06277459767449045, 67.12713756174359503, -90.81910829216803904 ) ) ;
#3125 = CARTESIAN_POINT ( 'NONE',  ( -22.39999999999999858, 76.00000000001195133, -103.0231074845243171 ) ) ;
#3126 = CARTESIAN_POINT ( 'NONE',  ( -16.89268316805465986, 30.21221237062500720, -234.8082435139909592 ) ) ;
#3127 = AXIS2_PLACEMENT_3D ( 'NONE', #204024, #189618, #46231 ) ;
#3129 = DIRECTION ( 'NONE',  ( -1.000000000000000000, 0.000000000000000000, 0.000000000000000000 ) ) ;
#3128 = VECTOR ( 'NONE', #167945, 1000.000000000000000 ) ;
#3130 = CARTESIAN_POINT ( 'NONE',  ( -20.00857864376270001, 9.150000000011157653, -54.65000000000000568 ) ) ;
#3131 = VECTOR ( 'NONE', #229340, 1000.000000000000000 ) ;
#3132 = ADVANCED_FACE ( 'NONE', ( #134852 ), #6048, .F. ) ;
#3134 = ORIENTED_EDGE ( 'NONE', *, *, #46189, .F. ) ;
#3133 = DIRECTION ( 'NONE',  ( 0.2834754621636358940, -0.7201664435733010627, -0.6332471523047666917 ) ) ;
#3135 = CARTESIAN_POINT ( 'NONE',  ( -21.07928932188134041, 6.328516656409859387, -33.40110485434536969 ) ) ;
#3136 = CIRCLE ( 'NONE', #161595, 0.1000000000000052097 ) ;
#3137 = CARTESIAN_POINT ( 'NONE',  ( -21.05000000000000071, -11.65000000000000036, 3.469446951953614189E-15 ) ) ;
#3138 = CARTESIAN_POINT ( 'NONE',  ( -21.65000000000000213, 11.52084357182974372, -219.8296352432475942 ) ) ;
#3139 = CARTESIAN_POINT ( 'NONE',  ( -20.64999999999999858, 70.12557831835937350, -215.6322690948981915 ) ) ;
#3140 = VECTOR ( 'NONE', #25579, 1000.000000000000000 ) ;
#3141 = DIRECTION ( 'NONE',  ( 0.000000000000000000, 0.000000000000000000, 1.000000000000000000 ) ) ;
#3142 = EDGE_CURVE ( 'NONE', #183490, #176803, #185137, .T. ) ;
#3144 = ORIENTED_EDGE ( 'NONE', *, *, #59982, .T. ) ;
#3143 = DIRECTION ( 'NONE',  ( 0.000000000000000000, 0.000000000000000000, 1.000000000000000000 ) ) ;
#3145 = CARTESIAN_POINT ( 'NONE',  ( -21.05000000000000071, 74.83729825007360148, -61.42310748452432989 ) ) ;
#3146 = EDGE_CURVE ( 'NONE', #192257, #198238, #114021, .T. ) ;
#3147 = FACE_OUTER_BOUND ( 'NONE', #106294, .T. ) ;
#3148 = LINE ( 'NONE', #162265, #65679 ) ;
#3149 = EDGE_LOOP ( 'NONE', ( #96305, #247720, #133107, #55062 ) ) ;
#3150 = CARTESIAN_POINT ( 'NONE',  ( -20.54999999999999716, 9.593045456726526865, -211.4478935133083439 ) ) ;
#3151 = CARTESIAN_POINT ( 'NONE',  ( 21.04999999999999716, 76.00000000001242029, -176.5637644362255969 ) ) ;
#3152 = DIRECTION ( 'NONE',  ( -1.000000000000000000, 2.952720810173289112E-16, 2.061873921506763405E-30 ) ) ;
#3153 = CARTESIAN_POINT ( 'NONE',  ( -18.51555513499781469, 78.14120754265996993, -231.3589029833907489 ) ) ;
#3154 = VECTOR ( 'NONE', #203310, 1000.000000000000000 ) ;
#3155 = VERTEX_POINT ( 'NONE', #90603 ) ;
#3156 = CARTESIAN_POINT ( 'NONE',  ( -16.87683809663752399, 9.950000000011137047, -87.09763598180374800 ) ) ;
#3157 = AXIS2_PLACEMENT_3D ( 'NONE', #39913, #180686, #43735 ) ;
#3158 = VERTEX_POINT ( 'NONE', #133592 ) ;
#3159 = ORIENTED_EDGE ( 'NONE', *, *, #39886, .F. ) ;
#3160 = VECTOR ( 'NONE', #84787, 1000.000000000000000 ) ;
#3161 = CARTESIAN_POINT ( 'NONE',  ( 18.79999999999999716, -1.885425182446134107, -11.59641995933507808 ) ) ;
#3163 = DIRECTION ( 'NONE',  ( 0.000000000000000000, 0.2617529984165152257, 0.9651348961777124202 ) ) ;
#3162 = CIRCLE ( 'NONE', #44884, 0.1000000000000105804 ) ;
#3164 = AXIS2_PLACEMENT_3D ( 'NONE', #144993, #97845, #54883 ) ;
#3165 = DIRECTION ( 'NONE',  ( -1.000000000000000000, -0.000000000000000000, -0.000000000000000000 ) ) ;
#3166 = DIRECTION ( 'NONE',  ( 0.9880948137434723000, -0.1484822917196433334, 0.04026969206407598340 ) ) ;
#3167 = VERTEX_POINT ( 'NONE', #31960 ) ;
#3168 = AXIS2_PLACEMENT_3D ( 'NONE', #4861, #204369, #84373 ) ;
#3169 = DIRECTION ( 'NONE',  ( 0.000000000000000000, 0.000000000000000000, -1.000000000000000000 ) ) ;
#3170 = DIRECTION ( 'NONE',  ( 0.000000000000000000, 0.2617529984164915779, 0.9651348961777189706 ) ) ;
#3171 = CARTESIAN_POINT ( 'NONE',  ( 21.04116576186338250, 13.00484560748014928, -210.7852636494204148 ) ) ;
#3172 = CARTESIAN_POINT ( 'NONE',  ( -23.25000000000000000, 43.62273694548321146, -253.2814864317374770 ) ) ;
#3173 = LINE ( 'NONE', #98393, #198770 ) ;
#3174 = VECTOR ( 'NONE', #70464, 1000.000000000000000 ) ;
#3175 = CARTESIAN_POINT ( 'NONE',  ( 18.52643265882457868, 10.31973158071402885, -206.5505334713354273 ) ) ;
#3176 = CIRCLE ( 'NONE', #94767, 0.09999999999999939493 ) ;
#3177 = ORIENTED_EDGE ( 'NONE', *, *, #218307, .T. ) ;
#3178 = EDGE_LOOP ( 'NONE', ( #184403, #2222, #237367, #225597 ) ) ;
#3179 = VERTEX_POINT ( 'NONE', #174054 ) ;
#3180 = CARTESIAN_POINT ( 'NONE',  ( -16.80100914604134488, 9.943149094103565844, -20.81704412728764453 ) ) ;
#3181 = VERTEX_POINT ( 'NONE', #111472 ) ;
#3182 = DIRECTION ( 'NONE',  ( 0.000000000000000000, 0.9915357197604982575, -0.1298341882519033486 ) ) ;
#3183 = CARTESIAN_POINT ( 'NONE',  ( 22.57320508075687115, 64.25000000001165290, -69.52310748452440237 ) ) ;
#3184 = DIRECTION ( 'NONE',  ( 1.000000000000000000, 0.000000000000000000, 0.000000000000000000 ) ) ;
#3185 = VERTEX_POINT ( 'NONE', #110175 ) ;
#3186 = CARTESIAN_POINT ( 'NONE',  ( -21.05000000000000071, -12.41227409413852811, -97.60000000000005116 ) ) ;
#3187 = ORIENTED_EDGE ( 'NONE', *, *, #39610, .F. ) ;
#3188 = CARTESIAN_POINT ( 'NONE',  ( -13.11924609551136456, 9.431689550535260480, -152.2792900322361049 ) ) ;
#3189 = VECTOR ( 'NONE', #148385, 1000.000000000000227 ) ;
#3190 = EDGE_CURVE ( 'NONE', #167877, #163056, #52762, .T. ) ;
#3192 = VERTEX_POINT ( 'NONE', #252248 ) ;
#3191 = CARTESIAN_POINT ( 'NONE',  ( -23.25000000000000000, 87.34033503009941057, -206.5987052159188124 ) ) ;
#3193 = CARTESIAN_POINT ( 'NONE',  ( -23.49999999999994316, 64.25000000001119815, -21.92310748452479174 ) ) ;
#3194 = AXIS2_PLACEMENT_3D ( 'NONE', #216657, #253210, #96674 ) ;
#3195 = CARTESIAN_POINT ( 'NONE',  ( -23.15000000000000213, 74.07476635515205032, -90.29286395139820343 ) ) ;
#3196 = EDGE_CURVE ( 'NONE', #319, #15812, #176975, .T. ) ;
#3197 = CIRCLE ( 'NONE', #211509, 0.09999999999998712696 ) ;
#3198 = VERTEX_POINT ( 'NONE', #56592 ) ;
#3199 = VECTOR ( 'NONE', #91874, 1000.000000000000000 ) ;
#3200 = CARTESIAN_POINT ( 'NONE',  ( -18.50000000000000000, 11.65000000001115588, -200.9999999999999432 ) ) ;
#3202 = EDGE_CURVE ( 'NONE', #8358, #150070, #56109, .T. ) ;
#3201 = DIRECTION ( 'NONE',  ( 0.000000000000000000, 1.000000000000000000, 6.982962677686266711E-15 ) ) ;
#3203 = CARTESIAN_POINT ( 'NONE',  ( -20.64999999999999858, 7.150000000011155876, -112.7500000000000284 ) ) ;
#3205 = EDGE_CURVE ( 'NONE', #165685, #140605, #97793, .T. ) ;
#3204 = ORIENTED_EDGE ( 'NONE', *, *, #117094, .T. ) ;
#3206 = CARTESIAN_POINT ( 'NONE',  ( 18.79999999999999716, 11.49641995933507843, 1.885425182446133885 ) ) ;
#3207 = CARTESIAN_POINT ( 'NONE',  ( -23.15000000000000213, 87.75000000001276135, -215.2731074845242745 ) ) ;
#3208 = DIRECTION ( 'NONE',  ( -1.000000000000000000, 0.000000000000000000, 0.000000000000000000 ) ) ;
#3209 = AXIS2_PLACEMENT_3D ( 'NONE', #140254, #135122, #215946 ) ;
#3210 = ORIENTED_EDGE ( 'NONE', *, *, #21143, .F. ) ;
#3211 = AXIS2_PLACEMENT_3D ( 'NONE', #225352, #131399, #89696 ) ;
#3212 = AXIS2_PLACEMENT_3D ( 'NONE', #200042, #21426, #136171 ) ;
#3213 = CIRCLE ( 'NONE', #119782, 0.09999999999999938105 ) ;
#3214 = VECTOR ( 'NONE', #210563, 1000.000000000000000 ) ;
#3215 = EDGE_CURVE ( 'NONE', #62956, #234572, #251947, .T. ) ;
#3216 = EDGE_CURVE ( 'NONE', #27454, #61108, #172890, .T. ) ;
#3217 = ORIENTED_EDGE ( 'NONE', *, *, #114180, .F. ) ;
#3218 = EDGE_LOOP ( 'NONE', ( #256453, #86591, #101772, #248090 ) ) ;
#3219 = DIRECTION ( 'NONE',  ( -0.000000000000000000, 0.9910465087640860649, 0.1335171055202901413 ) ) ;
#3220 = CARTESIAN_POINT ( 'NONE',  ( -16.87683809663752044, 66.05000000001255955, -183.4254715027207396 ) ) ;
#3222 = ORIENTED_EDGE ( 'NONE', *, *, #11743, .T. ) ;
#3221 = DIRECTION ( 'NONE',  ( -0.000000000000000000, -6.982962677686266711E-15, 1.000000000000000000 ) ) ;
#3223 = CARTESIAN_POINT ( 'NONE',  ( 20.99780126800918723, 11.60538868788781031, -127.0873525717055657 ) ) ;
#3224 = CARTESIAN_POINT ( 'NONE',  ( -23.25000000000000000, 76.00000000001192291, -98.87310748452431142 ) ) ;
#3225 = DIRECTION ( 'NONE',  ( 0.000000000000000000, 0.01562499999998609446, -0.9998779222360101304 ) ) ;
#3226 = DIRECTION ( 'NONE',  ( 0.000000000000000000, 0.000000000000000000, -1.000000000000000000 ) ) ;
#3227 = AXIS2_PLACEMENT_3D ( 'NONE', #114821, #96517, #75710 ) ;
#3228 = FACE_OUTER_BOUND ( 'NONE', #214729, .T. ) ;
#3231 = ORIENTED_EDGE ( 'NONE', *, *, #111916, .F. ) ;
#3230 = EDGE_CURVE ( 'NONE', #75355, #172688, #14651, .T. ) ;
#3229 = CARTESIAN_POINT ( 'NONE',  ( -20.54999999999999716, 62.04148992963929743, -247.7470044306132024 ) ) ;
#3233 = ORIENTED_EDGE ( 'NONE', *, *, #62140, .T. ) ;
#3232 = FACE_OUTER_BOUND ( 'NONE', #130749, .T. ) ;
#3234 = CYLINDRICAL_SURFACE ( 'NONE', #24908, 12.87499999999999822 ) ;
#3235 = ORIENTED_EDGE ( 'NONE', *, *, #61703, .F. ) ;
#3236 = ORIENTED_EDGE ( 'NONE', *, *, #31490, .T. ) ;
#3237 = EDGE_CURVE ( 'NONE', #175273, #231640, #180435, .T. ) ;
#3238 = CARTESIAN_POINT ( 'NONE',  ( -21.44999999999999929, 7.250000000011155521, -54.75000000000000000 ) ) ;
#3239 = DIRECTION ( 'NONE',  ( -1.000000000000000000, 0.000000000000000000, -0.000000000000000000 ) ) ;
#3240 = CARTESIAN_POINT ( 'NONE',  ( -18.40000000000000213, 61.64185094745226934, -212.6324159020321076 ) ) ;
#3241 = DIRECTION ( 'NONE',  ( 0.000000000000000000, 1.000000000000000000, -6.308085367188393199E-16 ) ) ;
#3243 = EDGE_CURVE ( 'NONE', #207394, #52103, #218615, .T. ) ;
#3242 = DIRECTION ( 'NONE',  ( 1.000000000000000000, -2.952720810173289112E-16, -2.061873921506763405E-30 ) ) ;
#3244 = ORIENTED_EDGE ( 'NONE', *, *, #4230, .F. ) ;
#3245 = EDGE_CURVE ( 'NONE', #236296, #187409, #215683, .T. ) ;
#3246 = CARTESIAN_POINT ( 'NONE',  ( 20.94999999999999929, 10.52493806863738790, -207.3780514093641330 ) ) ;
#3247 = ORIENTED_EDGE ( 'NONE', *, *, #121550, .T. ) ;
#3248 = VERTEX_POINT ( 'NONE', #160888 ) ;
#3249 = DIRECTION ( 'NONE',  ( 0.000000000000000000, -0.4999999999999799605, 0.8660254037844502539 ) ) ;
#3250 = EDGE_CURVE ( 'NONE', #251583, #12856, #116604, .T. ) ;
#3251 = AXIS2_PLACEMENT_3D ( 'NONE', #102544, #214215, #195948 ) ;
#3252 = VECTOR ( 'NONE', #158401, 1000.000000000000000 ) ;
#3253 = ORIENTED_EDGE ( 'NONE', *, *, #83176, .F. ) ;
#3254 = CIRCLE ( 'NONE', #215646, 12.87499999999999822 ) ;
#3255 = CARTESIAN_POINT ( 'NONE',  ( 20.94999999999999574, 1.162701749949165642, -75.10000000000003695 ) ) ;
#3256 = DIRECTION ( 'NONE',  ( 1.000000000000000000, -0.000000000000000000, 0.000000000000000000 ) ) ;
#3257 = VERTEX_POINT ( 'NONE', #1776 ) ;
#3258 = DIRECTION ( 'NONE',  ( 0.000000000000000000, 0.7216758089626587047, -0.6922311945860948335 ) ) ;
#3259 = VERTEX_POINT ( 'NONE', #80009 ) ;
#3260 = EDGE_CURVE ( 'NONE', #174607, #231943, #119182, .T. ) ;
#3261 = DIRECTION ( 'NONE',  ( -1.000000000000000000, -2.952720810173289112E-16, 0.000000000000000000 ) ) ;
#3262 = ORIENTED_EDGE ( 'NONE', *, *, #256802, .F. ) ;
#3263 = CARTESIAN_POINT ( 'NONE',  ( -23.49999999999994316, 77.16254490893143725, -44.02310748452479316 ) ) ;
#3264 = EDGE_CURVE ( 'NONE', #96501, #16498, #64510, .T. ) ;
#3265 = CARTESIAN_POINT ( 'NONE',  ( -22.50000000000000000, -0.02128009951114784304, -200.9022904438449757 ) ) ;
#3266 = AXIS2_PLACEMENT_3D ( 'NONE', #28334, #204352, #226470 ) ;
#3267 = EDGE_LOOP ( 'NONE', ( #217053, #59577, #2324, #33032 ) ) ;
#3269 = DIRECTION ( 'NONE',  ( 0.000000000000000000, -1.000000000000000000, -7.272083257015735086E-15 ) ) ;
#3268 = CIRCLE ( 'NONE', #36650, 0.1000000000000000472 ) ;
#3271 = ORIENTED_EDGE ( 'NONE', *, *, #83209, .F. ) ;
#3270 = DIRECTION ( 'NONE',  ( 0.000000000000000000, 0.9126074666063772600, 0.4088369013363274962 ) ) ;
#3272 = CARTESIAN_POINT ( 'NONE',  ( 20.95512820512820440, 67.12384868372447499, -191.3731074845244109 ) ) ;
#3273 = ORIENTED_EDGE ( 'NONE', *, *, #6673, .F. ) ;
#3274 =( BOUNDED_CURVE ( )  B_SPLINE_CURVE ( 3, ( #69912, #15062, #71190, #209393 ),
 .UNSPECIFIED., .F., .T. ) 
 B_SPLINE_CURVE_WITH_KNOTS ( ( 4, 4 ),
 ( 0.5235987755983128045, 1.570796326794896558 ),
 .UNSPECIFIED. ) 
 CURVE ( )  GEOMETRIC_REPRESENTATION_ITEM ( )  RATIONAL_B_SPLINE_CURVE ( ( 1.000000000000000000, 0.9106836025229614329, 0.9106836025229614329, 1.000000000000000000 ) ) 
 REPRESENTATION_ITEM ( '' )  );
#3275 = AXIS2_PLACEMENT_3D ( 'NONE', #31311, #49554, #73002 ) ;
#3276 = DIRECTION ( 'NONE',  ( 0.000000000000000000, -0.01562499999999307672, 0.9998779222360100194 ) ) ;
#3277 = ORIENTED_EDGE ( 'NONE', *, *, #253791, .T. ) ;
#3278 = DIRECTION ( 'NONE',  ( 0.000000000000000000, -0.8814952561688429444, 0.4721928772777349570 ) ) ;
#3279 = CARTESIAN_POINT ( 'NONE',  ( 22.49999999999999645, 25.99095500300091643, -254.2329670263966364 ) ) ;
#3280 = LINE ( 'NONE', #159827, #249424 ) ;
#3281 = CARTESIAN_POINT ( 'NONE',  ( -16.86337532320261090, 9.979967204235514089, -121.4489244689828382 ) ) ;
#3282 = FACE_OUTER_BOUND ( 'NONE', #75299, .T. ) ;
#3283 = CARTESIAN_POINT ( 'NONE',  ( -21.05000000000000071, 43.48442877397276618, -245.2193771921251084 ) ) ;
#3284 = VERTEX_POINT ( 'NONE', #236539 ) ;
#3285 = DIRECTION ( 'NONE',  ( 0.7071067811864846231, 0.2890913453341779626, -0.6453109281989296564 ) ) ;
#3286 = FACE_OUTER_BOUND ( 'NONE', #114005, .T. ) ;
#3287 = CARTESIAN_POINT ( 'NONE',  ( -23.25000000000000000, -11.75000000000000000, 11.75000000000000000 ) ) ;
#3288 = DIRECTION ( 'NONE',  ( 0.000000000000000000, 6.982962677686266711E-15, -1.000000000000000000 ) ) ;
#3289 = ORIENTED_EDGE ( 'NONE', *, *, #81130, .F. ) ;
#3290 = CARTESIAN_POINT ( 'NONE',  ( -23.25000000000000000, 0.000000000000000000, 0.000000000000000000 ) ) ;
#3291 = EDGE_LOOP ( 'NONE', ( #132921, #218359, #207662, #185863 ) ) ;
#3292 = CARTESIAN_POINT ( 'NONE',  ( -20.93284271247462058, 64.25000000001176659, -76.53791325517833855 ) ) ;
#3293 = AXIS2_PLACEMENT_3D ( 'NONE', #186793, #146346, #126800 ) ;
#3294 = ORIENTED_EDGE ( 'NONE', *, *, #79730, .F. ) ;
#3295 = VECTOR ( 'NONE', #57949, 1000.000000000000000 ) ;
#3296 = DIRECTION ( 'NONE',  ( -1.000000000000000000, -0.000000000000000000, -0.000000000000000000 ) ) ;
#3297 = CARTESIAN_POINT ( 'NONE',  ( -20.89878130938411616, 10.32747123227773045, -72.57740328502492844 ) ) ;
#3298 = ORIENTED_EDGE ( 'NONE', *, *, #77797, .T. ) ;
#3300 = EDGE_LOOP ( 'NONE', ( #4920, #124689, #155253, #176443 ) ) ;
#3299 = DIRECTION ( 'NONE',  ( 0.000000000000000000, 0.000000000000000000, -1.000000000000000000 ) ) ;
#3301 = FACE_OUTER_BOUND ( 'NONE', #12226, .T. ) ;
#3302 = ORIENTED_EDGE ( 'NONE', *, *, #217551, .F. ) ;
#3303 = AXIS2_PLACEMENT_3D ( 'NONE', #137524, #577, #41037 ) ;
#3304 = CARTESIAN_POINT ( 'NONE',  ( -21.14999999999999858, 10.30543449102040476, -228.0143625250146329 ) ) ;
#3305 = CARTESIAN_POINT ( 'NONE',  ( -18.59999999999999787, 47.89822068137787170, -246.3100470504847692 ) ) ;
#3306 = ORIENTED_EDGE ( 'NONE', *, *, #174471, .F. ) ;
#3307 = ORIENTED_EDGE ( 'NONE', *, *, #195812, .F. ) ;
#3308 = DIRECTION ( 'NONE',  ( -1.000000000000000000, 0.000000000000000000, 0.000000000000000000 ) ) ;
#3310 = EDGE_CURVE ( 'NONE', #9515, #60454, #152023, .T. ) ;
#3309 = CARTESIAN_POINT ( 'NONE',  ( -16.92973740335258270, 14.21246129500415734, -219.3008027365993087 ) ) ;
#3311 = CARTESIAN_POINT ( 'NONE',  ( -16.86578989773641979, 66.01519019875325966, -123.9877723711466047 ) ) ;
#3312 = AXIS2_PLACEMENT_3D ( 'NONE', #228448, #66790, #146311 ) ;
#3313 = ORIENTED_EDGE ( 'NONE', *, *, #74677, .F. ) ;
#3314 = ORIENTED_EDGE ( 'NONE', *, *, #87761, .T. ) ;
#3316 = DIRECTION ( 'NONE',  ( 0.000000000000000000, -0.000000000000000000, 1.000000000000000000 ) ) ;
#3315 = AXIS2_PLACEMENT_3D ( 'NONE', #86205, #206185, #121545 ) ;
#3317 = EDGE_CURVE ( 'NONE', #147707, #22276, #128205, .T. ) ;
#3318 =( BOUNDED_SURFACE ( )  B_SPLINE_SURFACE ( 3, 2, ( 
 ( #250457, #11879, #228340 ),
 ( #130504, #9282, #52241 ),
 ( #247891, #229623, #88794 ),
 ( #54812, #230921, #151384 ),
 ( #69275, #13147, #91396 ),
 ( #131795, #170978, #74433 ) ),
 .UNSPECIFIED., .F., .F., .F. ) 
 B_SPLINE_SURFACE_WITH_KNOTS ( ( 4, 2, 4 ),
 ( 3, 3 ),
 ( 4.712388980384689674, 5.497787143782137953, 6.283185307179586232 ),
 ( 0.000000000000000000, 1.000000000000000000 ),
 .UNSPECIFIED. ) 
 GEOMETRIC_REPRESENTATION_ITEM ( )  RATIONAL_B_SPLINE_SURFACE ( (
 ( 1.000000000000000000, 0.7071067811865475727, 1.000000000000000000),
 ( 1.000000000000000000, 0.7727932973487801060, 1.000000000000000000),
 ( 1.000000000000000000, 0.8282379607654416498, 1.000000000000000000),
 ( 1.000000000000000000, 0.9038128468035157015, 1.000000000000000000),
 ( 1.000000000000000000, 0.9240297172246855206, 1.000000000000000000),
 ( 1.000000000000000000, 0.9238795325112961754, 1.000000000000000000) ) ) 
 REPRESENTATION_ITEM ( '' )  SURFACE ( )  );
#3320 = ORIENTED_EDGE ( 'NONE', *, *, #171838, .T. ) ;
#3319 = CARTESIAN_POINT ( 'NONE',  ( 18.41356215285961540, 85.50000000001192291, -95.99103808782463432 ) ) ;
#3321 = EDGE_CURVE ( 'NONE', #81803, #120417, #89439, .T. ) ;
#3322 = DIRECTION ( 'NONE',  ( 0.000000000000000000, -2.255140518769784599E-13, 1.000000000000000000 ) ) ;
#3323 = EDGE_CURVE ( 'NONE', #174107, #101850, #22667, .T. ) ;
#3324 = DIRECTION ( 'NONE',  ( -4.701977403289178058E-30, 0.2617529984164863599, 0.9651348961777203028 ) ) ;
#3325 = CARTESIAN_POINT ( 'NONE',  ( 18.49999999999999289, 53.32357432685029153, -235.0179440783709879 ) ) ;
#3327 = CARTESIAN_POINT ( 'NONE',  ( -23.25000000000000000, 4.250000000000000000, -12.15000000000000391 ) ) ;
#3326 = LINE ( 'NONE', #39936, #119321 ) ;
#3328 = LINE ( 'NONE', #37363, #107087 ) ;
#3329 = CARTESIAN_POINT ( 'NONE',  ( -21.05000000000000071, 11.40444339177023458, -198.6185779617709670 ) ) ;
#3330 = VECTOR ( 'NONE', #13475, 1000.000000000000000 ) ;
#3331 = CARTESIAN_POINT ( 'NONE',  ( -16.86422026484316916, 60.90187991312446059, -221.1017989589733759 ) ) ;
#3332 = CARTESIAN_POINT ( 'NONE',  ( -20.54999999999999716, 78.50726470275243685, -228.6618886302502176 ) ) ;
#3333 = ORIENTED_EDGE ( 'NONE', *, *, #85396, .T. ) ;
#3334 = CIRCLE ( 'NONE', #82440, 0.09999999999999939493 ) ;
#3335 = CIRCLE ( 'NONE', #128446, 0.1000000000000054040 ) ;
#3336 = AXIS2_PLACEMENT_3D ( 'NONE', #15491, #131566, #112020 ) ;
#3337 = ORIENTED_EDGE ( 'NONE', *, *, #7308, .T. ) ;
#3338 = EDGE_CURVE ( 'NONE', #3782, #136922, #3056, .T. ) ;
#3339 = DIRECTION ( 'NONE',  ( 1.000000000000000000, 0.000000000000000000, 0.000000000000000000 ) ) ;
#3340 = ORIENTED_EDGE ( 'NONE', *, *, #155397, .F. ) ;
#3341 = VECTOR ( 'NONE', #152131, 1000.000000000000227 ) ;
#3342 = DIRECTION ( 'NONE',  ( 0.000000000000000000, 0.000000000000000000, 1.000000000000000000 ) ) ;
#3343 = VERTEX_POINT ( 'NONE', #17496 ) ;
#3344 = CARTESIAN_POINT ( 'NONE',  ( -21.05000000000000071, 69.45934304831114048, -169.9231074845244223 ) ) ;
#3346 = ORIENTED_EDGE ( 'NONE', *, *, #240068, .T. ) ;
#3345 = EDGE_LOOP ( 'NONE', ( #239006, #182794, #63827, #133263 ) ) ;
#3347 = FACE_OUTER_BOUND ( 'NONE', #161235, .T. ) ;
#3348 = ORIENTED_EDGE ( 'NONE', *, *, #224270, .F. ) ;
#3349 = AXIS2_PLACEMENT_3D ( 'NONE', #125486, #167213, #82469 ) ;
#3350 = AXIS2_PLACEMENT_3D ( 'NONE', #60232, #155528, #40721 ) ;
#3351 = EDGE_LOOP ( 'NONE', ( #132448, #60959, #223622 ) ) ;
#3352 = SPHERICAL_SURFACE ( 'NONE', #4676, 0.1000000000000000056 ) ;
#3354 = CLOSED_SHELL ( 'NONE', ( #66761, #19567, #56713, #119115, #153453, #98265, #119086, #56516, #199323, #173094, #32378, #148677, #104582, #13184, #39626, #190476, #190951, #51676, #28817, #105007, #190046, #7462, #168773, #199139, #152618, #215761, #161559, #162438, #2201, #161248, #150199, #215913, #121562, #154167, #34032, #217275, #52897, #158738, #15752, #213383, #126531, #151268, #90680, #212783, #203830, #66859, #180074, #64338, #19005, #95564, #257720, #120766, #138913 ) ) ;
#3353 = FACE_OUTER_BOUND ( 'NONE', #18056, .T. ) ;
#3356 = VERTEX_POINT ( 'NONE', #257335 ) ;
#3355 = DIRECTION ( 'NONE',  ( 0.000000000000000000, 0.7035695228903320331, 0.7106264324241468033 ) ) ;
#3357 = EDGE_CURVE ( 'NONE', #79018, #152525, #99576, .T. ) ;
#3358 = CARTESIAN_POINT ( 'NONE',  ( 20.41140022480496796, 39.35226318247610067, -236.9372322472320320 ) ) ;
#3359 = CYLINDRICAL_SURFACE ( 'NONE', #28672, 0.1000000000000000472 ) ;
#3361 = EDGE_LOOP ( 'NONE', ( #54331, #120515, #209399, #88518, #138557, #223536 ) ) ;
#3360 = DIRECTION ( 'NONE',  ( -1.000000000000000000, 0.000000000000000000, 0.000000000000000000 ) ) ;
#3362 = DIRECTION ( 'NONE',  ( 1.000000000000000000, 0.000000000000000000, 0.000000000000000000 ) ) ;
#3363 = VERTEX_POINT ( 'NONE', #40952 ) ;
#3364 = FACE_OUTER_BOUND ( 'NONE', #36710, .T. ) ;
#3366 = ORIENTED_EDGE ( 'NONE', *, *, #228409, .F. ) ;
#3365 = CARTESIAN_POINT ( 'NONE',  ( -17.29158576265543346, 65.63525233399415981, -125.1058657293165339 ) ) ;
#3367 = AXIS2_PLACEMENT_3D ( 'NONE', #139042, #2121, #238167 ) ;
#3368 = CARTESIAN_POINT ( 'NONE',  ( 18.50211644919734866, 10.30207779525984790, -172.9895520716782755 ) ) ;
#3369 = CARTESIAN_POINT ( 'NONE',  ( -13.54036565897076194, 27.85878770204270793, -234.1150007431636766 ) ) ;
#3370 = AXIS2_PLACEMENT_3D ( 'NONE', #161532, #144492, #238481 ) ;
#3372 = EDGE_CURVE ( 'NONE', #231654, #112321, #202363, .T. ) ;
#3371 = DIRECTION ( 'NONE',  ( 0.000000000000000000, 0.000000000000000000, -1.000000000000000000 ) ) ;
#3373 = VERTEX_POINT ( 'NONE', #245552 ) ;
#3375 = CARTESIAN_POINT ( 'NONE',  ( 20.74625933824090396, 8.882913521095439080, -109.0551710241217620 ) ) ;
#3374 = CARTESIAN_POINT ( 'NONE',  ( -17.04295772865489766, 10.02489942527116362, -121.3500000000000227 ) ) ;
#3376 = CARTESIAN_POINT ( 'NONE',  ( -15.75000000000000355, 66.65000000001185754, -86.27310748452437394 ) ) ;
#3377 = AXIS2_PLACEMENT_3D ( 'NONE', #211336, #250451, #93944 ) ;
#3378 = CARTESIAN_POINT ( 'NONE',  ( -23.25000000000000000, 76.00000000001234923, -165.9731074845243768 ) ) ;
#3379 = CARTESIAN_POINT ( 'NONE',  ( 23.25000000000000000, 87.65000000001192859, -106.1231074845242262 ) ) ;
#3380 = CARTESIAN_POINT ( 'NONE',  ( 21.05000000000000071, 69.55000000001261640, -193.5060803140843859 ) ) ;
#3381 = ORIENTED_EDGE ( 'NONE', *, *, #198032, .F. ) ;
#3382 = EDGE_LOOP ( 'NONE', ( #256344, #215257, #222788, #187858 ) ) ;
#3384 = ORIENTED_EDGE ( 'NONE', *, *, #68692, .T. ) ;
#3383 = AXIS2_PLACEMENT_3D ( 'NONE', #216656, #120169, #1451 ) ;
#3385 = DIRECTION ( 'NONE',  ( 1.000000000000000000, -0.000000000000000000, -0.000000000000000000 ) ) ;
#3386 = ORIENTED_EDGE ( 'NONE', *, *, #208781, .T. ) ;
#3387 = LINE ( 'NONE', #163776, #126680 ) ;
#3388 = ORIENTED_EDGE ( 'NONE', *, *, #110340, .T. ) ;
#3389 = DIRECTION ( 'NONE',  ( -2.252264143451594314E-15, 0.1298341882520054891, 0.9915357197604850459 ) ) ;
#3390 = CARTESIAN_POINT ( 'NONE',  ( -17.27223548800067121, 14.81849529660560449, -220.4251374982360403 ) ) ;
#3391 = VECTOR ( 'NONE', #82559, 1000.000000000000000 ) ;
#3392 = AXIS2_PLACEMENT_3D ( 'NONE', #227620, #89393, #26895 ) ;
#3393 = CIRCLE ( 'NONE', #245024, 0.09999999999999983902 ) ;
#3394 = ORIENTED_EDGE ( 'NONE', *, *, #60215, .F. ) ;
#3395 = CIRCLE ( 'NONE', #186600, 0.2000000000000057288 ) ;
#3396 = CARTESIAN_POINT ( 'NONE',  ( 13.77030915526559340, 9.456007326080465347, -152.4886334941467965 ) ) ;
#3397 = FILL_AREA_STYLE ('',( #140345 ) ) ;
#3398 = VECTOR ( 'NONE', #104015, 1000.000000000000000 ) ;
#3399 = ORIENTED_EDGE ( 'NONE', *, *, #228972, .F. ) ;
#3400 = ORIENTED_EDGE ( 'NONE', *, *, #247327, .T. ) ;
#3401 = ORIENTED_EDGE ( 'NONE', *, *, #73318, .T. ) ;
#3402 = EDGE_CURVE ( 'NONE', #83068, #179010, #22840, .T. ) ;
#3403 = CARTESIAN_POINT ( 'NONE',  ( 21.15000000000005187, 83.90000000001120384, -37.27310748452479316 ) ) ;
#3404 = CARTESIAN_POINT ( 'NONE',  ( 21.05000000000000071, 65.27628289530454708, -124.3731074845243825 ) ) ;
#3405 = CARTESIAN_POINT ( 'NONE',  ( 22.57320508075687115, 11.75000000001115552, -134.0000000000000000 ) ) ;
#3406 = EDGE_CURVE ( 'NONE', #87320, #174077, #146417, .T. ) ;
#3407 = CARTESIAN_POINT ( 'NONE',  ( 18.49999999999999645, 1.728086936805617757, -87.38443500516778784 ) ) ;
#3408 = DIRECTION ( 'NONE',  ( 0.000000000000000000, 0.000000000000000000, -1.000000000000000000 ) ) ;
#3409 = DIRECTION ( 'NONE',  ( 0.000000000000000000, -0.9770955615653312831, -0.2128009952263621163 ) ) ;
#3411 = CARTESIAN_POINT ( 'NONE',  ( 23.14999999999999858, 28.08470566095357057, -239.2860081655328770 ) ) ;
#3410 = LINE ( 'NONE', #221177, #99736 ) ;
#3412 = LINE ( 'NONE', #5978, #199873 ) ;
#3414 = ORIENTED_EDGE ( 'NONE', *, *, #74007, .F. ) ;
#3413 = CARTESIAN_POINT ( 'NONE',  ( 21.30740335185485890, 69.44334207798394232, -103.1220420103002056 ) ) ;
#3415 = CARTESIAN_POINT ( 'NONE',  ( -16.89268316805466341, 12.41449167011727361, -211.2369018264743090 ) ) ;
#3416 = EDGE_CURVE ( 'NONE', #191238, #119515, #188141, .T. ) ;
#3417 = EDGE_CURVE ( 'NONE', #164555, #164130, #10368, .T. ) ;
#3418 = ORIENTED_EDGE ( 'NONE', *, *, #5501, .T. ) ;
#3419 = DIRECTION ( 'NONE',  ( 0.000000000000000000, 0.000000000000000000, -1.000000000000000000 ) ) ;
#3420 = VECTOR ( 'NONE', #7726, 1000.000000000000000 ) ;
#3421 = DIRECTION ( 'NONE',  ( 0.000000000000000000, 0.000000000000000000, -1.000000000000000000 ) ) ;
#3422 = CARTESIAN_POINT ( 'NONE',  ( 19.81427058490522697, 64.33143601962973435, -44.77310748452440947 ) ) ;
#3423 = ORIENTED_EDGE ( 'NONE', *, *, #134881, .T. ) ;
#3424 = EDGE_CURVE ( 'NONE', #145089, #128091, #166032, .T. ) ;
#3425 = VECTOR ( 'NONE', #198220, 1000.000000000000000 ) ;
#3426 = EDGE_CURVE ( 'NONE', #121993, #223188, #5613, .T. ) ;
#3427 = CARTESIAN_POINT ( 'NONE',  ( 18.49999999999999645, 74.36282728704168221, -124.9409541190522930 ) ) ;
#3428 = CARTESIAN_POINT ( 'NONE',  ( 20.09999999999999787, 9.750000000011137757, -154.8500000000000227 ) ) ;
#3430 = EDGE_CURVE ( 'NONE', #238447, #230022, #43469, .T. ) ;
#3429 = EDGE_CURVE ( 'NONE', #99053, #141610, #225942, .T. ) ;
#3431 = EDGE_LOOP ( 'NONE', ( #63263, #200596, #67160, #172659 ) ) ;
#3432 = VERTEX_POINT ( 'NONE', #107308 ) ;
#3433 = DIRECTION ( 'NONE',  ( -0.000000000000000000, -0.2617529984165031243, -0.9651348961777157509 ) ) ;
#3434 = ORIENTED_EDGE ( 'NONE', *, *, #212308, .F. ) ;
#3435 = FACE_OUTER_BOUND ( 'NONE', #49851, .T. ) ;
#3436 = CARTESIAN_POINT ( 'NONE',  ( -18.33981767444291577, -9.569575789792940768, -174.3191618437252259 ) ) ;
#3437 = EDGE_CURVE ( 'NONE', #62835, #152894, #43667, .T. ) ;
#3438 = CARTESIAN_POINT ( 'NONE',  ( 6.000000000000061284, 64.65000000001120384, -22.12310748452479103 ) ) ;
#3439 = DIRECTION ( 'NONE',  ( -0.7071067811865456854, 0.7071067811865493491, 0.000000000000000000 ) ) ;
#3440 = EDGE_LOOP ( 'NONE', ( #18861, #77108, #11709, #127194 ) ) ;
#3441 = B_SPLINE_CURVE_WITH_KNOTS ( 'NONE', 3,
 ( #211266, #151311, #112184, #92581, #100273, #179856, #80714, #244612 ),
 .UNSPECIFIED., .F., .F.,
 ( 4, 2, 2, 4 ),
 ( 0.000000000000000000, 0.0001094981963948473395, 0.0002189963927896946790, 0.0004379927855793893580 ),
 .UNSPECIFIED. ) ;
#3442 = CARTESIAN_POINT ( 'NONE',  ( 20.85000000000000142, -1.263275465206102233, -175.4018646667464338 ) ) ;
#3443 = EDGE_CURVE ( 'NONE', #226270, #123360, #243570, .T. ) ;
#3444 = CARTESIAN_POINT ( 'NONE',  ( -21.05000000000000071, 69.70000000001212470, -136.4231074845243654 ) ) ;
#3445 = FACE_OUTER_BOUND ( 'NONE', #188794, .T. ) ;
#3446 = AXIS2_PLACEMENT_3D ( 'NONE', #8011, #107086, #130501 ) ;
#3447 = DIRECTION ( 'NONE',  ( -0.000000000000000000, -0.000000000000000000, -1.000000000000000000 ) ) ;
#3448 = CIRCLE ( 'NONE', #245466, 0.4000000000000114575 ) ;
#3449 = EDGE_CURVE ( 'NONE', #86236, #255967, #27127, .T. ) ;
#3450 = TOROIDAL_SURFACE ( 'NONE', #240798, 0.2000000000000000111, 0.1000000000000000056 ) ;
#3451 = EDGE_CURVE ( 'NONE', #97145, #11718, #114587, .T. ) ;
#3452 = ORIENTED_EDGE ( 'NONE', *, *, #212330, .T. ) ;
#3453 = EDGE_CURVE ( 'NONE', #117897, #214500, #203837, .T. ) ;
#3455 = ORIENTED_EDGE ( 'NONE', *, *, #196481, .T. ) ;
#3454 = DIRECTION ( 'NONE',  ( 0.000000000000000000, 0.1332476588733589318, 0.9910827722268049644 ) ) ;
#3456 = CARTESIAN_POINT ( 'NONE',  ( -20.94999999999999929, 74.83729825007431202, -162.1231074845243540 ) ) ;
#3457 = CARTESIAN_POINT ( 'NONE',  ( -21.05000000000000071, 34.01125473724786730, -243.8802146427611888 ) ) ;
#3458 = DIRECTION ( 'NONE',  ( 1.000000000000000000, 0.000000000000000000, 0.000000000000000000 ) ) ;
#3459 = CARTESIAN_POINT ( 'NONE',  ( 18.49999999999999645, 23.98305617022077030, -253.3362246115443099 ) ) ;
#3460 = EDGE_CURVE ( 'NONE', #164289, #27688, #85326, .T. ) ;
#3461 = CARTESIAN_POINT ( 'NONE',  ( 21.70464131381650219, 10.47921085838517286, -227.4781768778995570 ) ) ;
#3462 = DIRECTION ( 'NONE',  ( 0.000000000000000000, 0.2617529984164915779, 0.9651348961777187485 ) ) ;
#3463 = ORIENTED_EDGE ( 'NONE', *, *, #183596, .F. ) ;
#3464 = CARTESIAN_POINT ( 'NONE',  ( 18.49999999999999645, -1.164121893230052995, -108.4148480855716485 ) ) ;
#3465 = CARTESIAN_POINT ( 'NONE',  ( -23.25000000000000000, 61.57587952878035509, -212.2000740415318774 ) ) ;
#3466 = AXIS2_PLACEMENT_3D ( 'NONE', #55087, #130799, #193365 ) ;
#3468 = ADVANCED_FACE ( 'NONE', ( #222092 ), #6925, .T. ) ;
#3467 = CARTESIAN_POINT ( 'NONE',  ( -18.37151313414733522, 77.36519577919750645, -241.8028021193905204 ) ) ;
#3469 = DIRECTION ( 'NONE',  ( 0.000000000000000000, -6.982962677686266711E-15, 1.000000000000000000 ) ) ;
#3470 = AXIS2_PLACEMENT_3D ( 'NONE', #11906, #173578, #195682 ) ;
#3471 = LINE ( 'NONE', #122154, #188091 ) ;
#3472 = CARTESIAN_POINT ( 'NONE',  ( -18.59999999999999787, 1.115600667400684642E-11, -100.5000000000000284 ) ) ;
#3473 = AXIS2_PLACEMENT_3D ( 'NONE', #183624, #201899, #126197 ) ;
#3474 = VERTEX_POINT ( 'NONE', #8228 ) ;
#3475 = ORIENTED_EDGE ( 'NONE', *, *, #196797, .F. ) ;
#3476 = FACE_OUTER_BOUND ( 'NONE', #56653, .T. ) ;
#3477 = CYLINDRICAL_SURFACE ( 'NONE', #1021, 0.09999999999999939493 ) ;
#3478 = CARTESIAN_POINT ( 'NONE',  ( 22.49999999999999645, 11.64976291803192154, 0.08880997638692984808 ) ) ;
#3479 = DIRECTION ( 'NONE',  ( -1.000000000000000000, 0.000000000000000000, 0.000000000000000000 ) ) ;
#3480 = ADVANCED_FACE ( 'NONE', ( #253236 ), #231128, .T. ) ;
#3481 = ORIENTED_EDGE ( 'NONE', *, *, #98752, .T. ) ;
#3482 = SPHERICAL_SURFACE ( 'NONE', #72528, 0.1000000000000000056 ) ;
#3483 = DIRECTION ( 'NONE',  ( 1.000000000000000000, 0.000000000000000000, 0.000000000000000000 ) ) ;
#3484 = DIRECTION ( 'NONE',  ( 2.952720810173289112E-16, -1.000000000000000000, 0.000000000000000000 ) ) ;
#3485 = CIRCLE ( 'NONE', #28683, 0.1000000000000009354 ) ;
#3486 = CIRCLE ( 'NONE', #149273, 0.1000000000000045852 ) ;
#3487 = VECTOR ( 'NONE', #222857, 1000.000000000000000 ) ;
#3488 = ORIENTED_EDGE ( 'NONE', *, *, #212736, .T. ) ;
#3489 = CARTESIAN_POINT ( 'NONE',  ( -23.15000000000000213, 64.35000000001195986, -110.0379132551783385 ) ) ;
#3490 = ORIENTED_EDGE ( 'NONE', *, *, #228821, .F. ) ;
#3491 = DIRECTION ( 'NONE',  ( 1.000000000000000000, 0.000000000000000000, 0.000000000000000000 ) ) ;
#3492 = DIRECTION ( 'NONE',  ( 0.000000000000000000, -0.5000000000000078826, -0.8660254037844340447 ) ) ;
#3493 = AXIS2_PLACEMENT_3D ( 'NONE', #198496, #2847, #155560 ) ;
#3494 = DIRECTION ( 'NONE',  ( 1.000000000000000000, 0.000000000000000000, 0.000000000000000000 ) ) ;
#3495 = CARTESIAN_POINT ( 'NONE',  ( 18.55121869061587958, 65.67252876774509218, -63.94570419949945261 ) ) ;
#3496 = DIRECTION ( 'NONE',  ( -1.836970198721029934E-16, -0.9651348961777157509, 0.2617529984165031243 ) ) ;
#3497 = DIRECTION ( 'NONE',  ( 1.000000000000000000, 0.000000000000000000, 0.000000000000000000 ) ) ;
#3498 = CARTESIAN_POINT ( 'NONE',  ( 23.24999999999999289, 6.650000000011155876, -179.6499999999999773 ) ) ;
#3499 = DIRECTION ( 'NONE',  ( 1.000000000000000000, 0.000000000000000000, 0.000000000000000000 ) ) ;
#3500 = LINE ( 'NONE', #242117, #129013 ) ;
#3501 = EDGE_CURVE ( 'NONE', #252739, #56541, #35327, .T. ) ;
#3502 = CYLINDRICAL_SURFACE ( 'NONE', #158986, 0.09999999999999939493 ) ;
#3503 = DIRECTION ( 'NONE',  ( 0.000000000000000000, 0.000000000000000000, -1.000000000000000000 ) ) ;
#3504 = CARTESIAN_POINT ( 'NONE',  ( 18.44444291854881968, -9.490101180943229409, -40.12890396489097355 ) ) ;
#3505 = AXIS2_PLACEMENT_3D ( 'NONE', #115541, #17711, #15180 ) ;
#3506 = AXIS2_PLACEMENT_3D ( 'NONE', #201284, #25239, #22679 ) ;
#3507 = EDGE_CURVE ( 'NONE', #100941, #21635, #181051, .T. ) ;
#3508 = AXIS2_PLACEMENT_3D ( 'NONE', #91775, #253408, #94328 ) ;
#3509 = CARTESIAN_POINT ( 'NONE',  ( 23.24999999999999289, 69.35000000001254250, -182.3731074845244109 ) ) ;
#3510 = CARTESIAN_POINT ( 'NONE',  ( 20.94560253601876809, 56.04839098492278993, -227.9897245711965752 ) ) ;
#3511 = ORIENTED_EDGE ( 'NONE', *, *, #221935, .T. ) ;
#3512 = CARTESIAN_POINT ( 'NONE',  ( 18.59999999999999076, 70.05000000001213323, -126.2174051794894893 ) ) ;
#3514 = EDGE_CURVE ( 'NONE', #51281, #78587, #255988, .T. ) ;
#3513 = CARTESIAN_POINT ( 'NONE',  ( 18.59999999999997655, 42.20719072976272912, -239.1935934412594804 ) ) ;
#3515 = ADVANCED_FACE ( 'NONE', ( #193286 ), #10790, .T. ) ;
#3516 = ORIENTED_EDGE ( 'NONE', *, *, #242810, .F. ) ;
#3517 = CARTESIAN_POINT ( 'NONE',  ( -22.49756042579671700, 0.07804633702833754794, -55.35013503889771869 ) ) ;
#3518 = CARTESIAN_POINT ( 'NONE',  ( 21.06600267594171783, 67.22483393081238034, -157.8188447021496756 ) ) ;
#3519 = ADVANCED_FACE ( 'NONE', ( #52457 ), #189416, .F. ) ;
#3520 = AXIS2_PLACEMENT_3D ( 'NONE', #45822, #6691, #234733 ) ;
#3521 = DIRECTION ( 'NONE',  ( 0.000000000000000000, -6.982962677686266711E-15, 1.000000000000000000 ) ) ;
#3522 = EDGE_LOOP ( 'NONE', ( #71921, #197661, #218501, #242337 ) ) ;
#3523 = CARTESIAN_POINT ( 'NONE',  ( -23.15000000000000213, 2.000000000011154189, -147.2246219227621111 ) ) ;
#3524 = DIRECTION ( 'NONE',  ( 0.000000000000000000, -1.000000000000000000, 0.000000000000000000 ) ) ;
#3525 = CIRCLE ( 'NONE', #170183, 12.87499999999999112 ) ;
#3526 = EDGE_LOOP ( 'NONE', ( #230708, #143177, #157804, #12102, #33859 ) ) ;
#3527 = EDGE_CURVE ( 'NONE', #108916, #13565, #239493, .T. ) ;
#3528 = AXIS2_PLACEMENT_3D ( 'NONE', #68817, #111787, #191348 ) ;
#3529 = VECTOR ( 'NONE', #32726, 1000.000000000000000 ) ;
#3530 = AXIS2_PLACEMENT_3D ( 'NONE', #224361, #202239, #103111 ) ;
#3532 = ORIENTED_EDGE ( 'NONE', *, *, #224204, .T. ) ;
#3531 = AXIS2_PLACEMENT_3D ( 'NONE', #90822, #13875, #93397 ) ;
#3533 = DIRECTION ( 'NONE',  ( -1.000000000000000000, -1.836970198721029934E-16, 0.000000000000000000 ) ) ;
#3534 = ORIENTED_EDGE ( 'NONE', *, *, #99608, .F. ) ;
#3535 = AXIS2_PLACEMENT_3D ( 'NONE', #250930, #150574, #129718 ) ;
#3536 = CARTESIAN_POINT ( 'NONE',  ( 20.94999999999999929, 87.29603075034721371, -106.0710066441880883 ) ) ;
#3537 = CARTESIAN_POINT ( 'NONE',  ( -16.97683809663752186, 29.49590395944697718, -234.5399335999045718 ) ) ;
#3539 = DIRECTION ( 'NONE',  ( -1.000000000000000000, 0.000000000000000000, 0.000000000000000000 ) ) ;
#3538 = PRODUCT_DEFINITION_CONTEXT ( 'detailed design', #205831, 'design' ) ;
#3540 = CARTESIAN_POINT ( 'NONE',  ( 24.30000000000000071, 3.175288713399624818, -347.0000000000001137 ) ) ;
#3541 = DIRECTION ( 'NONE',  ( 0.000000000000000000, 0.000000000000000000, -1.000000000000000000 ) ) ;
#3542 = DIRECTION ( 'NONE',  ( 1.000000000000000000, 0.000000000000000000, 0.000000000000000000 ) ) ;
#3543 = DIRECTION ( 'NONE',  ( 0.000000000000000000, 0.1495327102803283015, 0.9887567792719397231 ) ) ;
#3545 = VERTEX_POINT ( 'NONE', #55023 ) ;
#3544 = DIRECTION ( 'NONE',  ( 0.000000000000000000, -6.982962677686266711E-15, 1.000000000000000000 ) ) ;
#3546 = VERTEX_POINT ( 'NONE', #229830 ) ;
#3548 = LINE ( 'NONE', #184755, #102058 ) ;
#3547 = DIRECTION ( 'NONE',  ( -1.000000000000000000, 0.000000000000000000, -0.000000000000000000 ) ) ;
#3550 = ORIENTED_EDGE ( 'NONE', *, *, #73181, .T. ) ;
#3549 = CARTESIAN_POINT ( 'NONE',  ( -16.87683809663752399, 61.23280479334032123, -220.3417702668378126 ) ) ;
#3551 = ORIENTED_EDGE ( 'NONE', *, *, #74542, .T. ) ;
#3552 = EDGE_CURVE ( 'NONE', #140123, #187124, #76972, .T. ) ;
#3553 = CARTESIAN_POINT ( 'NONE',  ( -18.40000000000000213, 70.35000000001159037, -56.87310748452436115 ) ) ;
#3554 = CIRCLE ( 'NONE', #82636, 0.1000000000000028644 ) ;
#3555 = AXIS2_PLACEMENT_3D ( 'NONE', #127927, #67945, #88768 ) ;
#3556 = CARTESIAN_POINT ( 'NONE',  ( 18.49999999999999645, 77.63717271298244782, -124.9409541190522788 ) ) ;
#3557 = CARTESIAN_POINT ( 'NONE',  ( -20.94999999999999929, 0.000000000000000000, -29.50000000000000355 ) ) ;
#3558 = DIRECTION ( 'NONE',  ( 2.168404344971008868E-16, 0.000000000000000000, 1.000000000000000000 ) ) ;
#3559 = DIRECTION ( 'NONE',  ( 0.000000000000000000, 0.000000000000000000, 1.000000000000000000 ) ) ;
#3560 = EDGE_CURVE ( 'NONE', #188358, #1091, #227182, .T. ) ;
#3561 = AXIS2_PLACEMENT_3D ( 'NONE', #138729, #236573, #1812 ) ;
#3562 = EDGE_CURVE ( 'NONE', #89391, #17786, #52208, .T. ) ;
#3563 = AXIS2_PLACEMENT_3D ( 'NONE', #112483, #207733, #130743 ) ;
#3564 = CARTESIAN_POINT ( 'NONE',  ( 22.39999999999999503, 68.20922040163857503, -103.1231074845243540 ) ) ;
#3565 = ORIENTED_EDGE ( 'NONE', *, *, #6376, .T. ) ;
#3566 = ORIENTED_EDGE ( 'NONE', *, *, #101725, .F. ) ;
#3567 = DIRECTION ( 'NONE',  ( -0.000000000000000000, 7.272083257015735086E-15, -1.000000000000000000 ) ) ;
#3568 = TOROIDAL_SURFACE ( 'NONE', #149353, 11.90000000000000391, 0.1000000000000000056 ) ;
#3569 = ORIENTED_EDGE ( 'NONE', *, *, #71773, .F. ) ;
#3570 = CARTESIAN_POINT ( 'NONE',  ( 21.05000000000000071, 0.09779029132038109806, -27.24218538951847535 ) ) ;
#3571 = ORIENTED_EDGE ( 'NONE', *, *, #196703, .F. ) ;
#3572 = DIRECTION ( 'NONE',  ( -0.000000000000000000, 1.000000000000000000, 7.525063763929033127E-15 ) ) ;
#3573 = AXIS2_PLACEMENT_3D ( 'NONE', #101158, #99893, #221145 ) ;
#3574 = EDGE_CURVE ( 'NONE', #35839, #131459, #32963, .T. ) ;
#3575 = CARTESIAN_POINT ( 'NONE',  ( 20.85000000000000142, -1.835859311432481045, -112.0044391687985694 ) ) ;
#3576 = CARTESIAN_POINT ( 'NONE',  ( 18.49999999999999289, 65.74999999739246448, -44.83593553489160399 ) ) ;
#3577 = ADVANCED_FACE ( 'NONE', ( #214129 ), #171191, .F. ) ;
#3578 = CARTESIAN_POINT ( 'NONE',  ( -20.64999999999999858, 7.150000000011155876, -88.15000000000004832 ) ) ;
#3579 = ORIENTED_EDGE ( 'NONE', *, *, #234613, .F. ) ;
#3580 = AXIS2_PLACEMENT_3D ( 'NONE', #150002, #70479, #28794 ) ;
#3581 = ADVANCED_FACE ( 'NONE', ( #95454 ), #132014, .F. ) ;
#3582 = CARTESIAN_POINT ( 'NONE',  ( -21.05439746398122836, 11.74999999999999645, -6.989916487484737928 ) ) ;
#3583 = ORIENTED_EDGE ( 'NONE', *, *, #166001, .T. ) ;
#3584 = DIRECTION ( 'NONE',  ( 0.000000000000000000, -1.000000000000000000, -6.982962677686265922E-15 ) ) ;
#3585 = AXIS2_PLACEMENT_3D ( 'NONE', #15020, #95797, #72430 ) ;
#3587 = PLANE ( 'NONE',  #247838 ) ;
#3586 = AXIS2_PLACEMENT_3D ( 'NONE', #179881, #40396, #42924 ) ;
#3588 = CARTESIAN_POINT ( 'NONE',  ( -23.49999999999994316, 82.84256550613280012, -26.34830530078816935 ) ) ;
#3589 = EDGE_CURVE ( 'NONE', #13363, #127614, #172478, .T. ) ;
#3590 = AXIS2_PLACEMENT_3D ( 'NONE', #42427, #164940, #20316 ) ;
#3591 = FACE_OUTER_BOUND ( 'NONE', #215374, .T. ) ;
#3592 = VERTEX_POINT ( 'NONE', #115024 ) ;
#3593 = CARTESIAN_POINT ( 'NONE',  ( -20.94684162615585876, 64.25000000176534343, -96.18146348457848660 ) ) ;
#3594 = ORIENTED_EDGE ( 'NONE', *, *, #227408, .F. ) ;
#3597 = ORIENTED_EDGE ( 'NONE', *, *, #121516, .T. ) ;
#3596 = CARTESIAN_POINT ( 'NONE',  ( 21.30000000000002558, 76.00000000001165290, -69.52310748452431710 ) ) ;
#3595 = DIRECTION ( 'NONE',  ( 0.000000000000000000, 0.000000000000000000, -1.000000000000000000 ) ) ;
#3598 = CARTESIAN_POINT ( 'NONE',  ( 20.95000000000005258, 65.15000000001120384, -51.02310748452479316 ) ) ;
#3599 = ORIENTED_EDGE ( 'NONE', *, *, #207278, .T. ) ;
#3600 = FACE_OUTER_BOUND ( 'NONE', #170206, .T. ) ;
#3601 = VERTEX_POINT ( 'NONE', #94161 ) ;
#3602 = DIRECTION ( 'NONE',  ( 0.000000000000000000, 0.9915357197604882655, -0.1298341882519791490 ) ) ;
#3603 = ADVANCED_FACE ( 'NONE', ( #73359 ), #209701, .T. ) ;
#3604 = CARTESIAN_POINT ( 'NONE',  ( -20.64999999999999858, 71.65000000001151648, -48.37310748452434694 ) ) ;
#3605 = DIRECTION ( 'NONE',  ( 1.186688945009009831E-16, 1.000000000000000000, 6.982962677686266711E-15 ) ) ;
#3606 = CARTESIAN_POINT ( 'NONE',  ( -18.43569575749026512, -9.519327731081288491, -73.97297637655937308 ) ) ;
#3607 = CIRCLE ( 'NONE', #32711, 0.09999999999999520384 ) ;
#3608 = CARTESIAN_POINT ( 'NONE',  ( 12.25000000000000000, 9.350000000011140955, -50.24999999999999289 ) ) ;
#3609 = ORIENTED_EDGE ( 'NONE', *, *, #83186, .F. ) ;
#3610 = CARTESIAN_POINT ( 'NONE',  ( -21.45000000000000284, 10.13883017033223943, -211.3290274220034632 ) ) ;
#3611 = DIRECTION ( 'NONE',  ( 0.000000000000000000, 1.000000000000000000, 0.000000000000000000 ) ) ;
#3612 = ORIENTED_EDGE ( 'NONE', *, *, #3016, .T. ) ;
#3613 = CARTESIAN_POINT ( 'NONE',  ( 18.59999999999999787, -8.150000000000007461, 33.00000000000000000 ) ) ;
#3614 = EDGE_LOOP ( 'NONE', ( #51488, #246574, #212234, #72556 ) ) ;
#3615 = CARTESIAN_POINT ( 'NONE',  ( -18.40000000000000213, 59.60579174656471224, -220.6800530043423976 ) ) ;
#3616 = DIRECTION ( 'NONE',  ( 0.000000000000000000, 0.8814952561688444987, -0.4721928772777320149 ) ) ;
#3617 = CARTESIAN_POINT ( 'NONE',  ( 21.02374657821582815, 36.02918351771350558, -236.0543695115171943 ) ) ;
#3619 = ORIENTED_EDGE ( 'NONE', *, *, #97666, .T. ) ;
#3618 = CARTESIAN_POINT ( 'NONE',  ( 20.27550659511088682, 60.75776438711819338, -224.5153016389302536 ) ) ;
#3620 = FACE_OUTER_BOUND ( 'NONE', #218003, .T. ) ;
#3621 = CARTESIAN_POINT ( 'NONE',  ( 20.95512820512820440, 67.12384868372450342, -194.9644784893834810 ) ) ;
#3622 = ORIENTED_EDGE ( 'NONE', *, *, #219274, .T. ) ;
#3623 = AXIS2_PLACEMENT_3D ( 'NONE', #139481, #83340, #242436 ) ;
#3625 = CIRCLE ( 'NONE', #190928, 0.09999999999998898659 ) ;
#3624 = DIRECTION ( 'NONE',  ( 0.000000000000000000, 1.000000000000000000, 6.982962677686266711E-15 ) ) ;
#3626 = CARTESIAN_POINT ( 'NONE',  ( -18.59999999999999787, 68.97833521811179480, -99.18954208262705663 ) ) ;
#3627 = ORIENTED_EDGE ( 'NONE', *, *, #30473, .T. ) ;
#3628 = AXIS2_PLACEMENT_3D ( 'NONE', #8302, #107375, #206488 ) ;
#3629 = CARTESIAN_POINT ( 'NONE',  ( -21.93340585897931660, 65.31415710917114836, -242.9239163822773833 ) ) ;
#3630 = EDGE_CURVE ( 'NONE', #75413, #244844, #231309, .T. ) ;
#3631 = VERTEX_POINT ( 'NONE', #104098 ) ;
#3632 = DIRECTION ( 'NONE',  ( 0.000000000000000000, -0.8660254037844412611, -0.4999999999999956701 ) ) ;
#3633 = VECTOR ( 'NONE', #143905, 1000.000000000000000 ) ;
#3634 = ORIENTED_EDGE ( 'NONE', *, *, #235606, .T. ) ;
#3636 = ORIENTED_EDGE ( 'NONE', *, *, #249338, .T. ) ;
#3635 = CARTESIAN_POINT ( 'NONE',  ( -23.15000000000000213, 71.75000000001229239, -157.6731074845243654 ) ) ;
#3637 = EDGE_CURVE ( 'NONE', #115507, #150045, #236250, .T. ) ;
#3640 = ORIENTED_EDGE ( 'NONE', *, *, #137886, .T. ) ;
#3639 = ORIENTED_EDGE ( 'NONE', *, *, #125512, .T. ) ;
#3638 = DIRECTION ( 'NONE',  ( 0.000000000000000000, 0.000000000000000000, -1.000000000000000000 ) ) ;
#3641 = EDGE_CURVE ( 'NONE', #164331, #49841, #197958, .T. ) ;
#3643 = VECTOR ( 'NONE', #113953, 1000.000000000000000 ) ;
#3642 = SPHERICAL_SURFACE ( 'NONE', #149609, 0.1000000000000000056 ) ;
#3645 = EDGE_CURVE ( 'NONE', #255042, #137088, #210458, .T. ) ;
#3644 = TOROIDAL_SURFACE ( 'NONE', #124480, 0.2000000000000000111, 0.1000000000000000056 ) ;
#3646 = DIRECTION ( 'NONE',  ( 1.000000000000000000, 0.000000000000000000, 0.000000000000000000 ) ) ;
#3647 = CARTESIAN_POINT ( 'NONE',  ( -21.05000000000000071, 11.60000000001115517, -194.0717967697244717 ) ) ;
#3648 = CIRCLE ( 'NONE', #103591, 0.09999999999999609201 ) ;
#3650 = DIRECTION ( 'NONE',  ( -3.469446951953605354E-14, 1.000000000000000000, 0.000000000000000000 ) ) ;
#3649 = CARTESIAN_POINT ( 'NONE',  ( 20.94788355080264353, 46.36250628750308778, -243.0620573837410063 ) ) ;
#3651 = DIRECTION ( 'NONE',  ( 0.000000000000000000, 0.000000000000000000, -1.000000000000000000 ) ) ;
#3652 = FACE_OUTER_BOUND ( 'NONE', #75740, .T. ) ;
#3653 = AXIS2_PLACEMENT_3D ( 'NONE', #213131, #137431, #235256 ) ;
#3655 = LINE ( 'NONE', #165308, #64083 ) ;
#3654 = CARTESIAN_POINT ( 'NONE',  ( 18.59999999999999432, 68.20313450767837082, -227.8297066677462794 ) ) ;
#3656 = VERTEX_POINT ( 'NONE', #242346 ) ;
#3657 = ORIENTED_EDGE ( 'NONE', *, *, #144860, .T. ) ;
#3658 = DIRECTION ( 'NONE',  ( 0.000000000000000000, 0.4088369013363283844, -0.9126074666063769270 ) ) ;
#3660 = ORIENTED_EDGE ( 'NONE', *, *, #146679, .T. ) ;
#3659 = CARTESIAN_POINT ( 'NONE',  ( -23.15000000000000213, 20.06933876993645782, -235.7297789824848451 ) ) ;
#3661 = ORIENTED_EDGE ( 'NONE', *, *, #115872, .F. ) ;
#3662 = ADVANCED_FACE ( 'NONE', ( #2440, #200665 ), #63707, .T. ) ;
#3663 = DIRECTION ( 'NONE',  ( 0.000000000000000000, -0.9893560106964500722, 0.1455152366551550613 ) ) ;
#3664 =( BOUNDED_SURFACE ( )  B_SPLINE_SURFACE ( 3, 2, ( 
 ( #19306, #57123, #238346 ),
 ( #222611, #68705, #205626 ),
 ( #204345, #146932, #4840 ),
 ( #225181, #84353, #3582 ),
 ( #43998, #23180, #166547 ),
 ( #148232, #63553, #246062 ) ),
 .UNSPECIFIED., .F., .F., .F. ) 
 B_SPLINE_SURFACE_WITH_KNOTS ( ( 4, 2, 4 ),
 ( 3, 3 ),
 ( 1.570796326794895448, 2.356194490192343505, 3.141592653589791784 ),
 ( 0.000000000000000000, 1.000000000000000000 ),
 .UNSPECIFIED. ) 
 GEOMETRIC_REPRESENTATION_ITEM ( )  RATIONAL_B_SPLINE_SURFACE ( (
 ( 1.000000000000000000, 0.7071067811865414665, 1.000000000000000000),
 ( 1.000000000000000000, 0.6611148371779385080, 1.000000000000000000),
 ( 1.000000000000000000, 0.6092287576695514240, 1.000000000000000000),
 ( 1.000000000000000000, 0.5278258667058023379, 1.000000000000000000),
 ( 1.000000000000000000, 0.4993418825334033362, 1.000000000000000000),
 ( 1.000000000000000000, 0.4999999999999952816, 1.000000000000000000) ) ) 
 REPRESENTATION_ITEM ( '' )  SURFACE ( )  );
#3665 = ORIENTED_EDGE ( 'NONE', *, *, #11859, .T. ) ;
#3666 = DIRECTION ( 'NONE',  ( 0.000000000000000000, 0.8496786552930077896, 0.5273008465188219196 ) ) ;
#3667 = VERTEX_POINT ( 'NONE', #221482 ) ;
#3668 = CARTESIAN_POINT ( 'NONE',  ( 5.551115123125782702E-14, 64.75000000001119815, -36.02310748452479316 ) ) ;
#3669 = DIRECTION ( 'NONE',  ( -0.000000000000000000, 0.08413937888704209334, -0.9964539953858898569 ) ) ;
#3670 = VECTOR ( 'NONE', #42801, 1000.000000000000000 ) ;
#3671 = AXIS2_PLACEMENT_3D ( 'NONE', #253657, #234100, #252367 ) ;
#3673 = VERTEX_POINT ( 'NONE', #57599 ) ;
#3672 = ORIENTED_EDGE ( 'NONE', *, *, #139542, .F. ) ;
#3674 = VERTEX_POINT ( 'NONE', #234980 ) ;
#3675 = DIRECTION ( 'NONE',  ( 0.000000000000000000, -0.2605042016806740079, 0.9654727137038698892 ) ) ;
#3676 = ORIENTED_EDGE ( 'NONE', *, *, #72005, .T. ) ;
#3677 = VERTEX_POINT ( 'NONE', #183674 ) ;
#3678 = DIRECTION ( 'NONE',  ( 0.000000000000000000, 0.000000000000000000, -1.000000000000000000 ) ) ;
#3679 = DIRECTION ( 'NONE',  ( 0.000000000000000000, 0.9126074666063771490, 0.4088369013363281623 ) ) ;
#3681 = ORIENTED_EDGE ( 'NONE', *, *, #123545, .F. ) ;
#3680 = CARTESIAN_POINT ( 'NONE',  ( 18.50000000000000355, -9.399999999988846611, -107.3820418481727188 ) ) ;
#3682 = EDGE_CURVE ( 'NONE', #245768, #11304, #135849, .T. ) ;
#3683 = EDGE_CURVE ( 'NONE', #63258, #88307, #177154, .T. ) ;
#3684 = CIRCLE ( 'NONE', #20273, 0.09999999999998898659 ) ;
#3686 = DIRECTION ( 'NONE',  ( 0.000000000000000000, -7.026728003956686545E-15, 1.000000000000000000 ) ) ;
#3685 = CARTESIAN_POINT ( 'NONE',  ( 20.94999999999999929, 6.550000000011156231, -146.1500000000000341 ) ) ;
#3687 = CARTESIAN_POINT ( 'NONE',  ( -23.15000000000000213, 11.65000000000000036, -21.25000000000000000 ) ) ;
#3688 = DIRECTION ( 'NONE',  ( 0.000000000000000000, -0.1575844902526687130, -0.9875055080513762684 ) ) ;
#3689 = CARTESIAN_POINT ( 'NONE',  ( -18.59999999999999787, 11.65000000001115232, -174.5148057706539930 ) ) ;
#3690 = VERTEX_POINT ( 'NONE', #175050 ) ;
#3691 = ORIENTED_EDGE ( 'NONE', *, *, #87920, .F. ) ;
#3692 = CYLINDRICAL_SURFACE ( 'NONE', #151941, 0.09999999999998898659 ) ;
#3693 = CARTESIAN_POINT ( 'NONE',  ( -20.64999999999999858, 62.08148826970418099, -247.6553521922769221 ) ) ;
#3694 = ADVANCED_FACE ( 'NONE', ( #215402 ), #202068, .T. ) ;
#3695 = ORIENTED_EDGE ( 'NONE', *, *, #142615, .F. ) ;
#3696 = VECTOR ( 'NONE', #121970, 1000.000000000000000 ) ;
#3698 = DIRECTION ( 'NONE',  ( 0.000000000000000000, -0.2617529984165152257, -0.9651348961777124202 ) ) ;
#3697 = AXIS2_PLACEMENT_3D ( 'NONE', #243963, #192993, #251669 ) ;
#3699 = CIRCLE ( 'NONE', #145157, 0.09999999999999913125 ) ;
#3700 = CARTESIAN_POINT ( 'NONE',  ( 23.14999999999999858, 28.36802138732021206, -238.7571110118315971 ) ) ;
#3701 = DIRECTION ( 'NONE',  ( 0.000000000000000000, 0.9770955615653316162, 0.2128009952263604232 ) ) ;
#3702 = AXIS2_PLACEMENT_3D ( 'NONE', #237308, #118663, #57358 ) ;
#3703 = EDGE_LOOP ( 'NONE', ( #146190, #206631, #770, #170790 ) ) ;
#3704 = ORIENTED_EDGE ( 'NONE', *, *, #145562, .F. ) ;
#3705 = CYLINDRICAL_SURFACE ( 'NONE', #68011, 0.09999999999998898659 ) ;
#3706 = DIRECTION ( 'NONE',  ( 0.000000000000000000, -0.9910827722268055195, -0.1332476588733540468 ) ) ;
#3707 = EDGE_LOOP ( 'NONE', ( #147886, #11127, #247421, #75243, #48211 ) ) ;
#3708 = DIRECTION ( 'NONE',  ( 2.952720810173289112E-16, 1.000000000000000000, 6.938893903907222067E-15 ) ) ;
#3709 = ORIENTED_EDGE ( 'NONE', *, *, #153407, .F. ) ;
#3710 = LINE ( 'NONE', #63682, #23429 ) ;
#3711 = DIRECTION ( 'NONE',  ( 0.000000000000000000, 1.000000000000000000, 0.000000000000000000 ) ) ;
#3712 = DIRECTION ( 'NONE',  ( -0.7071067811865127117, -0.7071067811865821007, 0.000000000000000000 ) ) ;
#3713 = CIRCLE ( 'NONE', #161968, 0.1000000000000054040 ) ;
#3714 = CIRCLE ( 'NONE', #170360, 0.1000000000000028644 ) ;
#3715 = LINE ( 'NONE', #141943, #86577 ) ;
#3716 = EDGE_CURVE ( 'NONE', #81112, #156105, #220238, .T. ) ;
#3717 = CARTESIAN_POINT ( 'NONE',  ( -21.45000000000000284, 68.29142135624952914, -148.8731074845244109 ) ) ;
#3718 = ORIENTED_EDGE ( 'NONE', *, *, #81496, .F. ) ;
#3719 = CIRCLE ( 'NONE', #57866, 0.09999999999999939493 ) ;
#3720 = CARTESIAN_POINT ( 'NONE',  ( 18.46163235739460973, -9.480150806907175820, -207.6576105398774530 ) ) ;
#3723 = ORIENTED_EDGE ( 'NONE', *, *, #164192, .T. ) ;
#3722 = ORIENTED_EDGE ( 'NONE', *, *, #247076, .T. ) ;
#3721 = AXIS2_PLACEMENT_3D ( 'NONE', #28798, #106985, #228244 ) ;
#3724 = EDGE_LOOP ( 'NONE', ( #134071, #184153, #130157, #227487 ) ) ;
#3725 = AXIS2_PLACEMENT_3D ( 'NONE', #91067, #12837, #192749 ) ;
#3726 = AXIS2_PLACEMENT_3D ( 'NONE', #190397, #149995, #26180 ) ;
#3727 = VERTEX_POINT ( 'NONE', #122412 ) ;
#3728 = EDGE_CURVE ( 'NONE', #151965, #936, #31045, .T. ) ;
#3729 = CARTESIAN_POINT ( 'NONE',  ( -16.92925196614875460, 66.02766820360217537, -157.4063626368076143 ) ) ;
#3730 = CARTESIAN_POINT ( 'NONE',  ( -18.50000000000000355, -7.661125819576635188, -210.0861952081431241 ) ) ;
#3731 = DIRECTION ( 'NONE',  ( 0.000000000000000000, -1.000000000000000000, 0.000000000000000000 ) ) ;
#3732 = CARTESIAN_POINT ( 'NONE',  ( -22.50000000000000000, 76.00000000001213607, -136.5231074845242745 ) ) ;
#3733 = DIRECTION ( 'NONE',  ( 0.000000000000000000, 0.000000000000000000, -1.000000000000000000 ) ) ;
#3734 = VECTOR ( 'NONE', #55279, 1000.000000000000114 ) ;
#3736 = FACE_OUTER_BOUND ( 'NONE', #255407, .T. ) ;
#3735 = CARTESIAN_POINT ( 'NONE',  ( 22.40736611211992368, -3.140208063160686791, -228.2318569537739847 ) ) ;
#3738 = VERTEX_POINT ( 'NONE', #126244 ) ;
#3737 = CARTESIAN_POINT ( 'NONE',  ( 18.46932045258622068, 77.27562233161933136, -241.9521456325934139 ) ) ;
#3739 = CARTESIAN_POINT ( 'NONE',  ( -21.05000000000000071, 6.299230910103437608, -167.4015624999996703 ) ) ;
#3740 = ORIENTED_EDGE ( 'NONE', *, *, #54654, .T. ) ;
#3741 = EDGE_CURVE ( 'NONE', #199662, #64464, #206355, .T. ) ;
#3742 = CARTESIAN_POINT ( 'NONE',  ( 22.14074124539698829, 33.54719148015350072, -242.8474189545858053 ) ) ;
#3743 = EDGE_CURVE ( 'NONE', #108503, #194746, #27319, .T. ) ;
#3744 = ORIENTED_EDGE ( 'NONE', *, *, #115559, .F. ) ;
#3745 = VERTEX_POINT ( 'NONE', #105366 ) ;
#3747 = DIRECTION ( 'NONE',  ( 0.000000000000000000, 0.9126074666063769270, 0.4088369013363280513 ) ) ;
#3746 = B_SPLINE_CURVE_WITH_KNOTS ( 'NONE', 3,
 ( #178586, #79433, #1178, #119892, #145509, #67264, #19492, #146776, #39066, #225032, #124681, #97699, #204200 ),
 .UNSPECIFIED., .F., .F.,
 ( 4, 3, 3, 3, 4 ),
 ( -3.224855718271604415E-06, 0.000000000000000000, 6.199515528660412213E-06, 4.034952380126980364E-05, 7.452715123698976899E-05 ),
 .UNSPECIFIED. ) ;
#3748 = FACE_OUTER_BOUND ( 'NONE', #190198, .T. ) ;
#3749 = CARTESIAN_POINT ( 'NONE',  ( -16.82055514392378015, 66.05000000001153637, -48.69990555906626639 ) ) ;
#3750 = CARTESIAN_POINT ( 'NONE',  ( 13.22261339317536333, 9.436552840015579591, -82.17795547276035961 ) ) ;
#3751 = TOROIDAL_SURFACE ( 'NONE', #103672, 12.97499999999999787, 0.1000000000000000056 ) ;
#3752 = EDGE_CURVE ( 'NONE', #211300, #23430, #77158, .T. ) ;
#3753 = DIRECTION ( 'NONE',  ( -1.000000000000000000, 0.000000000000000000, 0.000000000000000000 ) ) ;
#3754 = EDGE_CURVE ( 'NONE', #152520, #159793, #93340, .T. ) ;
#3755 = ORIENTED_EDGE ( 'NONE', *, *, #215318, .F. ) ;
#3756 = ORIENTED_EDGE ( 'NONE', *, *, #27419, .F. ) ;
#3757 = CARTESIAN_POINT ( 'NONE',  ( -20.94999999999994600, 65.15000000001120384, -3.123107484524795474 ) ) ;
#3758 = EDGE_LOOP ( 'NONE', ( #143290, #59485 ) ) ;
#3759 = DIRECTION ( 'NONE',  ( 0.000000000000000000, -0.000000000000000000, 1.000000000000000000 ) ) ;
#3760 = DIRECTION ( 'NONE',  ( 1.000000000000000000, 0.000000000000000000, 0.000000000000000000 ) ) ;
#3761 = DIRECTION ( 'NONE',  ( 1.000000000000000000, 0.000000000000000000, 0.000000000000000000 ) ) ;
#3763 = EDGE_CURVE ( 'NONE', #73834, #174422, #152206, .T. ) ;
#3762 = DIRECTION ( 'NONE',  ( 0.000000000000000000, -6.688090509790120484E-15, 1.000000000000000000 ) ) ;
#3764 = LINE ( 'NONE', #113751, #157160 ) ;
#3765 = LINE ( 'NONE', #83270, #171587 ) ;
#3766 = CYLINDRICAL_SURFACE ( 'NONE', #129363, 0.5000000000000007772 ) ;
#3767 = VECTOR ( 'NONE', #32686, 1000.000000000000000 ) ;
#3768 = CARTESIAN_POINT ( 'NONE',  ( -21.44999999999999929, 68.85000000001200249, -115.3731074845243540 ) ) ;
#3769 = CARTESIAN_POINT ( 'NONE',  ( 18.57071067811864040, 65.82071067813045318, -81.77310748452437394 ) ) ;
#3770 = VECTOR ( 'NONE', #210131, 1000.000000000000000 ) ;
#3771 = DIRECTION ( 'NONE',  ( 0.000000000000000000, -0.2605042016806647931, -0.9654727137038724427 ) ) ;
#3772 = ADVANCED_FACE ( 'NONE', ( #188791 ), #88385, .F. ) ;
#3773 = CARTESIAN_POINT ( 'NONE',  ( -18.59999999999999787, 65.66751761918668251, -97.42826094061121012 ) ) ;
#3774 = CYLINDRICAL_SURFACE ( 'NONE', #90563, 0.09999999999999939493 ) ;
#3775 = EDGE_CURVE ( 'NONE', #58594, #93811, #73111, .T. ) ;
#3776 = EDGE_CURVE ( 'NONE', #194531, #154195, #66290, .T. ) ;
#3777 = CIRCLE ( 'NONE', #7887, 0.09999999999998898659 ) ;
#3778 = EDGE_LOOP ( 'NONE', ( #190876, #80289, #77411, #221569 ) ) ;
#3779 =( BOUNDED_CURVE ( )  B_SPLINE_CURVE ( 3, ( #133703, #148137, #228966, #213227 ),
 .UNSPECIFIED., .F., .T. ) 
 B_SPLINE_CURVE_WITH_KNOTS ( ( 4, 4 ),
 ( 0.5235987755982449698, 1.570796326794896558 ),
 .UNSPECIFIED. ) 
 CURVE ( )  GEOMETRIC_REPRESENTATION_ITEM ( )  RATIONAL_B_SPLINE_CURVE ( ( 1.000000000000000000, 0.9106836025229499976, 0.9106836025229499976, 1.000000000000000000 ) ) 
 REPRESENTATION_ITEM ( '' )  );
#3780 = ADVANCED_FACE ( 'NONE', ( #170576 ), #39783, .T. ) ;
#3781 = CARTESIAN_POINT ( 'NONE',  ( -16.89268316805465986, 30.21221237062500720, -234.8082435139909592 ) ) ;
#3782 = VERTEX_POINT ( 'NONE', #147084 ) ;
#3783 = FACE_OUTER_BOUND ( 'NONE', #172469, .T. ) ;
#3784 = EDGE_CURVE ( 'NONE', #34439, #163489, #243754, .T. ) ;
#3785 = DIRECTION ( 'NONE',  ( 0.000000000000000000, 0.000000000000000000, 1.000000000000000000 ) ) ;
#3786 = CARTESIAN_POINT ( 'NONE',  ( 21.05000000000005400, 64.25000000001119815, -29.92310748452479174 ) ) ;
#3787 = AXIS2_PLACEMENT_3D ( 'NONE', #105429, #165459, #242401 ) ;
#3788 = ADVANCED_FACE ( 'NONE', ( #107980 ), #50540, .T. ) ;
#3789 = EDGE_LOOP ( 'NONE', ( #234210, #119558, #13967, #16047 ) ) ;
#3790 = DIRECTION ( 'NONE',  ( 0.000000000000000000, 0.000000000000000000, 1.000000000000000000 ) ) ;
#3791 = AXIS2_PLACEMENT_3D ( 'NONE', #250887, #113949, #197334 ) ;
#3792 = DIRECTION ( 'NONE',  ( 1.000000000000000000, 0.000000000000000000, -0.000000000000000000 ) ) ;
#3794 = EDGE_CURVE ( 'NONE', #51518, #244889, #127241, .T. ) ;
#3793 = DIRECTION ( 'NONE',  ( 0.000000000000000000, -0.008583690987135041833, 0.9999631594459055250 ) ) ;
#3795 = DIRECTION ( 'NONE',  ( 0.000000000000000000, -1.000000000000000000, 0.000000000000000000 ) ) ;
#3796 = FACE_OUTER_BOUND ( 'NONE', #113310, .T. ) ;
#3797 = CIRCLE ( 'NONE', #224540, 12.97499999999998721 ) ;
#3798 = LINE ( 'NONE', #208438, #32156 ) ;
#3799 = ORIENTED_EDGE ( 'NONE', *, *, #36730, .T. ) ;
#3800 = CARTESIAN_POINT ( 'NONE',  ( 21.14999999999999858, 76.00000000001229239, -157.8731074845243540 ) ) ;
#3802 = EDGE_LOOP ( 'NONE', ( #9739, #90486, #211997, #23603 ) ) ;
#3801 = CARTESIAN_POINT ( 'NONE',  ( 22.50000000000000000, 11.64957080755595520, -167.3999999999999773 ) ) ;
#3803 = DIRECTION ( 'NONE',  ( 1.000000000000000000, 0.000000000000000000, 0.000000000000000000 ) ) ;
#3804 = FACE_OUTER_BOUND ( 'NONE', #211597, .T. ) ;
#3805 = EDGE_CURVE ( 'NONE', #147427, #17741, #181237, .T. ) ;
#3806 = CARTESIAN_POINT ( 'NONE',  ( -18.59999999999999787, 79.28756800457986742, -196.2274082906208434 ) ) ;
#3807 = ORIENTED_EDGE ( 'NONE', *, *, #193638, .F. ) ;
#3808 = CARTESIAN_POINT ( 'NONE',  ( 21.05000000000000071, 76.00000000001244871, -170.0231074845243597 ) ) ;
#3809 = EDGE_CURVE ( 'NONE', #256921, #971, #244914, .T. ) ;
#3810 = ITEM_DEFINED_TRANSFORMATION ( 'NONE', 'NONE', #44510,  #2425 ) ;
#3811 = FACE_OUTER_BOUND ( 'NONE', #174490, .T. ) ;
#3812 = VERTEX_POINT ( 'NONE', #226623 ) ;
#3813 = CARTESIAN_POINT ( 'NONE',  ( 20.05000000000002913, 68.75000000001183764, -90.37310748452435405 ) ) ;
#3814 = DIRECTION ( 'NONE',  ( 2.952720810173289112E-16, -1.000000000000000000, 0.000000000000000000 ) ) ;
#3815 = DIRECTION ( 'NONE',  ( -1.000000000000000000, 0.000000000000000000, 0.000000000000000000 ) ) ;
#3816 = ORIENTED_EDGE ( 'NONE', *, *, #140021, .T. ) ;
#3817 = ORIENTED_EDGE ( 'NONE', *, *, #192515, .F. ) ;
#3818 = CARTESIAN_POINT ( 'NONE',  ( -18.59999999999999787, 7.250000000011155521, -54.85000000000000142 ) ) ;
#3819 = DIRECTION ( 'NONE',  ( 1.000000000000000000, 0.000000000000000000, 0.000000000000000000 ) ) ;
#3820 = DIRECTION ( 'NONE',  ( -1.000000000000000000, -0.000000000000000000, -0.000000000000000000 ) ) ;
#3821 = CARTESIAN_POINT ( 'NONE',  ( -21.05000000000000071, 1.115600667400684642E-11, -167.4999999999999716 ) ) ;
#3822 = CARTESIAN_POINT ( 'NONE',  ( 18.59999999999999076, 10.49142135624846617, -125.2500000000000568 ) ) ;
#3823 = DIRECTION ( 'NONE',  ( -1.000000000000000000, 0.000000000000000000, 0.000000000000000000 ) ) ;
#3825 = DIRECTION ( 'NONE',  ( -1.000000000000000000, 0.000000000000000000, -0.000000000000000000 ) ) ;
#3824 = CARTESIAN_POINT ( 'NONE',  ( 21.07094088545303734, 6.320167221916491052, 0.09889370255222132422 ) ) ;
#3826 = AXIS2_PLACEMENT_3D ( 'NONE', #135317, #170669, #229316 ) ;
#3827 = EDGE_CURVE ( 'NONE', #61003, #159998, #167986, .T. ) ;
#3829 = DIRECTION ( 'NONE',  ( -0.000000000000000000, 0.8660254037844411501, 0.4999999999999956701 ) ) ;
#3828 = CIRCLE ( 'NONE', #149595, 11.89999999999999325 ) ;
#3830 = DIRECTION ( 'NONE',  ( 1.000000000000000000, 0.000000000000000000, 0.000000000000000000 ) ) ;
#3831 = CARTESIAN_POINT ( 'NONE',  ( 20.94999999999999929, -12.41227409413852811, -197.9999999999999432 ) ) ;
#3832 = CIRCLE ( 'NONE', #182907, 4.041421356237310469 ) ;
#3834 = CARTESIAN_POINT ( 'NONE',  ( 20.95035502843362707, 18.75477178125364830, -228.0741875901196636 ) ) ;
#3833 = CIRCLE ( 'NONE', #158000, 0.09999999999999939493 ) ;
#3835 = ORIENTED_EDGE ( 'NONE', *, *, #241766, .F. ) ;
#3836 = ADVANCED_FACE ( 'NONE', ( #227925 ), #196486, .F. ) ;
#3837 = ORIENTED_EDGE ( 'NONE', *, *, #83653, .F. ) ;
#3838 = FACE_OUTER_BOUND ( 'NONE', #154431, .T. ) ;
#3839 = DIRECTION ( 'NONE',  ( -1.000000000000000000, -0.000000000000000000, -0.000000000000000000 ) ) ;
#3841 = CARTESIAN_POINT ( 'NONE',  ( -21.14999999999999858, 6.540656951701240729, 0.000000000000000000 ) ) ;
#3840 = CARTESIAN_POINT ( 'NONE',  ( -21.05000000000000071, 69.74168394267991289, -103.0888090948464111 ) ) ;
#3842 = CIRCLE ( 'NONE', #241184, 0.09999999999999982514 ) ;
#3843 = DIRECTION ( 'NONE',  ( 0.000000000000000000, 0.000000000000000000, -1.000000000000000000 ) ) ;
#3844 = DIRECTION ( 'NONE',  ( 0.000000000000000000, 0.000000000000000000, -1.000000000000000000 ) ) ;
#3845 = DIRECTION ( 'NONE',  ( 1.734723475976817507E-14, -1.000000000000000000, 0.000000000000000000 ) ) ;
#3846 = ORIENTED_EDGE ( 'NONE', *, *, #68339, .T. ) ;
#3847 = CARTESIAN_POINT ( 'NONE',  ( 18.69999999999999929, 13.48082180182240819, -2.152770446119438130 ) ) ;
#3848 = ORIENTED_EDGE ( 'NONE', *, *, #131238, .F. ) ;
#3849 = AXIS2_PLACEMENT_3D ( 'NONE', #227179, #228489, #109795 ) ;
#3850 = VECTOR ( 'NONE', #190444, 1000.000000000000000 ) ;
#3852 = AXIS2_PLACEMENT_3D ( 'NONE', #94641, #230302, #169093 ) ;
#3851 = PLANE ( 'NONE',  #205364 ) ;
#3853 = ORIENTED_EDGE ( 'NONE', *, *, #166112, .T. ) ;
#3854 = ADVANCED_FACE ( 'NONE', ( #93540 ), #12753, .F. ) ;
#3855 = LINE ( 'NONE', #162947, #197306 ) ;
#3856 = AXIS2_PLACEMENT_3D ( 'NONE', #158051, #117590, #255772 ) ;
#3857 = DIRECTION ( 'NONE',  ( 1.000000000000000000, -7.304098846218134667E-16, -5.100424963727256530E-30 ) ) ;
#3858 = ORIENTED_EDGE ( 'NONE', *, *, #46431, .F. ) ;
#3859 = CARTESIAN_POINT ( 'NONE',  ( -18.58222699835055280, 18.41441690808118636, -236.9991004306322964 ) ) ;
#3860 = EDGE_LOOP ( 'NONE', ( #233354, #254636, #169036, #209580 ) ) ;
#3861 = DIRECTION ( 'NONE',  ( 0.000000000000000000, 0.000000000000000000, -1.000000000000000000 ) ) ;
#3862 = DIRECTION ( 'NONE',  ( -0.000000000000000000, 0.000000000000000000, -1.000000000000000000 ) ) ;
#3863 = DIRECTION ( 'NONE',  ( 0.000000000000000000, 0.2605042016806672911, -0.9654727137038716656 ) ) ;
#3864 = CARTESIAN_POINT ( 'NONE',  ( -18.45140287520616695, 77.16972416950922309, -241.7973009820151162 ) ) ;
#3865 = CARTESIAN_POINT ( 'NONE',  ( -21.45000000000000284, 12.05403912736948158, -220.1228874760914209 ) ) ;
#3866 = CARTESIAN_POINT ( 'NONE',  ( 21.05000000000000071, 5.500000000011153745, -179.9052660189130677 ) ) ;
#3867 = DIRECTION ( 'NONE',  ( 1.000000000000000000, -0.000000000000000000, -0.000000000000000000 ) ) ;
#3869 = ORIENTED_EDGE ( 'NONE', *, *, #251492, .T. ) ;
#3868 = CARTESIAN_POINT ( 'NONE',  ( -20.54999999999999716, 76.00000000001246292, -171.9231074845243938 ) ) ;
#3871 = FACE_OUTER_BOUND ( 'NONE', #63190, .T. ) ;
#3870 = CARTESIAN_POINT ( 'NONE',  ( -16.88853107394619002, 9.950878483358135185, -188.3529363468922213 ) ) ;
#3872 = VERTEX_POINT ( 'NONE', #191398 ) ;
#3874 = ORIENTED_EDGE ( 'NONE', *, *, #30580, .F. ) ;
#3873 = CARTESIAN_POINT ( 'NONE',  ( -20.94999999999999929, 86.27712145182582049, -209.5223386573213702 ) ) ;
#3875 = AXIS2_PLACEMENT_3D ( 'NONE', #112275, #53568, #151402 ) ;
#3876 = VERTEX_POINT ( 'NONE', #136499 ) ;
#3877 = DIRECTION ( 'NONE',  ( 1.000000000000000000, 0.000000000000000000, 0.000000000000000000 ) ) ;
#3878 = CARTESIAN_POINT ( 'NONE',  ( -22.39999999999999858, 11.65000000000000036, -3.469446951953614189E-15 ) ) ;
#3879 = CARTESIAN_POINT ( 'NONE',  ( 20.12500000000000000, 66.25000000001161027, -61.41133620241011215 ) ) ;
#3880 = ORIENTED_EDGE ( 'NONE', *, *, #42529, .T. ) ;
#3881 = FACE_OUTER_BOUND ( 'NONE', #8935, .T. ) ;
#3882 = CARTESIAN_POINT ( 'NONE',  ( 21.05000000000000071, 77.16270174995010223, -128.6231074845242972 ) ) ;
#3883 = AXIS2_PLACEMENT_3D ( 'NONE', #159584, #1770, #138685 ) ;
#3884 = DIRECTION ( 'NONE',  ( 0.000000000000000000, 1.000000000000000000, 6.982962677686266711E-15 ) ) ;
#3885 = DIRECTION ( 'NONE',  ( 0.000000000000000000, 0.000000000000000000, 1.000000000000000000 ) ) ;
#3886 = EDGE_CURVE ( 'NONE', #23293, #73958, #175665, .T. ) ;
#3887 = DIRECTION ( 'NONE',  ( -0.000000000000000000, 0.1350103645451807555, 0.9908441862701610203 ) ) ;
#3888 = ADVANCED_FACE ( 'NONE', ( #216046 ), #176967, .T. ) ;
#3889 = DIRECTION ( 'NONE',  ( 2.710505431213777355E-16, -1.000000000000000000, 0.000000000000000000 ) ) ;
#3890 = ORIENTED_EDGE ( 'NONE', *, *, #51001, .T. ) ;
#3891 = VERTEX_POINT ( 'NONE', #14024 ) ;
#3892 = CIRCLE ( 'NONE', #237121, 0.2000000000000057288 ) ;
#3893 = CARTESIAN_POINT ( 'NONE',  ( 20.94999999999999574, 6.350000000011161383, -110.3438220896831581 ) ) ;
#3894 = AXIS2_PLACEMENT_3D ( 'NONE', #143952, #104798, #245635 ) ;
#3895 = ORIENTED_EDGE ( 'NONE', *, *, #166766, .F. ) ;
#3896 = CARTESIAN_POINT ( 'NONE',  ( -21.64999999999999858, 7.350000000011155166, -54.75000000000000000 ) ) ;
#3898 = VERTEX_POINT ( 'NONE', #75297 ) ;
#3897 = AXIS2_PLACEMENT_3D ( 'NONE', #95566, #57713, #237656 ) ;
#3899 = DIRECTION ( 'NONE',  ( -0.000000000000000000, -0.000000000000000000, -1.000000000000000000 ) ) ;
#3900 = EDGE_CURVE ( 'NONE', #95339, #150427, #193876, .T. ) ;
#3901 = CARTESIAN_POINT ( 'NONE',  ( -23.15000000000000213, -11.74999999998884448, -88.75000000000004263 ) ) ;
#3902 = CARTESIAN_POINT ( 'NONE',  ( -21.05000000000000071, 14.05000000001115623, -173.0136950707609458 ) ) ;
#3903 = CARTESIAN_POINT ( 'NONE',  ( 21.05000000000000071, 64.27847795353595473, -247.1247091181747066 ) ) ;
#3904 = ADVANCED_FACE ( 'NONE', ( #253891 ), #55660, .T. ) ;
#3905 = CARTESIAN_POINT ( 'NONE',  ( 21.14999999999999858, 10.71339244341104013, -179.7500000000000000 ) ) ;
#3906 = ORIENTED_EDGE ( 'NONE', *, *, #25606, .T. ) ;
#3907 = AXIS2_PLACEMENT_3D ( 'NONE', #83576, #212, #160613 ) ;
#3908 = CIRCLE ( 'NONE', #212212, 11.64999999999999325 ) ;
#3909 = FACE_OUTER_BOUND ( 'NONE', #209598, .T. ) ;
#3910 = CARTESIAN_POINT ( 'NONE',  ( -16.88460203013674388, 66.04524099677682614, -182.6572156749861904 ) ) ;
#3911 = EDGE_CURVE ( 'NONE', #240371, #242014, #2139, .T. ) ;
#3912 = DIRECTION ( 'NONE',  ( 0.000000000000000000, 0.2128009952263605897, -0.9770955615653313941 ) ) ;
#3913 = DIRECTION ( 'NONE',  ( -0.000000000000000000, 6.982962677686266711E-15, -1.000000000000000000 ) ) ;
#3914 = ORIENTED_EDGE ( 'NONE', *, *, #196909, .T. ) ;
#3916 = DIRECTION ( 'NONE',  ( 0.000000000000000000, 0.000000000000000000, 1.000000000000000000 ) ) ;
#3915 = CARTESIAN_POINT ( 'NONE',  ( 21.05000000000000071, 28.40523720341322544, -239.6697522603257937 ) ) ;
#3917 = ORIENTED_EDGE ( 'NONE', *, *, #146920, .F. ) ;
#3919 = ORIENTED_EDGE ( 'NONE', *, *, #245952, .T. ) ;
#3918 = DIRECTION ( 'NONE',  ( 1.000000000000000000, 0.000000000000000000, 0.000000000000000000 ) ) ;
#3920 = CIRCLE ( 'NONE', #78718, 11.65000000000000036 ) ;
#3921 = ORIENTED_EDGE ( 'NONE', *, *, #230794, .T. ) ;
#3922 = CARTESIAN_POINT ( 'NONE',  ( -1.820710678118657944, -9.929289321870186313, -58.25000000000000000 ) ) ;
#3923 = CIRCLE ( 'NONE', #78891, 7.799999999999999822 ) ;
#3924 = AXIS2_PLACEMENT_3D ( 'NONE', #6274, #153213, #187520 ) ;
#3925 = DIRECTION ( 'NONE',  ( 1.000000000000000000, 0.000000000000000000, 0.000000000000000000 ) ) ;
#3926 = DIRECTION ( 'NONE',  ( 0.000000000000000000, 0.000000000000000000, -1.000000000000000000 ) ) ;
#3927 = ORIENTED_EDGE ( 'NONE', *, *, #472, .T. ) ;
#3928 = CARTESIAN_POINT ( 'NONE',  ( 18.57071067811864040, 10.17928932189250091, -54.75000000000000000 ) ) ;
#3929 = CIRCLE ( 'NONE', #149694, 11.74999999999999645 ) ;
#3930 = EDGE_CURVE ( 'NONE', #16721, #171947, #116964, .T. ) ;
#3931 = DIRECTION ( 'NONE',  ( 0.000000000000000000, 6.982962677686267499E-15, -1.000000000000000000 ) ) ;
#3933 = CARTESIAN_POINT ( 'NONE',  ( -21.05000000000000071, 11.75000000001115552, -59.98519422934605672 ) ) ;
#3932 = DIRECTION ( 'NONE',  ( -1.000000000000000000, 0.000000000000000000, 0.000000000000000000 ) ) ;
#3934 = EDGE_LOOP ( 'NONE', ( #188992, #180900, #27949, #5598 ) ) ;
#3935 = PRODUCT_DEFINITION_SHAPE ( 'NONE', 'NONE',  #258122 ) ;
#3936 = ORIENTED_EDGE ( 'NONE', *, *, #105558, .T. ) ;
#3937 = CARTESIAN_POINT ( 'NONE',  ( 19.90621891164687440, 64.25000000001176659, -78.19466220664698142 ) ) ;
#3938 = AXIS2_PLACEMENT_3D ( 'NONE', #43164, #19759, #137124 ) ;
#3939 = CARTESIAN_POINT ( 'NONE',  ( -16.81744102076749314, 22.97806745954242302, -230.9350634111226270 ) ) ;
#3940 = DIRECTION ( 'NONE',  ( 0.000000000000000000, 0.1455152366551700771, 0.9893560106964479628 ) ) ;
#3941 = ORIENTED_EDGE ( 'NONE', *, *, #226784, .F. ) ;
#3942 = CARTESIAN_POINT ( 'NONE',  ( 21.05000000000000071, 44.06843597547144498, -258.9974126733343951 ) ) ;
#3943 = ORIENTED_EDGE ( 'NONE', *, *, #98583, .T. ) ;
#3944 = FACE_OUTER_BOUND ( 'NONE', #53028, .T. ) ;
#3945 = ORIENTED_EDGE ( 'NONE', *, *, #118195, .F. ) ;
#3946 = VECTOR ( 'NONE', #228098, 1000.000000000000000 ) ;
#3947 = AXIS2_PLACEMENT_3D ( 'NONE', #87728, #96399, #175983 ) ;
#3948 = FACE_OUTER_BOUND ( 'NONE', #220229, .T. ) ;
#3949 = AXIS2_PLACEMENT_3D ( 'NONE', #96722, #255786, #137164 ) ;
#3950 = EDGE_CURVE ( 'NONE', #215500, #203407, #135413, .T. ) ;
#3951 = ORIENTED_EDGE ( 'NONE', *, *, #210536, .F. ) ;
#3952 = ORIENTED_EDGE ( 'NONE', *, *, #184238, .T. ) ;
#3953 = ORIENTED_EDGE ( 'NONE', *, *, #123060, .F. ) ;
#3954 = DIRECTION ( 'NONE',  ( 1.000000000000000000, -1.836970198721029934E-16, -1.282749433769087582E-30 ) ) ;
#3955 = ORIENTED_EDGE ( 'NONE', *, *, #88344, .T. ) ;
#3957 = VERTEX_POINT ( 'NONE', #154831 ) ;
#3956 = CARTESIAN_POINT ( 'NONE',  ( 20.73486653747088582, 7.250000000011182166, -143.2500000000000284 ) ) ;
#3958 = EDGE_CURVE ( 'NONE', #94619, #150045, #110663, .T. ) ;
#3959 = ORIENTED_EDGE ( 'NONE', *, *, #89948, .T. ) ;
#3960 = CIRCLE ( 'NONE', #87156, 4.049999999999998046 ) ;
#3963 = ORIENTED_EDGE ( 'NONE', *, *, #30172, .T. ) ;
#3962 = ORIENTED_EDGE ( 'NONE', *, *, #237201, .F. ) ;
#3961 = CARTESIAN_POINT ( 'NONE',  ( 18.58685178364170199, 78.17487933103092246, -231.4413402867085665 ) ) ;
#3964 = AXIS2_PLACEMENT_3D ( 'NONE', #112383, #135770, #35439 ) ;
#3965 = EDGE_CURVE ( 'NONE', #120372, #6846, #74023, .T. ) ;
#3966 = EDGE_CURVE ( 'NONE', #102057, #206913, #135597, .T. ) ;
#3967 = ORIENTED_EDGE ( 'NONE', *, *, #25384, .T. ) ;
#3968 = CARTESIAN_POINT ( 'NONE',  ( 20.94999999999999929, 5.900000000011162093, -157.2809002353436654 ) ) ;
#3969 = AXIS2_PLACEMENT_3D ( 'NONE', #198040, #199350, #145435 ) ;
#3970 = CARTESIAN_POINT ( 'NONE',  ( 20.95512820512820440, 67.12384868372450342, -194.9644784893834810 ) ) ;
#3971 = CYLINDRICAL_SURFACE ( 'NONE', #113661, 0.09999999999999609201 ) ;
#3972 = ORIENTED_EDGE ( 'NONE', *, *, #193163, .F. ) ;
#3973 = DIRECTION ( 'NONE',  ( 0.000000000000000000, 0.4999999999999799605, -0.8660254037844502539 ) ) ;
#3975 = ORIENTED_EDGE ( 'NONE', *, *, #60651, .T. ) ;
#3974 = CARTESIAN_POINT ( 'NONE',  ( 21.76363531954645936, 7.012936547882880234, -167.4009981257005393 ) ) ;
#3976 = DIRECTION ( 'NONE',  ( -1.000000000000000000, 0.000000000000000000, 0.000000000000000000 ) ) ;
#3978 = ORIENTED_EDGE ( 'NONE', *, *, #16744, .T. ) ;
#3977 = DIRECTION ( 'NONE',  ( 0.000000000000000000, -1.000000000000000000, 0.000000000000000000 ) ) ;
#3979 = ADVANCED_FACE ( 'NONE', ( #36157 ), #255129, .F. ) ;
#3980 = VERTEX_POINT ( 'NONE', #233084 ) ;
#3981 = EDGE_CURVE ( 'NONE', #165098, #91127, #72733, .T. ) ;
#3982 = ORIENTED_EDGE ( 'NONE', *, *, #140128, .T. ) ;
#3983 = ORIENTED_EDGE ( 'NONE', *, *, #184256, .T. ) ;
#3984 = TOROIDAL_SURFACE ( 'NONE', #49779, 1.900000000000002576, 0.1000000000000000056 ) ;
#3985 = CARTESIAN_POINT ( 'NONE',  ( -18.59999999999999787, 48.05114133249968944, -246.4758750954581785 ) ) ;
#3986 = CARTESIAN_POINT ( 'NONE',  ( -18.50000000000000000, 51.38014393322265505, -230.1906178717505611 ) ) ;
#3988 = ORIENTED_EDGE ( 'NONE', *, *, #147676, .T. ) ;
#3987 = ORIENTED_EDGE ( 'NONE', *, *, #66005, .T. ) ;
#3989 = ORIENTED_EDGE ( 'NONE', *, *, #212952, .F. ) ;
#3990 = CARTESIAN_POINT ( 'NONE',  ( 21.05095171578076574, 61.94553090543893603, -221.8162262668083429 ) ) ;
#3991 = ORIENTED_EDGE ( 'NONE', *, *, #92230, .F. ) ;
#3992 = VERTEX_POINT ( 'NONE', #33625 ) ;
#3993 = ADVANCED_FACE ( 'NONE', ( #192658 ), #256336, .T. ) ;
#3994 = DIRECTION ( 'NONE',  ( 0.000000000000000000, -0.3042567129660006531, -0.9525900758537875213 ) ) ;
#3996 = ORIENTED_EDGE ( 'NONE', *, *, #128666, .F. ) ;
#3995 = DIRECTION ( 'NONE',  ( -0.000000000000000000, -0.000000000000000000, -1.000000000000000000 ) ) ;
#3997 = ADVANCED_FACE ( 'NONE', ( #76540 ), #219910, .T. ) ;
#3998 = FACE_OUTER_BOUND ( 'NONE', #59322, .T. ) ;
#3999 = EDGE_CURVE ( 'NONE', #43854, #174426, #199068, .T. ) ;
#4001 = CARTESIAN_POINT ( 'NONE',  ( -20.94999999999999929, 77.36087058720393372, -94.95010955743333625 ) ) ;
#4000 = CARTESIAN_POINT ( 'NONE',  ( -16.94389599338512298, 22.96018495058455855, -230.8787477556889769 ) ) ;
#4002 = ORIENTED_EDGE ( 'NONE', *, *, #27353, .T. ) ;
#4004 = ORIENTED_EDGE ( 'NONE', *, *, #206924, .T. ) ;
#4003 = VERTEX_POINT ( 'NONE', #79093 ) ;
#4006 = VECTOR ( 'NONE', #114156, 1000.000000000000000 ) ;
#4005 = DIRECTION ( 'NONE',  ( 0.000000000000000000, -1.000000000000000000, -6.982962677686265922E-15 ) ) ;
#4007 = AXIS2_PLACEMENT_3D ( 'NONE', #88671, #45719, #148692 ) ;
#4008 = AXIS2_PLACEMENT_3D ( 'NONE', #177996, #118002, #136252 ) ;
#4009 = AXIS2_PLACEMENT_3D ( 'NONE', #139379, #58560, #59837 ) ;
#4010 = VERTEX_POINT ( 'NONE', #217321 ) ;
#4011 = TOROIDAL_SURFACE ( 'NONE', #33279, 0.2000000000000000111, 0.1000000000000000056 ) ;
#4012 = CARTESIAN_POINT ( 'NONE',  ( 18.39999999999999503, 64.25000000001230660, -157.3731074845244393 ) ) ;
#4013 = ORIENTED_EDGE ( 'NONE', *, *, #8450, .T. ) ;
#4014 = ADVANCED_FACE ( 'NONE', ( #179523 ), #139050, .T. ) ;
#4015 = ORIENTED_EDGE ( 'NONE', *, *, #254264, .T. ) ;
#4016 = CARTESIAN_POINT ( 'NONE',  ( 20.94999999999999574, 1.835341550235567887, -179.0551512925629538 ) ) ;
#4017 = ORIENTED_EDGE ( 'NONE', *, *, #162333, .F. ) ;
#4018 = CARTESIAN_POINT ( 'NONE',  ( 21.05000000000000426, 34.11496337544747348, -243.6628028815440530 ) ) ;
#4019 = ORIENTED_EDGE ( 'NONE', *, *, #92586, .T. ) ;
#4020 = CARTESIAN_POINT ( 'NONE',  ( 20.01093837587850288, 64.25000000001220712, -145.2687100499267672 ) ) ;
#4021 = DIRECTION ( 'NONE',  ( 0.000000000000000000, 0.000000000000000000, 1.000000000000000000 ) ) ;
#4023 = CARTESIAN_POINT ( 'NONE',  ( -16.89935556175728593, 9.950000000011007373, -120.8603236371143765 ) ) ;
#4022 = DIRECTION ( 'NONE',  ( 0.000000000000000000, 0.8700118002898321601, -0.4930308989875230585 ) ) ;
#4024 = PLANE ( 'NONE',  #89798 ) ;
#4026 = LINE ( 'NONE', #83533, #145039 ) ;
#4025 = AXIS2_PLACEMENT_3D ( 'NONE', #10207, #28519, #144551 ) ;
#4027 = CARTESIAN_POINT ( 'NONE',  ( -18.59999999999999787, 11.65000000001115232, -107.5148057706540357 ) ) ;
#4028 = EDGE_CURVE ( 'NONE', #21614, #76960, #152386, .T. ) ;
#4029 = AXIS2_PLACEMENT_3D ( 'NONE', #147918, #173619, #116173 ) ;
#4030 = FACE_OUTER_BOUND ( 'NONE', #48518, .T. ) ;
#4031 = CARTESIAN_POINT ( 'NONE',  ( 20.73486653747088937, 41.93205750249717312, -238.6967134976849820 ) ) ;
#4032 = ORIENTED_EDGE ( 'NONE', *, *, #186651, .F. ) ;
#4033 = AXIS2_PLACEMENT_3D ( 'NONE', #105698, #91313, #28815 ) ;
#4035 = EDGE_LOOP ( 'NONE', ( #65126, #86189, #98111, #18707 ) ) ;
#4034 = ORIENTED_EDGE ( 'NONE', *, *, #172720, .T. ) ;
#4036 = VERTEX_POINT ( 'NONE', #200353 ) ;
#4037 = EDGE_CURVE ( 'NONE', #98180, #34831, #193791, .T. ) ;
#4038 = PLANE ( 'NONE',  #36375 ) ;
#4039 = DIRECTION ( 'NONE',  ( -0.000000000000000000, 6.982962677686266711E-15, -1.000000000000000000 ) ) ;
#4041 = CARTESIAN_POINT ( 'NONE',  ( -12.47155713865592119, 9.375669526425772560, -15.86779000938594031 ) ) ;
#4040 = FACE_OUTER_BOUND ( 'NONE', #165999, .T. ) ;
#4042 = CARTESIAN_POINT ( 'NONE',  ( -18.59999999999999787, 1.851028230152016674, -145.6539132694225032 ) ) ;
#4043 = VERTEX_POINT ( 'NONE', #141655 ) ;
#4044 = EDGE_CURVE ( 'NONE', #218042, #236168, #21721, .T. ) ;
#4045 = CYLINDRICAL_SURFACE ( 'NONE', #163268, 0.09999999999999939493 ) ;
#4046 = CARTESIAN_POINT ( 'NONE',  ( 23.25000000000000000, 85.00000000001232081, -160.1291383618718385 ) ) ;
#4047 = LINE ( 'NONE', #83558, #118219 ) ;
#4048 = EDGE_CURVE ( 'NONE', #7443, #96501, #218993, .T. ) ;
#4049 = CYLINDRICAL_SURFACE ( 'NONE', #224627, 0.09999999999999771572 ) ;
#4050 = ORIENTED_EDGE ( 'NONE', *, *, #162882, .T. ) ;
#4051 = TOROIDAL_SURFACE ( 'NONE', #120778, 0.2000000000000000111, 0.1000000000000000056 ) ;
#4052 = CARTESIAN_POINT ( 'NONE',  ( 18.49999999999999645, -9.419209763409250868, -7.247769462758938630 ) ) ;
#4053 = EDGE_CURVE ( 'NONE', #133516, #58292, #156501, .T. ) ;
#4054 = CARTESIAN_POINT ( 'NONE',  ( -21.05000000000000071, 0.03175835306658782164, -94.24115287691907383 ) ) ;
#4055 = EDGE_CURVE ( 'NONE', #2919, #77481, #242036, .T. ) ;
#4056 = ORIENTED_EDGE ( 'NONE', *, *, #10821, .F. ) ;
#4057 = CARTESIAN_POINT ( 'NONE',  ( 18.54999999999999716, 14.15900158805616371, -219.2550725561364686 ) ) ;
#4058 = DIRECTION ( 'NONE',  ( -1.000000000000000000, 0.000000000000000000, 0.000000000000000000 ) ) ;
#4059 = VECTOR ( 'NONE', #190730, 1000.000000000000000 ) ;
#4060 = CARTESIAN_POINT ( 'NONE',  ( 18.59999999999999432, 1.162701749949165642, -175.4999999999999716 ) ) ;
#4061 = CARTESIAN_POINT ( 'NONE',  ( 20.90000000000000213, 6.783826713665066066, 9.593862367105556288 ) ) ;
#4062 = DIRECTION ( 'NONE',  ( 0.000000000000000000, -0.9908441862701596881, -0.1350103645451904977 ) ) ;
#4063 = DIRECTION ( 'NONE',  ( 1.000000000000000000, 0.000000000000000000, 0.000000000000000000 ) ) ;
#4064 = VERTEX_POINT ( 'NONE', #19141 ) ;
#4065 = DIRECTION ( 'NONE',  ( -1.000000000000000000, -1.652117596168391700E-15, -1.153667551319263085E-29 ) ) ;
#4066 = CARTESIAN_POINT ( 'NONE',  ( -23.25000000000000000, 77.83585931145546510, -91.41866831572575336 ) ) ;
#4067 = DIRECTION ( 'NONE',  ( -1.000000000000000000, 0.000000000000000000, 0.000000000000000000 ) ) ;
#4069 = CARTESIAN_POINT ( 'NONE',  ( 18.54999999999999716, 22.41143600680915426, -231.9928577185252152 ) ) ;
#4068 = DIRECTION ( 'NONE',  ( -1.000000000000000000, -0.000000000000000000, -0.000000000000000000 ) ) ;
#4070 = CARTESIAN_POINT ( 'NONE',  ( -18.59999999999999787, 1.261786168576181755, -175.5864989635454378 ) ) ;
#4071 = DIRECTION ( 'NONE',  ( 0.000000000000000000, 0.000000000000000000, -1.000000000000000000 ) ) ;
#4072 = DIRECTION ( 'NONE',  ( 1.000000000000000000, 0.000000000000000000, 0.000000000000000000 ) ) ;
#4073 = AXIS2_PLACEMENT_3D ( 'NONE', #251745, #73144, #232206 ) ;
#4075 = ORIENTED_EDGE ( 'NONE', *, *, #146740, .T. ) ;
#4074 = DIRECTION ( 'NONE',  ( 1.000000000000000000, 0.000000000000000000, -0.000000000000000000 ) ) ;
#4076 = EDGE_CURVE ( 'NONE', #96396, #69997, #60755, .T. ) ;
#4078 = EDGE_CURVE ( 'NONE', #48315, #45489, #98157, .T. ) ;
#4077 = AXIS2_PLACEMENT_3D ( 'NONE', #31474, #53573, #110979 ) ;
#4079 = TOROIDAL_SURFACE ( 'NONE', #237322, 11.65000000000000036, 0.1000000000000000056 ) ;
#4080 = ADVANCED_FACE ( 'NONE', ( #122104 ), #257691, .F. ) ;
#4081 = TOROIDAL_SURFACE ( 'NONE', #249613, 11.65000000000000036, 0.1000000000000000056 ) ;
#4082 = AXIS2_PLACEMENT_3D ( 'NONE', #103246, #4162, #197548 ) ;
#4083 = CARTESIAN_POINT ( 'NONE',  ( -16.94445028196807002, 66.00793639031427062, -115.6304376629428106 ) ) ;
#4084 = ADVANCED_FACE ( 'NONE', ( #201627 ), #252299, .F. ) ;
#4085 = CARTESIAN_POINT ( 'NONE',  ( 21.78635804494511419, 65.29411581985623059, -242.6195740507382084 ) ) ;
#4086 = EDGE_CURVE ( 'NONE', #103201, #133004, #31593, .T. ) ;
#4087 = PLANE ( 'NONE',  #187789 ) ;
#4088 = EDGE_LOOP ( 'NONE', ( #66233, #92551, #202705, #247143 ) ) ;
#4089 = CIRCLE ( 'NONE', #8204, 0.09999999999999939493 ) ;
#4090 = DIRECTION ( 'NONE',  ( 1.000000000000000000, 0.000000000000000000, 0.000000000000000000 ) ) ;
#4091 = CIRCLE ( 'NONE', #187454, 0.2000000000000057288 ) ;
#4092 = CIRCLE ( 'NONE', #149872, 12.87499999999999822 ) ;
#4093 = DIRECTION ( 'NONE',  ( 0.000000000000000000, 0.000000000000000000, -1.000000000000000000 ) ) ;
#4094 = CARTESIAN_POINT ( 'NONE',  ( -20.94999999999999929, 11.64999999999999680, -26.71613433702190576 ) ) ;
#4095 = CIRCLE ( 'NONE', #29082, 0.09999999999999766020 ) ;
#4096 = AXIS2_PLACEMENT_3D ( 'NONE', #226436, #206904, #28301 ) ;
#4097 = EDGE_CURVE ( 'NONE', #224786, #244466, #201310, .T. ) ;
#4098 = VERTEX_POINT ( 'NONE', #98635 ) ;
#4099 = DIRECTION ( 'NONE',  ( 0.000000000000000000, 0.000000000000000000, 1.000000000000000000 ) ) ;
#4101 = EDGE_LOOP ( 'NONE', ( #159843, #251637, #155073, #209880 ) ) ;
#4100 = CARTESIAN_POINT ( 'NONE',  ( -21.05000000000000071, 18.24178995542692050, -237.7003448530951459 ) ) ;
#4103 = CARTESIAN_POINT ( 'NONE',  ( 21.12230431290518951, 0.005209851689007149664, 6.457566653293008052 ) ) ;
#4102 = CARTESIAN_POINT ( 'NONE',  ( -20.94999999999999929, 1.115600667400684642E-11, -96.50000000000004263 ) ) ;
#4104 = CIRCLE ( 'NONE', #91590, 0.1000000000000028644 ) ;
#4105 = DIRECTION ( 'NONE',  ( 1.000000000000000000, 0.000000000000000000, 0.000000000000000000 ) ) ;
#4106 = ORIENTED_EDGE ( 'NONE', *, *, #82251, .F. ) ;
#4107 = EDGE_CURVE ( 'NONE', #13417, #257729, #243935, .T. ) ;
#4108 = CARTESIAN_POINT ( 'NONE',  ( -18.59999999999999787, 64.35000000001208775, -129.5083017138703667 ) ) ;
#4109 = CARTESIAN_POINT ( 'NONE',  ( -21.05000000000000071, 69.29728574394107454, -247.8047749431123918 ) ) ;
#4110 = VERTEX_POINT ( 'NONE', #11138 ) ;
#4111 = DIRECTION ( 'NONE',  ( 1.000000000000000000, -0.000000000000000000, -0.000000000000000000 ) ) ;
#4112 = DIRECTION ( 'NONE',  ( -2.952720810173288619E-16, 0.4721928772777346239, 0.8814952561688430555 ) ) ;
#4113 = CARTESIAN_POINT ( 'NONE',  ( 18.59999999999999787, 16.52766025697963315, -240.8672687545768270 ) ) ;
#4114 = CARTESIAN_POINT ( 'NONE',  ( -2.995603634470891112E-16, 84.13386079949725627, -218.4216076940958260 ) ) ;
#4115 = ORIENTED_EDGE ( 'NONE', *, *, #127897, .F. ) ;
#4116 = ORIENTED_EDGE ( 'NONE', *, *, #251473, .T. ) ;
#4117 = B_SPLINE_CURVE_WITH_KNOTS ( 'NONE', 3,
 ( #131527, #152407, #188942, #250195, #230642, #71580, #228073, #51971, #151102, #247625, #128972, #10318, #109381, #208520, #231934, #29891 ),
 .UNSPECIFIED., .F., .F.,
 ( 4, 3, 3, 3, 3, 4 ),
 ( 0.000000000000000000, 2.209833635978096787E-05, 5.595056164119028614E-05, 8.979992002654958564E-05, 0.0001236482757198868287, 0.0001574984039362969566 ),
 .UNSPECIFIED. ) ;
#4118 = CARTESIAN_POINT ( 'NONE',  ( 22.45463910399149299, 76.00000000001263345, -81.17267829470745255 ) ) ;
#4119 = TOROIDAL_SURFACE ( 'NONE', #116560, 0.2000000000000000111, 0.1000000000000000056 ) ;
#4120 = CARTESIAN_POINT ( 'NONE',  ( -23.25000000000000000, -11.64999999998884483, -55.25000000000004974 ) ) ;
#4121 = CARTESIAN_POINT ( 'NONE',  ( 21.05000000000000071, 43.57568952063339651, -245.1784935019914826 ) ) ;
#4122 = FACE_OUTER_BOUND ( 'NONE', #6960, .T. ) ;
#4123 = FACE_OUTER_BOUND ( 'NONE', #96548, .T. ) ;
#4124 = AXIS2_PLACEMENT_3D ( 'NONE', #9097, #110753, #115900 ) ;
#4126 = CYLINDRICAL_SURFACE ( 'NONE', #182630, 0.1000000000000028644 ) ;
#4125 = DIRECTION ( 'NONE',  ( 0.000000000000000000, 0.8814952561688437216, -0.4721928772777334582 ) ) ;
#4127 = CARTESIAN_POINT ( 'NONE',  ( -16.83199030136658081, 66.06935196689811107, -56.75070646186691903 ) ) ;
#4128 = CARTESIAN_POINT ( 'NONE',  ( -18.40000000000000213, 46.91436717984746707, -255.3877622108296634 ) ) ;
#4129 = ORIENTED_EDGE ( 'NONE', *, *, #11231, .F. ) ;
#4130 = VECTOR ( 'NONE', #187871, 1000.000000000000000 ) ;
#4132 = ORIENTED_EDGE ( 'NONE', *, *, #31243, .T. ) ;
#4131 = DIRECTION ( 'NONE',  ( 2.557131231893036985E-16, -0.8496786552930077896, -0.5273008465188220306 ) ) ;
#4133 = CARTESIAN_POINT ( 'NONE',  ( 20.94999999999999929, 65.27628289530480288, -162.3581939154368285 ) ) ;
#4134 = FACE_OUTER_BOUND ( 'NONE', #203796, .T. ) ;
#4136 = DIRECTION ( 'NONE',  ( 0.000000000000000000, -0.9770955615653543758, -0.2128009952262553683 ) ) ;
#4135 = CARTESIAN_POINT ( 'NONE',  ( -21.65000000000000213, 66.05000000001261640, -190.7731074845244166 ) ) ;
#4137 = EDGE_CURVE ( 'NONE', #102962, #83472, #88070, .T. ) ;
#4138 = ORIENTED_EDGE ( 'NONE', *, *, #21133, .F. ) ;
#4140 = DIRECTION ( 'NONE',  ( -0.000000000000000000, 1.000000000000000000, -0.000000000000000000 ) ) ;
#4139 = CARTESIAN_POINT ( 'NONE',  ( -16.82542659449980604, 66.06550010858417465, -56.77847188449814553 ) ) ;
#4141 = DIRECTION ( 'NONE',  ( -1.000000000000000000, -0.000000000000000000, -0.000000000000000000 ) ) ;
#4142 = DIRECTION ( 'NONE',  ( 2.952720810173289605E-16, 0.9651348961777155289, -0.2617529984165038459 ) ) ;
#4143 = DIRECTION ( 'NONE',  ( 1.186688945009009831E-16, -1.000000000000000000, 0.000000000000000000 ) ) ;
#4144 = DIRECTION ( 'NONE',  ( 0.000000000000000000, -6.853228547068871147E-15, 1.000000000000000000 ) ) ;
#4145 = ORIENTED_EDGE ( 'NONE', *, *, #72590, .T. ) ;
#4147 = ORIENTED_EDGE ( 'NONE', *, *, #135727, .F. ) ;
#4146 = AXIS2_PLACEMENT_3D ( 'NONE', #228967, #90718, #131136 ) ;
#4148 = CIRCLE ( 'NONE', #145598, 0.09999999999999939493 ) ;
#4149 = DIRECTION ( 'NONE',  ( 0.000000000000000000, 0.8814952561688476074, -0.4721928772777262417 ) ) ;
#4150 = VERTEX_POINT ( 'NONE', #46390 ) ;
#4151 = ADVANCED_FACE ( 'NONE', ( #146760 ), #27513, .T. ) ;
#4152 = LINE ( 'NONE', #44579, #184468 ) ;
#4153 = AXIS2_PLACEMENT_3D ( 'NONE', #240403, #61755, #224670 ) ;
#4154 = VERTEX_POINT ( 'NONE', #90655 ) ;
#4155 = DIRECTION ( 'NONE',  ( 0.000000000000000000, 0.8814952561688429444, -0.4721928772777345684 ) ) ;
#4156 = CARTESIAN_POINT ( 'NONE',  ( 20.95000000000005613, 66.15000000001120384, -5.923107484524795296 ) ) ;
#4157 = DIRECTION ( 'NONE',  ( 0.000000000000000000, -1.000000000000000000, -0.000000000000000000 ) ) ;
#4158 = ORIENTED_EDGE ( 'NONE', *, *, #56990, .T. ) ;
#4159 = DIRECTION ( 'NONE',  ( 0.000000000000000000, 0.000000000000000000, 1.000000000000000000 ) ) ;
#4160 = DIRECTION ( 'NONE',  ( 1.000000000000000000, 0.000000000000000000, 0.000000000000000000 ) ) ;
#4161 = LINE ( 'NONE', #6736, #145171 ) ;
#4162 = DIRECTION ( 'NONE',  ( 1.000000000000000000, -0.000000000000000000, -0.000000000000000000 ) ) ;
#4163 = CARTESIAN_POINT ( 'NONE',  ( -16.97683809663753252, 44.70268985058793731, -235.0448293460806894 ) ) ;
#4165 = AXIS2_PLACEMENT_3D ( 'NONE', #175488, #100708, #155931 ) ;
#4164 = CARTESIAN_POINT ( 'NONE',  ( -20.54999999999999716, 13.65786464920749843, -219.7735913778983559 ) ) ;
#4166 = AXIS2_PLACEMENT_3D ( 'NONE', #98148, #180297, #238993 ) ;
#4167 = CARTESIAN_POINT ( 'NONE',  ( -20.64999999999999858, 71.75000000001259082, -191.2731074845243882 ) ) ;
#4168 = ORIENTED_EDGE ( 'NONE', *, *, #29647, .F. ) ;
#4170 = DIRECTION ( 'NONE',  ( 0.000000000000000000, 0.000000000000000000, 1.000000000000000000 ) ) ;
#4169 = DIRECTION ( 'NONE',  ( 0.000000000000000000, 0.000000000000000000, 1.000000000000000000 ) ) ;
#4171 = ORIENTED_EDGE ( 'NONE', *, *, #257302, .F. ) ;
#4173 = ORIENTED_EDGE ( 'NONE', *, *, #60970, .F. ) ;
#4172 = CARTESIAN_POINT ( 'NONE',  ( -23.15000000000000213, 73.50000000001186606, -89.79848556176223440 ) ) ;
#4174 = ORIENTED_EDGE ( 'NONE', *, *, #158792, .F. ) ;
#4175 = LINE ( 'NONE', #60294, #24131 ) ;
#4176 = CARTESIAN_POINT ( 'NONE',  ( -23.25000000000000000, 1.115651490242849210E-11, -62.85000000000004405 ) ) ;
#4177 = DIRECTION ( 'NONE',  ( -1.000000000000000000, 0.000000000000000000, 0.000000000000000000 ) ) ;
#4178 = DIRECTION ( 'NONE',  ( 0.000000000000000000, 0.9126074666063769270, 0.4088369013363280513 ) ) ;
#4179 = VERTEX_POINT ( 'NONE', #68547 ) ;
#4180 = CARTESIAN_POINT ( 'NONE',  ( -18.59999999999999787, 77.83534155023670564, -158.3679561919613548 ) ) ;
#4181 = DIRECTION ( 'NONE',  ( 0.000000000000000000, -0.000000000000000000, -1.000000000000000000 ) ) ;
#4182 = ORIENTED_EDGE ( 'NONE', *, *, #94931, .F. ) ;
#4183 = EDGE_CURVE ( 'NONE', #226447, #156407, #227604, .T. ) ;
#4184 = CARTESIAN_POINT ( 'NONE',  ( -21.05000000000000071, 1.115650877919449575E-11, -104.6000000000000512 ) ) ;
#4185 = VECTOR ( 'NONE', #99583, 1000.000000000000000 ) ;
#4186 = CIRCLE ( 'NONE', #149967, 0.1999999999999945155 ) ;
#4188 = AXIS2_PLACEMENT_3D ( 'NONE', #227607, #206772, #110226 ) ;
#4187 = CARTESIAN_POINT ( 'NONE',  ( -22.39999999999999858, -0.09999999999999939493, 11.64957080754479968 ) ) ;
#4189 = EDGE_LOOP ( 'NONE', ( #58272, #152750, #93323, #114633 ) ) ;
#4190 = CARTESIAN_POINT ( 'NONE',  ( -21.55000000000000426, 12.09451175070297069, -220.1140729702605370 ) ) ;
#4191 = CIRCLE ( 'NONE', #204094, 0.09999999999999635569 ) ;
#4192 = DIRECTION ( 'NONE',  ( 1.000000000000000000, 0.000000000000000000, 0.000000000000000000 ) ) ;
#4193 = ORIENTED_EDGE ( 'NONE', *, *, #40686, .F. ) ;
#4194 = CARTESIAN_POINT ( 'NONE',  ( 22.50000000000000000, 76.00000000001237765, -170.0231074845243597 ) ) ;
#4195 = EDGE_CURVE ( 'NONE', #239043, #28788, #35690, .T. ) ;
#4196 = DIRECTION ( 'NONE',  ( 1.000000000000000000, 0.000000000000000000, 0.000000000000000000 ) ) ;
#4197 = CARTESIAN_POINT ( 'NONE',  ( 18.59999999999999787, 79.28756800457986742, -196.2274082906208434 ) ) ;
#4198 = EDGE_CURVE ( 'NONE', #73777, #33295, #248030, .T. ) ;
#4199 = DIRECTION ( 'NONE',  ( 0.000000000000000000, -6.938893903907222067E-15, 1.000000000000000000 ) ) ;
#4200 = AXIS2_PLACEMENT_3D ( 'NONE', #93253, #131103, #114098 ) ;
#4201 = CIRCLE ( 'NONE', #229074, 0.09999999999999939493 ) ;
#4202 = EDGE_CURVE ( 'NONE', #193535, #175419, #29454, .T. ) ;
#4203 = DIRECTION ( 'NONE',  ( 1.000000000000000000, -0.000000000000000000, -0.000000000000000000 ) ) ;
#4204 = DIRECTION ( 'NONE',  ( 0.000000000000000000, 0.008583690987127922528, 0.9999631594459055250 ) ) ;
#4205 = CARTESIAN_POINT ( 'NONE',  ( 18.54999999999999716, 48.78215419113038109, -213.4964773079645681 ) ) ;
#4206 = ORIENTED_EDGE ( 'NONE', *, *, #65773, .F. ) ;
#4207 = DIRECTION ( 'NONE',  ( 1.000000000000000000, 0.000000000000000000, 0.000000000000000000 ) ) ;
#4208 = ORIENTED_EDGE ( 'NONE', *, *, #36987, .F. ) ;
#4209 = CARTESIAN_POINT ( 'NONE',  ( -16.87036670365549895, 12.42497885867826390, -211.1079079717509046 ) ) ;
#4210 = FACE_OUTER_BOUND ( 'NONE', #202192, .T. ) ;
#4212 = VERTEX_POINT ( 'NONE', #125929 ) ;
#4211 = DIRECTION ( 'NONE',  ( -1.000000000000000000, 0.000000000000000000, 0.000000000000000000 ) ) ;
#4214 = ORIENTED_EDGE ( 'NONE', *, *, #33008, .F. ) ;
#4213 = LINE ( 'NONE', #22529, #191256 ) ;
#4215 = ADVANCED_FACE ( 'NONE', ( #127233 ), #108938, .F. ) ;
#4216 = DIRECTION ( 'NONE',  ( 0.000000000000000000, 0.8814952561688449428, -0.4721928772777310157 ) ) ;
#4217 = CARTESIAN_POINT ( 'NONE',  ( -23.25000000000000000, -0.1008583690987122083, 11.74956712348939192 ) ) ;
#4218 = CARTESIAN_POINT ( 'NONE',  ( 21.05000000000000071, 84.66355140188167638, -179.5472086025916099 ) ) ;
#4219 = CARTESIAN_POINT ( 'NONE',  ( 20.94999999999999929, -1.835341550213257733, -179.0551512925629538 ) ) ;
#4221 = EDGE_LOOP ( 'NONE', ( #8046, #166375, #35510, #225171 ) ) ;
#4220 = DIRECTION ( 'NONE',  ( 0.000000000000000000, -6.467318590049456648E-15, 1.000000000000000000 ) ) ;
#4222 = EDGE_CURVE ( 'NONE', #245289, #125503, #205470, .T. ) ;
#4223 = DIRECTION ( 'NONE',  ( -0.000000000000000000, -1.000000000000000000, 6.308085367188393199E-16 ) ) ;
#4224 = VERTEX_POINT ( 'NONE', #69846 ) ;
#4225 = ORIENTED_EDGE ( 'NONE', *, *, #100171, .F. ) ;
#4226 = CARTESIAN_POINT ( 'NONE',  ( -18.37151313414641152, 85.57101412579034161, -62.70644457528530324 ) ) ;
#4227 = CARTESIAN_POINT ( 'NONE',  ( 19.75857864376269291, 34.58225676390223668, -235.1091250528070589 ) ) ;
#4228 = ORIENTED_EDGE ( 'NONE', *, *, #146920, .T. ) ;
#4229 = CARTESIAN_POINT ( 'NONE',  ( 20.85000000000000142, 46.01276039807270024, -256.6622985126337539 ) ) ;
#4230 = EDGE_CURVE ( 'NONE', #108499, #179534, #145500, .T. ) ;
#4231 = CARTESIAN_POINT ( 'NONE',  ( -16.86379686415369861, 9.975217759264314310, -180.0666101109096928 ) ) ;
#4232 = ORIENTED_EDGE ( 'NONE', *, *, #44939, .T. ) ;
#4233 = AXIS2_PLACEMENT_3D ( 'NONE', #118675, #177380, #41702 ) ;
#4234 = DIRECTION ( 'NONE',  ( 1.000000000000000000, -0.000000000000000000, -0.000000000000000000 ) ) ;
#4235 = CIRCLE ( 'NONE', #137327, 0.09999999999999892308 ) ;
#4236 = LINE ( 'NONE', #83747, #80498 ) ;
#4237 = EDGE_CURVE ( 'NONE', #105073, #97258, #44028, .T. ) ;
#4238 = ORIENTED_EDGE ( 'NONE', *, *, #139069, .F. ) ;
#4239 = ORIENTED_EDGE ( 'NONE', *, *, #103625, .F. ) ;
#4240 = CARTESIAN_POINT ( 'NONE',  ( -18.59999999999999787, 43.52285900727589762, -245.0935880436369985 ) ) ;
#4241 = VECTOR ( 'NONE', #33020, 1000.000000000000000 ) ;
#4242 = VERTEX_POINT ( 'NONE', #184631 ) ;
#4243 = CARTESIAN_POINT ( 'NONE',  ( -16.81744102076749314, 9.950000000011142376, -46.15000000000000568 ) ) ;
#4244 = ORIENTED_EDGE ( 'NONE', *, *, #116881, .T. ) ;
#4246 = ORIENTED_EDGE ( 'NONE', *, *, #174461, .T. ) ;
#4245 = CARTESIAN_POINT ( 'NONE',  ( 22.10000000000000142, -3.262756495241484158E-15, 33.00000000000000000 ) ) ;
#4247 = VECTOR ( 'NONE', #78793, 1000.000000000000114 ) ;
#4249 = EDGE_CURVE ( 'NONE', #242555, #177524, #149919, .T. ) ;
#4248 = AXIS2_PLACEMENT_3D ( 'NONE', #172280, #73165, #212655 ) ;
#4250 = DIRECTION ( 'NONE',  ( 0.000000000000000000, -7.429790795770647916E-15, 1.000000000000000000 ) ) ;
#4251 = VERTEX_POINT ( 'NONE', #112805 ) ;
#4252 = CARTESIAN_POINT ( 'NONE',  ( 22.40000000000020819, -0.1008583690885111045, -88.75043287651033097 ) ) ;
#4253 = ORIENTED_EDGE ( 'NONE', *, *, #193929, .F. ) ;
#4255 = VERTEX_POINT ( 'NONE', #251002 ) ;
#4254 = ORIENTED_EDGE ( 'NONE', *, *, #248219, .T. ) ;
#4256 = DIRECTION ( 'NONE',  ( -1.000000000000000000, -0.000000000000000000, -0.000000000000000000 ) ) ;
#4257 = ADVANCED_FACE ( 'NONE', ( #151954 ), #73703, .F. ) ;
#4258 = CARTESIAN_POINT ( 'NONE',  ( -21.02374657821576065, 56.16603649953788135, -228.1013850333971504 ) ) ;
#4259 = ORIENTED_EDGE ( 'NONE', *, *, #86054, .F. ) ;
#4260 = AXIS2_PLACEMENT_3D ( 'NONE', #174190, #175452, #257470 ) ;
#4261 = CIRCLE ( 'NONE', #137536, 0.4999999999999944489 ) ;
#4262 = AXIS2_PLACEMENT_3D ( 'NONE', #181726, #124322, #42219 ) ;
#4263 = VECTOR ( 'NONE', #56005, 1000.000000000000227 ) ;
#4264 = VERTEX_POINT ( 'NONE', #16296 ) ;
#4265 = DIRECTION ( 'NONE',  ( 1.000000000000000000, 0.000000000000000000, 0.000000000000000000 ) ) ;
#4266 = FACE_OUTER_BOUND ( 'NONE', #120318, .T. ) ;
#4267 = EDGE_CURVE ( 'NONE', #92180, #44902, #131505, .T. ) ;
#4269 = EDGE_LOOP ( 'NONE', ( #127506, #27287, #231040, #171760 ) ) ;
#4268 = DIRECTION ( 'NONE',  ( 0.000000000000000000, 0.2617529984165033463, 0.9651348961777157509 ) ) ;
#4270 = DIRECTION ( 'NONE',  ( 0.000000000000000000, 1.000000000000000000, 0.000000000000000000 ) ) ;
#4271 = ORIENTED_EDGE ( 'NONE', *, *, #97443, .T. ) ;
#4272 = CARTESIAN_POINT ( 'NONE',  ( -18.50000972452446035, 65.70673848566998743, -131.0638252334829303 ) ) ;
#4273 = LINE ( 'NONE', #83780, #222849 ) ;
#4275 = EDGE_LOOP ( 'NONE', ( #20359, #19749, #40015, #160917 ) ) ;
#4274 = EDGE_CURVE ( 'NONE', #43942, #115699, #15002, .T. ) ;
#4276 = EDGE_CURVE ( 'NONE', #213072, #257480, #21560, .T. ) ;
#4277 = CARTESIAN_POINT ( 'NONE',  ( -16.87683809663752399, 39.52051071501344381, -224.9973737707144892 ) ) ;
#4278 = VECTOR ( 'NONE', #28057, 1000.000000000000000 ) ;
#4279 = CARTESIAN_POINT ( 'NONE',  ( 20.95512820512820440, 67.12384868372348024, -60.96447848938343839 ) ) ;
#4280 = ORIENTED_EDGE ( 'NONE', *, *, #147191, .T. ) ;
#4281 = DIRECTION ( 'NONE',  ( -3.265361837132813093E-16, -1.000000000000000000, 7.445645354460596589E-46 ) ) ;
#4282 = ORIENTED_EDGE ( 'NONE', *, *, #241945, .T. ) ;
#4283 = EDGE_CURVE ( 'NONE', #197213, #196891, #210615, .T. ) ;
#4285 = ORIENTED_EDGE ( 'NONE', *, *, #18161, .T. ) ;
#4284 = ORIENTED_EDGE ( 'NONE', *, *, #157000, .T. ) ;
#4286 = ORIENTED_EDGE ( 'NONE', *, *, #13491, .F. ) ;
#4287 = LINE ( 'NONE', #179126, #207392 ) ;
#4288 = VERTEX_POINT ( 'NONE', #12440 ) ;
#4289 = CARTESIAN_POINT ( 'NONE',  ( -23.39999999999994529, 82.64476912853859858, -26.37791261425322986 ) ) ;
#4290 = ORIENTED_EDGE ( 'NONE', *, *, #18183, .F. ) ;
#4291 = ADVANCED_FACE ( 'NONE', ( #154533 ), #56637, .F. ) ;
#4292 = FACE_OUTER_BOUND ( 'NONE', #27883, .T. ) ;
#4293 = EDGE_CURVE ( 'NONE', #207287, #106082, #167326, .T. ) ;
#4294 = CARTESIAN_POINT ( 'NONE',  ( 22.39999999999999503, 1.115600667400684642E-11, -92.70922040162665212 ) ) ;
#4295 = CIRCLE ( 'NONE', #124940, 0.1999999999999987899 ) ;
#4296 = VERTEX_POINT ( 'NONE', #150647 ) ;
#4297 = AXIS2_PLACEMENT_3D ( 'NONE', #208281, #144409, #68762 ) ;
#4298 = ORIENTED_EDGE ( 'NONE', *, *, #160551, .T. ) ;
#4299 = ORIENTED_EDGE ( 'NONE', *, *, #222834, .F. ) ;
#4300 = AXIS2_PLACEMENT_3D ( 'NONE', #149727, #72766, #250086 ) ;
#4301 = FACE_OUTER_BOUND ( 'NONE', #156765, .T. ) ;
#4302 = EDGE_CURVE ( 'NONE', #79726, #255690, #25842, .T. ) ;
#4303 = EDGE_LOOP ( 'NONE', ( #202943, #2316, #5119, #203165, #34482, #231347, #128376, #168284, #195736, #122157, #112154, #131721, #69827, #42740, #256729, #184778, #204213, #171842 ) ) ;
#4304 = ADVANCED_FACE ( 'NONE', ( #76225 ), #192429, .F. ) ;
#4305 = CARTESIAN_POINT ( 'NONE',  ( 20.73486653747088582, 7.250000000011182166, -54.35000000000000142 ) ) ;
#4306 = CARTESIAN_POINT ( 'NONE',  ( -18.36973785203556275, 33.92374417663404529, -235.0677769530471153 ) ) ;
#4307 = CARTESIAN_POINT ( 'NONE',  ( 20.85000000000000142, 1.115600667400684642E-11, -208.7999999999999545 ) ) ;
#4308 = CARTESIAN_POINT ( 'NONE',  ( -21.05315837450971372, 11.75000000001115019, -127.1583560044167456 ) ) ;
#4309 = DIRECTION ( 'NONE',  ( 1.000000000000000000, 0.000000000000000000, -0.000000000000000000 ) ) ;
#4310 = CARTESIAN_POINT ( 'NONE',  ( -20.54999999999999716, -8.999999999988844479, -191.1060308773475356 ) ) ;
#4311 = LINE ( 'NONE', #83820, #97983 ) ;
#4312 = AXIS2_PLACEMENT_3D ( 'NONE', #227846, #24541, #124912 ) ;
#4314 = CARTESIAN_POINT ( 'NONE',  ( 21.04999999999897042, 34.03633519070044855, -243.8225528959771680 ) ) ;
#4313 = DIRECTION ( 'NONE',  ( 0.000000000000000000, -1.000000000000000000, -6.352154140967427193E-15 ) ) ;
#4315 = DIRECTION ( 'NONE',  ( 0.000000000000000000, 0.9126074666063660468, 0.4088369013363524762 ) ) ;
#4316 = CARTESIAN_POINT ( 'NONE',  ( -23.15000000000000213, 11.75000000001115552, -122.2500000000000284 ) ) ;
#4317 = EDGE_CURVE ( 'NONE', #121941, #54351, #253580, .T. ) ;
#4318 = DIRECTION ( 'NONE',  ( -1.000000000000000000, -0.000000000000000000, -0.000000000000000000 ) ) ;
#4319 = DIRECTION ( 'NONE',  ( 0.000000000000000000, -0.2558827019434133376, 0.9667078373770113808 ) ) ;
#4320 = AXIS2_PLACEMENT_3D ( 'NONE', #130411, #206106, #245244 ) ;
#4321 = ORIENTED_EDGE ( 'NONE', *, *, #46739, .T. ) ;
#4322 = AXIS2_PLACEMENT_3D ( 'NONE', #78111, #237208, #136805 ) ;
#4323 = AXIS2_PLACEMENT_3D ( 'NONE', #118176, #97282, #184241 ) ;
#4325 = EDGE_LOOP ( 'NONE', ( #243895, #125884, #223275, #245663 ) ) ;
#4324 = FACE_OUTER_BOUND ( 'NONE', #130623, .T. ) ;
#4326 = VERTEX_POINT ( 'NONE', #215732 ) ;
#4327 = CARTESIAN_POINT ( 'NONE',  ( -23.25000000000000355, 5.649999999999983480, -12.65000000000000213 ) ) ;
#4328 = CARTESIAN_POINT ( 'NONE',  ( 20.72390388899090752, 10.58996311843487348, -141.5113482957463873 ) ) ;
#4329 = DIRECTION ( 'NONE',  ( 0.000000000000000000, -1.000000000000000000, 0.000000000000000000 ) ) ;
#4330 = ORIENTED_EDGE ( 'NONE', *, *, #17648, .F. ) ;
#4331 = EDGE_CURVE ( 'NONE', #236679, #115361, #92459, .T. ) ;
#4332 = SURFACE_SIDE_STYLE ('',( #183004 ) ) ;
#4334 = CIRCLE ( 'NONE', #191650, 0.1000000000000054040 ) ;
#4333 = DIRECTION ( 'NONE',  ( 0.000000000000000000, -0.1480365673253065117, 0.9889818879709274535 ) ) ;
#4335 = CIRCLE ( 'NONE', #125175, 0.1999999999999987899 ) ;
#4336 = EDGE_CURVE ( 'NONE', #102291, #145138, #146428, .T. ) ;
#4337 = DIRECTION ( 'NONE',  ( -1.000000000000000000, -1.836970198721029934E-16, 0.000000000000000000 ) ) ;
#4338 = EDGE_LOOP ( 'NONE', ( #190349, #102327, #187713, #1044 ) ) ;
#4339 = CARTESIAN_POINT ( 'NONE',  ( 21.14999999999999503, 87.75000000001190870, -100.1231074845242262 ) ) ;
#4340 = CARTESIAN_POINT ( 'NONE',  ( 21.93642651522410603, 68.67283376068586165, -69.52310748452435973 ) ) ;
#4341 = FACE_OUTER_BOUND ( 'NONE', #74736, .T. ) ;
#4342 = EDGE_CURVE ( 'NONE', #56249, #236861, #91948, .T. ) ;
#4343 = CARTESIAN_POINT ( 'NONE',  ( 21.05000000000000071, 40.81669639643743608, -238.0718206589051533 ) ) ;
#4345 = EDGE_LOOP ( 'NONE', ( #249029, #104041, #136351 ) ) ;
#4344 = DIRECTION ( 'NONE',  ( 0.000000000000000000, 6.982962677686266711E-15, -1.000000000000000000 ) ) ;
#4346 = DIRECTION ( 'NONE',  ( 0.000000000000000000, -1.000000000000000000, -6.352154140967427193E-15 ) ) ;
#4348 = ORIENTED_EDGE ( 'NONE', *, *, #256323, .T. ) ;
#4347 = FACE_OUTER_BOUND ( 'NONE', #98803, .T. ) ;
#4350 = EDGE_CURVE ( 'NONE', #5985, #49319, #54855, .T. ) ;
#4349 = DIRECTION ( 'NONE',  ( 0.000000000000000000, 0.000000000000000000, 1.000000000000000000 ) ) ;
#4351 = DIRECTION ( 'NONE',  ( -1.000000000000000000, -0.000000000000000000, -0.000000000000000000 ) ) ;
#4352 = EDGE_LOOP ( 'NONE', ( #172143, #231080, #89656, #195062 ) ) ;
#4353 = DIRECTION ( 'NONE',  ( 1.301042606982683418E-14, -0.8660254037844330455, 0.5000000000000096589 ) ) ;
#4354 = CARTESIAN_POINT ( 'NONE',  ( 22.39999999999999503, 75.90000000001273861, -211.3138870828977360 ) ) ;
#4355 = VECTOR ( 'NONE', #136966, 1000.000000000000000 ) ;
#4358 = CARTESIAN_POINT ( 'NONE',  ( -22.50000000000000000, 76.00000000001165290, -69.52310748452431710 ) ) ;
#4357 = AXIS2_PLACEMENT_3D ( 'NONE', #8233, #146422, #108602 ) ;
#4356 = CARTESIAN_POINT ( 'NONE',  ( -20.85000000000000142, 10.33248238083634440, -173.0948465439131496 ) ) ;
#4360 = EDGE_CURVE ( 'NONE', #175273, #226817, #46659, .T. ) ;
#4359 = LINE ( 'NONE', #147745, #220275 ) ;
#4361 = DIRECTION ( 'NONE',  ( 0.000000000000000000, 0.000000000000000000, -1.000000000000000000 ) ) ;
#4362 = VECTOR ( 'NONE', #88073, 1000.000000000000000 ) ;
#4363 = CARTESIAN_POINT ( 'NONE',  ( -18.39999999999999858, 11.47316190337362762, -143.3259460668079726 ) ) ;
#4364 = DIRECTION ( 'NONE',  ( -1.000000000000000000, 0.000000000000000000, -0.000000000000000000 ) ) ;
#4365 = CARTESIAN_POINT ( 'NONE',  ( -16.79363873026997922, 9.948850229429586634, -87.84615378144552267 ) ) ;
#4366 = VERTEX_POINT ( 'NONE', #252291 ) ;
#4367 = EDGE_CURVE ( 'NONE', #14895, #145261, #133645, .T. ) ;
#4368 = FACE_OUTER_BOUND ( 'NONE', #235275, .T. ) ;
#4369 = AXIS2_PLACEMENT_3D ( 'NONE', #234059, #89413, #172863 ) ;
#4371 = ADVANCED_FACE ( 'NONE', ( #59199 ), #236581, .F. ) ;
#4370 = ADVANCED_FACE ( 'NONE', ( #539 ), #103482, .F. ) ;
#4372 = ORIENTED_EDGE ( 'NONE', *, *, #23, .F. ) ;
#4373 = VERTEX_POINT ( 'NONE', #217017 ) ;
#4374 = DIRECTION ( 'NONE',  ( -1.000000000000000000, -0.000000000000000000, -0.000000000000000000 ) ) ;
#4375 = DIRECTION ( 'NONE',  ( 1.000000000000000000, -0.000000000000000000, -0.000000000000000000 ) ) ;
#4376 = VERTEX_POINT ( 'NONE', #177924 ) ;
#4377 = CIRCLE ( 'NONE', #200209, 11.70000000000001528 ) ;
#4378 = EDGE_LOOP ( 'NONE', ( #221382, #75733, #121298 ) ) ;
#4379 = FILL_AREA_STYLE ('',( #140027 ) ) ;
#4380 = ORIENTED_EDGE ( 'NONE', *, *, #156821, .T. ) ;
#4381 = EDGE_CURVE ( 'NONE', #175608, #105012, #100619, .T. ) ;
#4382 = PLANE ( 'NONE',  #204321 ) ;
#4383 = EDGE_CURVE ( 'NONE', #211078, #144573, #72330, .T. ) ;
#4384 = ORIENTED_EDGE ( 'NONE', *, *, #151834, .T. ) ;
#4385 = DIRECTION ( 'NONE',  ( 0.000000000000000000, -6.938893903907229955E-15, 1.000000000000000000 ) ) ;
#4386 = CARTESIAN_POINT ( 'NONE',  ( 23.14999999999999858, 76.00000000001142553, -36.02310748452432421 ) ) ;
#4387 = DIRECTION ( 'NONE',  ( 1.000000000000000000, 0.000000000000000000, 0.000000000000000000 ) ) ;
#4388 = DIRECTION ( 'NONE',  ( 0.000000000000000000, -7.086529944415894657E-15, 1.000000000000000000 ) ) ;
#4389 = EDGE_CURVE ( 'NONE', #219189, #179208, #238207, .T. ) ;
#4390 =( BOUNDED_CURVE ( )  B_SPLINE_CURVE ( 3, ( #73328, #206387, #207681, #32928 ),
 .UNSPECIFIED., .F., .F. ) 
 B_SPLINE_CURVE_WITH_KNOTS ( ( 4, 4 ),
 ( 1.570796326794908992, 2.617993877991502849 ),
 .UNSPECIFIED. ) 
 CURVE ( )  GEOMETRIC_REPRESENTATION_ITEM ( )  RATIONAL_B_SPLINE_CURVE ( ( 1.000000000000000000, 0.9106836025229597675, 0.9106836025229597675, 1.000000000000000000 ) ) 
 REPRESENTATION_ITEM ( '' )  );
#4391 = LINE ( 'NONE', #223436, #145725 ) ;
#4392 = CARTESIAN_POINT ( 'NONE',  ( -23.25000000000000000, 42.20719072976272912, -239.1935934412594804 ) ) ;
#4394 = ORIENTED_EDGE ( 'NONE', *, *, #30246, .F. ) ;
#4393 = CARTESIAN_POINT ( 'NONE',  ( -23.15000000000000213, 76.00000000001142553, -36.02310748452432421 ) ) ;
#4396 = LINE ( 'NONE', #25275, #216752 ) ;
#4395 = DIRECTION ( 'NONE',  ( -5.603264701231745086E-32, 0.9126074666063770380, 0.4088369013363283289 ) ) ;
#4398 = LINE ( 'NONE', #83900, #111498 ) ;
#4397 = CIRCLE ( 'NONE', #229457, 0.5000000000000004441 ) ;
#4399 = EDGE_CURVE ( 'NONE', #31301, #67239, #34070, .T. ) ;
#4400 = ORIENTED_EDGE ( 'NONE', *, *, #98880, .F. ) ;
#4401 = LINE ( 'NONE', #225991, #106266 ) ;
#4402 = DIRECTION ( 'NONE',  ( 1.000000000000000000, 0.000000000000000000, 0.000000000000000000 ) ) ;
#4403 = ORIENTED_EDGE ( 'NONE', *, *, #207992, .F. ) ;
#4404 = EDGE_CURVE ( 'NONE', #46929, #195949, #102184, .T. ) ;
#4405 = VECTOR ( 'NONE', #221213, 1000.000000000000000 ) ;
#4407 = CARTESIAN_POINT ( 'NONE',  ( -16.93415306273742260, 66.00437773999949798, -115.6130505421639612 ) ) ;
#4406 = CYLINDRICAL_SURFACE ( 'NONE', #232860, 0.1000000000000028644 ) ;
#4408 = AXIS2_PLACEMENT_3D ( 'NONE', #61633, #124191, #163311 ) ;
#4409 = DIRECTION ( 'NONE',  ( 0.000000000000000000, -0.9126074666063660468, -0.4088369013363524762 ) ) ;
#4410 = ORIENTED_EDGE ( 'NONE', *, *, #186572, .F. ) ;
#4411 = LINE ( 'NONE', #142627, #230215 ) ;
#4412 = CARTESIAN_POINT ( 'NONE',  ( -20.85000000000000142, 70.22659352830977753, -197.9852579278363578 ) ) ;
#4413 = CARTESIAN_POINT ( 'NONE',  ( -18.39999999999999858, -0.9152171842607119689, -242.2974985173726452 ) ) ;
#4414 = CARTESIAN_POINT ( 'NONE',  ( -22.45354308602486881, 2.198902233671630347E-07, -122.2495671095367271 ) ) ;
#4415 = EDGE_CURVE ( 'NONE', #116285, #215160, #79963, .T. ) ;
#4416 = VERTEX_POINT ( 'NONE', #39711 ) ;
#4417 = EDGE_LOOP ( 'NONE', ( #70885, #113290, #59142, #181456 ) ) ;
#4419 = ADVANCED_FACE ( 'NONE', ( #78783 ), #158382, .T. ) ;
#4418 = CARTESIAN_POINT ( 'NONE',  ( 21.04999999999999716, 67.12872031401622053, -90.87310748452436826 ) ) ;
#4420 = DIRECTION ( 'NONE',  ( 1.000000000000000000, 0.000000000000000000, 0.000000000000000000 ) ) ;
#4421 = LINE ( 'NONE', #83919, #253429 ) ;
#4422 = CARTESIAN_POINT ( 'NONE',  ( 23.14999999999999858, 62.92003201576280702, -207.2439188921395612 ) ) ;
#4423 = AXIS2_PLACEMENT_3D ( 'NONE', #184718, #244688, #46486 ) ;
#4424 = DIRECTION ( 'NONE',  ( 2.952720810173289605E-16, -0.4721928772777354011, -0.8814952561688425003 ) ) ;
#4426 = DIRECTION ( 'NONE',  ( 1.000000000000000000, -0.000000000000000000, -0.000000000000000000 ) ) ;
#4425 = AXIS2_PLACEMENT_3D ( 'NONE', #251126, #90774, #188601 ) ;
#4428 = EDGE_LOOP ( 'NONE', ( #21008, #208272, #77657, #210809 ) ) ;
#4427 = LINE ( 'NONE', #245626, #204503 ) ;
#4429 = CARTESIAN_POINT ( 'NONE',  ( -20.54999999999999716, 49.53130139001177668, -254.0846532093228802 ) ) ;
#4430 = CARTESIAN_POINT ( 'NONE',  ( 21.05000000000000071, 69.55000000001207638, -126.5060803140843291 ) ) ;
#4431 = DIRECTION ( 'NONE',  ( 1.000000000000000000, 7.304098846218134667E-16, 4.639676173203993355E-30 ) ) ;
#4432 = AXIS2_PLACEMENT_3D ( 'NONE', #7971, #69238, #27565 ) ;
#4433 = DIRECTION ( 'NONE',  ( -0.000000000000000000, -0.9876197685951252359, -0.1568667991644863424 ) ) ;
#4434 = EDGE_CURVE ( 'NONE', #116513, #191184, #88152, .T. ) ;
#4435 = DIRECTION ( 'NONE',  ( -1.000000000000000000, 0.000000000000000000, 0.000000000000000000 ) ) ;
#4437 = ORIENTED_EDGE ( 'NONE', *, *, #100995, .T. ) ;
#4436 = DIRECTION ( 'NONE',  ( 0.000000000000000000, 0.000000000000000000, 1.000000000000000000 ) ) ;
#4438 = CARTESIAN_POINT ( 'NONE',  ( -18.59999999999999787, -9.849999999999994316, 30.09999999999999787 ) ) ;
#4439 = CYLINDRICAL_SURFACE ( 'NONE', #132897, 0.1000000000000013933 ) ;
#4440 = CIRCLE ( 'NONE', #245878, 0.09999999999998898659 ) ;
#4441 = DIRECTION ( 'NONE',  ( 1.000000000000000000, 0.000000000000000000, 0.000000000000000000 ) ) ;
#4442 = AXIS2_PLACEMENT_3D ( 'NONE', #189892, #12560, #172941 ) ;
#4443 = ORIENTED_EDGE ( 'NONE', *, *, #111141, .T. ) ;
#4444 = CARTESIAN_POINT ( 'NONE',  ( -18.50000000000000000, 77.86671491006991630, -191.7704322382423356 ) ) ;
#4445 = CARTESIAN_POINT ( 'NONE',  ( -16.93710578446422943, 66.05000000001201954, -115.9419114683237098 ) ) ;
#4446 = CARTESIAN_POINT ( 'NONE',  ( 23.24999999999999645, 76.00000000001170974, -69.52310748452431710 ) ) ;
#4447 = DIRECTION ( 'NONE',  ( 0.000000000000000000, 0.000000000000000000, -1.000000000000000000 ) ) ;
#4448 = ORIENTED_EDGE ( 'NONE', *, *, #176572, .F. ) ;
#4449 = EDGE_CURVE ( 'NONE', #168532, #177623, #63085, .T. ) ;
#4451 = CARTESIAN_POINT ( 'NONE',  ( -16.79270642812319281, 9.946244216949068573, -87.83893327856206668 ) ) ;
#4450 = AXIS2_PLACEMENT_3D ( 'NONE', #178287, #240806, #197811 ) ;
#4452 = AXIS2_PLACEMENT_3D ( 'NONE', #124185, #104573, #126735 ) ;
#4453 = CIRCLE ( 'NONE', #62735, 0.2000000000000057288 ) ;
#4454 = VERTEX_POINT ( 'NONE', #157078 ) ;
#4455 = CIRCLE ( 'NONE', #87652, 0.1000000000000028644 ) ;
#4456 = AXIS2_PLACEMENT_3D ( 'NONE', #164138, #66314, #182423 ) ;
#4457 = CYLINDRICAL_SURFACE ( 'NONE', #84992, 0.8750000000000007772 ) ;
#4458 = DIRECTION ( 'NONE',  ( 0.000000000000000000, 0.2617529984165030688, 0.9651348961777157509 ) ) ;
#4459 = CARTESIAN_POINT ( 'NONE',  ( 21.05000000000000071, 67.22371710471912820, -60.96447848938343839 ) ) ;
#4460 = DIRECTION ( 'NONE',  ( -1.000000000000000000, 0.000000000000000000, -0.000000000000000000 ) ) ;
#4461 = ORIENTED_EDGE ( 'NONE', *, *, #125617, .F. ) ;
#4462 =( BOUNDED_SURFACE ( )  B_SPLINE_SURFACE ( 3, 2, ( 
 ( #12331, #73595, #13599 ),
 ( #14894, #112695, #133536 ),
 ( #38300, #137372, #215627 ),
 ( #177827, #37030, #16183 ) ),
 .UNSPECIFIED., .F., .F., .F. ) 
 B_SPLINE_SURFACE_WITH_KNOTS ( ( 4, 4 ),
 ( 3, 3 ),
 ( 3.658908243880901523, 4.712388980384689674 ),
 ( 0.000000000000000000, 1.000000000000000000 ),
 .UNSPECIFIED. ) 
 GEOMETRIC_REPRESENTATION_ITEM ( )  RATIONAL_B_SPLINE_SURFACE ( (
 ( 1.000000000000000000, 0.8984936768950373409, 1.000000000000000000),
 ( 1.000000000000000000, 0.8646876308614469542, 1.000000000000000000),
 ( 1.000000000000000000, 0.7953136715914278509, 1.000000000000000000),
 ( 1.000000000000000000, 0.7071067811863926966, 1.000000000000000000) ) ) 
 REPRESENTATION_ITEM ( '' )  SURFACE ( )  );
#4463 = CARTESIAN_POINT ( 'NONE',  ( 18.52928932188133970, 65.72071067813116940, -178.8731074845244109 ) ) ;
#4464 = AXIS2_PLACEMENT_3D ( 'NONE', #195491, #169524, #249035 ) ;
#4465 = CARTESIAN_POINT ( 'NONE',  ( 21.05000000000000071, 12.97080753594469371, -210.6099088122175260 ) ) ;
#4466 = CARTESIAN_POINT ( 'NONE',  ( 14.22916352759893499, 9.457410930290162554, -18.49991590874628500 ) ) ;
#4467 = CYLINDRICAL_SURFACE ( 'NONE', #252945, 0.1999999999999987899 ) ;
#4468 = LINE ( 'NONE', #124440, #236351 ) ;
#4469 = VERTEX_POINT ( 'NONE', #123082 ) ;
#4471 = ORIENTED_EDGE ( 'NONE', *, *, #199536, .T. ) ;
#4470 = CARTESIAN_POINT ( 'NONE',  ( 23.14999999999999858, 5.000000000011153745, -45.90526601891310321 ) ) ;
#4472 = EDGE_LOOP ( 'NONE', ( #138854, #61855, #52121, #154961 ) ) ;
#4473 = FACE_OUTER_BOUND ( 'NONE', #94359, .T. ) ;
#4474 = EDGE_LOOP ( 'NONE', ( #236923, #257024, #23491, #250902 ) ) ;
#4475 = CARTESIAN_POINT ( 'NONE',  ( 21.05000000000000071, 61.16604239671102761, -234.3115055913011417 ) ) ;
#4476 = DIRECTION ( 'NONE',  ( 0.000000000000000000, 0.000000000000000000, -1.000000000000000000 ) ) ;
#4477 = CARTESIAN_POINT ( 'NONE',  ( 18.49999999999999645, -1.835341550224411922, -11.55515129256297868 ) ) ;
#4478 = ORIENTED_EDGE ( 'NONE', *, *, #31768, .T. ) ;
#4479 = CARTESIAN_POINT ( 'NONE',  ( 20.85000000000000142, 75.83895117929343144, -136.8072973288845731 ) ) ;
#4480 = DIRECTION ( 'NONE',  ( -0.000000000000000000, -0.8700118002898321601, 0.4930308989875230030 ) ) ;
#4481 = ORIENTED_EDGE ( 'NONE', *, *, #28307, .F. ) ;
#4482 = CARTESIAN_POINT ( 'NONE',  ( -14.56336952470180535, 9.446645344706400493, -152.4108064561002607 ) ) ;
#4484 = EDGE_LOOP ( 'NONE', ( #89886, #139177, #104314, #247561 ) ) ;
#4483 = DIRECTION ( 'NONE',  ( 0.000000000000000000, 0.000000000000000000, -1.000000000000000000 ) ) ;
#4485 = EDGE_CURVE ( 'NONE', #37535, #192064, #104897, .T. ) ;
#4486 = CARTESIAN_POINT ( 'NONE',  ( -23.25000000000000000, 59.07123845373075710, -221.0531397865252075 ) ) ;
#4487 = FACE_OUTER_BOUND ( 'NONE', #73704, .T. ) ;
#4488 = CIRCLE ( 'NONE', #150265, 0.09999999999998898659 ) ;
#4489 = EDGE_LOOP ( 'NONE', ( #43750, #79077, #56309 ) ) ;
#4490 =( BOUNDED_CURVE ( )  B_SPLINE_CURVE ( 3, ( #197429, #177892, #78756, #21397 ),
 .UNSPECIFIED., .F., .F. ) 
 B_SPLINE_CURVE_WITH_KNOTS ( ( 4, 4 ),
 ( 3.141592653589793116, 4.712388980384689674 ),
 .UNSPECIFIED. ) 
 CURVE ( )  GEOMETRIC_REPRESENTATION_ITEM ( )  RATIONAL_B_SPLINE_CURVE ( ( 1.000000000000000000, 0.8047378541243649375, 0.8047378541243649375, 1.000000000000000000 ) ) 
 REPRESENTATION_ITEM ( '' )  );
#4491 = CARTESIAN_POINT ( 'NONE',  ( 21.05000000000000071, 6.450000000011156587, -43.51702717044002355 ) ) ;
#4492 = DIRECTION ( 'NONE',  ( 3.469446951953635015E-14, -0.2617529984165031243, -0.9651348961777157509 ) ) ;
#4493 = VECTOR ( 'NONE', #152257, 999.9999999999998863 ) ;
#4494 = FACE_OUTER_BOUND ( 'NONE', #152266, .T. ) ;
#4495 = VERTEX_POINT ( 'NONE', #77492 ) ;
#4496 = CARTESIAN_POINT ( 'NONE',  ( -20.94999999999999929, 1.835341550235567887, -179.0551512925629538 ) ) ;
#4497 = EDGE_CURVE ( 'NONE', #223333, #104459, #188153, .T. ) ;
#4498 = CARTESIAN_POINT ( 'NONE',  ( -21.14999999999999858, 6.540656951712397138, -100.5000000000000284 ) ) ;
#4499 = EDGE_CURVE ( 'NONE', #202644, #229956, #208991, .T. ) ;
#4500 = ORIENTED_EDGE ( 'NONE', *, *, #247571, .F. ) ;
#4501 = AXIS2_PLACEMENT_3D ( 'NONE', #40352, #119871, #22044 ) ;
#4502 = ADVANCED_FACE ( 'NONE', ( #239168 ), #136558, .F. ) ;
#4503 = TOROIDAL_SURFACE ( 'NONE', #208558, 3.899999999999999467, 0.1000000000000000056 ) ;
#4505 = ORIENTED_EDGE ( 'NONE', *, *, #81415, .F. ) ;
#4504 = TOROIDAL_SURFACE ( 'NONE', #33617, 0.6000000000000009770, 0.1000000000000000056 ) ;
#4506 = CARTESIAN_POINT ( 'NONE',  ( 21.05000012384953223, 65.37127970113806441, -191.3451301544890271 ) ) ;
#4507 = EDGE_CURVE ( 'NONE', #154018, #102756, #203882, .T. ) ;
#4508 = VERTEX_POINT ( 'NONE', #25272 ) ;
#4509 = ADVANCED_FACE ( 'NONE', ( #227299 ), #246856, .F. ) ;
#4510 = CARTESIAN_POINT ( 'NONE',  ( 18.59999999999999076, 11.65000000001115943, -192.3499999999999659 ) ) ;
#4511 = DIRECTION ( 'NONE',  ( -1.000000000000000000, 0.000000000000000000, 0.000000000000000000 ) ) ;
#4513 = EDGE_LOOP ( 'NONE', ( #223686, #58460, #163466, #94679 ) ) ;
#4512 = PLANE ( 'NONE',  #154316 ) ;
#4514 = CARTESIAN_POINT ( 'NONE',  ( 21.05000000000000071, 30.48727911274996671, -240.1192265702093209 ) ) ;
#4515 = LINE ( 'NONE', #204009, #149005 ) ;
#4516 = ADVANCED_FACE ( 'NONE', ( #147781 ), #243006, .F. ) ;
#4517 = DIRECTION ( 'NONE',  ( -1.000000000000000000, -0.000000000000000000, -0.000000000000000000 ) ) ;
#4518 = FACE_OUTER_BOUND ( 'NONE', #201056, .T. ) ;
#4519 = CARTESIAN_POINT ( 'NONE',  ( 18.59999999999999076, 76.00000000001126921, -203.5231074845248997 ) ) ;
#4520 = CARTESIAN_POINT ( 'NONE',  ( 21.04999999999998650, 69.35000000001228670, -157.7731074845243882 ) ) ;
#4522 = EDGE_LOOP ( 'NONE', ( #199880, #169518, #244690, #47708 ) ) ;
#4521 = CARTESIAN_POINT ( 'NONE',  ( 23.14999999999999858, 76.00000000001170974, -69.52310748452431710 ) ) ;
#4524 = ORIENTED_EDGE ( 'NONE', *, *, #235188, .T. ) ;
#4523 = DIRECTION ( 'NONE',  ( 0.000000000000000000, 0.000000000000000000, 1.000000000000000000 ) ) ;
#4525 = DIRECTION ( 'NONE',  ( -1.000000000000000000, 2.952720810173289112E-16, 2.061873921506763405E-30 ) ) ;
#4526 = EDGE_CURVE ( 'NONE', #89014, #40840, #196516, .T. ) ;
#4527 = VECTOR ( 'NONE', #115219, 1000.000000000000000 ) ;
#4528 = ORIENTED_EDGE ( 'NONE', *, *, #129617, .T. ) ;
#4529 = CARTESIAN_POINT ( 'NONE',  ( 23.24999999999999289, 6.650000000011155876, -112.8500000000000369 ) ) ;
#4530 = DIRECTION ( 'NONE',  ( 1.000000000000000000, 0.000000000000000000, 0.000000000000000000 ) ) ;
#4531 = CARTESIAN_POINT ( 'NONE',  ( 22.50000000000000000, 11.64957080755595520, -66.90000000000004832 ) ) ;
#4532 = EDGE_CURVE ( 'NONE', #61324, #88196, #133977, .T. ) ;
#4533 = CARTESIAN_POINT ( 'NONE',  ( 21.14999999999999503, 79.23417978893664326, -236.1056577391152587 ) ) ;
#4534 = DIRECTION ( 'NONE',  ( 0.000000000000000000, 1.000000000000000000, 0.000000000000000000 ) ) ;
#4535 = ORIENTED_EDGE ( 'NONE', *, *, #10188, .T. ) ;
#4536 = EDGE_CURVE ( 'NONE', #162009, #47690, #142343, .T. ) ;
#4537 = CARTESIAN_POINT ( 'NONE',  ( -23.25000000000000000, 12.62988036037870643, -223.4632815780722410 ) ) ;
#4538 = ORIENTED_EDGE ( 'NONE', *, *, #28793, .F. ) ;
#4539 = AXIS2_PLACEMENT_3D ( 'NONE', #62462, #83268, #199418 ) ;
#4540 = AXIS2_PLACEMENT_3D ( 'NONE', #92996, #130840, #50020 ) ;
#4541 = CARTESIAN_POINT ( 'NONE',  ( -20.94999999999999929, 77.16270174995034381, -161.9231074845243370 ) ) ;
#4542 = AXIS2_PLACEMENT_3D ( 'NONE', #211607, #72103, #195906 ) ;
#4543 = ORIENTED_EDGE ( 'NONE', *, *, #151028, .F. ) ;
#4544 = CARTESIAN_POINT ( 'NONE',  ( 21.13435531349789542, 76.00000000001271871, -210.0168285481172177 ) ) ;
#4545 = AXIS2_PLACEMENT_3D ( 'NONE', #30449, #113816, #149115 ) ;
#4546 = CARTESIAN_POINT ( 'NONE',  ( 20.94999999999999929, 0.000000000000000000, 0.000000000000000000 ) ) ;
#4547 = ADVANCED_FACE ( 'NONE', ( #29154 ), #4951, .T. ) ;
#4548 = VERTEX_POINT ( 'NONE', #49944 ) ;
#4549 = CARTESIAN_POINT ( 'NONE',  ( -16.93344882324368683, 66.00341123272436050, -149.1100817897194872 ) ) ;
#4550 = ORIENTED_EDGE ( 'NONE', *, *, #190924, .F. ) ;
#4551 = CARTESIAN_POINT ( 'NONE',  ( -13.77178122865954535, 9.456028260519072859, -48.51119803506571770 ) ) ;
#4552 = ORIENTED_EDGE ( 'NONE', *, *, #61719, .T. ) ;
#4553 = VECTOR ( 'NONE', #242409, 1000.000000000000000 ) ;
#4554 = DIRECTION ( 'NONE',  ( 0.000000000000000000, -0.000000000000000000, 1.000000000000000000 ) ) ;
#4555 = DIRECTION ( 'NONE',  ( 2.952720810173289112E-16, -1.000000000000000000, 0.000000000000000000 ) ) ;
#4556 = ORIENTED_EDGE ( 'NONE', *, *, #168618, .F. ) ;
#4557 = CARTESIAN_POINT ( 'NONE',  ( -23.25000000000000000, 40.09675592080785123, -251.3927149226265385 ) ) ;
#4559 = VERTEX_POINT ( 'NONE', #183058 ) ;
#4558 = CARTESIAN_POINT ( 'NONE',  ( -23.15000000000000213, 74.00000000001223555, -149.2477294072864709 ) ) ;
#4560 = CARTESIAN_POINT ( 'NONE',  ( 21.08804582317328169, 67.12183383292068584, -191.1731076551165245 ) ) ;
#4561 = VERTEX_POINT ( 'NONE', #129496 ) ;
#4562 = EDGE_CURVE ( 'NONE', #242093, #38707, #242304, .T. ) ;
#4563 = ORIENTED_EDGE ( 'NONE', *, *, #93210, .F. ) ;
#4564 = CARTESIAN_POINT ( 'NONE',  ( 21.14999999999999503, 44.10931966560507789, -259.0886734199950183 ) ) ;
#4566 = CARTESIAN_POINT ( 'NONE',  ( 19.80993210785551284, 64.25000000001347189, -178.7559897356397016 ) ) ;
#4565 = VECTOR ( 'NONE', #97094, 999.9999999999998863 ) ;
#4567 = EDGE_CURVE ( 'NONE', #210362, #230778, #17452, .T. ) ;
#4568 = LINE ( 'NONE', #240629, #36491 ) ;
#4569 = DIRECTION ( 'NONE',  ( 1.000000000000000000, -0.000000000000000000, -0.000000000000000000 ) ) ;
#4570 = AXIS2_PLACEMENT_3D ( 'NONE', #158414, #237910, #257415 ) ;
#4572 = ORIENTED_EDGE ( 'NONE', *, *, #213257, .F. ) ;
#4571 = ADVANCED_FACE ( 'NONE', ( #125636 ), #205153, .T. ) ;
#4574 = ADVANCED_FACE ( 'NONE', ( #225984 ), #117600, .F. ) ;
#4573 = CARTESIAN_POINT ( 'NONE',  ( -20.85000000000000142, 77.83585931145498193, -24.51866831572578675 ) ) ;
#4575 = CARTESIAN_POINT ( 'NONE',  ( -17.01825945287481545, 9.949999999999983302, -20.75000000000000000 ) ) ;
#4576 = LINE ( 'NONE', #205343, #7262 ) ;
#4577 = DIRECTION ( 'NONE',  ( 0.000000000000000000, 0.2617529984165031243, 0.9651348961777157509 ) ) ;
#4578 = VECTOR ( 'NONE', #143083, 1000.000000000000000 ) ;
#4579 = ORIENTED_EDGE ( 'NONE', *, *, #106491, .T. ) ;
#4580 = CARTESIAN_POINT ( 'NONE',  ( -21.05000000000000071, 76.09999996531153954, -109.5006596670177856 ) ) ;
#4582 = EDGE_CURVE ( 'NONE', #215029, #71326, #205056, .T. ) ;
#4581 = ORIENTED_EDGE ( 'NONE', *, *, #81512, .T. ) ;
#4583 = CARTESIAN_POINT ( 'NONE',  ( 12.29592348164039350, 9.355806591641288250, -116.7911025315462155 ) ) ;
#4584 = VERTEX_POINT ( 'NONE', #31708 ) ;
#4585 = CIRCLE ( 'NONE', #112944, 0.09999999999999982514 ) ;
#4586 = CARTESIAN_POINT ( 'NONE',  ( -18.59999999999999787, 1.115600667400684642E-11, -100.5000000000000426 ) ) ;
#4587 = CYLINDRICAL_SURFACE ( 'NONE', #47816, 11.74999999999999822 ) ;
#4588 = EDGE_CURVE ( 'NONE', #89932, #39964, #221625, .T. ) ;
#4589 = ORIENTED_EDGE ( 'NONE', *, *, #231552, .F. ) ;
#4590 = AXIS2_PLACEMENT_3D ( 'NONE', #176333, #219279, #15986 ) ;
#4592 = ORIENTED_EDGE ( 'NONE', *, *, #8605, .T. ) ;
#4591 = CARTESIAN_POINT ( 'NONE',  ( -21.14999999999994174, 76.00000000001119815, -36.02310748452479316 ) ) ;
#4593 = DIRECTION ( 'NONE',  ( -1.000000000000000000, 0.000000000000000000, 0.000000000000000000 ) ) ;
#4594 = ORIENTED_EDGE ( 'NONE', *, *, #97948, .T. ) ;
#4595 = CARTESIAN_POINT ( 'NONE',  ( -18.59999999999999787, 77.26178616857662007, -61.43660852097883662 ) ) ;
#4596 = DIRECTION ( 'NONE',  ( -1.000000000000000000, 0.000000000000000000, 0.000000000000000000 ) ) ;
#4597 = VERTEX_POINT ( 'NONE', #113770 ) ;
#4598 = FACE_OUTER_BOUND ( 'NONE', #209660, .T. ) ;
#4599 = CYLINDRICAL_SURFACE ( 'NONE', #219888, 0.09999999999999939493 ) ;
#4600 = CIRCLE ( 'NONE', #66975, 0.2000000000000057288 ) ;
#4601 = AXIS2_PLACEMENT_3D ( 'NONE', #205285, #111017, #151447 ) ;
#4602 = ORIENTED_EDGE ( 'NONE', *, *, #239549, .F. ) ;
#4603 = ORIENTED_EDGE ( 'NONE', *, *, #233075, .F. ) ;
#4604 = ADVANCED_FACE ( 'NONE', ( #210325 ), #48229, .F. ) ;
#4605 = TOROIDAL_SURFACE ( 'NONE', #196159, 0.2000000000000000111, 0.1000000000000000056 ) ;
#4606 = CARTESIAN_POINT ( 'NONE',  ( 20.85000000000000142, 76.00000000001142553, -36.02310748452432421 ) ) ;
#4607 = TOROIDAL_SURFACE ( 'NONE', #125448, 0.2000000000000000111, 0.1000000000000000056 ) ;
#4608 = EDGE_CURVE ( 'NONE', #13885, #18401, #253276, .T. ) ;
#4609 = ADVANCED_FACE ( 'NONE', ( #111212 ), #190783, .T. ) ;
#4610 = AXIS2_PLACEMENT_3D ( 'NONE', #249161, #168372, #208749 ) ;
#4611 = TOROIDAL_SURFACE ( 'NONE', #142186, 1.900000000000002576, 0.1000000000000000056 ) ;
#4613 = ORIENTED_EDGE ( 'NONE', *, *, #172783, .T. ) ;
#4612 = CARTESIAN_POINT ( 'NONE',  ( -20.94999999999999929, 64.75617845954087670, -200.4736850529726269 ) ) ;
#4614 = DIRECTION ( 'NONE',  ( 1.000000000000000000, -0.000000000000000000, -0.000000000000000000 ) ) ;
#4615 = CARTESIAN_POINT ( 'NONE',  ( -18.59999999999999787, 22.25400410509136151, -231.2278641261850680 ) ) ;
#4616 = DIRECTION ( 'NONE',  ( -0.000000000000000000, -0.2617529984165031243, -0.9651348961777157509 ) ) ;
#4618 = LINE ( 'NONE', #163716, #49347 ) ;
#4617 = CARTESIAN_POINT ( 'NONE',  ( -16.93970660449832621, 65.98715860837630487, -90.47082574872992211 ) ) ;
#4619 = CARTESIAN_POINT ( 'NONE',  ( -23.25000000000000000, 1.580567032079710055, -244.0902705724231794 ) ) ;
#4620 = EDGE_CURVE ( 'NONE', #124526, #191326, #56349, .T. ) ;
#4621 = CARTESIAN_POINT ( 'NONE',  ( -16.87845715379269507, 60.92491586797685699, -221.0649567566318581 ) ) ;
#4622 = CIRCLE ( 'NONE', #221106, 0.1000000000000124678 ) ;
#4623 = CIRCLE ( 'NONE', #250355, 0.1000000000000028644 ) ;
#4625 = ORIENTED_EDGE ( 'NONE', *, *, #59939, .F. ) ;
#4624 = VECTOR ( 'NONE', #241905, 1000.000000000000000 ) ;
#4626 = VERTEX_POINT ( 'NONE', #150350 ) ;
#4627 = DIRECTION ( 'NONE',  ( 4.239556034732056743E-17, -0.1298341882520022972, -0.9915357197604853789 ) ) ;
#4628 = EDGE_LOOP ( 'NONE', ( #107414, #44209, #172063, #253771 ) ) ;
#4629 = CARTESIAN_POINT ( 'NONE',  ( 21.05000000000000071, 76.00000000001244871, -170.0231074845243597 ) ) ;
#4631 = EDGE_CURVE ( 'NONE', #125569, #82116, #135885, .T. ) ;
#4630 = ORIENTED_EDGE ( 'NONE', *, *, #141720, .T. ) ;
#4632 = CARTESIAN_POINT ( 'NONE',  ( 20.90851465518106167, 65.67467670974440352, -130.9531731826884879 ) ) ;
#4633 = VERTEX_POINT ( 'NONE', #133350 ) ;
#4634 = DIRECTION ( 'NONE',  ( 1.000000000000000000, -0.000000000000000000, -0.000000000000000000 ) ) ;
#4635 = ORIENTED_EDGE ( 'NONE', *, *, #56654, .F. ) ;
#4636 = ORIENTED_EDGE ( 'NONE', *, *, #215592, .T. ) ;
#4637 = DIRECTION ( 'NONE',  ( 1.000000000000000000, -0.000000000000000000, -0.000000000000000000 ) ) ;
#4638 = CARTESIAN_POINT ( 'NONE',  ( -21.09316766718153247, 75.96073659769731989, -109.3932607969990300 ) ) ;
#4640 = ORIENTED_EDGE ( 'NONE', *, *, #248109, .T. ) ;
#4639 = CARTESIAN_POINT ( 'NONE',  ( 19.97071067811864609, 64.27928932189283273, -44.87310748452440379 ) ) ;
#4641 = CARTESIAN_POINT ( 'NONE',  ( 20.90851465518106167, 65.67467670974416194, -97.45317318268841689 ) ) ;
#4643 = ORIENTED_EDGE ( 'NONE', *, *, #147244, .T. ) ;
#4642 = CARTESIAN_POINT ( 'NONE',  ( -20.54999999999999716, 67.23127455305835554, -235.8551265064784559 ) ) ;
#4644 = DIRECTION ( 'NONE',  ( 3.265361837132813093E-16, -1.000000000000000000, -0.000000000000000000 ) ) ;
#4645 = ORIENTED_EDGE ( 'NONE', *, *, #42670, .T. ) ;
#4646 = DIRECTION ( 'NONE',  ( 0.000000000000000000, -1.000000000000000000, -6.982962677686266711E-15 ) ) ;
#4647 = AXIS2_PLACEMENT_3D ( 'NONE', #67449, #124868, #126129 ) ;
#4649 = ORIENTED_EDGE ( 'NONE', *, *, #16713, .T. ) ;
#4648 = CARTESIAN_POINT ( 'NONE',  ( 20.94999999999999929, 7.128833340094563376, -233.7327013124401276 ) ) ;
#4650 = DIRECTION ( 'NONE',  ( -1.000000000000000000, 0.000000000000000000, 0.000000000000000000 ) ) ;
#4652 = ADVANCED_FACE ( 'NONE', ( #94203 ), #34277, .F. ) ;
#4651 = CARTESIAN_POINT ( 'NONE',  ( -12.92414019175887319, 27.57398452308369485, -234.0009067267211833 ) ) ;
#4653 = FACE_OUTER_BOUND ( 'NONE', #73563, .T. ) ;
#4654 = ORIENTED_EDGE ( 'NONE', *, *, #72986, .T. ) ;
#4656 = DIRECTION ( 'NONE',  ( -0.7071067811865127117, -0.7071067811865821007, 0.000000000000000000 ) ) ;
#4655 = CARTESIAN_POINT ( 'NONE',  ( 21.05000000000000071, 76.00000000001195133, -103.0231074845243171 ) ) ;
#4658 = EDGE_CURVE ( 'NONE', #120086, #62040, #214166, .T. ) ;
#4657 = CARTESIAN_POINT ( 'NONE',  ( -18.39999999999999858, 58.31215475832291162, -223.8520309854405923 ) ) ;
#4659 = DIRECTION ( 'NONE',  ( -1.000000000000000000, 0.000000000000000000, 0.000000000000000000 ) ) ;
#4660 = DIRECTION ( 'NONE',  ( 0.000000000000000000, -0.000000000000000000, -1.000000000000000000 ) ) ;
#4661 = ORIENTED_EDGE ( 'NONE', *, *, #26163, .T. ) ;
#4662 = ORIENTED_EDGE ( 'NONE', *, *, #157310, .T. ) ;
#4663 = VERTEX_POINT ( 'NONE', #116361 ) ;
#4664 = EDGE_CURVE ( 'NONE', #195479, #141753, #238865, .T. ) ;
#4666 = CIRCLE ( 'NONE', #79505, 4.000000000000002665 ) ;
#4665 = DIRECTION ( 'NONE',  ( 0.000000000000000000, 0.000000000000000000, -1.000000000000000000 ) ) ;
#4667 = EDGE_CURVE ( 'NONE', #230514, #46846, #113497, .T. ) ;
#4668 = ORIENTED_EDGE ( 'NONE', *, *, #81405, .F. ) ;
#4669 = FACE_OUTER_BOUND ( 'NONE', #170070, .T. ) ;
#4670 = ORIENTED_EDGE ( 'NONE', *, *, #143665, .F. ) ;
#4671 = DIRECTION ( 'NONE',  ( -0.7071067811865475727, 0.7071067811865475727, 4.937700262164531476E-15 ) ) ;
#4672 = DIRECTION ( 'NONE',  ( 0.000000000000000000, 0.000000000000000000, 1.000000000000000000 ) ) ;
#4673 = EDGE_LOOP ( 'NONE', ( #3086, #81837, #84082, #145393 ) ) ;
#4674 = CARTESIAN_POINT ( 'NONE',  ( 23.24999999999999645, -0.5844558071354983841, -223.2480615698803490 ) ) ;
#4675 = AXIS2_PLACEMENT_3D ( 'NONE', #54422, #132692, #33632 ) ;
#4677 = ORIENTED_EDGE ( 'NONE', *, *, #44155, .F. ) ;
#4676 = AXIS2_PLACEMENT_3D ( 'NONE', #41251, #22970, #236843 ) ;
#4678 = EDGE_CURVE ( 'NONE', #12698, #64183, #240, .T. ) ;
#4679 = ORIENTED_EDGE ( 'NONE', *, *, #44245, .F. ) ;
#4680 = ADVANCED_FACE ( 'NONE', ( #61515 ), #67520, .T. ) ;
#4681 = VERTEX_POINT ( 'NONE', #138446 ) ;
#4682 = CIRCLE ( 'NONE', #150470, 0.09999999999998898659 ) ;
#4683 = CARTESIAN_POINT ( 'NONE',  ( 20.94999999999999574, 76.00000000001195133, -103.0231074845243171 ) ) ;
#4684 = LINE ( 'NONE', #226296, #32672 ) ;
#4685 = DIRECTION ( 'NONE',  ( 1.000000000000000000, 0.000000000000000000, 0.000000000000000000 ) ) ;
#4686 = CARTESIAN_POINT ( 'NONE',  ( 15.57250062127603130, 27.00310224281249205, -233.7483545961832760 ) ) ;
#4687 = FACE_OUTER_BOUND ( 'NONE', #165645, .T. ) ;
#4688 = DIRECTION ( 'NONE',  ( 0.5000000000001141309, 0.000000000000000000, -0.8660254037843729824 ) ) ;
#4690 = FACE_OUTER_BOUND ( 'NONE', #81853, .T. ) ;
#4689 = CARTESIAN_POINT ( 'NONE',  ( -18.59999999999999787, -8.350000000000004974, 10.52591260281975138 ) ) ;
#4691 = DIRECTION ( 'NONE',  ( -0.000000000000000000, -1.000000000000000000, 0.000000000000000000 ) ) ;
#4693 = ORIENTED_EDGE ( 'NONE', *, *, #226947, .F. ) ;
#4692 = DIRECTION ( 'NONE',  ( 1.000000000000000000, 0.000000000000000000, 0.000000000000000000 ) ) ;
#4695 = CARTESIAN_POINT ( 'NONE',  ( 21.05000000000000071, 76.00000000001213607, -136.5231074845243313 ) ) ;
#4694 = DIRECTION ( 'NONE',  ( 1.000000000000000000, 0.000000000000000000, 0.000000000000000000 ) ) ;
#4696 = CARTESIAN_POINT ( 'NONE',  ( 23.24999999999999645, 36.65892442174935439, -249.5511627012433848 ) ) ;
#4697 = VERTEX_POINT ( 'NONE', #39409 ) ;
#4698 = CARTESIAN_POINT ( 'NONE',  ( 20.95462737510932882, 10.55678195165489441, -74.56995005656234810 ) ) ;
#4699 = CARTESIAN_POINT ( 'NONE',  ( 20.94999999999999574, 74.26374286841520700, -191.9544551555068779 ) ) ;
#4700 = DIRECTION ( 'NONE',  ( 0.000000000000000000, 1.000000000000000000, 6.982962677686266711E-15 ) ) ;
#4701 = EDGE_LOOP ( 'NONE', ( #5823, #16617, #150156, #163158, #256925, #53521 ) ) ;
#4702 = ADVANCED_FACE ( 'NONE', ( #141054 ), #1034, .T. ) ;
#4703 = AXIS2_PLACEMENT_3D ( 'NONE', #177790, #57793, #79908 ) ;
#4704 = EDGE_CURVE ( 'NONE', #24606, #236196, #84216, .T. ) ;
#4705 = CARTESIAN_POINT ( 'NONE',  ( 21.14250536705908345, 69.48182782313196526, -203.5231074845243882 ) ) ;
#4706 = CARTESIAN_POINT ( 'NONE',  ( -18.42554971533676778, 78.24001056755894012, -231.5466539090771505 ) ) ;
#4707 = ORIENTED_EDGE ( 'NONE', *, *, #186594, .T. ) ;
#4708 = ORIENTED_EDGE ( 'NONE', *, *, #21185, .T. ) ;
#4709 = DIRECTION ( 'NONE',  ( 1.000000000000000000, 0.000000000000000000, 0.000000000000000000 ) ) ;
#4710 = ORIENTED_EDGE ( 'NONE', *, *, #63243, .F. ) ;
#4711 = DIRECTION ( 'NONE',  ( 8.673617379884089115E-15, -0.9126074666063771490, -0.4088369013363281623 ) ) ;
#4712 = CARTESIAN_POINT ( 'NONE',  ( -18.50000000000000000, -9.399999999988850163, -174.3820418481726904 ) ) ;
#4713 = CARTESIAN_POINT ( 'NONE',  ( -22.39999999999999858, 11.65000000001115588, -134.0000000000000284 ) ) ;
#4715 = ADVANCED_FACE ( 'NONE', ( #22404 ), #82321, .T. ) ;
#4714 = CARTESIAN_POINT ( 'NONE',  ( -21.45000000000000284, 21.65523568329831505, -232.7692078405380300 ) ) ;
#4716 = VERTEX_POINT ( 'NONE', #176342 ) ;
#4717 = DIRECTION ( 'NONE',  ( 0.000000000000000000, 0.000000000000000000, -1.000000000000000000 ) ) ;
#4718 = CIRCLE ( 'NONE', #150495, 0.1999999999999987899 ) ;
#4720 = CARTESIAN_POINT ( 'NONE',  ( -18.50000000000000000, 64.35000000001230092, -157.8731074845244393 ) ) ;
#4719 = AXIS2_PLACEMENT_3D ( 'NONE', #81751, #60931, #23123 ) ;
#4722 = EDGE_CURVE ( 'NONE', #151819, #250043, #105082, .T. ) ;
#4721 = CARTESIAN_POINT ( 'NONE',  ( -20.54999999999999716, 85.00000000001188027, -93.12913836187181005 ) ) ;
#4723 = DIRECTION ( 'NONE',  ( 6.938893903907224433E-15, 1.000000000000000000, 7.272083257015735086E-15 ) ) ;
#4724 = EDGE_LOOP ( 'NONE', ( #257166, #51514, #35181, #232346 ) ) ;
#4726 = VERTEX_POINT ( 'NONE', #62794 ) ;
#4725 = DIRECTION ( 'NONE',  ( 1.000000000000000000, 0.000000000000000000, 0.000000000000000000 ) ) ;
#4727 = DIRECTION ( 'NONE',  ( -0.000000000000000000, 0.1350103645451945777, -0.9908441862701590219 ) ) ;
#4728 = CARTESIAN_POINT ( 'NONE',  ( 18.51997666896904349, 78.16595003815976384, -231.4192470149134522 ) ) ;
#4729 = ADVANCED_FACE ( 'NONE', ( #21127 ), #98030, .F. ) ;
#4730 = CARTESIAN_POINT ( 'NONE',  ( -16.91256925476569606, 9.985731158139328656, -87.96764248900531413 ) ) ;
#4731 = CARTESIAN_POINT ( 'NONE',  ( 20.94999999999999574, 14.00000000001115730, -105.9270925303825663 ) ) ;
#4732 = DIRECTION ( 'NONE',  ( 0.000000000000000000, -1.000000000000000000, 0.000000000000000000 ) ) ;
#4733 = DIRECTION ( 'NONE',  ( -1.073024830501117725E-15, 0.2128009952263604232, -0.9770955615653316162 ) ) ;
#4734 = VERTEX_POINT ( 'NONE', #142315 ) ;
#4735 = CARTESIAN_POINT ( 'NONE',  ( -21.44999999999999929, 7.350000000011155166, -146.3500000000000227 ) ) ;
#4736 = PLANE ( 'NONE',  #31685 ) ;
#4737 = CARTESIAN_POINT ( 'NONE',  ( 20.94999999999999574, 87.65000000001212754, -133.6231074845242119 ) ) ;
#4738 = DIRECTION ( 'NONE',  ( -1.000000000000000000, 0.000000000000000000, 0.000000000000000000 ) ) ;
#4739 = CARTESIAN_POINT ( 'NONE',  ( 16.27683809663749770, 60.62847850914943137, -224.4802381816402033 ) ) ;
#4740 = VERTEX_POINT ( 'NONE', #36845 ) ;
#4741 = VERTEX_POINT ( 'NONE', #195903 ) ;
#4742 = CYLINDRICAL_SURFACE ( 'NONE', #50154, 0.1000000000000124678 ) ;
#4743 = DIRECTION ( 'NONE',  ( 0.000000000000000000, 0.000000000000000000, 1.000000000000000000 ) ) ;
#4744 = DIRECTION ( 'NONE',  ( 0.000000000000000000, 8.673617379884087537E-15, -1.000000000000000000 ) ) ;
#4745 = DIRECTION ( 'NONE',  ( -1.000000000000000000, -0.000000000000000000, -0.000000000000000000 ) ) ;
#4746 = AXIS2_PLACEMENT_3D ( 'NONE', #20853, #156523, #174815 ) ;
#4747 = ORIENTED_EDGE ( 'NONE', *, *, #148032, .F. ) ;
#4748 = SPHERICAL_SURFACE ( 'NONE', #55724, 0.1000000000000000056 ) ;
#4749 = CARTESIAN_POINT ( 'NONE',  ( -21.05000000000000071, 44.15969672213208952, -258.9565289832007693 ) ) ;
#4750 = AXIS2_PLACEMENT_3D ( 'NONE', #53847, #112544, #250751 ) ;
#4751 = LINE ( 'NONE', #103856, #208949 ) ;
#4752 = CARTESIAN_POINT ( 'NONE',  ( -18.59999999999999787, 1.750000000011155743, -45.16951155790164307 ) ) ;
#4753 = AXIS2_PLACEMENT_3D ( 'NONE', #90814, #188641, #248618 ) ;
#4754 = TOROIDAL_SURFACE ( 'NONE', #38128, 2.699999999999999734, 0.1000000000000000056 ) ;
#4755 = ORIENTED_EDGE ( 'NONE', *, *, #229318, .F. ) ;
#4756 = CARTESIAN_POINT ( 'NONE',  ( 20.94999999999999929, 5.500000000011153745, -45.90526601891310321 ) ) ;
#4757 = CIRCLE ( 'NONE', #133781, 12.77500000000000036 ) ;
#4758 = ORIENTED_EDGE ( 'NONE', *, *, #125966, .T. ) ;
#4759 = DIRECTION ( 'NONE',  ( 1.000000000000000000, 0.000000000000000000, 0.000000000000000000 ) ) ;
#4760 = CARTESIAN_POINT ( 'NONE',  ( 18.39999999999999503, 11.74999999999998224, -20.85000000000000142 ) ) ;
#4761 = DIRECTION ( 'NONE',  ( -0.000000000000000000, 7.109473446599835262E-15, -1.000000000000000000 ) ) ;
#4762 = FACE_OUTER_BOUND ( 'NONE', #199336, .T. ) ;
#4763 = CARTESIAN_POINT ( 'NONE',  ( -16.77683809663752257, 9.945835743215301505, -46.16394901910421567 ) ) ;
#4764 = CARTESIAN_POINT ( 'NONE',  ( -20.54999999999999361, 11.65000000001115232, -121.8500000000000369 ) ) ;
#4766 = CARTESIAN_POINT ( 'NONE',  ( -18.51555513499604899, -9.352657054504497580, -7.195169895697221207 ) ) ;
#4765 = AXIS2_PLACEMENT_3D ( 'NONE', #235255, #93177, #56589 ) ;
#4767 = CARTESIAN_POINT ( 'NONE',  ( -18.52328366898031931, -9.642321089030096104, -107.2148193375700913 ) ) ;
#4768 = DIRECTION ( 'NONE',  ( 3.469446951953728416E-14, -0.8660254037844309360, 0.5000000000000134337 ) ) ;
#4769 = FACE_OUTER_BOUND ( 'NONE', #202123, .T. ) ;
#4770 = ADVANCED_FACE ( 'NONE', ( #257087 ), #174721, .F. ) ;
#4771 = DIRECTION ( 'NONE',  ( 0.000000000000000000, -7.116814260417668513E-15, 1.000000000000000000 ) ) ;
#4772 = DIRECTION ( 'NONE',  ( 0.000000000000000000, 6.982962677686267499E-15, -1.000000000000000000 ) ) ;
#4773 = AXIS2_PLACEMENT_3D ( 'NONE', #245058, #126391, #243776 ) ;
#4774 = VECTOR ( 'NONE', #46, 1000.000000000000114 ) ;
#4775 = CARTESIAN_POINT ( 'NONE',  ( -23.15000000000000213, 28.62564411244411744, -258.1944495455016977 ) ) ;
#4776 = FACE_OUTER_BOUND ( 'NONE', #15537, .T. ) ;
#4777 = ORIENTED_EDGE ( 'NONE', *, *, #127089, .F. ) ;
#4778 = VECTOR ( 'NONE', #237927, 1000.000000000000000 ) ;
#4779 = CARTESIAN_POINT ( 'NONE',  ( 18.44444291854882323, 85.49010118095534949, -129.8942035196332938 ) ) ;
#4780 = CARTESIAN_POINT ( 'NONE',  ( 18.59999999999999432, 1.162701749949165642, -75.10000000000003695 ) ) ;
#4781 = ADVANCED_FACE ( 'NONE', ( #187891 ), #28855, .F. ) ;
#4782 = CIRCLE ( 'NONE', #221456, 0.09999999999999635569 ) ;
#4783 = ORIENTED_EDGE ( 'NONE', *, *, #77886, .F. ) ;
#4784 = FACE_OUTER_BOUND ( 'NONE', #23526, .T. ) ;
#4785 = CARTESIAN_POINT ( 'NONE',  ( 21.08832698747859169, 67.22463560659508630, -157.7943900180602554 ) ) ;
#4786 = EDGE_CURVE ( 'NONE', #244261, #47603, #83599, .T. ) ;
#4787 = CARTESIAN_POINT ( 'NONE',  ( -21.14999999999994174, 83.90000000001120384, -34.77310748452479316 ) ) ;
#4788 = EDGE_LOOP ( 'NONE', ( #164385, #234012, #149234 ) ) ;
#4789 = DIRECTION ( 'NONE',  ( 0.000000000000000000, 0.000000000000000000, 1.000000000000000000 ) ) ;
#4790 = DIRECTION ( 'NONE',  ( 0.000000000000000000, 0.000000000000000000, -1.000000000000000000 ) ) ;
#4791 = AXIS2_PLACEMENT_3D ( 'NONE', #168113, #123809, #202059 ) ;
#4792 = VERTEX_POINT ( 'NONE', #64074 ) ;
#4793 = CIRCLE ( 'NONE', #46499, 11.75000000000001066 ) ;
#4794 =( BOUNDED_SURFACE ( )  B_SPLINE_SURFACE ( 3, 2, ( 
 ( #64703, #180813, #239501 ),
 ( #179541, #850, #161255 ),
 ( #122121, #63409, #201646 ),
 ( #139068, #120862, #98653 ) ),
 .UNSPECIFIED., .F., .F., .T. ) 
 B_SPLINE_SURFACE_WITH_KNOTS ( ( 4, 4 ),
 ( 3, 3 ),
 ( 0.0008258556059633813742, 0.0009616864997632797044 ),
 ( 0.000000000000000000, 1.000000000000000000 ),
 .UNSPECIFIED. ) 
 GEOMETRIC_REPRESENTATION_ITEM ( )  RATIONAL_B_SPLINE_SURFACE ( (
 ( 1.000000000000000000, 0.9152888060719355234, 1.000000000000000000),
 ( 1.000000000000000000, 0.9327727094138189567, 1.000000000000000000),
 ( 1.000000000000000000, 0.9369023509258441740, 1.000000000000000000),
 ( 1.000000000000000000, 0.9246339933864472505, 1.000000000000000000) ) ) 
 REPRESENTATION_ITEM ( '' )  SURFACE ( )  );
#4795 = AXIS2_PLACEMENT_3D ( 'NONE', #2213, #144278, #204268 ) ;
#4796 = TOROIDAL_SURFACE ( 'NONE', #205294, 0.2000000000000000111, 0.1000000000000000056 ) ;
#4797 = ORIENTED_EDGE ( 'NONE', *, *, #236602, .F. ) ;
#4798 = ADVANCED_FACE ( 'NONE', ( #143609 ), #159316, .T. ) ;
#4799 = EDGE_LOOP ( 'NONE', ( #91549, #131922 ) ) ;
#4800 = EDGE_CURVE ( 'NONE', #45011, #152028, #223139, .T. ) ;
#4801 = CARTESIAN_POINT ( 'NONE',  ( -20.54999999999999716, 75.47649400317826007, -205.4533772768803317 ) ) ;
#4802 = CARTESIAN_POINT ( 'NONE',  ( 22.45463910399149299, 1.026727559903828595E-11, -21.85042918981591953 ) ) ;
#4803 = CYLINDRICAL_SURFACE ( 'NONE', #182232, 1.749999999999998002 ) ;
#4804 = DIRECTION ( 'NONE',  ( -1.000000000000000000, -0.000000000000000000, -0.000000000000000000 ) ) ;
#4805 = EDGE_CURVE ( 'NONE', #202789, #17741, #202306, .T. ) ;
#4806 = CYLINDRICAL_SURFACE ( 'NONE', #66996, 0.1000000000000048767 ) ;
#4807 = LINE ( 'NONE', #59639, #118306 ) ;
#4808 = CARTESIAN_POINT ( 'NONE',  ( 20.04142135623730070, 51.28888318656201761, -230.2315015618842153 ) ) ;
#4809 = CARTESIAN_POINT ( 'NONE',  ( 18.59999999999998366, 70.22659352830977753, -197.9852579278363578 ) ) ;
#4811 = ORIENTED_EDGE ( 'NONE', *, *, #17564, .T. ) ;
#4810 = CARTESIAN_POINT ( 'NONE',  ( 18.48413544395648955, 87.07667984079645862, -199.6026701993346535 ) ) ;
#4812 = ORIENTED_EDGE ( 'NONE', *, *, #226171, .F. ) ;
#4814 = DIRECTION ( 'NONE',  ( 0.000000000000000000, 1.000000000000000000, 0.000000000000000000 ) ) ;
#4813 = CYLINDRICAL_SURFACE ( 'NONE', #8136, 0.09999999999999939493 ) ;
#4816 = ORIENTED_EDGE ( 'NONE', *, *, #249441, .T. ) ;
#4815 = CARTESIAN_POINT ( 'NONE',  ( 18.59999999999999787, -11.75000000000000000, 29.89999999999999858 ) ) ;
#4817 = ORIENTED_EDGE ( 'NONE', *, *, #228153, .F. ) ;
#4818 = FACE_OUTER_BOUND ( 'NONE', #36515, .T. ) ;
#4819 = AXIS2_PLACEMENT_3D ( 'NONE', #225635, #224375, #10480 ) ;
#4820 = CARTESIAN_POINT ( 'NONE',  ( 20.84451136049651510, 10.62014191481791769, -174.9939245595323598 ) ) ;
#4821 = EDGE_CURVE ( 'NONE', #146255, #134756, #167065, .T. ) ;
#4822 = CARTESIAN_POINT ( 'NONE',  ( -18.59999999999999787, 61.57587952878036930, -212.2000740415318774 ) ) ;
#4823 = CARTESIAN_POINT ( 'NONE',  ( -20.85000000000000142, 11.75000000001115552, -67.00000000000000000 ) ) ;
#4824 = DIRECTION ( 'NONE',  ( 0.000000000000000000, -0.9893560106964500722, 0.1455152366551550613 ) ) ;
#4825 = AXIS2_PLACEMENT_3D ( 'NONE', #135112, #256290, #235506 ) ;
#4826 = EDGE_CURVE ( 'NONE', #84341, #60618, #165768, .T. ) ;
#4827 = CARTESIAN_POINT ( 'NONE',  ( 23.14999999999999147, 80.15000000001238334, -170.0231074845243313 ) ) ;
#4828 = ORIENTED_EDGE ( 'NONE', *, *, #139777, .F. ) ;
#4829 = ORIENTED_EDGE ( 'NONE', *, *, #56787, .F. ) ;
#4830 = DIRECTION ( 'NONE',  ( -5.603264701231743991E-32, 1.897661533703520143E-16, -1.000000000000000000 ) ) ;
#4831 = ORIENTED_EDGE ( 'NONE', *, *, #1329, .T. ) ;
#4832 = CARTESIAN_POINT ( 'NONE',  ( 23.14999999999999858, 54.32225538558145672, -236.1594012422037281 ) ) ;
#4833 = VERTEX_POINT ( 'NONE', #9232 ) ;
#4834 = FACE_OUTER_BOUND ( 'NONE', #224629, .T. ) ;
#4835 = CIRCLE ( 'NONE', #79679, 0.1000000000000021844 ) ;
#4836 = DIRECTION ( 'NONE',  ( -0.000000000000000000, -6.982962677686266711E-15, 1.000000000000000000 ) ) ;
#4837 = DIRECTION ( 'NONE',  ( 0.000000000000000000, 0.9126074666063777041, 0.4088369013363266080 ) ) ;
#4838 = CARTESIAN_POINT ( 'NONE',  ( -21.11101077989000530, 75.98471473109843544, -209.9467922192504830 ) ) ;
#4839 = ORIENTED_EDGE ( 'NONE', *, *, #225038, .T. ) ;
#4840 = CARTESIAN_POINT ( 'NONE',  ( -21.12844524849339223, 11.74999999999999645, -6.904413470842653666 ) ) ;
#4841 = ORIENTED_EDGE ( 'NONE', *, *, #254794, .F. ) ;
#4842 = DIRECTION ( 'NONE',  ( 0.000000000000000000, 6.467318590049456648E-15, -1.000000000000000000 ) ) ;
#4843 = LINE ( 'NONE', #143086, #181226 ) ;
#4844 = DIRECTION ( 'NONE',  ( 1.000000000000000000, -6.938893903907222067E-15, -4.845403715540888588E-29 ) ) ;
#4845 = CARTESIAN_POINT ( 'NONE',  ( -21.05000000000000071, 18.18127959618848166, -237.5711165786817389 ) ) ;
#4846 = EDGE_LOOP ( 'NONE', ( #125717, #11484, #187456 ) ) ;
#4848 = DIRECTION ( 'NONE',  ( 1.000000000000000000, 0.000000000000000000, 0.000000000000000000 ) ) ;
#4847 = AXIS2_PLACEMENT_3D ( 'NONE', #43855, #240775, #838 ) ;
#4849 = ORIENTED_EDGE ( 'NONE', *, *, #241298, .T. ) ;
#4852 = ORIENTED_EDGE ( 'NONE', *, *, #206248, .F. ) ;
#4851 = DIRECTION ( 'NONE',  ( -1.000000000000000000, -0.000000000000000000, -0.000000000000000000 ) ) ;
#4850 = CARTESIAN_POINT ( 'NONE',  ( -16.87683809663752399, 21.23804903844422043, -46.15000000000000568 ) ) ;
#4853 = CIRCLE ( 'NONE', #63136, 0.3999999999999975797 ) ;
#4854 = CARTESIAN_POINT ( 'NONE',  ( 20.85000000000000142, 1.115600667400684642E-11, -100.5000000000000426 ) ) ;
#4855 = ORIENTED_EDGE ( 'NONE', *, *, #232881, .F. ) ;
#4856 = VECTOR ( 'NONE', #232844, 1000.000000000000000 ) ;
#4857 = EDGE_CURVE ( 'NONE', #66884, #695, #104458, .T. ) ;
#4858 = CARTESIAN_POINT ( 'NONE',  ( 21.14999999999999858, 76.00000000001203659, -114.6726782920691221 ) ) ;
#4859 = ORIENTED_EDGE ( 'NONE', *, *, #16669, .F. ) ;
#4860 = EDGE_CURVE ( 'NONE', #147579, #46909, #26030, .T. ) ;
#4861 = CARTESIAN_POINT ( 'NONE',  ( -20.94999999999999929, 76.00000000001195133, -103.0231074845243171 ) ) ;
#4862 = ADVANCED_FACE ( 'NONE', ( #65354 ), #247849, .T. ) ;
#4863 = DIRECTION ( 'NONE',  ( 1.000000000000000000, 0.000000000000000000, 0.000000000000000000 ) ) ;
#4864 = ADVANCED_FACE ( 'NONE', ( #243987 ), #45794, .T. ) ;
#4865 = DIRECTION ( 'NONE',  ( 0.000000000000000000, -1.000000000000000000, 0.000000000000000000 ) ) ;
#4866 = CARTESIAN_POINT ( 'NONE',  ( -16.87331047859651179, 9.949999999999986855, -12.65000000000000213 ) ) ;
#4867 = CIRCLE ( 'NONE', #238115, 0.1000000000000028644 ) ;
#4869 = ORIENTED_EDGE ( 'NONE', *, *, #159782, .F. ) ;
#4868 = ADVANCED_FACE ( 'NONE', ( #86176 ), #204851, .T. ) ;
#4870 = DIRECTION ( 'NONE',  ( 0.000000000000000000, -1.000000000000000000, -6.982962677686265922E-15 ) ) ;
#4871 = CARTESIAN_POINT ( 'NONE',  ( -20.64999999999999858, 7.150000000011155876, -79.35000000000005116 ) ) ;
#4872 = CARTESIAN_POINT ( 'NONE',  ( 23.25000000000000000, 84.59626168225477727, -78.97323500167453858 ) ) ;
#4873 = EDGE_CURVE ( 'NONE', #42259, #227290, #67711, .T. ) ;
#4874 = VERTEX_POINT ( 'NONE', #131751 ) ;
#4875 = PLANE ( 'NONE',  #142623 ) ;
#4878 = EDGE_CURVE ( 'NONE', #143179, #227912, #188325, .T. ) ;
#4877 = ADVANCED_FACE ( 'NONE', ( #114762 ), #130049, .F. ) ;
#4876 = ORIENTED_EDGE ( 'NONE', *, *, #63288, .T. ) ;
#4879 = DIRECTION ( 'NONE',  ( 1.000000000000000000, 0.000000000000000000, 0.000000000000000000 ) ) ;
#4880 = CARTESIAN_POINT ( 'NONE',  ( -23.25000000000000355, 65.95000000001225260, -149.2731074845244450 ) ) ;
#4881 = FACE_OUTER_BOUND ( 'NONE', #132115, .T. ) ;
#4883 = EDGE_LOOP ( 'NONE', ( #222595, #34866, #210855, #3951 ) ) ;
#4882 = CARTESIAN_POINT ( 'NONE',  ( -16.93710578446435733, 44.38079422868823087, -235.1890346188039018 ) ) ;
#4884 = SPHERICAL_SURFACE ( 'NONE', #33767, 0.1000000000000000056 ) ;
#4885 = FACE_OUTER_BOUND ( 'NONE', #96604, .T. ) ;
#4886 = ADVANCED_FACE ( 'NONE', ( #191765 ), #209166, .T. ) ;
#4887 = AXIS2_PLACEMENT_3D ( 'NONE', #223235, #103280, #105847 ) ;
#4888 = VECTOR ( 'NONE', #125605, 1000.000000000000000 ) ;
#4889 = DIRECTION ( 'NONE',  ( 0.000000000000000000, -1.000000000000000000, -7.105427357601001859E-15 ) ) ;
#4890 = ORIENTED_EDGE ( 'NONE', *, *, #102475, .T. ) ;
#4891 = AXIS2_PLACEMENT_3D ( 'NONE', #94551, #97087, #98364 ) ;
#4892 = CARTESIAN_POINT ( 'NONE',  ( 21.03675099975491136, 8.875180032784809825, -12.32554213677804711 ) ) ;
#4893 = CARTESIAN_POINT ( 'NONE',  ( 21.14999999999999858, 6.257814610487280937, -167.4022097086911742 ) ) ;
#4895 = ORIENTED_EDGE ( 'NONE', *, *, #192868, .T. ) ;
#4894 = ADVANCED_FACE ( 'NONE', ( #232156 ), #96719, .F. ) ;
#4897 = EDGE_CURVE ( 'NONE', #77748, #167959, #218213, .T. ) ;
#4896 = CARTESIAN_POINT ( 'NONE',  ( -16.94309007106720699, 9.992226192581142641, -146.6057912825555150 ) ) ;
#4898 = ORIENTED_EDGE ( 'NONE', *, *, #92333, .T. ) ;
#4899 = ADVANCED_FACE ( 'NONE', ( #229581 ), #180157, .F. ) ;
#4901 = EDGE_LOOP ( 'NONE', ( #51368, #3718, #192595, #84933 ) ) ;
#4900 = LINE ( 'NONE', #234236, #76259 ) ;
#4902 = EDGE_CURVE ( 'NONE', #133931, #141019, #46843, .T. ) ;
#4903 = AXIS2_PLACEMENT_3D ( 'NONE', #58003, #77562, #160992 ) ;
#4906 = ORIENTED_EDGE ( 'NONE', *, *, #143097, .T. ) ;
#4905 = VERTEX_POINT ( 'NONE', #173509 ) ;
#4904 = CARTESIAN_POINT ( 'NONE',  ( -18.69999999999999929, -8.175168544775697654, 10.42878401658402510 ) ) ;
#4907 = CARTESIAN_POINT ( 'NONE',  ( -18.34374000495060386, 11.47316190337362585, -76.25000000000004263 ) ) ;
#4908 = DIRECTION ( 'NONE',  ( 1.000000000000000000, 0.000000000000000000, 0.000000000000000000 ) ) ;
#4909 = DIRECTION ( 'NONE',  ( 0.000000000000000000, 0.000000000000000000, 1.000000000000000000 ) ) ;
#4911 = CARTESIAN_POINT ( 'NONE',  ( -16.94878442675511465, 9.991729102990998257, -20.88821957563787635 ) ) ;
#4910 = CARTESIAN_POINT ( 'NONE',  ( 22.45301702632625762, 0.01521087972134078925, -88.85020777573963358 ) ) ;
#4912 = CARTESIAN_POINT ( 'NONE',  ( 20.94999999999999929, 9.374458193048763377, -220.5475659691911119 ) ) ;
#4913 = CARTESIAN_POINT ( 'NONE',  ( -18.41431012584569160, 64.51252797080344692, -60.29634349762607570 ) ) ;
#4914 = CARTESIAN_POINT ( 'NONE',  ( -23.39999999999994529, 77.16254490893143725, -43.82310748452479743 ) ) ;
#4915 = ORIENTED_EDGE ( 'NONE', *, *, #74996, .F. ) ;
#4916 = ORIENTED_EDGE ( 'NONE', *, *, #135592, .T. ) ;
#4917 = CARTESIAN_POINT ( 'NONE',  ( -20.96428641294179940, 64.25000000001175238, -76.34821430658305985 ) ) ;
#4919 = ORIENTED_EDGE ( 'NONE', *, *, #101395, .T. ) ;
#4918 = FACE_OUTER_BOUND ( 'NONE', #132654, .T. ) ;
#4920 = ORIENTED_EDGE ( 'NONE', *, *, #52238, .T. ) ;
#4921 = DIRECTION ( 'NONE',  ( 0.000000000000000000, -6.938893903907222067E-15, 1.000000000000000000 ) ) ;
#4922 = ORIENTED_EDGE ( 'NONE', *, *, #21957, .T. ) ;
#4923 = CYLINDRICAL_SURFACE ( 'NONE', #204373, 0.09999999999999156786 ) ;
#4924 = VECTOR ( 'NONE', #143583, 1000.000000000000000 ) ;
#4925 = EDGE_LOOP ( 'NONE', ( #85855, #225126, #183330, #204374 ) ) ;
#4926 = AXIS2_PLACEMENT_3D ( 'NONE', #165212, #88211, #11279 ) ;
#4928 = TOROIDAL_SURFACE ( 'NONE', #146407, 12.77500000000000036, 0.1000000000000000056 ) ;
#4927 = DIRECTION ( 'NONE',  ( 1.000000000000000000, 0.000000000000000000, 0.000000000000000000 ) ) ;
#4929 = DIRECTION ( 'NONE',  ( 0.000000000000000000, 0.000000000000000000, -1.000000000000000000 ) ) ;
#4931 = ORIENTED_EDGE ( 'NONE', *, *, #197138, .T. ) ;
#4930 = VERTEX_POINT ( 'NONE', #210023 ) ;
#4932 = EDGE_LOOP ( 'NONE', ( #33198, #168707, #132928, #25831, #21150, #214008, #212168, #69739, #25757, #173618, #44280, #232212 ) ) ;
#4934 = CYLINDRICAL_SURFACE ( 'NONE', #161394, 3.999999999999994671 ) ;
#4933 = AXIS2_PLACEMENT_3D ( 'NONE', #107040, #189166, #66654 ) ;
#4935 = ORIENTED_EDGE ( 'NONE', *, *, #77415, .T. ) ;
#4936 = ORIENTED_EDGE ( 'NONE', *, *, #228633, .F. ) ;
#4937 = DIRECTION ( 'NONE',  ( 0.000000000000000000, 1.000000000000000000, 0.000000000000000000 ) ) ;
#4938 = FACE_OUTER_BOUND ( 'NONE', #210313, .T. ) ;
#4939 = VECTOR ( 'NONE', #199116, 1000.000000000000000 ) ;
#4941 = ORIENTED_EDGE ( 'NONE', *, *, #240103, .F. ) ;
#4940 = FACE_BOUND ( 'NONE', #195587, .T. ) ;
#4942 = CYLINDRICAL_SURFACE ( 'NONE', #178171, 0.1000000000000101225 ) ;
#4943 = CARTESIAN_POINT ( 'NONE',  ( -21.05000000000000071, 36.65892442174472876, -249.5511627012454596 ) ) ;
#4945 = ORIENTED_EDGE ( 'NONE', *, *, #129543, .F. ) ;
#4944 = CARTESIAN_POINT ( 'NONE',  ( -21.14999999999999858, 34.01125473725046078, -243.8802146427659352 ) ) ;
#4946 = DIRECTION ( 'NONE',  ( -1.000000000000000000, 2.952720810173289112E-16, 2.061873921506763405E-30 ) ) ;
#4947 = ORIENTED_EDGE ( 'NONE', *, *, #77275, .T. ) ;
#4948 = DIRECTION ( 'NONE',  ( 0.000000000000000000, -0.9893560106964500722, 0.1455152366551550613 ) ) ;
#4949 = AXIS2_PLACEMENT_3D ( 'NONE', #2433, #151606, #132011 ) ;
#4950 = VERTEX_POINT ( 'NONE', #228298 ) ;
#4951 = TOROIDAL_SURFACE ( 'NONE', #175701, 3.899999999999999467, 0.1000000000000000056 ) ;
#4953 = EDGE_CURVE ( 'NONE', #197578, #6436, #33985, .T. ) ;
#4952 = CARTESIAN_POINT ( 'NONE',  ( -20.85000000000000142, 77.36242903720540198, -128.6342262366031548 ) ) ;
#4955 = ORIENTED_EDGE ( 'NONE', *, *, #96401, .T. ) ;
#4954 = VECTOR ( 'NONE', #64817, 1000.000000000000000 ) ;
#4956 = CARTESIAN_POINT ( 'NONE',  ( 21.05000000000000071, 10.72371710471867701, -45.65000000000000568 ) ) ;
#4957 = ADVANCED_FACE ( 'NONE', ( #152637 ), #11837, .T. ) ;
#4958 = AXIS2_PLACEMENT_3D ( 'NONE', #62286, #6145, #25730 ) ;
#4959 = CARTESIAN_POINT ( 'NONE',  ( -18.59999999999999787, 25.52560498759422103, -248.6860249505299407 ) ) ;
#4960 = CARTESIAN_POINT ( 'NONE',  ( 21.05000000000000426, 18.68963942977167747, -227.9427330617897951 ) ) ;
#4961 = ORIENTED_EDGE ( 'NONE', *, *, #41112, .F. ) ;
#4962 = ORIENTED_EDGE ( 'NONE', *, *, #99767, .F. ) ;
#4963 = VECTOR ( 'NONE', #214813, 1000.000000000000000 ) ;
#4964 = EDGE_CURVE ( 'NONE', #92370, #236193, #209352, .T. ) ;
#4965 = DIRECTION ( 'NONE',  ( 0.000000000000000000, 1.000000000000000000, 0.000000000000000000 ) ) ;
#4967 = EDGE_CURVE ( 'NONE', #172933, #119804, #217712, .T. ) ;
#4966 = DIRECTION ( 'NONE',  ( 0.000000000000000000, -1.000000000000000000, -6.982962677686265922E-15 ) ) ;
#4968 = VERTEX_POINT ( 'NONE', #208742 ) ;
#4969 = LINE ( 'NONE', #44136, #34956 ) ;
#4970 = EDGE_LOOP ( 'NONE', ( #100228, #145811, #149572, #10042 ) ) ;
#4971 = DIRECTION ( 'NONE',  ( -0.000000000000000000, 0.9126074666063770380, 0.4088369013363281068 ) ) ;
#4972 = AXIS2_PLACEMENT_3D ( 'NONE', #118422, #119707, #160127 ) ;
#4974 = DIRECTION ( 'NONE',  ( 0.000000000000000000, 0.000000000000000000, -1.000000000000000000 ) ) ;
#4973 = DIRECTION ( 'NONE',  ( 1.000000000000000000, 0.000000000000000000, 0.000000000000000000 ) ) ;
#4975 = CARTESIAN_POINT ( 'NONE',  ( -21.05000000000000071, 5.900000000011162093, -56.78090023534362984 ) ) ;
#4976 = DIRECTION ( 'NONE',  ( 0.000000000000000000, 1.000000000000000000, 2.891205793294679805E-16 ) ) ;
#4977 = ORIENTED_EDGE ( 'NONE', *, *, #107367, .F. ) ;
#4978 = CARTESIAN_POINT ( 'NONE',  ( 18.59999999999999432, 58.44755627554218336, -246.4682640075163818 ) ) ;
#4979 = CIRCLE ( 'NONE', #17474, 0.09999999999999939493 ) ;
#4980 = AXIS2_PLACEMENT_3D ( 'NONE', #38781, #37505, #72799 ) ;
#4981 = AXIS2_PLACEMENT_3D ( 'NONE', #178018, #257471, #78871 ) ;
#4982 = EDGE_CURVE ( 'NONE', #20839, #87080, #213859, .T. ) ;
#4984 = EDGE_LOOP ( 'NONE', ( #126112, #175224, #76786, #211562 ) ) ;
#4983 = ORIENTED_EDGE ( 'NONE', *, *, #169940, .F. ) ;
#4986 = ORIENTED_EDGE ( 'NONE', *, *, #180218, .F. ) ;
#4985 = VECTOR ( 'NONE', #115695, 1000.000000000000000 ) ;
#4987 = EDGE_CURVE ( 'NONE', #180142, #93776, #213635, .T. ) ;
#4988 = EDGE_LOOP ( 'NONE', ( #64498, #105626, #179814, #211539 ) ) ;
#4989 = CARTESIAN_POINT ( 'NONE',  ( -20.54999999999999716, 74.00000000001199396, -115.8477294072864083 ) ) ;
#4990 = DIRECTION ( 'NONE',  ( -0.000000000000000000, 0.000000000000000000, -1.000000000000000000 ) ) ;
#4991 = FACE_OUTER_BOUND ( 'NONE', #10154, .T. ) ;
#4992 = FACE_OUTER_BOUND ( 'NONE', #63102, .T. ) ;
#4993 = DIRECTION ( 'NONE',  ( 0.000000000000000000, 0.000000000000000000, -1.000000000000000000 ) ) ;
#4995 = CARTESIAN_POINT ( 'NONE',  ( -22.00356870069946780, 1.195803586275321404E-11, -160.2457576382543323 ) ) ;
#4994 = DIRECTION ( 'NONE',  ( 1.000000000000000000, 0.000000000000000000, 0.000000000000000000 ) ) ;
#4997 = ORIENTED_EDGE ( 'NONE', *, *, #167753, .T. ) ;
#4996 = CARTESIAN_POINT ( 'NONE',  ( -23.25000000000000000, 1.115600667400684642E-11, -141.9000000000000341 ) ) ;
#4998 = CARTESIAN_POINT ( 'NONE',  ( -22.59999999999999787, 1.115600667400684642E-11, -33.50000000000000000 ) ) ;
#4999 = ORIENTED_EDGE ( 'NONE', *, *, #252051, .F. ) ;
#5000 = DIRECTION ( 'NONE',  ( 0.000000000000000000, 0.1480365673253065117, -0.9889818879709273425 ) ) ;
#5001 = ORIENTED_EDGE ( 'NONE', *, *, #69830, .T. ) ;
#5002 = VERTEX_POINT ( 'NONE', #74388 ) ;
#5003 = PLANE ( 'NONE',  #54402 ) ;
#5004 = DIRECTION ( 'NONE',  ( 0.000000000000000000, 0.3488585713686311318, 0.9371753822965249725 ) ) ;
#5005 = CARTESIAN_POINT ( 'NONE',  ( -23.25000000000000000, -11.48912529307605546, -30.39999999999999858 ) ) ;
#5006 = ADVANCED_FACE ( 'NONE', ( #54773 ), #95197, .F. ) ;
#5007 = DIRECTION ( 'NONE',  ( 1.000000000000000000, 0.000000000000000000, 0.000000000000000000 ) ) ;
#5008 = EDGE_CURVE ( 'NONE', #91161, #71888, #195606, .T. ) ;
#5009 = VECTOR ( 'NONE', #50544, 1000.000000000000114 ) ;
#5010 = DIRECTION ( 'NONE',  ( -3.265361837132813093E-16, 1.000000000000000000, 0.000000000000000000 ) ) ;
#5011 = ORIENTED_EDGE ( 'NONE', *, *, #117671, .T. ) ;
#5012 = ORIENTED_EDGE ( 'NONE', *, *, #187956, .T. ) ;
#5013 = ORIENTED_EDGE ( 'NONE', *, *, #211283, .T. ) ;
#5014 = CARTESIAN_POINT ( 'NONE',  ( -21.05000000000000071, 11.75000000001115552, -126.9851942293460922 ) ) ;
#5015 = CARTESIAN_POINT ( 'NONE',  ( -16.94445028196807002, 63.05630424923659660, -213.0754291771441729 ) ) ;
#5016 = CARTESIAN_POINT ( 'NONE',  ( -21.55000000000000426, 21.67479455268075128, -232.7326951115107647 ) ) ;
#5017 = DIRECTION ( 'NONE',  ( 0.000000000000000000, -0.4930308989875248349, -0.8700118002898312719 ) ) ;
#5018 = DIRECTION ( 'NONE',  ( 0.000000000000000000, 0.5859227990963212784, 0.8103668758649578141 ) ) ;
#5020 = EDGE_CURVE ( 'NONE', #220745, #159966, #178615, .T. ) ;
#5019 = CARTESIAN_POINT ( 'NONE',  ( -21.14999999999994174, 87.51781941433023349, -37.75951082105083145 ) ) ;
#5021 = CARTESIAN_POINT ( 'NONE',  ( -21.05000000000000071, 76.00000000001267608, -203.5231074845243597 ) ) ;
#5022 = FACE_OUTER_BOUND ( 'NONE', #214561, .T. ) ;
#5023 = LINE ( 'NONE', #84540, #16809 ) ;
#5024 = EDGE_CURVE ( 'NONE', #177416, #254300, #176071, .T. ) ;
#5025 = CARTESIAN_POINT ( 'NONE',  ( -21.11825140030068582, 6.296246187023214702, -199.6213722296933213 ) ) ;
#5026 = DIRECTION ( 'NONE',  ( -0.000000000000000000, 0.000000000000000000, 1.000000000000000000 ) ) ;
#5027 = EDGE_CURVE ( 'NONE', #201418, #101718, #142707, .T. ) ;
#5028 = DIRECTION ( 'NONE',  ( 0.000000000000000000, -0.9910465087640861759, -0.1335171055202901691 ) ) ;
#5030 = EDGE_LOOP ( 'NONE', ( #14695, #138245, #135726, #191638 ) ) ;
#5029 = AXIS2_PLACEMENT_3D ( 'NONE', #75671, #16976, #93922 ) ;
#5031 = LINE ( 'NONE', #44202, #91258 ) ;
#5032 = ORIENTED_EDGE ( 'NONE', *, *, #250398, .T. ) ;
#5033 = EDGE_CURVE ( 'NONE', #41243, #104053, #19525, .T. ) ;
#5034 = DIRECTION ( 'NONE',  ( 0.000000000000000000, 0.2617529984165026802, 0.9651348961777159730 ) ) ;
#5035 = DIRECTION ( 'NONE',  ( -1.284434275755705296E-16, 0.7071067811865471286, -0.7071067811865479058 ) ) ;
#5036 = CARTESIAN_POINT ( 'NONE',  ( 20.94999999999999929, 76.00000000001126921, -203.5231074845248997 ) ) ;
#5037 = ORIENTED_EDGE ( 'NONE', *, *, #400, .F. ) ;
#5038 = CARTESIAN_POINT ( 'NONE',  ( -20.85000000000000142, 7.783179459866052419, -245.3643104511423303 ) ) ;
#5039 = ADVANCED_FACE ( 'NONE', ( #238552 ), #80745, .T. ) ;
#5040 = DIRECTION ( 'NONE',  ( 1.000000000000000000, 0.000000000000000000, 0.000000000000000000 ) ) ;
#5041 = DIRECTION ( 'NONE',  ( -1.000000000000000000, -1.394253735153569469E-16, -2.602809386958778209E-16 ) ) ;
#5042 = DIRECTION ( 'NONE',  ( 0.000000000000000000, -6.467318590049456648E-15, 1.000000000000000000 ) ) ;
#5043 = CIRCLE ( 'NONE', #38389, 0.5000000000000004441 ) ;
#5044 = CARTESIAN_POINT ( 'NONE',  ( 18.59999999999999787, -1.835341550213255957, -112.0551512925630107 ) ) ;
#5046 = CARTESIAN_POINT ( 'NONE',  ( 22.45301702632625762, 75.98478912030228116, -181.6728997087847404 ) ) ;
#5045 = AXIS2_PLACEMENT_3D ( 'NONE', #113863, #55136, #212965 ) ;
#5047 = EDGE_LOOP ( 'NONE', ( #159442, #30952, #98191, #241110 ) ) ;
#5048 = DIRECTION ( 'NONE',  ( 1.000000000000000000, 0.000000000000000000, 0.000000000000000000 ) ) ;
#5050 = ORIENTED_EDGE ( 'NONE', *, *, #87797, .T. ) ;
#5049 = DIRECTION ( 'NONE',  ( -1.000000000000000000, 0.000000000000000000, 0.000000000000000000 ) ) ;
#5051 = CARTESIAN_POINT ( 'NONE',  ( 22.49999999999999645, 0.1008583691098678403, -122.2504328765106152 ) ) ;
#5052 = CARTESIAN_POINT ( 'NONE',  ( -20.15000000000000568, 9.291421356248463326, -45.75000000000000000 ) ) ;
#5053 = ORIENTED_EDGE ( 'NONE', *, *, #61150, .F. ) ;
#5054 = CARTESIAN_POINT ( 'NONE',  ( -18.59999999999999787, 11.64999999999999680, -6.914805770653999595 ) ) ;
#5055 = CONTEXT_DEPENDENT_SHAPE_REPRESENTATION ( #15856, #218239 ) ;
#5056 = DIRECTION ( 'NONE',  ( 0.000000000000000000, 0.000000000000000000, 1.000000000000000000 ) ) ;
#5057 = CIRCLE ( 'NONE', #175795, 0.09999999999999939493 ) ;
#5058 = ORIENTED_EDGE ( 'NONE', *, *, #177675, .F. ) ;
#5059 = AXIS2_PLACEMENT_3D ( 'NONE', #146006, #202143, #125179 ) ;
#5060 = DIRECTION ( 'NONE',  ( 0.000000000000000000, -1.000000000000000000, -0.000000000000000000 ) ) ;
#5061 = CARTESIAN_POINT ( 'NONE',  ( 15.74999999999999645, 9.350000000011139178, -184.2499999999999716 ) ) ;
#5062 = CARTESIAN_POINT ( 'NONE',  ( 23.14999999999999503, 6.550000000011156231, -155.2500000000000284 ) ) ;
#5063 = ORIENTED_EDGE ( 'NONE', *, *, #101790, .T. ) ;
#5064 = ORIENTED_EDGE ( 'NONE', *, *, #209922, .F. ) ;
#5065 = CARTESIAN_POINT ( 'NONE',  ( -18.50000000000000000, 9.150000000011157653, -155.7499999999999716 ) ) ;
#5066 = DIRECTION ( 'NONE',  ( -1.000000000000000000, -0.000000000000000000, -0.000000000000000000 ) ) ;
#5067 = LINE ( 'NONE', #45514, #195066 ) ;
#5068 = DIRECTION ( 'NONE',  ( -1.000000000000000000, -0.000000000000000000, -0.000000000000000000 ) ) ;
#5069 = DIRECTION ( 'NONE',  ( 0.000000000000000000, 0.2128009952263403282, -0.9770955615653358350 ) ) ;
#5070 = AXIS2_PLACEMENT_3D ( 'NONE', #190245, #88544, #226786 ) ;
#5071 = CIRCLE ( 'NONE', #67453, 0.09999999999999975575 ) ;
#5072 = CARTESIAN_POINT ( 'NONE',  ( 20.94999999999999574, -11.74999999998883560, -170.3999999999999773 ) ) ;
#5075 = CARTESIAN_POINT ( 'NONE',  ( -18.44362607810620958, -9.490496158073669974, -74.05795386684718551 ) ) ;
#5074 = AXIS2_PLACEMENT_3D ( 'NONE', #178977, #39462, #199804 ) ;
#5073 = CARTESIAN_POINT ( 'NONE',  ( -18.59999999999999787, -7.631834139420953456, -210.1304494778855769 ) ) ;
#5076 = DIRECTION ( 'NONE',  ( -0.000000000000000000, 0.4088369013363276072, -0.9126074666063772600 ) ) ;
#5077 = DIRECTION ( 'NONE',  ( -1.000000000000000000, 2.952720810173289112E-16, 2.061873921506763405E-30 ) ) ;
#5078 = DIRECTION ( 'NONE',  ( 0.000000000000000000, 0.000000000000000000, -1.000000000000000000 ) ) ;
#5079 = CARTESIAN_POINT ( 'NONE',  ( -20.64999999999999858, -8.663551401858004652, -43.02410111806730697 ) ) ;
#5080 = VERTEX_POINT ( 'NONE', #116060 ) ;
#5081 = VERTEX_POINT ( 'NONE', #59894 ) ;
#5082 = DIRECTION ( 'NONE',  ( 0.000000000000000000, -0.8700118002898321601, 0.4930308989875230030 ) ) ;
#5083 = DIRECTION ( 'NONE',  ( -2.978066053179069723E-16, -1.000000000000000000, -7.147358527629766941E-15 ) ) ;
#5085 = CARTESIAN_POINT ( 'NONE',  ( -12.92414019175887141, 13.06404166453377336, -216.7291753257208313 ) ) ;
#5084 = FACE_OUTER_BOUND ( 'NONE', #29685, .T. ) ;
#5086 = CARTESIAN_POINT ( 'NONE',  ( 20.95035502843362707, 39.28946691834322280, -236.8917208353130093 ) ) ;
#5087 = CARTESIAN_POINT ( 'NONE',  ( 19.75857864376268935, 11.65000000001115943, -158.7500000000000284 ) ) ;
#5089 = ADVANCED_FACE ( 'NONE', ( #220296 ), #92822, .T. ) ;
#5088 = FACE_OUTER_BOUND ( 'NONE', #168490, .T. ) ;
#5090 = DIRECTION ( 'NONE',  ( 1.000000000000000000, 0.000000000000000000, 0.000000000000000000 ) ) ;
#5092 = ORIENTED_EDGE ( 'NONE', *, *, #212065, .T. ) ;
#5091 = CIRCLE ( 'NONE', #150860, 7.900000000000000355 ) ;
#5093 = EDGE_CURVE ( 'NONE', #256646, #6741, #42763, .T. ) ;
#5094 = EDGE_CURVE ( 'NONE', #73306, #188929, #47029, .T. ) ;
#5095 = CARTESIAN_POINT ( 'NONE',  ( -21.05000000000000071, 0.6713328740235187109, -212.7808875799876205 ) ) ;
#5096 = EDGE_LOOP ( 'NONE', ( #171863, #77285, #145124, #24622 ) ) ;
#5097 = CARTESIAN_POINT ( 'NONE',  ( -18.79999999999999716, -8.150000000000005684, 32.89999999999999858 ) ) ;
#5098 = VECTOR ( 'NONE', #103092, 1000.000000000000000 ) ;
#5099 = DIRECTION ( 'NONE',  ( -0.000000000000000000, -0.000000000000000000, 1.000000000000000000 ) ) ;
#5100 = ORIENTED_EDGE ( 'NONE', *, *, #205800, .F. ) ;
#5101 = CARTESIAN_POINT ( 'NONE',  ( -18.54148534481894828, 18.40294846151842378, -236.9778203247716419 ) ) ;
#5102 = EDGE_CURVE ( 'NONE', #104336, #84696, #96887, .T. ) ;
#5103 = CIRCLE ( 'NONE', #63385, 0.09999999999999939493 ) ;
#5104 = ORIENTED_EDGE ( 'NONE', *, *, #80572, .T. ) ;
#5105 = CARTESIAN_POINT ( 'NONE',  ( -21.07094088545304444, 69.67983277809517517, -69.62200118707659158 ) ) ;
#5107 = CIRCLE ( 'NONE', #188303, 0.09999999999999949207 ) ;
#5106 = DIRECTION ( 'NONE',  ( 0.000000000000000000, 6.853228547068871147E-15, -1.000000000000000000 ) ) ;
#5108 = DIRECTION ( 'NONE',  ( 0.000000000000000000, 0.000000000000000000, 1.000000000000000000 ) ) ;
#5109 = DIRECTION ( 'NONE',  ( 0.000000000000000000, 0.2617529984165030132, 0.9651348961777158619 ) ) ;
#5110 = DIRECTION ( 'NONE',  ( -1.000000000000000000, 0.000000000000000000, 0.000000000000000000 ) ) ;
#5111 = DIRECTION ( 'NONE',  ( -1.000000000000000000, -0.000000000000000000, -0.000000000000000000 ) ) ;
#5113 = DIRECTION ( 'NONE',  ( -0.000000000000000000, 1.000000000000000000, -0.000000000000000000 ) ) ;
#5112 = AXIS2_PLACEMENT_3D ( 'NONE', #37838, #200737, #217709 ) ;
#5114 = AXIS2_PLACEMENT_3D ( 'NONE', #193228, #94104, #74592 ) ;
#5116 = ORIENTED_EDGE ( 'NONE', *, *, #116924, .F. ) ;
#5115 = CARTESIAN_POINT ( 'NONE',  ( 20.53930447208010790, 67.02285131248707728, -128.0806003429518967 ) ) ;
#5118 = CARTESIAN_POINT ( 'NONE',  ( -11.60000000000000320, -11.75000000000000000, 12.30000000000000426 ) ) ;
#5117 = DIRECTION ( 'NONE',  ( -1.000000000000000000, -0.000000000000000000, 0.000000000000000000 ) ) ;
#5119 = ORIENTED_EDGE ( 'NONE', *, *, #1753, .F. ) ;
#5121 = ORIENTED_EDGE ( 'NONE', *, *, #73238, .F. ) ;
#5120 = CARTESIAN_POINT ( 'NONE',  ( -23.25000000000000000, 76.00000000001139711, -32.12310748452431852 ) ) ;
#5122 = ORIENTED_EDGE ( 'NONE', *, *, #64906, .F. ) ;
#5123 = CARTESIAN_POINT ( 'NONE',  ( 20.04142135623731136, 11.75000000001116085, -91.76715728752543555 ) ) ;
#5124 = TOROIDAL_SURFACE ( 'NONE', #150720, 11.90000000000000213, 0.1000000000000000056 ) ;
#5125 = CARTESIAN_POINT ( 'NONE',  ( -21.30740335185486245, 30.63482136116474663, -252.1414780222814898 ) ) ;
#5126 = VECTOR ( 'NONE', #238340, 1000.000000000000114 ) ;
#5127 = VERTEX_POINT ( 'NONE', #40399 ) ;
#5128 = EDGE_CURVE ( 'NONE', #195513, #4326, #1230, .T. ) ;
#5130 = ADVANCED_FACE ( 'NONE', ( #157789 ), #156492, .F. ) ;
#5129 = DIRECTION ( 'NONE',  ( 1.000000000000000000, 0.000000000000000000, 0.000000000000000000 ) ) ;
#5131 = CARTESIAN_POINT ( 'NONE',  ( 20.95512828230152280, 8.876151312336450161, -112.7024302655031391 ) ) ;
#5132 = FACE_OUTER_BOUND ( 'NONE', #10293, .T. ) ;
#5133 = DIRECTION ( 'NONE',  ( -0.000000000000000000, -1.000000000000000000, 0.000000000000000000 ) ) ;
#5134 = AXIS2_PLACEMENT_3D ( 'NONE', #210609, #250995, #127226 ) ;
#5135 = AXIS2_PLACEMENT_3D ( 'NONE', #189164, #174783, #90046 ) ;
#5136 = EDGE_CURVE ( 'NONE', #32549, #242536, #181169, .T. ) ;
#5137 = DIRECTION ( 'NONE',  ( 1.000000000000000000, 0.000000000000000000, 0.000000000000000000 ) ) ;
#5138 = AXIS2_PLACEMENT_3D ( 'NONE', #54235, #206906, #28304 ) ;
#5139 = CIRCLE ( 'NONE', #75915, 0.09999999999998898659 ) ;
#5140 = ORIENTED_EDGE ( 'NONE', *, *, #83826, .F. ) ;
#5141 = ORIENTED_EDGE ( 'NONE', *, *, #198600, .F. ) ;
#5142 = CARTESIAN_POINT ( 'NONE',  ( -18.59999999999999787, 76.00000000001190870, -103.0231074845243029 ) ) ;
#5143 = VECTOR ( 'NONE', #108671, 1000.000000000000000 ) ;
#5144 = ORIENTED_EDGE ( 'NONE', *, *, #202970, .F. ) ;
#5145 = LINE ( 'NONE', #84673, #125891 ) ;
#5146 = VERTEX_POINT ( 'NONE', #155204 ) ;
#5148 = AXIS2_PLACEMENT_3D ( 'NONE', #92777, #212749, #174953 ) ;
#5147 = LINE ( 'NONE', #204648, #196811 ) ;
#5149 = AXIS2_PLACEMENT_3D ( 'NONE', #98365, #136225, #198792 ) ;
#5150 = CARTESIAN_POINT ( 'NONE',  ( 19.97071067695831559, 11.72071067695831914, -24.67625343280356276 ) ) ;
#5151 = DIRECTION ( 'NONE',  ( 0.000000000000000000, -0.8814952561688476074, 0.4721928772777262417 ) ) ;
#5152 = CARTESIAN_POINT ( 'NONE',  ( -21.08621493067320785, 30.84153651989748823, -252.0957046748300456 ) ) ;
#5153 = CARTESIAN_POINT ( 'NONE',  ( 23.24999999999999645, 65.63681063784667913, -232.2959573867136100 ) ) ;
#5154 = VERTEX_POINT ( 'NONE', #57330 ) ;
#5155 = ADVANCED_FACE ( 'NONE', ( #136886 ), #234711, .T. ) ;
#5156 = DIRECTION ( 'NONE',  ( 0.000000000000000000, 0.000000000000000000, -1.000000000000000000 ) ) ;
#5157 = LINE ( 'NONE', #187701, #187984 ) ;
#5158 = CARTESIAN_POINT ( 'NONE',  ( 18.51565452909320086, 85.35285933884857457, -62.32819816329048024 ) ) ;
#5159 = DIRECTION ( 'NONE',  ( 0.000000000000000000, 0.9126074666063773710, 0.4088369013363269966 ) ) ;
#5160 = ORIENTED_EDGE ( 'NONE', *, *, #161803, .T. ) ;
#5162 = CARTESIAN_POINT ( 'NONE',  ( -23.15000000000000213, 1.115600667400684642E-11, -100.5000000000000426 ) ) ;
#5161 = DIRECTION ( 'NONE',  ( -1.000000000000000000, -8.674042436075348305E-17, -1.619280515896124405E-16 ) ) ;
#5163 = VECTOR ( 'NONE', #189839, 1000.000000000000114 ) ;
#5164 = ORIENTED_EDGE ( 'NONE', *, *, #218595, .F. ) ;
#5166 = ORIENTED_EDGE ( 'NONE', *, *, #236314, .F. ) ;
#5165 = FACE_OUTER_BOUND ( 'NONE', #44928, .T. ) ;
#5167 = AXIS2_PLACEMENT_3D ( 'NONE', #198540, #19927, #99422 ) ;
#5168 = ORIENTED_EDGE ( 'NONE', *, *, #174506, .T. ) ;
#5169 = CARTESIAN_POINT ( 'NONE',  ( -21.05000000000000071, 14.05000000001115623, -72.51369507076104526 ) ) ;
#5170 = AXIS2_PLACEMENT_3D ( 'NONE', #62143, #118263, #37456 ) ;
#5171 = DIRECTION ( 'NONE',  ( 0.000000000000000000, -0.4105728183244014562, -0.9118278131605539460 ) ) ;
#5172 = EDGE_CURVE ( 'NONE', #224378, #167778, #163580, .T. ) ;
#5173 = PLANE ( 'NONE',  #191830 ) ;
#5174 = ORIENTED_EDGE ( 'NONE', *, *, #183969, .F. ) ;
#5175 = DIRECTION ( 'NONE',  ( 1.000000000000000000, 0.000000000000000000, 0.000000000000000000 ) ) ;
#5177 = DIRECTION ( 'NONE',  ( 0.000000000000000000, 0.000000000000000000, 1.000000000000000000 ) ) ;
#5176 =( BOUNDED_SURFACE ( )  B_SPLINE_SURFACE ( 3, 2, ( 
 ( #36770, #154155, #152866 ),
 ( #193246, #251921, #137118 ),
 ( #138371, #133265, #38041 ),
 ( #18451, #176269, #155437 ) ),
 .UNSPECIFIED., .F., .F., .F. ) 
 B_SPLINE_SURFACE_WITH_KNOTS ( ( 4, 4 ),
 ( 3, 3 ),
 ( 0.3000847527772383394, 0.5552748953338751958 ),
 ( 0.000000000000000000, 1.000000000000000000 ),
 .UNSPECIFIED. ) 
 GEOMETRIC_REPRESENTATION_ITEM ( )  RATIONAL_B_SPLINE_SURFACE ( (
 ( 1.000000000000000000, 0.9152888060719235330, 1.000000000000000000),
 ( 1.000000000000000000, 0.9104333467450104189, 1.000000000000000000),
 ( 1.000000000000000000, 0.9035312726220521284, 1.000000000000000000),
 ( 1.000000000000000000, 0.8946697475931482124, 1.000000000000000000) ) ) 
 REPRESENTATION_ITEM ( '' )  SURFACE ( )  );
#5178 = EDGE_CURVE ( 'NONE', #81533, #219794, #242675, .T. ) ;
#5180 = LINE ( 'NONE', #243818, #171590 ) ;
#5179 = FACE_OUTER_BOUND ( 'NONE', #4325, .T. ) ;
#5181 = ADVANCED_FACE ( 'NONE', ( #177337 ), #58618, .F. ) ;
#5183 = ORIENTED_EDGE ( 'NONE', *, *, #51226, .F. ) ;
#5182 = CARTESIAN_POINT ( 'NONE',  ( 21.12642695952774119, 0.09890328318936439378, 6.375659922035173288 ) ) ;
#5184 = VERTEX_POINT ( 'NONE', #48055 ) ;
#5185 = CARTESIAN_POINT ( 'NONE',  ( -23.15000000000000213, 56.16603649944111254, -228.1013850343386764 ) ) ;
#5186 = CIRCLE ( 'NONE', #175931, 0.09999999999999178990 ) ;
#5187 = DIRECTION ( 'NONE',  ( 0.000000000000000000, 0.2128009952263568982, -0.9770955615653323934 ) ) ;
#5188 = ADVANCED_FACE ( 'NONE', ( #244973 ), #230202, .F. ) ;
#5189 = DIRECTION ( 'NONE',  ( 0.7071359030027419834, 0.000000000000000000, 0.7070776581709371511 ) ) ;
#5191 = EDGE_CURVE ( 'NONE', #218147, #21197, #117774, .T. ) ;
#5190 = ORIENTED_EDGE ( 'NONE', *, *, #234752, .F. ) ;
#5192 = CARTESIAN_POINT ( 'NONE',  ( -20.54999999999999716, 84.66355140188147743, -160.4990063664569959 ) ) ;
#5193 = ORIENTED_EDGE ( 'NONE', *, *, #215598, .T. ) ;
#5194 = CARTESIAN_POINT ( 'NONE',  ( 21.04999999999999716, 18.86217927868475641, -229.9540340038553552 ) ) ;
#5195 = CIRCLE ( 'NONE', #217579, 0.09999999999999609201 ) ;
#5196 = DIRECTION ( 'NONE',  ( 0.000000000000000000, 6.982962677686266711E-15, -1.000000000000000000 ) ) ;
#5197 = PLANE ( 'NONE',  #39129 ) ;
#5198 = ADVANCED_FACE ( 'NONE', ( #142018 ), #147152, .T. ) ;
#5199 = ORIENTED_EDGE ( 'NONE', *, *, #5853, .T. ) ;
#5200 = DIRECTION ( 'NONE',  ( 0.000000000000000000, -1.000000000000000000, 0.000000000000000000 ) ) ;
#5201 = EDGE_CURVE ( 'NONE', #121060, #158295, #151109, .T. ) ;
#5202 = DIRECTION ( 'NONE',  ( 1.000000000000000000, 0.000000000000000000, 0.000000000000000000 ) ) ;
#5203 = ADVANCED_FACE ( 'NONE', ( #27252 ), #55198, .T. ) ;
#5204 = ADVANCED_FACE ( 'NONE', ( #241146 ), #246268, .F. ) ;
#5206 = ORIENTED_EDGE ( 'NONE', *, *, #78423, .T. ) ;
#5205 = AXIS2_PLACEMENT_3D ( 'NONE', #2510, #202017, #20831 ) ;
#5207 = VERTEX_POINT ( 'NONE', #162901 ) ;
#5208 = ORIENTED_EDGE ( 'NONE', *, *, #201225, .F. ) ;
#5209 = EDGE_CURVE ( 'NONE', #212963, #116440, #236687, .T. ) ;
#5210 = CARTESIAN_POINT ( 'NONE',  ( 21.14999999999999503, 76.10085836911045476, -81.27267460801371612 ) ) ;
#5211 = VERTEX_POINT ( 'NONE', #203281 ) ;
#5213 = ORIENTED_EDGE ( 'NONE', *, *, #110331, .F. ) ;
#5212 = DIRECTION ( 'NONE',  ( 1.000000000000000000, 0.000000000000000000, 0.000000000000000000 ) ) ;
#5215 = EDGE_CURVE ( 'NONE', #221285, #43098, #101150, .T. ) ;
#5214 = ORIENTED_EDGE ( 'NONE', *, *, #219203, .F. ) ;
#5216 = ADVANCED_FACE ( 'NONE', ( #46761 ), #238579, .F. ) ;
#5218 = EDGE_LOOP ( 'NONE', ( #192245, #102500, #98596 ) ) ;
#5217 = ORIENTED_EDGE ( 'NONE', *, *, #209765, .T. ) ;
#5219 = EDGE_CURVE ( 'NONE', #4376, #65749, #82013, .T. ) ;
#5220 = FACE_OUTER_BOUND ( 'NONE', #10923, .T. ) ;
#5221 = CIRCLE ( 'NONE', #213335, 0.09999999999999895084 ) ;
#5222 = VERTEX_POINT ( 'NONE', #122475 ) ;
#5223 = CARTESIAN_POINT ( 'NONE',  ( -20.64999999999999858, 68.85000000001254250, -182.3731074845244109 ) ) ;
#5224 = CARTESIAN_POINT ( 'NONE',  ( -21.52071067811865746, 7.779289321892505882, -121.7500000000000426 ) ) ;
#5225 = CIRCLE ( 'NONE', #184307, 0.8750000000000007772 ) ;
#5226 = CARTESIAN_POINT ( 'NONE',  ( -18.48179518608914762, 86.98986899361442227, -199.3650623953066372 ) ) ;
#5227 = ORIENTED_EDGE ( 'NONE', *, *, #155710, .F. ) ;
#5228 = VECTOR ( 'NONE', #257686, 1000.000000000000000 ) ;
#5229 = CYLINDRICAL_SURFACE ( 'NONE', #232941, 0.09999999999999939493 ) ;
#5231 = ORIENTED_EDGE ( 'NONE', *, *, #65234, .F. ) ;
#5230 = DIRECTION ( 'NONE',  ( 0.000000000000000000, 0.000000000000000000, -1.000000000000000000 ) ) ;
#5232 = DIRECTION ( 'NONE',  ( -0.000000000000000000, -1.000000000000000000, -6.982962677686266711E-15 ) ) ;
#5234 = ORIENTED_EDGE ( 'NONE', *, *, #205645, .F. ) ;
#5233 = FACE_OUTER_BOUND ( 'NONE', #141337, .T. ) ;
#5235 = EDGE_CURVE ( 'NONE', #252597, #46377, #121893, .T. ) ;
#5236 = VERTEX_POINT ( 'NONE', #145862 ) ;
#5237 = CARTESIAN_POINT ( 'NONE',  ( -21.05000000000000071, -12.41227409413852811, -64.10000000000000853 ) ) ;
#5238 = AXIS2_PLACEMENT_3D ( 'NONE', #179155, #96972, #176575 ) ;
#5239 = AXIS2_PLACEMENT_3D ( 'NONE', #172038, #151164, #134139 ) ;
#5240 = VERTEX_POINT ( 'NONE', #165455 ) ;
#5241 = ORIENTED_EDGE ( 'NONE', *, *, #38418, .T. ) ;
#5242 = CARTESIAN_POINT ( 'NONE',  ( -23.15000000000000213, 1.115600667400684642E-11, -134.0000000000000000 ) ) ;
#5243 = DIRECTION ( 'NONE',  ( 0.000000000000000000, -6.688090509790097607E-15, 1.000000000000000000 ) ) ;
#5245 = VERTEX_POINT ( 'NONE', #204561 ) ;
#5244 = EDGE_LOOP ( 'NONE', ( #218896, #68781, #179464, #128259, #210819 ) ) ;
#5246 = VERTEX_POINT ( 'NONE', #42928 ) ;
#5247 = DIRECTION ( 'NONE',  ( -1.020425574104004196E-15, 0.000000000000000000, 1.000000000000000000 ) ) ;
#5248 = ORIENTED_EDGE ( 'NONE', *, *, #158209, .T. ) ;
#5249 = EDGE_LOOP ( 'NONE', ( #237507, #58905, #168146, #41404 ) ) ;
#5251 = DIRECTION ( 'NONE',  ( 1.000000000000000000, 0.000000000000000000, 0.000000000000000000 ) ) ;
#5250 = VECTOR ( 'NONE', #75745, 1000.000000000000000 ) ;
#5253 = ORIENTED_EDGE ( 'NONE', *, *, #117741, .T. ) ;
#5252 = DIRECTION ( 'NONE',  ( -1.000000000000000000, -3.265361837132813093E-16, 0.000000000000000000 ) ) ;
#5254 = CARTESIAN_POINT ( 'NONE',  ( -20.94999999999999929, 1.115600667400684642E-11, -100.5000000000000426 ) ) ;
#5256 = CARTESIAN_POINT ( 'NONE',  ( 18.40000000000000568, -9.499999999988851584, -107.4993620971801533 ) ) ;
#5255 = SPHERICAL_SURFACE ( 'NONE', #48957, 0.1000000000000000056 ) ;
#5257 = ORIENTED_EDGE ( 'NONE', *, *, #248881, .F. ) ;
#5258 = AXIS2_PLACEMENT_3D ( 'NONE', #114103, #256122, #115391 ) ;
#5259 = VECTOR ( 'NONE', #162666, 1000.000000000000000 ) ;
#5261 = ORIENTED_EDGE ( 'NONE', *, *, #145268, .T. ) ;
#5260 = ORIENTED_EDGE ( 'NONE', *, *, #66223, .F. ) ;
#5262 = CIRCLE ( 'NONE', #122000, 0.1000000000000016431 ) ;
#5263 = CARTESIAN_POINT ( 'NONE',  ( 20.85000000000000142, 7.120270961708750512, -137.6595630418393625 ) ) ;
#5265 = EDGE_CURVE ( 'NONE', #191603, #242965, #100975, .T. ) ;
#5264 = CYLINDRICAL_SURFACE ( 'NONE', #95320, 11.79999999999999716 ) ;
#5266 = ORIENTED_EDGE ( 'NONE', *, *, #96420, .F. ) ;
#5267 = EDGE_CURVE ( 'NONE', #51098, #120640, #224118, .T. ) ;
#5268 = DIRECTION ( 'NONE',  ( 0.000000000000000000, 0.000000000000000000, -1.000000000000000000 ) ) ;
#5269 = EDGE_LOOP ( 'NONE', ( #3917, #73423, #72451, #48501, #135786, #131245, #1807, #203760, #223010, #75485, #240595, #144430, #181249, #67501, #196745, #142239 ) ) ;
#5270 = VERTEX_POINT ( 'NONE', #205849 ) ;
#5271 = DIRECTION ( 'NONE',  ( 0.000000000000000000, 1.897661533703519897E-16, -1.000000000000000000 ) ) ;
#5272 = EDGE_CURVE ( 'NONE', #182849, #86438, #106732, .T. ) ;
#5273 = ORIENTED_EDGE ( 'NONE', *, *, #158998, .T. ) ;
#5274 = DIRECTION ( 'NONE',  ( 0.000000000000000000, 1.000000000000000000, 0.000000000000000000 ) ) ;
#5275 = CARTESIAN_POINT ( 'NONE',  ( 21.04999999999999716, 34.10062737184202319, -243.7890691661991696 ) ) ;
#5276 = ORIENTED_EDGE ( 'NONE', *, *, #110552, .T. ) ;
#5277 = DIRECTION ( 'NONE',  ( 0.000000000000000000, -0.9875055080513754913, 0.1575844902526733482 ) ) ;
#5278 = DIRECTION ( 'NONE',  ( 1.000000000000000000, 0.000000000000000000, 0.000000000000000000 ) ) ;
#5280 = FACE_OUTER_BOUND ( 'NONE', #970, .T. ) ;
#5279 = CARTESIAN_POINT ( 'NONE',  ( 18.59999999999999076, 36.65892442174935439, -249.5511627012433848 ) ) ;
#5281 = DIRECTION ( 'NONE',  ( -0.000000000000000000, 6.982962677686266711E-15, -1.000000000000000000 ) ) ;
#5282 = DIRECTION ( 'NONE',  ( 0.000000000000000000, 0.2466408114429753939, 0.9691069652678959701 ) ) ;
#5283 = CARTESIAN_POINT ( 'NONE',  ( -20.64999999999999858, 11.60058429089262333, -246.3380203656811887 ) ) ;
#5284 = CARTESIAN_POINT ( 'NONE',  ( -23.15000000000000213, -11.64999999998884483, -33.50000000000000000 ) ) ;
#5285 = EDGE_CURVE ( 'NONE', #50999, #149564, #9442, .T. ) ;
#5286 = AXIS2_PLACEMENT_3D ( 'NONE', #39953, #119475, #99861 ) ;
#5287 = ORIENTED_EDGE ( 'NONE', *, *, #238878, .F. ) ;
#5288 = AXIS2_PLACEMENT_3D ( 'NONE', #6576, #69150, #148680 ) ;
#5290 = EDGE_LOOP ( 'NONE', ( #54995, #145368, #185205, #101216 ) ) ;
#5289 = ORIENTED_EDGE ( 'NONE', *, *, #192125, .T. ) ;
#5291 = ORIENTED_EDGE ( 'NONE', *, *, #144515, .F. ) ;
#5292 = CYLINDRICAL_SURFACE ( 'NONE', #3008, 0.09999999999999939493 ) ;
#5293 = AXIS2_PLACEMENT_3D ( 'NONE', #33222, #153170, #96961 ) ;
#5294 = DIRECTION ( 'NONE',  ( 0.000000000000000000, 0.000000000000000000, 1.000000000000000000 ) ) ;
#5296 = CARTESIAN_POINT ( 'NONE',  ( -17.01764560440334151, 9.950000000011138823, -146.7499999992111270 ) ) ;
#5295 = DIRECTION ( 'NONE',  ( 0.5932847527679310229, -0.8049926720990042694, 0.000000000000000000 ) ) ;
#5297 = DIRECTION ( 'NONE',  ( 0.000000000000000000, -0.9126074666063660468, -0.4088369013363524762 ) ) ;
#5298 = ORIENTED_EDGE ( 'NONE', *, *, #26181, .T. ) ;
#5299 = AXIS2_PLACEMENT_3D ( 'NONE', #140383, #159989, #178273 ) ;
#5300 = DIRECTION ( 'NONE',  ( 1.000000000000000000, 0.000000000000000000, 0.000000000000000000 ) ) ;
#5301 = DIRECTION ( 'NONE',  ( 1.000000000000000000, 0.000000000000000000, 0.000000000000000000 ) ) ;
#5302 = TOROIDAL_SURFACE ( 'NONE', #96876, 0.2000000000000000111, 0.1000000000000000056 ) ;
#5303 = FACE_OUTER_BOUND ( 'NONE', #73296, .T. ) ;
#5304 = CIRCLE ( 'NONE', #26380, 0.09999999999998898659 ) ;
#5305 = CIRCLE ( 'NONE', #151089, 0.1000000000000013933 ) ;
#5306 = DIRECTION ( 'NONE',  ( -0.000000000000000000, 7.109473446599835262E-15, -1.000000000000000000 ) ) ;
#5307 = ORIENTED_EDGE ( 'NONE', *, *, #83225, .T. ) ;
#5308 = AXIS2_PLACEMENT_3D ( 'NONE', #2184, #99988, #179578 ) ;
#5309 = CARTESIAN_POINT ( 'NONE',  ( -13.39999999999994529, 64.35000000001120668, -18.32310748452479388 ) ) ;
#5310 = AXIS2_PLACEMENT_3D ( 'NONE', #90810, #33465, #214612 ) ;
#5311 = DIRECTION ( 'NONE',  ( 0.000000000000000000, 1.000000000000000000, 0.000000000000000000 ) ) ;
#5312 = ORIENTED_EDGE ( 'NONE', *, *, #49985, .T. ) ;
#5313 = DIRECTION ( 'NONE',  ( 0.000000000000000000, -0.9910465087640860649, -0.1335171055202901413 ) ) ;
#5314 = CARTESIAN_POINT ( 'NONE',  ( 12.25000000000000000, 9.850000000011137402, -83.75000000000004263 ) ) ;
#5315 = FACE_OUTER_BOUND ( 'NONE', #40208, .T. ) ;
#5316 = CARTESIAN_POINT ( 'NONE',  ( -20.64999999999999858, 1.148907358139439339E-11, -201.0000000000015064 ) ) ;
#5317 = DIRECTION ( 'NONE',  ( 0.7071067811865388020, -0.7071067811865561215, 0.000000000000000000 ) ) ;
#5318 = FACE_OUTER_BOUND ( 'NONE', #251989, .T. ) ;
#5319 = ORIENTED_EDGE ( 'NONE', *, *, #230682, .F. ) ;
#5320 = CARTESIAN_POINT ( 'NONE',  ( 28.12018973533754362, 11.62642356364896123, 33.00000000000000000 ) ) ;
#5322 = ADVANCED_FACE ( 'NONE', ( #208442 ), #252479, .F. ) ;
#5321 = CYLINDRICAL_SURFACE ( 'NONE', #138035, 0.09999999999998898659 ) ;
#5323 = CARTESIAN_POINT ( 'NONE',  ( 21.05000000000000071, 12.10919762232931518, -206.2073353557311748 ) ) ;
#5324 = AXIS2_PLACEMENT_3D ( 'NONE', #23396, #102872, #182453 ) ;
#5326 = CYLINDRICAL_SURFACE ( 'NONE', #199567, 0.09999999999999864553 ) ;
#5325 = CARTESIAN_POINT ( 'NONE',  ( 20.94999999999999929, 74.16465844978765176, -124.9679561919613207 ) ) ;
#5327 = CARTESIAN_POINT ( 'NONE',  ( 18.59999999999999076, 69.35000000001151932, -48.37310748452436826 ) ) ;
#5328 = EDGE_CURVE ( 'NONE', #216196, #51264, #73472, .T. ) ;
#5329 = CARTESIAN_POINT ( 'NONE',  ( 22.48660254037844197, 64.35000000001164722, -69.57310748452439952 ) ) ;
#5330 = AXIS2_PLACEMENT_3D ( 'NONE', #135100, #155992, #94700 ) ;
#5331 = DIRECTION ( 'NONE',  ( 1.000000000000000000, 0.000000000000000000, 0.000000000000000000 ) ) ;
#5332 = CARTESIAN_POINT ( 'NONE',  ( 21.00000000000000000, 66.25000000001223555, -148.8731074845244393 ) ) ;
#5334 = ORIENTED_EDGE ( 'NONE', *, *, #186868, .F. ) ;
#5333 = CARTESIAN_POINT ( 'NONE',  ( 22.00411653889230834, 29.99888786984128330, -252.4262548924342013 ) ) ;
#5335 = AXIS2_PLACEMENT_3D ( 'NONE', #234878, #56209, #253136 ) ;
#5336 = CIRCLE ( 'NONE', #192815, 9.500000000000001776 ) ;
#5337 = VECTOR ( 'NONE', #70660, 1000.000000000000000 ) ;
#5338 = EDGE_CURVE ( 'NONE', #108560, #45688, #219167, .T. ) ;
#5339 = TOROIDAL_SURFACE ( 'NONE', #55389, 0.4000000000000010214, 0.1000000000000000056 ) ;
#5340 = EDGE_CURVE ( 'NONE', #128962, #161509, #256529, .T. ) ;
#5341 = EDGE_CURVE ( 'NONE', #220738, #17623, #13744, .T. ) ;
#5342 = SPHERICAL_SURFACE ( 'NONE', #191634, 0.1000000000000000056 ) ;
#5343 = CARTESIAN_POINT ( 'NONE',  ( 21.12642695952774119, 65.46697144162916970, -241.9826101524681690 ) ) ;
#5344 = ADVANCED_FACE ( 'NONE', ( #35895 ), #102618, .F. ) ;
#5345 = CARTESIAN_POINT ( 'NONE',  ( 14.87567385445976953, 9.430764995433476017, -149.2305373947504847 ) ) ;
#5346 = AXIS2_PLACEMENT_3D ( 'NONE', #241271, #39229, #101705 ) ;
#5347 = VERTEX_POINT ( 'NONE', #252336 ) ;
#5348 = AXIS2_PLACEMENT_3D ( 'NONE', #162640, #84313, #25690 ) ;
#5350 = CARTESIAN_POINT ( 'NONE',  ( 18.39999999999999858, 85.50000000001263345, -196.4910380878246201 ) ) ;
#5349 = AXIS2_PLACEMENT_3D ( 'NONE', #145713, #27099, #7497 ) ;
#5351 = DIRECTION ( 'NONE',  ( -2.812466655313718795E-14, -0.8096735173027139743, 0.5868805631290339164 ) ) ;
#5352 = DIRECTION ( 'NONE',  ( 0.000000000000000000, -0.2128009952263605342, 0.9770955615653315052 ) ) ;
#5353 = EDGE_LOOP ( 'NONE', ( #45507, #106957, #187708, #91716 ) ) ;
#5354 = DIRECTION ( 'NONE',  ( 0.000000000000000000, 0.000000000000000000, -1.000000000000000000 ) ) ;
#5356 = ORIENTED_EDGE ( 'NONE', *, *, #92045, .T. ) ;
#5355 = CARTESIAN_POINT ( 'NONE',  ( -23.25000000000000000, 86.45856254523214091, -209.4679346046102921 ) ) ;
#5358 = DIRECTION ( 'NONE',  ( 0.000000000000000000, 0.000000000000000000, 1.000000000000000000 ) ) ;
#5357 = CARTESIAN_POINT ( 'NONE',  ( 23.14999999999999503, 28.91254064196106910, -237.8576372133405528 ) ) ;
#5359 = EDGE_CURVE ( 'NONE', #164486, #156950, #77501, .T. ) ;
#5360 = DIRECTION ( 'NONE',  ( 0.000000000000000000, -1.000000000000000000, 0.000000000000000000 ) ) ;
#5361 = EDGE_LOOP ( 'NONE', ( #211147, #159509, #135371, #128073 ) ) ;
#5362 = DIRECTION ( 'NONE',  ( -1.000000000000000000, -1.594516344651357984E-15, 4.324467345337419894E-16 ) ) ;
#5363 = DIRECTION ( 'NONE',  ( 1.000000000000000000, 0.000000000000000000, 0.000000000000000000 ) ) ;
#5364 = DIRECTION ( 'NONE',  ( -0.000000000000000000, 0.9126074666063770380, 0.4088369013363281068 ) ) ;
#5365 = LINE ( 'NONE', #4109, #231437 ) ;
#5366 = FACE_OUTER_BOUND ( 'NONE', #139534, .T. ) ;
#5367 = VERTEX_POINT ( 'NONE', #17576 ) ;
#5368 = DIRECTION ( 'NONE',  ( 1.000000000000000000, -0.000000000000000000, 0.000000000000000000 ) ) ;
#5369 = CIRCLE ( 'NONE', #117819, 0.09999999999999939493 ) ;
#5370 = DIRECTION ( 'NONE',  ( 1.000000000000000000, 0.000000000000000000, 0.000000000000000000 ) ) ;
#5371 = CIRCLE ( 'NONE', #159540, 2.699999999999999289 ) ;
#5372 = DIRECTION ( 'NONE',  ( 0.000000000000000000, 0.2617529984165031243, 0.9651348961777157509 ) ) ;
#5373 = CARTESIAN_POINT ( 'NONE',  ( 23.14999999999999503, 13.98997548377052524, -210.4902890347897255 ) ) ;
#5374 = ORIENTED_EDGE ( 'NONE', *, *, #139850, .T. ) ;
#5375 = B_SPLINE_CURVE_WITH_KNOTS ( 'NONE', 3,
 ( #77278, #156859, #155582, #57709, #39484, #159409, #60280, #178999, #237651, #198516 ),
 .UNSPECIFIED., .F., .F.,
 ( 4, 2, 2, 2, 4 ),
 ( 0.000000000000000000, 4.221631689691002302E-05, 8.443263379382004604E-05, 0.0001688652675875677487, 0.0003377305351749838717 ),
 .UNSPECIFIED. ) ;
#5376 = ORIENTED_EDGE ( 'NONE', *, *, #101397, .F. ) ;
#5377 = CARTESIAN_POINT ( 'NONE',  ( 22.45380639572249493, 75.99999985734224595, -81.27354037563121381 ) ) ;
#5378 = CARTESIAN_POINT ( 'NONE',  ( -18.59999999999999787, 7.128833340093095217, -233.7327013124392749 ) ) ;
#5379 = CARTESIAN_POINT ( 'NONE',  ( 21.05000000000000071, 64.25000000001195133, -110.0379132551783243 ) ) ;
#5380 = CARTESIAN_POINT ( 'NONE',  ( -22.39999999999999503, 68.20922040163854660, -103.1231074845243540 ) ) ;
#5381 = CARTESIAN_POINT ( 'NONE',  ( 18.39999999999999858, 46.96039402156216624, -255.3459641718773128 ) ) ;
#5383 = CARTESIAN_POINT ( 'NONE',  ( -18.50000000000000711, 64.35000000001190301, -96.00830171387039513 ) ) ;
#5382 = DIRECTION ( 'NONE',  ( -0.000000000000000000, -0.2617529984165031243, -0.9651348961777157509 ) ) ;
#5384 = CARTESIAN_POINT ( 'NONE',  ( -18.59999999999999787, 14.06640494040441602, -210.3712993791105532 ) ) ;
#5385 = CARTESIAN_POINT ( 'NONE',  ( -18.59999999999999787, -11.75000000000000000, 5.900000000000001243 ) ) ;
#5386 = CARTESIAN_POINT ( 'NONE',  ( -18.51555513499156902, 47.04900152148760384, -255.1448163970531766 ) ) ;
#5387 = DIRECTION ( 'NONE',  ( 1.000000000000000000, 0.000000000000000000, 0.000000000000000000 ) ) ;
#5388 = EDGE_CURVE ( 'NONE', #251327, #24262, #144137, .T. ) ;
#5389 = AXIS2_PLACEMENT_3D ( 'NONE', #48719, #30468, #109974 ) ;
#5391 = ORIENTED_EDGE ( 'NONE', *, *, #159553, .T. ) ;
#5390 = CARTESIAN_POINT ( 'NONE',  ( 15.51872946208854565, 62.79551507739390814, -216.3883973845401556 ) ) ;
#5392 = CARTESIAN_POINT ( 'NONE',  ( -21.03571358705756467, 64.25000000001209344, -129.6980006624665123 ) ) ;
#5393 = FACE_OUTER_BOUND ( 'NONE', #178484, .T. ) ;
#5395 = CARTESIAN_POINT ( 'NONE',  ( -18.59999999999999787, 18.41524492703432614, -237.0006385043383546 ) ) ;
#5394 = DIRECTION ( 'NONE',  ( -1.000000000000000000, 0.000000000000000000, 0.000000000000000000 ) ) ;
#5396 = ORIENTED_EDGE ( 'NONE', *, *, #163258, .F. ) ;
#5397 = CARTESIAN_POINT ( 'NONE',  ( -16.87333278164152617, 66.11739021543287720, -56.38993967837032528 ) ) ;
#5398 = DIRECTION ( 'NONE',  ( -1.000000000000000000, 0.000000000000000000, 0.000000000000000000 ) ) ;
#5399 = DIRECTION ( 'NONE',  ( 1.000000000000000000, 0.000000000000000000, 0.000000000000000000 ) ) ;
#5400 = CARTESIAN_POINT ( 'NONE',  ( -20.94999999999999929, 1.835341550235567887, -145.5551512925629822 ) ) ;
#5402 = ADVANCED_FACE ( 'NONE', ( #232812 ), #38438, .T. ) ;
#5401 = CARTESIAN_POINT ( 'NONE',  ( -12.30589683808040746, 66.64325398293431135, -186.3197477631601942 ) ) ;
#5403 = ORIENTED_EDGE ( 'NONE', *, *, #105661, .F. ) ;
#5404 = ORIENTED_EDGE ( 'NONE', *, *, #5739, .F. ) ;
#5405 = EDGE_CURVE ( 'NONE', #89629, #9372, #194275, .T. ) ;
#5406 = EDGE_CURVE ( 'NONE', #74587, #77399, #27693, .T. ) ;
#5408 = AXIS2_PLACEMENT_3D ( 'NONE', #72456, #75041, #172871 ) ;
#5407 = FACE_OUTER_BOUND ( 'NONE', #155631, .T. ) ;
#5409 = VERTEX_POINT ( 'NONE', #97085 ) ;
#5410 = CARTESIAN_POINT ( 'NONE',  ( 16.87683809663750267, 66.05000000001157900, -56.87310748452439668 ) ) ;
#5411 = EDGE_LOOP ( 'NONE', ( #58456, #83418, #41218, #62892 ) ) ;
#5412 = AXIS2_PLACEMENT_3D ( 'NONE', #127689, #11600, #188938 ) ;
#5413 = DIRECTION ( 'NONE',  ( 1.000000000000000000, -0.000000000000000000, -0.000000000000000000 ) ) ;
#5414 = CARTESIAN_POINT ( 'NONE',  ( -18.50000000000000000, 68.50594083727658301, -224.0235912779512830 ) ) ;
#5415 = AXIS2_PLACEMENT_3D ( 'NONE', #88065, #107656, #232452 ) ;
#5416 = CARTESIAN_POINT ( 'NONE',  ( -20.99749315643147440, 62.82351852664101699, -207.2177435904692118 ) ) ;
#5417 = ORIENTED_EDGE ( 'NONE', *, *, #72508, .T. ) ;
#5418 = ADVANCED_FACE ( 'NONE', ( #15043 ), #247547, .F. ) ;
#5419 = EDGE_CURVE ( 'NONE', #69020, #118333, #194968, .T. ) ;
#5420 = DIRECTION ( 'NONE',  ( -1.000000000000000000, 0.000000000000000000, 0.000000000000000000 ) ) ;
#5421 = CARTESIAN_POINT ( 'NONE',  ( -21.05000000000000071, 65.61575147395463148, -242.1939180743342774 ) ) ;
#5422 = LINE ( 'NONE', #25047, #40807 ) ;
#5423 = CIRCLE ( 'NONE', #109491, 4.000000000000003553 ) ;
#5425 = DIRECTION ( 'NONE',  ( 0.000000000000000000, 7.086529944415886769E-15, -1.000000000000000000 ) ) ;
#5424 = AXIS2_PLACEMENT_3D ( 'NONE', #32197, #167863, #90851 ) ;
#5426 = DIRECTION ( 'NONE',  ( 1.000000000000000000, 0.000000000000000000, 0.000000000000000000 ) ) ;
#5427 = PRODUCT_DEFINITION ( 'UNKNOWN', '', #69634, #100050 ) ;
#5429 = VECTOR ( 'NONE', #9922, 1000.000000000000000 ) ;
#5428 = DIRECTION ( 'NONE',  ( 1.000000000000000000, 0.000000000000000000, -0.000000000000000000 ) ) ;
#5430 = CARTESIAN_POINT ( 'NONE',  ( 21.05995757104869526, 11.16948182890036456, -211.0481761046111444 ) ) ;
#5431 = ORIENTED_EDGE ( 'NONE', *, *, #201112, .T. ) ;
#5433 = CARTESIAN_POINT ( 'NONE',  ( 18.57071067811864040, 65.82071067813016896, -48.27310748452439526 ) ) ;
#5432 = CARTESIAN_POINT ( 'NONE',  ( -21.10000000000000142, 0.000000000000000000, 0.000000000000000000 ) ) ;
#5434 = ORIENTED_EDGE ( 'NONE', *, *, #76568, .T. ) ;
#5436 = ORIENTED_EDGE ( 'NONE', *, *, #13960, .T. ) ;
#5435 = DIRECTION ( 'NONE',  ( -1.000000000000000000, 0.000000000000000000, 0.000000000000000000 ) ) ;
#5437 = ORIENTED_EDGE ( 'NONE', *, *, #247175, .T. ) ;
#5438 = CYLINDRICAL_SURFACE ( 'NONE', #153147, 0.09999999999999939493 ) ;
#5439 = DIRECTION ( 'NONE',  ( 0.000000000000000000, -1.000000000000000000, 0.000000000000000000 ) ) ;
#5440 = CARTESIAN_POINT ( 'NONE',  ( -20.64999999999999858, -9.399999999988850163, -76.89396912265249284 ) ) ;
#5441 = EDGE_CURVE ( 'NONE', #13799, #85212, #56825, .T. ) ;
#5442 = VECTOR ( 'NONE', #97334, 1000.000000000000227 ) ;
#5443 = DIRECTION ( 'NONE',  ( -1.000000000000000000, 0.000000000000000000, 0.000000000000000000 ) ) ;
#5444 = ORIENTED_EDGE ( 'NONE', *, *, #234755, .F. ) ;
#5445 = ADVANCED_FACE ( 'NONE', ( #76269 ), #155842, .F. ) ;
#5446 = EDGE_CURVE ( 'NONE', #145746, #180772, #223268, .T. ) ;
#5447 = CARTESIAN_POINT ( 'NONE',  ( -21.05000000000000071, -1.835341550224411922, -11.65515129256297833 ) ) ;
#5448 = CARTESIAN_POINT ( 'NONE',  ( -16.80100426158792004, 66.05684947961613318, -157.3401617316904151 ) ) ;
#5449 = AXIS2_PLACEMENT_3D ( 'NONE', #115099, #52541, #210357 ) ;
#5450 = VERTEX_POINT ( 'NONE', #138779 ) ;
#5451 = AXIS2_PLACEMENT_3D ( 'NONE', #235450, #77650, #257532 ) ;
#5452 = AXIS2_PLACEMENT_3D ( 'NONE', #94920, #75405, #174535 ) ;
#5453 = CARTESIAN_POINT ( 'NONE',  ( -20.85882249326303040, 10.33248238082519066, -39.09484654391314962 ) ) ;
#5454 = AXIS2_PLACEMENT_3D ( 'NONE', #134936, #37173, #154569 ) ;
#5455 = CARTESIAN_POINT ( 'NONE',  ( -23.25000000000000000, -1.835859311432481045, -212.5044391687984842 ) ) ;
#5456 = EDGE_LOOP ( 'NONE', ( #217930, #251861, #121783, #237435 ) ) ;
#5457 = DIRECTION ( 'NONE',  ( 1.000000000000000000, 0.000000000000000000, 0.000000000000000000 ) ) ;
#5458 = ORIENTED_EDGE ( 'NONE', *, *, #77598, .T. ) ;
#5459 = DIRECTION ( 'NONE',  ( 0.000000000000000000, 1.000000000000000000, 1.626303258728238113E-15 ) ) ;
#5460 = ORIENTED_EDGE ( 'NONE', *, *, #190126, .F. ) ;
#5461 = CARTESIAN_POINT ( 'NONE',  ( -15.55912972643740488, 8.490870273573721150, -54.45000000000000284 ) ) ;
#5462 = DIRECTION ( 'NONE',  ( -1.000000000000000000, -2.885090398161910739E-16, -6.283419270304611573E-17 ) ) ;
#5463 = CARTESIAN_POINT ( 'NONE',  ( 23.15000000000000213, -9.000000000000001776, -9.893969122652443104 ) ) ;
#5464 = CARTESIAN_POINT ( 'NONE',  ( -21.53752568617696284, 6.610297987518923613, -199.4590530230520073 ) ) ;
#5465 = ADVANCED_FACE ( 'NONE', ( #39755 ), #110853, .F. ) ;
#5466 = AXIS2_PLACEMENT_3D ( 'NONE', #229635, #129254, #77924 ) ;
#5467 = CIRCLE ( 'NONE', #184545, 0.5999999999999998668 ) ;
#5468 = CARTESIAN_POINT ( 'NONE',  ( -23.15000000000000213, 74.07476635515199348, -82.25335101765045920 ) ) ;
#5469 = FACE_OUTER_BOUND ( 'NONE', #199782, .T. ) ;
#5470 = CARTESIAN_POINT ( 'NONE',  ( -22.39999999999999858, 1.115600667400684642E-11, -25.70922040162659883 ) ) ;
#5471 = ORIENTED_EDGE ( 'NONE', *, *, #188128, .F. ) ;
#5473 = DIRECTION ( 'NONE',  ( -1.000000000000000000, -3.265361837132813093E-16, 0.000000000000000000 ) ) ;
#5472 = CARTESIAN_POINT ( 'NONE',  ( -21.11825140030083148, 69.55459243459225149, -170.0303111051570681 ) ) ;
#5474 = VERTEX_POINT ( 'NONE', #78825 ) ;
#5475 = AXIS2_PLACEMENT_3D ( 'NONE', #11030, #170147, #249650 ) ;
#5476 = DIRECTION ( 'NONE',  ( 1.000000000000000000, 0.000000000000000000, 0.000000000000000000 ) ) ;
#5477 = ADVANCED_FACE ( 'NONE', ( #18868 ), #102222, .T. ) ;
#5478 = DIRECTION ( 'NONE',  ( -1.000000000000000000, -0.000000000000000000, -0.000000000000000000 ) ) ;
#5479 = CIRCLE ( 'NONE', #38834, 0.09999999999999939493 ) ;
#5481 = ORIENTED_EDGE ( 'NONE', *, *, #83550, .F. ) ;
#5480 = CARTESIAN_POINT ( 'NONE',  ( -21.05000000000000071, 74.16465844978787914, -158.4679561919613775 ) ) ;
#5483 = ORIENTED_EDGE ( 'NONE', *, *, #91685, .F. ) ;
#5482 = CARTESIAN_POINT ( 'NONE',  ( 21.06086055315975258, 67.22529248505534838, -57.32078532937043747 ) ) ;
#5484 = CARTESIAN_POINT ( 'NONE',  ( -16.77683809663752257, 51.61886293219124155, -231.9464690156495692 ) ) ;
#5485 = CARTESIAN_POINT ( 'NONE',  ( -20.85000000000000142, 14.78417726655519715, -235.8865342417136333 ) ) ;
#5486 = FACE_OUTER_BOUND ( 'NONE', #100643, .T. ) ;
#5487 = VECTOR ( 'NONE', #95802, 1000.000000000000000 ) ;
#5488 = EDGE_CURVE ( 'NONE', #224848, #11139, #90169, .T. ) ;
#5489 = DIRECTION ( 'NONE',  ( 1.000000000000000000, 0.000000000000000000, 0.000000000000000000 ) ) ;
#5491 = ORIENTED_EDGE ( 'NONE', *, *, #140323, .T. ) ;
#5490 = FACE_OUTER_BOUND ( 'NONE', #234913, .T. ) ;
#5492 = AXIS2_PLACEMENT_3D ( 'NONE', #118115, #215910, #52998 ) ;
#5493 = CIRCLE ( 'NONE', #226231, 11.79999999999999893 ) ;
#5494 = EDGE_CURVE ( 'NONE', #39258, #231042, #160972, .T. ) ;
#5495 = VECTOR ( 'NONE', #36429, 999.9999999999998863 ) ;
#5496 = PRODUCT ( 'Injection Molded Chain Links 12', 'Injection Molded Chain Links 12', '', ( #57338 ) ) ;
#5497 = AXIS2_PLACEMENT_3D ( 'NONE', #49125, #45281, #7425 ) ;
#5499 = EDGE_CURVE ( 'NONE', #86809, #96525, #240038, .T. ) ;
#5498 = FACE_OUTER_BOUND ( 'NONE', #139366, .T. ) ;
#5501 = EDGE_CURVE ( 'NONE', #118363, #143932, #44230, .T. ) ;
#5500 = ORIENTED_EDGE ( 'NONE', *, *, #154025, .F. ) ;
#5502 = ORIENTED_EDGE ( 'NONE', *, *, #170963, .F. ) ;
#5503 = DIRECTION ( 'NONE',  ( -1.000000000000000000, -0.000000000000000000, -0.000000000000000000 ) ) ;
#5504 = CARTESIAN_POINT ( 'NONE',  ( 19.97071067695909363, 34.41526977942278620, -235.0529015606424537 ) ) ;
#5505 = CIRCLE ( 'NONE', #47202, 0.1000000000000024342 ) ;
#5506 = VERTEX_POINT ( 'NONE', #198789 ) ;
#5507 = CARTESIAN_POINT ( 'NONE',  ( -23.15000000000000213, 1.115600667400684642E-11, -134.0000000000000000 ) ) ;
#5508 = CIRCLE ( 'NONE', #238770, 0.09999999999999939493 ) ;
#5509 = DIRECTION ( 'NONE',  ( -3.265361837132812600E-16, 0.4721928772777346239, 0.8814952561688430555 ) ) ;
#5510 = CIRCLE ( 'NONE', #130441, 0.1000000000000045158 ) ;
#5511 = ORIENTED_EDGE ( 'NONE', *, *, #72077, .F. ) ;
#5513 = EDGE_CURVE ( 'NONE', #25987, #78948, #201362, .T. ) ;
#5512 = DIRECTION ( 'NONE',  ( 0.000000000000000000, 0.000000000000000000, 1.000000000000000000 ) ) ;
#5514 = EDGE_CURVE ( 'NONE', #172081, #182847, #137408, .T. ) ;
#5515 = AXIS2_PLACEMENT_3D ( 'NONE', #225739, #168413, #165816 ) ;
#5516 = ORIENTED_EDGE ( 'NONE', *, *, #237595, .T. ) ;
#5517 = AXIS2_PLACEMENT_3D ( 'NONE', #72795, #245307, #253946 ) ;
#5518 = VERTEX_POINT ( 'NONE', #140086 ) ;
#5519 = CARTESIAN_POINT ( 'NONE',  ( -18.47130263965439667, -9.471155585952800493, -73.68340476547700746 ) ) ;
#5520 = ORIENTED_EDGE ( 'NONE', *, *, #136132, .T. ) ;
#5521 = ADVANCED_FACE ( 'NONE', ( #41032 ), #100926, .F. ) ;
#5522 = DIRECTION ( 'NONE',  ( 0.000000000000000000, -0.2128009952263568982, 0.9770955615653323934 ) ) ;
#5523 = ORIENTED_EDGE ( 'NONE', *, *, #39101, .F. ) ;
#5525 = ORIENTED_EDGE ( 'NONE', *, *, #232673, .F. ) ;
#5524 = DIRECTION ( 'NONE',  ( -3.265361837132812600E-16, -0.4088369013363282178, 0.9126074666063768159 ) ) ;
#5526 = DIRECTION ( 'NONE',  ( -1.000000000000000000, -0.000000000000000000, -0.000000000000000000 ) ) ;
#5527 = ORIENTED_EDGE ( 'NONE', *, *, #208102, .F. ) ;
#5528 = CYLINDRICAL_SURFACE ( 'NONE', #168096, 0.09999999999999939493 ) ;
#5530 = VERTEX_POINT ( 'NONE', #220908 ) ;
#5529 = ADVANCED_FACE ( 'NONE', ( #98362 ), #1855, .F. ) ;
#5532 = ORIENTED_EDGE ( 'NONE', *, *, #10692, .F. ) ;
#5531 = VERTEX_POINT ( 'NONE', #42296 ) ;
#5533 = DIRECTION ( 'NONE',  ( -0.000000000000000000, -0.000000000000000000, 1.000000000000000000 ) ) ;
#5534 = EDGE_CURVE ( 'NONE', #81245, #109039, #143949, .T. ) ;
#5535 = CARTESIAN_POINT ( 'NONE',  ( -16.90128866880176162, 14.16540792955462713, -219.2666506534965833 ) ) ;
#5537 = ORIENTED_EDGE ( 'NONE', *, *, #215031, .F. ) ;
#5536 = AXIS2_PLACEMENT_3D ( 'NONE', #156306, #234515, #174613 ) ;
#5538 = VECTOR ( 'NONE', #97161, 1000.000000000000000 ) ;
#5539 = CIRCLE ( 'NONE', #151333, 0.09999999999999939493 ) ;
#5540 = CIRCLE ( 'NONE', #38903, 11.75000000000000000 ) ;
#5541 = ORIENTED_EDGE ( 'NONE', *, *, #47352, .T. ) ;
#5542 = DIRECTION ( 'NONE',  ( -1.000000000000000000, 0.000000000000000000, 0.000000000000000000 ) ) ;
#5543 = CARTESIAN_POINT ( 'NONE',  ( -21.64999999999999858, 65.69978428250288971, -213.4221254243406065 ) ) ;
#5545 = VERTEX_POINT ( 'NONE', #257423 ) ;
#5544 = DIRECTION ( 'NONE',  ( 1.000000000000000000, 0.000000000000000000, 0.000000000000000000 ) ) ;
#5546 = LINE ( 'NONE', #227177, #18846 ) ;
#5547 = ORIENTED_EDGE ( 'NONE', *, *, #119274, .F. ) ;
#5548 = EDGE_CURVE ( 'NONE', #71381, #37214, #65060, .T. ) ;
#5549 = DIRECTION ( 'NONE',  ( 0.000000000000000000, -0.4999999999999413247, 0.8660254037844724584 ) ) ;
#5550 = CARTESIAN_POINT ( 'NONE',  ( -23.15000000000000213, 70.05000000001149374, -46.32880978955918039 ) ) ;
#5551 = ADVANCED_FACE ( 'NONE', ( #89121 ), #244118, .F. ) ;
#5552 = VERTEX_POINT ( 'NONE', #125677 ) ;
#5553 = CARTESIAN_POINT ( 'NONE',  ( 20.73486653747088226, 7.250000000000026645, -12.65000000000000568 ) ) ;
#5554 = DIRECTION ( 'NONE',  ( 1.000000000000000000, 0.000000000000000000, -0.000000000000000000 ) ) ;
#5555 = ORIENTED_EDGE ( 'NONE', *, *, #109757, .F. ) ;
#5556 = DIRECTION ( 'NONE',  ( 1.000000000000000000, -0.000000000000000000, 0.000000000000000000 ) ) ;
#5557 = VERTEX_POINT ( 'NONE', #44865 ) ;
#5559 = EDGE_LOOP ( 'NONE', ( #184908, #121556, #8120, #6395 ) ) ;
#5558 = VERTEX_POINT ( 'NONE', #65704 ) ;
#5560 = AXIS2_PLACEMENT_3D ( 'NONE', #50988, #227078, #210112 ) ;
#5561 = ORIENTED_EDGE ( 'NONE', *, *, #13863, .T. ) ;
#5562 = FACE_OUTER_BOUND ( 'NONE', #232632, .T. ) ;
#5563 = VERTEX_POINT ( 'NONE', #10882 ) ;
#5564 = PLANE ( 'NONE',  #171594 ) ;
#5565 = ORIENTED_EDGE ( 'NONE', *, *, #214767, .F. ) ;
#5566 = LINE ( 'NONE', #25180, #35634 ) ;
#5567 = CARTESIAN_POINT ( 'NONE',  ( -23.15000000000000213, 76.00000000001142553, -36.02310748452432421 ) ) ;
#5568 = VERTEX_POINT ( 'NONE', #108688 ) ;
#5569 = VERTEX_POINT ( 'NONE', #87812 ) ;
#5570 = AXIS2_PLACEMENT_3D ( 'NONE', #82463, #165915, #62935 ) ;
#5571 = ORIENTED_EDGE ( 'NONE', *, *, #60961, .F. ) ;
#5572 = EDGE_CURVE ( 'NONE', #138951, #109875, #19264, .T. ) ;
#5573 = TOROIDAL_SURFACE ( 'NONE', #184657, 0.2000000000000000111, 0.1000000000000000056 ) ;
#5574 = DIRECTION ( 'NONE',  ( -0.4999999999999799050, -6.047423072554995242E-15, 0.8660254037844502539 ) ) ;
#5575 = ORIENTED_EDGE ( 'NONE', *, *, #252743, .F. ) ;
#5576 = DIRECTION ( 'NONE',  ( 0.000000000000000000, 0.000000000000000000, 1.000000000000000000 ) ) ;
#5578 = ORIENTED_EDGE ( 'NONE', *, *, #156178, .F. ) ;
#5577 = DIRECTION ( 'NONE',  ( 1.000000000000000000, -0.000000000000000000, -0.000000000000000000 ) ) ;
#5579 = CYLINDRICAL_SURFACE ( 'NONE', #230350, 2.000000000000001776 ) ;
#5580 = CARTESIAN_POINT ( 'NONE',  ( -20.85000000000000142, 11.75000000001115197, -127.2161343370219413 ) ) ;
#5581 = DIRECTION ( 'NONE',  ( 0.000000000000000000, 0.8814952561688425003, -0.4721928772777359007 ) ) ;
#5582 = CARTESIAN_POINT ( 'NONE',  ( -18.40000000000000213, 64.51332499825393541, -60.27310748452440947 ) ) ;
#5583 = DIRECTION ( 'NONE',  ( 0.000000000000000000, -6.982962677686266711E-15, 1.000000000000000000 ) ) ;
#5585 = CARTESIAN_POINT ( 'NONE',  ( 21.04999999999999716, 34.05155896670549254, -243.7673268003813973 ) ) ;
#5584 = DIRECTION ( 'NONE',  ( 1.000000000000000000, 0.000000000000000000, 0.000000000000000000 ) ) ;
#5586 = CARTESIAN_POINT ( 'NONE',  ( 20.94999999999999574, 4.313202326203132486, -245.5540684919841681 ) ) ;
#5587 = LINE ( 'NONE', #42189, #232001 ) ;
#5588 = AXIS2_PLACEMENT_3D ( 'NONE', #65713, #188233, #109969 ) ;
#5589 = FACE_OUTER_BOUND ( 'NONE', #108619, .T. ) ;
#5590 = EDGE_CURVE ( 'NONE', #157652, #184585, #173459, .T. ) ;
#5591 = FACE_OUTER_BOUND ( 'NONE', #69074, .T. ) ;
#5592 = AXIS2_PLACEMENT_3D ( 'NONE', #226437, #11275, #47803 ) ;
#5593 = VERTEX_POINT ( 'NONE', #70879 ) ;
#5594 = AXIS2_PLACEMENT_3D ( 'NONE', #19810, #141034, #40682 ) ;
#5595 = TOROIDAL_SURFACE ( 'NONE', #163854, 11.65000000000000036, 0.1000000000000000056 ) ;
#5597 = VERTEX_POINT ( 'NONE', #205200 ) ;
#5596 = DIRECTION ( 'NONE',  ( 0.000000000000000000, 0.000000000000000000, 1.000000000000000000 ) ) ;
#5598 = ORIENTED_EDGE ( 'NONE', *, *, #204717, .F. ) ;
#5599 = DIRECTION ( 'NONE',  ( 1.000000000000000000, 0.000000000000000000, 0.000000000000000000 ) ) ;
#5600 = CARTESIAN_POINT ( 'NONE',  ( 20.94999999999999929, 77.83534155023671985, -158.4679561919613491 ) ) ;
#5601 = CARTESIAN_POINT ( 'NONE',  ( -18.40000000000000213, 59.46930106059529919, -220.6430355403071530 ) ) ;
#5602 = ORIENTED_EDGE ( 'NONE', *, *, #18960, .T. ) ;
#5603 = AXIS2_PLACEMENT_3D ( 'NONE', #192623, #71408, #150925 ) ;
#5604 = CIRCLE ( 'NONE', #151405, 0.1000000000000028644 ) ;
#5606 = CIRCLE ( 'NONE', #118061, 0.09999999999999939493 ) ;
#5605 = CARTESIAN_POINT ( 'NONE',  ( 18.52928932188133970, 54.95214567929435390, -230.0923768967488456 ) ) ;
#5607 = CARTESIAN_POINT ( 'NONE',  ( -16.89208623190940273, 9.951577948975481647, -20.85527220321827002 ) ) ;
#5608 = ORIENTED_EDGE ( 'NONE', *, *, #160778, .F. ) ;
#5609 = FACE_OUTER_BOUND ( 'NONE', #173510, .T. ) ;
#5610 = DIRECTION ( 'NONE',  ( 0.000000000000000000, -1.000000000000000000, -6.982962677686266711E-15 ) ) ;
#5611 = CARTESIAN_POINT ( 'NONE',  ( 21.05000000000000071, 65.27628289530407812, -61.85819391543678591 ) ) ;
#5612 = DIRECTION ( 'NONE',  ( 0.000000000000000000, -0.1298341882519953860, -0.9915357197604862671 ) ) ;
#5614 = ORIENTED_EDGE ( 'NONE', *, *, #113183, .T. ) ;
#5613 = LINE ( 'NONE', #43495, #1943 ) ;
#5615 = CARTESIAN_POINT ( 'NONE',  ( -18.59999999999999787, -1.164121893230052995, -208.7148480855715604 ) ) ;
#5616 = DIRECTION ( 'NONE',  ( -0.000000000000000000, 0.8103668758649578141, -0.5859227990963212784 ) ) ;
#5617 = CIRCLE ( 'NONE', #234605, 3.999999999999999112 ) ;
#5618 = FACE_OUTER_BOUND ( 'NONE', #69055, .T. ) ;
#5620 = DIRECTION ( 'NONE',  ( 0.000000000000000000, 0.9126074666063660468, 0.4088369013363524762 ) ) ;
#5619 = AXIS2_PLACEMENT_3D ( 'NONE', #78324, #57471, #236128 ) ;
#5622 = ORIENTED_EDGE ( 'NONE', *, *, #200586, .F. ) ;
#5621 = CIRCLE ( 'NONE', #205546, 11.79999999999999005 ) ;
#5623 = CARTESIAN_POINT ( 'NONE',  ( -16.94062896051973865, 66.00728089491161654, -157.4205909424056244 ) ) ;
#5624 = LINE ( 'NONE', #147743, #27863 ) ;
#5625 = VECTOR ( 'NONE', #40415, 1000.000000000000000 ) ;
#5627 = CARTESIAN_POINT ( 'NONE',  ( -21.05000000000000071, 48.05114133249968944, -246.4758750954581785 ) ) ;
#5626 = CARTESIAN_POINT ( 'NONE',  ( -17.27223548803312170, 65.65460260865577879, -80.88950130532087712 ) ) ;
#5628 = PLANE ( 'NONE',  #16445 ) ;
#5630 = EDGE_CURVE ( 'NONE', #159923, #8256, #202616, .T. ) ;
#5629 = DIRECTION ( 'NONE',  ( -0.000000000000000000, -6.982962677686266711E-15, 1.000000000000000000 ) ) ;
#5631 = CARTESIAN_POINT ( 'NONE',  ( -18.59999999999999787, 10.33248238082518711, -39.09484654391314962 ) ) ;
#5632 = DIRECTION ( 'NONE',  ( 0.000000000000000000, -0.9651348961777157509, 0.2617529984165027912 ) ) ;
#5633 = CARTESIAN_POINT ( 'NONE',  ( 20.85000000000000142, 67.32498692201720303, -236.1680459564915679 ) ) ;
#5634 = ORIENTED_EDGE ( 'NONE', *, *, #24282, .F. ) ;
#5635 = DIRECTION ( 'NONE',  ( -1.836970198721029934E-16, -1.000000000000000000, -6.982962677686266711E-15 ) ) ;
#5636 = ORIENTED_EDGE ( 'NONE', *, *, #236832, .T. ) ;
#5637 = ORIENTED_EDGE ( 'NONE', *, *, #44504, .T. ) ;
#5638 = ADVANCED_FACE ( 'NONE', ( #167403 ), #152586, .T. ) ;
#5639 = DIRECTION ( 'NONE',  ( 1.000000000000000000, 0.000000000000000000, 0.000000000000000000 ) ) ;
#5640 = DIRECTION ( 'NONE',  ( 0.000000000000000000, -0.8814952561688430555, 0.4721928772777345684 ) ) ;
#5641 = EDGE_LOOP ( 'NONE', ( #55625, #28021, #137201, #171340, #191403, #157430, #157861, #4004, #95452, #186498, #98889, #93403, #171168, #205692, #15359, #12002, #3890, #68696 ) ) ;
#5642 = EDGE_CURVE ( 'NONE', #3546, #29211, #145229, .T. ) ;
#5643 = VERTEX_POINT ( 'NONE', #129545 ) ;
#5644 = AXIS2_PLACEMENT_3D ( 'NONE', #203006, #257799, #139162 ) ;
#5645 = EDGE_CURVE ( 'NONE', #194417, #150252, #248397, .T. ) ;
#5646 = VERTEX_POINT ( 'NONE', #244333 ) ;
#5647 = AXIS2_PLACEMENT_3D ( 'NONE', #119995, #164237, #200781 ) ;
#5648 = CARTESIAN_POINT ( 'NONE',  ( -18.59999999999999787, 66.65000000001157332, -57.37310748452438247 ) ) ;
#5649 = ORIENTED_EDGE ( 'NONE', *, *, #5201, .T. ) ;
#5650 = LINE ( 'NONE', #245587, #121614 ) ;
#5651 = DIRECTION ( 'NONE',  ( 0.000000000000000000, 0.000000000000000000, -1.000000000000000000 ) ) ;
#5652 = CARTESIAN_POINT ( 'NONE',  ( -20.64999999999999858, 4.350000000011156054, -79.35000000000005116 ) ) ;
#5653 = DIRECTION ( 'NONE',  ( 1.000000000000000000, -0.000000000000000000, 0.000000000000000000 ) ) ;
#5654 = DIRECTION ( 'NONE',  ( 0.000000000000000000, 0.9770955615653260651, 0.2128009952263853755 ) ) ;
#5655 = AXIS2_PLACEMENT_3D ( 'NONE', #250337, #71720, #32617 ) ;
#5656 = CARTESIAN_POINT ( 'NONE',  ( -16.81744102076748959, 30.20632856012693424, -234.8070450048000737 ) ) ;
#5657 = CARTESIAN_POINT ( 'NONE',  ( 18.59999999999999076, 11.65000000001115943, -125.3500000000000512 ) ) ;
#5659 = EDGE_LOOP ( 'NONE', ( #189875, #147682, #217332, #52542 ) ) ;
#5658 = DIRECTION ( 'NONE',  ( 0.000000000000000000, 0.5000000000000729417, 0.8660254037843965191 ) ) ;
#5661 = DIRECTION ( 'NONE',  ( 0.000000000000000000, 1.000000000000000000, 0.000000000000000000 ) ) ;
#5660 = DIRECTION ( 'NONE',  ( -0.000000000000000000, 1.000000000000000000, 1.626303258728266709E-15 ) ) ;
#5662 = EDGE_CURVE ( 'NONE', #23751, #207855, #135963, .T. ) ;
#5663 = CARTESIAN_POINT ( 'NONE',  ( -21.00023020733502932, 76.00000000001170974, -75.91397672979267952 ) ) ;
#5664 = ORIENTED_EDGE ( 'NONE', *, *, #30064, .F. ) ;
#5665 = DIRECTION ( 'NONE',  ( -0.000000000000000000, -6.982962677686266711E-15, 1.000000000000000000 ) ) ;
#5666 = CIRCLE ( 'NONE', #97222, 7.900000000000004796 ) ;
#5667 = LINE ( 'NONE', #46097, #2219 ) ;
#5668 = LINE ( 'NONE', #203891, #204156 ) ;
#5669 = VERTEX_POINT ( 'NONE', #7013 ) ;
#5670 = CIRCLE ( 'NONE', #201331, 0.09999999999999824307 ) ;
#5672 = CARTESIAN_POINT ( 'NONE',  ( -16.93344882324368683, 66.00341123272413313, -115.6100817897194446 ) ) ;
#5671 = CARTESIAN_POINT ( 'NONE',  ( 18.59999999999999787, 74.13328508995475374, -124.7704322382423072 ) ) ;
#5673 = AXIS2_PLACEMENT_3D ( 'NONE', #230738, #74254, #93769 ) ;
#5674 = FACE_OUTER_BOUND ( 'NONE', #24234, .T. ) ;
#5675 = VERTEX_POINT ( 'NONE', #209073 ) ;
#5676 = AXIS2_PLACEMENT_3D ( 'NONE', #169481, #209857, #11663 ) ;
#5677 = CARTESIAN_POINT ( 'NONE',  ( 21.05000000000000071, 6.540656951712401579, -67.10000000000005116 ) ) ;
#5678 = FACE_OUTER_BOUND ( 'NONE', #72669, .T. ) ;
#5679 = FACE_OUTER_BOUND ( 'NONE', #105384, .T. ) ;
#5680 = CYLINDRICAL_SURFACE ( 'NONE', #99218, 0.09999999999998898659 ) ;
#5681 = ORIENTED_EDGE ( 'NONE', *, *, #75557, .T. ) ;
#5682 = AXIS2_PLACEMENT_3D ( 'NONE', #237276, #58610, #218978 ) ;
#5683 = ORIENTED_EDGE ( 'NONE', *, *, #45182, .T. ) ;
#5684 = ADVANCED_FACE ( 'NONE', ( #107395, #5704 ), #26604, .F. ) ;
#5685 = DIRECTION ( 'NONE',  ( -1.000000000000000000, -1.836970198721029934E-16, -0.000000000000000000 ) ) ;
#5687 = TOROIDAL_SURFACE ( 'NONE', #51472, 3.899999999999999467, 0.1000000000000000056 ) ;
#5686 = CARTESIAN_POINT ( 'NONE',  ( 21.04999999999999716, 10.68430915749624077, -41.02669679032685224 ) ) ;
#5688 = CARTESIAN_POINT ( 'NONE',  ( 23.24999999999999289, 64.35000000001150511, -48.17310748452440095 ) ) ;
#5689 = DIRECTION ( 'NONE',  ( 1.000000000000000000, 0.000000000000000000, 0.000000000000000000 ) ) ;
#5690 = FACE_OUTER_BOUND ( 'NONE', #7131, .T. ) ;
#5691 = CARTESIAN_POINT ( 'NONE',  ( -21.05000000000000071, 76.00000000001195133, -103.0231074845243171 ) ) ;
#5692 = AXIS2_PLACEMENT_3D ( 'NONE', #149296, #214378, #55268 ) ;
#5693 = ORIENTED_EDGE ( 'NONE', *, *, #151891, .T. ) ;
#5694 = CARTESIAN_POINT ( 'NONE',  ( -18.50000000000000000, 64.25000000001215028, -136.4231074845243938 ) ) ;
#5695 = AXIS2_PLACEMENT_3D ( 'NONE', #156949, #193497, #119089 ) ;
#5696 = EDGE_CURVE ( 'NONE', #199802, #29646, #40145, .T. ) ;
#5698 = ORIENTED_EDGE ( 'NONE', *, *, #205981, .F. ) ;
#5697 = CARTESIAN_POINT ( 'NONE',  ( -18.59999999999999787, 77.83585931145546510, -91.51866831572576189 ) ) ;
#5699 = CIRCLE ( 'NONE', #59682, 0.5000000000000004441 ) ;
#5700 = CARTESIAN_POINT ( 'NONE',  ( 20.94999999999999929, 68.87972903831379767, -32.36354444268504693 ) ) ;
#5701 = CARTESIAN_POINT ( 'NONE',  ( -21.08376601933334271, 75.93622398908182447, -75.86505475580005964 ) ) ;
#5702 = CARTESIAN_POINT ( 'NONE',  ( 23.24999999999999645, 76.00000000001126921, -203.5231074845248997 ) ) ;
#5703 = CARTESIAN_POINT ( 'NONE',  ( -20.54999999999999716, 1.115600667400684642E-11, -67.00000000000000000 ) ) ;
#5705 = ORIENTED_EDGE ( 'NONE', *, *, #138962, .F. ) ;
#5704 = FACE_BOUND ( 'NONE', #121045, .T. ) ;
#5706 = CARTESIAN_POINT ( 'NONE',  ( 20.94999999999999929, 1.835341550235569663, -179.0551512925629538 ) ) ;
#5707 = DIRECTION ( 'NONE',  ( 1.000000000000000000, 0.000000000000000000, 0.000000000000000000 ) ) ;
#5708 = CARTESIAN_POINT ( 'NONE',  ( -23.25000000000000000, -11.65000000000000036, -3.100000000000001865 ) ) ;
#5709 = DIRECTION ( 'NONE',  ( 0.000000000000000000, -0.1350103645451945777, 0.9908441862701591329 ) ) ;
#5710 = EDGE_CURVE ( 'NONE', #101017, #15694, #148464, .T. ) ;
#5711 = ORIENTED_EDGE ( 'NONE', *, *, #65569, .F. ) ;
#5712 = DIRECTION ( 'NONE',  ( 0.000000000000000000, 0.000000000000000000, 1.000000000000000000 ) ) ;
#5713 = CARTESIAN_POINT ( 'NONE',  ( -16.89935556175729303, 66.05000000001200533, -116.1627838474090879 ) ) ;
#5714 = DIRECTION ( 'NONE',  ( -1.000000000000000000, 0.000000000000000000, 0.000000000000000000 ) ) ;
#5715 = EDGE_CURVE ( 'NONE', #72090, #186373, #147827, .T. ) ;
#5716 = CARTESIAN_POINT ( 'NONE',  ( -21.64999999999999858, 66.65000000001209912, -127.2731074845243597 ) ) ;
#5717 = AXIS2_PLACEMENT_3D ( 'NONE', #62953, #23861, #5524 ) ;
#5719 = ORIENTED_EDGE ( 'NONE', *, *, #166631, .F. ) ;
#5718 = AXIS2_PLACEMENT_3D ( 'NONE', #201146, #23829, #241560 ) ;
#5720 = DIRECTION ( 'NONE',  ( -1.000000000000000000, 0.000000000000000000, -0.000000000000000000 ) ) ;
#5721 = AXIS2_PLACEMENT_3D ( 'NONE', #82782, #162383, #142775 ) ;
#5722 = CIRCLE ( 'NONE', #205640, 0.1000000000000024342 ) ;
#5723 = ORIENTED_EDGE ( 'NONE', *, *, #51650, .F. ) ;
#5724 = DIRECTION ( 'NONE',  ( 1.186688945009010077E-16, 0.4088369013363281623, -0.9126074666063771490 ) ) ;
#5725 = DIRECTION ( 'NONE',  ( 0.000000000000000000, -0.8814952561688430555, 0.4721928772777346239 ) ) ;
#5726 = EDGE_CURVE ( 'NONE', #229949, #185034, #136120, .T. ) ;
#5727 = CARTESIAN_POINT ( 'NONE',  ( -20.85000000000000142, 69.34766280046808617, -247.6726305063181428 ) ) ;
#5728 = DIRECTION ( 'NONE',  ( 0.000000000000000000, 0.000000000000000000, 1.000000000000000000 ) ) ;
#5729 = VERTEX_POINT ( 'NONE', #66989 ) ;
#5730 = EDGE_CURVE ( 'NONE', #252297, #221637, #31944, .T. ) ;
#5732 = EDGE_CURVE ( 'NONE', #34312, #177630, #90361, .T. ) ;
#5731 = CARTESIAN_POINT ( 'NONE',  ( -21.05000000000000071, 36.65892442174472876, -249.5511627012454596 ) ) ;
#5733 = CARTESIAN_POINT ( 'NONE',  ( -23.25000000000000000, 76.00000000001126921, -203.5231074845248997 ) ) ;
#5734 = CARTESIAN_POINT ( 'NONE',  ( 18.54999999999999716, 19.41435213583508812, -230.3874019357809289 ) ) ;
#5735 = CARTESIAN_POINT ( 'NONE',  ( 18.51697539158856642, 10.31565961587946312, -206.5364194119177910 ) ) ;
#5736 = VERTEX_POINT ( 'NONE', #235065 ) ;
#5738 = VERTEX_POINT ( 'NONE', #13450 ) ;
#5737 = CARTESIAN_POINT ( 'NONE',  ( 21.05000000000000071, 24.07562609839690992, -252.7152152143214892 ) ) ;
#5739 = EDGE_CURVE ( 'NONE', #218080, #156566, #112553, .T. ) ;
#5740 = EDGE_LOOP ( 'NONE', ( #98996, #255463, #253948, #152510 ) ) ;
#5741 = AXIS2_PLACEMENT_3D ( 'NONE', #203374, #102964, #142102 ) ;
#5742 = CARTESIAN_POINT ( 'NONE',  ( 21.05000000000000071, 14.88773611405353314, -236.3451124650200370 ) ) ;
#5743 = ORIENTED_EDGE ( 'NONE', *, *, #20973, .T. ) ;
#5744 = DIRECTION ( 'NONE',  ( 0.000000000000000000, -0.7397360091702744889, 0.6728971962616842051 ) ) ;
#5745 = CARTESIAN_POINT ( 'NONE',  ( -21.05000000000000071, 6.257814610492678398, -100.4022097086908047 ) ) ;
#5746 = DIRECTION ( 'NONE',  ( -0.000000000000000000, 1.000000000000000000, 6.982962677686266711E-15 ) ) ;
#5747 = ORIENTED_EDGE ( 'NONE', *, *, #122807, .T. ) ;
#5748 = EDGE_CURVE ( 'NONE', #87766, #92561, #231862, .T. ) ;
#5749 = EDGE_CURVE ( 'NONE', #45962, #165391, #119411, .T. ) ;
#5750 = LINE ( 'NONE', #120613, #173992 ) ;
#5751 = FACE_OUTER_BOUND ( 'NONE', #251156, .T. ) ;
#5752 = CARTESIAN_POINT ( 'NONE',  ( 20.73486653747088582, 7.250000000011182166, -79.65000000000004832 ) ) ;
#5753 = ORIENTED_EDGE ( 'NONE', *, *, #221990, .F. ) ;
#5754 = CARTESIAN_POINT ( 'NONE',  ( -13.77083647240106501, 9.457410930301316299, -152.4999159087463170 ) ) ;
#5756 = ORIENTED_EDGE ( 'NONE', *, *, #127109, .T. ) ;
#5755 = DIRECTION ( 'NONE',  ( 0.000000000000000000, 0.9126074666063771490, 0.4088369013363276627 ) ) ;
#5757 = CARTESIAN_POINT ( 'NONE',  ( -23.25000000000000000, 71.65000000001180069, -81.87310748452433984 ) ) ;
#5758 = CARTESIAN_POINT ( 'NONE',  ( 22.60000000000000142, 76.00000000001213607, -136.5231074845242745 ) ) ;
#5759 = AXIS2_PLACEMENT_3D ( 'NONE', #241292, #245127, #63921 ) ;
#5760 = AXIS2_PLACEMENT_3D ( 'NONE', #10284, #7718, #128943 ) ;
#5761 = VERTEX_POINT ( 'NONE', #95538 ) ;
#5762 = AXIS2_PLACEMENT_3D ( 'NONE', #31364, #249105, #129143 ) ;
#5763 = CARTESIAN_POINT ( 'NONE',  ( 21.04999999999999716, 69.69554417806466518, -170.0020720079842533 ) ) ;
#5764 = DIRECTION ( 'NONE',  ( 1.000000000000000000, 0.000000000000000000, 0.000000000000000000 ) ) ;
#5765 = DIRECTION ( 'NONE',  ( 1.000000000000000000, 0.000000000000000000, 0.000000000000000000 ) ) ;
#5766 = ORIENTED_EDGE ( 'NONE', *, *, #104102, .T. ) ;
#5767 = CARTESIAN_POINT ( 'NONE',  ( 20.05000000000002913, 7.250000000011171508, -143.2500000000000284 ) ) ;
#5768 = ADVANCED_FACE ( 'NONE', ( #210368 ), #21591, .F. ) ;
#5769 = EDGE_CURVE ( 'NONE', #165685, #235545, #23767, .T. ) ;
#5770 = LINE ( 'NONE', #162320, #105725 ) ;
#5771 = VERTEX_POINT ( 'NONE', #130815 ) ;
#5773 = EDGE_CURVE ( 'NONE', #169487, #131901, #227722, .T. ) ;
#5772 = B_SPLINE_CURVE_WITH_KNOTS ( 'NONE', 3,
 ( #142272, #80999, #103132, #39355, #238817, #182709, #24923, #198400, #2750, #121465, #240104, #200967, #161869, #164419, #22356, #138394, #19782, #61459, #99279 ),
 .UNSPECIFIED., .F., .F.,
 ( 4, 3, 3, 3, 3, 3, 4 ),
 ( -2.000416914658901521E-06, 0.000000000000000000, 4.714008503744565809E-05, 9.979203887777271477E-05, 0.0001372215519229478891, 0.0001635031576220937453, 0.0001900083748504128364 ),
 .UNSPECIFIED. ) ;
#5774 = AXIS2_PLACEMENT_3D ( 'NONE', #63187, #142723, #222246 ) ;
#5775 = AXIS2_PLACEMENT_3D ( 'NONE', #53628, #14526, #213987 ) ;
#5776 = AXIS2_PLACEMENT_3D ( 'NONE', #160117, #148227, #105203 ) ;
#5777 = EDGE_LOOP ( 'NONE', ( #43621, #52826, #235891, #20818 ) ) ;
#5778 = CARTESIAN_POINT ( 'NONE',  ( -18.50000000000000000, 1.115600667400684642E-11, -134.0000000000000284 ) ) ;
#5779 = AXIS2_PLACEMENT_3D ( 'NONE', #226845, #9087, #49499 ) ;
#5780 = ORIENTED_EDGE ( 'NONE', *, *, #101632, .F. ) ;
#5781 = CARTESIAN_POINT ( 'NONE',  ( 18.57399277249656322, 10.33112638555854268, -39.09012289269746532 ) ) ;
#5782 = CARTESIAN_POINT ( 'NONE',  ( -16.81744102076748959, 9.950000000011138823, -154.8500000000000227 ) ) ;
#5784 = ORIENTED_EDGE ( 'NONE', *, *, #101625, .T. ) ;
#5783 = CARTESIAN_POINT ( 'NONE',  ( -23.15000000000000213, 59.16775194334852728, -221.0793150863668473 ) ) ;
#5785 = CARTESIAN_POINT ( 'NONE',  ( 18.54999999999999716, 67.25000000001149658, -48.67310748452438673 ) ) ;
#5786 = CARTESIAN_POINT ( 'NONE',  ( 20.95512820512820440, 10.62384868372303615, -88.25000000000005684 ) ) ;
#5787 = CARTESIAN_POINT ( 'NONE',  ( 20.09999999999999787, 66.25000000001259082, -182.6731074845244223 ) ) ;
#5788 = DIRECTION ( 'NONE',  ( 1.000000000000000000, 0.000000000000000000, 0.000000000000000000 ) ) ;
#5789 = LINE ( 'NONE', #211742, #239282 ) ;
#5790 = CARTESIAN_POINT ( 'NONE',  ( 22.60000000000000142, 31.76322370622491320, -238.8696546380523671 ) ) ;
#5791 = VECTOR ( 'NONE', #160905, 1000.000000000000000 ) ;
#5792 = EDGE_CURVE ( 'NONE', #223717, #120532, #19467, .T. ) ;
#5793 = FACE_OUTER_BOUND ( 'NONE', #103559, .T. ) ;
#5794 = AXIS2_PLACEMENT_3D ( 'NONE', #133231, #58478, #216281 ) ;
#5795 = FACE_OUTER_BOUND ( 'NONE', #237734, .T. ) ;
#5797 = EDGE_LOOP ( 'NONE', ( #16794, #21298, #95358, #113360 ) ) ;
#5796 = CARTESIAN_POINT ( 'NONE',  ( -20.85000000000000142, 76.32388570108278714, -170.0655178952103768 ) ) ;
#5799 = DIRECTION ( 'NONE',  ( 0.000000000000000000, 0.000000000000000000, -1.000000000000000000 ) ) ;
#5798 = AXIS2_PLACEMENT_3D ( 'NONE', #147551, #105827, #48441 ) ;
#5800 = ORIENTED_EDGE ( 'NONE', *, *, #205657, .F. ) ;
#5801 = EDGE_CURVE ( 'NONE', #109224, #231948, #229923, .T. ) ;
#5802 = DIRECTION ( 'NONE',  ( 1.000000000000000000, 0.000000000000000000, 0.000000000000000000 ) ) ;
#5803 = CIRCLE ( 'NONE', #172468, 4.100000000000006750 ) ;
#5805 = EDGE_CURVE ( 'NONE', #221522, #152534, #94250, .T. ) ;
#5804 = CARTESIAN_POINT ( 'NONE',  ( -18.59999999999999787, 74.83729825007431202, -162.0231074845243597 ) ) ;
#5806 = VECTOR ( 'NONE', #156639, 1000.000000000000114 ) ;
#5807 = CARTESIAN_POINT ( 'NONE',  ( 22.49999999999999645, 11.64976291804307884, -66.91119002361310208 ) ) ;
#5808 = EDGE_CURVE ( 'NONE', #242911, #151077, #68597, .T. ) ;
#5809 = CARTESIAN_POINT ( 'NONE',  ( 20.77766267348356166, 65.55095760939391880, -195.9303985686467513 ) ) ;
#5810 = DIRECTION ( 'NONE',  ( -1.000000000000000000, 0.000000000000000000, 0.000000000000000000 ) ) ;
#5811 = AXIS2_PLACEMENT_3D ( 'NONE', #13241, #193159, #54900 ) ;
#5812 = EDGE_CURVE ( 'NONE', #155056, #32241, #211000, .T. ) ;
#5814 = VERTEX_POINT ( 'NONE', #166973 ) ;
#5813 = AXIS2_PLACEMENT_3D ( 'NONE', #1619, #57740, #19931 ) ;
#5816 = CIRCLE ( 'NONE', #205744, 0.09999999999999939493 ) ;
#5815 = CARTESIAN_POINT ( 'NONE',  ( -21.14999999999999858, 56.01362831242966678, -232.7091905853083347 ) ) ;
#5817 = FACE_OUTER_BOUND ( 'NONE', #229242, .T. ) ;
#5818 = EDGE_LOOP ( 'NONE', ( #54429, #182624, #172408, #107111 ) ) ;
#5820 = EDGE_CURVE ( 'NONE', #30385, #143067, #206060, .T. ) ;
#5819 = CARTESIAN_POINT ( 'NONE',  ( 21.05000000000000071, 76.09999993531981488, -210.0011857056192071 ) ) ;
#5821 = ADVANCED_FACE ( 'NONE', ( #49555 ), #245194, .T. ) ;
#5822 = CARTESIAN_POINT ( 'NONE',  ( -23.25000000000000000, 1.910280373842936141, -180.1313678551989028 ) ) ;
#5823 = ORIENTED_EDGE ( 'NONE', *, *, #102453, .T. ) ;
#5824 = CARTESIAN_POINT ( 'NONE',  ( 20.99999999999999645, 61.13238474529445909, -221.0940783352693586 ) ) ;
#5825 = ORIENTED_EDGE ( 'NONE', *, *, #188834, .T. ) ;
#5826 = EDGE_CURVE ( 'NONE', #47156, #195886, #250319, .T. ) ;
#5827 = CARTESIAN_POINT ( 'NONE',  ( -21.59142135623730852, 68.15000000001205649, -124.2731074845243597 ) ) ;
#5828 = EDGE_LOOP ( 'NONE', ( #85955, #132514, #152160, #122344 ) ) ;
#5829 = DIRECTION ( 'NONE',  ( 0.000000000000000000, 0.000000000000000000, -1.000000000000000000 ) ) ;
#5830 = AXIS2_PLACEMENT_3D ( 'NONE', #96527, #176117, #157857 ) ;
#5831 = CARTESIAN_POINT ( 'NONE',  ( 13.88302573338719093, 9.457410944778567696, -182.5000839737900549 ) ) ;
#5832 = ORIENTED_EDGE ( 'NONE', *, *, #223359, .T. ) ;
#5833 = AXIS2_PLACEMENT_3D ( 'NONE', #21551, #101019, #180617 ) ;
#5834 = CARTESIAN_POINT ( 'NONE',  ( 11.60000000000000142, -8.350000000000004974, 10.95857864376269575 ) ) ;
#5836 = ORIENTED_EDGE ( 'NONE', *, *, #184423, .T. ) ;
#5835 = CARTESIAN_POINT ( 'NONE',  ( 12.25000000000000355, 9.350000000011142731, -50.02151937182512142 ) ) ;
#5837 = AXIS2_PLACEMENT_3D ( 'NONE', #3540, #257818, #144314 ) ;
#5838 = ADVANCED_FACE ( 'NONE', ( #230777 ), #190369, .F. ) ;
#5839 = CARTESIAN_POINT ( 'NONE',  ( -22.59999970745345976, 76.00935637734023942, -215.2736206921935889 ) ) ;
#5840 = ADVANCED_FACE ( 'NONE', ( #229483 ), #186506, .F. ) ;
#5841 = EDGE_LOOP ( 'NONE', ( #6235, #137887, #13606, #71947 ) ) ;
#5842 = CIRCLE ( 'NONE', #135014, 0.3999999999999994671 ) ;
#5843 = EDGE_CURVE ( 'NONE', #214983, #50484, #202785, .T. ) ;
#5844 = AXIS2_PLACEMENT_3D ( 'NONE', #92228, #51805, #130070 ) ;
#5845 = ORIENTED_EDGE ( 'NONE', *, *, #247835, .T. ) ;
#5846 = FACE_OUTER_BOUND ( 'NONE', #240759, .T. ) ;
#5847 = DIRECTION ( 'NONE',  ( -1.000000000000000000, 0.000000000000000000, 0.000000000000000000 ) ) ;
#5849 = EDGE_CURVE ( 'NONE', #220874, #255276, #171161, .T. ) ;
#5848 = DIRECTION ( 'NONE',  ( 0.000000000000000000, 0.4999999999999966693, -0.8660254037844405950 ) ) ;
#5850 = VECTOR ( 'NONE', #8636, 1000.000000000000000 ) ;
#5851 = FACE_OUTER_BOUND ( 'NONE', #133371, .T. ) ;
#5852 = CARTESIAN_POINT ( 'NONE',  ( 21.14999999999999858, -11.74999999998884448, -179.7499999999999716 ) ) ;
#5853 = EDGE_CURVE ( 'NONE', #130606, #231975, #161109, .T. ) ;
#5854 = LINE ( 'NONE', #7143, #179632 ) ;
#5855 = AXIS2_PLACEMENT_3D ( 'NONE', #225282, #144464, #10117 ) ;
#5856 = ORIENTED_EDGE ( 'NONE', *, *, #86765, .F. ) ;
#5857 = DIRECTION ( 'NONE',  ( -1.000000000000000000, 0.000000000000000000, -0.000000000000000000 ) ) ;
#5858 = CIRCLE ( 'NONE', #30852, 0.09999999999999939493 ) ;
#5859 = DIRECTION ( 'NONE',  ( 4.408576920032447355E-17, -0.1290532225515392817, -0.9916376685811522096 ) ) ;
#5860 = CARTESIAN_POINT ( 'NONE',  ( -21.14999999999999858, 34.07612324756792077, -243.5412266404783566 ) ) ;
#5862 = DIRECTION ( 'NONE',  ( -1.000000000000000000, 0.000000000000000000, 0.000000000000000000 ) ) ;
#5861 = AXIS2_PLACEMENT_3D ( 'NONE', #33591, #251289, #72697 ) ;
#5863 = VERTEX_POINT ( 'NONE', #52100 ) ;
#5864 = CARTESIAN_POINT ( 'NONE',  ( 20.94999999999999929, 68.00417547777207972, -224.2303273613012493 ) ) ;
#5865 = ORIENTED_EDGE ( 'NONE', *, *, #220751, .T. ) ;
#5867 = ORIENTED_EDGE ( 'NONE', *, *, #104362, .T. ) ;
#5866 = AXIS2_PLACEMENT_3D ( 'NONE', #24498, #103982, #227801 ) ;
#5868 = DIRECTION ( 'NONE',  ( 0.000000000000000000, 0.000000000000000000, 1.000000000000000000 ) ) ;
#5869 = DIRECTION ( 'NONE',  ( 0.000000000000000000, -6.938893903907222067E-15, 1.000000000000000000 ) ) ;
#5870 = ORIENTED_EDGE ( 'NONE', *, *, #192865, .T. ) ;
#5872 = EDGE_LOOP ( 'NONE', ( #232333, #241894, #46898, #25422 ) ) ;
#5871 = CARTESIAN_POINT ( 'NONE',  ( 20.85000000000000142, 86.55507603484990398, -209.4941099044519319 ) ) ;
#5873 = EDGE_CURVE ( 'NONE', #84325, #105422, #111038, .T. ) ;
#5874 = CARTESIAN_POINT ( 'NONE',  ( -5.899999999999938183, 64.65000000001120384, -22.12310748452479103 ) ) ;
#5875 = VERTEX_POINT ( 'NONE', #149959 ) ;
#5876 = AXIS2_PLACEMENT_3D ( 'NONE', #111557, #192376, #224112 ) ;
#5877 = CARTESIAN_POINT ( 'NONE',  ( -22.43310005002225438, 0.005636942152031573783, -21.85033787286560525 ) ) ;
#5878 = CARTESIAN_POINT ( 'NONE',  ( 23.24999999999999645, 5.599999999999996980, -12.40526601891309788 ) ) ;
#5880 = ORIENTED_EDGE ( 'NONE', *, *, #20517, .F. ) ;
#5879 = ADVANCED_FACE ( 'NONE', ( #69140 ), #48670, .F. ) ;
#5881 = AXIS2_PLACEMENT_3D ( 'NONE', #7189, #104978, #240678 ) ;
#5882 = LINE ( 'NONE', #127130, #156042 ) ;
#5883 = DIRECTION ( 'NONE',  ( -1.000000000000000000, 0.000000000000000000, 0.000000000000000000 ) ) ;
#5885 = VERTEX_POINT ( 'NONE', #97634 ) ;
#5884 = AXIS2_PLACEMENT_3D ( 'NONE', #209920, #151229, #31306 ) ;
#5886 = CIRCLE ( 'NONE', #155782, 0.1000000000000028644 ) ;
#5887 = VECTOR ( 'NONE', #138797, 1000.000000000000000 ) ;
#5888 = CARTESIAN_POINT ( 'NONE',  ( -20.94999999999999929, 14.05000000001115623, -72.51369507076104526 ) ) ;
#5889 = ADVANCED_FACE ( 'NONE', ( #135486 ), #195509, .F. ) ;
#5890 =( REPRESENTATION_RELATIONSHIP ('NONE','NONE', #36900, #196772 ) REPRESENTATION_RELATIONSHIP_WITH_TRANSFORMATION ( #68939 )SHAPE_REPRESENTATION_RELATIONSHIP( ) );
#5891 = FACE_OUTER_BOUND ( 'NONE', #211353, .T. ) ;
#5893 = EDGE_LOOP ( 'NONE', ( #147012, #187117, #127902, #186541 ) ) ;
#5892 = DIRECTION ( 'NONE',  ( 1.000000000000000000, 0.000000000000000000, 0.000000000000000000 ) ) ;
#5894 = CARTESIAN_POINT ( 'NONE',  ( 21.05000000000000071, 85.00000000001179501, -79.41707660717668205 ) ) ;
#5895 = CARTESIAN_POINT ( 'NONE',  ( -22.49510344025093644, 75.93287232181748436, -81.17307758963858078 ) ) ;
#5896 = DIRECTION ( 'NONE',  ( 0.000000000000000000, -0.07893460099012303277, 0.9968797965484756940 ) ) ;
#5898 = LINE ( 'NONE', #224948, #78373 ) ;
#5897 = CARTESIAN_POINT ( 'NONE',  ( -16.94309007106720344, 66.00777380744186473, -90.41731620196888741 ) ) ;
#5899 = CARTESIAN_POINT ( 'NONE',  ( 20.94999999999999929, 39.29335463311362275, -236.8946393634875278 ) ) ;
#5900 = DIRECTION ( 'NONE',  ( 0.000000000000000000, 0.4999999999999478195, -0.8660254037844686836 ) ) ;
#5901 = CIRCLE ( 'NONE', #97473, 0.1000000000000024342 ) ;
#5902 = EDGE_CURVE ( 'NONE', #88904, #188870, #44410, .T. ) ;
#5903 = CARTESIAN_POINT ( 'NONE',  ( -21.65000000000000213, 7.250000000011138646, -42.75000000000000000 ) ) ;
#5904 = AXIS2_PLACEMENT_3D ( 'NONE', #105179, #107792, #11271 ) ;
#5905 = AXIS2_PLACEMENT_3D ( 'NONE', #63005, #180402, #223358 ) ;
#5906 = ORIENTED_EDGE ( 'NONE', *, *, #51001, .F. ) ;
#5907 = ORIENTED_EDGE ( 'NONE', *, *, #56458, .T. ) ;
#5908 = CARTESIAN_POINT ( 'NONE',  ( 23.14999999999999858, 76.00000000001188027, -99.02310748452428868 ) ) ;
#5909 =( BOUNDED_SURFACE ( )  B_SPLINE_SURFACE ( 3, 2, ( 
 ( #223577, #222277, #99769 ),
 ( #80197, #180625, #98466 ),
 ( #44966, #43682, #1961 ),
 ( #161068, #221013, #103622 ),
 ( #201455, #22858, #244436 ),
 ( #146601, #104891, #249593 ),
 ( #226128, #125769, #9678 ),
 ( #230013, #184462, #224863 ),
 ( #85338, #168809, #164908 ),
 ( #5809, #65803, #185756 ),
 ( #8411, #26706, #89212 ),
 ( #245733, #145333, #86622 ) ),
 .UNSPECIFIED., .F., .F., .F. ) 
 B_SPLINE_SURFACE_WITH_KNOTS ( ( 4, 2, 2, 2, 2, 4 ),
 ( 3, 3 ),
 ( 3.174653483277205090, 3.943930578431714018, 4.713207673586222946, 5.482484768740731873, 5.867123316317986337, 6.251761863895240801 ),
 ( 0.000000000000000000, 1.000000000000000000 ),
 .UNSPECIFIED. ) 
 GEOMETRIC_REPRESENTATION_ITEM ( )  RATIONAL_B_SPLINE_SURFACE ( (
 ( 1.000000000000000000, 0.8659465255642114778, 1.000000000000000000),
 ( 1.000000000000000000, 0.8648614068487343598, 1.000000000000000000),
 ( 1.000000000000000000, 0.8489031841324523597, 1.000000000000000000),
 ( 1.000000000000000000, 0.7927507630160768315, 1.000000000000000000),
 ( 1.000000000000000000, 0.7523013859006951742, 1.000000000000000000),
 ( 1.000000000000000000, 0.6616226951198839190, 1.000000000000000000),
 ( 1.000000000000000000, 0.6112214368721479163, 1.000000000000000000),
 ( 1.000000000000000000, 0.5507684314500016498, 1.000000000000000000),
 ( 1.000000000000000000, 0.5333267243152196579, 1.000000000000000000),
 ( 1.000000000000000000, 0.5084565446481067452, 1.000000000000000000),
 ( 1.000000000000000000, 0.5010722703449013160, 1.000000000000000000),
 ( 1.000000000000000000, 0.5001234037138888588, 1.000000000000000000) ) ) 
 REPRESENTATION_ITEM ( '' )  SURFACE ( )  );
#5910 = ORIENTED_EDGE ( 'NONE', *, *, #3429, .F. ) ;
#5911 = FACE_OUTER_BOUND ( 'NONE', #43050, .T. ) ;
#5912 = ORIENTED_EDGE ( 'NONE', *, *, #141759, .T. ) ;
#5913 = CARTESIAN_POINT ( 'NONE',  ( -21.05000000000000071, -1.835341550213255957, -45.05515129256298223 ) ) ;
#5914 = ORIENTED_EDGE ( 'NONE', *, *, #18329, .F. ) ;
#5915 = FACE_OUTER_BOUND ( 'NONE', #191720, .T. ) ;
#5916 = ORIENTED_EDGE ( 'NONE', *, *, #213904, .T. ) ;
#5917 = ORIENTED_EDGE ( 'NONE', *, *, #233349, .T. ) ;
#5918 = CARTESIAN_POINT ( 'NONE',  ( 20.04142135623731136, 54.45778349825307885, -228.7022971282791843 ) ) ;
#5919 = CIRCLE ( 'NONE', #118588, 3.899999999999987033 ) ;
#5920 = DIRECTION ( 'NONE',  ( -1.000000000000000000, -7.304098846218133681E-16, 4.217023435051677994E-16 ) ) ;
#5922 = ORIENTED_EDGE ( 'NONE', *, *, #28924, .T. ) ;
#5921 = FACE_OUTER_BOUND ( 'NONE', #110133, .T. ) ;
#5923 = CARTESIAN_POINT ( 'NONE',  ( 20.89878130938411616, 65.67252876774529113, -97.44570419949944551 ) ) ;
#5925 = VERTEX_POINT ( 'NONE', #136778 ) ;
#5924 = DIRECTION ( 'NONE',  ( 1.186688945009010077E-16, 0.4088369013363281068, -0.9126074666063770380 ) ) ;
#5926 = FACE_OUTER_BOUND ( 'NONE', #220597, .T. ) ;
#5927 = CARTESIAN_POINT ( 'NONE',  ( 21.00000000000000000, 9.750000000011153745, -146.3500000000000227 ) ) ;
#5929 = ORIENTED_EDGE ( 'NONE', *, *, #20813, .F. ) ;
#5928 = CYLINDRICAL_SURFACE ( 'NONE', #160450, 0.1000000000000055844 ) ;
#5930 = DIRECTION ( 'NONE',  ( -1.000000000000000000, -7.304098846218134667E-16, 0.000000000000000000 ) ) ;
#5931 = CARTESIAN_POINT ( 'NONE',  ( -15.75000000000000355, 26.30888228346803004, -233.3999513616626587 ) ) ;
#5932 = ADVANCED_FACE ( 'NONE', ( #55943 ), #75561, .F. ) ;
#5933 = CARTESIAN_POINT ( 'NONE',  ( -16.89020380669786192, 9.950000000011137047, -113.2574111481105916 ) ) ;
#5934 = ORIENTED_EDGE ( 'NONE', *, *, #123495, .T. ) ;
#5936 = LINE ( 'NONE', #162487, #220593 ) ;
#5935 = DIRECTION ( 'NONE',  ( 0.000000000000000000, 0.000000000000000000, -1.000000000000000000 ) ) ;
#5937 = CARTESIAN_POINT ( 'NONE',  ( 18.58143601961936042, 10.43572941510541519, -91.75000000000005684 ) ) ;
#5938 = TOROIDAL_SURFACE ( 'NONE', #47632, 0.2000000000000000111, 0.1000000000000000056 ) ;
#5939 = CARTESIAN_POINT ( 'NONE',  ( 20.95512820512820440, 65.37615131630040821, -157.8229454651000481 ) ) ;
#5940 = AXIS2_PLACEMENT_3D ( 'NONE', #35010, #75408, #79205 ) ;
#5941 = CARTESIAN_POINT ( 'NONE',  ( -20.94999999999999929, 0.5663372425336981042, -209.0641885820623997 ) ) ;
#5942 = CARTESIAN_POINT ( 'NONE',  ( 18.49999999999999289, 65.75000000001223555, -148.6731074845244223 ) ) ;
#5943 = ORIENTED_EDGE ( 'NONE', *, *, #46844, .T. ) ;
#5945 = ORIENTED_EDGE ( 'NONE', *, *, #220027, .F. ) ;
#5944 = TOROIDAL_SURFACE ( 'NONE', #147448, 0.6000000000000004219, 0.1000000000000000056 ) ;
#5946 = ORIENTED_EDGE ( 'NONE', *, *, #48496, .F. ) ;
#5947 = AXIS2_PLACEMENT_3D ( 'NONE', #243603, #7560, #224027 ) ;
#5948 = CARTESIAN_POINT ( 'NONE',  ( 11.60000000000006182, 66.35000000001119247, -18.42310748452479530 ) ) ;
#5949 = EDGE_LOOP ( 'NONE', ( #245874, #16097, #62746, #24845 ) ) ;
#5950 = LINE ( 'NONE', #201602, #14273 ) ;
#5951 = ORIENTED_EDGE ( 'NONE', *, *, #74570, .F. ) ;
#5952 = ADVANCED_FACE ( 'NONE', ( #234602 ), #190161, .T. ) ;
#5953 = CARTESIAN_POINT ( 'NONE',  ( -21.00023020733437562, 6.390869245278860689, -100.5000000000000426 ) ) ;
#5954 = CARTESIAN_POINT ( 'NONE',  ( -16.94107738177414291, 14.24304960796391661, -219.3391119284832484 ) ) ;
#5955 = EDGE_CURVE ( 'NONE', #33564, #163131, #115226, .T. ) ;
#5956 = EDGE_LOOP ( 'NONE', ( #13408, #181635, #113316, #249009 ) ) ;
#5957 = AXIS2_PLACEMENT_3D ( 'NONE', #230984, #186715, #206266 ) ;
#5958 = CARTESIAN_POINT ( 'NONE',  ( 15.51872946208854920, 9.376580978055097049, -151.6269462470119720 ) ) ;
#5959 = SURFACE_STYLE_USAGE ( .BOTH. , #82919 ) ;
#5960 = EDGE_CURVE ( 'NONE', #62684, #109264, #73642, .T. ) ;
#5961 = CIRCLE ( 'NONE', #151763, 0.09999999999999939493 ) ;
#5962 = ORIENTED_EDGE ( 'NONE', *, *, #10052, .F. ) ;
#5963 = ORIENTED_EDGE ( 'NONE', *, *, #227280, .F. ) ;
#5964 = TOROIDAL_SURFACE ( 'NONE', #18467, 0.4000000000000005773, 0.1000000000000000056 ) ;
#5965 = ORIENTED_EDGE ( 'NONE', *, *, #2964, .F. ) ;
#5966 = CIRCLE ( 'NONE', #126795, 0.09999999999999939493 ) ;
#5967 = EDGE_CURVE ( 'NONE', #85621, #150821, #244297, .T. ) ;
#5968 = CARTESIAN_POINT ( 'NONE',  ( -21.05000000000000071, 77.83534155023701828, -191.9679561919613491 ) ) ;
#5969 = LINE ( 'NONE', #183356, #211709 ) ;
#5970 = CARTESIAN_POINT ( 'NONE',  ( 18.59999999999999787, -1.835859311432481045, -145.5044391687985694 ) ) ;
#5971 = AXIS2_PLACEMENT_3D ( 'NONE', #189833, #230237, #11197 ) ;
#5973 = EDGE_CURVE ( 'NONE', #155471, #154908, #136935, .T. ) ;
#5972 = DIRECTION ( 'NONE',  ( 0.000000000000000000, -7.056502275159890832E-15, 1.000000000000000000 ) ) ;
#5974 = CARTESIAN_POINT ( 'NONE',  ( 18.59999999999999076, 74.16465844978765176, -124.8679561919613263 ) ) ;
#5975 = DIRECTION ( 'NONE',  ( 0.000000000000000000, 0.2128009952263568982, -0.9770955615653323934 ) ) ;
#5977 = CYLINDRICAL_SURFACE ( 'NONE', #90984, 0.09999999999999939493 ) ;
#5976 = DIRECTION ( 'NONE',  ( 2.952720810173289112E-16, -1.000000000000000000, 0.000000000000000000 ) ) ;
#5978 = CARTESIAN_POINT ( 'NONE',  ( -18.50000000000000000, 77.68707439010432836, -216.3376804510660065 ) ) ;
#5980 = VERTEX_POINT ( 'NONE', #96357 ) ;
#5979 = CARTESIAN_POINT ( 'NONE',  ( -20.88420186297724612, 10.33025634372637391, -139.5870929282639281 ) ) ;
#5982 = CARTESIAN_POINT ( 'NONE',  ( 21.07971444708685738, 69.67020791838538685, -103.1109309208422502 ) ) ;
#5981 = CARTESIAN_POINT ( 'NONE',  ( -23.15000000000000213, 1.115600667400684642E-11, -198.9999999999999432 ) ) ;
#5983 = EDGE_CURVE ( 'NONE', #141624, #80942, #52749, .T. ) ;
#5984 = CARTESIAN_POINT ( 'NONE',  ( -20.85000000000000142, 10.33248238083634440, -139.5948465439131780 ) ) ;
#5985 = VERTEX_POINT ( 'NONE', #78085 ) ;
#5986 = CYLINDRICAL_SURFACE ( 'NONE', #212989, 4.049999999999998046 ) ;
#5987 = CARTESIAN_POINT ( 'NONE',  ( 20.05000000000002913, 52.72272256579930882, -234.4105091754867658 ) ) ;
#5988 = DIRECTION ( 'NONE',  ( 0.000000000000000000, -6.982962677686266711E-15, 1.000000000000000000 ) ) ;
#5989 = AXIS2_PLACEMENT_3D ( 'NONE', #157843, #198201, #58671 ) ;
#5990 = ORIENTED_EDGE ( 'NONE', *, *, #196107, .F. ) ;
#5991 = AXIS2_PLACEMENT_3D ( 'NONE', #4510, #204003, #64503 ) ;
#5992 = ADVANCED_FACE ( 'NONE', ( #92517 ), #212494, .F. ) ;
#5993 = CARTESIAN_POINT ( 'NONE',  ( -20.15000000000000568, 9.291421356248463326, -88.15000000000004832 ) ) ;
#5994 = AXIS2_PLACEMENT_3D ( 'NONE', #96587, #176178, #87171 ) ;
#5995 = DIRECTION ( 'NONE',  ( 0.7071067811865463515, -0.7071067811865487940, 0.000000000000000000 ) ) ;
#5996 = DIRECTION ( 'NONE',  ( 0.000000000000000000, -7.056502275159890043E-15, 1.000000000000000000 ) ) ;
#5997 = VERTEX_POINT ( 'NONE', #76809 ) ;
#5998 = ORIENTED_EDGE ( 'NONE', *, *, #178086, .F. ) ;
#5999 = CARTESIAN_POINT ( 'NONE',  ( -20.85000000000000142, 77.16412189325286874, -61.70825939895269840 ) ) ;
#6000 = ORIENTED_EDGE ( 'NONE', *, *, #134569, .F. ) ;
#6001 = CARTESIAN_POINT ( 'NONE',  ( 21.00000000000000000, 6.726092018229619995, 9.512212474619552438 ) ) ;
#6002 = DIRECTION ( 'NONE',  ( 1.000000000000000000, -0.000000000000000000, -0.000000000000000000 ) ) ;
#6003 = FACE_OUTER_BOUND ( 'NONE', #87757, .T. ) ;
#6004 = DIRECTION ( 'NONE',  ( 1.000000000000000000, 0.000000000000000000, 0.000000000000000000 ) ) ;
#6005 = ORIENTED_EDGE ( 'NONE', *, *, #14562, .F. ) ;
#6006 = CIRCLE ( 'NONE', #155889, 4.049999999999998046 ) ;
#6007 = AXIS2_PLACEMENT_3D ( 'NONE', #40490, #136975, #58704 ) ;
#6008 = EDGE_CURVE ( 'NONE', #78597, #149927, #157685, .T. ) ;
#6009 = VECTOR ( 'NONE', #98401, 1000.000000000000000 ) ;
#6010 = CARTESIAN_POINT ( 'NONE',  ( 21.97500000000000497, 63.38346053167636995, -212.7939182281409956 ) ) ;
#6011 = DIRECTION ( 'NONE',  ( -1.000000000000000000, 0.000000000000000000, 0.000000000000000000 ) ) ;
#6012 = CARTESIAN_POINT ( 'NONE',  ( -17.01473183483379614, 63.05955705323258798, -213.2241350765465882 ) ) ;
#6013 = DIRECTION ( 'NONE',  ( 0.000000000000000000, 1.000000000000000000, 7.116814260417668513E-15 ) ) ;
#6014 = ORIENTED_EDGE ( 'NONE', *, *, #146369, .F. ) ;
#6015 = DIRECTION ( 'NONE',  ( 0.000000000000000000, -0.8660254037844387076, 0.4999999999999998335 ) ) ;
#6016 =( BOUNDED_CURVE ( )  B_SPLINE_CURVE ( 3, ( #39404, #195897, #154234, #57633 ),
 .UNSPECIFIED., .F., .F. ) 
 B_SPLINE_CURVE_WITH_KNOTS ( ( 4, 4 ),
 ( 3.192897208853993085, 4.712388980384689674 ),
 .UNSPECIFIED. ) 
 CURVE ( )  GEOMETRIC_REPRESENTATION_ITEM ( )  RATIONAL_B_SPLINE_CURVE ( ( 1.000000000000000000, 0.8166740347213228279, 0.8166740347213228279, 1.000000000000000000 ) ) 
 REPRESENTATION_ITEM ( '' )  );
#6017 = EDGE_CURVE ( 'NONE', #51884, #83940, #56090, .T. ) ;
#6019 = ORIENTED_EDGE ( 'NONE', *, *, #64587, .T. ) ;
#6018 = DIRECTION ( 'NONE',  ( 0.000000000000000000, 0.000000000000000000, 1.000000000000000000 ) ) ;
#6020 = CARTESIAN_POINT ( 'NONE',  ( 18.54999999999999716, 52.34166666667851331, -86.27310748452447342 ) ) ;
#6021 = CARTESIAN_POINT ( 'NONE',  ( 18.49351773456764292, 78.22584867798236985, -231.3920583907407718 ) ) ;
#6022 = CARTESIAN_POINT ( 'NONE',  ( 20.94999999999997442, 79.28756800457986742, -196.2274082906208434 ) ) ;
#6023 = DIRECTION ( 'NONE',  ( -4.408576920032448588E-17, -0.9594490217226103734, -0.2818822000686205254 ) ) ;
#6024 = CARTESIAN_POINT ( 'NONE',  ( -20.64999999999999858, 1.115600667400684642E-11, -67.00000000000004263 ) ) ;
#6025 = DIRECTION ( 'NONE',  ( 0.000000000000000000, 0.000000000000000000, -1.000000000000000000 ) ) ;
#6026 = VERTEX_POINT ( 'NONE', #174688 ) ;
#6027 = DIRECTION ( 'NONE',  ( -1.000000000000000000, 0.000000000000000000, 0.000000000000000000 ) ) ;
#6028 = AXIS2_PLACEMENT_3D ( 'NONE', #127679, #32457, #111975 ) ;
#6029 = CARTESIAN_POINT ( 'NONE',  ( 21.97500000000000497, 9.749999999999998224, -21.25000000000000000 ) ) ;
#6031 = AXIS2_PLACEMENT_3D ( 'NONE', #77027, #156615, #236108 ) ;
#6030 = FACE_OUTER_BOUND ( 'NONE', #166234, .T. ) ;
#6032 = VECTOR ( 'NONE', #33427, 1000.000000000000000 ) ;
#6033 = DIRECTION ( 'NONE',  ( 1.000000000000000000, 0.000000000000000000, 0.000000000000000000 ) ) ;
#6034 = DIRECTION ( 'NONE',  ( 1.000000000000000000, 0.000000000000000000, 0.000000000000000000 ) ) ;
#6035 = EDGE_CURVE ( 'NONE', #42531, #162376, #254152, .T. ) ;
#6036 = ORIENTED_EDGE ( 'NONE', *, *, #19436, .T. ) ;
#6037 = EDGE_LOOP ( 'NONE', ( #250271, #144712, #218739, #5711 ) ) ;
#6038 = AXIS2_PLACEMENT_3D ( 'NONE', #69690, #202757, #107504 ) ;
#6039 = CYLINDRICAL_SURFACE ( 'NONE', #138402, 0.09999999999998898659 ) ;
#6040 = DIRECTION ( 'NONE',  ( 1.000000000000000000, 0.000000000000000000, 0.000000000000000000 ) ) ;
#6041 = CIRCLE ( 'NONE', #31038, 0.1000000000000055844 ) ;
#6042 = CARTESIAN_POINT ( 'NONE',  ( 20.99551997958289107, 17.15237243733800554, -224.5408061578818888 ) ) ;
#6043 = EDGE_CURVE ( 'NONE', #244261, #167528, #106925, .T. ) ;
#6044 = CARTESIAN_POINT ( 'NONE',  ( -21.65000000000000213, 66.05000000001157900, -56.77310748452439526 ) ) ;
#6045 = VECTOR ( 'NONE', #249518, 1000.000000000000000 ) ;
#6046 = B_SPLINE_CURVE_WITH_KNOTS ( 'NONE', 3,
 ( #52130, #88677, #9171, #146104, #7908, #211220, #87408, #112145, #108281, #191697 ),
 .UNSPECIFIED., .F., .F.,
 ( 4, 2, 2, 2, 4 ),
 ( 0.000000000000000000, 0.0001584437871625804257, 0.0002376656807438308212, 0.0002772766275344220699, 0.0003168875743250132914 ),
 .UNSPECIFIED. ) ;
#6048 = TOROIDAL_SURFACE ( 'NONE', #39418, 12.97499999999999787, 0.1000000000000000056 ) ;
#6047 = FACE_OUTER_BOUND ( 'NONE', #104293, .T. ) ;
#6049 = ADVANCED_FACE ( 'NONE', ( #20713 ), #161507, .F. ) ;
#6051 = ADVANCED_FACE ( 'NONE', ( #1100 ), #83198, .T. ) ;
#6050 = LINE ( 'NONE', #105119, #217304 ) ;
#6052 = AXIS2_PLACEMENT_3D ( 'NONE', #128601, #209409, #126016 ) ;
#6053 = CIRCLE ( 'NONE', #143438, 0.1000000000000028644 ) ;
#6054 = CARTESIAN_POINT ( 'NONE',  ( -20.96428641294375339, 17.15731666422713531, -224.5635080354877857 ) ) ;
#6055 = VERTEX_POINT ( 'NONE', #79363 ) ;
#6056 = DIRECTION ( 'NONE',  ( 0.000000000000000000, -6.240597636138643358E-14, -1.000000000000000000 ) ) ;
#6057 = EDGE_CURVE ( 'NONE', #196694, #210729, #183625, .T. ) ;
#6058 = ORIENTED_EDGE ( 'NONE', *, *, #149060, .F. ) ;
#6059 = CARTESIAN_POINT ( 'NONE',  ( -21.04999999999999716, 75.98514436511781867, -75.86746652656786694 ) ) ;
#6060 = DIRECTION ( 'NONE',  ( 3.469446951953515108E-14, 0.000000000000000000, 1.000000000000000000 ) ) ;
#6062 = AXIS2_PLACEMENT_3D ( 'NONE', #232507, #73439, #108683 ) ;
#6061 = CYLINDRICAL_SURFACE ( 'NONE', #220171, 11.80000000000000959 ) ;
#6063 = CARTESIAN_POINT ( 'NONE',  ( 23.14999999999999858, 71.22429906543263201, -124.6743393804783722 ) ) ;
#6064 = CARTESIAN_POINT ( 'NONE',  ( -23.15000000000000213, 4.250000000000000000, -12.25000000000000000 ) ) ;
#6065 = DIRECTION ( 'NONE',  ( -0.000000000000000000, 0.000000000000000000, -1.000000000000000000 ) ) ;
#6066 = CARTESIAN_POINT ( 'NONE',  ( -18.52186455168988388, -9.481018481442522017, -7.025016477914483914 ) ) ;
#6067 = CARTESIAN_POINT ( 'NONE',  ( 18.49999999999999289, 11.65000000001115943, -158.8500000000000227 ) ) ;
#6068 = CARTESIAN_POINT ( 'NONE',  ( -21.14999999999999858, 76.00000000001217870, -142.7816861282870207 ) ) ;
#6069 = AXIS2_PLACEMENT_3D ( 'NONE', #214392, #77426, #59133 ) ;
#6070 = FACE_OUTER_BOUND ( 'NONE', #190652, .T. ) ;
#6071 = CARTESIAN_POINT ( 'NONE',  ( -21.65000000000000213, 68.75000000001261924, -190.8731074845244109 ) ) ;
#6072 = FACE_OUTER_BOUND ( 'NONE', #149636, .T. ) ;
#6073 = VECTOR ( 'NONE', #209597, 1000.000000000000000 ) ;
#6074 = LINE ( 'NONE', #4775, #45466 ) ;
#6075 = CARTESIAN_POINT ( 'NONE',  ( -23.15000000000000213, 87.75000000001143974, -39.12310748452424747 ) ) ;
#6076 = CIRCLE ( 'NONE', #151868, 2.000000000000002665 ) ;
#6077 = AXIS2_PLACEMENT_3D ( 'NONE', #129564, #249515, #126983 ) ;
#6078 = VERTEX_POINT ( 'NONE', #203174 ) ;
#6079 = CARTESIAN_POINT ( 'NONE',  ( -23.25000000000000000, -0.09999999999999939493, 11.64957080754479968 ) ) ;
#6080 = DIRECTION ( 'NONE',  ( -1.000000000000000000, -0.000000000000000000, 0.000000000000000000 ) ) ;
#6081 = ADVANCED_FACE ( 'NONE', ( #19418 ), #215276, .F. ) ;
#6082 = EDGE_CURVE ( 'NONE', #57757, #57263, #165395, .T. ) ;
#6083 = ORIENTED_EDGE ( 'NONE', *, *, #255835, .T. ) ;
#6084 = DIRECTION ( 'NONE',  ( 0.000000000000000000, 1.000000000000000000, 0.000000000000000000 ) ) ;
#6085 = FACE_OUTER_BOUND ( 'NONE', #111620, .T. ) ;
#6086 = CARTESIAN_POINT ( 'NONE',  ( -23.25000000000000000, 87.65000000001214175, -136.5231074845242176 ) ) ;
#6087 = ORIENTED_EDGE ( 'NONE', *, *, #186968, .T. ) ;
#6088 = DIRECTION ( 'NONE',  ( -1.000000000000000000, -1.646408749285562691E-14, 1.073024830501117725E-15 ) ) ;
#6089 = DIRECTION ( 'NONE',  ( 0.000000000000000000, 0.9651348961777428404, -0.2617529984164035373 ) ) ;
#6090 = ADVANCED_FACE ( 'NONE', ( #201900 ), #84464, .F. ) ;
#6091 = EDGE_LOOP ( 'NONE', ( #38102, #245791, #227864, #8365 ) ) ;
#6092 = CARTESIAN_POINT ( 'NONE',  ( -23.15000000000000213, 1.115648428625851357E-11, -197.0999999999999659 ) ) ;
#6093 = AXIS2_PLACEMENT_3D ( 'NONE', #129224, #146201, #70562 ) ;
#6094 = ORIENTED_EDGE ( 'NONE', *, *, #145945, .F. ) ;
#6095 = CARTESIAN_POINT ( 'NONE',  ( 18.49999999999998934, 6.650000000011155876, -146.3500000000000227 ) ) ;
#6096 = CARTESIAN_POINT ( 'NONE',  ( 22.49999999999999645, 0.1000000000111554016, -21.85042919245519855 ) ) ;
#6097 = DIRECTION ( 'NONE',  ( 1.000000000000000000, 0.000000000000000000, 0.000000000000000000 ) ) ;
#6099 = CARTESIAN_POINT ( 'NONE',  ( 23.14999999999999503, 64.01960172407876826, -222.2915665888316141 ) ) ;
#6098 = UNCERTAINTY_MEASURE_WITH_UNIT (LENGTH_MEASURE( 1.000000000000000082E-05 ), #35512, 'distance_accuracy_value', 'NONE');
#6100 = CARTESIAN_POINT ( 'NONE',  ( -18.79999999999999716, 3.362550747017869490, 28.82623795144604983 ) ) ;
#6101 = CARTESIAN_POINT ( 'NONE',  ( -20.65000000000000568, 67.23581240663841641, -214.2531594801197627 ) ) ;
#6102 = CARTESIAN_POINT ( 'NONE',  ( 20.95000000000005969, 61.72892516158560028, -36.56695479651062897 ) ) ;
#6103 = DIRECTION ( 'NONE',  ( 0.000000000000000000, 0.000000000000000000, -1.000000000000000000 ) ) ;
#6104 = DIRECTION ( 'NONE',  ( 1.000000000000000000, 0.000000000000000000, 0.000000000000000000 ) ) ;
#6106 = VERTEX_POINT ( 'NONE', #59789 ) ;
#6105 = CARTESIAN_POINT ( 'NONE',  ( 18.47135592147650485, 86.89032914117082385, -199.5516226189558040 ) ) ;
#6107 = EDGE_LOOP ( 'NONE', ( #243201, #94752, #10728, #168857, #239938, #179576, #127777, #247988, #21830, #12390 ) ) ;
#6109 = DIRECTION ( 'NONE',  ( -2.952720810173289112E-16, 1.000000000000000000, 0.000000000000000000 ) ) ;
#6108 = LINE ( 'NONE', #225148, #116295 ) ;
#6111 = ORIENTED_EDGE ( 'NONE', *, *, #170334, .F. ) ;
#6110 = FACE_OUTER_BOUND ( 'NONE', #203931, .T. ) ;
#6112 = ADVANCED_FACE ( 'NONE', ( #23290 ), #40295, .T. ) ;
#6113 = ORIENTED_EDGE ( 'NONE', *, *, #148023, .T. ) ;
#6114 = LINE ( 'NONE', #47802, #12499 ) ;
#6115 = CARTESIAN_POINT ( 'NONE',  ( 20.30531438145591139, 10.09690106110208596, -175.2960178072733015 ) ) ;
#6116 = CIRCLE ( 'NONE', #247737, 0.1000000000000024342 ) ;
#6117 = CARTESIAN_POINT ( 'NONE',  ( -20.85000000000000142, 10.33248238083634440, -173.0948465439131496 ) ) ;
#6118 = EDGE_CURVE ( 'NONE', #156136, #177284, #7141, .T. ) ;
#6119 = DIRECTION ( 'NONE',  ( -2.940209281316621509E-16, 1.000000000000000000, -2.352167425053297207E-15 ) ) ;
#6120 = LINE ( 'NONE', #100076, #98789 ) ;
#6121 = EDGE_CURVE ( 'NONE', #47961, #246321, #58512, .T. ) ;
#6122 = CARTESIAN_POINT ( 'NONE',  ( -18.59999999999999787, 1.835341550224411922, -11.55515129256298046 ) ) ;
#6123 = ORIENTED_EDGE ( 'NONE', *, *, #147088, .T. ) ;
#6124 = EDGE_LOOP ( 'NONE', ( #162563, #54633, #136940, #122280 ) ) ;
#6125 = ADVANCED_FACE ( 'NONE', ( #160234 ), #100197, .T. ) ;
#6126 = DIRECTION ( 'NONE',  ( -0.000000000000000000, 1.000000000000000000, -0.000000000000000000 ) ) ;
#6127 = AXIS2_PLACEMENT_3D ( 'NONE', #129289, #229674, #227086 ) ;
#6128 = ORIENTED_EDGE ( 'NONE', *, *, #53047, .T. ) ;
#6129 = FACE_OUTER_BOUND ( 'NONE', #14252, .T. ) ;
#6130 = ORIENTED_EDGE ( 'NONE', *, *, #191183, .T. ) ;
#6131 = FACE_OUTER_BOUND ( 'NONE', #134886, .T. ) ;
#6132 = AXIS2_PLACEMENT_3D ( 'NONE', #186248, #205796, #5004 ) ;
#6133 = CIRCLE ( 'NONE', #210175, 0.09999999999999939493 ) ;
#6134 = EDGE_CURVE ( 'NONE', #166555, #204034, #173245, .T. ) ;
#6136 = EDGE_CURVE ( 'NONE', #172803, #54825, #119816, .T. ) ;
#6135 = EDGE_CURVE ( 'NONE', #21483, #189415, #86245, .T. ) ;
#6137 = CARTESIAN_POINT ( 'NONE',  ( -20.85000000000000142, 77.16412189325286874, -61.60825939895269698 ) ) ;
#6138 = CARTESIAN_POINT ( 'NONE',  ( -23.15000000000000213, 63.67210543329348837, -237.4495904216901465 ) ) ;
#6139 = CARTESIAN_POINT ( 'NONE',  ( -16.91256925476571027, 22.89123816192538996, -230.8480166193616299 ) ) ;
#6140 = ORIENTED_EDGE ( 'NONE', *, *, #45433, .F. ) ;
#6141 = FACE_OUTER_BOUND ( 'NONE', #190934, .T. ) ;
#6142 = ORIENTED_EDGE ( 'NONE', *, *, #100919, .F. ) ;
#6143 = DIRECTION ( 'NONE',  ( 3.265361837132813093E-16, 0.4088369013363281068, -0.9126074666063770380 ) ) ;
#6144 = CARTESIAN_POINT ( 'NONE',  ( -21.00023020733502221, 30.82656943040777620, -252.1639858803266918 ) ) ;
#6145 = DIRECTION ( 'NONE',  ( 1.186688945009009831E-16, 1.000000000000000000, 6.982962677686266711E-15 ) ) ;
#6146 = DIRECTION ( 'NONE',  ( 1.000000000000000000, -1.186688945009009831E-16, -8.286604613020806758E-31 ) ) ;
#6147 = ORIENTED_EDGE ( 'NONE', *, *, #257612, .T. ) ;
#6148 = DIRECTION ( 'NONE',  ( 1.000000000000000000, 0.000000000000000000, 0.000000000000000000 ) ) ;
#6150 = ORIENTED_EDGE ( 'NONE', *, *, #36982, .T. ) ;
#6149 = AXIS2_PLACEMENT_3D ( 'NONE', #115639, #130050, #114359 ) ;
#6153 = EDGE_LOOP ( 'NONE', ( #75190, #141513, #8813 ) ) ;
#6152 = DIRECTION ( 'NONE',  ( 1.000000000000000000, 0.000000000000000000, 0.000000000000000000 ) ) ;
#6151 = PLANE ( 'NONE',  #49341 ) ;
#6154 = ADVANCED_FACE ( 'NONE', ( #21993 ), #220184, .T. ) ;
#6155 = CARTESIAN_POINT ( 'NONE',  ( 21.05000000000000071, 18.71171618620643429, -229.8673829423568691 ) ) ;
#6156 = ADVANCED_FACE ( 'NONE', ( #165689 ), #61339, .F. ) ;
#6158 = ORIENTED_EDGE ( 'NONE', *, *, #5645, .T. ) ;
#6157 = VECTOR ( 'NONE', #130293, 1000.000000000000000 ) ;
#6159 = AXIS2_PLACEMENT_3D ( 'NONE', #215329, #154127, #177535 ) ;
#6160 = CARTESIAN_POINT ( 'NONE',  ( -18.59999999999999787, -1.835859311443637010, -45.00443916879852679 ) ) ;
#6161 = ORIENTED_EDGE ( 'NONE', *, *, #235307, .T. ) ;
#6163 = LINE ( 'NONE', #129650, #109600 ) ;
#6162 = CIRCLE ( 'NONE', #156044, 0.09999999999998898659 ) ;
#6164 = EDGE_CURVE ( 'NONE', #123515, #162622, #227930, .T. ) ;
#6165 = DIRECTION ( 'NONE',  ( 0.000000000000000000, -0.8777080977375132376, 0.4791956752371582251 ) ) ;
#6166 = CARTESIAN_POINT ( 'NONE',  ( -20.00857864376270001, 66.85000000001222986, -148.8731074845244393 ) ) ;
#6167 = CARTESIAN_POINT ( 'NONE',  ( -16.94107738177414291, 51.68386028857256065, -231.8469600742508021 ) ) ;
#6168 = AXIS2_PLACEMENT_3D ( 'NONE', #129587, #229963, #13497 ) ;
#6169 = AXIS2_PLACEMENT_3D ( 'NONE', #161352, #935, #60939 ) ;
#6170 = EDGE_CURVE ( 'NONE', #128905, #147319, #240397, .T. ) ;
#6171 = CIRCLE ( 'NONE', #151966, 0.3999999999999975797 ) ;
#6172 = ORIENTED_EDGE ( 'NONE', *, *, #225918, .F. ) ;
#6174 = EDGE_CURVE ( 'NONE', #200635, #241925, #48845, .T. ) ;
#6173 = DIRECTION ( 'NONE',  ( 0.000000000000000000, 0.2128009952263607285, -0.9770955615653316162 ) ) ;
#6175 = DIRECTION ( 'NONE',  ( 1.000000000000000000, 0.000000000000000000, 0.000000000000000000 ) ) ;
#6176 = CARTESIAN_POINT ( 'NONE',  ( -15.15766958671844300, 66.58946139148341103, -154.5904194873835422 ) ) ;
#6177 = EDGE_LOOP ( 'NONE', ( #250701, #217880, #50823, #12338, #150763 ) ) ;
#6178 = CARTESIAN_POINT ( 'NONE',  ( -20.64999999999999858, 65.79629777212066699, -213.4483007241822747 ) ) ;
#6179 = ORIENTED_EDGE ( 'NONE', *, *, #223678, .F. ) ;
#6180 = DIRECTION ( 'NONE',  ( 4.239556034732056743E-17, 0.08413937888704771384, -0.9964539953858891908 ) ) ;
#6181 = CIRCLE ( 'NONE', #231075, 0.3999999999999952482 ) ;
#6182 = AXIS2_PLACEMENT_3D ( 'NONE', #146848, #47751, #107741 ) ;
#6183 = CARTESIAN_POINT ( 'NONE',  ( 18.59999999999999787, 77.36242903720467723, -28.13422623660311217 ) ) ;
#6184 = CARTESIAN_POINT ( 'NONE',  ( 20.94999999999999929, 76.00000000001170974, -69.52310748452431710 ) ) ;
#6186 = ORIENTED_EDGE ( 'NONE', *, *, #117485, .F. ) ;
#6185 = CARTESIAN_POINT ( 'NONE',  ( -18.40000000000000213, 5.650000000011139001, -113.1500000000000341 ) ) ;
#6187 = EDGE_CURVE ( 'NONE', #82519, #50332, #66573, .T. ) ;
#6188 = CARTESIAN_POINT ( 'NONE',  ( -21.05000000000000071, 11.62071067812980907, -174.3684166523410113 ) ) ;
#6189 = CIRCLE ( 'NONE', #76929, 0.09999999999998898659 ) ;
#6190 = TOROIDAL_SURFACE ( 'NONE', #235162, 11.90000000000000391, 0.1000000000000000056 ) ;
#6191 = CARTESIAN_POINT ( 'NONE',  ( -13.54036565897075484, 62.93961911720150226, -215.5706779233118482 ) ) ;
#6192 = LINE ( 'NONE', #24504, #218486 ) ;
#6193 = VERTEX_POINT ( 'NONE', #46976 ) ;
#6194 = ADVANCED_FACE ( 'NONE', ( #146089 ), #27484, .F. ) ;
#6195 = LINE ( 'NONE', #66179, #251697 ) ;
#6196 = DIRECTION ( 'NONE',  ( -1.000000000000000000, -0.000000000000000000, -0.000000000000000000 ) ) ;
#6197 = ORIENTED_EDGE ( 'NONE', *, *, #80907, .T. ) ;
#6198 = CARTESIAN_POINT ( 'NONE',  ( 22.59066674512271078, 64.25000000001236344, -170.0536116081545117 ) ) ;
#6199 = ORIENTED_EDGE ( 'NONE', *, *, #96140, .F. ) ;
#6200 = FACE_OUTER_BOUND ( 'NONE', #214151, .T. ) ;
#6202 = ORIENTED_EDGE ( 'NONE', *, *, #111053, .F. ) ;
#6201 = FACE_OUTER_BOUND ( 'NONE', #134189, .T. ) ;
#6203 = EDGE_CURVE ( 'NONE', #72992, #129969, #28773, .T. ) ;
#6206 = ORIENTED_EDGE ( 'NONE', *, *, #232768, .F. ) ;
#6205 = VERTEX_POINT ( 'NONE', #108267 ) ;
#6204 = LINE ( 'NONE', #81867, #134721 ) ;
#6207 = DIRECTION ( 'NONE',  ( -1.000000000000000000, 0.000000000000000000, 0.000000000000000000 ) ) ;
#6208 = CARTESIAN_POINT ( 'NONE',  ( 21.05000000000000071, 85.00000000001149658, -45.91707660717670336 ) ) ;
#6209 = CIRCLE ( 'NONE', #76958, 0.1999999999999987899 ) ;
#6210 = DIRECTION ( 'NONE',  ( 0.000000000000000000, 0.2128009952263403282, -0.9770955615653358350 ) ) ;
#6212 = CARTESIAN_POINT ( 'NONE',  ( -18.50000000000000000, 11.66622623553636018, -211.0987209794895421 ) ) ;
#6211 = CARTESIAN_POINT ( 'NONE',  ( 20.84999999999999432, 68.97833521811159585, -65.68954208262705663 ) ) ;
#6213 = DIRECTION ( 'NONE',  ( -0.000000000000000000, 0.000000000000000000, 1.000000000000000000 ) ) ;
#6214 = CIRCLE ( 'NONE', #68600, 0.5000000000000004441 ) ;
#6215 = CARTESIAN_POINT ( 'NONE',  ( -21.14999999999999858, 0.09779029131994770863, -127.7421853895239252 ) ) ;
#6216 = DIRECTION ( 'NONE',  ( 0.000000000000000000, 0.000000000000000000, -1.000000000000000000 ) ) ;
#6217 = DIRECTION ( 'NONE',  ( -1.020425574104003999E-15, -0.8814952561688429444, 0.4721928772777345684 ) ) ;
#6218 = DIRECTION ( 'NONE',  ( -1.000000000000000000, 0.000000000000000000, -0.000000000000000000 ) ) ;
#6219 = VERTEX_POINT ( 'NONE', #91273 ) ;
#6220 = ORIENTED_EDGE ( 'NONE', *, *, #75887, .F. ) ;
#6221 = CARTESIAN_POINT ( 'NONE',  ( -20.94999999999999929, 64.36312671090729509, -76.34486669784918433 ) ) ;
#6222 = CIRCLE ( 'NONE', #185306, 0.1000000000000028644 ) ;
#6224 = ORIENTED_EDGE ( 'NONE', *, *, #16437, .T. ) ;
#6223 = DIRECTION ( 'NONE',  ( 0.000000000000000000, 0.000000000000000000, -1.000000000000000000 ) ) ;
#6225 = ORIENTED_EDGE ( 'NONE', *, *, #8142, .F. ) ;
#6226 = DIRECTION ( 'NONE',  ( 0.000000000000000000, 6.982962677686266711E-15, -1.000000000000000000 ) ) ;
#6227 = ORIENTED_EDGE ( 'NONE', *, *, #161028, .F. ) ;
#6228 = DIRECTION ( 'NONE',  ( -1.000000000000000000, -0.000000000000000000, -0.000000000000000000 ) ) ;
#6229 = AXIS2_PLACEMENT_3D ( 'NONE', #228561, #109867, #130726 ) ;
#6230 = ORIENTED_EDGE ( 'NONE', *, *, #55941, .F. ) ;
#6231 = CARTESIAN_POINT ( 'NONE',  ( -16.94389599337535657, 66.00880201025508143, -82.13075228632277458 ) ) ;
#6232 = DIRECTION ( 'NONE',  ( -1.000000000000000000, -0.000000000000000000, -0.000000000000000000 ) ) ;
#6234 = ORIENTED_EDGE ( 'NONE', *, *, #60981, .F. ) ;
#6233 = ORIENTED_EDGE ( 'NONE', *, *, #7821, .F. ) ;
#6235 = ORIENTED_EDGE ( 'NONE', *, *, #206955, .T. ) ;
#6236 = CYLINDRICAL_SURFACE ( 'NONE', #240486, 0.09999999999998304689 ) ;
#6237 = ORIENTED_EDGE ( 'NONE', *, *, #150073, .F. ) ;
#6238 = VERTEX_POINT ( 'NONE', #211210 ) ;
#6239 = DIRECTION ( 'NONE',  ( 1.000000000000000000, 0.000000000000000000, 0.000000000000000000 ) ) ;
#6240 = DIRECTION ( 'NONE',  ( -1.000000000000000000, 0.000000000000000000, 0.000000000000000000 ) ) ;
#6242 = EDGE_LOOP ( 'NONE', ( #236481, #171353, #241692, #160210 ) ) ;
#6241 = FACE_OUTER_BOUND ( 'NONE', #244298, .T. ) ;
#6243 = CARTESIAN_POINT ( 'NONE',  ( -21.45000000000000284, 68.29142135624910281, -81.77310748452435973 ) ) ;
#6244 = DIRECTION ( 'NONE',  ( 0.000000000000000000, 0.9167729611565434977, -0.3994087351226345284 ) ) ;
#6246 = ORIENTED_EDGE ( 'NONE', *, *, #108852, .F. ) ;
#6245 = CYLINDRICAL_SURFACE ( 'NONE', #84955, 0.5000000000000004441 ) ;
#6247 = FACE_OUTER_BOUND ( 'NONE', #245726, .T. ) ;
#6248 = ORIENTED_EDGE ( 'NONE', *, *, #21439, .T. ) ;
#6249 = DIRECTION ( 'NONE',  ( -0.000000000000000000, 1.000000000000000000, -0.000000000000000000 ) ) ;
#6250 = EDGE_LOOP ( 'NONE', ( #141493, #4410, #237741, #168444 ) ) ;
#6251 = CARTESIAN_POINT ( 'NONE',  ( 20.85000000000000142, 77.83585931145498193, -24.51866831572578320 ) ) ;
#6252 = CARTESIAN_POINT ( 'NONE',  ( -20.85000000000000142, 10.33248238082519421, -39.09484654391315672 ) ) ;
#6253 = EDGE_CURVE ( 'NONE', #109234, #200341, #151252, .T. ) ;
#6254 = ORIENTED_EDGE ( 'NONE', *, *, #244093, .T. ) ;
#6256 = CARTESIAN_POINT ( 'NONE',  ( 21.14999999999999858, 1.115600667400684642E-11, -45.65000000000000568 ) ) ;
#6255 = DIRECTION ( 'NONE',  ( 0.000000000000000000, 0.2617529984165152257, 0.9651348961777124202 ) ) ;
#6257 = B_SPLINE_CURVE_WITH_KNOTS ( 'NONE', 3,
 ( #215356, #152863, #193243, #54979, #176266, #94124, #92838, #231100, #214081, #173726 ),
 .UNSPECIFIED., .F., .F.,
 ( 4, 2, 2, 2, 4 ),
 ( 5.273673492279070357E-16, 9.930191194499300776E-05, 0.0001986038238894586325, 0.0003972076477784301329, 0.0007944152955563315004 ),
 .UNSPECIFIED. ) ;
#6258 = DIRECTION ( 'NONE',  ( 0.000000000000000000, 1.000000000000000000, 0.000000000000000000 ) ) ;
#6259 = CIRCLE ( 'NONE', #101927, 0.09999999999999939493 ) ;
#6260 = CARTESIAN_POINT ( 'NONE',  ( 23.25000000000000000, 87.75000000001276135, -215.2731074845242745 ) ) ;
#6261 = EDGE_LOOP ( 'NONE', ( #199812, #149038, #46766, #85249 ) ) ;
#6262 = VERTEX_POINT ( 'NONE', #169565 ) ;
#6263 = LINE ( 'NONE', #29732, #167808 ) ;
#6264 = FACE_OUTER_BOUND ( 'NONE', #167475, .T. ) ;
#6265 = EDGE_LOOP ( 'NONE', ( #107236, #91555, #43615, #102821 ) ) ;
#6266 = DIRECTION ( 'NONE',  ( 0.000000000000000000, 0.000000000000000000, 1.000000000000000000 ) ) ;
#6267 = VERTEX_POINT ( 'NONE', #228216 ) ;
#6268 = CARTESIAN_POINT ( 'NONE',  ( 22.39999999999999503, 11.65000000001116298, -100.4000000000000483 ) ) ;
#6269 = ORIENTED_EDGE ( 'NONE', *, *, #192947, .T. ) ;
#6270 = FACE_OUTER_BOUND ( 'NONE', #119082, .T. ) ;
#6271 = EDGE_CURVE ( 'NONE', #127256, #173093, #208661, .T. ) ;
#6272 = ADVANCED_FACE ( 'NONE', ( #149980 ), #168280, .F. ) ;
#6273 = CARTESIAN_POINT ( 'NONE',  ( -21.14999999999999858, -0.09999999998884338825, -55.35042919245524473 ) ) ;
#6274 = CARTESIAN_POINT ( 'NONE',  ( 21.05000000000000071, 1.115600667400684642E-11, -167.4999999999999716 ) ) ;
#6275 = ORIENTED_EDGE ( 'NONE', *, *, #14358, .T. ) ;
#6276 = LINE ( 'NONE', #164092, #140075 ) ;
#6277 = CIRCLE ( 'NONE', #106222, 0.1000000000000009492 ) ;
#6278 = B_SPLINE_CURVE_WITH_KNOTS ( 'NONE', 3,
 ( #237815, #158313, #59135, #56569, #17475, #77428, #157016, #236518, #38341, #138672, #159567, #22641, #124297, #3032, #31323, #170853 ),
 .UNSPECIFIED., .F., .F.,
 ( 4, 3, 3, 3, 3, 4 ),
 ( 0.000000000000000000, 2.372700795693357903E-05, 5.739057815866867708E-05, 9.073899019179633917E-05, 0.0001243544287365728779, 0.0001585386695601243641 ),
 .UNSPECIFIED. ) ;
#6279 = VERTEX_POINT ( 'NONE', #48280 ) ;
#6280 = ORIENTED_EDGE ( 'NONE', *, *, #5769, .T. ) ;
#6281 = VERTEX_POINT ( 'NONE', #32615 ) ;
#6282 = EDGE_CURVE ( 'NONE', #120700, #19871, #90266, .T. ) ;
#6283 = FACE_OUTER_BOUND ( 'NONE', #81257, .T. ) ;
#6284 = CARTESIAN_POINT ( 'NONE',  ( -21.04999999999994387, 67.75000000001118394, -3.123107484524795474 ) ) ;
#6285 = VECTOR ( 'NONE', #183755, 1000.000000000000000 ) ;
#6286 = DIRECTION ( 'NONE',  ( 0.000000000000000000, 0.000000000000000000, 1.000000000000000000 ) ) ;
#6288 = EDGE_CURVE ( 'NONE', #23890, #34850, #119612, .T. ) ;
#6287 = DIRECTION ( 'NONE',  ( 1.000000000000000000, -1.335000415235278971E-16, 2.979993593738921214E-16 ) ) ;
#6289 = DIRECTION ( 'NONE',  ( 0.000000000000000000, -0.000000000000000000, 1.000000000000000000 ) ) ;
#6291 = CARTESIAN_POINT ( 'NONE',  ( 20.95429693346636313, 59.03464676750856910, -225.7981132573195850 ) ) ;
#6290 = CARTESIAN_POINT ( 'NONE',  ( 21.95218792049437795, 68.79849243876499543, -69.62213592432428300 ) ) ;
#6293 = VERTEX_POINT ( 'NONE', #109526 ) ;
#6292 = CARTESIAN_POINT ( 'NONE',  ( -21.05000000000000426, 61.17066907964395739, -234.2475650577967770 ) ) ;
#6294 = CARTESIAN_POINT ( 'NONE',  ( -22.48970261584618058, 11.65000000001115588, -100.4446305117826199 ) ) ;
#6295 = ORIENTED_EDGE ( 'NONE', *, *, #119877, .F. ) ;
#6296 = EDGE_CURVE ( 'NONE', #191619, #130365, #88665, .T. ) ;
#6297 = DIRECTION ( 'NONE',  ( 1.000000000000000000, 0.000000000000000000, 0.000000000000000000 ) ) ;
#6299 = EDGE_LOOP ( 'NONE', ( #80627, #160268, #115535, #233046, #115487 ) ) ;
#6298 = B_SPLINE_CURVE_WITH_KNOTS ( 'NONE', 3,
 ( #12398, #206724, #47625, #209284, #185873, #7225, #8528 ),
 .UNSPECIFIED., .F., .F.,
 ( 4, 3, 4 ),
 ( 0.000000000000000000, 0.0009834301579439959709, 0.001767853679402671277 ),
 .UNSPECIFIED. ) ;
#6300 = ORIENTED_EDGE ( 'NONE', *, *, #89382, .F. ) ;
#6301 = DIRECTION ( 'NONE',  ( -0.000000000000000000, -0.000000000000000000, 1.000000000000000000 ) ) ;
#6302 = CARTESIAN_POINT ( 'NONE',  ( 18.49999999999999645, -1.866714910046153308, -78.75267524628205251 ) ) ;
#6303 = CARTESIAN_POINT ( 'NONE',  ( -16.84793658983433318, 66.05000000001152216, -48.75675416233475090 ) ) ;
#6304 = CARTESIAN_POINT ( 'NONE',  ( 21.05000000000000071, 65.27628289530511552, -195.8581939154368285 ) ) ;
#6305 = EDGE_CURVE ( 'NONE', #135871, #189087, #132067, .T. ) ;
#6306 = CIRCLE ( 'NONE', #235253, 0.09999999999999693856 ) ;
#6307 = AXIS2_PLACEMENT_3D ( 'NONE', #178600, #241134, #135573 ) ;
#6308 = CARTESIAN_POINT ( 'NONE',  ( -20.85000000000000142, 75.83895117929300511, -69.80729732888453043 ) ) ;
#6309 = VERTEX_POINT ( 'NONE', #52120 ) ;
#6311 = ORIENTED_EDGE ( 'NONE', *, *, #49953, .T. ) ;
#6310 = ADVANCED_FACE ( 'NONE', ( #249073 ), #138074, .T. ) ;
#6312 = CARTESIAN_POINT ( 'NONE',  ( 23.24999999999999645, 70.35000000001181775, -82.17310748452436542 ) ) ;
#6313 = ORIENTED_EDGE ( 'NONE', *, *, #61052, .T. ) ;
#6314 = DIRECTION ( 'NONE',  ( 0.000000000000000000, 0.000000000000000000, -1.000000000000000000 ) ) ;
#6315 = DIRECTION ( 'NONE',  ( 0.000000000000000000, 4.336808689942494997E-15, -1.000000000000000000 ) ) ;
#6316 = DIRECTION ( 'NONE',  ( -0.000000000000000000, -6.982962677686266711E-15, 1.000000000000000000 ) ) ;
#6317 = FACE_OUTER_BOUND ( 'NONE', #136998, .T. ) ;
#6318 = CARTESIAN_POINT ( 'NONE',  ( -23.49999999999994316, 83.90000000001120384, -34.77310748452479316 ) ) ;
#6319 = CARTESIAN_POINT ( 'NONE',  ( 20.85000000000000142, -11.64999999998883595, -97.60000000000005116 ) ) ;
#6320 = ORIENTED_EDGE ( 'NONE', *, *, #82715, .F. ) ;
#6321 = DIRECTION ( 'NONE',  ( 0.000000000000000000, -6.652207440891584540E-15, 1.000000000000000000 ) ) ;
#6322 = DIRECTION ( 'NONE',  ( 0.000000000000000000, -1.000000000000000000, -1.445602896647339410E-16 ) ) ;
#6323 = LINE ( 'NONE', #66317, #75083 ) ;
#6324 = EDGE_CURVE ( 'NONE', #218161, #132362, #252898, .T. ) ;
#6325 = CYLINDRICAL_SURFACE ( 'NONE', #67005, 0.09999999999999939493 ) ;
#6326 = DIRECTION ( 'NONE',  ( 2.557131231893037478E-16, -0.8660254037844385966, 0.5000000000000003331 ) ) ;
#6327 = VECTOR ( 'NONE', #192543, 1000.000000000000000 ) ;
#6328 = CARTESIAN_POINT ( 'NONE',  ( 19.92426406871192412, 64.25000000001196554, -111.6731074845243938 ) ) ;
#6329 = TOROIDAL_SURFACE ( 'NONE', #193774, 0.2000000000000000111, 0.1000000000000000056 ) ;
#6330 = AXIS2_PLACEMENT_3D ( 'NONE', #125937, #26882, #9854 ) ;
#6331 = AXIS2_PLACEMENT_3D ( 'NONE', #97898, #139602, #174963 ) ;
#6332 = ORIENTED_EDGE ( 'NONE', *, *, #86956, .T. ) ;
#6333 = CARTESIAN_POINT ( 'NONE',  ( -21.00023020733438628, 69.60913075474442735, -136.5231074845243597 ) ) ;
#6334 = ORIENTED_EDGE ( 'NONE', *, *, #161570, .F. ) ;
#6335 = DIRECTION ( 'NONE',  ( 0.000000000000000000, -6.982962677686266711E-15, 1.000000000000000000 ) ) ;
#6336 = CARTESIAN_POINT ( 'NONE',  ( 20.94999999999999929, 7.128833340093095217, -233.7327013124392749 ) ) ;
#6337 = CARTESIAN_POINT ( 'NONE',  ( 21.13461538461538680, 61.88829803306103372, -221.6099259868126978 ) ) ;
#6338 = EDGE_LOOP ( 'NONE', ( #138069, #96805, #146440, #85639, #237293, #119797, #214292, #19813, #201555, #226893, #63864, #34099, #246031, #198278, #182307, #138358, #110013, #79622, #4831, #258028, #43273, #38444, #115687, #99190, #85011 ) ) ;
#6339 = CARTESIAN_POINT ( 'NONE',  ( -23.49999999999994316, 77.83551161375991967, -47.52760213295649550 ) ) ;
#6340 = LINE ( 'NONE', #108033, #219074 ) ;
#6341 = SURFACE_STYLE_USAGE ( .BOTH. , #205841 ) ;
#6342 = CARTESIAN_POINT ( 'NONE',  ( 20.85000000000000142, 74.98773774893902555, -233.8732236541320333 ) ) ;
#6343 = B_SPLINE_CURVE_WITH_KNOTS ( 'NONE', 3,
 ( #13492, #214255, #190869, #30495, #33091, #12220, #52594, #9620, #132143, #233820 ),
 .UNSPECIFIED., .F., .F.,
 ( 4, 3, 3, 4 ),
 ( 1.950915401637565782E-15, 8.145022132826850876E-06, 1.905645951092260044E-05, 2.061107371225642508E-05 ),
 .UNSPECIFIED. ) ;
#6344 = DIRECTION ( 'NONE',  ( 0.000000000000000000, -1.000000000000000000, -6.982962677686265922E-15 ) ) ;
#6345 = AXIS2_PLACEMENT_3D ( 'NONE', #64875, #166581, #66167 ) ;
#6346 = CARTESIAN_POINT ( 'NONE',  ( 22.42196299218230493, 75.99755832602515682, -181.6727191871738114 ) ) ;
#6347 = VECTOR ( 'NONE', #108233, 1000.000000000000000 ) ;
#6348 = EDGE_CURVE ( 'NONE', #248319, #79944, #173820, .T. ) ;
#6350 = EDGE_CURVE ( 'NONE', #239536, #56104, #164638, .T. ) ;
#6349 = AXIS2_PLACEMENT_3D ( 'NONE', #141744, #42651, #117064 ) ;
#6351 = VERTEX_POINT ( 'NONE', #14324 ) ;
#6352 = ORIENTED_EDGE ( 'NONE', *, *, #186996, .T. ) ;
#6353 = CARTESIAN_POINT ( 'NONE',  ( -20.85000000000000142, 77.83585931145570669, -125.0186683157258045 ) ) ;
#6355 = ORIENTED_EDGE ( 'NONE', *, *, #201949, .T. ) ;
#6354 = DIRECTION ( 'NONE',  ( 0.000000000000000000, 1.000000000000000000, -6.308085367188393199E-16 ) ) ;
#6356 = DIRECTION ( 'NONE',  ( 1.000000000000000000, 0.000000000000000000, 0.000000000000000000 ) ) ;
#6357 = LINE ( 'NONE', #23399, #111952 ) ;
#6358 = EDGE_CURVE ( 'NONE', #84754, #3667, #18142, .T. ) ;
#6359 = ADVANCED_FACE ( 'NONE', ( #173425 ), #223612, .T. ) ;
#6360 = ORIENTED_EDGE ( 'NONE', *, *, #128761, .F. ) ;
#6361 = CARTESIAN_POINT ( 'NONE',  ( 22.49999999999999645, 11.64957080755595520, -33.40000000000000568 ) ) ;
#6362 = CIRCLE ( 'NONE', #31358, 0.2000000000000000944 ) ;
#6363 = CONTEXT_DEPENDENT_SHAPE_REPRESENTATION ( #224100, #41372 ) ;
#6364 = AXIS2_PLACEMENT_3D ( 'NONE', #189883, #156897, #71237 ) ;
#6365 = AXIS2_PLACEMENT_3D ( 'NONE', #256007, #39624, #239076 ) ;
#6366 = LINE ( 'NONE', #104173, #108876 ) ;
#6367 = EDGE_CURVE ( 'NONE', #114275, #169539, #111221, .T. ) ;
#6368 = VERTEX_POINT ( 'NONE', #255417 ) ;
#6369 = CARTESIAN_POINT ( 'NONE',  ( 21.14999999999999503, 76.10000000001174669, -81.17267829206912211 ) ) ;
#6370 = EDGE_CURVE ( 'NONE', #145384, #168942, #252279, .T. ) ;
#6371 = EDGE_CURVE ( 'NONE', #170856, #86374, #27500, .T. ) ;
#6372 = CIRCLE ( 'NONE', #152152, 11.64999999999999325 ) ;
#6373 =( NAMED_UNIT ( * ) PLANE_ANGLE_UNIT ( ) SI_UNIT ( $, .RADIAN. ) );
#6375 = EDGE_LOOP ( 'NONE', ( #175652, #142207, #234862, #192897, #188378 ) ) ;
#6374 = CIRCLE ( 'NONE', #152154, 2.000000000000003553 ) ;
#6376 = EDGE_CURVE ( 'NONE', #131459, #210784, #186243, .T. ) ;
#6377 = ORIENTED_EDGE ( 'NONE', *, *, #192254, .F. ) ;
#6378 = DIRECTION ( 'NONE',  ( -1.000000000000000000, -1.394253735153569469E-16, -2.602809386958778209E-16 ) ) ;
#6379 = CIRCLE ( 'NONE', #131280, 0.09999999999999939493 ) ;
#6380 = FACE_OUTER_BOUND ( 'NONE', #50974, .T. ) ;
#6381 = CARTESIAN_POINT ( 'NONE',  ( -18.59999999999999787, 76.00000000001165290, -69.52310748452431710 ) ) ;
#6382 = AXIS2_PLACEMENT_3D ( 'NONE', #245737, #226131, #228753 ) ;
#6383 = DIRECTION ( 'NONE',  ( 0.000000000000000000, -0.8814952561688476074, 0.4721928772777262417 ) ) ;
#6384 = CARTESIAN_POINT ( 'NONE',  ( -23.25000000000000000, 10.33248238083634440, -206.5948465439131496 ) ) ;
#6385 = EDGE_CURVE ( 'NONE', #157944, #157060, #127976, .T. ) ;
#6386 = DIRECTION ( 'NONE',  ( 0.000000000000000000, 0.9770955615653310611, 0.2128009952263620608 ) ) ;
#6387 = CARTESIAN_POINT ( 'NONE',  ( -20.09999999999999787, 5.552655413246003313, 16.61686199900910310 ) ) ;
#6389 = CARTESIAN_POINT ( 'NONE',  ( -18.50000000000000000, -9.399999999988850163, -74.29725975966333351 ) ) ;
#6388 = DIRECTION ( 'NONE',  ( -1.000000000000000000, -0.000000000000000000, -0.000000000000000000 ) ) ;
#6391 = EDGE_CURVE ( 'NONE', #54263, #230368, #227356, .T. ) ;
#6390 = DIRECTION ( 'NONE',  ( 0.000000000000000000, 8.673617379883997607E-15, -1.000000000000000000 ) ) ;
#6392 = DIRECTION ( 'NONE',  ( -1.000000000000000000, 0.000000000000000000, 0.000000000000000000 ) ) ;
#6393 = CARTESIAN_POINT ( 'NONE',  ( -21.05000000000000071, -1.261786168565025568, -8.086498963545480478 ) ) ;
#6394 = VERTEX_POINT ( 'NONE', #55962 ) ;
#6395 = ORIENTED_EDGE ( 'NONE', *, *, #145586, .F. ) ;
#6396 = PLANE ( 'NONE',  #106716 ) ;
#6397 = FACE_OUTER_BOUND ( 'NONE', #98533, .T. ) ;
#6399 = DIRECTION ( 'NONE',  ( 0.000000000000000000, 0.000000000000000000, -1.000000000000000000 ) ) ;
#6398 = DIRECTION ( 'NONE',  ( 0.000000000000000000, 0.000000000000000000, 1.000000000000000000 ) ) ;
#6400 = EDGE_CURVE ( 'NONE', #192900, #109505, #117252, .T. ) ;
#6401 = CARTESIAN_POINT ( 'NONE',  ( 20.95566103547454517, 39.28266729857053008, -236.7406927167233164 ) ) ;
#6402 = DIRECTION ( 'NONE',  ( -1.000000000000000000, 0.000000000000000000, 0.000000000000000000 ) ) ;
#6403 = EDGE_CURVE ( 'NONE', #151965, #228728, #177252, .T. ) ;
#6404 = EDGE_CURVE ( 'NONE', #120532, #144062, #15613, .T. ) ;
#6405 = VERTEX_POINT ( 'NONE', #251622 ) ;
#6406 = ORIENTED_EDGE ( 'NONE', *, *, #148673, .F. ) ;
#6407 = AXIS2_PLACEMENT_3D ( 'NONE', #253710, #234151, #55485 ) ;
#6408 = CARTESIAN_POINT ( 'NONE',  ( -12.60829076262180060, 9.389529397466734650, -17.81710791289367535 ) ) ;
#6409 = ORIENTED_EDGE ( 'NONE', *, *, #168690, .F. ) ;
#6410 = DIRECTION ( 'NONE',  ( 0.000000000000000000, 0.000000000000000000, -1.000000000000000000 ) ) ;
#6411 = CIRCLE ( 'NONE', #102065, 0.09999999999999939493 ) ;
#6412 = DIRECTION ( 'NONE',  ( 1.000000000000000000, -9.792504721693619684E-16, -4.386921467590155985E-16 ) ) ;
#6413 = AXIS2_PLACEMENT_3D ( 'NONE', #131595, #92464, #211138 ) ;
#6414 = AXIS2_PLACEMENT_3D ( 'NONE', #95159, #213823, #176007 ) ;
#6415 = ORIENTED_EDGE ( 'NONE', *, *, #149911, .F. ) ;
#6416 = CARTESIAN_POINT ( 'NONE',  ( -18.50000000000000000, 18.34743685832668447, -236.8753540304231535 ) ) ;
#6417 = ORIENTED_EDGE ( 'NONE', *, *, #255113, .T. ) ;
#6419 = AXIS2_PLACEMENT_3D ( 'NONE', #86399, #246781, #103402 ) ;
#6418 = DIRECTION ( 'NONE',  ( 1.000000000000000000, 0.000000000000000000, 0.000000000000000000 ) ) ;
#6421 = AXIS2_PLACEMENT_3D ( 'NONE', #127541, #85804, #106667 ) ;
#6420 = FACE_OUTER_BOUND ( 'NONE', #184848, .T. ) ;
#6422 = CARTESIAN_POINT ( 'NONE',  ( 18.39999999999999147, 67.17743825834591576, -160.7731074845244166 ) ) ;
#6423 = CARTESIAN_POINT ( 'NONE',  ( 23.15000000000000213, 48.79765034352288922, -253.5326144460178170 ) ) ;
#6424 = DIRECTION ( 'NONE',  ( -0.000000000000000000, 0.9770955615653313941, 0.2128009952263603954 ) ) ;
#6425 = PLANE ( 'NONE',  #254044 ) ;
#6426 = AXIS2_PLACEMENT_3D ( 'NONE', #87153, #48037, #84551 ) ;
#6427 = CARTESIAN_POINT ( 'NONE',  ( -20.94999999999999929, 69.34766280046808617, -247.6726305063181428 ) ) ;
#6428 = PLANE ( 'NONE',  #186510 ) ;
#6430 = ORIENTED_EDGE ( 'NONE', *, *, #165763, .T. ) ;
#6429 = CARTESIAN_POINT ( 'NONE',  ( 18.44208962362797166, -0.7486949262819061479, -242.4509058008785303 ) ) ;
#6432 = CARTESIAN_POINT ( 'NONE',  ( -18.59999999999999787, 77.26327546522863088, -28.12124281777790813 ) ) ;
#6431 = DIRECTION ( 'NONE',  ( -1.000000000000000000, -0.000000000000000000, 0.000000000000000000 ) ) ;
#6433 = ORIENTED_EDGE ( 'NONE', *, *, #105260, .T. ) ;
#6435 = ORIENTED_EDGE ( 'NONE', *, *, #9915, .F. ) ;
#6434 = LINE ( 'NONE', #49421, #102552 ) ;
#6436 = VERTEX_POINT ( 'NONE', #95115 ) ;
#6437 = CARTESIAN_POINT ( 'NONE',  ( -20.54999999999999716, -9.499999999988846255, -124.1060308773475924 ) ) ;
#6438 = FACE_OUTER_BOUND ( 'NONE', #168608, .T. ) ;
#6439 = DIRECTION ( 'NONE',  ( 1.000000000000000000, -0.000000000000000000, -0.000000000000000000 ) ) ;
#6440 = DIRECTION ( 'NONE',  ( -1.000000000000000000, 0.000000000000000000, -0.000000000000000000 ) ) ;
#6442 = LINE ( 'NONE', #229362, #56421 ) ;
#6441 = AXIS2_PLACEMENT_3D ( 'NONE', #57822, #177822, #216905 ) ;
#6443 = ORIENTED_EDGE ( 'NONE', *, *, #104986, .F. ) ;
#6444 = CARTESIAN_POINT ( 'NONE',  ( -21.05000000000000071, 74.26374286841490857, -158.4544551555068779 ) ) ;
#6445 = EDGE_CURVE ( 'NONE', #165216, #98224, #155126, .T. ) ;
#6446 = CARTESIAN_POINT ( 'NONE',  ( 21.14250536705908345, 69.48182782313142525, -136.5231074845243313 ) ) ;
#6447 = EDGE_LOOP ( 'NONE', ( #197308, #76668, #190493 ) ) ;
#6448 = ORIENTED_EDGE ( 'NONE', *, *, #85791, .T. ) ;
#6449 = ADVANCED_FACE ( 'NONE', ( #84482 ), #194061, .F. ) ;
#6450 = CARTESIAN_POINT ( 'NONE',  ( -21.05000000000000071, -11.64999999998884306, -97.60000000000005116 ) ) ;
#6451 = AXIS2_PLACEMENT_3D ( 'NONE', #100519, #240077, #138373 ) ;
#6452 = EDGE_LOOP ( 'NONE', ( #162533, #85119, #184964, #206073 ) ) ;
#6453 = AXIS2_PLACEMENT_3D ( 'NONE', #231278, #209118, #70930 ) ;
#6454 = CARTESIAN_POINT ( 'NONE',  ( -23.15000000000000213, 76.00000000001165290, -69.52310748452431710 ) ) ;
#6455 = VERTEX_POINT ( 'NONE', #243608 ) ;
#6456 = CARTESIAN_POINT ( 'NONE',  ( 18.59999999999999076, 65.50857864377418593, -44.77310748452440237 ) ) ;
#6457 = EDGE_CURVE ( 'NONE', #130735, #141605, #65422, .T. ) ;
#6458 = EDGE_CURVE ( 'NONE', #81259, #130316, #85858, .T. ) ;
#6459 = LINE ( 'NONE', #165554, #167683 ) ;
#6460 = LINE ( 'NONE', #199564, #197511 ) ;
#6461 = LINE ( 'NONE', #100409, #198078 ) ;
#6462 = CYLINDRICAL_SURFACE ( 'NONE', #24828, 0.1000000000000028644 ) ;
#6463 = ORIENTED_EDGE ( 'NONE', *, *, #103505, .F. ) ;
#6464 = FACE_OUTER_BOUND ( 'NONE', #103057, .T. ) ;
#6465 = FACE_OUTER_BOUND ( 'NONE', #213956, .T. ) ;
#6466 = FACE_OUTER_BOUND ( 'NONE', #42091, .T. ) ;
#6467 = DIRECTION ( 'NONE',  ( 1.000000000000000000, 0.000000000000000000, 0.000000000000000000 ) ) ;
#6468 = ORIENTED_EDGE ( 'NONE', *, *, #228087, .T. ) ;
#6469 = AXIS2_PLACEMENT_3D ( 'NONE', #223394, #44779, #100847 ) ;
#6471 = DIRECTION ( 'NONE',  ( 0.000000000000000000, -0.2617529984164506107, -0.9651348961777299618 ) ) ;
#6470 = CARTESIAN_POINT ( 'NONE',  ( 23.14999999999999858, 79.90000000001141700, -36.02310748452429578 ) ) ;
#6472 = EDGE_LOOP ( 'NONE', ( #186807, #107140, #52630, #256998 ) ) ;
#6474 = ORIENTED_EDGE ( 'NONE', *, *, #218509, .F. ) ;
#6473 = CARTESIAN_POINT ( 'NONE',  ( 23.14999999999999858, 2.000000000011158630, -200.9999999999999432 ) ) ;
#6475 = EDGE_LOOP ( 'NONE', ( #86672, #149683, #69792, #79971, #80467 ) ) ;
#6476 = DIRECTION ( 'NONE',  ( -3.787827842127535236E-15, 0.7397360091702777085, 0.6728971962616808744 ) ) ;
#6477 = EDGE_CURVE ( 'NONE', #178909, #150487, #106720, .T. ) ;
#6478 = CARTESIAN_POINT ( 'NONE',  ( -21.15000000000000213, 33.98486250090727623, -243.5821103306120108 ) ) ;
#6479 = CARTESIAN_POINT ( 'NONE',  ( -20.64999999999999858, 68.85000000001180354, -81.87310748452436826 ) ) ;
#6480 = AXIS2_PLACEMENT_3D ( 'NONE', #71215, #13790, #54188 ) ;
#6481 = ORIENTED_EDGE ( 'NONE', *, *, #210862, .F. ) ;
#6482 = DIRECTION ( 'NONE',  ( 0.000000000000000000, -0.1350103645451876944, -0.9908441862701601321 ) ) ;
#6483 = CARTESIAN_POINT ( 'NONE',  ( 20.94999999999999929, 1.115625160336667635E-11, -198.9999999999999432 ) ) ;
#6485 = CARTESIAN_POINT ( 'NONE',  ( 18.49999999999999289, 53.24180694658302571, -234.8354225850497130 ) ) ;
#6484 = CARTESIAN_POINT ( 'NONE',  ( -21.14999999999999858, -0.09999999998884338825, -88.85042919245522341 ) ) ;
#6487 = VERTEX_POINT ( 'NONE', #119836 ) ;
#6486 = FACE_OUTER_BOUND ( 'NONE', #102106, .T. ) ;
#6488 = ADVANCED_FACE ( 'NONE', ( #40313 ), #144484, .T. ) ;
#6489 = ORIENTED_EDGE ( 'NONE', *, *, #233999, .F. ) ;
#6491 = EDGE_CURVE ( 'NONE', #88642, #28434, #23384, .T. ) ;
#6490 = CARTESIAN_POINT ( 'NONE',  ( 20.01093837587850288, 64.25000000001176659, -78.26871004992719350 ) ) ;
#6492 = DIRECTION ( 'NONE',  ( -3.469446951953635015E-14, 1.000000000000000000, 0.000000000000000000 ) ) ;
#6493 = VECTOR ( 'NONE', #161128, 1000.000000000000000 ) ;
#6494 = VECTOR ( 'NONE', #41657, 999.9999999999998863 ) ;
#6495 = CARTESIAN_POINT ( 'NONE',  ( -21.55000000000000071, 7.150000000011155876, -54.75000000000000000 ) ) ;
#6496 = VERTEX_POINT ( 'NONE', #242317 ) ;
#6497 = DIRECTION ( 'NONE',  ( 0.000000000000000000, 0.9999631594459055250, 0.008583690987131395445 ) ) ;
#6498 = VERTEX_POINT ( 'NONE', #220205 ) ;
#6499 = DIRECTION ( 'NONE',  ( 0.000000000000000000, -0.4856429311786307212, -0.8741572761215384846 ) ) ;
#6500 = FACE_OUTER_BOUND ( 'NONE', #91520, .T. ) ;
#6501 = LINE ( 'NONE', #22244, #168340 ) ;
#6502 = VERTEX_POINT ( 'NONE', #121130 ) ;
#6503 = EDGE_CURVE ( 'NONE', #103588, #211037, #118553, .T. ) ;
#6504 = DIRECTION ( 'NONE',  ( -1.000000000000000000, -0.000000000000000000, -0.000000000000000000 ) ) ;
#6505 = EDGE_CURVE ( 'NONE', #71110, #176580, #200639, .T. ) ;
#6506 = EDGE_LOOP ( 'NONE', ( #55695, #98187, #155795, #189013 ) ) ;
#6507 = AXIS2_PLACEMENT_3D ( 'NONE', #60089, #40582, #100483 ) ;
#6508 = EDGE_CURVE ( 'NONE', #1155, #152762, #206692, .T. ) ;
#6509 = FACE_OUTER_BOUND ( 'NONE', #52436, .T. ) ;
#6510 = AXIS2_PLACEMENT_3D ( 'NONE', #197917, #213641, #75448 ) ;
#6511 = VECTOR ( 'NONE', #193335, 1000.000000000000000 ) ;
#6512 = AXIS2_PLACEMENT_3D ( 'NONE', #122655, #183891, #200883 ) ;
#6513 = ORIENTED_EDGE ( 'NONE', *, *, #168309, .F. ) ;
#6514 = ORIENTED_EDGE ( 'NONE', *, *, #140101, .F. ) ;
#6515 = ORIENTED_EDGE ( 'NONE', *, *, #105356, .T. ) ;
#6516 = COLOUR_RGB ( '', 0.31764706, 0.68627451, 0.89019608) ;
#6517 = DIRECTION ( 'NONE',  ( 0.000000000000000000, 0.000000000000000000, 1.000000000000000000 ) ) ;
#6518 = ORIENTED_EDGE ( 'NONE', *, *, #146395, .F. ) ;
#6520 = VERTEX_POINT ( 'NONE', #22008 ) ;
#6519 = LINE ( 'NONE', #87327, #113687 ) ;
#6521 = EDGE_CURVE ( 'NONE', #14542, #228147, #214880, .T. ) ;
#6522 = EDGE_LOOP ( 'NONE', ( #124280, #145993, #52232 ) ) ;
#6524 = ORIENTED_EDGE ( 'NONE', *, *, #71085, .F. ) ;
#6523 = EDGE_LOOP ( 'NONE', ( #72870, #3988, #143811, #185322 ) ) ;
#6525 = EDGE_CURVE ( 'NONE', #79894, #139796, #61115, .T. ) ;
#6526 = CARTESIAN_POINT ( 'NONE',  ( -18.47130263965434338, -9.471155585952871547, -107.1834047654770501 ) ) ;
#6527 = EDGE_LOOP ( 'NONE', ( #140506, #171485, #186288, #118148, #94080, #23167, #138620, #134191 ) ) ;
#6528 = CARTESIAN_POINT ( 'NONE',  ( -21.65000000000000213, 42.13647595316535188, -239.1530172309881834 ) ) ;
#6529 = FACE_OUTER_BOUND ( 'NONE', #118842, .T. ) ;
#6530 = CIRCLE ( 'NONE', #252226, 0.5000000000000001110 ) ;
#6531 = CARTESIAN_POINT ( 'NONE',  ( -22.50000000000000000, 64.25000000001215028, -136.5231074845243597 ) ) ;
#6532 = CARTESIAN_POINT ( 'NONE',  ( -18.49372193242232854, 86.88397309856780737, -199.4657796619476926 ) ) ;
#6533 = AXIS2_PLACEMENT_3D ( 'NONE', #29911, #88553, #208540 ) ;
#6534 = ORIENTED_EDGE ( 'NONE', *, *, #60005, .T. ) ;
#6535 = ORIENTED_EDGE ( 'NONE', *, *, #6927, .T. ) ;
#6536 = B_SPLINE_CURVE_WITH_KNOTS ( 'NONE', 3,
 ( #153527, #116913, #215994, #131338, #196439, #111789, #115631, #175620, #235563, #191350 ),
 .UNSPECIFIED., .F., .F.,
 ( 4, 3, 3, 4 ),
 ( 1.903130014847812777E-15, 3.877043166998987006E-05, 7.336897548476661868E-05, 7.659383120239605946E-05 ),
 .UNSPECIFIED. ) ;
#6537 = DIRECTION ( 'NONE',  ( -1.000000000000000000, 0.000000000000000000, -0.000000000000000000 ) ) ;
#6539 = ORIENTED_EDGE ( 'NONE', *, *, #13153, .T. ) ;
#6538 = CARTESIAN_POINT ( 'NONE',  ( -20.64999999999999858, 4.350000000011156054, -88.15000000000004832 ) ) ;
#6541 = CARTESIAN_POINT ( 'NONE',  ( 23.14999999999999858, 1.115600667400684642E-11, -200.9999999999999432 ) ) ;
#6540 = AXIS2_PLACEMENT_3D ( 'NONE', #9314, #45874, #49726 ) ;
#6543 = ORIENTED_EDGE ( 'NONE', *, *, #198849, .F. ) ;
#6542 = DIRECTION ( 'NONE',  ( 0.000000000000000000, -0.8660254037844377084, -0.5000000000000016653 ) ) ;
#6544 = ORIENTED_EDGE ( 'NONE', *, *, #136042, .F. ) ;
#6545 = DIRECTION ( 'NONE',  ( 0.7071359030027289938, -0.1504668293610967600, 0.6908824414808452108 ) ) ;
#6546 = AXIS2_PLACEMENT_3D ( 'NONE', #179968, #238647, #1297 ) ;
#6547 = CIRCLE ( 'NONE', #77276, 0.09999999999999895084 ) ;
#6548 = TOROIDAL_SURFACE ( 'NONE', #256271, 11.90000000000000391, 0.1000000000000000056 ) ;
#6549 = ORIENTED_EDGE ( 'NONE', *, *, #88998, .F. ) ;
#6550 = ORIENTED_EDGE ( 'NONE', *, *, #64079, .F. ) ;
#6551 = DIRECTION ( 'NONE',  ( -1.000000000000000000, 0.000000000000000000, -0.000000000000000000 ) ) ;
#6552 = CARTESIAN_POINT ( 'NONE',  ( 18.49999999999999645, 70.05000000001193428, -92.71740517948948934 ) ) ;
#6555 = ORIENTED_EDGE ( 'NONE', *, *, #188635, .F. ) ;
#6554 = VERTEX_POINT ( 'NONE', #140651 ) ;
#6553 = AXIS2_PLACEMENT_3D ( 'NONE', #44071, #45349, #123609 ) ;
#6556 = VERTEX_POINT ( 'NONE', #181089 ) ;
#6557 = CARTESIAN_POINT ( 'NONE',  ( -21.05000000000000071, 11.65000000001115588, -100.6000000000000369 ) ) ;
#6558 = EDGE_LOOP ( 'NONE', ( #242649, #64671, #163331, #148147 ) ) ;
#6559 = AXIS2_PLACEMENT_3D ( 'NONE', #139775, #159376, #219324 ) ;
#6560 = ORIENTED_EDGE ( 'NONE', *, *, #203534, .F. ) ;
#6561 = LINE ( 'NONE', #45690, #17779 ) ;
#6563 = EDGE_LOOP ( 'NONE', ( #198308, #69993, #18518, #163987 ) ) ;
#6562 = DIRECTION ( 'NONE',  ( 0.000000000000000000, 0.000000000000000000, -1.000000000000000000 ) ) ;
#6564 = CARTESIAN_POINT ( 'NONE',  ( 20.85000000000000142, 14.61354176542825201, -235.9279552357344016 ) ) ;
#6565 = AXIS2_PLACEMENT_3D ( 'NONE', #138192, #239899, #83345 ) ;
#6566 = CIRCLE ( 'NONE', #102390, 0.1000000000000028644 ) ;
#6568 = DIRECTION ( 'NONE',  ( 0.000000000000000000, -0.1350103645451835865, -0.9908441862701605762 ) ) ;
#6567 = CARTESIAN_POINT ( 'NONE',  ( -23.49999999999994316, 87.50449464844290048, -37.85861909827351468 ) ) ;
#6569 = CARTESIAN_POINT ( 'NONE',  ( 18.59999999999999432, -9.480686695278969012, -40.44111516875785384 ) ) ;
#6570 = DIRECTION ( 'NONE',  ( 0.000000000000000000, -8.881784197001252323E-16, 1.000000000000000000 ) ) ;
#6571 = ORIENTED_EDGE ( 'NONE', *, *, #229001, .F. ) ;
#6572 = ORIENTED_EDGE ( 'NONE', *, *, #7037, .F. ) ;
#6573 = DIRECTION ( 'NONE',  ( 1.000000000000000000, 0.000000000000000000, 0.000000000000000000 ) ) ;
#6574 = EDGE_CURVE ( 'NONE', #152148, #207925, #10893, .T. ) ;
#6575 = ORIENTED_EDGE ( 'NONE', *, *, #103185, .F. ) ;
#6576 = CARTESIAN_POINT ( 'NONE',  ( -20.94999999999999929, 77.36087058720413268, -128.4501095574333362 ) ) ;
#6577 = ORIENTED_EDGE ( 'NONE', *, *, #18649, .T. ) ;
#6578 = ORIENTED_EDGE ( 'NONE', *, *, #233545, .T. ) ;
#6579 = CARTESIAN_POINT ( 'NONE',  ( -20.94684162548481154, 64.25000000001264766, -196.6814634889770446 ) ) ;
#6580 = ADVANCED_FACE ( 'NONE', ( #183648 ), #102783, .T. ) ;
#6581 = CARTESIAN_POINT ( 'NONE',  ( 21.05000000000000071, 5.850000000011156942, -157.3675027757221017 ) ) ;
#6582 = ORIENTED_EDGE ( 'NONE', *, *, #197667, .F. ) ;
#6583 = CARTESIAN_POINT ( 'NONE',  ( -21.03571358705782401, 11.75000000001115197, -107.3251068220583733 ) ) ;
#6584 = CARTESIAN_POINT ( 'NONE',  ( 23.24999999999999645, 5.076932660807368158, -234.1795834024155170 ) ) ;
#6585 = ORIENTED_EDGE ( 'NONE', *, *, #29050, .F. ) ;
#6586 = CARTESIAN_POINT ( 'NONE',  ( 19.75857864376269291, 64.25000000001220712, -145.1731074845244223 ) ) ;
#6587 = DIRECTION ( 'NONE',  ( 0.000000000000000000, 0.000000000000000000, 1.000000000000000000 ) ) ;
#6589 = DIRECTION ( 'NONE',  ( 0.000000000000000000, -0.8660254037844420383, 0.4999999999999943379 ) ) ;
#6588 = CARTESIAN_POINT ( 'NONE',  ( -21.14999999999999858, 1.115600667400684642E-11, -27.24142135623730354 ) ) ;
#6590 = CYLINDRICAL_SURFACE ( 'NONE', #127416, 0.09999999999999108213 ) ;
#6591 = ADVANCED_FACE ( 'NONE', ( #63678 ), #24587, .F. ) ;
#6593 = ADVANCED_FACE ( 'NONE', ( #161525 ), #226595, .T. ) ;
#6592 = CARTESIAN_POINT ( 'NONE',  ( 21.14261333020286671, 65.28430735075738767, -157.7731074845242176 ) ) ;
#6594 = DIRECTION ( 'NONE',  ( 0.000000000000000000, -6.982962677686266711E-15, 1.000000000000000000 ) ) ;
#6595 = AXIS2_PLACEMENT_3D ( 'NONE', #16166, #39589, #196065 ) ;
#6596 = CARTESIAN_POINT ( 'NONE',  ( -21.05000000000000071, 87.65000000001246860, -172.9231074845242802 ) ) ;
#6597 = VECTOR ( 'NONE', #2390, 1000.000000000000000 ) ;
#6598 = CIRCLE ( 'NONE', #223076, 1.749999999999999778 ) ;
#6599 = ORIENTED_EDGE ( 'NONE', *, *, #86054, .T. ) ;
#6600 = VECTOR ( 'NONE', #206978, 1000.000000000000000 ) ;
#6602 = ORIENTED_EDGE ( 'NONE', *, *, #70734, .T. ) ;
#6601 = ORIENTED_EDGE ( 'NONE', *, *, #246686, .F. ) ;
#6603 = VERTEX_POINT ( 'NONE', #79381 ) ;
#6604 = EDGE_CURVE ( 'NONE', #21528, #91963, #145776, .T. ) ;
#6605 = FACE_OUTER_BOUND ( 'NONE', #125180, .T. ) ;
#6606 = CARTESIAN_POINT ( 'NONE',  ( 23.15000000000000213, 85.60000000001149090, -45.91707660717669626 ) ) ;
#6607 = CIRCLE ( 'NONE', #56478, 0.5000000000000004441 ) ;
#6609 = DIRECTION ( 'NONE',  ( -1.000000000000000000, -0.000000000000000000, -0.000000000000000000 ) ) ;
#6608 = CARTESIAN_POINT ( 'NONE',  ( 18.52928932188133970, 10.27928932189250411, -188.8499999999999659 ) ) ;
#6610 = CARTESIAN_POINT ( 'NONE',  ( 21.05000000000000071, 67.22371710471985295, -161.4644784893834810 ) ) ;
#6612 = ORIENTED_EDGE ( 'NONE', *, *, #198342, .T. ) ;
#6611 = VECTOR ( 'NONE', #235610, 1000.000000000000000 ) ;
#6613 = CARTESIAN_POINT ( 'NONE',  ( 18.59999999999999076, 63.65372963998873246, -224.5957079722776655 ) ) ;
#6614 = CARTESIAN_POINT ( 'NONE',  ( -23.25000000000000000, 71.75000000001259082, -191.3731074845243825 ) ) ;
#6615 = AXIS2_PLACEMENT_3D ( 'NONE', #27885, #109942, #10861 ) ;
#6616 = DIRECTION ( 'NONE',  ( 1.000000000000000000, 0.000000000000000000, 0.000000000000000000 ) ) ;
#6617 = FACE_OUTER_BOUND ( 'NONE', #63562, .T. ) ;
#6618 = EDGE_LOOP ( 'NONE', ( #184516, #123347, #166057, #91264 ) ) ;
#6619 = CARTESIAN_POINT ( 'NONE',  ( -18.59999999999999787, 66.75000000001253397, -182.3731074845244393 ) ) ;
#6620 = ORIENTED_EDGE ( 'NONE', *, *, #195990, .F. ) ;
#6622 = VERTEX_POINT ( 'NONE', #227898 ) ;
#6621 = EDGE_CURVE ( 'NONE', #245711, #241330, #148364, .T. ) ;
#6623 = CARTESIAN_POINT ( 'NONE',  ( -18.38639463286148867, 64.51980042617591948, -93.77310748452438816 ) ) ;
#6624 = CARTESIAN_POINT ( 'NONE',  ( -23.25000000000000000, 74.00000000001180922, -82.74772940728641402 ) ) ;
#6625 = EDGE_CURVE ( 'NONE', #163980, #63679, #110833, .T. ) ;
#6626 = CIRCLE ( 'NONE', #52402, 0.09999999999999739653 ) ;
#6627 = DIRECTION ( 'NONE',  ( 0.000000000000000000, -8.267618268485210697E-15, 1.000000000000000000 ) ) ;
#6628 = DIRECTION ( 'NONE',  ( -0.7071067811865475727, -0.7071067811865475727, -0.000000000000000000 ) ) ;
#6629 = CARTESIAN_POINT ( 'NONE',  ( -21.04999999999999361, 6.344723404090243157, 0.01471785652417695149 ) ) ;
#6630 = ORIENTED_EDGE ( 'NONE', *, *, #98151, .T. ) ;
#6631 = LINE ( 'NONE', #66619, #179762 ) ;
#6632 = CARTESIAN_POINT ( 'NONE',  ( -23.15000000000000213, 11.75000000001115552, -55.25000000000004974 ) ) ;
#6634 = CARTESIAN_POINT ( 'NONE',  ( 18.49999999999999645, 77.29973367124323147, -179.9949779616549392 ) ) ;
#6633 = DIRECTION ( 'NONE',  ( -0.000000000000000000, -6.982962677686266711E-15, 1.000000000000000000 ) ) ;
#6635 = CARTESIAN_POINT ( 'NONE',  ( -18.54270223418607699, 85.62410550289533262, -163.2821724341169158 ) ) ;
#6636 = ADVANCED_FACE ( 'NONE', ( #10138 ), #109221, .T. ) ;
#6637 = CARTESIAN_POINT ( 'NONE',  ( -23.15000000000000213, -7.761787541757065867, -236.6467894636467975 ) ) ;
#6638 = DIRECTION ( 'NONE',  ( 0.000000000000000000, 0.4088369013363276072, -0.9126074666063773710 ) ) ;
#6639 = CARTESIAN_POINT ( 'NONE',  ( 21.00000000000000000, 0.000000000000000000, 0.000000000000000000 ) ) ;
#6640 = CIRCLE ( 'NONE', #123172, 0.09999999999999061029 ) ;
#6643 = ORIENTED_EDGE ( 'NONE', *, *, #222134, .T. ) ;
#6642 = AXIS2_PLACEMENT_3D ( 'NONE', #102787, #25865, #126223 ) ;
#6641 = DIRECTION ( 'NONE',  ( -3.265361837132813093E-16, -0.9651348961777146407, 0.2617529984165072321 ) ) ;
#6644 = AXIS2_PLACEMENT_3D ( 'NONE', #237677, #232569, #16091 ) ;
#6645 = CIRCLE ( 'NONE', #214927, 4.041421356237310469 ) ;
#6646 = B_SPLINE_CURVE_WITH_KNOTS ( 'NONE', 3,
 ( #211395, #31505, #73199, #150155, #13204, #253070, #34078, #247940, #9332, #113574 ),
 .UNSPECIFIED., .F., .F.,
 ( 4, 2, 2, 2, 4 ),
 ( 0.000000000000000000, 0.0001584437871624345463, 0.0002376656807436883299, 0.0002772766275343508378, 0.0003168875743250132914 ),
 .UNSPECIFIED. ) ;
#6647 = DIRECTION ( 'NONE',  ( 0.000000000000000000, 0.2605042016806672911, -0.9654727137038716656 ) ) ;
#6648 = CARTESIAN_POINT ( 'NONE',  ( -21.64999999999999858, 21.35054858842499925, -233.1262234518674177 ) ) ;
#6649 = AXIS2_PLACEMENT_3D ( 'NONE', #142927, #174758, #96432 ) ;
#6650 = CARTESIAN_POINT ( 'NONE',  ( -21.14999999999999858, 64.35000000001232934, -163.2392418215462726 ) ) ;
#6651 = ORIENTED_EDGE ( 'NONE', *, *, #208543, .F. ) ;
#6652 = SPHERICAL_SURFACE ( 'NONE', #72367, 0.1000000000000000056 ) ;
#6653 = DIRECTION ( 'NONE',  ( 0.000000000000000000, 0.000000000000000000, -1.000000000000000000 ) ) ;
#6654 = DIRECTION ( 'NONE',  ( 0.000000000000000000, 0.000000000000000000, -1.000000000000000000 ) ) ;
#6655 = EDGE_CURVE ( 'NONE', #239248, #236182, #177510, .T. ) ;
#6656 = AXIS2_PLACEMENT_3D ( 'NONE', #106149, #185713, #7061 ) ;
#6657 = ADVANCED_FACE ( 'NONE', ( #49255 ), #105340, .F. ) ;
#6658 = EDGE_LOOP ( 'NONE', ( #138022, #37695, #68643, #254245 ) ) ;
#6659 = CARTESIAN_POINT ( 'NONE',  ( 20.94999999999999929, 85.00000000001188027, -93.12913836187181005 ) ) ;
#6661 = VERTEX_POINT ( 'NONE', #47965 ) ;
#6660 = CARTESIAN_POINT ( 'NONE',  ( -20.00857864376270001, 63.96254146938299101, -212.9509700271909196 ) ) ;
#6663 = CARTESIAN_POINT ( 'NONE',  ( -23.49999999999994316, 77.73640333653723644, -47.54092689884382850 ) ) ;
#6662 = DIRECTION ( 'NONE',  ( -0.7071067811865475727, 0.7071067811865475727, 4.937700262164531476E-15 ) ) ;
#6665 = EDGE_CURVE ( 'NONE', #113549, #91113, #147059, .T. ) ;
#6664 = CARTESIAN_POINT ( 'NONE',  ( -18.34374000495060386, 11.47316190337362585, -143.2500000000000284 ) ) ;
#6666 = EDGE_CURVE ( 'NONE', #196907, #165093, #235721, .T. ) ;
#6667 = ORIENTED_EDGE ( 'NONE', *, *, #215420, .T. ) ;
#6668 = LINE ( 'NONE', #107048, #26196 ) ;
#6669 = CARTESIAN_POINT ( 'NONE',  ( 0.000000000000000000, 0.000000000000000000, 0.000000000000000000 ) ) ;
#6670 = DIRECTION ( 'NONE',  ( 0.000000000000000000, 0.2128009952264976468, -0.9770955615653015291 ) ) ;
#6671 = FACE_OUTER_BOUND ( 'NONE', #25142, .T. ) ;
#6672 = CARTESIAN_POINT ( 'NONE',  ( 20.94999999999999929, 1.148907358139439339E-11, -201.0000000000015064 ) ) ;
#6673 = EDGE_CURVE ( 'NONE', #157057, #20693, #202412, .T. ) ;
#6674 = ORIENTED_EDGE ( 'NONE', *, *, #249816, .F. ) ;
#6675 = CARTESIAN_POINT ( 'NONE',  ( 21.30000000000002558, 76.00000000001270450, -207.5731074845243427 ) ) ;
#6676 = FACE_OUTER_BOUND ( 'NONE', #76516, .T. ) ;
#6677 = ADVANCED_FACE ( 'NONE', ( #124955 ), #130068, .T. ) ;
#6678 = VECTOR ( 'NONE', #139947, 1000.000000000000000 ) ;
#6679 = PRESENTATION_STYLE_ASSIGNMENT (( #107059 ) ) ;
#6681 = ADVANCED_FACE ( 'NONE', ( #6264 ), #165361, .F. ) ;
#6680 = ADVANCED_FACE ( 'NONE', ( #204469 ), #7565, .T. ) ;
#6682 = CARTESIAN_POINT ( 'NONE',  ( 20.94999999999999574, 87.39257802171802325, -166.9491579046923277 ) ) ;
#6683 = VERTEX_POINT ( 'NONE', #170550 ) ;
#6684 = EDGE_CURVE ( 'NONE', #256235, #45345, #77478, .T. ) ;
#6685 = ORIENTED_EDGE ( 'NONE', *, *, #206925, .T. ) ;
#6686 = DIRECTION ( 'NONE',  ( 1.000000000000000000, 0.000000000000000000, 0.000000000000000000 ) ) ;
#6687 = LINE ( 'NONE', #139761, #77800 ) ;
#6688 = CARTESIAN_POINT ( 'NONE',  ( -18.40000000000000213, 70.35000000001255671, -182.6731074845243938 ) ) ;
#6689 = EDGE_CURVE ( 'NONE', #213031, #95210, #256511, .T. ) ;
#6690 = CARTESIAN_POINT ( 'NONE',  ( -11.60000000000000320, -8.250000000000007105, 15.00000000000000355 ) ) ;
#6691 = DIRECTION ( 'NONE',  ( -1.000000000000000000, 0.000000000000000000, 0.000000000000000000 ) ) ;
#6692 = B_SPLINE_CURVE_WITH_KNOTS ( 'NONE', 3,
 ( #35298, #258102, #215173, #16992, #176079, #159081, #238588, #160369, #61236, #100334, #114792, #255528, #18259, #194358, #97762, #177367, #59926, #256808, #139473 ),
 .UNSPECIFIED., .F., .F.,
 ( 4, 3, 3, 3, 3, 3, 4 ),
 ( -2.000416914655991116E-06, 0.000000000000000000, 4.714008503746756575E-05, 9.979203887778493915E-05, 0.0001372215519229563188, 0.0001635031576221042350, 0.0001900083748504183658 ),
 .UNSPECIFIED. ) ;
#6694 =( NAMED_UNIT ( * ) SI_UNIT ( $, .STERADIAN. ) SOLID_ANGLE_UNIT ( ) );
#6693 = CARTESIAN_POINT ( 'NONE',  ( -16.78493832629887450, 12.41293291551535916, -211.2574046339461802 ) ) ;
#6695 = DIRECTION ( 'NONE',  ( 0.000000000000000000, 1.000000000000000000, 0.000000000000000000 ) ) ;
#6697 = EDGE_CURVE ( 'NONE', #116181, #165365, #27167, .T. ) ;
#6696 = CARTESIAN_POINT ( 'NONE',  ( -16.90257928357874917, 9.954106821116520010, -113.1362854301137446 ) ) ;
#6699 = EDGE_CURVE ( 'NONE', #145935, #165343, #240021, .T. ) ;
#6698 = CARTESIAN_POINT ( 'NONE',  ( 23.24999999999999289, 69.45000000001181206, -81.67310748452436542 ) ) ;
#6700 = AXIS2_PLACEMENT_3D ( 'NONE', #204237, #28213, #26924 ) ;
#6701 = DIRECTION ( 'NONE',  ( -2.840903330521631775E-16, 0.8700118002898321601, -0.4930308989875230030 ) ) ;
#6702 = AXIS2_PLACEMENT_3D ( 'NONE', #205697, #101423, #24532 ) ;
#6704 = ORIENTED_EDGE ( 'NONE', *, *, #18212, .T. ) ;
#6703 = CARTESIAN_POINT ( 'NONE',  ( -23.15000000000000213, 23.34004772283015328, -229.2004250369967338 ) ) ;
#6705 = CARTESIAN_POINT ( 'NONE',  ( -18.50000000000000000, 77.35494420175976416, -241.6200040285045532 ) ) ;
#6706 = CARTESIAN_POINT ( 'NONE',  ( -20.94999999999999929, 76.00000000001126921, -203.5231074845248997 ) ) ;
#6708 = DIRECTION ( 'NONE',  ( 2.952720810173289112E-16, -1.000000000000000000, -0.000000000000000000 ) ) ;
#6707 = DIRECTION ( 'NONE',  ( 0.000000000000000000, -0.2128009952263603677, 0.9770955615653313941 ) ) ;
#6709 = EDGE_CURVE ( 'NONE', #135650, #132399, #15161, .T. ) ;
#6710 = ORIENTED_EDGE ( 'NONE', *, *, #145332, .T. ) ;
#6711 = DIRECTION ( 'NONE',  ( 0.000000000000000000, 0.09425075112713275638, 0.9955484899852801162 ) ) ;
#6712 = DIRECTION ( 'NONE',  ( -1.000000000000000000, -0.000000000000000000, -0.000000000000000000 ) ) ;
#6713 = CYLINDRICAL_SURFACE ( 'NONE', #167884, 0.09999999999999939493 ) ;
#6714 = CARTESIAN_POINT ( 'NONE',  ( 20.94999999999999574, 1.115600667400684642E-11, -33.50000000000000000 ) ) ;
#6715 = CARTESIAN_POINT ( 'NONE',  ( 22.49999999999999645, 12.55707850971095141, -223.4244300710886364 ) ) ;
#6716 = VERTEX_POINT ( 'NONE', #51803 ) ;
#6717 = EDGE_CURVE ( 'NONE', #38064, #240443, #198798, .T. ) ;
#6718 = EDGE_LOOP ( 'NONE', ( #80451, #202088 ) ) ;
#6719 = EDGE_CURVE ( 'NONE', #122837, #142228, #56925, .T. ) ;
#6720 = DIRECTION ( 'NONE',  ( -0.000000000000000000, 1.265107689135680095E-16, -1.000000000000000000 ) ) ;
#6721 = VERTEX_POINT ( 'NONE', #131360 ) ;
#6722 = DIRECTION ( 'NONE',  ( 0.000000000000000000, 1.000000000000000000, 0.000000000000000000 ) ) ;
#6723 = AXIS2_PLACEMENT_3D ( 'NONE', #203649, #64142, #87531 ) ;
#6724 = EDGE_LOOP ( 'NONE', ( #189383, #205714, #127359, #144892 ) ) ;
#6725 = CARTESIAN_POINT ( 'NONE',  ( 15.74999999999999645, 62.10905854918434699, -217.1108499610991203 ) ) ;
#6726 = AXIS2_PLACEMENT_3D ( 'NONE', #63550, #141802, #183513 ) ;
#6727 = SPHERICAL_SURFACE ( 'NONE', #256450, 0.1000000000000000056 ) ;
#6728 = CARTESIAN_POINT ( 'NONE',  ( -20.95000000000000639, 62.88396779178383866, -206.9948552354529738 ) ) ;
#6730 = ORIENTED_EDGE ( 'NONE', *, *, #158461, .T. ) ;
#6729 = AXIS2_PLACEMENT_3D ( 'NONE', #15769, #191838, #53582 ) ;
#6731 = EDGE_CURVE ( 'NONE', #159966, #217031, #131686, .T. ) ;
#6732 =( BOUNDED_SURFACE ( )  B_SPLINE_SURFACE ( 3, 2, ( 
 ( #135536, #18173, #76853 ),
 ( #71747, #156440, #74337 ),
 ( #134250, #151283, #230826 ),
 ( #52148, #238501, #256730 ) ),
 .UNSPECIFIED., .F., .F., .F. ) 
 B_SPLINE_SURFACE_WITH_KNOTS ( ( 4, 4 ),
 ( 3, 3 ),
 ( 0.04058434257139476031, 0.04256401539001599538 ),
 ( 0.000000000000000000, 1.000000000000000000 ),
 .UNSPECIFIED. ) 
 GEOMETRIC_REPRESENTATION_ITEM ( )  RATIONAL_B_SPLINE_SURFACE ( (
 ( 1.000000000000000000, 0.7103081912008298859, 1.000000000000000000),
 ( 1.000000000000000000, 0.7104998333555424539, 1.000000000000000000),
 ( 1.000000000000000000, 0.7107238315755094460, 1.000000000000000000),
 ( 1.000000000000000000, 0.7110073749539290722, 1.000000000000000000) ) ) 
 REPRESENTATION_ITEM ( '' )  SURFACE ( )  );
#6733 = FACE_OUTER_BOUND ( 'NONE', #23969, .T. ) ;
#6735 = CARTESIAN_POINT ( 'NONE',  ( -17.01473183483380680, 66.05000000001201954, -115.7731074845243739 ) ) ;
#6734 = CIRCLE ( 'NONE', #69296, 0.09999999999999516220 ) ;
#6736 = CARTESIAN_POINT ( 'NONE',  ( -20.54999999999999716, 4.350000000011156054, -83.75000000000004263 ) ) ;
#6737 = DIRECTION ( 'NONE',  ( 1.000000000000000000, 0.000000000000000000, 0.000000000000000000 ) ) ;
#6738 = CARTESIAN_POINT ( 'NONE',  ( 20.94999999999999574, 77.83534155023670564, -158.4679561919613491 ) ) ;
#6739 = DIRECTION ( 'NONE',  ( 1.000000000000000000, 0.000000000000000000, 0.000000000000000000 ) ) ;
#6740 = CARTESIAN_POINT ( 'NONE',  ( 21.05000000000000071, 11.16079915604378492, -211.0041093385139561 ) ) ;
#6741 = VERTEX_POINT ( 'NONE', #96069 ) ;
#6743 = CARTESIAN_POINT ( 'NONE',  ( -22.49917693094574389, 75.91477003579109351, -215.1729032690550412 ) ) ;
#6742 = LINE ( 'NONE', #26321, #140859 ) ;
#6744 = EDGE_LOOP ( 'NONE', ( #54289, #34267, #208333, #87364, #145522, #78735 ) ) ;
#6746 = VERTEX_POINT ( 'NONE', #113089 ) ;
#6745 = CYLINDRICAL_SURFACE ( 'NONE', #194013, 0.09999999999999939493 ) ;
#6747 = CIRCLE ( 'NONE', #31727, 12.87499999999999822 ) ;
#6748 = ORIENTED_EDGE ( 'NONE', *, *, #30880, .T. ) ;
#6749 = FACE_OUTER_BOUND ( 'NONE', #109431, .T. ) ;
#6750 = AXIS2_PLACEMENT_3D ( 'NONE', #154510, #219569, #159617 ) ;
#6751 = CARTESIAN_POINT ( 'NONE',  ( 18.54999999999999716, 8.750000000011182166, -87.85000000000003695 ) ) ;
#6753 =( BOUNDED_SURFACE ( )  B_SPLINE_SURFACE ( 3, 2, ( 
 ( #208599, #29969, #127767 ),
 ( #109460, #89899, #249008 ),
 ( #70386, #213708, #194174 ),
 ( #232011, #235831, #54628 ) ),
 .UNSPECIFIED., .F., .F., .F. ) 
 B_SPLINE_SURFACE_WITH_KNOTS ( ( 4, 4 ),
 ( 3, 3 ),
 ( -4.228388472693467293E-18, 0.0003124336600439479731 ),
 ( 0.000000000000000000, 1.000000000000000000 ),
 .UNSPECIFIED. ) 
 GEOMETRIC_REPRESENTATION_ITEM ( )  RATIONAL_B_SPLINE_SURFACE ( (
 ( 1.000000000000000000, 0.7071067811865363595, 1.000000000000000000),
 ( 1.000000000000000000, 0.7089187706047865856, 1.000000000000000000),
 ( 1.000000000000000000, 0.7039288185054065616, 1.000000000000000000),
 ( 1.000000000000000000, 0.7040654476015160146, 1.000000000000000000) ) ) 
 REPRESENTATION_ITEM ( '' )  SURFACE ( )  );
#6752 = AXIS2_PLACEMENT_3D ( 'NONE', #255201, #76617, #156192 ) ;
#6754 = CARTESIAN_POINT ( 'NONE',  ( -21.65000000000000213, 68.75000000001189449, -93.77310748452435973 ) ) ;
#6755 = DIRECTION ( 'NONE',  ( 1.000000000000000000, 0.000000000000000000, 0.000000000000000000 ) ) ;
#6756 = ORIENTED_EDGE ( 'NONE', *, *, #62043, .F. ) ;
#6757 = DIRECTION ( 'NONE',  ( 1.000000000000000000, 0.000000000000000000, -3.469446951953635015E-14 ) ) ;
#6758 = CARTESIAN_POINT ( 'NONE',  ( -21.14999999999999858, -2.576749817950531707, -189.6385361693310756 ) ) ;
#6759 = AXIS2_PLACEMENT_3D ( 'NONE', #55558, #214663, #192549 ) ;
#6760 = ORIENTED_EDGE ( 'NONE', *, *, #134384, .T. ) ;
#6761 = CARTESIAN_POINT ( 'NONE',  ( 18.54147908293604274, -9.463261657916875791, -174.5489488967558600 ) ) ;
#6762 = EDGE_CURVE ( 'NONE', #161541, #211804, #135194, .T. ) ;
#6763 = AXIS2_PLACEMENT_3D ( 'NONE', #150871, #128755, #30962 ) ;
#6764 = FACE_OUTER_BOUND ( 'NONE', #239947, .T. ) ;
#6765 = VERTEX_POINT ( 'NONE', #173111 ) ;
#6766 = EDGE_CURVE ( 'NONE', #13648, #89168, #2669, .T. ) ;
#6767 = CARTESIAN_POINT ( 'NONE',  ( -16.85722902420155478, 9.950000000011137047, -146.7655474737703685 ) ) ;
#6768 =( BOUNDED_SURFACE ( )  B_SPLINE_SURFACE ( 3, 2, ( 
 ( #132982, #71725, #11760 ),
 ( #252905, #215066, #134232 ),
 ( #52127, #232086, #55970 ),
 ( #50832, #151261, #230804 ),
 ( #110825, #213785, #114686 ),
 ( #96384, #194253, #191694 ) ),
 .UNSPECIFIED., .F., .F., .F. ) 
 B_SPLINE_SURFACE_WITH_KNOTS ( ( 4, 2, 4 ),
 ( 3, 3 ),
 ( 0.0001792624049599585438, 0.0003686986002124638092, 0.0005581347954649691287 ),
 ( 0.000000000000000000, 1.000000000000000000 ),
 .UNSPECIFIED. ) 
 GEOMETRIC_REPRESENTATION_ITEM ( )  RATIONAL_B_SPLINE_SURFACE ( (
 ( 1.000000000000000000, 0.9238795325113041690, 1.000000000000000000),
 ( 1.000000000000000000, 0.9229318695237117565, 1.000000000000000000),
 ( 1.000000000000000000, 0.8926288119232198559, 1.000000000000000000),
 ( 1.000000000000000000, 0.8123777807270403661, 1.000000000000000000),
 ( 1.000000000000000000, 0.7629087100932245846, 1.000000000000000000),
 ( 1.000000000000000000, 0.7071067811865475727, 1.000000000000000000) ) ) 
 REPRESENTATION_ITEM ( '' )  SURFACE ( )  );
#6769 = EDGE_LOOP ( 'NONE', ( #215612, #37892, #40583, #175497 ) ) ;
#6770 = CARTESIAN_POINT ( 'NONE',  ( 18.49999999999999289, 7.120270961708750512, -204.6595630418393057 ) ) ;
#6771 = ORIENTED_EDGE ( 'NONE', *, *, #138555, .T. ) ;
#6772 = DIRECTION ( 'NONE',  ( 0.000000000000000000, 7.086529944415894657E-15, -1.000000000000000000 ) ) ;
#6773 = EDGE_CURVE ( 'NONE', #91812, #180800, #33600, .T. ) ;
#6774 = EDGE_CURVE ( 'NONE', #114431, #207366, #164992, .T. ) ;
#6775 = CARTESIAN_POINT ( 'NONE',  ( 21.05000000000000071, 70.50000000001230660, -157.6178414656113205 ) ) ;
#6776 = DIRECTION ( 'NONE',  ( 0.000000000000000000, 0.000000000000000000, -1.000000000000000000 ) ) ;
#6777 = DIRECTION ( 'NONE',  ( 0.000000000000000000, 0.9126074666063771490, 0.4088369013363281623 ) ) ;
#6778 = VECTOR ( 'NONE', #67739, 1000.000000000000000 ) ;
#6779 = VECTOR ( 'NONE', #68842, 1000.000000000000114 ) ;
#6780 = AXIS2_PLACEMENT_3D ( 'NONE', #145355, #104911, #28016 ) ;
#6781 = DIRECTION ( 'NONE',  ( -1.000000000000000000, 0.000000000000000000, 0.000000000000000000 ) ) ;
#6782 = CARTESIAN_POINT ( 'NONE',  ( -23.25000000000000000, 43.00579525902548994, -254.2551217332645876 ) ) ;
#6783 = CARTESIAN_POINT ( 'NONE',  ( 20.90851465518106167, 10.32532329027886320, -72.56993430183595706 ) ) ;
#6784 = ORIENTED_EDGE ( 'NONE', *, *, #116312, .F. ) ;
#6786 = CARTESIAN_POINT ( 'NONE',  ( 23.25000000000000000, 11.39998237908105594, -245.7725481090871540 ) ) ;
#6785 = CARTESIAN_POINT ( 'NONE',  ( 23.24999999999999645, 67.17743825834583049, -149.1731074845244223 ) ) ;
#6787 = AXIS2_PLACEMENT_3D ( 'NONE', #52394, #130658, #31601 ) ;
#6788 = ADVANCED_FACE ( 'NONE', ( #253861 ), #255107, .T. ) ;
#6789 = CARTESIAN_POINT ( 'NONE',  ( -21.05000000000000071, -1.249999999988843369, -41.50000000000000000 ) ) ;
#6790 = PLANE ( 'NONE',  #118645 ) ;
#6791 = DIRECTION ( 'NONE',  ( 0.000000000000000000, 0.000000000000000000, -1.000000000000000000 ) ) ;
#6793 = ORIENTED_EDGE ( 'NONE', *, *, #91326, .F. ) ;
#6792 = DIRECTION ( 'NONE',  ( -1.000000000000000000, 0.000000000000000000, 0.000000000000000000 ) ) ;
#6795 = ORIENTED_EDGE ( 'NONE', *, *, #218569, .T. ) ;
#6794 = DIRECTION ( 'NONE',  ( 2.895190717381441586E-16, -0.1335171055202867274, -0.9910465087640865089 ) ) ;
#6796 = DIRECTION ( 'NONE',  ( 0.000000000000000000, -0.5859227990963362664, -0.8103668758649469339 ) ) ;
#6798 = CARTESIAN_POINT ( 'NONE',  ( -18.59999999999999787, 14.77103648604101060, -236.4083752604501001 ) ) ;
#6797 = AXIS2_PLACEMENT_3D ( 'NONE', #11101, #232729, #136142 ) ;
#6799 = CARTESIAN_POINT ( 'NONE',  ( 19.97071067811864609, 64.27928932189355749, -145.3731074845244109 ) ) ;
#6800 = VECTOR ( 'NONE', #177965, 1000.000000000000000 ) ;
#6802 = ORIENTED_EDGE ( 'NONE', *, *, #216266, .F. ) ;
#6801 = CARTESIAN_POINT ( 'NONE',  ( 21.05000000000000071, 1.115600667400684642E-11, -67.00000000000000000 ) ) ;
#6803 = AXIS2_PLACEMENT_3D ( 'NONE', #143629, #84911, #144901 ) ;
#6804 = EDGE_CURVE ( 'NONE', #235011, #71456, #248215, .T. ) ;
#6805 = CARTESIAN_POINT ( 'NONE',  ( 22.59999999999999432, 11.74956712350054566, -167.3991416309012550 ) ) ;
#6806 = DIRECTION ( 'NONE',  ( 0.000000000000000000, 0.2128009952263601179, -0.9770955615653315052 ) ) ;
#6807 = VERTEX_POINT ( 'NONE', #234306 ) ;
#6808 = DIRECTION ( 'NONE',  ( 1.000000000000000000, 0.000000000000000000, 0.000000000000000000 ) ) ;
#6809 = EDGE_LOOP ( 'NONE', ( #51009, #6601, #240147, #222891 ) ) ;
#6810 = VECTOR ( 'NONE', #190001, 1000.000000000000000 ) ;
#6811 = LINE ( 'NONE', #247984, #69995 ) ;
#6812 = CARTESIAN_POINT ( 'NONE',  ( 23.14999999999999858, 1.115600667400684642E-11, -113.3750000000000284 ) ) ;
#6813 = ORIENTED_EDGE ( 'NONE', *, *, #218258, .T. ) ;
#6814 = ADVANCED_FACE ( 'NONE', ( #176939 ), #116938, .T. ) ;
#6815 = CYLINDRICAL_SURFACE ( 'NONE', #66673, 0.09999999999999939493 ) ;
#6816 = ADVANCED_FACE ( 'NONE', ( #15290 ), #77790, .T. ) ;
#6817 = FACE_OUTER_BOUND ( 'NONE', #122980, .T. ) ;
#6818 = ORIENTED_EDGE ( 'NONE', *, *, #133684, .T. ) ;
#6819 = AXIS2_PLACEMENT_3D ( 'NONE', #141345, #120528, #42255 ) ;
#6820 = TOROIDAL_SURFACE ( 'NONE', #36059, 7.800000000000000711, 0.1000000000000000056 ) ;
#6821 = CARTESIAN_POINT ( 'NONE',  ( -18.50000000000000000, 36.65892442174935439, -249.5511627012433848 ) ) ;
#6822 = VECTOR ( 'NONE', #10325, 1000.000000000000000 ) ;
#6823 = VECTOR ( 'NONE', #171824, 1000.000000000000000 ) ;
#6824 = EDGE_CURVE ( 'NONE', #174969, #245418, #65216, .T. ) ;
#6825 = EDGE_LOOP ( 'NONE', ( #13573, #220731, #21013, #48177 ) ) ;
#6826 = VERTEX_POINT ( 'NONE', #94797 ) ;
#6827 = DIRECTION ( 'NONE',  ( 0.000000000000000000, -0.9628525332200033038, 0.2700277750006890298 ) ) ;
#6828 = ORIENTED_EDGE ( 'NONE', *, *, #188454, .F. ) ;
#6829 = CARTESIAN_POINT ( 'NONE',  ( -16.92989143108097849, 9.950000000011137047, -46.38248387475668011 ) ) ;
#6830 = ORIENTED_EDGE ( 'NONE', *, *, #44908, .F. ) ;
#6832 = ORIENTED_EDGE ( 'NONE', *, *, #222160, .T. ) ;
#6831 = DIRECTION ( 'NONE',  ( -7.304098846218134667E-16, -1.000000000000000000, 0.000000000000000000 ) ) ;
#6833 = EDGE_CURVE ( 'NONE', #2694, #179081, #153548, .T. ) ;
#6834 = EDGE_CURVE ( 'NONE', #252182, #254440, #127775, .T. ) ;
#6835 = FACE_OUTER_BOUND ( 'NONE', #81617, .T. ) ;
#6836 = ORIENTED_EDGE ( 'NONE', *, *, #72956, .F. ) ;
#6837 = ORIENTED_EDGE ( 'NONE', *, *, #121046, .T. ) ;
#6839 = ORIENTED_EDGE ( 'NONE', *, *, #254228, .F. ) ;
#6838 = ORIENTED_EDGE ( 'NONE', *, *, #118794, .F. ) ;
#6840 = LINE ( 'NONE', #29022, #90510 ) ;
#6841 = EDGE_CURVE ( 'NONE', #129705, #5761, #6956, .T. ) ;
#6842 = TOROIDAL_SURFACE ( 'NONE', #31986, 7.800000000000000711, 0.1000000000000000056 ) ;
#6843 = CARTESIAN_POINT ( 'NONE',  ( -21.05000000000000071, 56.16603649944111254, -228.1013850343386764 ) ) ;
#6844 = VECTOR ( 'NONE', #230845, 1000.000000000000000 ) ;
#6845 = AXIS2_PLACEMENT_3D ( 'NONE', #118752, #156618, #215268 ) ;
#6846 = VERTEX_POINT ( 'NONE', #126886 ) ;
#6847 = VECTOR ( 'NONE', #33101, 1000.000000000000000 ) ;
#6848 = ORIENTED_EDGE ( 'NONE', *, *, #237786, .T. ) ;
#6849 = DIRECTION ( 'NONE',  ( 6.938893903907222067E-15, -1.000000000000000000, -0.000000000000000000 ) ) ;
#6850 = EDGE_CURVE ( 'NONE', #161618, #138960, #73630, .T. ) ;
#6851 = DIRECTION ( 'NONE',  ( -2.978066053179068737E-16, -0.9651348961777163060, 0.2617529984165009038 ) ) ;
#6853 = EDGE_LOOP ( 'NONE', ( #84461, #227284, #112253 ) ) ;
#6852 = CARTESIAN_POINT ( 'NONE',  ( -18.50000000000000000, 67.84340367245323478, -228.0791829662263410 ) ) ;
#6854 = FACE_OUTER_BOUND ( 'NONE', #28428, .T. ) ;
#6855 = ORIENTED_EDGE ( 'NONE', *, *, #39267, .T. ) ;
#6856 = DIRECTION ( 'NONE',  ( 0.000000000000000000, 0.000000000000000000, -1.000000000000000000 ) ) ;
#6857 = DIRECTION ( 'NONE',  ( 0.5932847527679299127, -0.8049926720990051576, 6.366092712777055223E-16 ) ) ;
#6858 = ORIENTED_EDGE ( 'NONE', *, *, #138586, .T. ) ;
#6859 = CARTESIAN_POINT ( 'NONE',  ( -13.39999999999994351, 64.25000000001119815, -23.72310748452479245 ) ) ;
#6860 = DIRECTION ( 'NONE',  ( 1.000000000000000000, 0.000000000000000000, 0.000000000000000000 ) ) ;
#6861 = B_SPLINE_CURVE_WITH_KNOTS ( 'NONE', 3,
 ( #223261, #122906, #124193, #221958, #181600, #102010, #81174, #120363, #2928, #160768 ),
 .UNSPECIFIED., .F., .F.,
 ( 4, 2, 2, 2, 4 ),
 ( 0.000000000000000000, 4.221631689684923993E-05, 8.443263379369847987E-05, 0.0001688652675874693031, 0.0003377305351749470630 ),
 .UNSPECIFIED. ) ;
#6862 = ORIENTED_EDGE ( 'NONE', *, *, #45278, .F. ) ;
#6863 = CARTESIAN_POINT ( 'NONE',  ( 19.81427058490526250, 54.47541967946905572, -228.7836307801017597 ) ) ;
#6864 = ORIENTED_EDGE ( 'NONE', *, *, #84048, .F. ) ;
#6866 = EDGE_LOOP ( 'NONE', ( #147269, #228066 ) ) ;
#6865 = VERTEX_POINT ( 'NONE', #183017 ) ;
#6867 = VERTEX_POINT ( 'NONE', #145140 ) ;
#6868 = CARTESIAN_POINT ( 'NONE',  ( 18.59999999999998366, 68.97833521811203639, -132.6895420826271277 ) ) ;
#6869 = ORIENTED_EDGE ( 'NONE', *, *, #131852, .T. ) ;
#6870 = CARTESIAN_POINT ( 'NONE',  ( -21.45000000000000284, 68.29142135624888965, -57.17310748452437963 ) ) ;
#6871 = VERTEX_POINT ( 'NONE', #206417 ) ;
#6872 = DIRECTION ( 'NONE',  ( 0.000000000000000000, 0.000000000000000000, -1.000000000000000000 ) ) ;
#6873 = VECTOR ( 'NONE', #147785, 1000.000000000000000 ) ;
#6874 = CARTESIAN_POINT ( 'NONE',  ( 21.08489834409762764, 43.58682864821898306, -234.8080148706948478 ) ) ;
#6875 = ORIENTED_EDGE ( 'NONE', *, *, #256861, .F. ) ;
#6876 = ORIENTED_EDGE ( 'NONE', *, *, #197856, .F. ) ;
#6877 = TOROIDAL_SURFACE ( 'NONE', #244190, 0.6000000000000009770, 0.1000000000000000056 ) ;
#6878 = ORIENTED_EDGE ( 'NONE', *, *, #167330, .T. ) ;
#6879 = VECTOR ( 'NONE', #66018, 1000.000000000000000 ) ;
#6880 = AXIS2_PLACEMENT_3D ( 'NONE', #241954, #104973, #62055 ) ;
#6881 = LINE ( 'NONE', #186825, #76412 ) ;
#6882 = ORIENTED_EDGE ( 'NONE', *, *, #108623, .F. ) ;
#6883 = PLANE ( 'NONE',  #183581 ) ;
#6884 = EDGE_CURVE ( 'NONE', #185125, #224829, #184278, .T. ) ;
#6886 = VERTEX_POINT ( 'NONE', #42216 ) ;
#6885 = DIRECTION ( 'NONE',  ( 0.000000000000000000, 0.000000000000000000, -1.000000000000000000 ) ) ;
#6887 = CARTESIAN_POINT ( 'NONE',  ( -23.15000000000000213, -8.999999999988846255, -110.3939691226524786 ) ) ;
#6888 = LINE ( 'NONE', #86395, #93401 ) ;
#6889 = CARTESIAN_POINT ( 'NONE',  ( -17.11825945287482753, 65.95000000001158469, -56.77310748452439526 ) ) ;
#6890 = FACE_OUTER_BOUND ( 'NONE', #177032, .T. ) ;
#6891 = CARTESIAN_POINT ( 'NONE',  ( -18.46856557590793102, 85.47421590779912037, -196.4211212436419771 ) ) ;
#6892 = EDGE_CURVE ( 'NONE', #257228, #71514, #223393, .T. ) ;
#6894 = DIRECTION ( 'NONE',  ( -0.000000000000000000, -0.1350103645451876666, 0.9908441862701600211 ) ) ;
#6893 = DIRECTION ( 'NONE',  ( 1.000000000000000000, 0.000000000000000000, 0.000000000000000000 ) ) ;
#6896 = EDGE_CURVE ( 'NONE', #3980, #208027, #219343, .T. ) ;
#6895 = DIRECTION ( 'NONE',  ( -0.000000000000000000, -0.9876197685951290106, 0.1568667991644625281 ) ) ;
#6897 = CARTESIAN_POINT ( 'NONE',  ( 19.90000000000000568, 4.631764625546185066, 22.00000000000000355 ) ) ;
#6898 = CARTESIAN_POINT ( 'NONE',  ( 21.05000000000000071, 82.09643798151613225, -215.4278993322501208 ) ) ;
#6899 = LINE ( 'NONE', #250328, #63716 ) ;
#6900 = CIRCLE ( 'NONE', #40250, 11.75000000000001066 ) ;
#6901 = ORIENTED_EDGE ( 'NONE', *, *, #21879, .T. ) ;
#6902 = AXIS2_PLACEMENT_3D ( 'NONE', #179372, #178088, #3258 ) ;
#6903 = CIRCLE ( 'NONE', #181879, 0.1000000000000028644 ) ;
#6905 = ORIENTED_EDGE ( 'NONE', *, *, #59058, .T. ) ;
#6904 = CARTESIAN_POINT ( 'NONE',  ( 21.15000000000005187, 64.25000000001119815, -36.02310748452479316 ) ) ;
#6906 = VECTOR ( 'NONE', #211064, 1000.000000000000000 ) ;
#6907 = VERTEX_POINT ( 'NONE', #63040 ) ;
#6908 = EDGE_CURVE ( 'NONE', #145911, #208704, #244272, .T. ) ;
#6909 = CARTESIAN_POINT ( 'NONE',  ( 20.99999999999999645, 9.750000000011137757, -113.1500000000000483 ) ) ;
#6910 = AXIS2_PLACEMENT_3D ( 'NONE', #46230, #188318, #67089 ) ;
#6911 = ADVANCED_FACE ( 'NONE', ( #103439 ), #206873, .T. ) ;
#6912 =( NAMED_UNIT ( * ) SI_UNIT ( $, .STERADIAN. ) SOLID_ANGLE_UNIT ( ) );
#6913 = ORIENTED_EDGE ( 'NONE', *, *, #36753, .F. ) ;
#6914 = CARTESIAN_POINT ( 'NONE',  ( -20.64999999999999858, 85.50000000001149658, -45.91707660717669626 ) ) ;
#6915 = DIRECTION ( 'NONE',  ( 0.000000000000000000, 0.4721928772777512218, 0.8814952561688340626 ) ) ;
#6916 = ORIENTED_EDGE ( 'NONE', *, *, #195915, .F. ) ;
#6917 = CARTESIAN_POINT ( 'NONE',  ( -20.94999999999999929, 87.48912529308852015, -173.1231074845242688 ) ) ;
#6918 = DIRECTION ( 'NONE',  ( -0.000000000000000000, -6.982962677686266711E-15, 1.000000000000000000 ) ) ;
#6919 = AXIS2_PLACEMENT_3D ( 'NONE', #250694, #147762, #72084 ) ;
#6920 = CARTESIAN_POINT ( 'NONE',  ( -20.65000000000000568, 5.650000000011139001, -42.75000000000000000 ) ) ;
#6921 = CIRCLE ( 'NONE', #161064, 0.5000000000000004441 ) ;
#6922 = ADVANCED_FACE ( 'NONE', ( #27817 ), #15362, .T. ) ;
#6923 = ADVANCED_FACE ( 'NONE', ( #121767 ), #166035, .T. ) ;
#6924 = CARTESIAN_POINT ( 'NONE',  ( 21.05000000000000071, -11.64999999998883595, -97.60000000000005116 ) ) ;
#6926 = EDGE_LOOP ( 'NONE', ( #195686, #46359, #248366 ) ) ;
#6925 = CYLINDRICAL_SURFACE ( 'NONE', #118695, 0.09999999999999939493 ) ;
#6927 = EDGE_CURVE ( 'NONE', #144623, #112954, #66902, .T. ) ;
#6928 = DIRECTION ( 'NONE',  ( 0.000000000000000000, -7.086529944415894657E-15, 1.000000000000000000 ) ) ;
#6929 = CARTESIAN_POINT ( 'NONE',  ( -18.40000000000000213, 85.50000000001186606, -96.42291809330220076 ) ) ;
#6930 = DIRECTION ( 'NONE',  ( 0.000000000000000000, 0.000000000000000000, -1.000000000000000000 ) ) ;
#6931 = DIRECTION ( 'NONE',  ( 0.000000000000000000, 0.000000000000000000, -1.000000000000000000 ) ) ;
#6932 = ORIENTED_EDGE ( 'NONE', *, *, #243618, .F. ) ;
#6933 = CYLINDRICAL_SURFACE ( 'NONE', #178184, 0.09999999999999867328 ) ;
#6934 = DIRECTION ( 'NONE',  ( 0.000000000000000000, 6.308085367182471812E-16, 1.000000000000000000 ) ) ;
#6936 = DIRECTION ( 'NONE',  ( 5.421010862427554711E-16, -1.000000000000000000, -3.252606517456533024E-15 ) ) ;
#6935 = CARTESIAN_POINT ( 'NONE',  ( 21.05000000000000071, 82.22731448072437388, -214.9453318841612486 ) ) ;
#6937 = CARTESIAN_POINT ( 'NONE',  ( -21.05000000000000071, -11.41227409413852989, -137.0000000000000000 ) ) ;
#6938 = CARTESIAN_POINT ( 'NONE',  ( -16.97683810757273193, 9.950000000011137047, -53.73642328753960129 ) ) ;
#6939 = AXIS2_PLACEMENT_3D ( 'NONE', #103708, #67182, #7187 ) ;
#6940 = EDGE_CURVE ( 'NONE', #131784, #210362, #256715, .T. ) ;
#6941 = CARTESIAN_POINT ( 'NONE',  ( -18.50000000000000000, -1.162701749926853712, -41.60000000000000142 ) ) ;
#6942 = LINE ( 'NONE', #9507, #138177 ) ;
#6943 = DIRECTION ( 'NONE',  ( -1.000000000000000000, -0.000000000000000000, -0.000000000000000000 ) ) ;
#6944 = ORIENTED_EDGE ( 'NONE', *, *, #59147, .T. ) ;
#6945 = FACE_OUTER_BOUND ( 'NONE', #196661, .T. ) ;
#6946 = ORIENTED_EDGE ( 'NONE', *, *, #257321, .T. ) ;
#6947 = ORIENTED_EDGE ( 'NONE', *, *, #242302, .T. ) ;
#6948 = FACE_OUTER_BOUND ( 'NONE', #54250, .T. ) ;
#6949 = FACE_OUTER_BOUND ( 'NONE', #146185, .T. ) ;
#6950 = ORIENTED_EDGE ( 'NONE', *, *, #133997, .F. ) ;
#6951 = CIRCLE ( 'NONE', #152742, 0.1000000000000028644 ) ;
#6952 = TOROIDAL_SURFACE ( 'NONE', #186021, 0.2000000000000000111, 0.1000000000000000056 ) ;
#6954 = EDGE_CURVE ( 'NONE', #124932, #295, #47319, .T. ) ;
#6953 = VERTEX_POINT ( 'NONE', #104705 ) ;
#6955 =( LENGTH_UNIT ( ) NAMED_UNIT ( * ) SI_UNIT ( .MILLI., .METRE. ) );
#6956 = CIRCLE ( 'NONE', #235907, 0.09999999999998898659 ) ;
#6957 = TOROIDAL_SURFACE ( 'NONE', #65217, 11.90000000000000391, 0.1000000000000000056 ) ;
#6958 = EDGE_LOOP ( 'NONE', ( #118174, #143884, #19606, #240312 ) ) ;
#6959 = CARTESIAN_POINT ( 'NONE',  ( -18.50000000000000000, 1.340746217944851715, -56.72713749457886223 ) ) ;
#6960 = EDGE_LOOP ( 'NONE', ( #51440, #18902, #50376, #104913 ) ) ;
#6961 = AXIS2_PLACEMENT_3D ( 'NONE', #185196, #28741, #84773 ) ;
#6962 = DIRECTION ( 'NONE',  ( 0.000000000000000000, 0.4999999999999088507, 0.8660254037844913322 ) ) ;
#6963 = DIRECTION ( 'NONE',  ( -0.000000000000000000, -0.2128009952263603677, 0.9770955615653313941 ) ) ;
#6964 = CARTESIAN_POINT ( 'NONE',  ( -18.59999999999999787, -1.263275465206102233, -141.9018646667464338 ) ) ;
#6965 = EDGE_CURVE ( 'NONE', #74752, #126029, #94437, .T. ) ;
#6966 = DIRECTION ( 'NONE',  ( -1.000000000000000000, -0.000000000000000000, -0.000000000000000000 ) ) ;
#6967 = DIRECTION ( 'NONE',  ( 0.000000000000000000, 1.000000000000000000, 2.891205793294679805E-16 ) ) ;
#6969 = EDGE_LOOP ( 'NONE', ( #195119, #41893, #28294, #169228 ) ) ;
#6968 = CARTESIAN_POINT ( 'NONE',  ( 21.11345278033178374, 44.20339642523578050, -236.4386460197867166 ) ) ;
#6971 = DIRECTION ( 'NONE',  ( 0.000000000000000000, 0.000000000000000000, -1.000000000000000000 ) ) ;
#6970 = CARTESIAN_POINT ( 'NONE',  ( -20.64999999999999858, 63.44052078637213299, -222.1345147897817185 ) ) ;
#6972 = CARTESIAN_POINT ( 'NONE',  ( -22.00411653889206320, 75.90096189422482098, -76.77655035216469059 ) ) ;
#6973 = ORIENTED_EDGE ( 'NONE', *, *, #40381, .F. ) ;
#6974 = CARTESIAN_POINT ( 'NONE',  ( 21.72449340488910607, 65.71604372252150483, -194.2731074845244166 ) ) ;
#6975 = DIRECTION ( 'NONE',  ( 0.2834754621636358940, 0.2834754621636501049, -0.9161240771326873977 ) ) ;
#6977 = EDGE_CURVE ( 'NONE', #165976, #221039, #131860, .T. ) ;
#6976 = LINE ( 'NONE', #246865, #66631 ) ;
#6979 = ORIENTED_EDGE ( 'NONE', *, *, #159504, .T. ) ;
#6978 = AXIS2_PLACEMENT_3D ( 'NONE', #192921, #53404, #33890 ) ;
#6980 = CIRCLE ( 'NONE', #219359, 0.1000000000000028644 ) ;
#6981 = DIRECTION ( 'NONE',  ( 0.000000000000000000, 0.000000000000000000, 1.000000000000000000 ) ) ;
#6982 = ORIENTED_EDGE ( 'NONE', *, *, #38828, .F. ) ;
#6983 = EDGE_CURVE ( 'NONE', #38016, #178965, #106004, .T. ) ;
#6984 = DIRECTION ( 'NONE',  ( 0.000000000000000000, -0.008583690987135041833, 0.9999631594459055250 ) ) ;
#6986 = EDGE_CURVE ( 'NONE', #87006, #101145, #124319, .T. ) ;
#6985 = DIRECTION ( 'NONE',  ( -0.000000000000000000, 0.9875055080513808203, -0.1575844902526395142 ) ) ;
#6987 = DIRECTION ( 'NONE',  ( 0.000000000000000000, 1.000000000000000000, -1.224646799147352961E-16 ) ) ;
#6988 = AXIS2_PLACEMENT_3D ( 'NONE', #27780, #242931, #224650 ) ;
#6989 = LINE ( 'NONE', #123103, #136643 ) ;
#6990 = EDGE_LOOP ( 'NONE', ( #61919, #4645, #17869, #90204 ) ) ;
#6991 = ORIENTED_EDGE ( 'NONE', *, *, #49751, .F. ) ;
#6992 = CARTESIAN_POINT ( 'NONE',  ( 20.97462148592276776, 67.12526242356128137, -90.76846315279371424 ) ) ;
#6993 = CYLINDRICAL_SURFACE ( 'NONE', #152394, 0.1000000000000028644 ) ;
#6994 = EDGE_CURVE ( 'NONE', #174500, #70441, #123486, .T. ) ;
#6995 = CARTESIAN_POINT ( 'NONE',  ( -20.54999999999999716, 84.73084112150681335, -45.62118220350859588 ) ) ;
#6996 = FACE_OUTER_BOUND ( 'NONE', #121391, .T. ) ;
#6997 = CIRCLE ( 'NONE', #231888, 7.899999999999990585 ) ;
#6998 = AXIS2_PLACEMENT_3D ( 'NONE', #111195, #87758, #90329 ) ;
#6999 = DIRECTION ( 'NONE',  ( 0.000000000000000000, -0.9126074666063770380, -0.4088369013363281068 ) ) ;
#7000 = TOROIDAL_SURFACE ( 'NONE', #61179, 1.900000000000002576, 0.1000000000000000056 ) ;
#7001 = VECTOR ( 'NONE', #150630, 1000.000000000000000 ) ;
#7003 = EDGE_CURVE ( 'NONE', #193731, #71999, #111015, .T. ) ;
#7002 = DIRECTION ( 'NONE',  ( -1.000000000000000000, 0.000000000000000000, -0.000000000000000000 ) ) ;
#7004 = ORIENTED_EDGE ( 'NONE', *, *, #124061, .F. ) ;
#7005 = PLANE ( 'NONE',  #57704 ) ;
#7007 = ORIENTED_EDGE ( 'NONE', *, *, #37064, .T. ) ;
#7006 = CARTESIAN_POINT ( 'NONE',  ( -20.85000000000000142, 64.35000000001171827, -69.52310748452438816 ) ) ;
#7008 = CARTESIAN_POINT ( 'NONE',  ( 23.15000000000000213, -11.74999999998883560, -164.4000000000000057 ) ) ;
#7009 = DIRECTION ( 'NONE',  ( 0.000000000000000000, 0.000000000000000000, 1.000000000000000000 ) ) ;
#7010 = CARTESIAN_POINT ( 'NONE',  ( -21.05000000000000071, 76.00000000001213607, -136.5231074845242745 ) ) ;
#7011 = EDGE_CURVE ( 'NONE', #212706, #184009, #23575, .T. ) ;
#7012 = FACE_OUTER_BOUND ( 'NONE', #241402, .T. ) ;
#7014 = VERTEX_POINT ( 'NONE', #208983 ) ;
#7013 = CARTESIAN_POINT ( 'NONE',  ( 18.69999999999999929, 11.49641995933507843, 1.885425182446133441 ) ) ;
#7015 = CARTESIAN_POINT ( 'NONE',  ( -20.94999999999999929, 67.99035824846625076, -233.0562353075630142 ) ) ;
#7016 = CARTESIAN_POINT ( 'NONE',  ( 21.14999999999999858, 10.71339244341104013, -179.7499999999999716 ) ) ;
#7017 = DIRECTION ( 'NONE',  ( 2.259780016855445309E-14, 0.9875055080513753802, -0.1575844902526748192 ) ) ;
#7018 = DIRECTION ( 'NONE',  ( 0.000000000000000000, 0.2534589355812664757, 0.9673461469267405910 ) ) ;
#7019 = ORIENTED_EDGE ( 'NONE', *, *, #66709, .F. ) ;
#7020 = CARTESIAN_POINT ( 'NONE',  ( 18.51565452909213505, -7.607553483789936344, -210.0204117391616023 ) ) ;
#7021 = DIRECTION ( 'NONE',  ( 1.000000000000000000, 0.000000000000000000, 0.000000000000000000 ) ) ;
#7022 = EDGE_CURVE ( 'NONE', #241641, #30238, #19448, .T. ) ;
#7023 = FACE_OUTER_BOUND ( 'NONE', #90596, .T. ) ;
#7024 = AXIS2_PLACEMENT_3D ( 'NONE', #61529, #218002, #41980 ) ;
#7025 = ADVANCED_FACE ( 'NONE', ( #171193 ), #173613, .F. ) ;
#7026 = CIRCLE ( 'NONE', #73514, 4.150000000000001243 ) ;
#7028 = AXIS2_PLACEMENT_3D ( 'NONE', #46881, #89863, #188982 ) ;
#7027 = CARTESIAN_POINT ( 'NONE',  ( 18.39999999999999858, -7.883686024897172295, -209.9138933503092233 ) ) ;
#7029 = VERTEX_POINT ( 'NONE', #207722 ) ;
#7030 = CARTESIAN_POINT ( 'NONE',  ( -16.93710578446422943, 9.950000000011137047, -87.58119601620070682 ) ) ;
#7031 = ORIENTED_EDGE ( 'NONE', *, *, #116250, .F. ) ;
#7033 = DIRECTION ( 'NONE',  ( 0.000000000000000000, 6.467318590049456648E-15, -1.000000000000000000 ) ) ;
#7032 = CIRCLE ( 'NONE', #169587, 0.09999999999999976963 ) ;
#7034 = CARTESIAN_POINT ( 'NONE',  ( 18.59999999999999076, 44.47083028126615289, -247.4212268238128161 ) ) ;
#7035 = ORIENTED_EDGE ( 'NONE', *, *, #22250, .F. ) ;
#7036 = EDGE_CURVE ( 'NONE', #136922, #116426, #111177, .T. ) ;
#7037 = EDGE_CURVE ( 'NONE', #22095, #91552, #248106, .T. ) ;
#7038 = CARTESIAN_POINT ( 'NONE',  ( -20.54999999999999716, 85.00000000001159606, -59.62913836187181715 ) ) ;
#7039 = CARTESIAN_POINT ( 'NONE',  ( 21.08804281139591907, 13.00663943612646456, -210.8067932428972426 ) ) ;
#7040 = CARTESIAN_POINT ( 'NONE',  ( -20.90000000000000213, 7.800000000000000711, 1.212568896937007867 ) ) ;
#7041 = CARTESIAN_POINT ( 'NONE',  ( 18.49999999999999645, 1.866714910057309273, -11.75267524628200633 ) ) ;
#7042 = AXIS2_PLACEMENT_3D ( 'NONE', #89309, #162786, #21991 ) ;
#7043 = FACE_OUTER_BOUND ( 'NONE', #25872, .T. ) ;
#7044 = ORIENTED_EDGE ( 'NONE', *, *, #158296, .F. ) ;
#7045 = ORIENTED_EDGE ( 'NONE', *, *, #161271, .T. ) ;
#7046 = ORIENTED_EDGE ( 'NONE', *, *, #66721, .T. ) ;
#7047 = CARTESIAN_POINT ( 'NONE',  ( -23.25000000000000000, 20.01397631055648674, -237.6853859230195098 ) ) ;
#7048 = VERTEX_POINT ( 'NONE', #150312 ) ;
#7049 = DIRECTION ( 'NONE',  ( -1.000000000000000000, 0.000000000000000000, 0.000000000000000000 ) ) ;
#7050 = CYLINDRICAL_SURFACE ( 'NONE', #251725, 0.1000000000000028644 ) ;
#7051 = CARTESIAN_POINT ( 'NONE',  ( -18.59999999999999787, 61.95000000001210338, -131.0094124137634140 ) ) ;
#7052 = VERTEX_POINT ( 'NONE', #250669 ) ;
#7053 = CARTESIAN_POINT ( 'NONE',  ( -16.89797118371640039, 66.02361927736686198, -56.96040085208282733 ) ) ;
#7054 = DIRECTION ( 'NONE',  ( 1.000000000000000000, -0.000000000000000000, -0.000000000000000000 ) ) ;
#7055 = AXIS2_PLACEMENT_3D ( 'NONE', #169954, #113775, #70836 ) ;
#7056 = CARTESIAN_POINT ( 'NONE',  ( 20.97107704358301916, 8.875478152032441059, -42.05897322938925953 ) ) ;
#7057 = ORIENTED_EDGE ( 'NONE', *, *, #238222, .T. ) ;
#7058 = LINE ( 'NONE', #206552, #199931 ) ;
#7060 = ORIENTED_EDGE ( 'NONE', *, *, #252807, .F. ) ;
#7059 = DIRECTION ( 'NONE',  ( 0.000000000000000000, 0.000000000000000000, 1.000000000000000000 ) ) ;
#7061 = DIRECTION ( 'NONE',  ( 0.000000000000000000, 0.6728971962617862346, -0.7397360091701815632 ) ) ;
#7062 = DIRECTION ( 'NONE',  ( 0.000000000000000000, -0.1350103645451904977, 0.9908441862701596881 ) ) ;
#7063 = VECTOR ( 'NONE', #62522, 1000.000000000000000 ) ;
#7064 = VECTOR ( 'NONE', #156266, 1000.000000000000000 ) ;
#7065 = EDGE_CURVE ( 'NONE', #116410, #94115, #227257, .T. ) ;
#7066 = VERTEX_POINT ( 'NONE', #52459 ) ;
#7068 = DIRECTION ( 'NONE',  ( 0.000000000000000000, 0.8814952561688444987, -0.4721928772777320149 ) ) ;
#7067 = STYLED_ITEM ( 'NONE', ( #12150 ), #181958 ) ;
#7069 = DIRECTION ( 'NONE',  ( 0.000000000000000000, 0.000000000000000000, -1.000000000000000000 ) ) ;
#7070 = DIRECTION ( 'NONE',  ( 0.000000000000000000, 0.9908441862701420355, 0.1350103645453197554 ) ) ;
#7072 = ORIENTED_EDGE ( 'NONE', *, *, #31430, .T. ) ;
#7071 = AXIS2_PLACEMENT_3D ( 'NONE', #256981, #39299, #223035 ) ;
#7073 = DIRECTION ( 'NONE',  ( 0.000000000000000000, 0.000000000000000000, 1.000000000000000000 ) ) ;
#7074 = CIRCLE ( 'NONE', #90458, 11.64999999999999325 ) ;
#7075 = DIRECTION ( 'NONE',  ( 0.000000000000000000, -6.308085367188393199E-16, -1.000000000000000000 ) ) ;
#7076 = ORIENTED_EDGE ( 'NONE', *, *, #210416, .T. ) ;
#7077 = EDGE_CURVE ( 'NONE', #97749, #124985, #252652, .T. ) ;
#7078 = CIRCLE ( 'NONE', #236039, 0.09999999999998898659 ) ;
#7079 = ORIENTED_EDGE ( 'NONE', *, *, #220901, .T. ) ;
#7080 = DIRECTION ( 'NONE',  ( 0.000000000000000000, -0.1207987311150348075, 0.9926770202643947494 ) ) ;
#7081 = EDGE_LOOP ( 'NONE', ( #137334, #244755, #197345, #78990 ) ) ;
#7082 = CIRCLE ( 'NONE', #2982, 0.1000000000000004496 ) ;
#7083 = CARTESIAN_POINT ( 'NONE',  ( 5.899999999999995914, -11.34999999999999964, 10.00000000000000178 ) ) ;
#7084 = DIRECTION ( 'NONE',  ( 0.000000000000000000, 0.000000000000000000, -1.000000000000000000 ) ) ;
#7086 = ORIENTED_EDGE ( 'NONE', *, *, #216150, .F. ) ;
#7085 = FACE_OUTER_BOUND ( 'NONE', #89310, .T. ) ;
#7087 = CARTESIAN_POINT ( 'NONE',  ( 21.05000000000000071, 49.57218508014540959, -254.1759139559835035 ) ) ;
#7089 = AXIS2_PLACEMENT_3D ( 'NONE', #40529, #180014, #164298 ) ;
#7088 = CARTESIAN_POINT ( 'NONE',  ( 18.59999999999999432, 2.899901325892992876, -187.5321506284477096 ) ) ;
#7090 =( LENGTH_UNIT ( ) NAMED_UNIT ( * ) SI_UNIT ( .MILLI., .METRE. ) );
#7091 = DIRECTION ( 'NONE',  ( 0.000000000000000000, 0.000000000000000000, 1.000000000000000000 ) ) ;
#7092 = VECTOR ( 'NONE', #95438, 1000.000000000000000 ) ;
#7093 = CARTESIAN_POINT ( 'NONE',  ( -23.25000000000000000, 1.115626384983466744E-11, -98.40000000000004832 ) ) ;
#7094 = FACE_OUTER_BOUND ( 'NONE', #234507, .T. ) ;
#7095 = DIRECTION ( 'NONE',  ( 0.000000000000000000, 0.000000000000000000, -1.000000000000000000 ) ) ;
#7096 = CARTESIAN_POINT ( 'NONE',  ( -18.51555513499605254, -9.352657054493127120, -107.6951698956974752 ) ) ;
#7098 = EDGE_LOOP ( 'NONE', ( #85149, #3534, #25127, #118805 ) ) ;
#7097 = CARTESIAN_POINT ( 'NONE',  ( -23.49999999999994316, 89.48413628383013929, -38.12477508515532065 ) ) ;
#7099 = DIRECTION ( 'NONE',  ( 0.000000000000000000, -0.000000000000000000, 1.000000000000000000 ) ) ;
#7100 = ORIENTED_EDGE ( 'NONE', *, *, #23377, .F. ) ;
#7101 = CARTESIAN_POINT ( 'NONE',  ( -20.54999999999999716, 74.00000000001199396, -116.2477294072864140 ) ) ;
#7102 = LINE ( 'NONE', #72239, #98639 ) ;
#7103 = CYLINDRICAL_SURFACE ( 'NONE', #36513, 0.1000000000000024342 ) ;
#7104 = CARTESIAN_POINT ( 'NONE',  ( -21.14999999999999858, 64.35000000001195986, -103.0231074845244024 ) ) ;
#7105 = ORIENTED_EDGE ( 'NONE', *, *, #92846, .T. ) ;
#7106 = FACE_BOUND ( 'NONE', #163423, .T. ) ;
#7107 = DIRECTION ( 'NONE',  ( 1.000000000000000000, 0.000000000000000000, 0.000000000000000000 ) ) ;
#7108 = EDGE_CURVE ( 'NONE', #167847, #138780, #231144, .T. ) ;
#7109 = AXIS2_PLACEMENT_3D ( 'NONE', #211838, #171456, #51434 ) ;
#7110 = VERTEX_POINT ( 'NONE', #53764 ) ;
#7111 = DIRECTION ( 'NONE',  ( -1.000000000000000000, 0.000000000000000000, 0.000000000000000000 ) ) ;
#7113 = FACE_OUTER_BOUND ( 'NONE', #29039, .T. ) ;
#7112 = CIRCLE ( 'NONE', #248750, 0.1000000000000002692 ) ;
#7114 = EDGE_CURVE ( 'NONE', #123224, #33432, #36211, .T. ) ;
#7115 = EDGE_LOOP ( 'NONE', ( #128642, #151182, #239024, #106601 ) ) ;
#7116 = DIRECTION ( 'NONE',  ( -1.000000000000000000, 0.000000000000000000, 0.000000000000000000 ) ) ;
#7117 = ORIENTED_EDGE ( 'NONE', *, *, #134058, .T. ) ;
#7118 = CARTESIAN_POINT ( 'NONE',  ( -15.52965525596987995, 9.375538102059161716, -49.36987588099083979 ) ) ;
#7119 = ORIENTED_EDGE ( 'NONE', *, *, #224264, .F. ) ;
#7120 = ADVANCED_FACE ( 'NONE', ( #51163 ), #132016, .F. ) ;
#7121 = DIRECTION ( 'NONE',  ( 0.000000000000000000, 0.000000000000000000, -1.000000000000000000 ) ) ;
#7122 = AXIS2_PLACEMENT_3D ( 'NONE', #137369, #257277, #96934 ) ;
#7123 = CARTESIAN_POINT ( 'NONE',  ( 14.87567385445977131, 9.430764995433476017, -182.7305373947503995 ) ) ;
#7124 = AXIS2_PLACEMENT_3D ( 'NONE', #87440, #247813, #50866 ) ;
#7125 = CIRCLE ( 'NONE', #102797, 0.09999999999999724387 ) ;
#7126 = EDGE_LOOP ( 'NONE', ( #97862, #45176, #20917, #120791 ) ) ;
#7127 = EDGE_LOOP ( 'NONE', ( #144785, #97628, #100600, #155503 ) ) ;
#7128 = CARTESIAN_POINT ( 'NONE',  ( 23.14999999999999858, 76.00000000001195133, -103.0231074845243171 ) ) ;
#7129 = EDGE_CURVE ( 'NONE', #83334, #64314, #32966, .T. ) ;
#7131 = EDGE_LOOP ( 'NONE', ( #99939, #135295, #70914, #10022 ) ) ;
#7130 = CARTESIAN_POINT ( 'NONE',  ( 15.15590539855246810, 9.410682294279112625, -48.93114344194827936 ) ) ;
#7132 = CARTESIAN_POINT ( 'NONE',  ( 21.06277459767451887, 67.12713756174430557, -191.3191082921680959 ) ) ;
#7133 = ORIENTED_EDGE ( 'NONE', *, *, #245356, .T. ) ;
#7134 = AXIS2_PLACEMENT_3D ( 'NONE', #195495, #155089, #216299 ) ;
#7135 = ORIENTED_EDGE ( 'NONE', *, *, #213017, .T. ) ;
#7136 = DIRECTION ( 'NONE',  ( 0.000000000000000000, 0.000000000000000000, 1.000000000000000000 ) ) ;
#7137 = ADVANCED_FACE ( 'NONE', ( #49906 ), #86033, .F. ) ;
#7138 = CARTESIAN_POINT ( 'NONE',  ( -20.94999999999999929, 1.115600667400684642E-11, -41.40000000000000568 ) ) ;
#7139 = CARTESIAN_POINT ( 'NONE',  ( -18.59999999999999787, 64.35000000001245724, -170.0231074845244166 ) ) ;
#7140 = DIRECTION ( 'NONE',  ( 1.000000000000000000, -0.000000000000000000, -0.000000000000000000 ) ) ;
#7141 = CIRCLE ( 'NONE', #60739, 0.09999999999999459321 ) ;
#7142 = CARTESIAN_POINT ( 'NONE',  ( 20.94999999999999929, 85.00000000001261924, -193.6291383618718385 ) ) ;
#7143 = CARTESIAN_POINT ( 'NONE',  ( 20.09999999999999787, 66.25000000001190870, -93.77310748452438816 ) ) ;
#7144 = AXIS2_PLACEMENT_3D ( 'NONE', #54493, #111927, #31130 ) ;
#7145 = VERTEX_POINT ( 'NONE', #193289 ) ;
#7146 = CARTESIAN_POINT ( 'NONE',  ( -16.94275863006528482, 66.01050395134502935, -182.6314101024478589 ) ) ;
#7147 = CARTESIAN_POINT ( 'NONE',  ( -16.97683809663752186, 9.850000000011137402, -187.5976359818036485 ) ) ;
#7148 = CARTESIAN_POINT ( 'NONE',  ( 23.14999999999999858, 5.600000000011153389, -121.5947339810869465 ) ) ;
#7149 = DIRECTION ( 'NONE',  ( -0.1538461538461510236, 0.9880948137434718559, 0.000000000000000000 ) ) ;
#7150 = VERTEX_POINT ( 'NONE', #112470 ) ;
#7151 = CARTESIAN_POINT ( 'NONE',  ( -20.54999999999999716, 21.35054858842500281, -233.1262234518673893 ) ) ;
#7152 = EDGE_LOOP ( 'NONE', ( #189631, #130382, #202844, #220491 ) ) ;
#7153 = CARTESIAN_POINT ( 'NONE',  ( 12.25000000000000000, 9.350000000011140955, -117.2500000000000284 ) ) ;
#7155 = ORIENTED_EDGE ( 'NONE', *, *, #14600, .F. ) ;
#7154 = CIRCLE ( 'NONE', #44603, 1.749999999999999778 ) ;
#7156 = CARTESIAN_POINT ( 'NONE',  ( 20.94999999999999929, 76.00000000001244871, -170.0231074845243597 ) ) ;
#7157 = VERTEX_POINT ( 'NONE', #128171 ) ;
#7158 = ORIENTED_EDGE ( 'NONE', *, *, #140661, .T. ) ;
#7160 = ORIENTED_EDGE ( 'NONE', *, *, #198394, .T. ) ;
#7159 = DIRECTION ( 'NONE',  ( 0.000000000000000000, 0.000000000000000000, -1.000000000000000000 ) ) ;
#7161 = FACE_OUTER_BOUND ( 'NONE', #33646, .T. ) ;
#7162 = EDGE_LOOP ( 'NONE', ( #253259, #75554, #117177, #254547 ) ) ;
#7163 = DIRECTION ( 'NONE',  ( -0.000000000000000000, 1.000000000000000000, 6.982962677686266711E-15 ) ) ;
#7164 = FACE_OUTER_BOUND ( 'NONE', #187489, .T. ) ;
#7165 = ORIENTED_EDGE ( 'NONE', *, *, #233097, .T. ) ;
#7166 = DIRECTION ( 'NONE',  ( 1.000000000000000000, -0.000000000000000000, -0.000000000000000000 ) ) ;
#7167 = CARTESIAN_POINT ( 'NONE',  ( 18.59999999999999787, -1.736705739456431807, -145.5174225876237699 ) ) ;
#7168 = TOROIDAL_SURFACE ( 'NONE', #202997, 7.800000000000000711, 0.1000000000000000056 ) ;
#7169 = VECTOR ( 'NONE', #250079, 1000.000000000000000 ) ;
#7170 = CIRCLE ( 'NONE', #215474, 1.500000000000001332 ) ;
#7171 = VERTEX_POINT ( 'NONE', #251962 ) ;
#7172 = EDGE_CURVE ( 'NONE', #5985, #39887, #248387, .T. ) ;
#7173 = DIRECTION ( 'NONE',  ( -1.000000000000000000, 0.000000000000000000, 0.000000000000000000 ) ) ;
#7174 = ADVANCED_FACE ( 'NONE', ( #12098 ), #152902, .F. ) ;
#7175 = CARTESIAN_POINT ( 'NONE',  ( 20.94999999999999929, 1.115600667400684642E-11, -200.9999999999999432 ) ) ;
#7177 = ORIENTED_EDGE ( 'NONE', *, *, #192145, .F. ) ;
#7176 = CARTESIAN_POINT ( 'NONE',  ( -16.83794237512073622, 9.926359221118632448, -46.30354215869895995 ) ) ;
#7178 = CYLINDRICAL_SURFACE ( 'NONE', #136916, 0.1000000000000024342 ) ;
#7179 = CARTESIAN_POINT ( 'NONE',  ( 20.04142135623730070, 11.75000000001115907, -55.25000000000004974 ) ) ;
#7180 = CARTESIAN_POINT ( 'NONE',  ( 18.59999999999999787, 77.26327546522911405, -95.12124281777788326 ) ) ;
#7181 = EDGE_CURVE ( 'NONE', #86370, #155283, #202595, .T. ) ;
#7184 = DIRECTION ( 'NONE',  ( 2.715809747126116508E-16, -0.4721928772777347905, -0.8814952561688429444 ) ) ;
#7183 = CIRCLE ( 'NONE', #61372, 0.2000000000000057288 ) ;
#7182 = CARTESIAN_POINT ( 'NONE',  ( 23.24999999999999289, 3.801854678198143933, -188.1465607323988252 ) ) ;
#7186 = ADVANCED_FACE ( 'NONE', ( #238827 ), #58872, .T. ) ;
#7185 = CARTESIAN_POINT ( 'NONE',  ( -20.94403535211772294, 65.69367753730709580, -164.5189238066348594 ) ) ;
#7187 = DIRECTION ( 'NONE',  ( 0.000000000000000000, -0.9651348961777028723, 0.2617529984165503087 ) ) ;
#7188 = CIRCLE ( 'NONE', #3085, 0.09999999999999939493 ) ;
#7189 = CARTESIAN_POINT ( 'NONE',  ( -21.14999999999999858, 64.35000000001160458, -62.73924182154625129 ) ) ;
#7190 = DIRECTION ( 'NONE',  ( -1.000000000000000000, 0.000000000000000000, 0.000000000000000000 ) ) ;
#7191 = EDGE_LOOP ( 'NONE', ( #70922, #171395, #104279, #39728 ) ) ;
#7192 = VECTOR ( 'NONE', #13538, 1000.000000000000000 ) ;
#7193 = ORIENTED_EDGE ( 'NONE', *, *, #7172, .F. ) ;
#7194 = DIRECTION ( 'NONE',  ( 7.304098846218134667E-16, -1.000000000000000000, -6.982962677686267499E-15 ) ) ;
#7195 = ADVANCED_FACE ( 'NONE', ( #120200 ), #15957, .T. ) ;
#7196 = ORIENTED_EDGE ( 'NONE', *, *, #243405, .T. ) ;
#7197 = EDGE_CURVE ( 'NONE', #144708, #110957, #216687, .T. ) ;
#7198 = CARTESIAN_POINT ( 'NONE',  ( 20.95000000000000284, 64.40000000001218439, -143.4513107147999449 ) ) ;
#7199 = EDGE_CURVE ( 'NONE', #94319, #137100, #158053, .T. ) ;
#7200 = VERTEX_POINT ( 'NONE', #117591 ) ;
#7201 = SURFACE_SIDE_STYLE ('',( #51450 ) ) ;
#7202 = CARTESIAN_POINT ( 'NONE',  ( -21.05000000000000071, 69.58624026620211112, -169.9374944237204375 ) ) ;
#7203 = DIRECTION ( 'NONE',  ( 1.000000000000000000, 8.674042436075353235E-17, 1.619280515896125144E-16 ) ) ;
#7205 = ORIENTED_EDGE ( 'NONE', *, *, #63089, .T. ) ;
#7204 = CIRCLE ( 'NONE', #36295, 0.09999999999999993616 ) ;
#7206 = DIRECTION ( 'NONE',  ( 0.000000000000000000, 0.9770955615653259541, 0.2128009952263860971 ) ) ;
#7207 = ORIENTED_EDGE ( 'NONE', *, *, #94401, .F. ) ;
#7208 = VERTEX_POINT ( 'NONE', #173772 ) ;
#7209 = CARTESIAN_POINT ( 'NONE',  ( -20.54999999999999716, -7.079251802663311111, -212.6676826711374417 ) ) ;
#7210 = CARTESIAN_POINT ( 'NONE',  ( 20.94999999999999929, -12.41227409413852811, -97.50000000000004263 ) ) ;
#7212 = ORIENTED_EDGE ( 'NONE', *, *, #239908, .F. ) ;
#7211 = FACE_OUTER_BOUND ( 'NONE', #182132, .T. ) ;
#7213 = EDGE_CURVE ( 'NONE', #17135, #257228, #18497, .T. ) ;
#7214 = EDGE_CURVE ( 'NONE', #178016, #18401, #152930, .T. ) ;
#7215 = CARTESIAN_POINT ( 'NONE',  ( 20.93302460841142931, 65.68434038414356735, -97.48668807260655456 ) ) ;
#7217 = ORIENTED_EDGE ( 'NONE', *, *, #95506, .F. ) ;
#7216 = CARTESIAN_POINT ( 'NONE',  ( 21.14999999999999858, 69.35000000001259934, -191.2731074845243882 ) ) ;
#7218 = DIRECTION ( 'NONE',  ( 0.000000000000000000, -0.000000000000000000, -1.000000000000000000 ) ) ;
#7219 = EDGE_CURVE ( 'NONE', #156105, #99760, #132046, .T. ) ;
#7221 = CARTESIAN_POINT ( 'NONE',  ( -18.59999999999999787, 64.25000000001199396, -115.2731074845243739 ) ) ;
#7220 = VECTOR ( 'NONE', #75345, 1000.000000000000000 ) ;
#7223 = ORIENTED_EDGE ( 'NONE', *, *, #194295, .T. ) ;
#7222 = SPHERICAL_SURFACE ( 'NONE', #23073, 0.1000000000000000056 ) ;
#7224 = DIRECTION ( 'NONE',  ( 0.000000000000000000, 0.000000000000000000, 1.000000000000000000 ) ) ;
#7225 = CARTESIAN_POINT ( 'NONE',  ( -21.33487959338958362, 33.90926806716008457, -243.4133681147159223 ) ) ;
#7226 = CARTESIAN_POINT ( 'NONE',  ( -16.97683809663752186, 9.950000000011138823, -113.9023640181965220 ) ) ;
#7227 = AXIS2_PLACEMENT_3D ( 'NONE', #69301, #9308, #124140 ) ;
#7228 = DIRECTION ( 'NONE',  ( 4.336808689942128965E-15, -0.8660254037844367092, 0.5000000000000037748 ) ) ;
#7229 = DIRECTION ( 'NONE',  ( -0.000000000000000000, -6.982962677686266711E-15, 1.000000000000000000 ) ) ;
#7230 = CARTESIAN_POINT ( 'NONE',  ( 23.14999999999999503, 6.450000000011156587, -88.15000000000004832 ) ) ;
#7231 = AXIS2_PLACEMENT_3D ( 'NONE', #246042, #67396, #189916 ) ;
#7232 = VECTOR ( 'NONE', #136462, 1000.000000000000000 ) ;
#7233 = DIRECTION ( 'NONE',  ( -1.000000000000000000, 0.000000000000000000, -0.000000000000000000 ) ) ;
#7234 = CARTESIAN_POINT ( 'NONE',  ( 23.40000000000005542, 64.25000000001119815, -43.82310748452479743 ) ) ;
#7235 = VERTEX_POINT ( 'NONE', #177601 ) ;
#7236 = ORIENTED_EDGE ( 'NONE', *, *, #91337, .F. ) ;
#7237 = VERTEX_POINT ( 'NONE', #254503 ) ;
#7238 = CARTESIAN_POINT ( 'NONE',  ( 20.94999999999999574, 1.749999999999999778, -11.66951155790164485 ) ) ;
#7239 = CARTESIAN_POINT ( 'NONE',  ( 18.59999999999999076, 5.950000000011100632, -177.8057023050348278 ) ) ;
#7240 = AXIS2_PLACEMENT_3D ( 'NONE', #191657, #76799, #194213 ) ;
#7242 = EDGE_LOOP ( 'NONE', ( #166260, #234593, #62337 ) ) ;
#7241 = ADVANCED_FACE ( 'NONE', ( #19794 ), #74659, .T. ) ;
#7243 = CARTESIAN_POINT ( 'NONE',  ( 20.94999999999999574, 77.34908441863862549, -61.53660852097883804 ) ) ;
#7244 = ORIENTED_EDGE ( 'NONE', *, *, #66500, .T. ) ;
#7245 = EDGE_CURVE ( 'NONE', #171611, #9569, #123682, .T. ) ;
#7246 = AXIS2_PLACEMENT_3D ( 'NONE', #244605, #183368, #7275 ) ;
#7247 = CARTESIAN_POINT ( 'NONE',  ( -18.59999999999999787, 10.33248238083634440, -72.59484654391314962 ) ) ;
#7249 = EDGE_CURVE ( 'NONE', #34228, #126961, #138408, .T. ) ;
#7248 = ORIENTED_EDGE ( 'NONE', *, *, #16628, .F. ) ;
#7250 = CARTESIAN_POINT ( 'NONE',  ( 13.88638282980484462, 9.457426452500058645, -152.5000418684000749 ) ) ;
#7251 =( LENGTH_UNIT ( ) NAMED_UNIT ( * ) SI_UNIT ( .MILLI., .METRE. ) );
#7252 = B_SPLINE_CURVE_WITH_KNOTS ( 'NONE', 3,
 ( #65958, #243294, #103769, #125915, #145485, #184613, #5958, #85476, #205451, #146742, #102479, #26860, #106338, #7250, #3396, #204165, #185898, #162509, #25560, #62114, #86782, #187210, #127217, #107646, #43832, #141637, #223727, #142896, #88054, #202896 ),
 .UNSPECIFIED., .F., .F.,
 ( 4, 2, 2, 2, 2, 2, 2, 2, 2, 2, 2, 2, 2, 2, 4 ),
 ( 0.000000000000000000, 0.0003422764154113113887, 0.0006845528308226227774, 0.001026829246233936172, 0.001369105661645249458, 0.002053658492467934794, 0.002738211323290619913, 0.003080487738701959653, 0.003422764154113299394, 0.003765040569524640002, 0.004107316984935979742, 0.004449593400347319483, 0.004791869815758659223, 0.005134146231169999831, 0.005476422646581339572 ),
 .UNSPECIFIED. ) ;
#7253 = VECTOR ( 'NONE', #109318, 1000.000000000000000 ) ;
#7254 = ORIENTED_EDGE ( 'NONE', *, *, #146256, .T. ) ;
#7255 = ORIENTED_EDGE ( 'NONE', *, *, #152151, .F. ) ;
#7256 = VECTOR ( 'NONE', #184514, 1000.000000000000000 ) ;
#7257 = VERTEX_POINT ( 'NONE', #217950 ) ;
#7259 = DIRECTION ( 'NONE',  ( -0.000000000000000000, 6.982962677686266711E-15, -1.000000000000000000 ) ) ;
#7258 = AXIS2_PLACEMENT_3D ( 'NONE', #99228, #79667, #159246 ) ;
#7260 = CARTESIAN_POINT ( 'NONE',  ( 20.94999999999999929, 4.252251777740766236, -211.8999245327126744 ) ) ;
#7261 = FACE_OUTER_BOUND ( 'NONE', #253176, .T. ) ;
#7262 = VECTOR ( 'NONE', #228795, 1000.000000000000000 ) ;
#7263 = DIRECTION ( 'NONE',  ( 0.000000000000000000, 1.000000000000000000, 6.982962677686266711E-15 ) ) ;
#7264 = DIRECTION ( 'NONE',  ( 1.000000000000000000, 0.000000000000000000, 0.000000000000000000 ) ) ;
#7265 = AXIS2_PLACEMENT_3D ( 'NONE', #241260, #122598, #142137 ) ;
#7266 = CARTESIAN_POINT ( 'NONE',  ( -18.59999999999999787, 85.32100840337392356, -196.2871692354464130 ) ) ;
#7268 = CARTESIAN_POINT ( 'NONE',  ( 21.05000000000000071, 23.68770167995059239, -252.8127582590406348 ) ) ;
#7267 = FACE_OUTER_BOUND ( 'NONE', #8250, .T. ) ;
#7269 = CARTESIAN_POINT ( 'NONE',  ( 18.59999999999999432, -1.162701749938009677, -8.099999999999999645 ) ) ;
#7271 = ORIENTED_EDGE ( 'NONE', *, *, #144629, .F. ) ;
#7270 = CARTESIAN_POINT ( 'NONE',  ( -20.89878130938411616, 10.32747123227773045, -139.5774032850249569 ) ) ;
#7273 = DIRECTION ( 'NONE',  ( 0.2834754621636358940, 0.2834754621636501049, -0.9161240771326873977 ) ) ;
#7272 = LINE ( 'NONE', #176648, #234115 ) ;
#7274 = CIRCLE ( 'NONE', #186362, 6.258578643762696458 ) ;
#7275 = DIRECTION ( 'NONE',  ( 0.000000000000000000, 1.000000000000000000, 0.000000000000000000 ) ) ;
#7276 = ORIENTED_EDGE ( 'NONE', *, *, #119630, .F. ) ;
#7277 = CARTESIAN_POINT ( 'NONE',  ( 20.94999999999999574, 10.47338541491290442, -7.578654464248542943 ) ) ;
#7278 = DIRECTION ( 'NONE',  ( 1.000000000000000000, 0.000000000000000000, 0.000000000000000000 ) ) ;
#7280 = ADVANCED_FACE ( 'NONE', ( #99288 ), #178892, .F. ) ;
#7279 = CARTESIAN_POINT ( 'NONE',  ( -20.85000000000000142, -11.64999999998884483, -100.5000000000000426 ) ) ;
#7281 = VERTEX_POINT ( 'NONE', #135851 ) ;
#7282 = CARTESIAN_POINT ( 'NONE',  ( 18.59999999999999076, 10.49142135623730709, -24.85000000000000142 ) ) ;
#7283 = EDGE_CURVE ( 'NONE', #197466, #36195, #28019, .T. ) ;
#7284 = VECTOR ( 'NONE', #81931, 1000.000000000000114 ) ;
#7285 = DIRECTION ( 'NONE',  ( -1.000000000000000000, 0.000000000000000000, 0.000000000000000000 ) ) ;
#7286 = LINE ( 'NONE', #43862, #1067 ) ;
#7287 = AXIS2_PLACEMENT_3D ( 'NONE', #64117, #48391, #67962 ) ;
#7289 = VERTEX_POINT ( 'NONE', #79722 ) ;
#7288 = VECTOR ( 'NONE', #159658, 1000.000000000000000 ) ;
#7290 = EDGE_LOOP ( 'NONE', ( #8172, #210937, #256248, #219610 ) ) ;
#7291 = EDGE_CURVE ( 'NONE', #155707, #211751, #255774, .T. ) ;
#7293 = ADVANCED_FACE ( 'NONE', ( #214130 ), #137153, .F. ) ;
#7292 = CARTESIAN_POINT ( 'NONE',  ( 21.05000000000000071, 36.65892442174935439, -249.5511627012433848 ) ) ;
#7294 = ORIENTED_EDGE ( 'NONE', *, *, #240733, .T. ) ;
#7295 = FACE_OUTER_BOUND ( 'NONE', #254168, .T. ) ;
#7296 = CARTESIAN_POINT ( 'NONE',  ( 23.24999999999999645, 8.822561741677553471, -79.65000000000004832 ) ) ;
#7297 = CARTESIAN_POINT ( 'NONE',  ( 18.59999999999999076, 69.55000000001261640, -193.5060803140843859 ) ) ;
#7298 = FACE_OUTER_BOUND ( 'NONE', #47441, .T. ) ;
#7299 = ORIENTED_EDGE ( 'NONE', *, *, #21953, .F. ) ;
#7300 = EDGE_CURVE ( 'NONE', #15679, #53074, #219248, .T. ) ;
#7301 = FACE_OUTER_BOUND ( 'NONE', #204662, .T. ) ;
#7302 = AXIS2_PLACEMENT_3D ( 'NONE', #162830, #44157, #140674 ) ;
#7303 = CARTESIAN_POINT ( 'NONE',  ( -21.05000000000000071, 1.162701749949165642, -142.1000000000000227 ) ) ;
#7304 = AXIS2_PLACEMENT_3D ( 'NONE', #225617, #226931, #207388 ) ;
#7305 = DIRECTION ( 'NONE',  ( 0.000000000000000000, 0.000000000000000000, -1.000000000000000000 ) ) ;
#7306 = PLANE ( 'NONE',  #207492 ) ;
#7307 = CIRCLE ( 'NONE', #248938, 0.09999999999999967248 ) ;
#7308 = EDGE_CURVE ( 'NONE', #193539, #85480, #44490, .T. ) ;
#7309 = ORIENTED_EDGE ( 'NONE', *, *, #165586, .F. ) ;
#7311 = EDGE_CURVE ( 'NONE', #210821, #188126, #102796, .T. ) ;
#7310 = CARTESIAN_POINT ( 'NONE',  ( -20.85000000000000142, 11.65000000001115232, -60.21613433702190576 ) ) ;
#7312 = AXIS2_PLACEMENT_3D ( 'NONE', #21356, #56565, #254752 ) ;
#7314 = ORIENTED_EDGE ( 'NONE', *, *, #157983, .F. ) ;
#7313 = CARTESIAN_POINT ( 'NONE',  ( -18.59999999999999787, 44.10700160683882132, -235.9691471569721841 ) ) ;
#7315 = DIRECTION ( 'NONE',  ( 0.000000000000000000, -1.000000000000000000, -6.982962677686266711E-15 ) ) ;
#7316 = CYLINDRICAL_SURFACE ( 'NONE', #164223, 4.049999999999998046 ) ;
#7317 = CARTESIAN_POINT ( 'NONE',  ( 18.54999999999999716, 8.750000000011173285, -146.6500000000000341 ) ) ;
#7318 = EDGE_CURVE ( 'NONE', #149564, #18045, #245255, .T. ) ;
#7319 = LINE ( 'NONE', #86836, #187831 ) ;
#7320 = DIRECTION ( 'NONE',  ( 0.000000000000000000, 0.8814952561688437216, -0.4721928772777334582 ) ) ;
#7321 = AXIS2_PLACEMENT_3D ( 'NONE', #107219, #66819, #47231 ) ;
#7322 = DIRECTION ( 'NONE',  ( 0.000000000000000000, 0.06835365183351375939, -0.9976611540402997580 ) ) ;
#7323 = DIRECTION ( 'NONE',  ( 0.000000000000000000, -0.4088369013363280513, 0.9126074666063769270 ) ) ;
#7325 = VERTEX_POINT ( 'NONE', #45756 ) ;
#7324 = AXIS2_PLACEMENT_3D ( 'NONE', #133229, #212776, #41854 ) ;
#7326 = DIRECTION ( 'NONE',  ( 1.000000000000000000, -0.000000000000000000, -0.000000000000000000 ) ) ;
#7327 = DIRECTION ( 'NONE',  ( 1.000000000000000000, 0.000000000000000000, 0.000000000000000000 ) ) ;
#7328 = CIRCLE ( 'NONE', #90515, 0.09999999999999939493 ) ;
#7329 = CIRCLE ( 'NONE', #61503, 0.09999999999999638345 ) ;
#7330 = CARTESIAN_POINT ( 'NONE',  ( 21.13736287352038445, 12.29923930194942372, -219.6601089527135571 ) ) ;
#7331 = CIRCLE ( 'NONE', #128147, 0.09999999999999939493 ) ;
#7332 = EDGE_CURVE ( 'NONE', #8702, #160911, #181931, .T. ) ;
#7333 = CARTESIAN_POINT ( 'NONE',  ( 20.94999999999999929, 1.115600667400684642E-11, -67.00000000000000000 ) ) ;
#7334 = CARTESIAN_POINT ( 'NONE',  ( 20.94999999999999574, 77.34908441863935025, -162.0366085209788594 ) ) ;
#7335 = AXIS2_PLACEMENT_3D ( 'NONE', #132620, #110476, #33562 ) ;
#7336 = VERTEX_POINT ( 'NONE', #22367 ) ;
#7337 = ORIENTED_EDGE ( 'NONE', *, *, #135925, .T. ) ;
#7338 = DIRECTION ( 'NONE',  ( 0.000000000000000000, 1.000000000000000000, 6.982962677686266711E-15 ) ) ;
#7339 = ADVANCED_FACE ( 'NONE', ( #199722 ), #82128, .F. ) ;
#7340 = DIRECTION ( 'NONE',  ( 1.000000000000000000, 0.000000000000000000, 0.000000000000000000 ) ) ;
#7341 = CARTESIAN_POINT ( 'NONE',  ( 18.49999999999999289, 18.34711819382569686, -236.8747682978092541 ) ) ;
#7343 = EDGE_CURVE ( 'NONE', #126029, #74752, #223596, .T. ) ;
#7342 = DIRECTION ( 'NONE',  ( -1.000000000000000000, 0.000000000000000000, 0.000000000000000000 ) ) ;
#7344 = EDGE_CURVE ( 'NONE', #222829, #40059, #2761, .T. ) ;
#7345 = CARTESIAN_POINT ( 'NONE',  ( 21.95218792049437795, 7.201507561246661915, 0.09902843979991737822 ) ) ;
#7346 = VECTOR ( 'NONE', #50037, 1000.000000000000114 ) ;
#7347 = LINE ( 'NONE', #167735, #42360 ) ;
#7348 = DIRECTION ( 'NONE',  ( 1.186688945009010077E-16, 1.000000000000000000, 6.982962677686266711E-15 ) ) ;
#7349 = AXIS2_PLACEMENT_3D ( 'NONE', #218075, #139829, #39499 ) ;
#7350 = ORIENTED_EDGE ( 'NONE', *, *, #60333, .F. ) ;
#7351 = LINE ( 'NONE', #68620, #60898 ) ;
#7352 = ORIENTED_EDGE ( 'NONE', *, *, #149701, .F. ) ;
#7353 = ADVANCED_FACE ( 'NONE', ( #66614 ), #90336, .T. ) ;
#7354 = DIRECTION ( 'NONE',  ( 0.000000000000000000, 0.6728971962617483760, -0.7397360091702162022 ) ) ;
#7355 = CARTESIAN_POINT ( 'NONE',  ( -18.59999999999999787, 76.00000000001142553, -36.02310748452432421 ) ) ;
#7356 = CARTESIAN_POINT ( 'NONE',  ( 18.59999999999996945, 65.66751761918648356, -63.92826094061123143 ) ) ;
#7357 = CYLINDRICAL_SURFACE ( 'NONE', #240400, 0.09999999999999939493 ) ;
#7358 = DIRECTION ( 'NONE',  ( 0.000000000000000000, 0.000000000000000000, 1.000000000000000000 ) ) ;
#7359 = CARTESIAN_POINT ( 'NONE',  ( -21.64999999999999858, 7.250000000011148416, -155.2500000000000284 ) ) ;
#7360 = CARTESIAN_POINT ( 'NONE',  ( -18.34374000495060386, 20.70020979027691155, -227.9869476361872103 ) ) ;
#7361 = CARTESIAN_POINT ( 'NONE',  ( -20.85000000000000142, 78.45218979564165807, -232.7313097695096076 ) ) ;
#7362 = LINE ( 'NONE', #116736, #167353 ) ;
#7363 = DIRECTION ( 'NONE',  ( 0.000000000000000000, 0.9594490217226103734, 0.2818822000686205254 ) ) ;
#7364 = CARTESIAN_POINT ( 'NONE',  ( 18.49505816908823874, -9.437872553211134274, -40.27765720167089114 ) ) ;
#7365 = CIRCLE ( 'NONE', #199096, 0.09999999999999939493 ) ;
#7366 = AXIS2_PLACEMENT_3D ( 'NONE', #88416, #148434, #227959 ) ;
#7367 = DIRECTION ( 'NONE',  ( -1.000000000000000000, -2.952720810173289112E-16, 0.000000000000000000 ) ) ;
#7368 = CARTESIAN_POINT ( 'NONE',  ( -20.54999999999999716, -8.730841121484170131, -57.40192528101567149 ) ) ;
#7369 = ORIENTED_EDGE ( 'NONE', *, *, #104750, .F. ) ;
#7370 = LINE ( 'NONE', #204278, #172996 ) ;
#7371 = CARTESIAN_POINT ( 'NONE',  ( -23.25000000000000000, 76.00000000001170974, -69.52310748452431710 ) ) ;
#7372 = EDGE_CURVE ( 'NONE', #156337, #14506, #115466, .T. ) ;
#7373 = ORIENTED_EDGE ( 'NONE', *, *, #204842, .T. ) ;
#7374 = FACE_OUTER_BOUND ( 'NONE', #27606, .T. ) ;
#7375 = CARTESIAN_POINT ( 'NONE',  ( 21.04105312098486635, 11.29556661886501523, -211.1574496082819792 ) ) ;
#7376 = CARTESIAN_POINT ( 'NONE',  ( 23.14999999999999503, 6.649999999999999467, -21.35000000000000142 ) ) ;
#7377 = ORIENTED_EDGE ( 'NONE', *, *, #142662, .F. ) ;
#7378 = VECTOR ( 'NONE', #12927, 1000.000000000000000 ) ;
#7379 = CARTESIAN_POINT ( 'NONE',  ( 21.05000000000000071, -8.730841121484166578, -57.40192528101567149 ) ) ;
#7380 = DIRECTION ( 'NONE',  ( -1.000000000000000000, -0.000000000000000000, 0.000000000000000000 ) ) ;
#7381 = AXIS2_PLACEMENT_3D ( 'NONE', #14124, #233178, #149789 ) ;
#7382 = ADVANCED_FACE ( 'NONE', ( #5315 ), #21091, .F. ) ;
#7383 = ORIENTED_EDGE ( 'NONE', *, *, #151531, .F. ) ;
#7384 = CIRCLE ( 'NONE', #153185, 0.09999999999999939493 ) ;
#7385 = DIRECTION ( 'NONE',  ( -1.000000000000000000, 0.000000000000000000, 0.000000000000000000 ) ) ;
#7386 = ORIENTED_EDGE ( 'NONE', *, *, #155654, .F. ) ;
#7387 = CARTESIAN_POINT ( 'NONE',  ( -18.59999999999999787, 66.65000000001253966, -182.2731074845244166 ) ) ;
#7388 = PLANE ( 'NONE',  #183294 ) ;
#7389 = CARTESIAN_POINT ( 'NONE',  ( -23.25000000000000000, 77.83585931145498193, -24.51866831572578675 ) ) ;
#7390 = DIRECTION ( 'NONE',  ( -1.462545276649575732E-15, 0.1686199900910455851, -0.9856811345164804283 ) ) ;
#7391 = CARTESIAN_POINT ( 'NONE',  ( -16.83558968593882454, 66.05000000001230376, -157.3608022969076785 ) ) ;
#7392 = DIRECTION ( 'NONE',  ( 1.000000000000000000, 0.000000000000000000, 0.000000000000000000 ) ) ;
#7393 = DIRECTION ( 'NONE',  ( -1.000000000000000000, -0.000000000000000000, -0.000000000000000000 ) ) ;
#7394 = CYLINDRICAL_SURFACE ( 'NONE', #103913, 0.9000000000000014655 ) ;
#7396 = ORIENTED_EDGE ( 'NONE', *, *, #161251, .T. ) ;
#7395 = CARTESIAN_POINT ( 'NONE',  ( 18.46163235739475894, 86.89227388589759471, -199.5790731264802105 ) ) ;
#7397 = EDGE_LOOP ( 'NONE', ( #70818, #194925, #149759, #111299 ) ) ;
#7399 = CARTESIAN_POINT ( 'NONE',  ( -15.15564720441980739, 9.410708747058238899, -85.06920840584416510 ) ) ;
#7398 = FACE_BOUND ( 'NONE', #133633, .T. ) ;
#7400 = EDGE_LOOP ( 'NONE', ( #84665, #242052, #79957, #241776, #151890 ) ) ;
#7401 = AXIS2_PLACEMENT_3D ( 'NONE', #71744, #147411, #151279 ) ;
#7402 = ORIENTED_EDGE ( 'NONE', *, *, #234234, .F. ) ;
#7403 = CARTESIAN_POINT ( 'NONE',  ( 23.14999999999999858, 1.115600667400684642E-11, -100.5000000000000426 ) ) ;
#7405 = CYLINDRICAL_SURFACE ( 'NONE', #234567, 0.09999999999999939493 ) ;
#7404 = TOROIDAL_SURFACE ( 'NONE', #7800, 1.900000000000002576, 0.1000000000000000056 ) ;
#7406 = CARTESIAN_POINT ( 'NONE',  ( 21.14999999999999503, 1.115600667400684642E-11, -60.75000000000004974 ) ) ;
#7407 = CARTESIAN_POINT ( 'NONE',  ( 21.05000000000005400, 79.78873604695631627, -7.297728304630792806 ) ) ;
#7409 = CARTESIAN_POINT ( 'NONE',  ( 22.39999999999999503, 64.35000000001194564, -102.9231074845243938 ) ) ;
#7408 = VECTOR ( 'NONE', #60561, 1000.000000000000114 ) ;
#7410 = DIRECTION ( 'NONE',  ( 0.000000000000000000, 0.8777080977375072424, -0.4791956752371691608 ) ) ;
#7411 = ADVANCED_FACE ( 'NONE', ( #142284 ), #104421, .T. ) ;
#7413 = CIRCLE ( 'NONE', #211441, 0.1000000000000111355 ) ;
#7412 = CARTESIAN_POINT ( 'NONE',  ( -20.54999999999999716, 11.58468387039766512, -220.1227639117171861 ) ) ;
#7414 = ORIENTED_EDGE ( 'NONE', *, *, #221548, .F. ) ;
#7415 = EDGE_LOOP ( 'NONE', ( #78036, #87031, #93136, #49487 ) ) ;
#7416 = CARTESIAN_POINT ( 'NONE',  ( -23.25000000000000000, -11.65000000000000036, -30.39999999999999858 ) ) ;
#7417 = VECTOR ( 'NONE', #132201, 1000.000000000000000 ) ;
#7418 = AXIS2_PLACEMENT_3D ( 'NONE', #105013, #85457, #102456 ) ;
#7419 = ORIENTED_EDGE ( 'NONE', *, *, #156101, .F. ) ;
#7420 = PLANE ( 'NONE',  #84336 ) ;
#7421 = ORIENTED_EDGE ( 'NONE', *, *, #196813, .T. ) ;
#7423 = CARTESIAN_POINT ( 'NONE',  ( -16.87683809663752399, 9.864913447291341342, -154.2242815513039318 ) ) ;
#7422 = VECTOR ( 'NONE', #116765, 1000.000000000000000 ) ;
#7424 = AXIS2_PLACEMENT_3D ( 'NONE', #22645, #23933, #160865 ) ;
#7425 = DIRECTION ( 'NONE',  ( 0.000000000000000000, 0.000000000000000000, -1.000000000000000000 ) ) ;
#7426 = EDGE_CURVE ( 'NONE', #79795, #171400, #40507, .T. ) ;
#7427 = AXIS2_PLACEMENT_3D ( 'NONE', #54105, #193630, #15007 ) ;
#7428 = LINE ( 'NONE', #166544, #160863 ) ;
#7429 = CARTESIAN_POINT ( 'NONE',  ( -21.08035267497491816, 75.91731137523670725, -209.8548143243074264 ) ) ;
#7430 = ORIENTED_EDGE ( 'NONE', *, *, #10859, .F. ) ;
#7431 = APPLICATION_CONTEXT ( 'automotive_design' ) ;
#7432 = LINE ( 'NONE', #28329, #25634 ) ;
#7433 = ORIENTED_EDGE ( 'NONE', *, *, #233434, .F. ) ;
#7434 = EDGE_CURVE ( 'NONE', #147282, #2878, #15547, .T. ) ;
#7435 = DIRECTION ( 'NONE',  ( 1.000000000000000000, 1.186688945009010077E-16, 0.000000000000000000 ) ) ;
#7436 = LINE ( 'NONE', #12607, #73274 ) ;
#7437 = DIRECTION ( 'NONE',  ( 0.000000000000000000, 0.000000000000000000, 1.000000000000000000 ) ) ;
#7438 = CARTESIAN_POINT ( 'NONE',  ( 21.00000000000000000, 9.750000000011153745, -146.2500000000000284 ) ) ;
#7439 = ORIENTED_EDGE ( 'NONE', *, *, #26708, .F. ) ;
#7440 = CARTESIAN_POINT ( 'NONE',  ( -21.64999999999999858, 7.350000000011155166, -45.85000000000000142 ) ) ;
#7442 = EDGE_CURVE ( 'NONE', #171697, #210883, #219514, .T. ) ;
#7441 = VECTOR ( 'NONE', #223820, 1000.000000000000000 ) ;
#7443 = VERTEX_POINT ( 'NONE', #225648 ) ;
#7446 = ORIENTED_EDGE ( 'NONE', *, *, #221006, .T. ) ;
#7445 = LINE ( 'NONE', #126099, #93043 ) ;
#7444 = CARTESIAN_POINT ( 'NONE',  ( 18.43473516226031350, 46.97094695037121426, -255.3356945386573500 ) ) ;
#7447 = DIRECTION ( 'NONE',  ( 1.000000000000000000, 0.000000000000000000, 0.000000000000000000 ) ) ;
#7448 = AXIS2_PLACEMENT_3D ( 'NONE', #13607, #74890, #211811 ) ;
#7449 = EDGE_LOOP ( 'NONE', ( #81686, #132579, #171907, #9699 ) ) ;
#7450 = AXIS2_PLACEMENT_3D ( 'NONE', #220181, #96354, #136775 ) ;
#7451 = DIRECTION ( 'NONE',  ( 1.000000000000000000, -0.000000000000000000, -0.000000000000000000 ) ) ;
#7452 = VERTEX_POINT ( 'NONE', #4060 ) ;
#7453 = CIRCLE ( 'NONE', #69839, 0.09999999999999459321 ) ;
#7454 = VECTOR ( 'NONE', #213670, 1000.000000000000000 ) ;
#7456 = CARTESIAN_POINT ( 'NONE',  ( 22.60000000000000142, 0.1008583691098682150, -155.7504328765105868 ) ) ;
#7455 =( BOUNDED_CURVE ( )  B_SPLINE_CURVE ( 3, ( #37478, #119587, #118292, #40065 ),
 .UNSPECIFIED., .F., .F. ) 
 B_SPLINE_CURVE_WITH_KNOTS ( ( 4, 4 ),
 ( 3.192897208853993085, 4.712388980384689674 ),
 .UNSPECIFIED. ) 
 CURVE ( )  GEOMETRIC_REPRESENTATION_ITEM ( )  RATIONAL_B_SPLINE_CURVE ( ( 1.000000000000000000, 0.8166740347213228279, 0.8166740347213228279, 1.000000000000000000 ) ) 
 REPRESENTATION_ITEM ( '' )  );
#7457 = TOROIDAL_SURFACE ( 'NONE', #11581, 1.900000000000002576, 0.1000000000000000056 ) ;
#7458 = ADVANCED_FACE ( 'NONE', ( #81011 ), #236093, .F. ) ;
#7459 = CYLINDRICAL_SURFACE ( 'NONE', #21907, 7.900000000000003908 ) ;
#7460 = CARTESIAN_POINT ( 'NONE',  ( 23.15000000000000213, 69.09936979046463534, -247.6075824278584605 ) ) ;
#7461 = CARTESIAN_POINT ( 'NONE',  ( -23.15000000000000213, -11.64999999998884483, -97.40000000000004832 ) ) ;
#7462 = ADVANCED_FACE ( 'NONE', ( #65316 ), #200985, .T. ) ;
#7463 = ORIENTED_EDGE ( 'NONE', *, *, #65270, .T. ) ;
#7464 = CARTESIAN_POINT ( 'NONE',  ( 22.59999999999999787, 12.54152817314149715, -223.4164406214577241 ) ) ;
#7465 = CARTESIAN_POINT ( 'NONE',  ( -17.11825945287481332, 10.05000000001113847, -188.2499999999999716 ) ) ;
#7466 = CARTESIAN_POINT ( 'NONE',  ( 21.07933241753356768, 6.328645948390905218, -33.40662040958070378 ) ) ;
#7467 = VECTOR ( 'NONE', #160895, 1000.000000000000000 ) ;
#7468 = VERTEX_POINT ( 'NONE', #92575 ) ;
#7469 = LINE ( 'NONE', #23217, #88631 ) ;
#7471 = VERTEX_POINT ( 'NONE', #130426 ) ;
#7470 = AXIS2_PLACEMENT_3D ( 'NONE', #79898, #219424, #95634 ) ;
#7472 = CARTESIAN_POINT ( 'NONE',  ( 21.12230431290518951, 30.76357089822023738, -252.1864996923993090 ) ) ;
#7473 = CLOSED_SHELL ( 'NONE', ( #248885, #156414, #244097, #97757, #22956, #208919, #163552, #115611, #128513, #20482, #79103, #161161, #95090, #167472, #89690, #82642, #179085, #74440, #186703, #168736, #203307, #66624, #54874, #228346, #36670, #238368, #255410, #211723, #115822, #193030, #212788, #213699, #83286, #184157, #48220, #53750, #167890, #150883, #171546, #169532, #209817, #5879, #217750, #153821, #216971, #158966, #51866, #239319, #127587, #11398, #165897, #2735, #96949, #64419, #44432, #227744, #213742, #56756, #152634, #167641, #152498, #161909, #170310, #41104, #196591, #104612, #37233, #123844, #88546, #113577, #36664, #47110, #189584, #134233, #97413, #84253, #22281, #70956, #107079, #50697, #1198, #122288, #58992, #245621, #104360, #248476, #178154, #231636, #26161, #226587, #253427, #88233, #148447, #119349, #163257, #163642, #180957, #249779, #51597, #173773, #82026, #40640, #153162, #253389, #79996, #221027, #117648, #61388, #20198, #205341, #221074, #91165, #27798, #98125, #169736, #21901, #21705, #131556, #210470, #139399, #169780, #125076, #27325, #213547, #54693, #10276, #82346, #58343, #41440, #169140, #90464, #7174, #157496, #68792, #70942, #157947, #195589, #20870, #107861, #81487, #108059, #181989, #229986, #10007, #13095, #26343, #256694, #126533, #91082, #163700, #87103, #50801, #193783, #111873, #101780, #202442, #205758, #123410, #254584, #232703, #240505, #77480, #247807, #131998, #87378, #76048, #231024, #255054, #178590, #206666, #249933, #167217, #62603, #113456, #187102, #218937, #31649, #120373, #130451, #8486, #230779, #247881, #170108, #98914, #124471, #83346, #143041, #6112, #54258, #116219, #196245, #57068, #180015, #246284, #52886, #240024, #33277, #257168, #96125, #39393, #152065, #121553, #177485, #214379, #37050, #30316, #151286, #241006, #42079, #5529, #244444, #202400, #15305, #218634, #162274, #95022, #250578, #190909, #122773, #197635, #105707, #66491, #220114, #177762, #116179, #139393, #49792, #130294, #156854, #85360, #45781, #144378, #224790, #10393, #130395, #231648, #144928, #164652, #78712, #134803, #186395, #86637, #101620, #227166, #122713, #130755, #234876, #106111, #110559, #60449, #175163, #36009, #113315, #109525, #247787, #18263, #113891, #249920, #165752, #19661, #236594, #103885, #63105, #171669, #68743, #54862, #161817, #154221, #33155, #220445, #64429, #119918, #13742, #682, #6359, #152609, #23891, #74932, #32022, #14388, #115443, #53493, #211302, #35276, #237872, #22056, #33483, #39033, #84230, #108368, #235239, #183872, #165561, #197201, #150429, #48363, #145125, #64595, #46240, #57683, #197619, #194427, #130631, #80502, #218108, #108964, #102539, #67372, #47246, #255718, #216859, #97465, #126175, #208849, #63711, #235441, #237090, #3888, #114191, #75100, #245632, #228479, #100017, #158358, #48746, #111914, #251843, #190650, #98160, #69593, #216033, #55884, #64324, #44369, #201520, #115973, #77974, #108557, #83498, #168209, #118074, #156551, #66160, #45105, #121021, #201283, #64923, #45927, #183542, #56022, #213659, #122521, #227628, #141409, #78823, #7860, #60080, #207292, #228038, #252030, #105160, #82536, #161324, #252203, #196560, #252154, #55212, #253736, #65462, #225786, #224788, #207254, #71994, #143714, #232264, #42780, #24963, #13677, #194319, #257383, #94688, #180730, #38967, #74800, #248150, #208873, #49819, #151052, #248092, #224140, #145369, #241968, #243107, #184472, #26617, #196780, #217830, #248179, #145882, #242479, #143879, #251826, #224097, #211204, #169847, #157538, #49580, #180380, #147974, #4877, #193041, #126973, #161778, #232706, #55479, #254707, #80554, #33975, #188953, #192402, #137724, #239598, #58131, #155965, #101770, #87213, #175398, #95852, #3993, #75598, #21310, #28114, #128200, #20624, #46907, #40933, #65630, #2891, #71870, #196097, #81096, #59018, #21188, #64038, #158882, #84548, #51079, #189593, #202061, #63530, #167732, #7708, #169382, #254526, #127782, #78449, #176835, #218620, #228760, #121459, #233256, #184993, #156399, #49495, #72358, #23124, #226657, #95892, #45473, #173413, #63574, #26788, #23456, #65135, #230694, #78561, #123011, #82016 ) ) ;
#7474 = DIRECTION ( 'NONE',  ( 1.000000000000000000, -0.000000000000000000, -0.000000000000000000 ) ) ;
#7475 = DIRECTION ( 'NONE',  ( 0.000000000000000000, -0.2128009952263603677, 0.9770955615653313941 ) ) ;
#7477 = ORIENTED_EDGE ( 'NONE', *, *, #146192, .T. ) ;
#7476 = DIRECTION ( 'NONE',  ( 0.000000000000000000, -6.982962677686266711E-15, 1.000000000000000000 ) ) ;
#7478 = DIRECTION ( 'NONE',  ( -0.000000000000000000, -0.9126074666063769270, -0.4088369013363283844 ) ) ;
#7479 = EDGE_CURVE ( 'NONE', #192382, #106895, #229546, .T. ) ;
#7480 = LINE ( 'NONE', #186123, #235874 ) ;
#7481 = VECTOR ( 'NONE', #101192, 1000.000000000000000 ) ;
#7482 = DIRECTION ( 'NONE',  ( 0.000000000000000000, 1.000000000000000000, -6.308085367188393199E-16 ) ) ;
#7483 = EDGE_LOOP ( 'NONE', ( #54960, #114811, #91244, #151208, #142864 ) ) ;
#7484 = CARTESIAN_POINT ( 'NONE',  ( 22.39999999999999858, 7.790779598384538929, -133.9000000000000057 ) ) ;
#7485 = FACE_OUTER_BOUND ( 'NONE', #186602, .T. ) ;
#7486 = AXIS2_PLACEMENT_3D ( 'NONE', #112548, #178970, #175130 ) ;
#7487 = ORIENTED_EDGE ( 'NONE', *, *, #1783, .T. ) ;
#7488 = FACE_OUTER_BOUND ( 'NONE', #39131, .T. ) ;
#7489 = ORIENTED_EDGE ( 'NONE', *, *, #159553, .F. ) ;
#7490 = CIRCLE ( 'NONE', #136662, 0.1000000000000028644 ) ;
#7491 = ADVANCED_FACE ( 'NONE', ( #88712 ), #172179, .T. ) ;
#7492 = CARTESIAN_POINT ( 'NONE',  ( -21.05000000000000071, 62.92003201576280702, -207.2439188921395896 ) ) ;
#7494 = VERTEX_POINT ( 'NONE', #251663 ) ;
#7493 = DIRECTION ( 'NONE',  ( -1.000000000000000000, 2.775557561562908012E-13, 0.000000000000000000 ) ) ;
#7495 = AXIS2_PLACEMENT_3D ( 'NONE', #191302, #89583, #248672 ) ;
#7496 = ADVANCED_FACE ( 'NONE', ( #246520 ), #208708, .F. ) ;
#7499 = EDGE_LOOP ( 'NONE', ( #227090, #154755 ) ) ;
#7498 = ORIENTED_EDGE ( 'NONE', *, *, #197054, .F. ) ;
#7497 = DIRECTION ( 'NONE',  ( 0.000000000000000000, 0.000000000000000000, 1.000000000000000000 ) ) ;
#7500 = DIRECTION ( 'NONE',  ( 0.000000000000000000, 0.2617529984165152257, 0.9651348961777124202 ) ) ;
#7501 = CIRCLE ( 'NONE', #136674, 11.80000000000000426 ) ;
#7502 = DIRECTION ( 'NONE',  ( 0.000000000000000000, 0.000000000000000000, 1.000000000000000000 ) ) ;
#7503 = CIRCLE ( 'NONE', #140795, 1.749999999999998002 ) ;
#7504 = CARTESIAN_POINT ( 'NONE',  ( -18.50000000000000000, 11.64999999999999680, -12.14999999999999680 ) ) ;
#7505 = AXIS2_PLACEMENT_3D ( 'NONE', #237710, #254659, #136010 ) ;
#7507 = CARTESIAN_POINT ( 'NONE',  ( -12.68215100488889924, 66.60336962369382263, -51.61605009170610003 ) ) ;
#7506 = DIRECTION ( 'NONE',  ( -0.000000000000000000, -0.1298341882519953583, -0.9915357197604862671 ) ) ;
#7509 = EDGE_CURVE ( 'NONE', #26148, #61043, #169504, .T. ) ;
#7508 = LINE ( 'NONE', #30960, #94603 ) ;
#7510 = FACE_OUTER_BOUND ( 'NONE', #154028, .T. ) ;
#7511 = CARTESIAN_POINT ( 'NONE',  ( -16.93658623642890859, 44.08829270366707220, -235.2867806363773866 ) ) ;
#7512 = AXIS2_PLACEMENT_3D ( 'NONE', #116901, #96038, #196427 ) ;
#7513 = EDGE_CURVE ( 'NONE', #243580, #47477, #187861, .T. ) ;
#7514 = DIRECTION ( 'NONE',  ( 1.000000000000000000, -0.000000000000000000, 0.000000000000000000 ) ) ;
#7515 = CARTESIAN_POINT ( 'NONE',  ( -14.00000000000000178, 66.15000000001204228, -119.7731074845243739 ) ) ;
#7516 = VERTEX_POINT ( 'NONE', #127873 ) ;
#7517 = ORIENTED_EDGE ( 'NONE', *, *, #87360, .F. ) ;
#7518 = CARTESIAN_POINT ( 'NONE',  ( -20.99749315643147440, 64.25000000001175238, -76.53791325328415951 ) ) ;
#7520 = VERTEX_POINT ( 'NONE', #27526 ) ;
#7519 = CARTESIAN_POINT ( 'NONE',  ( 13.99999999999999822, 9.850000000011137402, -150.7500000000000284 ) ) ;
#7521 = VERTEX_POINT ( 'NONE', #191725 ) ;
#7522 = CARTESIAN_POINT ( 'NONE',  ( -18.59999999999999787, 77.16270174994990327, -94.92310748452430857 ) ) ;
#7523 = EDGE_CURVE ( 'NONE', #175634, #184179, #74919, .T. ) ;
#7524 = ORIENTED_EDGE ( 'NONE', *, *, #209466, .F. ) ;
#7525 = DIRECTION ( 'NONE',  ( 0.000000000000000000, 1.000000000000000000, 0.000000000000000000 ) ) ;
#7526 = AXIS2_PLACEMENT_3D ( 'NONE', #84636, #144642, #125111 ) ;
#7527 = EDGE_CURVE ( 'NONE', #56398, #72182, #168325, .T. ) ;
#7528 = EDGE_CURVE ( 'NONE', #157387, #18238, #244458, .T. ) ;
#7529 = ORIENTED_EDGE ( 'NONE', *, *, #241067, .F. ) ;
#7530 = CARTESIAN_POINT ( 'NONE',  ( -16.88005004766534967, 66.04989949669119653, -149.1727713725756530 ) ) ;
#7531 = DIRECTION ( 'NONE',  ( 0.000000000000000000, -1.000000000000000000, 0.000000000000000000 ) ) ;
#7533 = VERTEX_POINT ( 'NONE', #107002 ) ;
#7532 = EDGE_LOOP ( 'NONE', ( #140198, #128925, #234480, #166397 ) ) ;
#7534 = EDGE_LOOP ( 'NONE', ( #249804, #86820, #180964, #128455, #170519 ) ) ;
#7535 = ORIENTED_EDGE ( 'NONE', *, *, #246377, .F. ) ;
#7536 = VERTEX_POINT ( 'NONE', #207421 ) ;
#7537 = ADVANCED_FACE ( 'NONE', ( #147430 ), #31374, .F. ) ;
#7538 = CARTESIAN_POINT ( 'NONE',  ( -16.89208623190940273, 14.16166532508835729, -219.2598882133882512 ) ) ;
#7539 = CARTESIAN_POINT ( 'NONE',  ( -20.64999999999999858, 54.18213181965657554, -236.9344197582443883 ) ) ;
#7541 = ORIENTED_EDGE ( 'NONE', *, *, #146783, .F. ) ;
#7540 = CYLINDRICAL_SURFACE ( 'NONE', #93578, 0.09999999999998898659 ) ;
#7542 = DIRECTION ( 'NONE',  ( 0.000000000000000000, 0.8700118002898322711, -0.4930308989875231696 ) ) ;
#7544 = ORIENTED_EDGE ( 'NONE', *, *, #143935, .F. ) ;
#7543 = FACE_OUTER_BOUND ( 'NONE', #235873, .T. ) ;
#7545 = LINE ( 'NONE', #87060, #134449 ) ;
#7547 = ADVANCED_FACE ( 'NONE', ( #226966 ), #198678, .T. ) ;
#7546 = ORIENTED_EDGE ( 'NONE', *, *, #256226, .F. ) ;
#7548 = DIRECTION ( 'NONE',  ( -0.000000000000000000, 1.000000000000000000, 1.734723475976807292E-15 ) ) ;
#7549 = EDGE_LOOP ( 'NONE', ( #65986, #141549, #225808, #15787, #230435, #122686, #63645, #8949, #113853, #7446, #242313, #9996 ) ) ;
#7550 = DIRECTION ( 'NONE',  ( 0.000000000000000000, -1.000000000000000000, -6.982962677686265922E-15 ) ) ;
#7551 = CARTESIAN_POINT ( 'NONE',  ( -16.87036670365548474, 10.08494996325527460, -20.94999999999999929 ) ) ;
#7552 = ORIENTED_EDGE ( 'NONE', *, *, #134286, .T. ) ;
#7553 = AXIS2_PLACEMENT_3D ( 'NONE', #221879, #39459, #118971 ) ;
#7554 = AXIS2_PLACEMENT_3D ( 'NONE', #232486, #17281, #257105 ) ;
#7557 = DIRECTION ( 'NONE',  ( 1.000000000000000000, -0.000000000000000000, -0.000000000000000000 ) ) ;
#7556 = CIRCLE ( 'NONE', #186637, 0.1000000000000034472 ) ;
#7555 = FACE_OUTER_BOUND ( 'NONE', #97491, .T. ) ;
#7558 = VECTOR ( 'NONE', #93255, 1000.000000000000000 ) ;
#7559 = FACE_OUTER_BOUND ( 'NONE', #55007, .T. ) ;
#7560 = DIRECTION ( 'NONE',  ( 0.7071067811865493491, 0.7071067811865456854, 0.000000000000000000 ) ) ;
#7561 = EDGE_LOOP ( 'NONE', ( #157288, #41191, #185856, #75115 ) ) ;
#7562 = ORIENTED_EDGE ( 'NONE', *, *, #47275, .T. ) ;
#7563 =( BOUNDED_SURFACE ( )  B_SPLINE_SURFACE ( 3, 2, ( 
 ( #156830, #75978, #79799 ),
 ( #238908, #35600, #175129 ),
 ( #154281, #78530, #236331 ),
 ( #39454, #253319, #116398 ) ),
 .UNSPECIFIED., .F., .F., .F. ) 
 B_SPLINE_SURFACE_WITH_KNOTS ( ( 4, 4 ),
 ( 3, 3 ),
 ( 0.0006461284895273955529, 0.0007503702773985933402 ),
 ( 0.000000000000000000, 1.000000000000000000 ),
 .UNSPECIFIED. ) 
 GEOMETRIC_REPRESENTATION_ITEM ( )  RATIONAL_B_SPLINE_SURFACE ( (
 ( 1.000000000000000000, 0.7071067811865475727, 1.000000000000000000),
 ( 1.000000000000000000, 0.7076476444648740483, 1.000000000000000000),
 ( 1.000000000000000000, 0.7075727925191916956, 1.000000000000000000),
 ( 1.000000000000000000, 0.7071067811865475727, 1.000000000000000000) ) ) 
 REPRESENTATION_ITEM ( '' )  SURFACE ( )  );
#7564 = CARTESIAN_POINT ( 'NONE',  ( -23.15000000000000213, -11.48912529306489994, -130.9000000000000341 ) ) ;
#7565 = SPHERICAL_SURFACE ( 'NONE', #173438, 0.1000000000000000056 ) ;
#7567 = ORIENTED_EDGE ( 'NONE', *, *, #44290, .T. ) ;
#7566 = EDGE_CURVE ( 'NONE', #62026, #234461, #252834, .T. ) ;
#7568 = DIRECTION ( 'NONE',  ( 1.000000000000000000, 1.186688945009010077E-16, 0.000000000000000000 ) ) ;
#7569 = ORIENTED_EDGE ( 'NONE', *, *, #50019, .F. ) ;
#7570 = EDGE_CURVE ( 'NONE', #107985, #209093, #69204, .T. ) ;
#7571 = CARTESIAN_POINT ( 'NONE',  ( -23.15000000000000213, 24.23911354857403921, -250.5676753055308552 ) ) ;
#7572 = ORIENTED_EDGE ( 'NONE', *, *, #250128, .T. ) ;
#7573 = DIRECTION ( 'NONE',  ( 1.000000000000000000, 0.000000000000000000, 0.000000000000000000 ) ) ;
#7574 = CARTESIAN_POINT ( 'NONE',  ( -23.15000000000000213, 64.35000000001228670, -157.7731074845244450 ) ) ;
#7575 = CARTESIAN_POINT ( 'NONE',  ( 21.05000000000000071, 71.00000000001223555, -148.9283735034374843 ) ) ;
#7576 = AXIS2_PLACEMENT_3D ( 'NONE', #228645, #26588, #203917 ) ;
#7578 = ADVANCED_FACE ( 'NONE', ( #91315 ), #49611, .T. ) ;
#7577 = ORIENTED_EDGE ( 'NONE', *, *, #63158, .T. ) ;
#7579 = VECTOR ( 'NONE', #185692, 1000.000000000000000 ) ;
#7580 = PLANE ( 'NONE',  #223471 ) ;
#7581 = EDGE_LOOP ( 'NONE', ( #15111, #148890, #27897, #112780 ) ) ;
#7582 = AXIS2_PLACEMENT_3D ( 'NONE', #140304, #159910, #239435 ) ;
#7583 = ORIENTED_EDGE ( 'NONE', *, *, #146163, .F. ) ;
#7584 = ORIENTED_EDGE ( 'NONE', *, *, #228816, .T. ) ;
#7585 = FACE_OUTER_BOUND ( 'NONE', #102189, .T. ) ;
#7586 = DIRECTION ( 'NONE',  ( 1.000000000000000000, -0.000000000000000000, -0.000000000000000000 ) ) ;
#7587 = CARTESIAN_POINT ( 'NONE',  ( 21.05000000000000071, -9.499999999988844479, -157.6060308773475640 ) ) ;
#7588 = DIRECTION ( 'NONE',  ( 1.000000000000000000, -0.000000000000000000, -0.000000000000000000 ) ) ;
#7590 = CARTESIAN_POINT ( 'NONE',  ( -21.07016717457010913, 1.115541036281197940E-11, -161.1790591618990902 ) ) ;
#7589 = CARTESIAN_POINT ( 'NONE',  ( -18.40000000000000213, 11.33174054713631662, -113.1500000000000341 ) ) ;
#7592 = ORIENTED_EDGE ( 'NONE', *, *, #218958, .T. ) ;
#7591 = CARTESIAN_POINT ( 'NONE',  ( -18.59999999999999787, 85.40000000001226965, -162.7258477248610120 ) ) ;
#7593 = CARTESIAN_POINT ( 'NONE',  ( -20.94999999999999929, 4.436385504674529301, -245.3241086753762659 ) ) ;
#7594 = ORIENTED_EDGE ( 'NONE', *, *, #132477, .T. ) ;
#7595 = FACE_OUTER_BOUND ( 'NONE', #246010, .T. ) ;
#7596 = ORIENTED_EDGE ( 'NONE', *, *, #142375, .F. ) ;
#7597 = ORIENTED_EDGE ( 'NONE', *, *, #72224, .F. ) ;
#7598 = CARTESIAN_POINT ( 'NONE',  ( 20.84999999999999787, 64.25000000001195133, -109.9422547304830857 ) ) ;
#7599 = CARTESIAN_POINT ( 'NONE',  ( 21.05000000000000071, 64.23744694032048130, -224.5446448091673233 ) ) ;
#7601 = EDGE_CURVE ( 'NONE', #128539, #96616, #67889, .T. ) ;
#7600 = CARTESIAN_POINT ( 'NONE',  ( -21.05000000000000071, 75.96824164695762249, -209.7819546076044332 ) ) ;
#7602 = CARTESIAN_POINT ( 'NONE',  ( 20.85000000000000142, 62.88396779178381735, -206.9948552354529170 ) ) ;
#7603 = ADVANCED_FACE ( 'NONE', ( #39056 ), #248763, .T. ) ;
#7604 = VECTOR ( 'NONE', #252606, 1000.000000000000000 ) ;
#7605 = CIRCLE ( 'NONE', #28302, 0.09999999999999939493 ) ;
#7606 = AXIS2_PLACEMENT_3D ( 'NONE', #199146, #57031, #94896 ) ;
#7607 = LINE ( 'NONE', #44179, #34272 ) ;
#7608 = VERTEX_POINT ( 'NONE', #76866 ) ;
#7609 = ORIENTED_EDGE ( 'NONE', *, *, #157263, .T. ) ;
#7611 = EDGE_CURVE ( 'NONE', #59542, #39875, #182309, .T. ) ;
#7610 = DIRECTION ( 'NONE',  ( -1.000000000000000000, 7.304098846218135653E-16, -4.607487905232624742E-31 ) ) ;
#7612 = ORIENTED_EDGE ( 'NONE', *, *, #22453, .F. ) ;
#7613 = FACE_OUTER_BOUND ( 'NONE', #205747, .T. ) ;
#7614 = DIRECTION ( 'NONE',  ( 0.000000000000000000, -1.000000000000000000, -0.000000000000000000 ) ) ;
#7615 = ORIENTED_EDGE ( 'NONE', *, *, #155134, .T. ) ;
#7617 = FACE_OUTER_BOUND ( 'NONE', #74596, .T. ) ;
#7616 = CIRCLE ( 'NONE', #3493, 11.65000000000000568 ) ;
#7618 = CARTESIAN_POINT ( 'NONE',  ( 20.94999999999999929, 28.52545328903799415, -239.5221046041717443 ) ) ;
#7619 = DIRECTION ( 'NONE',  ( 2.827886303505249259E-16, -0.8660254037844411501, -0.4999999999999956701 ) ) ;
#7620 = CARTESIAN_POINT ( 'NONE',  ( 23.14999999999999858, 76.00000000001244871, -170.0231074845243597 ) ) ;
#7621 = ORIENTED_EDGE ( 'NONE', *, *, #96691, .F. ) ;
#7622 = DIRECTION ( 'NONE',  ( 0.000000000000000000, 0.000000000000000000, -1.000000000000000000 ) ) ;
#7623 = EDGE_CURVE ( 'NONE', #2878, #38279, #156455, .T. ) ;
#7624 = CARTESIAN_POINT ( 'NONE',  ( 18.59999999999999076, 54.53338637621133955, -228.6684279704127789 ) ) ;
#7625 = CARTESIAN_POINT ( 'NONE',  ( 23.04999999999999716, 44.59642007000408626, -236.3278401793003809 ) ) ;
#7626 = DIRECTION ( 'NONE',  ( 0.000000000000000000, 0.1332476588733448597, 0.9910827722268067408 ) ) ;
#7628 = ADVANCED_FACE ( 'NONE', ( #54739 ), #235940, .F. ) ;
#7627 = DIRECTION ( 'NONE',  ( 0.000000000000000000, 0.000000000000000000, -1.000000000000000000 ) ) ;
#7629 = AXIS2_PLACEMENT_3D ( 'NONE', #250846, #72240, #96882 ) ;
#7630 = CARTESIAN_POINT ( 'NONE',  ( 20.04142135623730070, 64.25000000001196554, -111.8731074845243825 ) ) ;
#7631 = VECTOR ( 'NONE', #126894, 1000.000000000000000 ) ;
#7632 = AXIS2_PLACEMENT_3D ( 'NONE', #159756, #78899, #38524 ) ;
#7633 = EDGE_CURVE ( 'NONE', #232481, #84528, #236355, .T. ) ;
#7634 = ORIENTED_EDGE ( 'NONE', *, *, #190682, .T. ) ;
#7637 = EDGE_CURVE ( 'NONE', #122601, #136730, #217643, .T. ) ;
#7636 = ADVANCED_FACE ( 'NONE', ( #173473 ), #216379, .F. ) ;
#7635 = AXIS2_PLACEMENT_3D ( 'NONE', #49675, #32725, #129220 ) ;
#7638 = DIRECTION ( 'NONE',  ( 0.000000000000000000, -0.1298341882519953860, -0.9915357197604862671 ) ) ;
#7639 = VERTEX_POINT ( 'NONE', #192987 ) ;
#7640 = DIRECTION ( 'NONE',  ( -1.000000000000000000, 0.000000000000000000, 0.000000000000000000 ) ) ;
#7641 = DIRECTION ( 'NONE',  ( -1.000000000000000000, -0.000000000000000000, -0.000000000000000000 ) ) ;
#7642 = DIRECTION ( 'NONE',  ( 0.000000000000000000, -7.429790795770644761E-15, 1.000000000000000000 ) ) ;
#7643 = CARTESIAN_POINT ( 'NONE',  ( 20.30466543256828160, 66.69576306075813932, -161.7694448331317005 ) ) ;
#7644 = CIRCLE ( 'NONE', #32803, 7.900000000000003908 ) ;
#7645 = VERTEX_POINT ( 'NONE', #176006 ) ;
#7646 = DIRECTION ( 'NONE',  ( -1.000000000000000000, -0.000000000000000000, -0.000000000000000000 ) ) ;
#7647 = CARTESIAN_POINT ( 'NONE',  ( -23.25000000000000000, 76.54968129668591814, -201.4963242025517047 ) ) ;
#7648 = CARTESIAN_POINT ( 'NONE',  ( -20.54999999999999716, 1.115600667400684642E-11, -167.5000000000000284 ) ) ;
#7649 = VECTOR ( 'NONE', #179943, 1000.000000000000000 ) ;
#7650 = EDGE_CURVE ( 'NONE', #31916, #195525, #71158, .T. ) ;
#7651 = CARTESIAN_POINT ( 'NONE',  ( 18.39999999999999503, 15.91777359887373500, -218.8720307647289758 ) ) ;
#7653 = EDGE_CURVE ( 'NONE', #74720, #206067, #111381, .T. ) ;
#7652 = AXIS2_PLACEMENT_3D ( 'NONE', #116257, #53697, #91548 ) ;
#7654 = DIRECTION ( 'NONE',  ( 1.000000000000000000, 0.000000000000000000, -0.000000000000000000 ) ) ;
#7655 = VECTOR ( 'NONE', #218555, 1000.000000000000000 ) ;
#7656 = AXIS2_PLACEMENT_3D ( 'NONE', #220481, #198330, #40587 ) ;
#7658 = VERTEX_POINT ( 'NONE', #118594 ) ;
#7657 = AXIS2_PLACEMENT_3D ( 'NONE', #154165, #15926, #58841 ) ;
#7659 = EDGE_LOOP ( 'NONE', ( #228235, #166303, #8737, #34445 ) ) ;
#7660 = CARTESIAN_POINT ( 'NONE',  ( 21.05000000000000071, -1.162701749926853712, -141.9000000000000341 ) ) ;
#7662 = CARTESIAN_POINT ( 'NONE',  ( -20.85000000000000142, 76.00000000001126921, -203.5231074845248997 ) ) ;
#7661 = AXIS2_PLACEMENT_3D ( 'NONE', #125665, #87803, #167395 ) ;
#7663 = DIRECTION ( 'NONE',  ( 0.000000000000000000, 0.4088369013363322146, -0.9126074666063751506 ) ) ;
#7665 = ADVANCED_FACE ( 'NONE', ( #196812 ), #134263, .F. ) ;
#7664 = DIRECTION ( 'NONE',  ( -1.000000000000000000, 2.952720810173289112E-16, 2.061873921506763405E-30 ) ) ;
#7666 = CARTESIAN_POINT ( 'NONE',  ( -22.47071067811865319, 68.27992525551431413, -170.1221999392270448 ) ) ;
#7667 = AXIS2_PLACEMENT_3D ( 'NONE', #75990, #142372, #103230 ) ;
#7668 = ORIENTED_EDGE ( 'NONE', *, *, #193963, .T. ) ;
#7670 = EDGE_CURVE ( 'NONE', #228463, #95688, #169696, .T. ) ;
#7669 = CYLINDRICAL_SURFACE ( 'NONE', #230566, 0.09999999999999939493 ) ;
#7671 = PRODUCT_CONTEXT ( 'NONE', #97263, 'mechanical' ) ;
#7672 = EDGE_CURVE ( 'NONE', #213598, #39469, #11444, .T. ) ;
#7673 = CYLINDRICAL_SURFACE ( 'NONE', #113340, 0.09999999999999939493 ) ;
#7674 = VERTEX_POINT ( 'NONE', #93869 ) ;
#7675 = DIRECTION ( 'NONE',  ( 0.000000000000000000, -1.000000000000000000, 0.000000000000000000 ) ) ;
#7676 = PRODUCT ( 'Injection Molded Chain Links 10', 'Injection Molded Chain Links 10', '', ( #19534 ) ) ;
#7677 = AXIS2_PLACEMENT_3D ( 'NONE', #245443, #5509, #66795 ) ;
#7678 = VECTOR ( 'NONE', #194343, 1000.000000000000000 ) ;
#7679 = ORIENTED_EDGE ( 'NONE', *, *, #235995, .T. ) ;
#7680 = ORIENTED_EDGE ( 'NONE', *, *, #256341, .F. ) ;
#7681 = EDGE_CURVE ( 'NONE', #61341, #249154, #15741, .T. ) ;
#7682 = CARTESIAN_POINT ( 'NONE',  ( -22.50000000000094147, 75.90000000001212754, -114.6726782920691363 ) ) ;
#7683 = DIRECTION ( 'NONE',  ( 1.000000000000000000, 0.000000000000000000, 0.000000000000000000 ) ) ;
#7684 = DIRECTION ( 'NONE',  ( 1.000000000000000000, 7.304098846218134667E-16, 0.000000000000000000 ) ) ;
#7685 = DIRECTION ( 'NONE',  ( 0.000000000000000000, 0.000000000000000000, 1.000000000000000000 ) ) ;
#7687 = CIRCLE ( 'NONE', #3561, 0.09999999999999971412 ) ;
#7686 = CYLINDRICAL_SURFACE ( 'NONE', #40353, 2.000000000000001776 ) ;
#7688 = DIRECTION ( 'NONE',  ( 0.000000000000000000, -0.9770955615653307280, -0.2128009952263642535 ) ) ;
#7689 = CARTESIAN_POINT ( 'NONE',  ( -21.65000000000000213, 63.02410583447655767, -221.9179669651492759 ) ) ;
#7690 = CIRCLE ( 'NONE', #70251, 0.6000000000000033085 ) ;
#7692 = LINE ( 'NONE', #241169, #95485 ) ;
#7691 = DIRECTION ( 'NONE',  ( -0.000000000000000000, 0.9934243067848629316, -0.1144908148674581572 ) ) ;
#7693 = EDGE_CURVE ( 'NONE', #199162, #107823, #57184, .T. ) ;
#7694 = CARTESIAN_POINT ( 'NONE',  ( 13.99999999999999822, 66.15000000001228386, -153.2731074845244450 ) ) ;
#7695 = CIRCLE ( 'NONE', #211716, 0.2000000000000057288 ) ;
#7696 = DIRECTION ( 'NONE',  ( -1.000000000000000000, -0.000000000000000000, -0.000000000000000000 ) ) ;
#7697 = CARTESIAN_POINT ( 'NONE',  ( -20.94999999999999929, 1.115650877919449575E-11, -104.6000000000000512 ) ) ;
#7698 = DIRECTION ( 'NONE',  ( 0.000000000000000000, 0.000000000000000000, 1.000000000000000000 ) ) ;
#7699 = VERTEX_POINT ( 'NONE', #95158 ) ;
#7700 = EDGE_LOOP ( 'NONE', ( #30733, #119395, #108441, #79226 ) ) ;
#7701 = DIRECTION ( 'NONE',  ( -1.000000000000000000, -0.000000000000000000, 0.000000000000000000 ) ) ;
#7702 = CARTESIAN_POINT ( 'NONE',  ( 18.49999999999999289, 11.04098673250373785, -220.4458636211660689 ) ) ;
#7704 = CARTESIAN_POINT ( 'NONE',  ( -12.26136940704872380, 12.75047551130877288, -215.6006359250795867 ) ) ;
#7703 = CARTESIAN_POINT ( 'NONE',  ( 18.59999999999999787, 1.115600667400684642E-11, -67.00000000000004263 ) ) ;
#7705 = TOROIDAL_SURFACE ( 'NONE', #224342, 11.65000000000000036, 0.1000000000000000056 ) ;
#7706 = CARTESIAN_POINT ( 'NONE',  ( 20.95556889135987788, 39.29078794878244452, -236.7330049007518085 ) ) ;
#7707 = CARTESIAN_POINT ( 'NONE',  ( 20.99999999999999645, 44.21724908628621620, -235.4814530999287285 ) ) ;
#7708 = ADVANCED_FACE ( 'NONE', ( #65008 ), #199414, .T. ) ;
#7709 = CARTESIAN_POINT ( 'NONE',  ( 20.94999999999999929, -9.399999999988844834, -157.6060308773475640 ) ) ;
#7710 = VECTOR ( 'NONE', #65599, 1000.000000000000000 ) ;
#7711 = ORIENTED_EDGE ( 'NONE', *, *, #121237, .T. ) ;
#7712 = EDGE_LOOP ( 'NONE', ( #249003, #24636, #213615, #252389, #187638 ) ) ;
#7713 = CIRCLE ( 'NONE', #240928, 0.1999999999999999833 ) ;
#7714 = TOROIDAL_SURFACE ( 'NONE', #20182, 4.150000000000000355, 0.1000000000000000056 ) ;
#7715 = CARTESIAN_POINT ( 'NONE',  ( -18.59999999999999787, 76.00000000001190870, -103.0231074845243029 ) ) ;
#7716 = CIRCLE ( 'NONE', #45111, 0.09999999999999520384 ) ;
#7717 = ORIENTED_EDGE ( 'NONE', *, *, #161502, .T. ) ;
#7718 = DIRECTION ( 'NONE',  ( 3.616040088954497272E-32, -1.224646799147352961E-16, 1.000000000000000000 ) ) ;
#7719 = FACE_OUTER_BOUND ( 'NONE', #237363, .T. ) ;
#7720 = ORIENTED_EDGE ( 'NONE', *, *, #122168, .F. ) ;
#7721 = PLANE ( 'NONE',  #139446 ) ;
#7722 = EDGE_LOOP ( 'NONE', ( #113643, #182598, #67132, #163751 ) ) ;
#7723 = CARTESIAN_POINT ( 'NONE',  ( 18.59999999999998366, 76.00000000001244871, -170.0231074845243597 ) ) ;
#7724 = CARTESIAN_POINT ( 'NONE',  ( -23.25000000000000000, 1.115600667400684642E-11, -74.90000000000000568 ) ) ;
#7726 = DIRECTION ( 'NONE',  ( 0.000000000000000000, -6.982962677686266711E-15, 1.000000000000000000 ) ) ;
#7725 = AXIS2_PLACEMENT_3D ( 'NONE', #166504, #84307, #46509 ) ;
#7727 = CARTESIAN_POINT ( 'NONE',  ( 18.50000000000000355, -9.421456145483672273, -141.2419820840187015 ) ) ;
#7728 = DIRECTION ( 'NONE',  ( -1.000000000000000000, 0.000000000000000000, 0.000000000000000000 ) ) ;
#7729 = DIRECTION ( 'NONE',  ( 1.000000000000000000, 3.265361837132813093E-16, -0.000000000000000000 ) ) ;
#7730 = CARTESIAN_POINT ( 'NONE',  ( -20.90000000000000213, 3.362550747017865493, 28.82623795144604983 ) ) ;
#7731 = CARTESIAN_POINT ( 'NONE',  ( -18.59999999999999787, 9.350000000011156942, -112.6500000000000341 ) ) ;
#7733 = EDGE_LOOP ( 'NONE', ( #7217, #208355, #59627, #19637, #88786, #256835, #173776, #129682, #205641, #128064, #129112, #127908 ) ) ;
#7732 = DIRECTION ( 'NONE',  ( 0.000000000000000000, 0.9999631594459053030, 0.008583690987162899758 ) ) ;
#7735 = DIRECTION ( 'NONE',  ( 1.186688945009009831E-16, -1.000000000000000000, 0.000000000000000000 ) ) ;
#7734 = FACE_OUTER_BOUND ( 'NONE', #89618, .T. ) ;
#7736 = ORIENTED_EDGE ( 'NONE', *, *, #143479, .T. ) ;
#7738 = VERTEX_POINT ( 'NONE', #243651 ) ;
#7737 = LINE ( 'NONE', #225465, #19392 ) ;
#7739 = EDGE_LOOP ( 'NONE', ( #132540, #11041, #38240, #23278 ) ) ;
#7740 = LINE ( 'NONE', #26020, #115878 ) ;
#7741 = CARTESIAN_POINT ( 'NONE',  ( -18.35235881385853318, 11.47341900772405054, -143.2500000000000284 ) ) ;
#7742 = CARTESIAN_POINT ( 'NONE',  ( 21.07954640115206502, 0.06600770715102041719, -127.6707123039770835 ) ) ;
#7743 = LINE ( 'NONE', #115819, #80759 ) ;
#7744 = CARTESIAN_POINT ( 'NONE',  ( 22.60000000000000142, 1.115600667400684642E-11, -134.0000000000000000 ) ) ;
#7745 = FACE_OUTER_BOUND ( 'NONE', #18036, .T. ) ;
#7746 = CARTESIAN_POINT ( 'NONE',  ( 20.02499999999999858, 9.750000000011153745, -121.6500000000000341 ) ) ;
#7747 = CARTESIAN_POINT ( 'NONE',  ( 20.94999999999999929, 67.23127455305841238, -235.8551265064783991 ) ) ;
#7748 = EDGE_CURVE ( 'NONE', #20386, #177453, #28214, .T. ) ;
#7749 = VECTOR ( 'NONE', #234423, 1000.000000000000000 ) ;
#7750 = VERTEX_POINT ( 'NONE', #242361 ) ;
#7751 = VERTEX_POINT ( 'NONE', #20777 ) ;
#7752 = AXIS2_PLACEMENT_3D ( 'NONE', #142539, #61733, #242929 ) ;
#7753 = CARTESIAN_POINT ( 'NONE',  ( -16.94275863009466576, 9.989496048673542461, -180.1083026179588558 ) ) ;
#7754 = AXIS2_PLACEMENT_3D ( 'NONE', #3125, #226013, #44846 ) ;
#7755 = ORIENTED_EDGE ( 'NONE', *, *, #129732, .F. ) ;
#7756 = CARTESIAN_POINT ( 'NONE',  ( 20.85000000000000142, 76.00000000001190870, -103.0231074845243029 ) ) ;
#7757 = ORIENTED_EDGE ( 'NONE', *, *, #158998, .F. ) ;
#7758 = CARTESIAN_POINT ( 'NONE',  ( 18.52928932188134326, 65.72071067813014622, -44.81452884076170307 ) ) ;
#7759 = CIRCLE ( 'NONE', #99304, 4.049999999999998046 ) ;
#7760 = CARTESIAN_POINT ( 'NONE',  ( 19.99999999738043144, 11.75000000000000888, -24.68717194963242534 ) ) ;
#7761 = CARTESIAN_POINT ( 'NONE',  ( -22.49510344025093644, -2.413535076292374182, -189.6025810811986219 ) ) ;
#7762 = EDGE_CURVE ( 'NONE', #89986, #28813, #7328, .T. ) ;
#7763 = SPHERICAL_SURFACE ( 'NONE', #73218, 0.1000000000000000056 ) ;
#7764 = CARTESIAN_POINT ( 'NONE',  ( -21.14999999999999858, -2.576749817950531707, -189.6385361693310756 ) ) ;
#7765 = VERTEX_POINT ( 'NONE', #141976 ) ;
#7766 = ADVANCED_FACE ( 'NONE', ( #200685 ), #144536, .F. ) ;
#7767 = FACE_OUTER_BOUND ( 'NONE', #137380, .T. ) ;
#7768 = AXIS2_PLACEMENT_3D ( 'NONE', #104633, #126804, #26435 ) ;
#7769 = AXIS2_PLACEMENT_3D ( 'NONE', #196791, #158995, #78125 ) ;
#7771 = AXIS2_PLACEMENT_3D ( 'NONE', #186684, #68002, #25055 ) ;
#7770 = CARTESIAN_POINT ( 'NONE',  ( 13.40000000000000036, -11.65000000000000036, 12.40000000000000391 ) ) ;
#7772 = CARTESIAN_POINT ( 'NONE',  ( 18.42595409746860469, 85.49999981257654724, -62.52374513277740675 ) ) ;
#7773 = DIRECTION ( 'NONE',  ( 0.000000000000000000, 0.1495327102803586661, -0.9887567792719350601 ) ) ;
#7774 = ORIENTED_EDGE ( 'NONE', *, *, #85512, .T. ) ;
#7775 = CARTESIAN_POINT ( 'NONE',  ( -23.25000000000000000, 87.65000000001172964, -72.52310748452423184 ) ) ;
#7776 = EDGE_LOOP ( 'NONE', ( #210936, #52274, #230403, #227395 ) ) ;
#7779 = ORIENTED_EDGE ( 'NONE', *, *, #27414, .F. ) ;
#7778 = CARTESIAN_POINT ( 'NONE',  ( -18.59999999999999787, 11.65000000001115232, -54.75000000000000000 ) ) ;
#7777 = FACE_OUTER_BOUND ( 'NONE', #142440, .T. ) ;
#7780 = ORIENTED_EDGE ( 'NONE', *, *, #178777, .F. ) ;
#7781 = AXIS2_PLACEMENT_3D ( 'NONE', #99878, #778, #80314 ) ;
#7782 = LINE ( 'NONE', #127729, #39398 ) ;
#7783 = CARTESIAN_POINT ( 'NONE',  ( -21.05000000000000071, 34.07612324756792077, -243.5412266404783566 ) ) ;
#7784 = ADVANCED_FACE ( 'NONE', ( #121178 ), #186412, .F. ) ;
#7785 = DIRECTION ( 'NONE',  ( 1.000000000000000000, 0.000000000000000000, 0.000000000000000000 ) ) ;
#7786 = VERTEX_POINT ( 'NONE', #59853 ) ;
#7787 = CARTESIAN_POINT ( 'NONE',  ( -18.59999999999999787, 1.340746217944851715, -23.22713749457881960 ) ) ;
#7788 = EDGE_CURVE ( 'NONE', #221912, #251583, #61502, .T. ) ;
#7789 = FACE_BOUND ( 'NONE', #83184, .T. ) ;
#7790 = ADVANCED_FACE ( 'NONE', ( #220256 ), #257076, .T. ) ;
#7792 = DIRECTION ( 'NONE',  ( -1.000000000000000000, 1.652117596168391700E-15, 0.000000000000000000 ) ) ;
#7791 = CARTESIAN_POINT ( 'NONE',  ( -22.59999999999999787, 11.74956712348939192, 0.1008583690987083364 ) ) ;
#7794 = ORIENTED_EDGE ( 'NONE', *, *, #219501, .F. ) ;
#7793 = FACE_OUTER_BOUND ( 'NONE', #103774, .T. ) ;
#7795 = EDGE_CURVE ( 'NONE', #64123, #131079, #232213, .T. ) ;
#7796 = ORIENTED_EDGE ( 'NONE', *, *, #113753, .F. ) ;
#7797 = TOROIDAL_SURFACE ( 'NONE', #228368, 0.6000000000000013101, 0.1000000000000000056 ) ;
#7798 = DIRECTION ( 'NONE',  ( 0.000000000000000000, -0.4088369013363281068, 0.9126074666063770380 ) ) ;
#7799 = CARTESIAN_POINT ( 'NONE',  ( 20.85000000000000142, 7.128833340094563376, -233.7327013124401276 ) ) ;
#7800 = AXIS2_PLACEMENT_3D ( 'NONE', #193210, #15873, #254422 ) ;
#7801 = AXIS2_PLACEMENT_3D ( 'NONE', #220657, #120312, #195007 ) ;
#7802 = DIRECTION ( 'NONE',  ( -1.000000000000000000, -0.000000000000000000, -0.000000000000000000 ) ) ;
#7803 = ORIENTED_EDGE ( 'NONE', *, *, #230075, .T. ) ;
#7804 = CARTESIAN_POINT ( 'NONE',  ( -21.14999999999994174, 76.00000000001119815, -36.02310748452479316 ) ) ;
#7805 = EDGE_CURVE ( 'NONE', #202204, #247441, #181131, .T. ) ;
#7806 = FACE_OUTER_BOUND ( 'NONE', #23507, .T. ) ;
#7807 = DIRECTION ( 'NONE',  ( -1.000000000000000000, 0.000000000000000000, 0.000000000000000000 ) ) ;
#7808 = EDGE_CURVE ( 'NONE', #248444, #169606, #115663, .T. ) ;
#7809 = ORIENTED_EDGE ( 'NONE', *, *, #170687, .F. ) ;
#7810 = DIRECTION ( 'NONE',  ( 0.000000000000000000, -1.776356839400250465E-15, -1.000000000000000000 ) ) ;
#7811 = ADVANCED_FACE ( 'NONE', ( #42892 ), #194793, .F. ) ;
#7812 = ORIENTED_EDGE ( 'NONE', *, *, #204325, .F. ) ;
#7813 = VECTOR ( 'NONE', #27399, 1000.000000000000000 ) ;
#7815 = AXIS2_PLACEMENT_3D ( 'NONE', #163813, #118600, #45136 ) ;
#7814 = CARTESIAN_POINT ( 'NONE',  ( 20.94999999999999929, 70.15000000001178648, -79.65560470880228650 ) ) ;
#7816 = CARTESIAN_POINT ( 'NONE',  ( -18.38817693311004575, 64.51850848411201866, -78.77310748452438816 ) ) ;
#7817 = CIRCLE ( 'NONE', #66054, 11.70000000000000284 ) ;
#7818 = EDGE_LOOP ( 'NONE', ( #154222, #123969, #193935, #23899 ) ) ;
#7819 = ORIENTED_EDGE ( 'NONE', *, *, #229517, .T. ) ;
#7820 = CIRCLE ( 'NONE', #132725, 0.09999999999999766020 ) ;
#7821 = EDGE_CURVE ( 'NONE', #60670, #157942, #236278, .T. ) ;
#7822 = CARTESIAN_POINT ( 'NONE',  ( -21.64999999999999858, 9.350000000011133849, -79.65000000000004832 ) ) ;
#7823 = VERTEX_POINT ( 'NONE', #23355 ) ;
#7825 = ORIENTED_EDGE ( 'NONE', *, *, #175402, .T. ) ;
#7824 = CARTESIAN_POINT ( 'NONE',  ( -22.50000000000088463, 0.04536165659882995804, -155.8494911657945750 ) ) ;
#7826 = VERTEX_POINT ( 'NONE', #184963 ) ;
#7827 = CIRCLE ( 'NONE', #37067, 4.049999999999998046 ) ;
#7829 = VERTEX_POINT ( 'NONE', #102832 ) ;
#7828 = ORIENTED_EDGE ( 'NONE', *, *, #54871, .T. ) ;
#7830 = DIRECTION ( 'NONE',  ( 1.000000000000000000, -0.000000000000000000, -0.000000000000000000 ) ) ;
#7832 = ORIENTED_EDGE ( 'NONE', *, *, #196051, .F. ) ;
#7831 = VECTOR ( 'NONE', #94934, 1000.000000000000000 ) ;
#7833 = CARTESIAN_POINT ( 'NONE',  ( -20.54999999999999716, 38.33376540847015690, -250.4483291680710693 ) ) ;
#7834 = FACE_OUTER_BOUND ( 'NONE', #70502, .T. ) ;
#7835 = FACE_OUTER_BOUND ( 'NONE', #12821, .T. ) ;
#7836 = ADVANCED_FACE ( 'NONE', ( #182412 ), #132225, .T. ) ;
#7837 = CIRCLE ( 'NONE', #249445, 0.1000000000000028644 ) ;
#7838 = CARTESIAN_POINT ( 'NONE',  ( -18.44232395689846271, 87.01022120691494877, -199.4197499265777367 ) ) ;
#7839 = VECTOR ( 'NONE', #95221, 1000.000000000000000 ) ;
#7840 = AXIS2_PLACEMENT_3D ( 'NONE', #172139, #113407, #14335 ) ;
#7841 = ORIENTED_EDGE ( 'NONE', *, *, #200893, .F. ) ;
#7842 = TOROIDAL_SURFACE ( 'NONE', #203651, 0.4000000000000012990, 0.1000000000000000056 ) ;
#7843 = ORIENTED_EDGE ( 'NONE', *, *, #71335, .T. ) ;
#7844 = DIRECTION ( 'NONE',  ( -3.469446951953738513E-14, 0.9770955615653543758, 0.2128009952262553683 ) ) ;
#7846 = ORIENTED_EDGE ( 'NONE', *, *, #75513, .T. ) ;
#7845 = CARTESIAN_POINT ( 'NONE',  ( -20.94999999999999929, 87.41227409416235616, -200.5231074845242745 ) ) ;
#7847 = LINE ( 'NONE', #245166, #50903 ) ;
#7849 = VERTEX_POINT ( 'NONE', #164129 ) ;
#7848 = CARTESIAN_POINT ( 'NONE',  ( 20.94999999999999929, 5.400000000011154988, -79.40526601891313874 ) ) ;
#7850 = AXIS2_PLACEMENT_3D ( 'NONE', #185540, #190706, #125561 ) ;
#7851 = EDGE_CURVE ( 'NONE', #89858, #69398, #83263, .T. ) ;
#7852 = ORIENTED_EDGE ( 'NONE', *, *, #79965, .T. ) ;
#7853 = DIRECTION ( 'NONE',  ( -1.000000000000000000, 0.000000000000000000, 0.000000000000000000 ) ) ;
#7854 = EDGE_CURVE ( 'NONE', #2577, #178267, #53114, .T. ) ;
#7855 = EDGE_CURVE ( 'NONE', #243110, #171479, #41406, .T. ) ;
#7856 = ORIENTED_EDGE ( 'NONE', *, *, #22074, .T. ) ;
#7857 = VERTEX_POINT ( 'NONE', #209662 ) ;
#7858 = DIRECTION ( 'NONE',  ( 0.000000000000000000, 0.9955484899852913294, -0.09425075112701486457 ) ) ;
#7860 = ADVANCED_FACE ( 'NONE', ( #10189 ), #11475, .T. ) ;
#7859 = CARTESIAN_POINT ( 'NONE',  ( -21.05000000000000071, 87.48912529308749697, -38.92310748452424463 ) ) ;
#7862 = EDGE_CURVE ( 'NONE', #39052, #77399, #198857, .T. ) ;
#7861 = AXIS2_PLACEMENT_3D ( 'NONE', #232656, #11018, #53993 ) ;
#7863 = AXIS2_PLACEMENT_3D ( 'NONE', #10554, #112228, #90061 ) ;
#7865 = EDGE_LOOP ( 'NONE', ( #35168, #113948, #236834, #98657 ) ) ;
#7864 = EDGE_LOOP ( 'NONE', ( #127313, #8381, #67814, #233894 ) ) ;
#7866 = ORIENTED_EDGE ( 'NONE', *, *, #229019, .F. ) ;
#7867 = DIRECTION ( 'NONE',  ( 0.000000000000000000, 0.000000000000000000, -1.000000000000000000 ) ) ;
#7868 = ORIENTED_EDGE ( 'NONE', *, *, #46523, .F. ) ;
#7869 = ORIENTED_EDGE ( 'NONE', *, *, #170864, .T. ) ;
#7870 = ADVANCED_FACE ( 'NONE', ( #51844 ), #169293, .F. ) ;
#7871 = CYLINDRICAL_SURFACE ( 'NONE', #200973, 0.1000000000000028644 ) ;
#7873 = EDGE_LOOP ( 'NONE', ( #39999, #120262, #11049, #39038 ) ) ;
#7872 = DIRECTION ( 'NONE',  ( -0.000000000000000000, 0.8660254037844383745, -0.5000000000000003331 ) ) ;
#7874 = PLANE ( 'NONE',  #156628 ) ;
#7876 = LINE ( 'NONE', #251602, #135844 ) ;
#7875 = CARTESIAN_POINT ( 'NONE',  ( 19.88284271247461987, 11.69142135624847256, -192.2499999999999432 ) ) ;
#7877 = FACE_OUTER_BOUND ( 'NONE', #162128, .T. ) ;
#7878 = CARTESIAN_POINT ( 'NONE',  ( -13.88555196119804158, 62.02985059084868169, -218.9026721699492555 ) ) ;
#7879 = ORIENTED_EDGE ( 'NONE', *, *, #155408, .F. ) ;
#7880 = AXIS2_PLACEMENT_3D ( 'NONE', #73088, #18213, #152619 ) ;
#7881 = TOROIDAL_SURFACE ( 'NONE', #153667, 0.2000000000000000111, 0.1000000000000000056 ) ;
#7882 = ORIENTED_EDGE ( 'NONE', *, *, #25314, .T. ) ;
#7883 = DIRECTION ( 'NONE',  ( 0.000000000000000000, -1.000000000000000000, 6.938893903907030216E-14 ) ) ;
#7884 = DIRECTION ( 'NONE',  ( 0.000000000000000000, 1.000000000000000000, 0.000000000000000000 ) ) ;
#7885 = AXIS2_PLACEMENT_3D ( 'NONE', #110637, #131483, #246303 ) ;
#7886 = ORIENTED_EDGE ( 'NONE', *, *, #244775, .T. ) ;
#7887 = AXIS2_PLACEMENT_3D ( 'NONE', #167629, #187189, #154497 ) ;
#7888 = EDGE_CURVE ( 'NONE', #202001, #77719, #165409, .T. ) ;
#7889 = LINE ( 'NONE', #87390, #55164 ) ;
#7890 = ORIENTED_EDGE ( 'NONE', *, *, #124839, .T. ) ;
#7891 = ORIENTED_EDGE ( 'NONE', *, *, #126743, .F. ) ;
#7892 = CARTESIAN_POINT ( 'NONE',  ( -21.05000000000000071, 87.75000000001247713, -173.1231074845242688 ) ) ;
#7893 = DIRECTION ( 'NONE',  ( -1.000000000000000000, -0.000000000000000000, -0.000000000000000000 ) ) ;
#7895 = EDGE_CURVE ( 'NONE', #133198, #84754, #48009, .T. ) ;
#7894 = ORIENTED_EDGE ( 'NONE', *, *, #34136, .T. ) ;
#7896 = CARTESIAN_POINT ( 'NONE',  ( -18.59999999999999787, 10.33248238082518711, -39.09484654391314962 ) ) ;
#7897 = CARTESIAN_POINT ( 'NONE',  ( 21.05095171578076574, 8.776179878782192745, -112.6658732766379103 ) ) ;
#7898 = ORIENTED_EDGE ( 'NONE', *, *, #118042, .F. ) ;
#7899 = ADVANCED_FACE ( 'NONE', ( #170591 ), #149002, .T. ) ;
#7900 = CARTESIAN_POINT ( 'NONE',  ( 19.80993210785544534, 64.25000000001219291, -145.2559897356397016 ) ) ;
#7901 = PLANE ( 'NONE',  #111991 ) ;
#7903 = DIRECTION ( 'NONE',  ( -1.000000000000000000, -0.000000000000000000, 0.000000000000000000 ) ) ;
#7902 = CARTESIAN_POINT ( 'NONE',  ( -21.05000000000000071, 69.65930857908919904, -248.3682875362397340 ) ) ;
#7904 = LINE ( 'NONE', #87405, #206527 ) ;
#7906 = CIRCLE ( 'NONE', #153687, 0.09999999999998802902 ) ;
#7905 = CARTESIAN_POINT ( 'NONE',  ( -21.05000000000000071, 44.06250559941687328, -258.7395785465160429 ) ) ;
#7907 = VECTOR ( 'NONE', #54135, 1000.000000000000000 ) ;
#7908 = CARTESIAN_POINT ( 'NONE',  ( 18.46858270002951841, -9.474202674699414573, -174.6020219347037994 ) ) ;
#7909 = DIRECTION ( 'NONE',  ( 1.000000000000000000, 0.000000000000000000, -0.000000000000000000 ) ) ;
#7910 = VECTOR ( 'NONE', #242891, 1000.000000000000227 ) ;
#7911 = ORIENTED_EDGE ( 'NONE', *, *, #185242, .T. ) ;
#7913 = ORIENTED_EDGE ( 'NONE', *, *, #211806, .T. ) ;
#7912 = EDGE_LOOP ( 'NONE', ( #135805, #181282, #84762, #136685, #79282, #45081, #100771, #232136, #223888, #189020, #255979, #98903, #211182, #42382, #48674, #124535 ) ) ;
#7914 = VERTEX_POINT ( 'NONE', #149715 ) ;
#7915 = DIRECTION ( 'NONE',  ( -1.020425574104004196E-15, 6.982962677686266711E-15, -1.000000000000000000 ) ) ;
#7916 = FACE_OUTER_BOUND ( 'NONE', #129895, .T. ) ;
#7917 = DIRECTION ( 'NONE',  ( 1.186688945009009831E-16, -1.000000000000000000, 0.000000000000000000 ) ) ;
#7918 = DIRECTION ( 'NONE',  ( -1.000000000000000000, 0.000000000000000000, 0.000000000000000000 ) ) ;
#7919 = ORIENTED_EDGE ( 'NONE', *, *, #222706, .F. ) ;
#7920 = AXIS2_PLACEMENT_3D ( 'NONE', #119347, #120650, #179337 ) ;
#7921 = FACE_OUTER_BOUND ( 'NONE', #107218, .T. ) ;
#7922 = CARTESIAN_POINT ( 'NONE',  ( -21.04999999999999716, 0.09843749999999835965, 6.299230910086880186 ) ) ;
#7923 = FACE_OUTER_BOUND ( 'NONE', #181610, .T. ) ;
#7924 = CARTESIAN_POINT ( 'NONE',  ( -21.05000000000000071, 1.316055977212907457, -230.7323992127457473 ) ) ;
#7925 = EDGE_LOOP ( 'NONE', ( #42889, #247048, #205687, #26138 ) ) ;
#7926 = CARTESIAN_POINT ( 'NONE',  ( 20.94999999999999574, -11.48912529306490349, -137.1000000000000227 ) ) ;
#7927 = EDGE_LOOP ( 'NONE', ( #165363, #39452, #248370, #167477, #89151 ) ) ;
#7928 = ORIENTED_EDGE ( 'NONE', *, *, #18329, .T. ) ;
#7929 = CARTESIAN_POINT ( 'NONE',  ( -18.34374000495060386, 64.52683809664941350, -93.77310748452440237 ) ) ;
#7930 = DIRECTION ( 'NONE',  ( -1.000000000000000000, -0.000000000000000000, -0.000000000000000000 ) ) ;
#7931 = CARTESIAN_POINT ( 'NONE',  ( 15.48841904831874849, 64.42574402712453718, -213.4910444358848167 ) ) ;
#7932 = CARTESIAN_POINT ( 'NONE',  ( 21.05000000000000071, 64.35000000001156195, -57.37310748452439668 ) ) ;
#7933 = CARTESIAN_POINT ( 'NONE',  ( 20.94999999999999574, 77.83534155023670564, -158.4679561919613491 ) ) ;
#7934 = CARTESIAN_POINT ( 'NONE',  ( -20.64999999999999858, 2.000000000011154189, -53.77537807723790309 ) ) ;
#7935 = VERTEX_POINT ( 'NONE', #248799 ) ;
#7936 = DIRECTION ( 'NONE',  ( 0.000000000000000000, 0.000000000000000000, -1.000000000000000000 ) ) ;
#7937 = CARTESIAN_POINT ( 'NONE',  ( -21.05000000000000071, -0.09999999998884474828, -60.45934304829881256 ) ) ;
#7938 = EDGE_CURVE ( 'NONE', #152113, #121066, #69897, .T. ) ;
#7940 = LINE ( 'NONE', #129167, #162321 ) ;
#7939 = CARTESIAN_POINT ( 'NONE',  ( 5.900000000000059863, 64.65000000001120384, -25.92310748452479174 ) ) ;
#7941 = CARTESIAN_POINT ( 'NONE',  ( -23.25000000000000000, 76.00000000001192291, -98.97310748452431994 ) ) ;
#7942 = DIRECTION ( 'NONE',  ( 1.000000000000000000, 0.000000000000000000, 0.000000000000000000 ) ) ;
#7943 = CIRCLE ( 'NONE', #12232, 0.1000000000000054040 ) ;
#7944 = AXIS2_PLACEMENT_3D ( 'NONE', #254463, #253203, #96667 ) ;
#7946 = EDGE_CURVE ( 'NONE', #49647, #62, #68886, .T. ) ;
#7945 = CARTESIAN_POINT ( 'NONE',  ( -20.54999999999999716, 71.75000000001229239, -157.6731074845243654 ) ) ;
#7947 = DIRECTION ( 'NONE',  ( -0.000000000000000000, -0.000000000000000000, 1.000000000000000000 ) ) ;
#7948 = CIRCLE ( 'NONE', #91500, 11.64999999999998614 ) ;
#7949 = CIRCLE ( 'NONE', #74603, 2.600000000000000089 ) ;
#7951 = ORIENTED_EDGE ( 'NONE', *, *, #115334, .F. ) ;
#7950 = DIRECTION ( 'NONE',  ( 0.000000000000000000, 0.000000000000000000, -1.000000000000000000 ) ) ;
#7952 = ADVANCED_FACE ( 'NONE', ( #49299 ), #66305, .T. ) ;
#7953 = AXIS2_PLACEMENT_3D ( 'NONE', #21126, #184014, #142314 ) ;
#7954 = EDGE_CURVE ( 'NONE', #72307, #111525, #207441, .T. ) ;
#7955 = AXIS2_PLACEMENT_3D ( 'NONE', #129170, #48337, #204831 ) ;
#7957 = TOROIDAL_SURFACE ( 'NONE', #32936, 0.9750000000000019762, 0.1000000000000000056 ) ;
#7956 = DIRECTION ( 'NONE',  ( -1.000000000000000000, -7.304098846218134667E-16, 0.000000000000000000 ) ) ;
#7958 = DIRECTION ( 'NONE',  ( -1.000000000000000000, 0.000000000000000000, -0.000000000000000000 ) ) ;
#7959 = VERTEX_POINT ( 'NONE', #128853 ) ;
#7961 = EDGE_CURVE ( 'NONE', #185072, #238459, #150976, .T. ) ;
#7960 = TOROIDAL_SURFACE ( 'NONE', #107716, 0.2000000000000000111, 0.1000000000000000056 ) ;
#7962 = DIRECTION ( 'NONE',  ( 0.000000000000000000, 1.000000000000000000, 6.938893903907222067E-15 ) ) ;
#7963 = EDGE_CURVE ( 'NONE', #67101, #163770, #110553, .T. ) ;
#7964 = DIRECTION ( 'NONE',  ( 0.000000000000000000, -0.6728971962616412394, -0.7397360091703134577 ) ) ;
#7965 = PLANE ( 'NONE',  #23796 ) ;
#7966 = ORIENTED_EDGE ( 'NONE', *, *, #255799, .F. ) ;
#7967 = CARTESIAN_POINT ( 'NONE',  ( 18.59999999999998721, 6.933893972137497030, -70.78564583437358237 ) ) ;
#7969 = VERTEX_POINT ( 'NONE', #147105 ) ;
#7968 = CARTESIAN_POINT ( 'NONE',  ( -16.82055514392394713, 9.950000000011197443, -188.3232019254582212 ) ) ;
#7970 = LINE ( 'NONE', #47062, #113125 ) ;
#7971 = CARTESIAN_POINT ( 'NONE',  ( 23.14999999999999858, 5.000000000011153745, -155.0947339810869323 ) ) ;
#7972 = ORIENTED_EDGE ( 'NONE', *, *, #96609, .F. ) ;
#7973 = CARTESIAN_POINT ( 'NONE',  ( -16.89155683852258250, 66.05000000001261640, -190.2457356349850386 ) ) ;
#7974 = DIRECTION ( 'NONE',  ( 0.000000000000000000, 0.000000000000000000, 1.000000000000000000 ) ) ;
#7975 = DIRECTION ( 'NONE',  ( -4.448008912761043807E-16, 1.000000000000000000, 0.000000000000000000 ) ) ;
#7976 = ADVANCED_FACE ( 'NONE', ( #191415 ), #12768, .T. ) ;
#7977 = LINE ( 'NONE', #109622, #218950 ) ;
#7978 = CARTESIAN_POINT ( 'NONE',  ( 21.05000000000000071, 67.22371710471941242, -94.53510676294000348 ) ) ;
#7979 = EDGE_LOOP ( 'NONE', ( #225849, #229391, #160463, #77323 ) ) ;
#7980 = DIRECTION ( 'NONE',  ( 1.000000000000000000, 0.000000000000000000, 0.000000000000000000 ) ) ;
#7981 = CARTESIAN_POINT ( 'NONE',  ( 23.14999999999999503, 53.32357432685029153, -235.0179440783709879 ) ) ;
#7982 = EDGE_CURVE ( 'NONE', #155422, #159476, #203135, .T. ) ;
#7983 = CIRCLE ( 'NONE', #157858, 1.749999999999998002 ) ;
#7984 = TOROIDAL_SURFACE ( 'NONE', #153772, 2.100000000000002309, 0.1000000000000000056 ) ;
#7985 =( LENGTH_UNIT ( ) NAMED_UNIT ( * ) SI_UNIT ( .MILLI., .METRE. ) );
#7986 = DIRECTION ( 'NONE',  ( 0.000000000000000000, 0.000000000000000000, 1.000000000000000000 ) ) ;
#7987 = ORIENTED_EDGE ( 'NONE', *, *, #121216, .F. ) ;
#7988 = VECTOR ( 'NONE', #37090, 1000.000000000000114 ) ;
#7989 = VERTEX_POINT ( 'NONE', #118269 ) ;
#7990 = ADVANCED_FACE ( 'NONE', ( #176985 ), #53150, .F. ) ;
#7991 = CARTESIAN_POINT ( 'NONE',  ( 21.13461538461538325, 65.38541703798651383, -124.2731074845243739 ) ) ;
#7992 = EDGE_CURVE ( 'NONE', #10114, #167448, #186598, .T. ) ;
#7993 = DIRECTION ( 'NONE',  ( -1.000000000000000000, 0.000000000000000000, 0.000000000000000000 ) ) ;
#7994 = DIRECTION ( 'NONE',  ( -0.000000000000000000, 1.000000000000000000, 0.000000000000000000 ) ) ;
#7995 = DIRECTION ( 'NONE',  ( 1.000000000000000000, 0.000000000000000000, 0.000000000000000000 ) ) ;
#7997 = CARTESIAN_POINT ( 'NONE',  ( 18.59999999999999076, 10.20857864377385127, -54.75000000000000000 ) ) ;
#7996 = DIRECTION ( 'NONE',  ( 0.000000000000000000, 0.000000000000000000, 1.000000000000000000 ) ) ;
#7998 = ADVANCED_FACE ( 'NONE', ( #175689 ), #78237, .T. ) ;
#8000 = CARTESIAN_POINT ( 'NONE',  ( -23.25000000000000000, 32.96286418198890544, -251.2069521516576174 ) ) ;
#7999 = AXIS2_PLACEMENT_3D ( 'NONE', #157090, #76238, #77504 ) ;
#8001 = CARTESIAN_POINT ( 'NONE',  ( -18.44085059012131822, 64.48598750652818978, -112.2828021654028419 ) ) ;
#8002 = DIRECTION ( 'NONE',  ( 0.000000000000000000, 6.938893903907234689E-15, -1.000000000000000000 ) ) ;
#8003 = AXIS2_PLACEMENT_3D ( 'NONE', #51252, #75987, #53858 ) ;
#8004 = FACE_OUTER_BOUND ( 'NONE', #18921, .T. ) ;
#8006 = ORIENTED_EDGE ( 'NONE', *, *, #197116, .F. ) ;
#8005 = CARTESIAN_POINT ( 'NONE',  ( 13.54577453029514444, 62.93791375105570296, -215.5805554555300887 ) ) ;
#8007 = DIRECTION ( 'NONE',  ( 1.000000000000000000, 0.000000000000000000, 0.000000000000000000 ) ) ;
#8008 = AXIS2_PLACEMENT_3D ( 'NONE', #61583, #79833, #198522 ) ;
#8009 = CARTESIAN_POINT ( 'NONE',  ( -23.25000000000000000, 4.350000000011156054, -146.2500000000000284 ) ) ;
#8011 = CARTESIAN_POINT ( 'NONE',  ( 21.05000000000000071, 1.115600667400684642E-11, -100.5000000000000426 ) ) ;
#8010 = DIRECTION ( 'NONE',  ( 1.000000000000000000, 0.000000000000000000, 0.000000000000000000 ) ) ;
#8012 = ORIENTED_EDGE ( 'NONE', *, *, #242193, .F. ) ;
#8013 = DIRECTION ( 'NONE',  ( 0.000000000000000000, 0.000000000000000000, -1.000000000000000000 ) ) ;
#8014 = CYLINDRICAL_SURFACE ( 'NONE', #183155, 0.09999999999998898659 ) ;
#8015 = EDGE_CURVE ( 'NONE', #54485, #165408, #55677, .T. ) ;
#8016 = CARTESIAN_POINT ( 'NONE',  ( -18.59999999999999787, 11.65000000001115232, -45.65000000000000568 ) ) ;
#8017 = DIRECTION ( 'NONE',  ( -0.7071067811865487940, 0.6909108974501226852, 0.1504730267678046352 ) ) ;
#8018 = CARTESIAN_POINT ( 'NONE',  ( 20.94999999999999929, 78.98983215084128062, -228.7927651294584450 ) ) ;
#8019 = VERTEX_POINT ( 'NONE', #56975 ) ;
#8020 = AXIS2_PLACEMENT_3D ( 'NONE', #82296, #161890, #62768 ) ;
#8021 = ORIENTED_EDGE ( 'NONE', *, *, #91479, .F. ) ;
#8022 = ADVANCED_FACE ( 'NONE', ( #54430 ), #253208, .F. ) ;
#8023 = CARTESIAN_POINT ( 'NONE',  ( 21.05000000000000071, 6.257814610487280937, -100.4022097086912311 ) ) ;
#8024 = ORIENTED_EDGE ( 'NONE', *, *, #16502, .F. ) ;
#8025 = DIRECTION ( 'NONE',  ( 1.000000000000000000, 0.000000000000000000, 0.000000000000000000 ) ) ;
#8026 = ORIENTED_EDGE ( 'NONE', *, *, #141615, .T. ) ;
#8027 = TOROIDAL_SURFACE ( 'NONE', #99554, 0.2000000000000000111, 0.1000000000000000056 ) ;
#8028 = FACE_OUTER_BOUND ( 'NONE', #180203, .T. ) ;
#8029 = TOROIDAL_SURFACE ( 'NONE', #20501, 11.70000000000000107, 0.1000000000000000056 ) ;
#8030 = AXIS2_PLACEMENT_3D ( 'NONE', #171208, #250684, #49920 ) ;
#8031 = CIRCLE ( 'NONE', #195480, 11.80000000000000426 ) ;
#8032 = PLANE ( 'NONE',  #1378 ) ;
#8033 = VERTEX_POINT ( 'NONE', #212246 ) ;
#8034 = AXIS2_PLACEMENT_3D ( 'NONE', #73330, #15921, #253206 ) ;
#8035 = CARTESIAN_POINT ( 'NONE',  ( -11.60000000000000320, -11.75000000000000000, 17.70000000000000639 ) ) ;
#8036 = CARTESIAN_POINT ( 'NONE',  ( -21.09096482362053493, 65.52752482441825066, -241.9864795316534867 ) ) ;
#8037 = CARTESIAN_POINT ( 'NONE',  ( -1.739115166359751170E-14, 11.65000000001114699, -79.25000000000004263 ) ) ;
#8038 = DIRECTION ( 'NONE',  ( -0.000000000000000000, -0.1686199900910312910, 0.9856811345164826488 ) ) ;
#8039 = CARTESIAN_POINT ( 'NONE',  ( -21.05000000000000071, 1.162701749949165642, -41.40000000000000568 ) ) ;
#8040 = DIRECTION ( 'NONE',  ( -1.000000000000000000, 0.000000000000000000, 0.000000000000000000 ) ) ;
#8041 = DIRECTION ( 'NONE',  ( 0.000000000000000000, 0.000000000000000000, -1.000000000000000000 ) ) ;
#8042 = ORIENTED_EDGE ( 'NONE', *, *, #205024, .T. ) ;
#8044 = FACE_OUTER_BOUND ( 'NONE', #239798, .T. ) ;
#8043 = CARTESIAN_POINT ( 'NONE',  ( -23.15000000000000213, 1.115600667400684642E-11, -167.4999999999999716 ) ) ;
#8045 = CIRCLE ( 'NONE', #41374, 0.1000000000000028644 ) ;
#8046 = ORIENTED_EDGE ( 'NONE', *, *, #97644, .F. ) ;
#8048 = VERTEX_POINT ( 'NONE', #17865 ) ;
#8047 = DIRECTION ( 'NONE',  ( -1.000000000000000000, 0.000000000000000000, 0.000000000000000000 ) ) ;
#8049 = VERTEX_POINT ( 'NONE', #173154 ) ;
#8050 = CARTESIAN_POINT ( 'NONE',  ( 20.94999999999999574, 68.13014604066189861, -227.7202878558733516 ) ) ;
#8051 = CARTESIAN_POINT ( 'NONE',  ( 18.53317502108576775, 10.32263460347359896, -72.56059579686719019 ) ) ;
#8052 = FACE_OUTER_BOUND ( 'NONE', #114743, .T. ) ;
#8053 = CARTESIAN_POINT ( 'NONE',  ( 20.95512820512820085, 65.37615131630020926, -128.8581939154367717 ) ) ;
#8054 = ORIENTED_EDGE ( 'NONE', *, *, #153797, .T. ) ;
#8055 = CARTESIAN_POINT ( 'NONE',  ( 20.94999999999999929, 71.00000000001158185, -57.11784146561126363 ) ) ;
#8056 = CARTESIAN_POINT ( 'NONE',  ( 18.49999999999999289, 10.25000000001115730, -158.6499999999999773 ) ) ;
#8057 = AXIS2_PLACEMENT_3D ( 'NONE', #75337, #94856, #133985 ) ;
#8058 = ORIENTED_EDGE ( 'NONE', *, *, #171497, .T. ) ;
#8059 = CIRCLE ( 'NONE', #70621, 0.9750000000000036415 ) ;
#8060 = DIRECTION ( 'NONE',  ( 1.000000000000000000, 0.000000000000000000, 0.000000000000000000 ) ) ;
#8061 = EDGE_CURVE ( 'NONE', #7150, #234336, #244819, .T. ) ;
#8063 = AXIS2_PLACEMENT_3D ( 'NONE', #192755, #17942, #14128 ) ;
#8062 = B_SPLINE_CURVE_WITH_KNOTS ( 'NONE', 3,
 ( #219873, #17811, #195213, #253853, #118214, #176931, #97326, #41276, #59481, #56916 ),
 .UNSPECIFIED., .F., .F.,
 ( 4, 3, 3, 4 ),
 ( 0.000000000000000000, 0.0002000000000002884074, 0.001000000000045112589, 0.001967863649472103085 ),
 .UNSPECIFIED. ) ;
#8064 = CARTESIAN_POINT ( 'NONE',  ( 6.000000000000060396, 64.25000000001119815, -25.92310748452479174 ) ) ;
#8065 = EDGE_LOOP ( 'NONE', ( #68434, #132216, #204611, #166288 ) ) ;
#8066 = DIRECTION ( 'NONE',  ( 0.000000000000000000, 0.000000000000000000, -1.000000000000000000 ) ) ;
#8067 = AXIS2_PLACEMENT_3D ( 'NONE', #217961, #75912, #141030 ) ;
#8068 = ORIENTED_EDGE ( 'NONE', *, *, #80450, .T. ) ;
#8069 = DIRECTION ( 'NONE',  ( 1.000000000000000000, 0.000000000000000000, 0.000000000000000000 ) ) ;
#8070 = ORIENTED_EDGE ( 'NONE', *, *, #171045, .T. ) ;
#8071 = CYLINDRICAL_SURFACE ( 'NONE', #58596, 0.1000000000000013656 ) ;
#8072 = EDGE_CURVE ( 'NONE', #153027, #239741, #199052, .T. ) ;
#8073 = CARTESIAN_POINT ( 'NONE',  ( -18.39999999999999858, 40.47920047438133651, -235.2678785906695396 ) ) ;
#8074 = CARTESIAN_POINT ( 'NONE',  ( 21.05000000000000071, 8.776282895303632259, -42.05862899514094977 ) ) ;
#8075 = DIRECTION ( 'NONE',  ( -1.000000000000000000, 1.207181226542539700E-16, -2.694675058168174199E-16 ) ) ;
#8076 = ADVANCED_FACE ( 'NONE', ( #34912 ), #75315, .F. ) ;
#8078 = EDGE_CURVE ( 'NONE', #15934, #56536, #149189, .T. ) ;
#8077 = AXIS2_PLACEMENT_3D ( 'NONE', #178306, #158746, #79159 ) ;
#8079 = VECTOR ( 'NONE', #6537, 1000.000000000000000 ) ;
#8080 = DIRECTION ( 'NONE',  ( 1.000000000000000000, 0.000000000000000000, -0.000000000000000000 ) ) ;
#8081 = CARTESIAN_POINT ( 'NONE',  ( 18.59999999999999076, 10.20857864377385127, -155.3500000000000227 ) ) ;
#8083 = CARTESIAN_POINT ( 'NONE',  ( 20.93975676684922504, 10.31104185824063180, -72.52045169831058047 ) ) ;
#8082 = AXIS2_PLACEMENT_3D ( 'NONE', #204972, #45921, #185436 ) ;
#8084 = EDGE_LOOP ( 'NONE', ( #68828, #88997 ) ) ;
#8086 = DIRECTION ( 'NONE',  ( 0.000000000000000000, 0.1350103645451946055, -0.9908441862701591329 ) ) ;
#8085 = CARTESIAN_POINT ( 'NONE',  ( -21.07928932188134041, 69.67148334361368711, -170.1220026301790540 ) ) ;
#8087 = ORIENTED_EDGE ( 'NONE', *, *, #57923, .T. ) ;
#8088 = DIRECTION ( 'NONE',  ( 2.952720810173289112E-16, 1.000000000000000000, 7.086529944415894657E-15 ) ) ;
#8089 = SPHERICAL_SURFACE ( 'NONE', #206107, 0.1000000000000000056 ) ;
#8090 = ADVANCED_FACE ( 'NONE', ( #255146 ), #74037, .F. ) ;
#8091 = CARTESIAN_POINT ( 'NONE',  ( -21.65000000000000213, 65.95000000001181206, -82.17310748452439384 ) ) ;
#8093 = ORIENTED_EDGE ( 'NONE', *, *, #45722, .T. ) ;
#8092 = CARTESIAN_POINT ( 'NONE',  ( -18.59999994787167310, -9.523637689750458435, -207.8824495347724337 ) ) ;
#8095 = ORIENTED_EDGE ( 'NONE', *, *, #190341, .F. ) ;
#8094 = DIRECTION ( 'NONE',  ( -1.000000000000000000, 0.000000000000000000, -0.000000000000000000 ) ) ;
#8096 = EDGE_CURVE ( 'NONE', #226091, #226316, #240751, .T. ) ;
#8097 = CYLINDRICAL_SURFACE ( 'NONE', #167345, 0.09999999999999939493 ) ;
#8098 = CARTESIAN_POINT ( 'NONE',  ( 23.24999999999999645, 11.75000000001113953, -176.7499999999999716 ) ) ;
#8100 = VERTEX_POINT ( 'NONE', #233102 ) ;
#8099 = DIRECTION ( 'NONE',  ( 0.000000000000000000, 0.000000000000000000, -1.000000000000000000 ) ) ;
#8101 = AXIS2_PLACEMENT_3D ( 'NONE', #7731, #5113, #84642 ) ;
#8102 = CARTESIAN_POINT ( 'NONE',  ( -23.15000000000000213, -8.663551401858004652, -143.5241011180673070 ) ) ;
#8103 = DIRECTION ( 'NONE',  ( 0.000000000000000000, 0.9968797965484670343, 0.07893460099023182075 ) ) ;
#8104 = EDGE_LOOP ( 'NONE', ( #9051, #232964, #127557, #58043, #78352 ) ) ;
#8105 = DIRECTION ( 'NONE',  ( 1.000000000000000000, 0.000000000000000000, 0.000000000000000000 ) ) ;
#8106 = EDGE_CURVE ( 'NONE', #170250, #20995, #163252, .T. ) ;
#8107 = VERTEX_POINT ( 'NONE', #115698 ) ;
#8108 = DIRECTION ( 'NONE',  ( -0.000000000000000000, -0.000000000000000000, 1.000000000000000000 ) ) ;
#8109 = LINE ( 'NONE', #107186, #126598 ) ;
#8110 = ORIENTED_EDGE ( 'NONE', *, *, #93148, .F. ) ;
#8112 = EDGE_CURVE ( 'NONE', #57960, #184752, #249141, .T. ) ;
#8111 = DIRECTION ( 'NONE',  ( 1.000000000000000000, 0.000000000000000000, 0.000000000000000000 ) ) ;
#8113 = CIRCLE ( 'NONE', #199669, 0.09999999999999939493 ) ;
#8114 = ORIENTED_EDGE ( 'NONE', *, *, #22855, .T. ) ;
#8115 = AXIS2_PLACEMENT_3D ( 'NONE', #112579, #13477, #92999 ) ;
#8116 = AXIS2_PLACEMENT_3D ( 'NONE', #30061, #151280, #109551 ) ;
#8117 = DIRECTION ( 'NONE',  ( 1.000000000000000000, 0.000000000000000000, 0.000000000000000000 ) ) ;
#8118 = VERTEX_POINT ( 'NONE', #15334 ) ;
#8119 = AXIS2_PLACEMENT_3D ( 'NONE', #19524, #117328, #255499 ) ;
#8120 = ORIENTED_EDGE ( 'NONE', *, *, #189483, .F. ) ;
#8121 = CARTESIAN_POINT ( 'NONE',  ( -18.48179518609235927, -9.518325300481611961, -73.88970557676125850 ) ) ;
#8122 = EDGE_LOOP ( 'NONE', ( #26697, #87654, #40215, #11669, #85136, #55965 ) ) ;
#8123 = DIRECTION ( 'NONE',  ( 0.000000000000000000, 0.1350103645451807555, 0.9908441862701609093 ) ) ;
#8124 = ORIENTED_EDGE ( 'NONE', *, *, #44046, .F. ) ;
#8126 = VERTEX_POINT ( 'NONE', #37459 ) ;
#8125 = CYLINDRICAL_SURFACE ( 'NONE', #151517, 0.09999999999999939493 ) ;
#8127 = CARTESIAN_POINT ( 'NONE',  ( -20.94999999999999929, 11.75000000001115197, -74.01480577065406408 ) ) ;
#8128 = ORIENTED_EDGE ( 'NONE', *, *, #5340, .F. ) ;
#8129 = ADVANCED_FACE ( 'NONE', ( #236921 ), #135240, .T. ) ;
#8130 = CARTESIAN_POINT ( 'NONE',  ( 20.84999999999999432, 77.16412189325330928, -128.6082593989527254 ) ) ;
#8131 = TOROIDAL_SURFACE ( 'NONE', #170676, 1.900000000000002576, 0.1000000000000000056 ) ;
#8132 = ORIENTED_EDGE ( 'NONE', *, *, #140855, .T. ) ;
#8135 = ORIENTED_EDGE ( 'NONE', *, *, #204998, .F. ) ;
#8134 = VERTEX_POINT ( 'NONE', #171859 ) ;
#8133 = DIRECTION ( 'NONE',  ( 1.000000000000000000, 0.000000000000000000, 0.000000000000000000 ) ) ;
#8137 = CARTESIAN_POINT ( 'NONE',  ( -20.64999999999999858, 73.60000000001200249, -116.2477294072864140 ) ) ;
#8136 = AXIS2_PLACEMENT_3D ( 'NONE', #64809, #85622, #68676 ) ;
#8138 = CARTESIAN_POINT ( 'NONE',  ( 17.23472005113827876, 63.05353557103203599, -211.8790868286480418 ) ) ;
#8139 = ORIENTED_EDGE ( 'NONE', *, *, #216232, .F. ) ;
#8140 = VECTOR ( 'NONE', #57598, 1000.000000000000000 ) ;
#8141 = EDGE_CURVE ( 'NONE', #255232, #208387, #202929, .T. ) ;
#8142 = EDGE_CURVE ( 'NONE', #128048, #79203, #99951, .T. ) ;
#8143 = ORIENTED_EDGE ( 'NONE', *, *, #72129, .F. ) ;
#8144 = DIRECTION ( 'NONE',  ( 0.000000000000000000, 0.9126074666063771490, 0.4088369013363281623 ) ) ;
#8145 = CARTESIAN_POINT ( 'NONE',  ( 21.05000000000000071, 4.813084112160680661, -45.44151775652382952 ) ) ;
#8147 = EDGE_LOOP ( 'NONE', ( #249487, #118290, #43417, #15641 ) ) ;
#8146 = DIRECTION ( 'NONE',  ( 1.000000000000000000, 0.000000000000000000, 0.000000000000000000 ) ) ;
#8148 = LINE ( 'NONE', #203771, #193827 ) ;
#8149 = ORIENTED_EDGE ( 'NONE', *, *, #71845, .F. ) ;
#8150 = EDGE_CURVE ( 'NONE', #234522, #142401, #243335, .T. ) ;
#8152 = ADVANCED_FACE ( 'NONE', ( #23040 ), #4794, .T. ) ;
#8151 = CARTESIAN_POINT ( 'NONE',  ( -23.25000000000000000, 1.115600667400684642E-11, -67.00000000000004263 ) ) ;
#8153 = CARTESIAN_POINT ( 'NONE',  ( 18.59999999999999076, 10.25000000001115552, -192.2499999999999716 ) ) ;
#8154 = EDGE_LOOP ( 'NONE', ( #211384, #232252, #151019, #196600 ) ) ;
#8155 = DIRECTION ( 'NONE',  ( 1.000000000000000000, 0.000000000000000000, -0.000000000000000000 ) ) ;
#8156 = CARTESIAN_POINT ( 'NONE',  ( 18.79999999999999716, 8.000000000000000000, 1.212568896937007867 ) ) ;
#8157 = EDGE_CURVE ( 'NONE', #69101, #143844, #83067, .T. ) ;
#8158 = VERTEX_POINT ( 'NONE', #24317 ) ;
#8160 = ORIENTED_EDGE ( 'NONE', *, *, #219294, .F. ) ;
#8159 = CARTESIAN_POINT ( 'NONE',  ( -20.54999999999999716, 78.17003882911672008, -228.8770135013149911 ) ) ;
#8161 = AXIS2_PLACEMENT_3D ( 'NONE', #252720, #233202, #32446 ) ;
#8163 = ADVANCED_FACE ( 'NONE', ( #124687 ), #132421, .T. ) ;
#8162 = DIRECTION ( 'NONE',  ( -0.000000000000000000, 0.8660254037844383745, -0.5000000000000003331 ) ) ;
#8165 = EDGE_CURVE ( 'NONE', #161497, #136482, #32498, .T. ) ;
#8164 = EDGE_CURVE ( 'NONE', #121991, #208753, #103349, .T. ) ;
#8167 = ORIENTED_EDGE ( 'NONE', *, *, #131549, .F. ) ;
#8166 = ORIENTED_EDGE ( 'NONE', *, *, #252973, .T. ) ;
#8168 = ORIENTED_EDGE ( 'NONE', *, *, #181764, .T. ) ;
#8169 = VERTEX_POINT ( 'NONE', #21742 ) ;
#8170 = DIRECTION ( 'NONE',  ( 0.000000000000000000, 0.8777080977375655291, -0.4791956752370622463 ) ) ;
#8171 = VECTOR ( 'NONE', #175043, 1000.000000000000000 ) ;
#8172 = ORIENTED_EDGE ( 'NONE', *, *, #199277, .T. ) ;
#8173 = CARTESIAN_POINT ( 'NONE',  ( -16.86445178670622980, 66.03778837089568299, -48.63233004640768087 ) ) ;
#8174 = DIRECTION ( 'NONE',  ( 1.000000000000000000, 0.000000000000000000, 0.000000000000000000 ) ) ;
#8175 = VERTEX_POINT ( 'NONE', #200371 ) ;
#8176 = ADVANCED_FACE ( 'NONE', ( #257710 ), #140377, .T. ) ;
#8177 = ORIENTED_EDGE ( 'NONE', *, *, #231117, .F. ) ;
#8178 = EDGE_CURVE ( 'NONE', #143511, #40310, #124050, .T. ) ;
#8179 = EDGE_CURVE ( 'NONE', #168030, #125538, #49195, .T. ) ;
#8181 = ORIENTED_EDGE ( 'NONE', *, *, #250406, .T. ) ;
#8180 = AXIS2_PLACEMENT_3D ( 'NONE', #169793, #217734, #76950 ) ;
#8182 = CIRCLE ( 'NONE', #153975, 0.09999999999999986677 ) ;
#8183 = EDGE_CURVE ( 'NONE', #171727, #182549, #159983, .T. ) ;
#8184 = DIRECTION ( 'NONE',  ( -2.578261006436900068E-14, 0.1350103645451904977, -0.9908441862701597991 ) ) ;
#8185 = ORIENTED_EDGE ( 'NONE', *, *, #57731, .F. ) ;
#8186 = CIRCLE ( 'NONE', #153980, 0.09999999999999459321 ) ;
#8187 = DIRECTION ( 'NONE',  ( 0.000000000000000000, 0.000000000000000000, -1.000000000000000000 ) ) ;
#8189 = VERTEX_POINT ( 'NONE', #60841 ) ;
#8188 = CARTESIAN_POINT ( 'NONE',  ( -18.59999999999999787, 67.23127455305835554, -235.8551265064784559 ) ) ;
#8190 = DIRECTION ( 'NONE',  ( 1.652117596168391700E-15, -1.000000000000000000, -6.982962677686266711E-15 ) ) ;
#8191 = DIRECTION ( 'NONE',  ( 1.000000000000000000, -0.000000000000000000, -0.000000000000000000 ) ) ;
#8192 = EDGE_CURVE ( 'NONE', #186298, #39957, #211529, .T. ) ;
#8193 = CIRCLE ( 'NONE', #29067, 0.1000000000000002554 ) ;
#8195 = VECTOR ( 'NONE', #217408, 1000.000000000000114 ) ;
#8194 = CARTESIAN_POINT ( 'NONE',  ( -16.87683809663752399, 9.950000000011142376, -146.6500000000000341 ) ) ;
#8196 = CARTESIAN_POINT ( 'NONE',  ( 21.00000000000000000, 66.25000000001199396, -115.3731074845243683 ) ) ;
#8197 = CARTESIAN_POINT ( 'NONE',  ( -18.41353343127310893, 85.50000000001263345, -196.4910380878245633 ) ) ;
#8199 = CYLINDRICAL_SURFACE ( 'NONE', #28734, 0.09999999999998898659 ) ;
#8198 = PLANE ( 'NONE',  #52843 ) ;
#8200 = DIRECTION ( 'NONE',  ( 0.000000000000000000, 0.8777080977375072424, -0.4791956752371691608 ) ) ;
#8201 = CARTESIAN_POINT ( 'NONE',  ( 22.45380639572713477, 75.99999985734899610, -181.7735403756410051 ) ) ;
#8202 = DIRECTION ( 'NONE',  ( 1.000000000000000000, 0.000000000000000000, 0.000000000000000000 ) ) ;
#8203 = ORIENTED_EDGE ( 'NONE', *, *, #1185, .T. ) ;
#8204 = AXIS2_PLACEMENT_3D ( 'NONE', #110220, #51506, #30725 ) ;
#8205 = VECTOR ( 'NONE', #251093, 1000.000000000000000 ) ;
#8206 = AXIS2_PLACEMENT_3D ( 'NONE', #18512, #175064, #58887 ) ;
#8207 = AXIS2_PLACEMENT_3D ( 'NONE', #72693, #68826, #152230 ) ;
#8208 = VECTOR ( 'NONE', #11597, 1000.000000000000000 ) ;
#8209 = VERTEX_POINT ( 'NONE', #141667 ) ;
#8211 = VERTEX_POINT ( 'NONE', #221196 ) ;
#8210 = CARTESIAN_POINT ( 'NONE',  ( -18.59999999999999787, 1.115600667400684642E-11, -200.9999999999999432 ) ) ;
#8212 = ORIENTED_EDGE ( 'NONE', *, *, #127289, .T. ) ;
#8213 = AXIS2_PLACEMENT_3D ( 'NONE', #31010, #132648, #133914 ) ;
#8214 = CARTESIAN_POINT ( 'NONE',  ( -17.29838795458362100, 65.62845014206578753, -91.62784876713939752 ) ) ;
#8215 = CARTESIAN_POINT ( 'NONE',  ( 20.11144452914042091, 9.933610851134151432, -141.8902934539496243 ) ) ;
#8216 = CARTESIAN_POINT ( 'NONE',  ( -18.50000000000000355, -1.263275465206102233, -141.9018646667464338 ) ) ;
#8217 = VERTEX_POINT ( 'NONE', #48989 ) ;
#8218 = SHAPE_REPRESENTATION_RELATIONSHIP ( 'NONE' , 'NONE' ,  #133560, #200717 ) ;
#8219 = CARTESIAN_POINT ( 'NONE',  ( 20.95512820512820795, 67.12384868372345181, -57.32293462539563222 ) ) ;
#8220 = FACE_OUTER_BOUND ( 'NONE', #58531, .T. ) ;
#8221 = CIRCLE ( 'NONE', #220604, 11.80000000000000426 ) ;
#8222 = ORIENTED_EDGE ( 'NONE', *, *, #162324, .T. ) ;
#8223 = DIRECTION ( 'NONE',  ( -1.000000000000000000, 0.000000000000000000, 0.000000000000000000 ) ) ;
#8224 = DIRECTION ( 'NONE',  ( 0.000000000000000000, 0.000000000000000000, -1.000000000000000000 ) ) ;
#8225 = CARTESIAN_POINT ( 'NONE',  ( 22.94999999999999929, 6.223900101154157483, 12.00000000000000000 ) ) ;
#8226 = CARTESIAN_POINT ( 'NONE',  ( 21.04999999999975557, 65.49746832288597886, -61.96427766744952237 ) ) ;
#8227 = FACE_OUTER_BOUND ( 'NONE', #199362, .T. ) ;
#8229 = ORIENTED_EDGE ( 'NONE', *, *, #28288, .F. ) ;
#8228 = CARTESIAN_POINT ( 'NONE',  ( 18.52928932188133970, 65.72071067813088519, -148.6731074845244223 ) ) ;
#8230 = CARTESIAN_POINT ( 'NONE',  ( 20.73486653747090003, 28.93140779147706709, -237.1870821964558900 ) ) ;
#8231 = CARTESIAN_POINT ( 'NONE',  ( -23.25000000000000000, 76.00000000001190870, -103.0231074845243029 ) ) ;
#8232 = CARTESIAN_POINT ( 'NONE',  ( 23.14999999999999858, 3.899999999999999467, -33.50000000000000000 ) ) ;
#8233 = CARTESIAN_POINT ( 'NONE',  ( -23.25000000000000000, -13.98128454229089357, -192.0195388455185821 ) ) ;
#8234 = EDGE_LOOP ( 'NONE', ( #7236, #24725, #141993, #49067 ) ) ;
#8235 = CARTESIAN_POINT ( 'NONE',  ( 20.94999999999999929, 62.04148992963929032, -247.7470044306132024 ) ) ;
#8236 = LINE ( 'NONE', #87741, #227715 ) ;
#8237 = EDGE_CURVE ( 'NONE', #35657, #237528, #115845, .T. ) ;
#8239 = DIRECTION ( 'NONE',  ( 0.000000000000000000, 0.000000000000000000, 1.000000000000000000 ) ) ;
#8238 = DIRECTION ( 'NONE',  ( 0.000000000000000000, -6.938893903907222067E-15, 1.000000000000000000 ) ) ;
#8240 = DIRECTION ( 'NONE',  ( 1.000000000000000000, -0.000000000000000000, -0.000000000000000000 ) ) ;
#8241 = CIRCLE ( 'NONE', #87319, 0.09999999999998898659 ) ;
#8242 = DIRECTION ( 'NONE',  ( -1.000000000000000000, 0.000000000000000000, 0.000000000000000000 ) ) ;
#8243 = CARTESIAN_POINT ( 'NONE',  ( 23.24999999999999645, 64.25000000001159606, -56.87310748452439668 ) ) ;
#8244 = CYLINDRICAL_SURFACE ( 'NONE', #255994, 0.1000000000000028644 ) ;
#8246 = EDGE_CURVE ( 'NONE', #235498, #165951, #9863, .T. ) ;
#8245 = CARTESIAN_POINT ( 'NONE',  ( 18.43565242384934066, 85.51932773110452501, -129.5501311079648872 ) ) ;
#8247 = CARTESIAN_POINT ( 'NONE',  ( -16.78270389226384296, 9.947372616628161524, -87.84120703691151277 ) ) ;
#8249 = ORIENTED_EDGE ( 'NONE', *, *, #204291, .F. ) ;
#8248 = AXIS2_PLACEMENT_3D ( 'NONE', #43210, #122764, #202282 ) ;
#8250 = EDGE_LOOP ( 'NONE', ( #41393, #142231, #124340, #101671, #151751 ) ) ;
#8251 = ORIENTED_EDGE ( 'NONE', *, *, #19825, .F. ) ;
#8252 = EDGE_CURVE ( 'NONE', #18469, #40984, #119978, .T. ) ;
#8253 = CARTESIAN_POINT ( 'NONE',  ( 20.94999999999999929, 65.27628289530409234, -61.85819391543678591 ) ) ;
#8254 = ADVANCED_FACE ( 'NONE', ( #187243 ), #53306, .T. ) ;
#8255 = DIRECTION ( 'NONE',  ( -1.000000000000000000, 0.000000000000000000, 1.073024830501117725E-15 ) ) ;
#8256 = VERTEX_POINT ( 'NONE', #65988 ) ;
#8257 = AXIS2_PLACEMENT_3D ( 'NONE', #124428, #203949, #4458 ) ;
#8258 = ORIENTED_EDGE ( 'NONE', *, *, #194341, .F. ) ;
#8259 = AXIS2_PLACEMENT_3D ( 'NONE', #155077, #115924, #95063 ) ;
#8260 = EDGE_LOOP ( 'NONE', ( #68690, #62572, #195289 ) ) ;
#8261 = CARTESIAN_POINT ( 'NONE',  ( -18.59999999999999787, 46.50671693017397246, -243.2369495081682942 ) ) ;
#8262 = CIRCLE ( 'NONE', #99796, 0.1999999999999987899 ) ;
#8263 = VERTEX_POINT ( 'NONE', #170275 ) ;
#8264 = EDGE_CURVE ( 'NONE', #13269, #162201, #108954, .T. ) ;
#8265 = CYLINDRICAL_SURFACE ( 'NONE', #38213, 0.1000000000000054040 ) ;
#8266 = CARTESIAN_POINT ( 'NONE',  ( -16.93211319090181988, 30.29384521580290013, -234.7972184746587914 ) ) ;
#8267 = EDGE_CURVE ( 'NONE', #74473, #120817, #70075, .T. ) ;
#8268 = DIRECTION ( 'NONE',  ( 1.000000000000000000, 0.000000000000000000, 0.000000000000000000 ) ) ;
#8269 = DIRECTION ( 'NONE',  ( 0.000000000000000000, -1.000000000000000000, 0.000000000000000000 ) ) ;
#8270 = LINE ( 'NONE', #68234, #108337 ) ;
#8271 = CARTESIAN_POINT ( 'NONE',  ( 22.39999999999999858, 7.790779598384538929, -66.90000000000004832 ) ) ;
#8273 = ORIENTED_EDGE ( 'NONE', *, *, #243138, .F. ) ;
#8272 = CARTESIAN_POINT ( 'NONE',  ( 20.95512820512820440, 44.11820694106862106, -236.4833523840365217 ) ) ;
#8275 = DIRECTION ( 'NONE',  ( 1.000000000000000000, 0.000000000000000000, 0.000000000000000000 ) ) ;
#8274 = DIRECTION ( 'NONE',  ( 0.000000000000000000, 0.9994937237965558774, 0.03181660087586650476 ) ) ;
#8276 = DIRECTION ( 'NONE',  ( -1.000000000000000000, -0.000000000000000000, -0.000000000000000000 ) ) ;
#8277 =( BOUNDED_SURFACE ( )  B_SPLINE_SURFACE ( 3, 2, ( 
 ( #34434, #151803, #252149 ),
 ( #91806, #113929, #214323 ),
 ( #35714, #158237, #198599 ),
 ( #241583, #390, #39571 ) ),
 .UNSPECIFIED., .F., .F., .F. ) 
 B_SPLINE_SURFACE_WITH_KNOTS ( ( 4, 4 ),
 ( 3, 3 ),
 ( 0.3000847527772385059, 0.5552748953338751958 ),
 ( 0.000000000000000000, 1.000000000000000000 ),
 .UNSPECIFIED. ) 
 GEOMETRIC_REPRESENTATION_ITEM ( )  RATIONAL_B_SPLINE_SURFACE ( (
 ( 1.000000000000000000, 0.9152888060719408525, 1.000000000000000000),
 ( 1.000000000000000000, 0.9104333467450420603, 1.000000000000000000),
 ( 1.000000000000000000, 0.9035312726220527946, 1.000000000000000000),
 ( 1.000000000000000000, 0.8946697475932202659, 1.000000000000000000) ) ) 
 REPRESENTATION_ITEM ( '' )  SURFACE ( )  );
#8278 = ORIENTED_EDGE ( 'NONE', *, *, #165648, .T. ) ;
#8279 = DIRECTION ( 'NONE',  ( 0.000000000000000000, 0.000000000000000000, -1.000000000000000000 ) ) ;
#8280 = CARTESIAN_POINT ( 'NONE',  ( 18.39999999999999503, 11.47316190337363828, -113.1500000000000341 ) ) ;
#8281 = CARTESIAN_POINT ( 'NONE',  ( -23.15000000000000213, 76.00000000001168132, -73.57310748452432847 ) ) ;
#8282 = EDGE_LOOP ( 'NONE', ( #25425, #85408, #157565, #183929 ) ) ;
#8283 = CARTESIAN_POINT ( 'NONE',  ( -18.50000000000000000, 76.00000000001165290, -69.52310748452431710 ) ) ;
#8284 = EDGE_CURVE ( 'NONE', #111708, #162622, #7501, .T. ) ;
#8285 = AXIS2_PLACEMENT_3D ( 'NONE', #182203, #225144, #3543 ) ;
#8286 = CIRCLE ( 'NONE', #187911, 0.5000000000000004441 ) ;
#8287 = CARTESIAN_POINT ( 'NONE',  ( -16.83558968593868954, 66.05000000001182059, -82.18541267214132517 ) ) ;
#8288 = EDGE_CURVE ( 'NONE', #13316, #159346, #153301, .T. ) ;
#8289 = EDGE_LOOP ( 'NONE', ( #122397, #183883, #202922, #205066, #55068, #46655 ) ) ;
#8290 = CYLINDRICAL_SURFACE ( 'NONE', #92832, 0.09999999999999939493 ) ;
#8291 = FACE_OUTER_BOUND ( 'NONE', #143303, .T. ) ;
#8292 =( BOUNDED_SURFACE ( )  B_SPLINE_SURFACE ( 3, 2, ( 
 ( #113888, #70943, #189586 ),
 ( #13515, #10950, #53916 ),
 ( #252106, #190889, #227407 ),
 ( #232582, #108750, #153063 ) ),
 .UNSPECIFIED., .F., .F., .F. ) 
 B_SPLINE_SURFACE_WITH_KNOTS ( ( 4, 4 ),
 ( 3, 3 ),
 ( 3.388131789017201356E-19, 0.0003124336117481281557 ),
 ( 0.000000000000000000, 1.000000000000000000 ),
 .UNSPECIFIED. ) 
 GEOMETRIC_REPRESENTATION_ITEM ( )  RATIONAL_B_SPLINE_SURFACE ( (
 ( 1.000000000000000000, 0.7040654476014488461, 1.000000000000000000),
 ( 1.000000000000000000, 0.7039193538784696003, 1.000000000000000000),
 ( 1.000000000000000000, 0.7089171279144220739, 1.000000000000000000),
 ( 1.000000000000000000, 0.7071067811864741870, 1.000000000000000000) ) ) 
 REPRESENTATION_ITEM ( '' )  SURFACE ( )  );
#8293 = CARTESIAN_POINT ( 'NONE',  ( -23.25000000000000000, 55.98745301258801987, -232.8057040749261262 ) ) ;
#8294 = CARTESIAN_POINT ( 'NONE',  ( -23.25000000000000355, 5.649999999999983480, -9.250000000000001776 ) ) ;
#8295 = ORIENTED_EDGE ( 'NONE', *, *, #197951, .F. ) ;
#8296 = ORIENTED_EDGE ( 'NONE', *, *, #10518, .T. ) ;
#8297 = EDGE_CURVE ( 'NONE', #233370, #89904, #230196, .T. ) ;
#8298 = EDGE_CURVE ( 'NONE', #105344, #76904, #51524, .T. ) ;
#8299 = PLANE ( 'NONE',  #36145 ) ;
#8300 = CARTESIAN_POINT ( 'NONE',  ( -20.64999999999999858, 74.00000000001180922, -82.74772940728641402 ) ) ;
#8301 = AXIS2_PLACEMENT_3D ( 'NONE', #253372, #119016, #96834 ) ;
#8302 = CARTESIAN_POINT ( 'NONE',  ( 20.94999999999999929, -1.835341550224413698, -11.55515129256298046 ) ) ;
#8304 = DIRECTION ( 'NONE',  ( 0.000000000000000000, 4.163336342344217877E-13, -1.000000000000000000 ) ) ;
#8303 = CIRCLE ( 'NONE', #74952, 0.1000000000000028644 ) ;
#8305 = VECTOR ( 'NONE', #207849, 1000.000000000000000 ) ;
#8306 = VECTOR ( 'NONE', #42552, 1000.000000000000000 ) ;
#8307 = EDGE_CURVE ( 'NONE', #190642, #86349, #30744, .T. ) ;
#8308 = CARTESIAN_POINT ( 'NONE',  ( 21.08198257630413508, 6.336596734026219480, -167.4273566762153678 ) ) ;
#8309 = CARTESIAN_POINT ( 'NONE',  ( 13.88638282980484107, 9.457426452500056868, -52.00004186840002518 ) ) ;
#8310 = CARTESIAN_POINT ( 'NONE',  ( -20.94999999999999929, 1.835341550235569663, -78.55515129256302487 ) ) ;
#8311 = VERTEX_POINT ( 'NONE', #248482 ) ;
#8313 =( BOUNDED_SURFACE ( )  B_SPLINE_SURFACE ( 3, 2, ( 
 ( #207553, #194418, #219073 ),
 ( #96549, #58707, #213958 ),
 ( #256878, #135684, #15790 ),
 ( #139536, #77005, #176137 ) ),
 .UNSPECIFIED., .F., .F., .F. ) 
 B_SPLINE_SURFACE_WITH_KNOTS ( ( 4, 4 ),
 ( 3, 3 ),
 ( 0.0008258556059633754111, 0.0009616864997633037737 ),
 ( 0.000000000000000000, 1.000000000000000000 ),
 .UNSPECIFIED. ) 
 GEOMETRIC_REPRESENTATION_ITEM ( )  RATIONAL_B_SPLINE_SURFACE ( (
 ( 1.000000000000000000, 0.9152888060719425178, 1.000000000000000000),
 ( 1.000000000000000000, 0.9327727094137996389, 1.000000000000000000),
 ( 1.000000000000000000, 0.9369023509258144200, 1.000000000000000000),
 ( 1.000000000000000000, 0.9246339933864667904, 1.000000000000000000) ) ) 
 REPRESENTATION_ITEM ( '' )  SURFACE ( )  );
#8312 = DIRECTION ( 'NONE',  ( 0.000000000000000000, -1.000000000000000000, -6.982962677686265922E-15 ) ) ;
#8314 = EDGE_CURVE ( 'NONE', #205773, #54224, #101501, .T. ) ;
#8316 = ORIENTED_EDGE ( 'NONE', *, *, #63567, .T. ) ;
#8315 = CARTESIAN_POINT ( 'NONE',  ( 21.05000000000000071, 8.776282895292474961, -12.15000000000000036 ) ) ;
#8317 = AXIS2_PLACEMENT_3D ( 'NONE', #58303, #195302, #136562 ) ;
#8318 = CARTESIAN_POINT ( 'NONE',  ( -20.94999999999999929, 1.162701749949165642, -41.40000000000000568 ) ) ;
#8319 = DIRECTION ( 'NONE',  ( 0.000000000000000000, -0.9915357197604792727, 0.1298341882520475943 ) ) ;
#8320 = CYLINDRICAL_SURFACE ( 'NONE', #196109, 4.049999999999998046 ) ;
#8321 = FACE_OUTER_BOUND ( 'NONE', #190599, .T. ) ;
#8323 = VERTEX_POINT ( 'NONE', #209344 ) ;
#8322 = DIRECTION ( 'NONE',  ( 1.000000000000000000, 0.000000000000000000, 0.000000000000000000 ) ) ;
#8324 = CARTESIAN_POINT ( 'NONE',  ( -18.57399277249657032, 65.66887361445387228, -164.4329845918269655 ) ) ;
#8325 = EDGE_CURVE ( 'NONE', #183282, #144164, #16102, .T. ) ;
#8326 = DIRECTION ( 'NONE',  ( 0.000000000000000000, 0.000000000000000000, -1.000000000000000000 ) ) ;
#8327 = CYLINDRICAL_SURFACE ( 'NONE', #32403, 0.09999999999999939493 ) ;
#8328 = ORIENTED_EDGE ( 'NONE', *, *, #146178, .T. ) ;
#8329 = CARTESIAN_POINT ( 'NONE',  ( 18.49999999999999645, 1.835341550235567887, -112.0551512925630249 ) ) ;
#8330 = CARTESIAN_POINT ( 'NONE',  ( -16.83233564386400971, 66.06977820342747520, -115.7985868210489997 ) ) ;
#8331 = CIRCLE ( 'NONE', #158370, 0.09999999999999939493 ) ;
#8332 = CARTESIAN_POINT ( 'NONE',  ( -23.24999999999999645, -9.599999999988845900, -73.70018939122203960 ) ) ;
#8333 = EDGE_CURVE ( 'NONE', #203922, #78455, #178413, .T. ) ;
#8334 = VERTEX_POINT ( 'NONE', #189794 ) ;
#8335 = CARTESIAN_POINT ( 'NONE',  ( -23.15000000000000213, 31.44980407958351165, -233.5445995079518866 ) ) ;
#8336 = CIRCLE ( 'NONE', #154110, 4.041421356237310469 ) ;
#8337 = ORIENTED_EDGE ( 'NONE', *, *, #251155, .F. ) ;
#8338 = LINE ( 'NONE', #33074, #105846 ) ;
#8339 = CARTESIAN_POINT ( 'NONE',  ( -20.65000000000000568, 68.75000000001207923, -123.8731074845243540 ) ) ;
#8340 = EDGE_CURVE ( 'NONE', #143787, #240784, #109903, .T. ) ;
#8341 = DIRECTION ( 'NONE',  ( 0.000000000000000000, 0.000000000000000000, -1.000000000000000000 ) ) ;
#8342 = ORIENTED_EDGE ( 'NONE', *, *, #13770, .F. ) ;
#8343 = CARTESIAN_POINT ( 'NONE',  ( 20.94999999999999929, 1.115600667400684642E-11, -200.9999999999999432 ) ) ;
#8344 = DIRECTION ( 'NONE',  ( 1.000000000000000000, -0.000000000000000000, -0.000000000000000000 ) ) ;
#8345 = DIRECTION ( 'NONE',  ( 0.000000000000000000, -0.9998779222360104635, -0.01562499999996343723 ) ) ;
#8347 = DIRECTION ( 'NONE',  ( 1.000000000000000000, 0.000000000000000000, 0.000000000000000000 ) ) ;
#8346 = VECTOR ( 'NONE', #155919, 999.9999999999998863 ) ;
#8348 = DIRECTION ( 'NONE',  ( 0.000000000000000000, -0.2128009952263608118, 0.9770955615653313941 ) ) ;
#8349 = VERTEX_POINT ( 'NONE', #206787 ) ;
#8351 = VERTEX_POINT ( 'NONE', #90676 ) ;
#8350 = CARTESIAN_POINT ( 'NONE',  ( -23.25000000000000000, 61.88149656937975607, -248.1136133839584090 ) ) ;
#8352 = VERTEX_POINT ( 'NONE', #247183 ) ;
#8353 = DIRECTION ( 'NONE',  ( 1.000000000000000000, -0.000000000000000000, -0.000000000000000000 ) ) ;
#8354 = ORIENTED_EDGE ( 'NONE', *, *, #249123, .F. ) ;
#8355 = CARTESIAN_POINT ( 'NONE',  ( 21.14999999999999858, 65.28660755661216797, -124.2731074845243739 ) ) ;
#8356 = CARTESIAN_POINT ( 'NONE',  ( 23.15000000000000213, -8.596261682231828516, -91.04987248284976431 ) ) ;
#8357 = VECTOR ( 'NONE', #28806, 1000.000000000000000 ) ;
#8358 = VERTEX_POINT ( 'NONE', #25591 ) ;
#8359 = LINE ( 'NONE', #9625, #132434 ) ;
#8360 = DIRECTION ( 'NONE',  ( 0.7071067811865388020, -0.7071067811865561215, 0.000000000000000000 ) ) ;
#8361 = FACE_OUTER_BOUND ( 'NONE', #85987, .T. ) ;
#8362 = EDGE_LOOP ( 'NONE', ( #69729, #35132, #24417, #47745 ) ) ;
#8363 = CARTESIAN_POINT ( 'NONE',  ( -21.05000000000000071, 87.48912529308798014, -105.9231074845242091 ) ) ;
#8365 = ORIENTED_EDGE ( 'NONE', *, *, #44147, .T. ) ;
#8364 = CYLINDRICAL_SURFACE ( 'NONE', #200842, 0.09999999999999939493 ) ;
#8366 = LINE ( 'NONE', #226086, #256594 ) ;
#8367 = DIRECTION ( 'NONE',  ( -0.7071067811865430208, 0.6909108974500454137, 0.1504730267681856082 ) ) ;
#8368 = AXIS2_PLACEMENT_3D ( 'NONE', #245016, #182499, #65096 ) ;
#8369 = VECTOR ( 'NONE', #108107, 1000.000000000000000 ) ;
#8370 = ORIENTED_EDGE ( 'NONE', *, *, #248103, .T. ) ;
#8371 = LINE ( 'NONE', #205258, #143519 ) ;
#8372 = CARTESIAN_POINT ( 'NONE',  ( -14.77738660682464200, 66.56344716000762674, -121.3451520117640712 ) ) ;
#8373 = DIRECTION ( 'NONE',  ( -0.000000000000000000, -0.9126074666063770380, -0.4088369013363281068 ) ) ;
#8374 = VERTEX_POINT ( 'NONE', #5999 ) ;
#8375 = CIRCLE ( 'NONE', #25130, 7.800000000000001599 ) ;
#8376 = ADVANCED_FACE ( 'NONE', ( #85513 ), #91965, .F. ) ;
#8377 = PLANE ( 'NONE',  #43223 ) ;
#8378 = CIRCLE ( 'NONE', #154156, 0.5000000000000004441 ) ;
#8379 = TOROIDAL_SURFACE ( 'NONE', #41707, 0.2000000000000000111, 0.1000000000000000056 ) ;
#8380 = ADVANCED_FACE ( 'NONE', ( #73719 ), #16309, .F. ) ;
#8381 = ORIENTED_EDGE ( 'NONE', *, *, #243551, .T. ) ;
#8382 = ADVANCED_FACE ( 'NONE', ( #155820 ), #112821, .F. ) ;
#8383 = CIRCLE ( 'NONE', #16774, 4.100000000000008527 ) ;
#8384 = VECTOR ( 'NONE', #143993, 999.9999999999998863 ) ;
#8385 = AXIS2_PLACEMENT_3D ( 'NONE', #32676, #27536, #211270 ) ;
#8386 = ORIENTED_EDGE ( 'NONE', *, *, #120907, .T. ) ;
#8387 = DIRECTION ( 'NONE',  ( 0.000000000000000000, 0.4930308989874729320, 0.8700118002898605818 ) ) ;
#8388 = CIRCLE ( 'NONE', #166629, 4.049999999999998046 ) ;
#8389 = VERTEX_POINT ( 'NONE', #151975 ) ;
#8390 = DIRECTION ( 'NONE',  ( 0.000000000000000000, -0.000000000000000000, 1.000000000000000000 ) ) ;
#8391 = EDGE_CURVE ( 'NONE', #152894, #220255, #175391, .T. ) ;
#8392 = CIRCLE ( 'NONE', #32802, 0.2000000000000000944 ) ;
#8393 = CARTESIAN_POINT ( 'NONE',  ( -16.84981964351528916, 66.08268176591369070, -182.8927090985447705 ) ) ;
#8395 = EDGE_LOOP ( 'NONE', ( #36790, #181896, #232032, #158705 ) ) ;
#8394 = CARTESIAN_POINT ( 'NONE',  ( 15.39793903038207112, 25.37811339336344929, -232.8563427119264873 ) ) ;
#8396 = LINE ( 'NONE', #10960, #11744 ) ;
#8397 = DIRECTION ( 'NONE',  ( 1.000000000000000000, 0.000000000000000000, -0.000000000000000000 ) ) ;
#8398 = CARTESIAN_POINT ( 'NONE',  ( 21.05000000000000071, 87.65000000001164437, -69.52310748452424605 ) ) ;
#8399 = FACE_OUTER_BOUND ( 'NONE', #57955, .T. ) ;
#8400 = DIRECTION ( 'NONE',  ( -1.000000000000000000, 3.265361837132813093E-16, 2.280189983783949500E-30 ) ) ;
#8401 = CARTESIAN_POINT ( 'NONE',  ( -2.995603634470829482E-16, 29.00069016757795026, -237.9048565010683376 ) ) ;
#8402 = DIRECTION ( 'NONE',  ( 1.000000000000000000, -7.304098846218133681E-16, -4.639676173203992654E-30 ) ) ;
#8404 = ORIENTED_EDGE ( 'NONE', *, *, #176839, .F. ) ;
#8403 = FACE_OUTER_BOUND ( 'NONE', #73943, .T. ) ;
#8405 = CARTESIAN_POINT ( 'NONE',  ( -23.15000000000000213, 1.115600667400684642E-11, -167.4999999999999716 ) ) ;
#8406 = ORIENTED_EDGE ( 'NONE', *, *, #238472, .F. ) ;
#8407 = DIRECTION ( 'NONE',  ( 0.000000000000000000, -7.026728003956683390E-15, 1.000000000000000000 ) ) ;
#8408 = LINE ( 'NONE', #47506, #2805 ) ;
#8409 = EDGE_CURVE ( 'NONE', #127854, #253340, #161849, .T. ) ;
#8410 = EDGE_CURVE ( 'NONE', #78107, #56045, #231497, .T. ) ;
#8411 = CARTESIAN_POINT ( 'NONE',  ( 20.87631937322877462, 65.52850496324685992, -195.9433616099437927 ) ) ;
#8412 = DIRECTION ( 'NONE',  ( 1.000000000000000000, 0.000000000000000000, 0.000000000000000000 ) ) ;
#8413 = ORIENTED_EDGE ( 'NONE', *, *, #8246, .F. ) ;
#8414 = AXIS2_PLACEMENT_3D ( 'NONE', #2948, #162056, #198589 ) ;
#8415 = CARTESIAN_POINT ( 'NONE',  ( 21.04999999999999716, 10.12429514711028666, -228.1852862148587064 ) ) ;
#8416 = CARTESIAN_POINT ( 'NONE',  ( -20.64999999999999858, 4.250000000011156409, -45.85000000000000142 ) ) ;
#8417 = AXIS2_PLACEMENT_3D ( 'NONE', #135443, #54626, #235829 ) ;
#8418 = EDGE_CURVE ( 'NONE', #79944, #210883, #257433, .T. ) ;
#8419 = ORIENTED_EDGE ( 'NONE', *, *, #17361, .F. ) ;
#8420 = AXIS2_PLACEMENT_3D ( 'NONE', #47549, #63273, #3285 ) ;
#8421 = DIRECTION ( 'NONE',  ( 0.000000000000000000, 0.000000000000000000, 1.000000000000000000 ) ) ;
#8422 = LINE ( 'NONE', #204038, #217879 ) ;
#8423 = ORIENTED_EDGE ( 'NONE', *, *, #165404, .T. ) ;
#8424 = CARTESIAN_POINT ( 'NONE',  ( -16.86379686415369861, 66.02478224075944979, -190.9564973736146953 ) ) ;
#8425 = EDGE_LOOP ( 'NONE', ( #174313, #122653, #121260 ) ) ;
#8426 = LINE ( 'NONE', #161086, #59093 ) ;
#8427 = EDGE_LOOP ( 'NONE', ( #194193, #49145, #32701, #63973 ) ) ;
#8428 = CIRCLE ( 'NONE', #41775, 0.09999999999998898659 ) ;
#8429 = FACE_OUTER_BOUND ( 'NONE', #91879, .T. ) ;
#8430 = EDGE_CURVE ( 'NONE', #51404, #22582, #120170, .T. ) ;
#8431 = CIRCLE ( 'NONE', #137580, 12.87499999999999822 ) ;
#8432 = CARTESIAN_POINT ( 'NONE',  ( -1.820710678118657944, 85.92928932189310842, -78.27310748452423184 ) ) ;
#8433 = ORIENTED_EDGE ( 'NONE', *, *, #69677, .T. ) ;
#8434 = ORIENTED_EDGE ( 'NONE', *, *, #81700, .T. ) ;
#8435 = DIRECTION ( 'NONE',  ( -0.000000000000000000, 0.2128009952263603677, -0.9770955615653313941 ) ) ;
#8436 = B_SPLINE_CURVE_WITH_KNOTS ( 'NONE', 3,
 ( #37919, #236090, #114864, #256887, #34083, #173609, #157891 ),
 .UNSPECIFIED., .F., .F.,
 ( 4, 3, 4 ),
 ( 0.000000000000000000, 0.0007844235214594318627, 0.001767853679404347454 ),
 .UNSPECIFIED. ) ;
#8438 = EDGE_LOOP ( 'NONE', ( #8472, #257065, #25713 ) ) ;
#8437 = CARTESIAN_POINT ( 'NONE',  ( 14.22821877134046531, 9.456028260519072859, -48.51119803506571060 ) ) ;
#8439 = CARTESIAN_POINT ( 'NONE',  ( 21.09787244211742419, 67.22462929267527443, -191.2838541002068666 ) ) ;
#8440 = VECTOR ( 'NONE', #57588, 1000.000000000000114 ) ;
#8441 = ORIENTED_EDGE ( 'NONE', *, *, #6376, .F. ) ;
#8442 = AXIS2_PLACEMENT_3D ( 'NONE', #197977, #37653, #221376 ) ;
#8443 = ADVANCED_FACE ( 'NONE', ( #13716 ), #55370, .T. ) ;
#8444 = ORIENTED_EDGE ( 'NONE', *, *, #28789, .F. ) ;
#8445 = DIRECTION ( 'NONE',  ( 0.8191520442889919096, -0.5735764363510460484, 0.000000000000000000 ) ) ;
#8446 = CYLINDRICAL_SURFACE ( 'NONE', #217872, 0.1000000000000013656 ) ;
#8447 = DIRECTION ( 'NONE',  ( 1.000000000000000000, 0.000000000000000000, 0.000000000000000000 ) ) ;
#8448 = EDGE_CURVE ( 'NONE', #91478, #194502, #116047, .T. ) ;
#8450 = EDGE_CURVE ( 'NONE', #35186, #166912, #78422, .T. ) ;
#8449 = CARTESIAN_POINT ( 'NONE',  ( -21.14999999999999858, 11.65000000001115588, -107.2838656629781866 ) ) ;
#8451 = CYLINDRICAL_SURFACE ( 'NONE', #206298, 0.09999999999999817368 ) ;
#8452 = DIRECTION ( 'NONE',  ( 0.000000000000000000, -0.9770955615653316162, -0.2128009952263604232 ) ) ;
#8453 = ORIENTED_EDGE ( 'NONE', *, *, #230162, .F. ) ;
#8454 = CARTESIAN_POINT ( 'NONE',  ( -16.94052228080552425, 66.01372026691369399, -182.6327319818550450 ) ) ;
#8455 = DIRECTION ( 'NONE',  ( 0.000000000000000000, -0.2617529984165031243, -0.9651348961777157509 ) ) ;
#8456 = CYLINDRICAL_SURFACE ( 'NONE', #257573, 0.1000000000000028644 ) ;
#8457 = AXIS2_PLACEMENT_3D ( 'NONE', #82873, #102439, #24248 ) ;
#8458 = DIRECTION ( 'NONE',  ( 0.000000000000000000, 0.9908441862701605762, 0.1350103645451835310 ) ) ;
#8459 = B_SPLINE_CURVE_WITH_KNOTS ( 'NONE', 3,
 ( #92915, #9529, #168669, #48657, #169948, #52500, #210322 ),
 .UNSPECIFIED., .F., .F.,
 ( 4, 3, 4 ),
 ( 0.000000000000000000, 0.0009834301579439998740, 0.001767853679402675614 ),
 .UNSPECIFIED. ) ;
#8460 = ORIENTED_EDGE ( 'NONE', *, *, #182641, .F. ) ;
#8461 = LINE ( 'NONE', #149270, #238692 ) ;
#8462 = EDGE_LOOP ( 'NONE', ( #194088, #90251, #198660, #143089 ) ) ;
#8463 = CARTESIAN_POINT ( 'NONE',  ( -20.94999999999999929, 76.00000000001165290, -69.52310748452431710 ) ) ;
#8464 = ORIENTED_EDGE ( 'NONE', *, *, #2918, .F. ) ;
#8465 = ADVANCED_FACE ( 'NONE', ( #194943 ), #116665, .F. ) ;
#8466 = ADVANCED_FACE ( 'NONE', ( #34586 ), #216540, .T. ) ;
#8467 = DIRECTION ( 'NONE',  ( 0.000000000000000000, 0.000000000000000000, 1.000000000000000000 ) ) ;
#8468 = DIRECTION ( 'NONE',  ( 0.000000000000000000, -0.9910465087640860649, 0.1335171055202901413 ) ) ;
#8469 = ORIENTED_EDGE ( 'NONE', *, *, #62876, .F. ) ;
#8470 = ORIENTED_EDGE ( 'NONE', *, *, #46537, .T. ) ;
#8472 = ORIENTED_EDGE ( 'NONE', *, *, #13200, .F. ) ;
#8471 = DIRECTION ( 'NONE',  ( -1.000000000000000000, -0.000000000000000000, -0.000000000000000000 ) ) ;
#8473 = DIRECTION ( 'NONE',  ( 0.000000000000000000, -0.9856811345164803173, -0.1686199900910455851 ) ) ;
#8474 = ORIENTED_EDGE ( 'NONE', *, *, #95101, .T. ) ;
#8475 = EDGE_CURVE ( 'NONE', #70449, #95060, #32689, .T. ) ;
#8476 = DIRECTION ( 'NONE',  ( 0.000000000000000000, 1.000000000000000000, 0.000000000000000000 ) ) ;
#8477 = CYLINDRICAL_SURFACE ( 'NONE', #210514, 0.09999999999999781286 ) ;
#8478 = ORIENTED_EDGE ( 'NONE', *, *, #239268, .T. ) ;
#8479 = ADVANCED_FACE ( 'NONE', ( #174123 ), #218310, .F. ) ;
#8481 = AXIS2_PLACEMENT_3D ( 'NONE', #64042, #24942, #240122 ) ;
#8480 = DIRECTION ( 'NONE',  ( 1.000000000000000000, 0.000000000000000000, 0.000000000000000000 ) ) ;
#8482 = VECTOR ( 'NONE', #159915, 1000.000000000000000 ) ;
#8484 = DIRECTION ( 'NONE',  ( -1.000000000000000000, 0.000000000000000000, 0.000000000000000000 ) ) ;
#8483 = AXIS2_PLACEMENT_3D ( 'NONE', #201322, #59202, #1822 ) ;
#8485 = EDGE_CURVE ( 'NONE', #134186, #96293, #140991, .T. ) ;
#8486 = ADVANCED_FACE ( 'NONE', ( #554 ), #195158, .F. ) ;
#8487 = ORIENTED_EDGE ( 'NONE', *, *, #215785, .F. ) ;
#8488 = VECTOR ( 'NONE', #210655, 1000.000000000000000 ) ;
#8489 = PLANE ( 'NONE',  #159865 ) ;
#8490 = EDGE_CURVE ( 'NONE', #11462, #149588, #249317, .T. ) ;
#8492 = ORIENTED_EDGE ( 'NONE', *, *, #175157, .T. ) ;
#8491 = DIRECTION ( 'NONE',  ( 1.000000000000000000, 0.000000000000000000, 0.000000000000000000 ) ) ;
#8493 = EDGE_CURVE ( 'NONE', #52785, #127250, #7713, .T. ) ;
#8494 = DIRECTION ( 'NONE',  ( 2.952720810173288619E-16, -1.000000000000000000, 0.000000000000000000 ) ) ;
#8495 = AXIS2_PLACEMENT_3D ( 'NONE', #47074, #186622, #90058 ) ;
#8496 = EDGE_CURVE ( 'NONE', #50189, #171936, #157583, .T. ) ;
#8497 = DIRECTION ( 'NONE',  ( 0.000000000000000000, 0.9126074666063545004, 0.4088369013363783999 ) ) ;
#8498 = CYLINDRICAL_SURFACE ( 'NONE', #3535, 0.09999999999999520384 ) ;
#8499 = LINE ( 'NONE', #245822, #165359 ) ;
#8501 = ADVANCED_FACE ( 'NONE', ( #63099 ), #162239, .T. ) ;
#8500 = CARTESIAN_POINT ( 'NONE',  ( 23.15000000000000213, -3.281532336344783030, -226.3283167004136942 ) ) ;
#8502 = CARTESIAN_POINT ( 'NONE',  ( 20.94999999999999929, -11.64999999998883595, -167.5000000000000000 ) ) ;
#8503 = DIRECTION ( 'NONE',  ( -4.701977403289178058E-30, 1.734723475976807094E-14, -1.000000000000000000 ) ) ;
#8504 = ORIENTED_EDGE ( 'NONE', *, *, #84140, .F. ) ;
#8505 = ORIENTED_EDGE ( 'NONE', *, *, #171145, .T. ) ;
#8506 = ORIENTED_EDGE ( 'NONE', *, *, #128820, .T. ) ;
#8507 = ADVANCED_FACE ( 'NONE', ( #41012 ), #160948, .T. ) ;
#8508 = CARTESIAN_POINT ( 'NONE',  ( 21.05000000000000071, 74.65091558138507821, -128.5366085209788309 ) ) ;
#8509 = CARTESIAN_POINT ( 'NONE',  ( 21.05000000000000071, 70.60000000001186038, -90.61784146561124942 ) ) ;
#8510 = ORIENTED_EDGE ( 'NONE', *, *, #32436, .T. ) ;
#8511 = DIRECTION ( 'NONE',  ( 0.000000000000000000, 0.000000000000000000, -1.000000000000000000 ) ) ;
#8512 = CIRCLE ( 'NONE', #141776, 0.09999999999999817368 ) ;
#8513 = B_SPLINE_CURVE_WITH_KNOTS ( 'NONE', 3,
 ( #115197, #194760, #112634, #31838, #16123, #91782, #192184, #111348, #136015, #73533, #95622, #231311, #76063, #175220, #254662, #52641, #30545, #59033, #21263 ),
 .UNSPECIFIED., .F., .F.,
 ( 4, 3, 3, 3, 3, 3, 4 ),
 ( 0.000000000000000000, 7.110282409889913185E-05, 0.0001508797727291429644, 0.0002027344179858502646, 0.0002343294522349018692, 0.0002454816334821173789, 0.0002619873080085545719 ),
 .UNSPECIFIED. ) ;
#8514 = CARTESIAN_POINT ( 'NONE',  ( -18.59999999999999787, 69.01799029515568407, -132.8269553662681233 ) ) ;
#8515 = VERTEX_POINT ( 'NONE', #98340 ) ;
#8516 = ORIENTED_EDGE ( 'NONE', *, *, #9222, .T. ) ;
#8517 = CARTESIAN_POINT ( 'NONE',  ( 18.39999999999999503, 43.39957528361355799, -233.6562381667159798 ) ) ;
#8518 = DIRECTION ( 'NONE',  ( 0.000000000000000000, 1.000000000000000000, 0.000000000000000000 ) ) ;
#8519 = ORIENTED_EDGE ( 'NONE', *, *, #202867, .T. ) ;
#8520 = AXIS2_PLACEMENT_3D ( 'NONE', #133955, #75308, #132695 ) ;
#8521 = DIRECTION ( 'NONE',  ( 0.000000000000000000, -0.2128009952263603677, 0.9770955615653313941 ) ) ;
#8523 = ORIENTED_EDGE ( 'NONE', *, *, #162197, .F. ) ;
#8522 = CARTESIAN_POINT ( 'NONE',  ( -16.98495255085916611, 65.99443563401705148, -82.15772469074488527 ) ) ;
#8524 = FACE_OUTER_BOUND ( 'NONE', #255435, .T. ) ;
#8525 = LINE ( 'NONE', #167616, #92328 ) ;
#8527 = ORIENTED_EDGE ( 'NONE', *, *, #195927, .F. ) ;
#8526 = DIRECTION ( 'NONE',  ( -1.000000000000000000, 0.000000000000000000, 0.000000000000000000 ) ) ;
#8528 = CARTESIAN_POINT ( 'NONE',  ( -21.14999999999999858, 33.98486250090727623, -243.5821103306120108 ) ) ;
#8529 = DIRECTION ( 'NONE',  ( 1.000000000000000000, -1.836970198721029934E-16, -1.282749433769087582E-30 ) ) ;
#8530 = CARTESIAN_POINT ( 'NONE',  ( -18.59999999999999787, 31.40887384169439756, -233.4092306946072313 ) ) ;
#8531 = EDGE_CURVE ( 'NONE', #137088, #28425, #179236, .T. ) ;
#8533 = CARTESIAN_POINT ( 'NONE',  ( 20.96937028524355640, 10.62446937163783289, -107.9914261011696510 ) ) ;
#8532 = DIRECTION ( 'NONE',  ( 0.000000000000000000, -1.000000000000000000, -6.982962677686266711E-15 ) ) ;
#8534 = CARTESIAN_POINT ( 'NONE',  ( 18.49999999999999289, 10.25000000263022848, -91.68717194963235784 ) ) ;
#8535 = VECTOR ( 'NONE', #201725, 1000.000000000000000 ) ;
#8536 = DIRECTION ( 'NONE',  ( 0.000000000000000000, 0.000000000000000000, 1.000000000000000000 ) ) ;
#8537 = EDGE_CURVE ( 'NONE', #4597, #235986, #45107, .T. ) ;
#8538 = CYLINDRICAL_SURFACE ( 'NONE', #134965, 0.1000000000000028644 ) ;
#8539 = DIRECTION ( 'NONE',  ( 0.000000000000000000, 2.775557561562812086E-13, 1.000000000000000000 ) ) ;
#8540 = VECTOR ( 'NONE', #11262, 1000.000000000000000 ) ;
#8541 = EDGE_LOOP ( 'NONE', ( #3333, #149503, #134538, #48320 ) ) ;
#8542 = ORIENTED_EDGE ( 'NONE', *, *, #151246, .T. ) ;
#8543 = ORIENTED_EDGE ( 'NONE', *, *, #215253, .T. ) ;
#8544 = DIRECTION ( 'NONE',  ( 0.000000000000000000, 0.000000000000000000, -1.000000000000000000 ) ) ;
#8545 = ORIENTED_EDGE ( 'NONE', *, *, #219137, .T. ) ;
#8547 = DIRECTION ( 'NONE',  ( 0.000000000000000000, -6.982962677686266711E-15, 1.000000000000000000 ) ) ;
#8546 = CIRCLE ( 'NONE', #37794, 12.87500000000000178 ) ;
#8548 = ORIENTED_EDGE ( 'NONE', *, *, #144022, .F. ) ;
#8549 = CARTESIAN_POINT ( 'NONE',  ( 23.14999999999999503, 64.35000000001146248, -43.03791325517834565 ) ) ;
#8550 = FACE_OUTER_BOUND ( 'NONE', #57139, .T. ) ;
#8551 = TOROIDAL_SURFACE ( 'NONE', #158425, 4.099999999999999645, 0.1000000000000000056 ) ;
#8552 = AXIS2_PLACEMENT_3D ( 'NONE', #234448, #233206, #134064 ) ;
#8553 = ORIENTED_EDGE ( 'NONE', *, *, #144050, .T. ) ;
#8554 = DIRECTION ( 'NONE',  ( 0.000000000000000000, 0.000000000000000000, 1.000000000000000000 ) ) ;
#8555 = SURFACE_SIDE_STYLE ('',( #107647 ) ) ;
#8556 = ADVANCED_FACE ( 'NONE', ( #103504 ), #200062, .T. ) ;
#8558 = ORIENTED_EDGE ( 'NONE', *, *, #58726, .T. ) ;
#8557 = AXIS2_PLACEMENT_3D ( 'NONE', #226669, #45474, #147133 ) ;
#8559 = ORIENTED_EDGE ( 'NONE', *, *, #126807, .T. ) ;
#8560 = VECTOR ( 'NONE', #171268, 1000.000000000000000 ) ;
#8561 = CIRCLE ( 'NONE', #16952, 0.1000000000000021844 ) ;
#8562 = EDGE_LOOP ( 'NONE', ( #255701, #145115, #165249, #119098 ) ) ;
#8563 = CIRCLE ( 'NONE', #175205, 0.5000000000000031086 ) ;
#8564 = AXIS2_PLACEMENT_3D ( 'NONE', #22063, #25911, #203248 ) ;
#8565 = DIRECTION ( 'NONE',  ( 2.952720810173289112E-16, 1.000000000000000000, 6.308085367188367561E-15 ) ) ;
#8566 = DIRECTION ( 'NONE',  ( -1.000000000000000000, 0.000000000000000000, -0.000000000000000000 ) ) ;
#8567 = CARTESIAN_POINT ( 'NONE',  ( 18.59999999999999076, 65.50857864377491069, -145.2731074845244450 ) ) ;
#8568 = DIRECTION ( 'NONE',  ( 0.000000000000000000, -1.000000000000000000, 0.000000000000000000 ) ) ;
#8569 = DIRECTION ( 'NONE',  ( 0.000000000000000000, 0.000000000000000000, 1.000000000000000000 ) ) ;
#8570 = DIRECTION ( 'NONE',  ( 0.000000000000000000, -0.8814952561688429444, 0.4721928772777348460 ) ) ;
#8571 = CARTESIAN_POINT ( 'NONE',  ( -20.94999999999999929, 7.120270961708750512, -104.1595630418393768 ) ) ;
#8573 = EDGE_LOOP ( 'NONE', ( #5190, #101742, #92941, #251946 ) ) ;
#8572 = CARTESIAN_POINT ( 'NONE',  ( 23.14999999999998792, 11.65000000001115588, -67.00000000000004263 ) ) ;
#8575 = CARTESIAN_POINT ( 'NONE',  ( 18.39999999999999503, 5.650000000011139001, -124.7500000000000426 ) ) ;
#8574 = CARTESIAN_POINT ( 'NONE',  ( 20.12481660106788084, 9.526343992285099205, -75.22614166909309574 ) ) ;
#8576 = CARTESIAN_POINT ( 'NONE',  ( 20.94999999999999574, 69.65000000001158753, -59.67928539484123718 ) ) ;
#8577 = ORIENTED_EDGE ( 'NONE', *, *, #62025, .T. ) ;
#8578 = CARTESIAN_POINT ( 'NONE',  ( -21.14999999999999503, 57.70204706108523141, -226.1016183162177526 ) ) ;
#8579 = CARTESIAN_POINT ( 'NONE',  ( 22.49999999999999645, 64.35012909624776967, -103.1056273753973329 ) ) ;
#8580 = CARTESIAN_POINT ( 'NONE',  ( -23.15000000000000213, 6.681951250119205987, -231.6808006331528986 ) ) ;
#8581 = ORIENTED_EDGE ( 'NONE', *, *, #11194, .F. ) ;
#8582 = CONICAL_SURFACE ( 'NONE', #129377, 4.299999999999970512, 0.7853981633974466137 ) ;
#8583 = DIRECTION ( 'NONE',  ( 1.000000000000000000, 0.000000000000000000, 0.000000000000000000 ) ) ;
#8584 = CARTESIAN_POINT ( 'NONE',  ( 21.05000000000005400, 82.72707916847673459, -26.51159310135756897 ) ) ;
#8585 = FACE_OUTER_BOUND ( 'NONE', #255240, .T. ) ;
#8586 = ORIENTED_EDGE ( 'NONE', *, *, #73518, .F. ) ;
#8587 = ORIENTED_EDGE ( 'NONE', *, *, #126989, .F. ) ;
#8588 = CARTESIAN_POINT ( 'NONE',  ( -18.59999999999999787, 11.65000000001115232, -146.1500000000000341 ) ) ;
#8589 = ORIENTED_EDGE ( 'NONE', *, *, #17279, .T. ) ;
#8590 = CARTESIAN_POINT ( 'NONE',  ( -20.85000000000000142, 14.80545736607782814, -235.9842437978701639 ) ) ;
#8591 = CARTESIAN_POINT ( 'NONE',  ( -20.94999999999999929, 74.16465844978787914, -158.4679561919613775 ) ) ;
#8592 = DIRECTION ( 'NONE',  ( 0.000000000000000000, 0.000000000000000000, -1.000000000000000000 ) ) ;
#8593 = ORIENTED_EDGE ( 'NONE', *, *, #120467, .F. ) ;
#8594 = EDGE_CURVE ( 'NONE', #20141, #222623, #20181, .T. ) ;
#8595 = AXIS2_PLACEMENT_3D ( 'NONE', #62647, #195754, #142169 ) ;
#8596 = CARTESIAN_POINT ( 'NONE',  ( -23.49999999999994316, 77.85126707825561709, -47.62635315998165453 ) ) ;
#8597 = FACE_OUTER_BOUND ( 'NONE', #119207, .T. ) ;
#8598 = CIRCLE ( 'NONE', #70980, 0.1000000000000124678 ) ;
#8599 = EDGE_CURVE ( 'NONE', #19886, #141624, #174333, .T. ) ;
#8600 = FACE_OUTER_BOUND ( 'NONE', #58788, .T. ) ;
#8601 = DIRECTION ( 'NONE',  ( 1.000000000000000000, 0.000000000000000000, 0.000000000000000000 ) ) ;
#8602 = VECTOR ( 'NONE', #204065, 1000.000000000000000 ) ;
#8603 = EDGE_LOOP ( 'NONE', ( #183168, #202275, #45569, #145165 ) ) ;
#8604 = DIRECTION ( 'NONE',  ( 1.000000000000000000, 0.000000000000000000, 0.000000000000000000 ) ) ;
#8605 = EDGE_CURVE ( 'NONE', #232010, #97749, #197477, .T. ) ;
#8606 = CIRCLE ( 'NONE', #62778, 0.1999999999999987899 ) ;
#8608 = ORIENTED_EDGE ( 'NONE', *, *, #561, .F. ) ;
#8607 = DIRECTION ( 'NONE',  ( -1.000000000000000000, 0.000000000000000000, 0.000000000000000000 ) ) ;
#8609 = CARTESIAN_POINT ( 'NONE',  ( -16.93860193097148326, 9.993107767340401182, -121.4001383673068801 ) ) ;
#8610 = CARTESIAN_POINT ( 'NONE',  ( 22.50000000000000000, 11.64957080755595520, -133.9000000000000057 ) ) ;
#8611 = FACE_OUTER_BOUND ( 'NONE', #73596, .T. ) ;
#8612 = CARTESIAN_POINT ( 'NONE',  ( -16.94107738177414291, 10.01423928514777373, -87.95000000000004547 ) ) ;
#8613 = ADVANCED_FACE ( 'NONE', ( #123100 ), #70272, .T. ) ;
#8614 = DIRECTION ( 'NONE',  ( -1.000000000000000000, -0.000000000000000000, -0.000000000000000000 ) ) ;
#8615 = ADVANCED_FACE ( 'NONE', ( #257399 ), #183075, .F. ) ;
#8616 = CARTESIAN_POINT ( 'NONE',  ( -18.59999999999999787, 9.350000000011156942, -179.8499999999999943 ) ) ;
#8617 = CARTESIAN_POINT ( 'NONE',  ( 13.40000000000000036, -9.650000000000002132, 15.00000000000000355 ) ) ;
#8618 = ORIENTED_EDGE ( 'NONE', *, *, #211407, .F. ) ;
#8619 = CARTESIAN_POINT ( 'NONE',  ( -20.85000000000000497, 11.74999999999999645, -26.58085275404129888 ) ) ;
#8620 = AXIS2_PLACEMENT_3D ( 'NONE', #113694, #152860, #232383 ) ;
#8621 = DIRECTION ( 'NONE',  ( 0.000000000000000000, -0.9998779222360097974, 0.01562500000000363945 ) ) ;
#8622 = CARTESIAN_POINT ( 'NONE',  ( -23.25000000000000000, 6.683038871553167226, -212.1840060551439819 ) ) ;
#8623 = CARTESIAN_POINT ( 'NONE',  ( 20.94999999999999574, 18.81166555858608902, -229.8642012822692777 ) ) ;
#8624 = EDGE_CURVE ( 'NONE', #118840, #171058, #136872, .T. ) ;
#8626 = AXIS2_PLACEMENT_3D ( 'NONE', #207408, #110856, #49601 ) ;
#8625 = DIRECTION ( 'NONE',  ( 0.000000000000000000, 0.000000000000000000, 1.000000000000000000 ) ) ;
#8627 = CARTESIAN_POINT ( 'NONE',  ( -17.78043020864321022, 10.85359211201684460, -190.6630491657201958 ) ) ;
#8628 = AXIS2_PLACEMENT_3D ( 'NONE', #94802, #152248, #93520 ) ;
#8629 = ORIENTED_EDGE ( 'NONE', *, *, #174392, .F. ) ;
#8630 = EDGE_LOOP ( 'NONE', ( #187142, #140200, #98638, #66259, #175709, #91850, #34871, #123145, #41679, #179427, #18883, #51049, #173763, #155058 ) ) ;
#8631 = AXIS2_PLACEMENT_3D ( 'NONE', #113043, #149624, #213409 ) ;
#8632 = CARTESIAN_POINT ( 'NONE',  ( -20.64999999999999858, 1.999999999999998224, -13.22462192276210224 ) ) ;
#8633 = CYLINDRICAL_SURFACE ( 'NONE', #97461, 0.09999999999998898659 ) ;
#8634 = DIRECTION ( 'NONE',  ( 0.000000000000000000, -1.000000000000000000, -6.982962677686265922E-15 ) ) ;
#8635 = ADVANCED_FACE ( 'NONE', ( #146483 ), #228627, .F. ) ;
#8636 = DIRECTION ( 'NONE',  ( -0.000000000000000000, 6.982962677686266711E-15, -1.000000000000000000 ) ) ;
#8637 = CARTESIAN_POINT ( 'NONE',  ( 21.05000000000000071, 8.776282895292474961, -8.558628995140949769 ) ) ;
#8638 = CARTESIAN_POINT ( 'NONE',  ( -21.05000000000000071, 70.10000000001235776, -159.8040077198679683 ) ) ;
#8639 = CARTESIAN_POINT ( 'NONE',  ( -16.93658623642901162, 9.980381671657131193, -12.61190272912918964 ) ) ;
#8640 = VERTEX_POINT ( 'NONE', #193027 ) ;
#8641 = CARTESIAN_POINT ( 'NONE',  ( -18.39999999999999858, 85.51932773110404185, -62.55013110796492271 ) ) ;
#8642 = ORIENTED_EDGE ( 'NONE', *, *, #67871, .T. ) ;
#8643 = DIRECTION ( 'NONE',  ( 0.000000000000000000, -0.2617529984165031243, -0.9651348961777157509 ) ) ;
#8644 = DIRECTION ( 'NONE',  ( 0.000000000000000000, 0.9126074666063545004, 0.4088369013363783999 ) ) ;
#8645 = CARTESIAN_POINT ( 'NONE',  ( -20.94999999999999929, 0.000000000000000000, 0.000000000000000000 ) ) ;
#8646 = DIRECTION ( 'NONE',  ( 6.938893903907225222E-15, 0.4088369013363283844, -0.9126074666063769270 ) ) ;
#8647 = FACE_OUTER_BOUND ( 'NONE', #161256, .T. ) ;
#8648 = CARTESIAN_POINT ( 'NONE',  ( 20.94999999999999929, 69.55000000001187743, -93.00608031408432907 ) ) ;
#8649 = LINE ( 'NONE', #88149, #118513 ) ;
#8650 = ORIENTED_EDGE ( 'NONE', *, *, #117411, .T. ) ;
#8651 = CARTESIAN_POINT ( 'NONE',  ( -16.93906926870270624, 22.92230643617488539, -230.8346921063524064 ) ) ;
#8652 = CARTESIAN_POINT ( 'NONE',  ( -13.39999999999994529, 67.65000000001118963, -16.98168612828748181 ) ) ;
#8653 = AXIS2_PLACEMENT_3D ( 'NONE', #196818, #160300, #140702 ) ;
#8654 = CYLINDRICAL_SURFACE ( 'NONE', #64915, 0.1000000000000076245 ) ;
#8655 = DIRECTION ( 'NONE',  ( 1.000000000000000000, 7.304098846218105085E-16, 4.217023435051676515E-16 ) ) ;
#8656 = VECTOR ( 'NONE', #27563, 1000.000000000000000 ) ;
#8657 = CARTESIAN_POINT ( 'NONE',  ( 18.52351027002948669, 85.64216290470703541, -96.30806053401445865 ) ) ;
#8658 = CARTESIAN_POINT ( 'NONE',  ( 20.94999999999999574, 64.37928932189383602, -176.8915241368654279 ) ) ;
#8659 = EDGE_CURVE ( 'NONE', #206737, #26294, #170063, .T. ) ;
#8660 = VECTOR ( 'NONE', #53853, 1000.000000000000000 ) ;
#8661 = VERTEX_POINT ( 'NONE', #30423 ) ;
#8662 = DIRECTION ( 'NONE',  ( 0.000000000000000000, 0.2617529984165036239, 0.9651348961777156399 ) ) ;
#8663 = DIRECTION ( 'NONE',  ( 1.000000000000000000, -0.000000000000000000, -0.000000000000000000 ) ) ;
#8664 = VERTEX_POINT ( 'NONE', #46109 ) ;
#8665 = EDGE_CURVE ( 'NONE', #121258, #109697, #107641, .T. ) ;
#8666 = ORIENTED_EDGE ( 'NONE', *, *, #174058, .F. ) ;
#8667 = CARTESIAN_POINT ( 'NONE',  ( -20.85000000000000142, 65.66751761918722252, -164.4282609406112670 ) ) ;
#8668 = FACE_OUTER_BOUND ( 'NONE', #237529, .T. ) ;
#8669 = CIRCLE ( 'NONE', #455, 0.1000000000000028644 ) ;
#8670 = CARTESIAN_POINT ( 'NONE',  ( -21.04999999999994387, 87.50449464844290048, -34.18759587077607165 ) ) ;
#8671 = ADVANCED_FACE ( 'NONE', ( #5678 ), #226001, .T. ) ;
#8672 = ORIENTED_EDGE ( 'NONE', *, *, #164104, .T. ) ;
#8674 = ADVANCED_FACE ( 'NONE', ( #8291 ), #166141, .T. ) ;
#8673 = DIRECTION ( 'NONE',  ( -3.787827842127535236E-15, 0.7397360091702777085, 0.6728971962616808744 ) ) ;
#8675 = DIRECTION ( 'NONE',  ( -1.000000000000000000, 0.000000000000000000, 0.000000000000000000 ) ) ;
#8676 = ORIENTED_EDGE ( 'NONE', *, *, #190134, .F. ) ;
#8677 = CARTESIAN_POINT ( 'NONE',  ( -21.04999999999999716, 76.08574093704538654, -109.4369337733372589 ) ) ;
#8678 = ORIENTED_EDGE ( 'NONE', *, *, #174264, .T. ) ;
#8679 = FACE_OUTER_BOUND ( 'NONE', #136288, .T. ) ;
#8680 = ADVANCED_FACE ( 'NONE', ( #246877 ), #29170, .T. ) ;
#8681 = DIRECTION ( 'NONE',  ( -2.952720810173289112E-16, 1.000000000000000000, 0.000000000000000000 ) ) ;
#8682 = AXIS2_PLACEMENT_3D ( 'NONE', #126977, #164827, #224775 ) ;
#8683 = FACE_OUTER_BOUND ( 'NONE', #14893, .T. ) ;
#8684 = DIRECTION ( 'NONE',  ( 0.000000000000000000, -0.9876197685951252359, -0.1568667991644863424 ) ) ;
#8686 = CARTESIAN_POINT ( 'NONE',  ( -23.25000000000000000, 11.75000000001115552, -146.1500000000000341 ) ) ;
#8685 = UNCERTAINTY_MEASURE_WITH_UNIT (LENGTH_MEASURE( 1.000000000000000082E-05 ), #87038, 'distance_accuracy_value', 'NONE');
#8687 = EDGE_CURVE ( 'NONE', #80054, #177338, #126943, .T. ) ;
#8688 = CARTESIAN_POINT ( 'NONE',  ( 20.94999999999999574, 55.13994374908182294, -226.9527081427897315 ) ) ;
#8689 = DIRECTION ( 'NONE',  ( -1.000000000000000000, 0.000000000000000000, 0.000000000000000000 ) ) ;
#8690 = LINE ( 'NONE', #69968, #162667 ) ;
#8691 = VECTOR ( 'NONE', #79131, 1000.000000000000000 ) ;
#8692 = DIRECTION ( 'NONE',  ( -1.000000000000000000, 0.000000000000000000, -0.000000000000000000 ) ) ;
#8693 = DIRECTION ( 'NONE',  ( 0.000000000000000000, -7.487053152578127080E-15, 1.000000000000000000 ) ) ;
#8695 = ORIENTED_EDGE ( 'NONE', *, *, #46095, .T. ) ;
#8694 = CARTESIAN_POINT ( 'NONE',  ( -23.15000000000000213, 64.25000000001277556, -215.2731074845244450 ) ) ;
#8696 = ORIENTED_EDGE ( 'NONE', *, *, #638, .F. ) ;
#8698 = CARTESIAN_POINT ( 'NONE',  ( -12.33960340485503338, 9.360749169926259938, -84.31457014060730160 ) ) ;
#8697 = CARTESIAN_POINT ( 'NONE',  ( 23.04999999999999716, 8.822561741677553471, -91.25000000000005684 ) ) ;
#8700 = VERTEX_POINT ( 'NONE', #93909 ) ;
#8699 = DIRECTION ( 'NONE',  ( 0.7071067811865475727, 0.7071067811865475727, 4.937700262164531476E-15 ) ) ;
#8701 = VECTOR ( 'NONE', #100095, 1000.000000000000000 ) ;
#8702 = VERTEX_POINT ( 'NONE', #244305 ) ;
#8703 = CARTESIAN_POINT ( 'NONE',  ( -23.15000000000000213, -11.48912529306489994, -97.40000000000004832 ) ) ;
#8704 = CARTESIAN_POINT ( 'NONE',  ( 21.13461538461538325, 67.11458296203740304, -90.67310748452436542 ) ) ;
#8706 = EDGE_CURVE ( 'NONE', #68947, #64432, #68256, .T. ) ;
#8705 = DIRECTION ( 'NONE',  ( 0.000000000000000000, 0.000000000000000000, 1.000000000000000000 ) ) ;
#8707 = VECTOR ( 'NONE', #57630, 1000.000000000000000 ) ;
#8708 = CARTESIAN_POINT ( 'NONE',  ( 21.30000000000002558, 76.00000000001165290, -69.52310748452431710 ) ) ;
#8709 = EDGE_CURVE ( 'NONE', #78560, #125024, #7906, .T. ) ;
#8710 = EDGE_CURVE ( 'NONE', #27906, #26421, #182876, .T. ) ;
#8711 = CARTESIAN_POINT ( 'NONE',  ( 23.14999999999999858, 8.111588099649802430, -211.9294447938511325 ) ) ;
#8712 = LINE ( 'NONE', #88213, #182042 ) ;
#8713 = CARTESIAN_POINT ( 'NONE',  ( 23.14999999999998437, 67.23127455305841238, -235.8551265064783991 ) ) ;
#8714 = EDGE_LOOP ( 'NONE', ( #255498, #165470, #247723, #119550 ) ) ;
#8715 = EDGE_LOOP ( 'NONE', ( #119483, #80069, #106394, #248552, #96259 ) ) ;
#8716 = DIRECTION ( 'NONE',  ( 0.000000000000000000, 0.000000000000000000, -1.000000000000000000 ) ) ;
#8717 = AXIS2_PLACEMENT_3D ( 'NONE', #215825, #196281, #137573 ) ;
#8718 = EDGE_LOOP ( 'NONE', ( #194100, #65864, #83870 ) ) ;
#8719 = DIRECTION ( 'NONE',  ( -0.000000000000000000, -6.982962677686266711E-15, 1.000000000000000000 ) ) ;
#8721 = VERTEX_POINT ( 'NONE', #206478 ) ;
#8720 = CIRCLE ( 'NONE', #187806, 0.1000000000000028644 ) ;
#8722 = FACE_OUTER_BOUND ( 'NONE', #158128, .T. ) ;
#8723 = VECTOR ( 'NONE', #103285, 1000.000000000000000 ) ;
#8724 = CIRCLE ( 'NONE', #192096, 0.09999999999999939493 ) ;
#8725 = FACE_OUTER_BOUND ( 'NONE', #113130, .T. ) ;
#8726 = DIRECTION ( 'NONE',  ( 0.000000000000000000, 0.000000000000000000, -1.000000000000000000 ) ) ;
#8727 = CARTESIAN_POINT ( 'NONE',  ( -23.15000000000000213, 0.000000000000000000, 0.000000000000000000 ) ) ;
#8728 = ORIENTED_EDGE ( 'NONE', *, *, #159407, .F. ) ;
#8729 = CIRCLE ( 'NONE', #104560, 2.100000000000002309 ) ;
#8731 = CIRCLE ( 'NONE', #83529, 0.09999999999999939493 ) ;
#8730 = LINE ( 'NONE', #102659, #4578 ) ;
#8732 = ORIENTED_EDGE ( 'NONE', *, *, #61703, .T. ) ;
#8733 = CARTESIAN_POINT ( 'NONE',  ( 21.97500000000000497, 14.04870287383362992, -219.6884709798078177 ) ) ;
#8734 = CYLINDRICAL_SURFACE ( 'NONE', #218974, 0.09999999999999939493 ) ;
#8735 = EDGE_CURVE ( 'NONE', #124002, #56789, #24664, .T. ) ;
#8736 = CARTESIAN_POINT ( 'NONE',  ( 18.48536876927990846, 8.873546741997410336, -245.4030630292437820 ) ) ;
#8737 = ORIENTED_EDGE ( 'NONE', *, *, #202652, .F. ) ;
#8738 = DIRECTION ( 'NONE',  ( 0.000000000000000000, -0.2617529984165152257, -0.9651348961777124202 ) ) ;
#8739 = VERTEX_POINT ( 'NONE', #207788 ) ;
#8741 = ORIENTED_EDGE ( 'NONE', *, *, #121649, .T. ) ;
#8740 = CARTESIAN_POINT ( 'NONE',  ( -18.39999999999999858, -9.599999999988844124, -107.5320693966997112 ) ) ;
#8742 = CIRCLE ( 'NONE', #225386, 0.1000000000000028644 ) ;
#8743 = CARTESIAN_POINT ( 'NONE',  ( -20.54999999999999716, 68.85000000001259934, -191.1731074845243938 ) ) ;
#8744 = VECTOR ( 'NONE', #154057, 1000.000000000000227 ) ;
#8746 = VERTEX_POINT ( 'NONE', #25290 ) ;
#8745 = AXIS2_PLACEMENT_3D ( 'NONE', #6672, #125351, #206170 ) ;
#8747 = VECTOR ( 'NONE', #120856, 1000.000000000000114 ) ;
#8748 = AXIS2_PLACEMENT_3D ( 'NONE', #226713, #131477, #71530 ) ;
#8749 = DIRECTION ( 'NONE',  ( 1.000000000000000000, -0.000000000000000000, -0.000000000000000000 ) ) ;
#8750 = EDGE_LOOP ( 'NONE', ( #71673, #162290, #212872, #225772 ) ) ;
#8751 = ADVANCED_FACE ( 'NONE', ( #188202 ), #49963, .T. ) ;
#8752 = DIRECTION ( 'NONE',  ( 1.000000000000000000, 0.000000000000000000, 0.000000000000000000 ) ) ;
#8753 = FACE_OUTER_BOUND ( 'NONE', #211188, .T. ) ;
#8754 = CARTESIAN_POINT ( 'NONE',  ( -17.27223548806215447, 52.62863847120288341, -231.0608408311660753 ) ) ;
#8755 = ADVANCED_FACE ( 'NONE', ( #9549 ), #86494, .F. ) ;
#8756 = CARTESIAN_POINT ( 'NONE',  ( -16.89797118371608775, 66.02361927736821201, -123.9604008520823157 ) ) ;
#8757 = VECTOR ( 'NONE', #12999, 1000.000000000000000 ) ;
#8758 = ORIENTED_EDGE ( 'NONE', *, *, #32710, .F. ) ;
#8759 = EDGE_CURVE ( 'NONE', #123338, #186188, #168688, .T. ) ;
#8760 = CARTESIAN_POINT ( 'NONE',  ( -21.05000000000000071, 1.658775325997247752, -230.6916041481598540 ) ) ;
#8761 = CARTESIAN_POINT ( 'NONE',  ( -13.43673303185030399, 66.55335100938341952, -154.9339441886012310 ) ) ;
#8762 = ORIENTED_EDGE ( 'NONE', *, *, #238929, .F. ) ;
#8763 = CARTESIAN_POINT ( 'NONE',  ( -23.25000000000000355, 19.98098358856834977, -229.3296076283783407 ) ) ;
#8764 = ORIENTED_EDGE ( 'NONE', *, *, #230041, .T. ) ;
#8765 = DIRECTION ( 'NONE',  ( 1.000000000000000000, -0.000000000000000000, -0.000000000000000000 ) ) ;
#8766 = EDGE_CURVE ( 'NONE', #68352, #179647, #20789, .T. ) ;
#8767 = EDGE_CURVE ( 'NONE', #144474, #1798, #157792, .T. ) ;
#8768 = DIRECTION ( 'NONE',  ( 1.000000000000000000, 0.000000000000000000, 0.000000000000000000 ) ) ;
#8769 = DIRECTION ( 'NONE',  ( -1.000000000000000000, 0.000000000000000000, -0.000000000000000000 ) ) ;
#8771 = VERTEX_POINT ( 'NONE', #76910 ) ;
#8770 = CARTESIAN_POINT ( 'NONE',  ( -16.84793658983368303, 44.21181828874585307, -235.2647337580439739 ) ) ;
#8772 = CARTESIAN_POINT ( 'NONE',  ( 21.14999999999999858, 8.786607556611267356, -45.85000000000000142 ) ) ;
#8773 = AXIS2_PLACEMENT_3D ( 'NONE', #107860, #183562, #64881 ) ;
#8774 = CARTESIAN_POINT ( 'NONE',  ( -12.25000000000000178, 62.59162599727320497, -217.2417264603073477 ) ) ;
#8775 = CARTESIAN_POINT ( 'NONE',  ( -23.25000000000000000, -1.149570369564537842, -208.8159124845019221 ) ) ;
#8776 = ORIENTED_EDGE ( 'NONE', *, *, #146384, .T. ) ;
#8777 = DIRECTION ( 'NONE',  ( 1.186688945009010077E-16, 1.000000000000000000, 6.982962677686266711E-15 ) ) ;
#8778 = CYLINDRICAL_SURFACE ( 'NONE', #94073, 0.09999999999999939493 ) ;
#8779 = ORIENTED_EDGE ( 'NONE', *, *, #133673, .T. ) ;
#8780 = CARTESIAN_POINT ( 'NONE',  ( 21.04999999999999716, 1.529241108124774984, -230.7757353094251584 ) ) ;
#8781 = CIRCLE ( 'NONE', #154383, 0.5000000000000007772 ) ;
#8782 = EDGE_CURVE ( 'NONE', #123203, #203424, #114032, .T. ) ;
#8783 = EDGE_CURVE ( 'NONE', #55258, #25682, #151495, .T. ) ;
#8784 = ORIENTED_EDGE ( 'NONE', *, *, #137079, .T. ) ;
#8786 = DIRECTION ( 'NONE',  ( 0.000000000000000000, -0.2617529984165152257, -0.9651348961777124202 ) ) ;
#8785 = CIRCLE ( 'NONE', #191973, 0.09999999999998898659 ) ;
#8788 = ORIENTED_EDGE ( 'NONE', *, *, #183323, .T. ) ;
#8787 = CARTESIAN_POINT ( 'NONE',  ( -18.59999999999999787, -1.164121893230052995, -208.9148480855715775 ) ) ;
#8789 = ADVANCED_FACE ( 'NONE', ( #54776 ), #134304, .T. ) ;
#8792 = ORIENTED_EDGE ( 'NONE', *, *, #73860, .T. ) ;
#8791 = ORIENTED_EDGE ( 'NONE', *, *, #149288, .F. ) ;
#8790 = LINE ( 'NONE', #111739, #238806 ) ;
#8793 = CARTESIAN_POINT ( 'NONE',  ( -20.54999999999999716, 4.250000000000000000, -12.35000000000000142 ) ) ;
#8794 = DIRECTION ( 'NONE',  ( 0.000000000000000000, 6.982962677686266711E-15, -1.000000000000000000 ) ) ;
#8795 = EDGE_CURVE ( 'NONE', #22560, #72929, #49582, .T. ) ;
#8796 = LINE ( 'NONE', #25788, #10927 ) ;
#8798 = CARTESIAN_POINT ( 'NONE',  ( -18.50000000000000000, 22.38308386859736032, -231.4104522272575082 ) ) ;
#8797 = CARTESIAN_POINT ( 'NONE',  ( 22.50000000000000000, 0.1000000000111554016, -88.85042919245522341 ) ) ;
#8799 = DIRECTION ( 'NONE',  ( -0.5932847527679310229, 0.8049926720990042694, -6.366092712777067056E-16 ) ) ;
#8801 = EDGE_CURVE ( 'NONE', #20836, #98230, #186979, .T. ) ;
#8800 = DIRECTION ( 'NONE',  ( -1.000000000000000000, -0.000000000000000000, -0.000000000000000000 ) ) ;
#8802 = AXIS2_PLACEMENT_3D ( 'NONE', #75305, #16608, #213493 ) ;
#8803 = PLANE ( 'NONE',  #222166 ) ;
#8804 = CIRCLE ( 'NONE', #154584, 4.099999999999988098 ) ;
#8805 = PLANE ( 'NONE',  #213182 ) ;
#8807 = ORIENTED_EDGE ( 'NONE', *, *, #53836, .F. ) ;
#8806 = AXIS2_PLACEMENT_3D ( 'NONE', #186390, #127694, #207236 ) ;
#8808 = ORIENTED_EDGE ( 'NONE', *, *, #234202, .F. ) ;
#8809 = EDGE_CURVE ( 'NONE', #165270, #200563, #95364, .T. ) ;
#8810 = CARTESIAN_POINT ( 'NONE',  ( -21.04386569057603751, 64.25000000001173817, -76.38027013274417243 ) ) ;
#8812 = EDGE_LOOP ( 'NONE', ( #103376, #205042, #31103, #218352 ) ) ;
#8811 = DIRECTION ( 'NONE',  ( 0.000000000000000000, 1.000000000000000000, 0.000000000000000000 ) ) ;
#8813 = ORIENTED_EDGE ( 'NONE', *, *, #145025, .F. ) ;
#8814 = DIRECTION ( 'NONE',  ( 1.000000000000000000, 0.000000000000000000, 0.000000000000000000 ) ) ;
#8815 = ORIENTED_EDGE ( 'NONE', *, *, #3958, .T. ) ;
#8816 = CARTESIAN_POINT ( 'NONE',  ( -21.05000000000000071, 87.39257802171779588, -133.4491579046922709 ) ) ;
#8817 = EDGE_CURVE ( 'NONE', #165054, #170816, #207830, .T. ) ;
#8818 = ORIENTED_EDGE ( 'NONE', *, *, #256549, .T. ) ;
#8819 = CIRCLE ( 'NONE', #162962, 0.09999999999999939493 ) ;
#8820 = DIRECTION ( 'NONE',  ( 0.000000000000000000, 1.000000000000000000, 0.000000000000000000 ) ) ;
#8821 = FACE_OUTER_BOUND ( 'NONE', #119933, .T. ) ;
#8823 = VERTEX_POINT ( 'NONE', #215147 ) ;
#8822 = ORIENTED_EDGE ( 'NONE', *, *, #192687, .T. ) ;
#8824 = ORIENTED_EDGE ( 'NONE', *, *, #9303, .T. ) ;
#8825 = CARTESIAN_POINT ( 'NONE',  ( 21.05933563467872105, 10.72452471209247626, -45.69364774895595360 ) ) ;
#8826 = ORIENTED_EDGE ( 'NONE', *, *, #24379, .T. ) ;
#8827 = VERTEX_POINT ( 'NONE', #116062 ) ;
#8828 = CARTESIAN_POINT ( 'NONE',  ( -16.89081410710458542, 14.16122750184362644, -219.2590969763894293 ) ) ;
#8829 = CARTESIAN_POINT ( 'NONE',  ( -21.05000000000000071, 87.65000000001215597, -139.5231074845243029 ) ) ;
#8831 = VERTEX_POINT ( 'NONE', #18235 ) ;
#8830 = CARTESIAN_POINT ( 'NONE',  ( -20.64999999999999858, 7.128833340094563376, -233.7327013124401276 ) ) ;
#8832 = DIRECTION ( 'NONE',  ( 1.000000000000000000, 0.000000000000000000, 0.000000000000000000 ) ) ;
#8833 = CARTESIAN_POINT ( 'NONE',  ( 22.00411653962159164, 7.253442868381325681, -167.4009618942313580 ) ) ;
#8835 = ORIENTED_EDGE ( 'NONE', *, *, #46738, .T. ) ;
#8834 = CARTESIAN_POINT ( 'NONE',  ( 20.94999999999999929, 1.115600667400684642E-11, -167.5000000000000284 ) ) ;
#8836 = DIRECTION ( 'NONE',  ( 1.000000000000000000, 0.000000000000000000, -0.000000000000000000 ) ) ;
#8837 = ORIENTED_EDGE ( 'NONE', *, *, #142433, .F. ) ;
#8838 = DIRECTION ( 'NONE',  ( 0.000000000000000000, 0.000000000000000000, -1.000000000000000000 ) ) ;
#8839 = ORIENTED_EDGE ( 'NONE', *, *, #76144, .T. ) ;
#8841 = CIRCLE ( 'NONE', #174928, 0.09999999999998898659 ) ;
#8840 = CARTESIAN_POINT ( 'NONE',  ( -21.00219873199062093, 18.70228113215760501, -226.7667091168536047 ) ) ;
#8842 = DIRECTION ( 'NONE',  ( 0.000000000000000000, 0.8814952561688444987, -0.4721928772777320149 ) ) ;
#8843 = AXIS2_PLACEMENT_3D ( 'NONE', #51309, #168777, #73507 ) ;
#8844 = AXIS2_PLACEMENT_3D ( 'NONE', #3523, #139167, #180897 ) ;
#8845 = AXIS2_PLACEMENT_3D ( 'NONE', #100596, #41969, #61518 ) ;
#8846 = ORIENTED_EDGE ( 'NONE', *, *, #156272, .T. ) ;
#8847 = DIRECTION ( 'NONE',  ( 0.000000000000000000, -3.469446951953635015E-14, 1.000000000000000000 ) ) ;
#8848 = DIRECTION ( 'NONE',  ( 0.000000000000000000, 0.2617529984165027912, 0.9651348961777158619 ) ) ;
#8849 = FACE_OUTER_BOUND ( 'NONE', #139835, .T. ) ;
#8850 = DIRECTION ( 'NONE',  ( -0.000000000000000000, 0.9126074666063770380, 0.4088369013363281068 ) ) ;
#8851 = ORIENTED_EDGE ( 'NONE', *, *, #153652, .F. ) ;
#8852 = ORIENTED_EDGE ( 'NONE', *, *, #142713, .F. ) ;
#8853 = DIRECTION ( 'NONE',  ( 0.000000000000000000, -1.000000000000000000, 0.000000000000000000 ) ) ;
#8854 = EDGE_CURVE ( 'NONE', #135145, #112587, #91087, .T. ) ;
#8855 = DIRECTION ( 'NONE',  ( 1.000000000000000000, 0.000000000000000000, 0.000000000000000000 ) ) ;
#8856 = ORIENTED_EDGE ( 'NONE', *, *, #3237, .F. ) ;
#8857 = DIRECTION ( 'NONE',  ( -1.186688945009010077E-16, 1.000000000000000000, 0.000000000000000000 ) ) ;
#8858 = ORIENTED_EDGE ( 'NONE', *, *, #9550, .F. ) ;
#8859 = DIRECTION ( 'NONE',  ( -1.000000000000000000, 0.000000000000000000, -1.020425574104004196E-15 ) ) ;
#8860 = VERTEX_POINT ( 'NONE', #96458 ) ;
#8861 = CARTESIAN_POINT ( 'NONE',  ( -20.94999999999999929, 87.65000000001215597, -139.6231074845242688 ) ) ;
#8862 = CIRCLE ( 'NONE', #208785, 0.5999999999999894307 ) ;
#8863 = DIRECTION ( 'NONE',  ( 0.000000000000000000, 0.000000000000000000, -1.000000000000000000 ) ) ;
#8864 = FACE_OUTER_BOUND ( 'NONE', #77644, .T. ) ;
#8865 = ORIENTED_EDGE ( 'NONE', *, *, #158198, .T. ) ;
#8866 = CARTESIAN_POINT ( 'NONE',  ( -16.79363873026997922, 63.08583527754588260, -213.1316346625713152 ) ) ;
#8867 = ADVANCED_FACE ( 'NONE', ( #176047 ), #132800, .F. ) ;
#8868 = ORIENTED_EDGE ( 'NONE', *, *, #118669, .F. ) ;
#8869 = ORIENTED_EDGE ( 'NONE', *, *, #63940, .F. ) ;
#8870 = VERTEX_POINT ( 'NONE', #138154 ) ;
#8871 = DIRECTION ( 'NONE',  ( -1.000000000000000000, 0.000000000000000000, 0.000000000000000000 ) ) ;
#8872 = FACE_OUTER_BOUND ( 'NONE', #159097, .T. ) ;
#8873 = CARTESIAN_POINT ( 'NONE',  ( -21.07933241753356413, 0.09337959043042155793, -127.6713540516202841 ) ) ;
#8874 = DIRECTION ( 'NONE',  ( 0.000000000000000000, 0.2128009952263630322, -0.9770955615653309501 ) ) ;
#8875 = CARTESIAN_POINT ( 'NONE',  ( -16.86578989773640913, 9.984809801258796469, -20.96466488662223426 ) ) ;
#8876 = AXIS2_PLACEMENT_3D ( 'NONE', #37847, #213888, #135622 ) ;
#8878 = DIRECTION ( 'NONE',  ( -0.000000000000000000, 0.000000000000000000, 1.000000000000000000 ) ) ;
#8877 = CARTESIAN_POINT ( 'NONE',  ( 19.97071067811864609, 62.37141908057012074, -208.9966201521278037 ) ) ;
#8880 = ORIENTED_EDGE ( 'NONE', *, *, #155449, .F. ) ;
#8879 = CARTESIAN_POINT ( 'NONE',  ( -20.54999999999999716, 4.350000000011156054, -54.75000000000000000 ) ) ;
#8881 = CARTESIAN_POINT ( 'NONE',  ( -21.05000000000000071, 77.83534155023646406, -124.9679561919613064 ) ) ;
#8882 = ORIENTED_EDGE ( 'NONE', *, *, #33405, .T. ) ;
#8883 = DIRECTION ( 'NONE',  ( 1.000000000000000000, 0.000000000000000000, 0.000000000000000000 ) ) ;
#8884 = ORIENTED_EDGE ( 'NONE', *, *, #128338, .T. ) ;
#8885 = ORIENTED_EDGE ( 'NONE', *, *, #197393, .T. ) ;
#8886 = DIRECTION ( 'NONE',  ( -1.000000000000000000, 2.952720810173289112E-16, 2.061873921506763405E-30 ) ) ;
#8887 = AXIS2_PLACEMENT_3D ( 'NONE', #189514, #173846, #74735 ) ;
#8888 = DIRECTION ( 'NONE',  ( 0.000000000000000000, 0.000000000000000000, -1.000000000000000000 ) ) ;
#8889 = DIRECTION ( 'NONE',  ( -1.000000000000000000, 0.000000000000000000, 0.000000000000000000 ) ) ;
#8890 = FACE_OUTER_BOUND ( 'NONE', #105921, .T. ) ;
#8891 = VECTOR ( 'NONE', #99785, 1000.000000000000000 ) ;
#8892 = CIRCLE ( 'NONE', #37954, 7.800000000000001599 ) ;
#8893 = ORIENTED_EDGE ( 'NONE', *, *, #15033, .T. ) ;
#8894 = ORIENTED_EDGE ( 'NONE', *, *, #170157, .T. ) ;
#8895 = AXIS2_PLACEMENT_3D ( 'NONE', #156485, #57321, #136878 ) ;
#8896 = DIRECTION ( 'NONE',  ( 0.000000000000000000, -0.9908441862701605762, -0.1350103645451835310 ) ) ;
#8897 = ORIENTED_EDGE ( 'NONE', *, *, #94348, .T. ) ;
#8898 = DIRECTION ( 'NONE',  ( 1.000000000000000000, 0.000000000000000000, 0.000000000000000000 ) ) ;
#8899 = CARTESIAN_POINT ( 'NONE',  ( -16.81744102076748959, 63.08573235307424198, -213.1276215869287967 ) ) ;
#8900 = VERTEX_POINT ( 'NONE', #159054 ) ;
#8901 = PLANE ( 'NONE',  #128007 ) ;
#8902 = DIRECTION ( 'NONE',  ( 0.000000000000000000, 0.000000000000000000, -1.000000000000000000 ) ) ;
#8903 = DIRECTION ( 'NONE',  ( 0.000000000000000000, 0.000000000000000000, 1.000000000000000000 ) ) ;
#8904 = DIRECTION ( 'NONE',  ( 0.000000000000000000, 0.000000000000000000, 1.000000000000000000 ) ) ;
#8905 = ORIENTED_EDGE ( 'NONE', *, *, #137376, .T. ) ;
#8906 = CARTESIAN_POINT ( 'NONE',  ( -16.27683809663751191, 9.350000000011133849, -109.7500000000000000 ) ) ;
#8908 = CARTESIAN_POINT ( 'NONE',  ( -21.05000000000000071, 11.65000000001115232, -140.7838656629781724 ) ) ;
#8907 = CIRCLE ( 'NONE', #163047, 0.1000000000000124678 ) ;
#8909 = CYLINDRICAL_SURFACE ( 'NONE', #254099, 0.09999999999999939493 ) ;
#8910 = CARTESIAN_POINT ( 'NONE',  ( -22.94999999999999929, 0.000000000000000000, -4.000000000000000000 ) ) ;
#8911 = DIRECTION ( 'NONE',  ( 1.000000000000000000, 0.000000000000000000, 0.000000000000000000 ) ) ;
#8912 = EDGE_CURVE ( 'NONE', #210276, #172249, #162026, .T. ) ;
#8913 = CARTESIAN_POINT ( 'NONE',  ( 18.41416235934317314, 77.13860723519889007, -241.8264964602988982 ) ) ;
#8914 = CIRCLE ( 'NONE', #175519, 0.5000000000000084377 ) ;
#8915 = ORIENTED_EDGE ( 'NONE', *, *, #88006, .F. ) ;
#8916 = AXIS2_PLACEMENT_3D ( 'NONE', #208122, #183733, #110271 ) ;
#8917 = ADVANCED_FACE ( 'NONE', ( #101580 ), #249505, .F. ) ;
#8918 = FACE_OUTER_BOUND ( 'NONE', #3345, .T. ) ;
#8919 = ORIENTED_EDGE ( 'NONE', *, *, #49941, .F. ) ;
#8920 = AXIS2_PLACEMENT_3D ( 'NONE', #232601, #90481, #248284 ) ;
#8921 = DIRECTION ( 'NONE',  ( 2.715809747126116508E-16, -1.000000000000000000, 0.000000000000000000 ) ) ;
#8922 = ADVANCED_FACE ( 'NONE', ( #62502 ), #203700, .T. ) ;
#8923 = PLANE ( 'NONE',  #39786 ) ;
#8924 = CARTESIAN_POINT ( 'NONE',  ( 21.13461538461538325, 61.86212273321938682, -221.7064394764304609 ) ) ;
#8925 = DIRECTION ( 'NONE',  ( 0.000000000000000000, 0.9993789003877945332, 0.03523937371297191506 ) ) ;
#8926 = ORIENTED_EDGE ( 'NONE', *, *, #241033, .T. ) ;
#8927 = FACE_OUTER_BOUND ( 'NONE', #1283, .T. ) ;
#8928 = DIRECTION ( 'NONE',  ( 0.000000000000000000, -0.4088369013363205573, 0.9126074666063803686 ) ) ;
#8929 = LINE ( 'NONE', #111892, #59102 ) ;
#8930 = EDGE_CURVE ( 'NONE', #1827, #118580, #216151, .T. ) ;
#8931 = AXIS2_PLACEMENT_3D ( 'NONE', #95889, #178029, #137576 ) ;
#8932 = VECTOR ( 'NONE', #225502, 1000.000000000000000 ) ;
#8933 = AXIS2_PLACEMENT_3D ( 'NONE', #215153, #78196, #33993 ) ;
#8934 = DIRECTION ( 'NONE',  ( -1.000000000000000000, -0.000000000000000000, -0.000000000000000000 ) ) ;
#8935 = EDGE_LOOP ( 'NONE', ( #88604, #159533, #142555, #252267 ) ) ;
#8936 = ORIENTED_EDGE ( 'NONE', *, *, #227286, .F. ) ;
#8937 = CARTESIAN_POINT ( 'NONE',  ( 20.94999999999999574, 63.65372963998873246, -224.5957079722776655 ) ) ;
#8938 = DIRECTION ( 'NONE',  ( -0.000000000000000000, 0.9770955615653316162, 0.2128009952263604232 ) ) ;
#8939 = LINE ( 'NONE', #164169, #155031 ) ;
#8940 = DIRECTION ( 'NONE',  ( 1.000000000000000000, 0.000000000000000000, -0.000000000000000000 ) ) ;
#8941 = CARTESIAN_POINT ( 'NONE',  ( -2.995603634470829482E-16, 11.01970663298110154, -220.3481540650095098 ) ) ;
#8942 = ADVANCED_FACE ( 'NONE', ( #61208 ), #41667, .F. ) ;
#8943 = ORIENTED_EDGE ( 'NONE', *, *, #83176, .T. ) ;
#8944 = CARTESIAN_POINT ( 'NONE',  ( 22.57320508075688892, 11.75000000001115552, -33.50000000000000000 ) ) ;
#8945 = ITEM_DEFINED_TRANSFORMATION ( 'NONE', 'NONE', #215183,  #2425 ) ;
#8946 = DIRECTION ( 'NONE',  ( -0.000000000000000000, -6.982962677686266711E-15, 1.000000000000000000 ) ) ;
#8947 = ORIENTED_EDGE ( 'NONE', *, *, #224270, .T. ) ;
#8948 = CARTESIAN_POINT ( 'NONE',  ( -18.59999999999999787, 68.22930980752001062, -227.7331931781284879 ) ) ;
#8949 = ORIENTED_EDGE ( 'NONE', *, *, #84400, .T. ) ;
#8950 = ORIENTED_EDGE ( 'NONE', *, *, #24372, .F. ) ;
#8951 = ORIENTED_EDGE ( 'NONE', *, *, #106969, .T. ) ;
#8952 = DIRECTION ( 'NONE',  ( 0.000000000000000000, 0.8814952561688476074, -0.4721928772777262417 ) ) ;
#8953 = DIRECTION ( 'NONE',  ( 0.000000000000000000, -5.204170427930272346E-14, -1.000000000000000000 ) ) ;
#8954 = CARTESIAN_POINT ( 'NONE',  ( 18.59999999999999787, -1.362429037193307435, -41.38888124792119783 ) ) ;
#8955 = AXIS2_PLACEMENT_3D ( 'NONE', #224922, #205360, #166289 ) ;
#8956 = ADVANCED_FACE ( 'NONE', ( #3804 ), #205852, .T. ) ;
#8957 = CARTESIAN_POINT ( 'NONE',  ( 18.45139536634707156, -9.486081720270041373, -140.6405116178106880 ) ) ;
#8958 = DIRECTION ( 'NONE',  ( 0.000000000000000000, 0.000000000000000000, -1.000000000000000000 ) ) ;
#8959 = CARTESIAN_POINT ( 'NONE',  ( -21.05000000000000071, -10.51247937907010233, -206.3598299697285654 ) ) ;
#8960 = CARTESIAN_POINT ( 'NONE',  ( -23.15000000000000213, 15.92646454033039660, -219.3818586450342707 ) ) ;
#8962 = LINE ( 'NONE', #152356, #78719 ) ;
#8961 = CARTESIAN_POINT ( 'NONE',  ( 20.95462737510932882, 65.44321804836815204, -95.45315742796208269 ) ) ;
#8963 = FACE_OUTER_BOUND ( 'NONE', #231454, .T. ) ;
#8964 = LINE ( 'NONE', #185030, #72973 ) ;
#8965 = CARTESIAN_POINT ( 'NONE',  ( 21.05000000000000071, 88.41227409416143246, -72.52310748452423184 ) ) ;
#8966 = CARTESIAN_POINT ( 'NONE',  ( 20.95017935633852346, 18.75476199923615894, -228.0766203067306321 ) ) ;
#8967 = ORIENTED_EDGE ( 'NONE', *, *, #50616, .F. ) ;
#8968 = ORIENTED_EDGE ( 'NONE', *, *, #146894, .T. ) ;
#8969 = CARTESIAN_POINT ( 'NONE',  ( -20.64999999999999858, 7.249999999999999112, -21.15000000000000213 ) ) ;
#8970 = DIRECTION ( 'NONE',  ( 0.000000000000000000, -0.000000000000000000, -1.000000000000000000 ) ) ;
#8972 = CARTESIAN_POINT ( 'NONE',  ( -14.87770893841226894, 13.10213769539062234, -216.8429874065679428 ) ) ;
#8971 = CARTESIAN_POINT ( 'NONE',  ( 21.05000000000005400, 67.65000000001118963, -25.06452884076209742 ) ) ;
#8973 = EDGE_CURVE ( 'NONE', #49158, #207350, #128691, .T. ) ;
#8974 = CARTESIAN_POINT ( 'NONE',  ( -20.00857864376270001, 52.21971469324220294, -232.5539039185337913 ) ) ;
#8975 = DIRECTION ( 'NONE',  ( 1.000000000000000000, 0.000000000000000000, 0.000000000000000000 ) ) ;
#8976 = FACE_OUTER_BOUND ( 'NONE', #249700, .T. ) ;
#8977 = VERTEX_POINT ( 'NONE', #200723 ) ;
#8978 = EDGE_CURVE ( 'NONE', #240371, #70373, #1209, .T. ) ;
#8979 = ORIENTED_EDGE ( 'NONE', *, *, #57919, .F. ) ;
#8980 = DIRECTION ( 'NONE',  ( -1.000000000000000000, 0.000000000000000000, 0.000000000000000000 ) ) ;
#8981 = VERTEX_POINT ( 'NONE', #160338 ) ;
#8982 = ADVANCED_FACE ( 'NONE', ( #244976 ), #104166, .T. ) ;
#8983 = CARTESIAN_POINT ( 'NONE',  ( 18.49999999999998934, 16.64998792410002793, -222.7039835543563981 ) ) ;
#8984 = AXIS2_PLACEMENT_3D ( 'NONE', #11144, #138437, #90662 ) ;
#8985 = CIRCLE ( 'NONE', #150633, 4.149999999999999467 ) ;
#8986 = CARTESIAN_POINT ( 'NONE',  ( 21.05000000000000071, -11.74999999998883560, -130.9000000000000341 ) ) ;
#8987 = CIRCLE ( 'NONE', #13103, 0.09999999999999939493 ) ;
#8988 = ORIENTED_EDGE ( 'NONE', *, *, #141241, .T. ) ;
#8989 = DIRECTION ( 'NONE',  ( 0.000000000000000000, -0.9126074666063770380, -0.4088369013363281068 ) ) ;
#8991 = EDGE_CURVE ( 'NONE', #155744, #13290, #45289, .T. ) ;
#8990 =( BOUNDED_SURFACE ( )  B_SPLINE_SURFACE ( 3, 2, ( 
 ( #51878, #11510, #153624 ),
 ( #252654, #36213, #171889 ),
 ( #133999, #213530, #71492 ),
 ( #114445, #253937, #234378 ) ),
 .UNSPECIFIED., .F., .F., .F. ) 
 B_SPLINE_SURFACE_WITH_KNOTS ( ( 4, 4 ),
 ( 3, 3 ),
 ( 0.04058434257139476725, 0.04256401539001602313 ),
 ( 0.000000000000000000, 1.000000000000000000 ),
 .UNSPECIFIED. ) 
 GEOMETRIC_REPRESENTATION_ITEM ( )  RATIONAL_B_SPLINE_SURFACE ( (
 ( 1.000000000000000000, 0.7103081912008347709, 1.000000000000000000),
 ( 1.000000000000000000, 0.7104998333557990264, 1.000000000000000000),
 ( 1.000000000000000000, 0.7107238315752896218, 1.000000000000000000),
 ( 1.000000000000000000, 0.7110073749539418397, 1.000000000000000000) ) ) 
 REPRESENTATION_ITEM ( '' )  SURFACE ( )  );
#8992 = ORIENTED_EDGE ( 'NONE', *, *, #86129, .T. ) ;
#8993 = CARTESIAN_POINT ( 'NONE',  ( -16.89268316805465986, 51.62340874627276577, -231.9425458505251072 ) ) ;
#8994 = CARTESIAN_POINT ( 'NONE',  ( 20.84999999999998721, 64.25000000001215028, -136.5231074845244166 ) ) ;
#8995 = FACE_OUTER_BOUND ( 'NONE', #238193, .T. ) ;
#8996 = EDGE_CURVE ( 'NONE', #207164, #190222, #245224, .T. ) ;
#8997 = DIRECTION ( 'NONE',  ( -1.000000000000000000, -2.952720810173289112E-16, 0.000000000000000000 ) ) ;
#8998 = EDGE_CURVE ( 'NONE', #195562, #121203, #16278, .T. ) ;
#8999 = CARTESIAN_POINT ( 'NONE',  ( -23.15000000000000213, 11.60000000001115517, -194.0717967697244717 ) ) ;
#9000 = CARTESIAN_POINT ( 'NONE',  ( 23.14999999999998437, 32.96286418198891255, -251.2069521516576174 ) ) ;
#9001 = AXIS2_PLACEMENT_3D ( 'NONE', #207166, #123773, #168075 ) ;
#9002 = DIRECTION ( 'NONE',  ( 0.000000000000000000, 0.000000000000000000, -1.000000000000000000 ) ) ;
#9003 = DIRECTION ( 'NONE',  ( -1.000000000000000000, -0.000000000000000000, -0.000000000000000000 ) ) ;
#9005 = ORIENTED_EDGE ( 'NONE', *, *, #60988, .T. ) ;
#9004 = DIRECTION ( 'NONE',  ( 0.000000000000000000, 0.008583690987128059571, -0.9999631594459056361 ) ) ;
#9007 = CYLINDRICAL_SURFACE ( 'NONE', #205954, 0.09999999999999543976 ) ;
#9006 = DIRECTION ( 'NONE',  ( 0.000000000000000000, -0.2617529984164955192, -0.9651348961777178603 ) ) ;
#9008 = VERTEX_POINT ( 'NONE', #84569 ) ;
#9010 = ORIENTED_EDGE ( 'NONE', *, *, #171322, .T. ) ;
#9009 = CARTESIAN_POINT ( 'NONE',  ( -20.94999999999999929, 64.25000000001210765, -129.5083017138703667 ) ) ;
#9011 = EDGE_LOOP ( 'NONE', ( #780, #32479, #208048, #236192 ) ) ;
#9012 = DIRECTION ( 'NONE',  ( 1.000000000000000000, 0.000000000000000000, 0.000000000000000000 ) ) ;
#9013 = DIRECTION ( 'NONE',  ( 0.000000000000000000, 1.000000000000000000, 6.982962677686266711E-15 ) ) ;
#9014 = EDGE_CURVE ( 'NONE', #66665, #239952, #6357, .T. ) ;
#9015 = CYLINDRICAL_SURFACE ( 'NONE', #167160, 12.87499999999999822 ) ;
#9016 = CARTESIAN_POINT ( 'NONE',  ( -21.55000000000000426, 68.29142135624935861, -124.1731074845243512 ) ) ;
#9017 = CARTESIAN_POINT ( 'NONE',  ( -20.85000000000000497, 11.75000000001115019, -93.58085275404135928 ) ) ;
#9018 = ADVANCED_FACE ( 'NONE', ( #182457 ), #162905, .F. ) ;
#9019 = EDGE_CURVE ( 'NONE', #138276, #142373, #199441, .T. ) ;
#9020 = CARTESIAN_POINT ( 'NONE',  ( -20.54999999999999716, 76.00000000001195133, -103.0231074845243171 ) ) ;
#9021 = DIRECTION ( 'NONE',  ( 3.469446951953635015E-14, 6.982962677686266711E-15, -1.000000000000000000 ) ) ;
#9022 = CARTESIAN_POINT ( 'NONE',  ( 20.94999999999999929, 11.16079915604378492, -211.0041093385139561 ) ) ;
#9023 = CIRCLE ( 'NONE', #83982, 0.09999999999999939493 ) ;
#9025 = AXIS2_PLACEMENT_3D ( 'NONE', #19185, #139091, #115721 ) ;
#9024 = DIRECTION ( 'NONE',  ( 0.000000000000000000, 0.9126074666063772600, 0.4088369013363274407 ) ) ;
#9026 = VERTEX_POINT ( 'NONE', #183732 ) ;
#9027 = ORIENTED_EDGE ( 'NONE', *, *, #91163, .F. ) ;
#9028 = CARTESIAN_POINT ( 'NONE',  ( -16.94333152886235894, 9.990342011461637028, -180.1079684689455576 ) ) ;
#9029 = VERTEX_POINT ( 'NONE', #5052 ) ;
#9030 = CARTESIAN_POINT ( 'NONE',  ( -20.54999999999999716, 76.00000000001259082, -190.5481074845243654 ) ) ;
#9031 = ORIENTED_EDGE ( 'NONE', *, *, #224221, .F. ) ;
#9032 = DIRECTION ( 'NONE',  ( 1.000000000000000000, 0.000000000000000000, 0.000000000000000000 ) ) ;
#9033 = EDGE_CURVE ( 'NONE', #63695, #99579, #164170, .T. ) ;
#9034 = CARTESIAN_POINT ( 'NONE',  ( 20.04142135623731136, 11.75000000000000711, -24.65000000000000213 ) ) ;
#9035 = CARTESIAN_POINT ( 'NONE',  ( -21.05000000000000071, 87.39257802171711376, -39.09705706435617856 ) ) ;
#9036 = ADVANCED_FACE ( 'NONE', ( #65056 ), #228665, .F. ) ;
#9037 = DIRECTION ( 'NONE',  ( 0.000000000000000000, 0.000000000000000000, -1.000000000000000000 ) ) ;
#9038 = CARTESIAN_POINT ( 'NONE',  ( 18.59999999999997655, 7.128833340094563376, -233.7327013124401276 ) ) ;
#9039 = ORIENTED_EDGE ( 'NONE', *, *, #252839, .T. ) ;
#9040 = AXIS2_PLACEMENT_3D ( 'NONE', #160031, #242098, #201694 ) ;
#9041 = ADVANCED_FACE ( 'NONE', ( #131447 ), #29822, .F. ) ;
#9042 = DIRECTION ( 'NONE',  ( 0.000000000000000000, 0.000000000000000000, -1.000000000000000000 ) ) ;
#9043 = CARTESIAN_POINT ( 'NONE',  ( 18.52165635395192211, 85.48115071129370790, -62.49826990166167207 ) ) ;
#9044 = DIRECTION ( 'NONE',  ( 0.000000000000000000, -0.7397360091702802620, 0.6728971962616779878 ) ) ;
#9045 = EDGE_LOOP ( 'NONE', ( #137340, #63394, #88915, #65293, #46744, #5458, #156315, #196128, #118082, #17668 ) ) ;
#9047 = DIRECTION ( 'NONE',  ( 0.000000000000000000, 6.982962677686266711E-15, -1.000000000000000000 ) ) ;
#9046 = DIRECTION ( 'NONE',  ( -1.836970198721029441E-16, 0.4721928772777346239, 0.8814952561688430555 ) ) ;
#9048 = ORIENTED_EDGE ( 'NONE', *, *, #60855, .T. ) ;
#9051 = ORIENTED_EDGE ( 'NONE', *, *, #119754, .T. ) ;
#9050 = DIRECTION ( 'NONE',  ( -0.7071067811865388020, -0.6233112732207694018, 0.3338907855510774847 ) ) ;
#9049 = CARTESIAN_POINT ( 'NONE',  ( -21.05000000000000071, 19.65328051035826817, -225.4506993556300074 ) ) ;
#9052 = ORIENTED_EDGE ( 'NONE', *, *, #74313, .T. ) ;
#9053 = FACE_OUTER_BOUND ( 'NONE', #183730, .T. ) ;
#9054 = DIRECTION ( 'NONE',  ( 1.000000000000000000, -0.000000000000000000, 0.000000000000000000 ) ) ;
#9055 = CARTESIAN_POINT ( 'NONE',  ( -23.15000000000000213, 2.500000000011156409, -113.7246219227621395 ) ) ;
#9056 = EDGE_LOOP ( 'NONE', ( #161483, #191140, #135960, #227489, #70748 ) ) ;
#9057 = DIRECTION ( 'NONE',  ( -1.000000000000000000, -0.000000000000000000, -0.000000000000000000 ) ) ;
#9058 = AXIS2_PLACEMENT_3D ( 'NONE', #124611, #201562, #162464 ) ;
#9059 = DIRECTION ( 'NONE',  ( 1.000000000000000000, 0.000000000000000000, 0.000000000000000000 ) ) ;
#9061 = DIRECTION ( 'NONE',  ( 1.000000000000000000, -0.000000000000000000, -0.000000000000000000 ) ) ;
#9060 = CARTESIAN_POINT ( 'NONE',  ( -23.15000000000000213, 4.250000000011156409, -146.2500000000000284 ) ) ;
#9063 = ORIENTED_EDGE ( 'NONE', *, *, #136347, .T. ) ;
#9062 = CARTESIAN_POINT ( 'NONE',  ( 21.05000000000000071, 11.60000000001116049, -93.57179676972454274 ) ) ;
#9064 = AXIS2_PLACEMENT_3D ( 'NONE', #204822, #167034, #48329 ) ;
#9065 = EDGE_CURVE ( 'NONE', #144497, #238714, #185645, .T. ) ;
#9066 = EDGE_LOOP ( 'NONE', ( #53795, #98468, #10820, #242292 ) ) ;
#9067 = CIRCLE ( 'NONE', #238188, 2.100000000000004530 ) ;
#9068 = EDGE_CURVE ( 'NONE', #123180, #143626, #83030, .T. ) ;
#9069 = PLANE ( 'NONE',  #111726 ) ;
#9070 = CARTESIAN_POINT ( 'NONE',  ( -20.94999999999999929, 87.48912529308779540, -72.62310748452422615 ) ) ;
#9071 = DIRECTION ( 'NONE',  ( 0.000000000000000000, 0.000000000000000000, -1.000000000000000000 ) ) ;
#9073 = EDGE_LOOP ( 'NONE', ( #187388, #75847, #24826, #154724, #207541, #171355 ) ) ;
#9072 = AXIS2_PLACEMENT_3D ( 'NONE', #86178, #187893, #225682 ) ;
#9074 = CARTESIAN_POINT ( 'NONE',  ( -16.85939681242906119, 9.905225185936460619, -188.0399219551914598 ) ) ;
#9075 = CIRCLE ( 'NONE', #129856, 0.2000000000000057288 ) ;
#9076 = EDGE_CURVE ( 'NONE', #74863, #7145, #79854, .T. ) ;
#9077 = DIRECTION ( 'NONE',  ( 3.265361837132813093E-16, -1.000000000000000000, -0.000000000000000000 ) ) ;
#9078 = CARTESIAN_POINT ( 'NONE',  ( 18.59999999999996945, 68.97833521811179480, -99.18954208262705663 ) ) ;
#9079 = ORIENTED_EDGE ( 'NONE', *, *, #3038, .T. ) ;
#9080 = DIRECTION ( 'NONE',  ( 0.000000000000000000, -1.000000000000000000, -7.272083257015735086E-15 ) ) ;
#9081 = ADVANCED_FACE ( 'NONE', ( #169338 ), #199820, .F. ) ;
#9082 = CIRCLE ( 'NONE', #242301, 0.6000000000000033085 ) ;
#9083 = AXIS2_PLACEMENT_3D ( 'NONE', #138737, #198747, #140040 ) ;
#9084 = EDGE_CURVE ( 'NONE', #124831, #48342, #28963, .T. ) ;
#9085 = ORIENTED_EDGE ( 'NONE', *, *, #33521, .T. ) ;
#9086 = AXIS2_PLACEMENT_3D ( 'NONE', #102636, #222588, #124808 ) ;
#9087 = DIRECTION ( 'NONE',  ( 1.000000000000000000, 0.000000000000000000, 0.000000000000000000 ) ) ;
#9088 = FACE_OUTER_BOUND ( 'NONE', #175262, .T. ) ;
#9089 = AXIS2_PLACEMENT_3D ( 'NONE', #212083, #30897, #191247 ) ;
#9090 = EDGE_CURVE ( 'NONE', #47325, #144142, #33064, .T. ) ;
#9091 = VERTEX_POINT ( 'NONE', #128895 ) ;
#9092 = EDGE_LOOP ( 'NONE', ( #197591, #215666, #188118, #202048 ) ) ;
#9094 = EDGE_CURVE ( 'NONE', #71933, #19158, #178793, .T. ) ;
#9093 = EDGE_CURVE ( 'NONE', #215045, #71039, #91458, .T. ) ;
#9096 =( BOUNDED_SURFACE ( )  B_SPLINE_SURFACE ( 3, 2, ( 
 ( #255834, #94234, #231206 ),
 ( #192079, #175117, #34301 ),
 ( #134628, #77231, #236316 ),
 ( #137217, #212911, #216749 ) ),
 .UNSPECIFIED., .F., .F., .T. ) 
 B_SPLINE_SURFACE_WITH_KNOTS ( ( 4, 4 ),
 ( 3, 3 ),
 ( 0.0008258556059633759532, 0.0009616864997632855591 ),
 ( 0.000000000000000000, 1.000000000000000000 ),
 .UNSPECIFIED. ) 
 GEOMETRIC_REPRESENTATION_ITEM ( )  RATIONAL_B_SPLINE_SURFACE ( (
 ( 1.000000000000000000, 0.9152888060719445162, 1.000000000000000000),
 ( 1.000000000000000000, 0.9327727094138025254, 1.000000000000000000),
 ( 1.000000000000000000, 0.9369023509258468385, 1.000000000000000000),
 ( 1.000000000000000000, 0.9246339933864583527, 1.000000000000000000) ) ) 
 REPRESENTATION_ITEM ( '' )  SURFACE ( )  );
#9095 = AXIS2_PLACEMENT_3D ( 'NONE', #115723, #195286, #58290 ) ;
#9097 = CARTESIAN_POINT ( 'NONE',  ( -18.59999999999999787, 64.35000000001180354, -81.67310748452439384 ) ) ;
#9098 = ORIENTED_EDGE ( 'NONE', *, *, #180528, .T. ) ;
#9100 = ORIENTED_EDGE ( 'NONE', *, *, #202724, .T. ) ;
#9099 = FACE_OUTER_BOUND ( 'NONE', #191861, .T. ) ;
#9101 = EDGE_CURVE ( 'NONE', #89222, #247713, #110599, .T. ) ;
#9102 = AXIS2_PLACEMENT_3D ( 'NONE', #36327, #195406, #207587 ) ;
#9103 = ORIENTED_EDGE ( 'NONE', *, *, #114700, .T. ) ;
#9105 = VERTEX_POINT ( 'NONE', #210995 ) ;
#9104 = ORIENTED_EDGE ( 'NONE', *, *, #202759, .F. ) ;
#9106 = CARTESIAN_POINT ( 'NONE',  ( -18.54260524012581612, -9.624219390062492607, -107.2407730457710073 ) ) ;
#9107 = ORIENTED_EDGE ( 'NONE', *, *, #206594, .T. ) ;
#9108 = DIRECTION ( 'NONE',  ( 1.000000000000000000, 0.000000000000000000, 0.000000000000000000 ) ) ;
#9109 = LINE ( 'NONE', #247715, #165948 ) ;
#9110 = EDGE_CURVE ( 'NONE', #134210, #163256, #241308, .T. ) ;
#9111 = EDGE_CURVE ( 'NONE', #13670, #12655, #20553, .T. ) ;
#9112 = AXIS2_PLACEMENT_3D ( 'NONE', #221239, #23086, #142976 ) ;
#9113 = LINE ( 'NONE', #112073, #255473 ) ;
#9114 = AXIS2_PLACEMENT_3D ( 'NONE', #146854, #110316, #247248 ) ;
#9116 = CARTESIAN_POINT ( 'NONE',  ( -18.50000000000000000, 86.87366311306884370, -199.3414869250131858 ) ) ;
#9115 = AXIS2_PLACEMENT_3D ( 'NONE', #190426, #93864, #13072 ) ;
#9117 = EDGE_LOOP ( 'NONE', ( #16086, #23583, #36112, #191588 ) ) ;
#9118 = VERTEX_POINT ( 'NONE', #127606 ) ;
#9119 = ADVANCED_FACE ( 'NONE', ( #88441 ), #236973, .F. ) ;
#9120 = DIRECTION ( 'NONE',  ( -1.000000000000000000, 0.000000000000000000, 0.000000000000000000 ) ) ;
#9122 = ORIENTED_EDGE ( 'NONE', *, *, #132131, .T. ) ;
#9121 = DIRECTION ( 'NONE',  ( -1.000000000000000000, -1.394253735153569469E-16, -2.602809386958778209E-16 ) ) ;
#9123 = LINE ( 'NONE', #241322, #88309 ) ;
#9125 = ORIENTED_EDGE ( 'NONE', *, *, #207561, .F. ) ;
#9124 = DIRECTION ( 'NONE',  ( -1.000000000000000000, -0.000000000000000000, -0.000000000000000000 ) ) ;
#9126 = ORIENTED_EDGE ( 'NONE', *, *, #57040, .F. ) ;
#9127 = ADVANCED_FACE ( 'NONE', ( #36226 ), #173200, .T. ) ;
#9128 = DIRECTION ( 'NONE',  ( -0.7070776581709311559, -0.1504792239192758452, 0.6909393522474779337 ) ) ;
#9129 = EDGE_CURVE ( 'NONE', #206263, #171099, #217385, .T. ) ;
#9130 = VERTEX_POINT ( 'NONE', #76605 ) ;
#9131 = CARTESIAN_POINT ( 'NONE',  ( -16.77431908686106254, 9.945805754529134290, -180.1641607823497395 ) ) ;
#9132 = LINE ( 'NONE', #202195, #123687 ) ;
#9133 = AXIS2_PLACEMENT_3D ( 'NONE', #143556, #100547, #43186 ) ;
#9135 = EDGE_LOOP ( 'NONE', ( #193769, #94768, #110377, #143501 ) ) ;
#9134 = ORIENTED_EDGE ( 'NONE', *, *, #153128, .F. ) ;
#9136 = ORIENTED_EDGE ( 'NONE', *, *, #207117, .F. ) ;
#9137 = CARTESIAN_POINT ( 'NONE',  ( -16.97048361161167662, 9.950000000011138823, -53.85888434443041461 ) ) ;
#9138 = ORIENTED_EDGE ( 'NONE', *, *, #207473, .F. ) ;
#9139 = EDGE_LOOP ( 'NONE', ( #207304, #218850, #222035, #211932 ) ) ;
#9140 = LINE ( 'NONE', #168256, #125943 ) ;
#9142 = ORIENTED_EDGE ( 'NONE', *, *, #172806, .F. ) ;
#9141 = CARTESIAN_POINT ( 'NONE',  ( -18.50000000000000000, 14.81796439977981272, -236.5325475414793743 ) ) ;
#9143 = EDGE_CURVE ( 'NONE', #232431, #170879, #78767, .T. ) ;
#9144 = DIRECTION ( 'NONE',  ( 0.000000000000000000, -1.000000000000000000, -2.891205793294679805E-16 ) ) ;
#9146 = DIRECTION ( 'NONE',  ( -1.000000000000000000, 0.000000000000000000, 0.000000000000000000 ) ) ;
#9145 = DIRECTION ( 'NONE',  ( 1.000000000000000000, 0.000000000000000000, 0.000000000000000000 ) ) ;
#9147 = CARTESIAN_POINT ( 'NONE',  ( -18.59999999999999787, 64.35000000001180354, -81.77310748452438816 ) ) ;
#9148 = CARTESIAN_POINT ( 'NONE',  ( -18.34374000495059676, 11.47316190337362940, -191.7499999999999716 ) ) ;
#9149 = VERTEX_POINT ( 'NONE', #14089 ) ;
#9150 = ORIENTED_EDGE ( 'NONE', *, *, #97280, .F. ) ;
#9151 = EDGE_CURVE ( 'NONE', #160216, #86831, #252666, .T. ) ;
#9152 = CARTESIAN_POINT ( 'NONE',  ( 18.49999999999999289, 69.55000000001159322, -59.50608031408435039 ) ) ;
#9153 = DIRECTION ( 'NONE',  ( 1.000000000000000000, -0.000000000000000000, -0.000000000000000000 ) ) ;
#9154 = ORIENTED_EDGE ( 'NONE', *, *, #53244, .F. ) ;
#9155 = CARTESIAN_POINT ( 'NONE',  ( -20.94999999999999929, 7.031312794766356511, -70.60915093822731592 ) ) ;
#9156 = ORIENTED_EDGE ( 'NONE', *, *, #78223, .F. ) ;
#9157 = ORIENTED_EDGE ( 'NONE', *, *, #174249, .T. ) ;
#9158 = DIRECTION ( 'NONE',  ( 1.000000000000000000, -0.000000000000000000, -0.000000000000000000 ) ) ;
#9159 = EDGE_CURVE ( 'NONE', #38036, #26254, #117023, .T. ) ;
#9160 = CARTESIAN_POINT ( 'NONE',  ( -18.35235881385853318, 64.52658099229918776, -127.2731074845243882 ) ) ;
#9161 = EDGE_LOOP ( 'NONE', ( #63328, #161217, #196096, #47365 ) ) ;
#9162 = CARTESIAN_POINT ( 'NONE',  ( -21.03922262424672596, 11.62390063401586637, -107.3592080428934850 ) ) ;
#9163 = FACE_OUTER_BOUND ( 'NONE', #97026, .T. ) ;
#9164 = VERTEX_POINT ( 'NONE', #154898 ) ;
#9165 = CARTESIAN_POINT ( 'NONE',  ( -5.999999999999938716, 64.75000000001119815, -25.92310748452479174 ) ) ;
#9166 = DIRECTION ( 'NONE',  ( 0.000000000000000000, 0.000000000000000000, 1.000000000000000000 ) ) ;
#9168 = CARTESIAN_POINT ( 'NONE',  ( 20.94999999999999929, 1.115600667400684642E-11, -167.5000000000000284 ) ) ;
#9167 = CARTESIAN_POINT ( 'NONE',  ( 18.39999999999999503, 5.650000000011139001, -188.3499999999999659 ) ) ;
#9169 = DIRECTION ( 'NONE',  ( 0.000000000000000000, 0.000000000000000000, 1.000000000000000000 ) ) ;
#9170 = CARTESIAN_POINT ( 'NONE',  ( -23.15000000000000213, 4.350000000011156054, -188.7499999999999716 ) ) ;
#9171 = CARTESIAN_POINT ( 'NONE',  ( 18.49505832270840600, -9.438028062771744331, -174.6984731748938486 ) ) ;
#9172 = DIRECTION ( 'NONE',  ( 6.938893903907222067E-15, 0.9651348961777157509, -0.2617529984165031243 ) ) ;
#9173 = AXIS2_PLACEMENT_3D ( 'NONE', #14393, #93893, #54761 ) ;
#9174 = ORIENTED_EDGE ( 'NONE', *, *, #111877, .T. ) ;
#9175 = EDGE_CURVE ( 'NONE', #241842, #198298, #95548, .T. ) ;
#9177 = ORIENTED_EDGE ( 'NONE', *, *, #169214, .T. ) ;
#9176 = ORIENTED_EDGE ( 'NONE', *, *, #116042, .T. ) ;
#9178 = ORIENTED_EDGE ( 'NONE', *, *, #172551, .F. ) ;
#9179 = DIRECTION ( 'NONE',  ( 0.000000000000000000, 0.8814952561688476074, -0.4721928772777262417 ) ) ;
#9180 = DIRECTION ( 'NONE',  ( -0.000000000000000000, -0.9126074666063771490, -0.4088369013363281623 ) ) ;
#9182 = FACE_OUTER_BOUND ( 'NONE', #128838, .T. ) ;
#9181 = DIRECTION ( 'NONE',  ( -0.000000000000000000, 0.9126074666063770380, 0.4088369013363281068 ) ) ;
#9183 = CARTESIAN_POINT ( 'NONE',  ( 21.14999999999999858, 11.75000000001116263, -45.65000000000000568 ) ) ;
#9184 = ORIENTED_EDGE ( 'NONE', *, *, #68451, .F. ) ;
#9185 = DIRECTION ( 'NONE',  ( 0.000000000000000000, 0.000000000000000000, 1.000000000000000000 ) ) ;
#9186 = EDGE_LOOP ( 'NONE', ( #86071, #220778, #105308, #152684 ) ) ;
#9187 = DIRECTION ( 'NONE',  ( 0.000000000000000000, 0.000000000000000000, -1.000000000000000000 ) ) ;
#9189 = CIRCLE ( 'NONE', #217443, 0.1000000000000028644 ) ;
#9188 = DIRECTION ( 'NONE',  ( 0.000000000000000000, 0.2617529984164955192, 0.9651348961777178603 ) ) ;
#9190 = CARTESIAN_POINT ( 'NONE',  ( -21.05000000000000071, 1.658775325997240868, -230.6916041481598540 ) ) ;
#9191 = VERTEX_POINT ( 'NONE', #97422 ) ;
#9192 = DIRECTION ( 'NONE',  ( 0.000000000000000000, 0.000000000000000000, 1.000000000000000000 ) ) ;
#9193 = LINE ( 'NONE', #30074, #75767 ) ;
#9194 = ORIENTED_EDGE ( 'NONE', *, *, #113879, .T. ) ;
#9195 = ORIENTED_EDGE ( 'NONE', *, *, #159099, .T. ) ;
#9196 = CARTESIAN_POINT ( 'NONE',  ( 19.75857864376268935, 64.35000000001177511, -78.27310748452438816 ) ) ;
#9197 = DIRECTION ( 'NONE',  ( 0.000000000000000000, 0.000000000000000000, 1.000000000000000000 ) ) ;
#9198 = CARTESIAN_POINT ( 'NONE',  ( -20.64999999999999858, 29.14863708059993286, -237.4168895852561434 ) ) ;
#9199 = CYLINDRICAL_SURFACE ( 'NONE', #52014, 0.09999999999999939493 ) ;
#9200 = DIRECTION ( 'NONE',  ( -0.000000000000000000, -0.4088369013363281068, 0.9126074666063770380 ) ) ;
#9201 = CARTESIAN_POINT ( 'NONE',  ( -21.05000000000000071, 6.413662734869507887, -0.08559286336229579573 ) ) ;
#9202 = EDGE_LOOP ( 'NONE', ( #123997, #81062, #37336, #1602 ) ) ;
#9203 = DIRECTION ( 'NONE',  ( 1.000000000000000000, 0.000000000000000000, 0.000000000000000000 ) ) ;
#9204 = CARTESIAN_POINT ( 'NONE',  ( -23.15000000000000213, 74.00000000001180922, -82.74772940728641402 ) ) ;
#9207 = DIRECTION ( 'NONE',  ( 0.000000000000000000, -0.8700118002898322711, 0.4930308989875231140 ) ) ;
#9206 = VECTOR ( 'NONE', #144673, 1000.000000000000000 ) ;
#9205 = CARTESIAN_POINT ( 'NONE',  ( -23.15000000000000213, 1.115600667400684642E-11, -200.9999999999999432 ) ) ;
#9210 = EDGE_CURVE ( 'NONE', #48580, #187169, #245401, .T. ) ;
#9209 = CARTESIAN_POINT ( 'NONE',  ( -18.39999999999999858, -9.599999999988849453, -107.1001893912220879 ) ) ;
#9208 = AXIS2_PLACEMENT_3D ( 'NONE', #207837, #29214, #9587 ) ;
#9211 = AXIS2_PLACEMENT_3D ( 'NONE', #172868, #77537, #257425 ) ;
#9212 = CARTESIAN_POINT ( 'NONE',  ( 22.60000000000000142, 76.00000000001237765, -170.0231074845243597 ) ) ;
#9213 = DIRECTION ( 'NONE',  ( -1.000000000000000000, 0.000000000000000000, -0.000000000000000000 ) ) ;
#9214 = CARTESIAN_POINT ( 'NONE',  ( 20.89878130938411616, 10.32747123227773045, -139.5774032850249569 ) ) ;
#9216 = VERTEX_POINT ( 'NONE', #33686 ) ;
#9215 = DIRECTION ( 'NONE',  ( 1.000000000000000000, -0.000000000000000000, -0.000000000000000000 ) ) ;
#9217 = EDGE_CURVE ( 'NONE', #198468, #23132, #24843, .T. ) ;
#9218 = VECTOR ( 'NONE', #142980, 1000.000000000000000 ) ;
#9219 = ADVANCED_FACE ( 'NONE', ( #216111 ), #175739, .T. ) ;
#9220 = CARTESIAN_POINT ( 'NONE',  ( 21.14999999999999858, 67.21339244341217523, -157.7731074845244166 ) ) ;
#9221 = CARTESIAN_POINT ( 'NONE',  ( 20.27550659511088682, 66.78395627750323627, -127.2731074845243597 ) ) ;
#9222 = EDGE_CURVE ( 'NONE', #221888, #61043, #41398, .T. ) ;
#9223 = VERTEX_POINT ( 'NONE', #256460 ) ;
#9224 = AXIS2_PLACEMENT_3D ( 'NONE', #114975, #155429, #234933 ) ;
#9225 = LINE ( 'NONE', #90039, #247305 ) ;
#9226 = DIRECTION ( 'NONE',  ( 5.603264701231746180E-32, -0.9126074666063769270, -0.4088369013363282733 ) ) ;
#9227 = DIRECTION ( 'NONE',  ( 0.000000000000000000, -1.265107689135680095E-16, 1.000000000000000000 ) ) ;
#9228 = EDGE_CURVE ( 'NONE', #156671, #193752, #220459, .T. ) ;
#9230 = ORIENTED_EDGE ( 'NONE', *, *, #227136, .F. ) ;
#9229 = EDGE_CURVE ( 'NONE', #26209, #193142, #166312, .T. ) ;
#9231 = CARTESIAN_POINT ( 'NONE',  ( -20.94999999999999929, 79.14291928130901965, -196.3819507745080557 ) ) ;
#9233 = ORIENTED_EDGE ( 'NONE', *, *, #179815, .T. ) ;
#9232 = CARTESIAN_POINT ( 'NONE',  ( -23.25000000000000000, 68.69389471299010097, -223.1641309873017462 ) ) ;
#9234 = CARTESIAN_POINT ( 'NONE',  ( 21.05000000000000071, 6.540656951712400691, -167.5999999999999659 ) ) ;
#9235 = AXIS2_PLACEMENT_3D ( 'NONE', #57515, #137072, #38001 ) ;
#9236 = EDGE_CURVE ( 'NONE', #170976, #73589, #213543, .T. ) ;
#9237 = CARTESIAN_POINT ( 'NONE',  ( -21.45000000000000284, 12.03275902784684703, -220.0251779199349187 ) ) ;
#9238 = ORIENTED_EDGE ( 'NONE', *, *, #132402, .T. ) ;
#9239 = CARTESIAN_POINT ( 'NONE',  ( -16.88783316861810491, 66.05000000001261640, -190.7708434425451003 ) ) ;
#9240 = VECTOR ( 'NONE', #231816, 1000.000000000000000 ) ;
#9241 = CARTESIAN_POINT ( 'NONE',  ( 0.000000000000000000, 0.000000000000000000, 0.000000000000000000 ) ) ;
#9242 = CARTESIAN_POINT ( 'NONE',  ( -20.90851465518106167, 65.67467670974397720, -63.95317318268842399 ) ) ;
#9243 = CYLINDRICAL_SURFACE ( 'NONE', #69136, 0.09999999999999939493 ) ;
#9246 = EDGE_CURVE ( 'NONE', #34631, #251858, #12192, .T. ) ;
#9245 = TOROIDAL_SURFACE ( 'NONE', #92438, 0.4000000000000005773, 0.1000000000000000056 ) ;
#9244 = SPHERICAL_SURFACE ( 'NONE', #225558, 0.1000000000000000056 ) ;
#9247 = ORIENTED_EDGE ( 'NONE', *, *, #23806, .T. ) ;
#9248 = AXIS2_PLACEMENT_3D ( 'NONE', #251866, #151523, #150232 ) ;
#9249 = LINE ( 'NONE', #105754, #104322 ) ;
#9250 = DIRECTION ( 'NONE',  ( 0.000000000000000000, -1.000000000000000000, -6.982962677686266711E-15 ) ) ;
#9251 = AXIS2_PLACEMENT_3D ( 'NONE', #37350, #157307, #122985 ) ;
#9252 = CIRCLE ( 'NONE', #59099, 0.09999999999999939493 ) ;
#9253 = DIRECTION ( 'NONE',  ( 0.000000000000000000, 0.000000000000000000, -1.000000000000000000 ) ) ;
#9254 = ORIENTED_EDGE ( 'NONE', *, *, #132070, .T. ) ;
#9255 = EDGE_LOOP ( 'NONE', ( #250165, #202311 ) ) ;
#9257 = AXIS2_PLACEMENT_3D ( 'NONE', #5970, #46382, #62124 ) ;
#9256 = CARTESIAN_POINT ( 'NONE',  ( 22.59999954896768770, 76.00882823225424545, -81.27361615859231847 ) ) ;
#9258 = EDGE_CURVE ( 'NONE', #76756, #159519, #16455, .T. ) ;
#9260 = AXIS2_PLACEMENT_3D ( 'NONE', #216723, #117629, #237584 ) ;
#9259 = CYLINDRICAL_SURFACE ( 'NONE', #190463, 0.1000000000000024342 ) ;
#9261 = DIRECTION ( 'NONE',  ( -1.000000000000000000, 0.000000000000000000, 0.000000000000000000 ) ) ;
#9262 = DIRECTION ( 'NONE',  ( 0.000000000000000000, 0.2128009952263268945, -0.9770955615653388326 ) ) ;
#9263 = CARTESIAN_POINT ( 'NONE',  ( -20.64999999999999858, 85.00000000001261924, -193.6291383618718385 ) ) ;
#9265 = CARTESIAN_POINT ( 'NONE',  ( 22.44352723754029810, -2.470007687997479717, -189.6151348049303635 ) ) ;
#9264 = FACE_OUTER_BOUND ( 'NONE', #74650, .T. ) ;
#9266 = AXIS2_PLACEMENT_3D ( 'NONE', #102322, #103618, #243152 ) ;
#9267 = VECTOR ( 'NONE', #125258, 1000.000000000000000 ) ;
#9268 = DIRECTION ( 'NONE',  ( -0.9880948137434723000, 0.1503223940869687358, 0.03273861465020812961 ) ) ;
#9269 = CARTESIAN_POINT ( 'NONE',  ( -21.65000000000000213, 7.708578643762696636, -21.25000000000000000 ) ) ;
#9271 = CARTESIAN_POINT ( 'NONE',  ( -23.25000000000000355, 13.44928205424795564, -207.5377222505711075 ) ) ;
#9270 = VECTOR ( 'NONE', #192080, 1000.000000000000000 ) ;
#9273 = ORIENTED_EDGE ( 'NONE', *, *, #14604, .F. ) ;
#9272 = CARTESIAN_POINT ( 'NONE',  ( 12.84435279558019438, 62.87834062276079550, -215.9526216959266094 ) ) ;
#9274 = CARTESIAN_POINT ( 'NONE',  ( 21.07928932188134397, 69.67148334361908724, -170.1220026301787982 ) ) ;
#9275 = CARTESIAN_POINT ( 'NONE',  ( -21.08134388332232589, -1.273944004185077805, -194.7942773797408336 ) ) ;
#9277 = DIRECTION ( 'NONE',  ( 1.000000000000000000, -0.000000000000000000, -0.000000000000000000 ) ) ;
#9276 = DIRECTION ( 'NONE',  ( 0.000000000000000000, 0.000000000000000000, -1.000000000000000000 ) ) ;
#9278 = AXIS2_PLACEMENT_3D ( 'NONE', #71171, #171568, #73744 ) ;
#9279 = EDGE_CURVE ( 'NONE', #132498, #199740, #55720, .T. ) ;
#9280 = ORIENTED_EDGE ( 'NONE', *, *, #193178, .T. ) ;
#9281 = LINE ( 'NONE', #28899, #197521 ) ;
#9282 = CARTESIAN_POINT ( 'NONE',  ( 19.80993210785465308, 64.25000000001242029, -111.7559897356370868 ) ) ;
#9283 = CARTESIAN_POINT ( 'NONE',  ( -23.24999999999999645, 85.60000000001240039, -163.3229180933022633 ) ) ;
#9284 = CARTESIAN_POINT ( 'NONE',  ( -21.11825140030087766, 69.55459243459219465, -103.0303111051572529 ) ) ;
#9286 = CARTESIAN_POINT ( 'NONE',  ( 22.48660254037844908, 12.63302488529802936, -223.3515224085915065 ) ) ;
#9285 = AXIS2_PLACEMENT_3D ( 'NONE', #25301, #41019, #39742 ) ;
#9287 = VERTEX_POINT ( 'NONE', #75358 ) ;
#9288 = ORIENTED_EDGE ( 'NONE', *, *, #98804, .T. ) ;
#9289 = CARTESIAN_POINT ( 'NONE',  ( 23.14999999999999858, 4.813084112160684214, -88.55848224347622022 ) ) ;
#9290 = ORIENTED_EDGE ( 'NONE', *, *, #13159, .T. ) ;
#9291 = CARTESIAN_POINT ( 'NONE',  ( -18.34374000495059676, 16.37079970714665933, -222.2530670965321349 ) ) ;
#9292 = AXIS2_PLACEMENT_3D ( 'NONE', #186308, #87176, #208452 ) ;
#9293 = ORIENTED_EDGE ( 'NONE', *, *, #157619, .F. ) ;
#9294 = EDGE_CURVE ( 'NONE', #205806, #219246, #148221, .T. ) ;
#9295 = DIRECTION ( 'NONE',  ( 0.000000000000000000, 0.000000000000000000, -1.000000000000000000 ) ) ;
#9296 = AXIS2_PLACEMENT_3D ( 'NONE', #147100, #105382, #226639 ) ;
#9297 = FACE_OUTER_BOUND ( 'NONE', #214035, .T. ) ;
#9298 = ORIENTED_EDGE ( 'NONE', *, *, #200597, .F. ) ;
#9299 = EDGE_CURVE ( 'NONE', #97104, #223391, #157952, .T. ) ;
#9300 = DIRECTION ( 'NONE',  ( 0.000000000000000000, -0.8454177738465993297, -0.5341055959866553016 ) ) ;
#9301 = B_SPLINE_CURVE_WITH_KNOTS ( 'NONE', 3,
 ( #195955, #232520, #56404, #152996, #92975, #34322 ),
 .UNSPECIFIED., .F., .F.,
 ( 4, 2, 4 ),
 ( 0.000000000000000000, 0.0002113392456166052376, 0.0004226784912332104752 ),
 .UNSPECIFIED. ) ;
#9302 = DIRECTION ( 'NONE',  ( -0.000000000000000000, 0.000000000000000000, -1.000000000000000000 ) ) ;
#9303 = EDGE_CURVE ( 'NONE', #196167, #30659, #62227, .T. ) ;
#9304 = DIRECTION ( 'NONE',  ( -0.000000000000000000, 0.9910827722268037432, 0.1332476588733682299 ) ) ;
#9305 = EDGE_CURVE ( 'NONE', #37875, #76136, #70639, .T. ) ;
#9306 = DIRECTION ( 'NONE',  ( 0.000000000000000000, 0.000000000000000000, -1.000000000000000000 ) ) ;
#9307 = CYLINDRICAL_SURFACE ( 'NONE', #103824, 0.09999999999998898659 ) ;
#9308 = DIRECTION ( 'NONE',  ( -1.000000000000000000, -0.000000000000000000, -0.000000000000000000 ) ) ;
#9309 = ORIENTED_EDGE ( 'NONE', *, *, #186911, .F. ) ;
#9310 = CIRCLE ( 'NONE', #213306, 0.1000000000000004774 ) ;
#9312 = CARTESIAN_POINT ( 'NONE',  ( -17.11825945287482753, 10.05000000001113847, -113.2500000000000284 ) ) ;
#9311 = DIRECTION ( 'NONE',  ( 1.000000000000000000, -1.836970198721029934E-16, -1.601412966608202925E-30 ) ) ;
#9313 = VERTEX_POINT ( 'NONE', #45181 ) ;
#9315 = ORIENTED_EDGE ( 'NONE', *, *, #234714, .T. ) ;
#9314 = CARTESIAN_POINT ( 'NONE',  ( 23.14999999999999503, 69.35000000001228670, -157.8731074845244109 ) ) ;
#9316 = ORIENTED_EDGE ( 'NONE', *, *, #201423, .F. ) ;
#9317 = DIRECTION ( 'NONE',  ( 0.000000000000000000, -7.026728003956686545E-15, 1.000000000000000000 ) ) ;
#9318 = CARTESIAN_POINT ( 'NONE',  ( 12.42718393586867087, 66.62934494888880010, -152.4972842285435490 ) ) ;
#9319 = CYLINDRICAL_SURFACE ( 'NONE', #147477, 0.09999999999999982514 ) ;
#9320 = EDGE_CURVE ( 'NONE', #127119, #14186, #63453, .T. ) ;
#9321 = CARTESIAN_POINT ( 'NONE',  ( -17.78043020864320667, 10.85359211201683927, -43.83695083427979000 ) ) ;
#9322 = ORIENTED_EDGE ( 'NONE', *, *, #163419, .T. ) ;
#9323 = DIRECTION ( 'NONE',  ( 0.000000000000000000, -6.982962677686266711E-15, 1.000000000000000000 ) ) ;
#9324 = CARTESIAN_POINT ( 'NONE',  ( 18.56308993302939925, 10.38069115533503961, -158.7392226389382870 ) ) ;
#9325 = ORIENTED_EDGE ( 'NONE', *, *, #232881, .T. ) ;
#9326 = CARTESIAN_POINT ( 'NONE',  ( 18.39999999999999858, -9.499999999988844479, -174.5320693966996544 ) ) ;
#9327 = DIRECTION ( 'NONE',  ( 0.000000000000000000, 0.000000000000000000, 1.000000000000000000 ) ) ;
#9328 = EDGE_LOOP ( 'NONE', ( #42578, #202523 ) ) ;
#9329 = DIRECTION ( 'NONE',  ( 0.000000000000000000, -1.000000000000000000, -6.982962677686266711E-15 ) ) ;
#9330 = EDGE_CURVE ( 'NONE', #144444, #18380, #3960, .T. ) ;
#9331 = ORIENTED_EDGE ( 'NONE', *, *, #112672, .T. ) ;
#9332 = CARTESIAN_POINT ( 'NONE',  ( 18.41356215285961184, -9.499999999988865795, -141.0320693966996544 ) ) ;
#9333 = ORIENTED_EDGE ( 'NONE', *, *, #192121, .F. ) ;
#9334 = ADVANCED_FACE ( 'NONE', ( #163857, #162586 ), #99990, .T. ) ;
#9335 = CARTESIAN_POINT ( 'NONE',  ( 21.05000000000000071, 64.40000000001175806, -76.45131071479988805 ) ) ;
#9336 = CARTESIAN_POINT ( 'NONE',  ( -20.85000000000000142, -1.851617760457748618, -145.6031897196037050 ) ) ;
#9337 = EDGE_CURVE ( 'NONE', #190642, #195198, #232937, .T. ) ;
#9338 = DIRECTION ( 'NONE',  ( 1.000000000000000000, 0.000000000000000000, 0.000000000000000000 ) ) ;
#9339 = CARTESIAN_POINT ( 'NONE',  ( -20.94999999999999929, 76.00000000001165290, -69.52310748452431710 ) ) ;
#9340 = DIRECTION ( 'NONE',  ( 0.000000000000000000, -1.000000000000000000, -2.891205793294679805E-16 ) ) ;
#9341 = VERTEX_POINT ( 'NONE', #80418 ) ;
#9342 = LINE ( 'NONE', #48472, #235524 ) ;
#9343 = ORIENTED_EDGE ( 'NONE', *, *, #33030, .T. ) ;
#9345 = CARTESIAN_POINT ( 'NONE',  ( -20.54999999999999716, 10.55064993524514705, -215.8448235403523370 ) ) ;
#9344 = FACE_OUTER_BOUND ( 'NONE', #223232, .T. ) ;
#9346 = VERTEX_POINT ( 'NONE', #183421 ) ;
#9347 = CARTESIAN_POINT ( 'NONE',  ( -0.8999999999999994671, -8.279289321881350361, 22.02928932188134326 ) ) ;
#9349 = DIRECTION ( 'NONE',  ( 0.000000000000000000, 6.982962677686266711E-15, -1.000000000000000000 ) ) ;
#9348 = AXIS2_PLACEMENT_3D ( 'NONE', #64988, #183669, #84506 ) ;
#9350 = DIRECTION ( 'NONE',  ( 1.000000000000000000, 0.000000000000000000, 0.000000000000000000 ) ) ;
#9351 = ORIENTED_EDGE ( 'NONE', *, *, #130059, .F. ) ;
#9353 = ORIENTED_EDGE ( 'NONE', *, *, #11897, .T. ) ;
#9352 = DIRECTION ( 'NONE',  ( -1.000000000000000000, 0.000000000000000000, 0.000000000000000000 ) ) ;
#9354 = DIRECTION ( 'NONE',  ( 1.000000000000000000, -2.952720810173289112E-16, -2.061873921506763405E-30 ) ) ;
#9356 = CARTESIAN_POINT ( 'NONE',  ( 18.49999999999999289, 15.47141130571843881, -222.9781839875250284 ) ) ;
#9355 = DIRECTION ( 'NONE',  ( 0.000000000000000000, 1.000000000000000000, 0.000000000000000000 ) ) ;
#9359 = ADVANCED_FACE ( 'NONE', ( #142973 ), #227979, .T. ) ;
#9358 = VERTEX_POINT ( 'NONE', #105116 ) ;
#9357 = CARTESIAN_POINT ( 'NONE',  ( -16.89268316805465986, 9.951721813253337601, -154.8557524785455541 ) ) ;
#9360 = CIRCLE ( 'NONE', #217634, 0.09999999999999939493 ) ;
#9361 = EDGE_LOOP ( 'NONE', ( #239588, #228154, #121598, #131714 ) ) ;
#9362 = ADVANCED_FACE ( 'NONE', ( #102551 ), #165136, .F. ) ;
#9363 = DIRECTION ( 'NONE',  ( 1.000000000000000000, 0.000000000000000000, 0.000000000000000000 ) ) ;
#9364 = DIRECTION ( 'NONE',  ( 1.000000000000000000, 0.000000000000000000, 0.000000000000000000 ) ) ;
#9365 = ORIENTED_EDGE ( 'NONE', *, *, #229920, .F. ) ;
#9366 = DIRECTION ( 'NONE',  ( -4.391705002472929091E-16, 1.000000000000000000, 0.000000000000000000 ) ) ;
#9367 = ORIENTED_EDGE ( 'NONE', *, *, #29750, .T. ) ;
#9368 = AXIS2_PLACEMENT_3D ( 'NONE', #122579, #109398, #69027 ) ;
#9369 = EDGE_CURVE ( 'NONE', #242139, #209946, #153869, .T. ) ;
#9370 = DIRECTION ( 'NONE',  ( 1.073024830501117725E-15, 6.982962677686266711E-15, -1.000000000000000000 ) ) ;
#9371 = CARTESIAN_POINT ( 'NONE',  ( -23.39999999999994529, 64.25000000001119815, -36.02310748452479316 ) ) ;
#9372 = VERTEX_POINT ( 'NONE', #170318 ) ;
#9373 = CARTESIAN_POINT ( 'NONE',  ( -20.65000000000000568, 68.75000000001188027, -90.37310748452435405 ) ) ;
#9374 = CIRCLE ( 'NONE', #30252, 0.1999999999999987899 ) ;
#9375 = EDGE_CURVE ( 'NONE', #176131, #94408, #108029, .T. ) ;
#9376 = CIRCLE ( 'NONE', #26156, 12.87499999999999822 ) ;
#9377 = VECTOR ( 'NONE', #120298, 1000.000000000000000 ) ;
#9378 = AXIS2_PLACEMENT_3D ( 'NONE', #76810, #192922, #255397 ) ;
#9379 = EDGE_CURVE ( 'NONE', #25295, #184016, #111584, .T. ) ;
#9380 = VERTEX_POINT ( 'NONE', #107722 ) ;
#9381 = CARTESIAN_POINT ( 'NONE',  ( 20.94999999999999929, 7.244009986534929446, -211.6437749090809177 ) ) ;
#9382 = ADVANCED_FACE ( 'NONE', ( #148138 ), #146833, .F. ) ;
#9383 = ORIENTED_EDGE ( 'NONE', *, *, #75208, .F. ) ;
#9384 = ORIENTED_EDGE ( 'NONE', *, *, #144395, .F. ) ;
#9386 = EDGE_CURVE ( 'NONE', #17591, #108265, #37297, .T. ) ;
#9385 = CARTESIAN_POINT ( 'NONE',  ( -18.59999999999999787, 68.22930980752001062, -227.7331931781284879 ) ) ;
#9387 = VERTEX_POINT ( 'NONE', #86855 ) ;
#9388 = CARTESIAN_POINT ( 'NONE',  ( -16.81930730667008334, 23.03959843057016244, -230.9827737272960917 ) ) ;
#9389 = VERTEX_POINT ( 'NONE', #127292 ) ;
#9391 = ORIENTED_EDGE ( 'NONE', *, *, #63587, .T. ) ;
#9390 = CARTESIAN_POINT ( 'NONE',  ( -23.25000000000000000, 85.00000000001179501, -79.41707660717668205 ) ) ;
#9392 = DIRECTION ( 'NONE',  ( 0.000000000000000000, 0.05689261644169250898, -0.9983803033886528011 ) ) ;
#9393 = B_SPLINE_CURVE_WITH_KNOTS ( 'NONE', 3,
 ( #141478, #123206, #166219, #22847, #121930, #43673 ),
 .UNSPECIFIED., .F., .F.,
 ( 4, 2, 4 ),
 ( 1.138412281109779656E-18, 0.0001569047307838638975, 0.0003138094615677266023 ),
 .UNSPECIFIED. ) ;
#9394 = EDGE_LOOP ( 'NONE', ( #140865, #151732, #121750 ) ) ;
#9395 = LINE ( 'NONE', #126783, #251614 ) ;
#9396 = ORIENTED_EDGE ( 'NONE', *, *, #184275, .F. ) ;
#9399 = EDGE_LOOP ( 'NONE', ( #90694, #116474, #251369, #160808, #204547 ) ) ;
#9398 = ORIENTED_EDGE ( 'NONE', *, *, #204945, .T. ) ;
#9397 = CARTESIAN_POINT ( 'NONE',  ( -16.94107738177415712, 65.98576071487495653, -56.97310748452439810 ) ) ;
#9400 = CARTESIAN_POINT ( 'NONE',  ( 20.94999999999999929, 7.120270961708750512, -171.1595630418393625 ) ) ;
#9402 = LINE ( 'NONE', #51064, #114930 ) ;
#9401 = AXIS2_PLACEMENT_3D ( 'NONE', #170061, #215550, #59012 ) ;
#9403 = ORIENTED_EDGE ( 'NONE', *, *, #123253, .F. ) ;
#9404 = VECTOR ( 'NONE', #164383, 1000.000000000000000 ) ;
#9405 = EDGE_CURVE ( 'NONE', #211645, #150463, #16638, .T. ) ;
#9406 = ADVANCED_FACE ( 'NONE', ( #248518 ), #41594, .T. ) ;
#9407 = EDGE_LOOP ( 'NONE', ( #142358, #176255, #155377, #196202 ) ) ;
#9408 = AXIS2_PLACEMENT_3D ( 'NONE', #213095, #18747, #239090 ) ;
#9410 = ORIENTED_EDGE ( 'NONE', *, *, #246327, .F. ) ;
#9409 = DIRECTION ( 'NONE',  ( -1.000000000000000000, -0.000000000000000000, -0.000000000000000000 ) ) ;
#9411 = CARTESIAN_POINT ( 'NONE',  ( -21.05000000000000071, 1.115600667400684642E-11, -67.00000000000000000 ) ) ;
#9412 = ORIENTED_EDGE ( 'NONE', *, *, #53208, .T. ) ;
#9413 = DIRECTION ( 'NONE',  ( -1.000000000000000000, -0.000000000000000000, -0.000000000000000000 ) ) ;
#9414 = CARTESIAN_POINT ( 'NONE',  ( 18.49999999999999289, 65.62657994473188694, -111.7573193598984176 ) ) ;
#9415 = CIRCLE ( 'NONE', #234262, 0.5000000000000004441 ) ;
#9416 = ORIENTED_EDGE ( 'NONE', *, *, #83284, .F. ) ;
#9418 = ADVANCED_FACE ( 'NONE', ( #150707 ), #189836, .T. ) ;
#9417 = DIRECTION ( 'NONE',  ( 1.000000000000000000, 0.000000000000000000, 0.000000000000000000 ) ) ;
#9419 = DIRECTION ( 'NONE',  ( -2.578261006436900068E-14, 0.8490545835447238510, 0.5283051335749973099 ) ) ;
#9420 = CIRCLE ( 'NONE', #84379, 0.1000000000000028644 ) ;
#9421 = AXIS2_PLACEMENT_3D ( 'NONE', #250287, #114625, #110769 ) ;
#9423 = VERTEX_POINT ( 'NONE', #88126 ) ;
#9422 = AXIS2_PLACEMENT_3D ( 'NONE', #67820, #226894, #127809 ) ;
#9424 = ADVANCED_FACE ( 'NONE', ( #227663 ), #51565, .T. ) ;
#9426 = VERTEX_POINT ( 'NONE', #171582 ) ;
#9425 = LINE ( 'NONE', #88950, #126444 ) ;
#9427 = SPHERICAL_SURFACE ( 'NONE', #181756, 0.1000000000000000056 ) ;
#9428 = CIRCLE ( 'NONE', #5308, 0.09999999999998898659 ) ;
#9429 = AXIS2_PLACEMENT_3D ( 'NONE', #214931, #132847, #251485 ) ;
#9431 = ORIENTED_EDGE ( 'NONE', *, *, #244263, .T. ) ;
#9430 = ORIENTED_EDGE ( 'NONE', *, *, #112083, .T. ) ;
#9432 = VERTEX_POINT ( 'NONE', #166454 ) ;
#9433 = DIRECTION ( 'NONE',  ( 0.000000000000000000, 0.4721928772778128947, 0.8814952561688012000 ) ) ;
#9434 = ORIENTED_EDGE ( 'NONE', *, *, #93467, .T. ) ;
#9435 = ORIENTED_EDGE ( 'NONE', *, *, #181041, .F. ) ;
#9436 = CARTESIAN_POINT ( 'NONE',  ( -20.94999999999999929, -1.835859311443635233, -45.00443916879852679 ) ) ;
#9437 = ORIENTED_EDGE ( 'NONE', *, *, #237116, .T. ) ;
#9438 = ADVANCED_FACE ( 'NONE', ( #128578 ), #125997, .F. ) ;
#9439 = DIRECTION ( 'NONE',  ( 0.000000000000000000, 0.9910827722268042983, 0.1332476588733650935 ) ) ;
#9440 = CIRCLE ( 'NONE', #196877, 0.1000000000000124678 ) ;
#9441 = DIRECTION ( 'NONE',  ( 1.000000000000000000, 0.000000000000000000, 0.000000000000000000 ) ) ;
#9443 = ORIENTED_EDGE ( 'NONE', *, *, #72576, .T. ) ;
#9442 = CIRCLE ( 'NONE', #155230, 0.1000000000000054040 ) ;
#9444 = EDGE_LOOP ( 'NONE', ( #80988, #109614, #195871, #99520 ) ) ;
#9445 = ADVANCED_FACE ( 'NONE', ( #29512 ), #28226, .F. ) ;
#9446 = CIRCLE ( 'NONE', #159487, 0.2000000000000005107 ) ;
#9447 = CARTESIAN_POINT ( 'NONE',  ( -23.25000000000000355, 5.650000000011139001, -154.8500000000000227 ) ) ;
#9448 = ORIENTED_EDGE ( 'NONE', *, *, #23057, .F. ) ;
#9449 = AXIS2_PLACEMENT_3D ( 'NONE', #19687, #104318, #222994 ) ;
#9450 = CIRCLE ( 'NONE', #230211, 0.09999999999999939493 ) ;
#9451 = FACE_OUTER_BOUND ( 'NONE', #250486, .T. ) ;
#9452 = VERTEX_POINT ( 'NONE', #7341 ) ;
#9453 = DIRECTION ( 'NONE',  ( -1.000000000000000000, -0.000000000000000000, -0.000000000000000000 ) ) ;
#9454 = ADVANCED_FACE ( 'NONE', ( #245964 ), #216528, .F. ) ;
#9455 = CIRCLE ( 'NONE', #225364, 0.2000000000000057288 ) ;
#9457 = ORIENTED_EDGE ( 'NONE', *, *, #147447, .F. ) ;
#9456 = DIRECTION ( 'NONE',  ( 0.000000000000000000, -1.000000000000000000, -0.000000000000000000 ) ) ;
#9458 = DIRECTION ( 'NONE',  ( -0.000000000000000000, -0.8814952561688430555, 0.4721928772777346239 ) ) ;
#9459 = CARTESIAN_POINT ( 'NONE',  ( 20.85000000000000142, -11.74999999998883560, -97.60000000000005116 ) ) ;
#9460 = DIRECTION ( 'NONE',  ( 1.000000000000000000, 3.265361837132813093E-16, -0.000000000000000000 ) ) ;
#9461 = DIRECTION ( 'NONE',  ( 0.000000000000000000, 0.000000000000000000, -1.000000000000000000 ) ) ;
#9462 = CARTESIAN_POINT ( 'NONE',  ( -21.14999999999999858, 64.35000000001208775, -129.7392418215462158 ) ) ;
#9464 = FACE_OUTER_BOUND ( 'NONE', #69921, .T. ) ;
#9463 = CYLINDRICAL_SURFACE ( 'NONE', #169628, 0.09999999999999543976 ) ;
#9465 = DIRECTION ( 'NONE',  ( 0.000000000000000000, 0.000000000000000000, 1.000000000000000000 ) ) ;
#9466 = CARTESIAN_POINT ( 'NONE',  ( -21.14999999999999858, 11.65000000001115588, -134.1000000000000227 ) ) ;
#9467 = AXIS2_PLACEMENT_3D ( 'NONE', #37202, #154593, #175434 ) ;
#9469 = EDGE_LOOP ( 'NONE', ( #147585, #148990, #257070, #106515 ) ) ;
#9468 = AXIS2_PLACEMENT_3D ( 'NONE', #110669, #72861, #148520 ) ;
#9470 = VECTOR ( 'NONE', #76242, 1000.000000000000000 ) ;
#9471 = ORIENTED_EDGE ( 'NONE', *, *, #216403, .F. ) ;
#9473 = ORIENTED_EDGE ( 'NONE', *, *, #1084, .F. ) ;
#9472 = CARTESIAN_POINT ( 'NONE',  ( -20.54999999999999716, 82.09643798151613225, -215.4278993322501208 ) ) ;
#9474 = ORIENTED_EDGE ( 'NONE', *, *, #181279, .T. ) ;
#9475 = DIRECTION ( 'NONE',  ( -1.000000000000000000, 7.304098846218163263E-16, -4.217023435051627211E-16 ) ) ;
#9476 = PLANE ( 'NONE',  #248521 ) ;
#9478 = DIRECTION ( 'NONE',  ( 1.000000000000000000, 0.000000000000000000, 0.000000000000000000 ) ) ;
#9477 = DIRECTION ( 'NONE',  ( -1.000000000000000000, 1.207181226542539700E-16, -2.694675058168174199E-16 ) ) ;
#9479 = ORIENTED_EDGE ( 'NONE', *, *, #226367, .T. ) ;
#9480 = ORIENTED_EDGE ( 'NONE', *, *, #178888, .T. ) ;
#9481 = CARTESIAN_POINT ( 'NONE',  ( 18.49713797159849094, -9.446482327567860438, -40.57145812161018483 ) ) ;
#9482 = CARTESIAN_POINT ( 'NONE',  ( 20.94999999999999929, 1.115600667400684642E-11, -202.9999999999999716 ) ) ;
#9483 = CIRCLE ( 'NONE', #26080, 0.2000000000000057288 ) ;
#9484 = ORIENTED_EDGE ( 'NONE', *, *, #121139, .T. ) ;
#9485 = CYLINDRICAL_SURFACE ( 'NONE', #38223, 0.09999999999998898659 ) ;
#9486 = DIRECTION ( 'NONE',  ( -0.000000000000000000, -0.000000000000000000, 1.000000000000000000 ) ) ;
#9487 = CARTESIAN_POINT ( 'NONE',  ( 20.90000000000000213, -1.212568896937008089, -7.800000000000000711 ) ) ;
#9488 = DIRECTION ( 'NONE',  ( -4.701977403289178058E-30, -2.433019743745433765E-14, 1.000000000000000000 ) ) ;
#9489 = VECTOR ( 'NONE', #16033, 1000.000000000000000 ) ;
#9490 = DIRECTION ( 'NONE',  ( -0.000000000000000000, -0.2128009952263603677, 0.9770955615653313941 ) ) ;
#9492 = ORIENTED_EDGE ( 'NONE', *, *, #147576, .F. ) ;
#9491 = DIRECTION ( 'NONE',  ( 1.000000000000000000, 0.000000000000000000, 0.000000000000000000 ) ) ;
#9493 = CARTESIAN_POINT ( 'NONE',  ( -16.77683809663752257, 52.34166666667924517, -186.7731074845245303 ) ) ;
#9494 = CARTESIAN_POINT ( 'NONE',  ( -40.23850191057533010, 61.64150943397345372, -36.51839050339276582 ) ) ;
#9495 = LINE ( 'NONE', #89028, #183353 ) ;
#9496 = CARTESIAN_POINT ( 'NONE',  ( 18.59999994388910238, 85.36356618708308019, -95.84199024772335918 ) ) ;
#9497 = ORIENTED_EDGE ( 'NONE', *, *, #194506, .T. ) ;
#9498 = DIRECTION ( 'NONE',  ( -0.000000000000000000, 0.9371753822965315228, -0.3488585713686134238 ) ) ;
#9499 = CARTESIAN_POINT ( 'NONE',  ( -17.11825945287482753, 66.05000000001230376, -157.2731074845244166 ) ) ;
#9501 = CYLINDRICAL_SURFACE ( 'NONE', #207748, 0.09999999999998898659 ) ;
#9500 = CARTESIAN_POINT ( 'NONE',  ( -20.64999999999999858, 1.115600667400684642E-11, -200.9999999999999432 ) ) ;
#9503 = EDGE_CURVE ( 'NONE', #39978, #208088, #212274, .T. ) ;
#9502 = DIRECTION ( 'NONE',  ( 0.000000000000000000, 7.116814260417668513E-15, -1.000000000000000000 ) ) ;
#9504 = CARTESIAN_POINT ( 'NONE',  ( -16.79270642812322123, 9.946244216949036598, -54.33893327856191746 ) ) ;
#9505 = CARTESIAN_POINT ( 'NONE',  ( -18.40000000000000213, 43.39957528361355799, -233.6562381667159798 ) ) ;
#9506 = CARTESIAN_POINT ( 'NONE',  ( 23.25000000000000000, -9.599999999988842347, -124.1060308773475924 ) ) ;
#9507 = CARTESIAN_POINT ( 'NONE',  ( -23.25000000000000000, -11.64999999998884483, -155.7499999999999716 ) ) ;
#9508 = LINE ( 'NONE', #224697, #110051 ) ;
#9509 = ORIENTED_EDGE ( 'NONE', *, *, #68971, .F. ) ;
#9510 = CIRCLE ( 'NONE', #42837, 0.1000000000000124678 ) ;
#9511 = ORIENTED_EDGE ( 'NONE', *, *, #209307, .T. ) ;
#9512 = ORIENTED_EDGE ( 'NONE', *, *, #170955, .F. ) ;
#9513 = PLANE ( 'NONE',  #94477 ) ;
#9514 = DIRECTION ( 'NONE',  ( -0.7071067811865127117, -0.7071067811865821007, 0.000000000000000000 ) ) ;
#9515 = VERTEX_POINT ( 'NONE', #149445 ) ;
#9516 = EDGE_CURVE ( 'NONE', #161437, #149939, #154045, .T. ) ;
#9517 = ORIENTED_EDGE ( 'NONE', *, *, #150988, .F. ) ;
#9518 =( NAMED_UNIT ( * ) SI_UNIT ( $, .STERADIAN. ) SOLID_ANGLE_UNIT ( ) );
#9519 = VECTOR ( 'NONE', #579, 1000.000000000000000 ) ;
#9520 = ORIENTED_EDGE ( 'NONE', *, *, #243357, .F. ) ;
#9521 = CARTESIAN_POINT ( 'NONE',  ( -21.59142135623730852, 7.850000000011158718, -79.25000000000004263 ) ) ;
#9522 = VERTEX_POINT ( 'NONE', #256152 ) ;
#9523 = AXIS2_PLACEMENT_3D ( 'NONE', #250194, #31188, #88524 ) ;
#9524 = CARTESIAN_POINT ( 'NONE',  ( 21.05000000000000071, -0.09999999999999939493, 0.000000000000000000 ) ) ;
#9525 = DIRECTION ( 'NONE',  ( 1.000000000000000000, 3.265361837132813093E-16, -0.000000000000000000 ) ) ;
#9526 = DIRECTION ( 'NONE',  ( 1.734723475976817507E-14, 1.000000000000000000, 6.982962677686266711E-15 ) ) ;
#9527 = AXIS2_PLACEMENT_3D ( 'NONE', #133334, #155498, #115051 ) ;
#9528 = ADVANCED_FACE ( 'NONE', ( #194989 ), #77555, .F. ) ;
#9529 = CARTESIAN_POINT ( 'NONE',  ( -22.16821283564876666, 7.558973340791935058, -67.00000000000004263 ) ) ;
#9530 = EDGE_CURVE ( 'NONE', #87211, #166805, #162377, .T. ) ;
#9531 = DIRECTION ( 'NONE',  ( 0.000000000000000000, 0.9126074666063770380, 0.4088369013363281068 ) ) ;
#9533 = ORIENTED_EDGE ( 'NONE', *, *, #49799, .T. ) ;
#9532 = CARTESIAN_POINT ( 'NONE',  ( 21.08804582317323906, 44.29990453334584544, -236.3997463056264792 ) ) ;
#9535 = CARTESIAN_POINT ( 'NONE',  ( 21.06277459767431992, 8.872862438279401687, -79.20399919235673281 ) ) ;
#9534 = FACE_BOUND ( 'NONE', #151284, .T. ) ;
#9536 = CARTESIAN_POINT ( 'NONE',  ( -18.40000000000000213, 64.52683809664974035, -149.0731074845244279 ) ) ;
#9537 = EDGE_LOOP ( 'NONE', ( #165368, #75255, #171496, #80000, #155976 ) ) ;
#9538 = DIRECTION ( 'NONE',  ( 0.000000000000000000, 0.000000000000000000, -1.000000000000000000 ) ) ;
#9540 = EDGE_CURVE ( 'NONE', #138314, #164116, #104079, .T. ) ;
#9539 = LINE ( 'NONE', #129504, #93814 ) ;
#9541 = DIRECTION ( 'NONE',  ( 0.000000000000000000, 0.008583690987127922528, 0.9999631594459055250 ) ) ;
#9542 = ORIENTED_EDGE ( 'NONE', *, *, #257419, .T. ) ;
#9543 = CIRCLE ( 'NONE', #155339, 0.09999999999999864553 ) ;
#9545 = CARTESIAN_POINT ( 'NONE',  ( 18.59999999999999076, 65.79142135624930177, -115.1731074845243796 ) ) ;
#9544 = CIRCLE ( 'NONE', #196983, 0.1000000000000028644 ) ;
#9546 = ADVANCED_FACE ( 'NONE', ( #75054 ), #154590, .T. ) ;
#9547 = FACE_OUTER_BOUND ( 'NONE', #246459, .T. ) ;
#9548 = ORIENTED_EDGE ( 'NONE', *, *, #230996, .T. ) ;
#9549 = FACE_OUTER_BOUND ( 'NONE', #129348, .T. ) ;
#9550 = EDGE_CURVE ( 'NONE', #19155, #133755, #33368, .T. ) ;
#9551 = AXIS2_PLACEMENT_3D ( 'NONE', #28457, #45406, #253860 ) ;
#9552 = CARTESIAN_POINT ( 'NONE',  ( 23.50000000000005684, 84.00000000001119815, -34.86056257560453986 ) ) ;
#9553 = CARTESIAN_POINT ( 'NONE',  ( 20.94999999999999929, 86.27712145182582049, -209.5223386573213702 ) ) ;
#9554 = ORIENTED_EDGE ( 'NONE', *, *, #108228, .F. ) ;
#9555 = EDGE_LOOP ( 'NONE', ( #157336, #192219, #228495, #84681 ) ) ;
#9556 = AXIS2_PLACEMENT_3D ( 'NONE', #250747, #72137, #211643 ) ;
#9557 = AXIS2_PLACEMENT_3D ( 'NONE', #45932, #167202, #1969 ) ;
#9558 = AXIS2_PLACEMENT_3D ( 'NONE', #183773, #82067, #62545 ) ;
#9559 = EDGE_CURVE ( 'NONE', #111950, #205893, #145595, .T. ) ;
#9560 = CIRCLE ( 'NONE', #126072, 0.3999999999999975797 ) ;
#9561 = DIRECTION ( 'NONE',  ( 0.000000000000000000, 1.000000000000000000, 7.272083257015735086E-15 ) ) ;
#9562 = CARTESIAN_POINT ( 'NONE',  ( 23.14999999999999147, 1.148907358139439339E-11, -201.0000000000015064 ) ) ;
#9563 = CARTESIAN_POINT ( 'NONE',  ( -21.05000000000000071, 65.56055025928534974, -241.8869259205440301 ) ) ;
#9564 = DIRECTION ( 'NONE',  ( -1.000000000000000000, 1.652117596168391700E-15, 0.000000000000000000 ) ) ;
#9565 = LINE ( 'NONE', #70863, #5143 ) ;
#9566 = LINE ( 'NONE', #244318, #140856 ) ;
#9567 = DIRECTION ( 'NONE',  ( 0.000000000000000000, -0.4088369013363276072, 0.9126074666063772600 ) ) ;
#9568 = DIRECTION ( 'NONE',  ( 0.000000000000000000, 0.000000000000000000, -1.000000000000000000 ) ) ;
#9569 = VERTEX_POINT ( 'NONE', #97106 ) ;
#9570 = DIRECTION ( 'NONE',  ( 2.952720810173289112E-16, 1.000000000000000000, 6.982962677686266711E-15 ) ) ;
#9572 = ORIENTED_EDGE ( 'NONE', *, *, #140285, .T. ) ;
#9571 = SPHERICAL_SURFACE ( 'NONE', #175486, 0.1000000000000000056 ) ;
#9573 = CARTESIAN_POINT ( 'NONE',  ( 21.07016717456945187, 69.67905916191212157, -170.0231074845244450 ) ) ;
#9574 = DIRECTION ( 'NONE',  ( -0.000000000000000000, 0.8814952561688430555, -0.4721928772777346239 ) ) ;
#9575 = CARTESIAN_POINT ( 'NONE',  ( -23.49999999999994316, 76.00000000001119815, -36.02310748452479316 ) ) ;
#9576 = CARTESIAN_POINT ( 'NONE',  ( -16.85697194749132422, 66.09145628588846932, -123.5881032169100564 ) ) ;
#9577 = DIRECTION ( 'NONE',  ( 0.000000000000000000, 0.2128009952263604232, -0.9770955615653315052 ) ) ;
#9579 = EDGE_LOOP ( 'NONE', ( #79499, #154636, #156367, #240531 ) ) ;
#9578 = DIRECTION ( 'NONE',  ( -1.000000000000000000, 1.207181226542539946E-16, -2.694675058168174692E-16 ) ) ;
#9580 = FACE_OUTER_BOUND ( 'NONE', #20599, .T. ) ;
#9581 = FACE_OUTER_BOUND ( 'NONE', #236060, .T. ) ;
#9582 = CARTESIAN_POINT ( 'NONE',  ( -21.05000000000000071, 1.360870587203197646, -75.07299792709100927 ) ) ;
#9583 = DIRECTION ( 'NONE',  ( -1.000000000000000000, 0.000000000000000000, 0.000000000000000000 ) ) ;
#9584 = ORIENTED_EDGE ( 'NONE', *, *, #105583, .F. ) ;
#9585 = CARTESIAN_POINT ( 'NONE',  ( -18.50000000000000000, 9.250000000011157297, -45.85000000000000142 ) ) ;
#9586 = ORIENTED_EDGE ( 'NONE', *, *, #186080, .F. ) ;
#9587 = DIRECTION ( 'NONE',  ( 0.000000000000000000, -0.1495327102803792052, -0.9887567792719320625 ) ) ;
#9588 = ORIENTED_EDGE ( 'NONE', *, *, #158958, .F. ) ;
#9589 = DIRECTION ( 'NONE',  ( 0.000000000000000000, 0.9875102702516471709, 0.1575546449569757979 ) ) ;
#9590 = ORIENTED_EDGE ( 'NONE', *, *, #12345, .F. ) ;
#9591 = ADVANCED_FACE ( 'NONE', ( #16352 ), #31524, .T. ) ;
#9592 = DIRECTION ( 'NONE',  ( 0.000000000000000000, 0.000000000000000000, -1.000000000000000000 ) ) ;
#9594 = EDGE_CURVE ( 'NONE', #55978, #251464, #257992, .T. ) ;
#9593 = CARTESIAN_POINT ( 'NONE',  ( -23.15000000000000213, 11.31726856452598184, -246.8669175193824969 ) ) ;
#9595 = VECTOR ( 'NONE', #206965, 1000.000000000000000 ) ;
#9596 = AXIS2_PLACEMENT_3D ( 'NONE', #211519, #53720, #14622 ) ;
#9597 = FACE_OUTER_BOUND ( 'NONE', #178134, .T. ) ;
#9598 = VERTEX_POINT ( 'NONE', #232832 ) ;
#9599 = EDGE_CURVE ( 'NONE', #207350, #138366, #73761, .T. ) ;
#9600 = EDGE_CURVE ( 'NONE', #8831, #166820, #83226, .T. ) ;
#9601 = AXIS2_PLACEMENT_3D ( 'NONE', #52207, #110911, #48366 ) ;
#9602 = DIRECTION ( 'NONE',  ( -0.000000000000000000, -1.000000000000000000, -5.421010862427649374E-16 ) ) ;
#9603 = AXIS2_PLACEMENT_3D ( 'NONE', #86969, #11319, #205648 ) ;
#9604 = ADVANCED_FACE ( 'NONE', ( #196240 ), #29142, .T. ) ;
#9605 = DIRECTION ( 'NONE',  ( 0.000000000000000000, 0.000000000000000000, -1.000000000000000000 ) ) ;
#9606 = CIRCLE ( 'NONE', #209518, 0.1000000000000060701 ) ;
#9607 = AXIS2_PLACEMENT_3D ( 'NONE', #221425, #19412, #24560 ) ;
#9608 = FACE_OUTER_BOUND ( 'NONE', #138982, .T. ) ;
#9609 = DIRECTION ( 'NONE',  ( -0.000000000000000000, 0.4721928772777345684, 0.8814952561688429444 ) ) ;
#9610 = ADVANCED_FACE ( 'NONE', ( #54162 ), #17593, .F. ) ;
#9612 = ADVANCED_FACE ( 'NONE', ( #117996 ), #114135, .F. ) ;
#9611 = DIRECTION ( 'NONE',  ( 1.000000000000000000, 0.000000000000000000, 0.000000000000000000 ) ) ;
#9613 = ORIENTED_EDGE ( 'NONE', *, *, #112829, .T. ) ;
#9615 = EDGE_LOOP ( 'NONE', ( #24514, #22576 ) ) ;
#9614 = CARTESIAN_POINT ( 'NONE',  ( 20.94983749550516450, 10.29766095125292402, -105.9743663933276139 ) ) ;
#9616 = VECTOR ( 'NONE', #61976, 1000.000000000000000 ) ;
#9617 = ORIENTED_EDGE ( 'NONE', *, *, #5024, .F. ) ;
#9618 = CARTESIAN_POINT ( 'NONE',  ( -23.25000000000000000, 1.115600667400684642E-11, -167.5000000000000284 ) ) ;
#9619 = ORIENTED_EDGE ( 'NONE', *, *, #125816, .T. ) ;
#9620 = CARTESIAN_POINT ( 'NONE',  ( -16.87435696428308063, 66.04999753708037247, -190.8731157193578554 ) ) ;
#9621 = CARTESIAN_POINT ( 'NONE',  ( 21.05000000000005400, 84.00000000001119815, -34.86056257560453986 ) ) ;
#9622 = EDGE_CURVE ( 'NONE', #110439, #230693, #33226, .T. ) ;
#9623 = CARTESIAN_POINT ( 'NONE',  ( -23.25000000000000000, 64.25000000001246292, -181.7731074845244450 ) ) ;
#9624 = ORIENTED_EDGE ( 'NONE', *, *, #169884, .F. ) ;
#9625 = CARTESIAN_POINT ( 'NONE',  ( -23.25000000000000355, 11.74999999999998224, -24.25000000000000000 ) ) ;
#9626 = CARTESIAN_POINT ( 'NONE',  ( 23.14999999999999147, 76.00000000001213607, -136.5231074845242745 ) ) ;
#9628 = DIRECTION ( 'NONE',  ( -0.000000000000000000, 1.000000000000000000, -0.000000000000000000 ) ) ;
#9627 = AXIS2_PLACEMENT_3D ( 'NONE', #83593, #141050, #198439 ) ;
#9629 = ORIENTED_EDGE ( 'NONE', *, *, #93887, .T. ) ;
#9630 = CIRCLE ( 'NONE', #17994, 0.2000000000000057288 ) ;
#9631 = EDGE_CURVE ( 'NONE', #11797, #189027, #78846, .T. ) ;
#9633 = ORIENTED_EDGE ( 'NONE', *, *, #3443, .T. ) ;
#9632 = CARTESIAN_POINT ( 'NONE',  ( -18.59999999999999787, -10.80884033489985363, 6.000000000000001776 ) ) ;
#9634 = CARTESIAN_POINT ( 'NONE',  ( -20.64999999999999858, 76.00000000001142553, -36.02310748452432421 ) ) ;
#9635 = DIRECTION ( 'NONE',  ( -1.020425574104004196E-15, 0.000000000000000000, -1.000000000000000000 ) ) ;
#9636 = TOROIDAL_SURFACE ( 'NONE', #109391, 6.258578643762712446, 0.1000000000000000056 ) ;
#9637 = EDGE_CURVE ( 'NONE', #143490, #186471, #124962, .T. ) ;
#9638 = ADVANCED_FACE ( 'NONE', ( #198810 ), #12542, .T. ) ;
#9639 = AXIS2_PLACEMENT_3D ( 'NONE', #97579, #38940, #256629 ) ;
#9640 = EDGE_LOOP ( 'NONE', ( #20436, #12534, #197916 ) ) ;
#9641 = AXIS2_PLACEMENT_3D ( 'NONE', #87517, #154917, #194037 ) ;
#9642 = AXIS2_PLACEMENT_3D ( 'NONE', #118101, #131576, #78943 ) ;
#9643 = DIRECTION ( 'NONE',  ( 0.7071067811865487940, 8.659560562354918067E-17, 0.7071067811865463515 ) ) ;
#9645 = ADVANCED_FACE ( 'NONE', ( #24054 ), #143967, .T. ) ;
#9644 = CARTESIAN_POINT ( 'NONE',  ( -18.44085059012131822, 40.40203773622608452, -235.2576840484422291 ) ) ;
#9646 = CIRCLE ( 'NONE', #38690, 0.1000000000000043771 ) ;
#9647 = DIRECTION ( 'NONE',  ( -1.000000000000000000, 0.000000000000000000, 0.000000000000000000 ) ) ;
#9648 = VERTEX_POINT ( 'NONE', #99685 ) ;
#9649 = LINE ( 'NONE', #187030, #117444 ) ;
#9650 = EDGE_CURVE ( 'NONE', #177551, #85751, #43602, .T. ) ;
#9651 = CARTESIAN_POINT ( 'NONE',  ( -20.54999999999999716, -11.74999999998884448, -83.75000000000004263 ) ) ;
#9652 = ADVANCED_FACE ( 'NONE', ( #257444 ), #159701, .F. ) ;
#9653 = EDGE_LOOP ( 'NONE', ( #183980, #91049, #165239, #27522, #210826, #235871, #71280, #170038, #172026, #238677, #31658, #148322 ) ) ;
#9654 = CIRCLE ( 'NONE', #126158, 0.09999999999999939493 ) ;
#9655 = AXIS2_PLACEMENT_3D ( 'NONE', #229032, #29571, #33429 ) ;
#9656 = AXIS2_PLACEMENT_3D ( 'NONE', #94681, #193797, #112978 ) ;
#9657 = CIRCLE ( 'NONE', #130273, 0.1000000000000002554 ) ;
#9658 = ORIENTED_EDGE ( 'NONE', *, *, #249757, .T. ) ;
#9659 = DIRECTION ( 'NONE',  ( 2.952720810173289112E-16, 1.000000000000000000, 6.982962677686266711E-15 ) ) ;
#9660 = VERTEX_POINT ( 'NONE', #219651 ) ;
#9661 = CARTESIAN_POINT ( 'NONE',  ( 22.47071067811865319, 68.27992525551410097, -136.6221999392269595 ) ) ;
#9662 = DIRECTION ( 'NONE',  ( 0.000000000000000000, -1.000000000000000000, -6.982962677686266711E-15 ) ) ;
#9664 = VERTEX_POINT ( 'NONE', #177985 ) ;
#9663 = CARTESIAN_POINT ( 'NONE',  ( 13.12220780326571834, 25.00864058361856834, -232.6119739634631287 ) ) ;
#9665 = CARTESIAN_POINT ( 'NONE',  ( 20.94999999999999929, 11.63687328911503727, -127.1782407866755307 ) ) ;
#9666 = DIRECTION ( 'NONE',  ( -3.265361837132813586E-16, 0.4721928772777345129, 0.8814952561688430555 ) ) ;
#9667 = DIRECTION ( 'NONE',  ( 0.000000000000000000, -0.7092521942343974484, -0.7049548389604062271 ) ) ;
#9668 = CARTESIAN_POINT ( 'NONE',  ( 22.47071067811865319, 29.57301391503007082, -252.6169816238249552 ) ) ;
#9669 = CARTESIAN_POINT ( 'NONE',  ( 18.59999999999999787, 1.115600667400684642E-11, -167.4999999999999716 ) ) ;
#9670 = CARTESIAN_POINT ( 'NONE',  ( -16.93388492042258875, 9.988541822527059466, -79.59945487681387988 ) ) ;
#9671 = DIRECTION ( 'NONE',  ( 0.000000000000000000, 0.000000000000000000, 1.000000000000000000 ) ) ;
#9673 = ORIENTED_EDGE ( 'NONE', *, *, #129870, .T. ) ;
#9672 = DIRECTION ( 'NONE',  ( 1.000000000000000000, -3.265361837132813093E-16, -2.280189983783949500E-30 ) ) ;
#9674 = CARTESIAN_POINT ( 'NONE',  ( 21.05000000000000071, 22.90266353732884852, -230.0169390150674076 ) ) ;
#9675 = CARTESIAN_POINT ( 'NONE',  ( 20.85000000000000142, 18.51199663233068193, -231.2535697180530292 ) ) ;
#9676 = CIRCLE ( 'NONE', #226127, 0.09999999999999892308 ) ;
#9677 = FACE_OUTER_BOUND ( 'NONE', #96, .T. ) ;
#9678 = CARTESIAN_POINT ( 'NONE',  ( 20.21567752745066215, 65.80188589878065386, -195.6404871368698082 ) ) ;
#9679 = FACE_OUTER_BOUND ( 'NONE', #185751, .T. ) ;
#9680 = VERTEX_POINT ( 'NONE', #82683 ) ;
#9681 = CARTESIAN_POINT ( 'NONE',  ( 21.05000000000000426, 10.05455514295651653, -228.1997025080316348 ) ) ;
#9682 = EDGE_CURVE ( 'NONE', #112295, #72558, #162279, .T. ) ;
#9683 = DIRECTION ( 'NONE',  ( 0.000000000000000000, 0.9126074666063660468, 0.4088369013363524762 ) ) ;
#9684 = EDGE_CURVE ( 'NONE', #219800, #150376, #140106, .T. ) ;
#9685 = EDGE_LOOP ( 'NONE', ( #49606, #141905, #236382, #237881 ) ) ;
#9686 = VECTOR ( 'NONE', #135382, 1000.000000000000000 ) ;
#9687 = CARTESIAN_POINT ( 'NONE',  ( 21.07954640115206857, 75.93399229287285834, -209.8523951805472620 ) ) ;
#9688 = CIRCLE ( 'NONE', #63869, 0.1000000000000013933 ) ;
#9689 = CARTESIAN_POINT ( 'NONE',  ( 23.24999999999999645, 11.75000000001113953, -143.2500000000000284 ) ) ;
#9690 = ADVANCED_FACE ( 'NONE', ( #179284 ), #66510, .F. ) ;
#9691 = ORIENTED_EDGE ( 'NONE', *, *, #115004, .T. ) ;
#9693 = EDGE_CURVE ( 'NONE', #17664, #122621, #141505, .T. ) ;
#9692 = DIRECTION ( 'NONE',  ( 0.000000000000000000, 0.1350103645451904977, -0.9908441862701596881 ) ) ;
#9694 = ORIENTED_EDGE ( 'NONE', *, *, #126812, .T. ) ;
#9695 = LINE ( 'NONE', #248314, #17435 ) ;
#9696 = VERTEX_POINT ( 'NONE', #142670 ) ;
#9697 = DIRECTION ( 'NONE',  ( -1.000000000000000000, -0.000000000000000000, -0.000000000000000000 ) ) ;
#9698 = DIRECTION ( 'NONE',  ( -0.000000000000000000, 0.9579639084728132081, 0.2868887416116073230 ) ) ;
#9699 = ORIENTED_EDGE ( 'NONE', *, *, #47874, .T. ) ;
#9700 = VERTEX_POINT ( 'NONE', #200106 ) ;
#9702 = DIRECTION ( 'NONE',  ( -1.000000000000000000, -0.000000000000000000, -0.000000000000000000 ) ) ;
#9701 = CIRCLE ( 'NONE', #255355, 0.1000000000000064448 ) ;
#9704 = EDGE_LOOP ( 'NONE', ( #36339, #163113 ) ) ;
#9703 = CARTESIAN_POINT ( 'NONE',  ( 14.56326696814971555, 9.446648990640015953, -48.58916329592317851 ) ) ;
#9705 = CARTESIAN_POINT ( 'NONE',  ( 20.85882249326303040, 65.66751761918648356, -63.92826094061123143 ) ) ;
#9706 = EDGE_LOOP ( 'NONE', ( #59840, #126281, #162537, #166902 ) ) ;
#9707 = CIRCLE ( 'NONE', #192889, 0.5000000000000004441 ) ;
#9708 = EDGE_CURVE ( 'NONE', #57757, #248466, #225787, .T. ) ;
#9709 = CIRCLE ( 'NONE', #142970, 0.09999999999999609201 ) ;
#9710 = VERTEX_POINT ( 'NONE', #59256 ) ;
#9711 = FACE_OUTER_BOUND ( 'NONE', #223953, .T. ) ;
#9712 = CARTESIAN_POINT ( 'NONE',  ( -20.54999999999999716, 68.75000000001260503, -191.2731074845244166 ) ) ;
#9713 = DIRECTION ( 'NONE',  ( 2.694716079187272946E-16, -1.000000000000000000, 0.000000000000000000 ) ) ;
#9714 = CARTESIAN_POINT ( 'NONE',  ( -20.64999999999999858, 4.350000000011156054, -146.3500000000000227 ) ) ;
#9715 = DIRECTION ( 'NONE',  ( 0.000000000000000000, -0.1568667991644863147, 0.9876197685951252359 ) ) ;
#9716 = DIRECTION ( 'NONE',  ( 0.000000000000000000, 0.000000000000000000, -1.000000000000000000 ) ) ;
#9717 = AXIS2_PLACEMENT_3D ( 'NONE', #174387, #22996, #82899 ) ;
#9718 = VERTEX_POINT ( 'NONE', #163543 ) ;
#9719 = DIRECTION ( 'NONE',  ( 0.000000000000000000, 1.000000000000000000, 2.891205793294679805E-16 ) ) ;
#9721 = EDGE_CURVE ( 'NONE', #173891, #186873, #183214, .T. ) ;
#9720 = DIRECTION ( 'NONE',  ( -0.000000000000000000, -2.891205793294679805E-16, 1.000000000000000000 ) ) ;
#9722 = CARTESIAN_POINT ( 'NONE',  ( 20.95346350065193519, 67.11282275083759430, -128.0113755374889877 ) ) ;
#9723 = CIRCLE ( 'NONE', #30605, 0.1000000000000028644 ) ;
#9724 = DIRECTION ( 'NONE',  ( 0.000000000000000000, 0.9126074666063772600, 0.4088369013363274407 ) ) ;
#9725 = ORIENTED_EDGE ( 'NONE', *, *, #89843, .F. ) ;
#9726 = EDGE_CURVE ( 'NONE', #34898, #137137, #62421, .T. ) ;
#9727 = CARTESIAN_POINT ( 'NONE',  ( 18.59999999999996945, 10.33248238083634440, -106.0948465439131922 ) ) ;
#9728 = VERTEX_POINT ( 'NONE', #83954 ) ;
#9729 = LINE ( 'NONE', #89263, #19195 ) ;
#9730 = ORIENTED_EDGE ( 'NONE', *, *, #18824, .T. ) ;
#9731 = CARTESIAN_POINT ( 'NONE',  ( -14.45443560709635733, 24.86329420051411532, -232.5114740807002534 ) ) ;
#9732 = CARTESIAN_POINT ( 'NONE',  ( -22.94999999999999929, 11.61130914238355771, -1.800000000000000044 ) ) ;
#9734 = ORIENTED_EDGE ( 'NONE', *, *, #47147, .T. ) ;
#9733 = AXIS2_PLACEMENT_3D ( 'NONE', #11114, #94484, #253554 ) ;
#9735 = VERTEX_POINT ( 'NONE', #29219 ) ;
#9737 = ORIENTED_EDGE ( 'NONE', *, *, #197200, .T. ) ;
#9736 = PLANE ( 'NONE',  #69833 ) ;
#9738 = CYLINDRICAL_SURFACE ( 'NONE', #229721, 0.09999999999999939493 ) ;
#9739 = ORIENTED_EDGE ( 'NONE', *, *, #212869, .F. ) ;
#9740 = EDGE_CURVE ( 'NONE', #132362, #141820, #70817, .T. ) ;
#9741 = CARTESIAN_POINT ( 'NONE',  ( -2.995603634470829482E-16, 53.33306769324366314, -234.7945388949160872 ) ) ;
#9742 = AXIS2_PLACEMENT_3D ( 'NONE', #153970, #155240, #230911 ) ;
#9743 = AXIS2_PLACEMENT_3D ( 'NONE', #171070, #194464, #193170 ) ;
#9744 = VECTOR ( 'NONE', #119027, 1000.000000000000000 ) ;
#9745 = FILL_AREA_STYLE ('',( #89275 ) ) ;
#9746 = ADVANCED_FACE ( 'NONE', ( #189542 ), #10903, .T. ) ;
#9747 = CIRCLE ( 'NONE', #43084, 0.09999999999999738265 ) ;
#9748 = ORIENTED_EDGE ( 'NONE', *, *, #249884, .F. ) ;
#9749 = CARTESIAN_POINT ( 'NONE',  ( 20.94999999999999929, -11.64999999998883595, -66.99999999999998579 ) ) ;
#9750 = CARTESIAN_POINT ( 'NONE',  ( 19.90000000000000568, 1.350000000000000089, 21.90000000000000213 ) ) ;
#9751 = ADVANCED_FACE ( 'NONE', ( #108711 ), #20930, .T. ) ;
#9752 = ORIENTED_EDGE ( 'NONE', *, *, #133818, .F. ) ;
#9753 = DIRECTION ( 'NONE',  ( 0.000000000000000000, 1.000000000000000000, 0.000000000000000000 ) ) ;
#9754 = FACE_OUTER_BOUND ( 'NONE', #156684, .T. ) ;
#9755 = EDGE_CURVE ( 'NONE', #128122, #12130, #141691, .T. ) ;
#9756 = DIRECTION ( 'NONE',  ( 0.000000000000000000, 0.000000000000000000, -1.000000000000000000 ) ) ;
#9758 = VERTEX_POINT ( 'NONE', #249516 ) ;
#9757 = CARTESIAN_POINT ( 'NONE',  ( 20.94999999999999929, 5.000000000011153745, -121.5947339810869465 ) ) ;
#9759 = DIRECTION ( 'NONE',  ( 0.000000000000000000, 0.07893460099012014619, -0.9968797965484758050 ) ) ;
#9760 = DIRECTION ( 'NONE',  ( 0.000000000000000000, 0.2128009952263485993, -0.9770955615653341697 ) ) ;
#9761 = CARTESIAN_POINT ( 'NONE',  ( 16.87683809663750267, 9.950000000011138823, -180.1499999999999773 ) ) ;
#9762 = ADVANCED_FACE ( 'NONE', ( #89139 ), #184378, .T. ) ;
#9763 = VECTOR ( 'NONE', #303, 1000.000000000000114 ) ;
#9765 = CARTESIAN_POINT ( 'NONE',  ( 19.75857864376268935, 64.25000000001220712, -145.1731074845244507 ) ) ;
#9764 = DIRECTION ( 'NONE',  ( -1.000000000000000000, 0.000000000000000000, 0.000000000000000000 ) ) ;
#9766 = CARTESIAN_POINT ( 'NONE',  ( -18.50000000000000000, 66.85000000001205933, -124.1731074845243512 ) ) ;
#9767 = DIRECTION ( 'NONE',  ( 0.000000000000000000, 0.9998779222360096863, -0.01562500000001061998 ) ) ;
#9768 = TOROIDAL_SURFACE ( 'NONE', #218044, 11.65000000000000036, 0.1000000000000000056 ) ;
#9769 = LINE ( 'NONE', #149310, #243214 ) ;
#9771 = DIRECTION ( 'NONE',  ( -1.000000000000000000, 0.000000000000000000, 0.000000000000000000 ) ) ;
#9770 = AXIS2_PLACEMENT_3D ( 'NONE', #17027, #195677, #41729 ) ;
#9772 = ORIENTED_EDGE ( 'NONE', *, *, #183432, .F. ) ;
#9773 = CIRCLE ( 'NONE', #155576, 0.09999999999998898659 ) ;
#9774 = EDGE_LOOP ( 'NONE', ( #117510, #3401, #180048 ) ) ;
#9775 = ORIENTED_EDGE ( 'NONE', *, *, #197486, .F. ) ;
#9776 =( BOUNDED_SURFACE ( )  B_SPLINE_SURFACE ( 3, 2, ( 
 ( #19100, #37407, #179487 ),
 ( #98598, #114362, #238142 ),
 ( #116927, #17809, #157371 ),
 ( #257649, #137750, #58210 ),
 ( #97321, #213453, #195209 ),
 ( #178211, #218571, #38676 ),
 ( #176928, #118210, #236863 ),
 ( #77777, #39987, #96061 ),
 ( #174383, #793, #175635 ),
 ( #79050, #253850, #156088 ) ),
 .UNSPECIFIED., .F., .F., .F. ) 
 B_SPLINE_SURFACE_WITH_KNOTS ( ( 4, 2, 2, 2, 4 ),
 ( 3, 3 ),
 ( 0.002161241639767792072, 0.002579950749617451571, 0.002789305304542281753, 0.002893982582004696845, 0.002998659859467111503 ),
 ( 0.000000000000000000, 1.000000000000000000 ),
 .UNSPECIFIED. ) 
 GEOMETRIC_REPRESENTATION_ITEM ( )  RATIONAL_B_SPLINE_SURFACE ( (
 ( 1.000000000000000000, 0.7071067811864923947, 1.000000000000000000),
 ( 1.000000000000000000, 0.7632447400663602277, 1.000000000000000000),
 ( 1.000000000000000000, 0.8158073005109875986, 1.000000000000000000),
 ( 1.000000000000000000, 0.8906973462395570973, 1.000000000000000000),
 ( 1.000000000000000000, 0.9149408947799901881, 1.000000000000000000),
 ( 1.000000000000000000, 0.9493368785275747568, 1.000000000000000000),
 ( 1.000000000000000000, 0.9605194247156804144, 1.000000000000000000),
 ( 1.000000000000000000, 0.9803630264780990311, 1.000000000000000000),
 ( 1.000000000000000000, 0.9900844824271254341, 1.000000000000000000),
 ( 1.000000000000000000, 0.9894588281429296250, 1.000000000000000000) ) ) 
 REPRESENTATION_ITEM ( '' )  SURFACE ( )  );
#9777 = DIRECTION ( 'NONE',  ( 0.000000000000000000, 0.000000000000000000, -1.000000000000000000 ) ) ;
#9778 = TOROIDAL_SURFACE ( 'NONE', #34762, 4.149999999999999467, 0.1000000000000000056 ) ;
#9779 = CARTESIAN_POINT ( 'NONE',  ( 20.95512820512820440, 65.37615131630045084, -162.3581939154368285 ) ) ;
#9780 = B_SPLINE_CURVE_WITH_KNOTS ( 'NONE', 3,
 ( #74471, #233524, #95276, #135670, #215227, #167783 ),
 .UNSPECIFIED., .F., .F.,
 ( 4, 2, 4 ),
 ( 0.000000000000000000, 0.0001891491689349690151, 0.0003782983378699380302 ),
 .UNSPECIFIED. ) ;
#9781 = ORIENTED_EDGE ( 'NONE', *, *, #163943, .T. ) ;
#9782 = CIRCLE ( 'NONE', #168063, 0.1000000000000052097 ) ;
#9784 = AXIS2_PLACEMENT_3D ( 'NONE', #95411, #255723, #116276 ) ;
#9783 =( NAMED_UNIT ( * ) PLANE_ANGLE_UNIT ( ) SI_UNIT ( $, .RADIAN. ) );
#9785 = CARTESIAN_POINT ( 'NONE',  ( -22.50000000000000000, 0.09999999999999939493, 11.64957080754479968 ) ) ;
#9786 = AXIS2_PLACEMENT_3D ( 'NONE', #40422, #44246, #101598 ) ;
#9787 = CARTESIAN_POINT ( 'NONE',  ( -21.05000000000000071, 76.00000000001267608, -203.5231074845243597 ) ) ;
#9788 = AXIS2_PLACEMENT_3D ( 'NONE', #87704, #229798, #90271 ) ;
#9789 = PRODUCT_DEFINITION_SHAPE ( 'NONE', 'NONE',  #160032 ) ;
#9790 = DIRECTION ( 'NONE',  ( -0.000000000000000000, 0.9770955615653313941, 0.2128009952263603954 ) ) ;
#9791 = VERTEX_POINT ( 'NONE', #26626 ) ;
#9792 = ORIENTED_EDGE ( 'NONE', *, *, #21908, .F. ) ;
#9793 = CIRCLE ( 'NONE', #180501, 0.09999999999999939493 ) ;
#9794 = DIRECTION ( 'NONE',  ( -1.020425574104004394E-15, -0.9126074666063770380, -0.4088369013363281068 ) ) ;
#9795 = DIRECTION ( 'NONE',  ( 0.000000000000000000, 0.000000000000000000, -1.000000000000000000 ) ) ;
#9796 = ORIENTED_EDGE ( 'NONE', *, *, #136240, .F. ) ;
#9797 = CARTESIAN_POINT ( 'NONE',  ( -18.34374000495060386, 64.52683809664912928, -60.27310748452440947 ) ) ;
#9798 = ORIENTED_EDGE ( 'NONE', *, *, #74787, .T. ) ;
#9799 = DIRECTION ( 'NONE',  ( 1.000000000000000000, 0.000000000000000000, 0.000000000000000000 ) ) ;
#9800 = DIRECTION ( 'NONE',  ( 1.000000000000000000, 0.000000000000000000, 0.000000000000000000 ) ) ;
#9801 = AXIS2_PLACEMENT_3D ( 'NONE', #71795, #168355, #7962 ) ;
#9803 = VERTEX_POINT ( 'NONE', #185679 ) ;
#9802 = CARTESIAN_POINT ( 'NONE',  ( -23.15000000000000213, 70.10000000001149090, -46.24220724918073699 ) ) ;
#9804 =( LENGTH_UNIT ( ) NAMED_UNIT ( * ) SI_UNIT ( .MILLI., .METRE. ) );
#9805 = CARTESIAN_POINT ( 'NONE',  ( 21.05000000000000071, 64.25000000001219291, -143.5379132551783812 ) ) ;
#9806 = DIRECTION ( 'NONE',  ( 1.000000000000000000, 0.000000000000000000, 0.000000000000000000 ) ) ;
#9807 = CARTESIAN_POINT ( 'NONE',  ( 21.05000000000000071, 14.80592234317787081, -236.3146577222204314 ) ) ;
#9808 = CIRCLE ( 'NONE', #47208, 0.1000000000000014488 ) ;
#9810 = CYLINDRICAL_SURFACE ( 'NONE', #145737, 0.09999999999999939493 ) ;
#9809 = DIRECTION ( 'NONE',  ( 0.000000000000000000, -0.9916376685811618685, 0.1290532225514649800 ) ) ;
#9811 = DIRECTION ( 'NONE',  ( 0.000000000000000000, 0.000000000000000000, -1.000000000000000000 ) ) ;
#9812 = FACE_OUTER_BOUND ( 'NONE', #109630, .T. ) ;
#9813 = DIRECTION ( 'NONE',  ( -3.469446951953635015E-14, 1.000000000000000000, 0.000000000000000000 ) ) ;
#9814 = DIRECTION ( 'NONE',  ( 0.000000000000000000, 1.000000000000000000, 3.662759245464225434E-15 ) ) ;
#9816 = ORIENTED_EDGE ( 'NONE', *, *, #114847, .F. ) ;
#9815 = TOROIDAL_SURFACE ( 'NONE', #155614, 11.65000000000000036, 0.1000000000000000056 ) ;
#9817 =( BOUNDED_CURVE ( )  B_SPLINE_CURVE ( 3, ( #226244, #5918, #104994, #163743 ),
 .UNSPECIFIED., .F., .F. ) 
 B_SPLINE_CURVE_WITH_KNOTS ( ( 4, 4 ),
 ( 0.000000000000000000, 1.570796326794908992 ),
 .UNSPECIFIED. ) 
 CURVE ( )  GEOMETRIC_REPRESENTATION_ITEM ( )  RATIONAL_B_SPLINE_CURVE ( ( 1.000000000000000000, 0.8047378541243619399, 0.8047378541243619399, 1.000000000000000000 ) ) 
 REPRESENTATION_ITEM ( '' )  );
#9819 = ORIENTED_EDGE ( 'NONE', *, *, #220508, .F. ) ;
#9818 = AXIS2_PLACEMENT_3D ( 'NONE', #74855, #59068, #38269 ) ;
#9820 = CYLINDRICAL_SURFACE ( 'NONE', #9733, 0.09999999999999641120 ) ;
#9821 = AXIS2_PLACEMENT_3D ( 'NONE', #53195, #14088, #74079 ) ;
#9822 = ORIENTED_EDGE ( 'NONE', *, *, #97299, .F. ) ;
#9823 = DIRECTION ( 'NONE',  ( 0.000000000000000000, -1.000000000000000000, 0.000000000000000000 ) ) ;
#9824 = ORIENTED_EDGE ( 'NONE', *, *, #106138, .T. ) ;
#9825 = DIRECTION ( 'NONE',  ( 0.000000000000000000, -0.8660254037844343777, 0.5000000000000074385 ) ) ;
#9826 = ADVANCED_FACE ( 'NONE', ( #150425 ), #229939, .T. ) ;
#9827 = DIRECTION ( 'NONE',  ( 0.000000000000000000, 0.8814952561688437216, -0.4721928772777334582 ) ) ;
#9828 = ADVANCED_FACE ( 'NONE', ( #125697 ), #126985, .T. ) ;
#9829 = ADVANCED_FACE ( 'NONE', ( #166152 ), #205217, .T. ) ;
#9830 = VERTEX_POINT ( 'NONE', #8339 ) ;
#9831 = FACE_OUTER_BOUND ( 'NONE', #34091, .T. ) ;
#9832 = CIRCLE ( 'NONE', #222196, 0.1000000000000028644 ) ;
#9833 = VECTOR ( 'NONE', #220998, 1000.000000000000000 ) ;
#9834 = ORIENTED_EDGE ( 'NONE', *, *, #1964, .T. ) ;
#9835 = VECTOR ( 'NONE', #51367, 1000.000000000000114 ) ;
#9837 = VERTEX_POINT ( 'NONE', #246919 ) ;
#9836 = TOROIDAL_SURFACE ( 'NONE', #147213, 0.2000000000000000111, 0.1000000000000000056 ) ;
#9838 = ORIENTED_EDGE ( 'NONE', *, *, #147461, .F. ) ;
#9839 = FACE_OUTER_BOUND ( 'NONE', #98438, .T. ) ;
#9840 = CARTESIAN_POINT ( 'NONE',  ( -18.59999999999999787, 74.93036000061670165, -233.6816308724374949 ) ) ;
#9841 = CARTESIAN_POINT ( 'NONE',  ( 13.12229106158773639, 27.68529808098226752, -234.0457819887454320 ) ) ;
#9842 = CARTESIAN_POINT ( 'NONE',  ( -18.59999999999999787, 77.85102823015243700, -57.86919421510181394 ) ) ;
#9843 = EDGE_CURVE ( 'NONE', #225728, #130099, #191622, .T. ) ;
#9845 = PLANE ( 'NONE',  #86860 ) ;
#9844 = DIRECTION ( 'NONE',  ( 0.000000000000000000, 7.109473446599835262E-15, -1.000000000000000000 ) ) ;
#9846 = CARTESIAN_POINT ( 'NONE',  ( 18.59999999999997655, 43.62273694548321856, -253.2814864317374770 ) ) ;
#9848 = ORIENTED_EDGE ( 'NONE', *, *, #230354, .F. ) ;
#9847 = DIRECTION ( 'NONE',  ( -1.000000000000000000, 0.000000000000000000, -0.000000000000000000 ) ) ;
#9850 = DIRECTION ( 'NONE',  ( 0.000000000000000000, 0.9856811345164803173, 0.1686199900910455851 ) ) ;
#9849 = CARTESIAN_POINT ( 'NONE',  ( -22.50000000000000000, 65.09550114356427741, -243.3481044654562879 ) ) ;
#9851 = DIRECTION ( 'NONE',  ( 0.000000000000000000, 0.8814952561688429444, -0.4721928772777347350 ) ) ;
#9852 = ORIENTED_EDGE ( 'NONE', *, *, #190425, .F. ) ;
#9853 = FACE_OUTER_BOUND ( 'NONE', #4925, .T. ) ;
#9854 = DIRECTION ( 'NONE',  ( 0.000000000000000000, 0.000000000000000000, -1.000000000000000000 ) ) ;
#9855 = SPHERICAL_SURFACE ( 'NONE', #149849, 0.1000000000000000056 ) ;
#9856 = ORIENTED_EDGE ( 'NONE', *, *, #170160, .F. ) ;
#9857 = LINE ( 'NONE', #172837, #95288 ) ;
#9858 = DIRECTION ( 'NONE',  ( -7.304098846218135653E-16, 0.9651348961777157509, -0.2617529984165031243 ) ) ;
#9859 = CARTESIAN_POINT ( 'NONE',  ( 13.22261339317535978, 66.56344716000741357, -87.84515201176407118 ) ) ;
#9860 = EDGE_LOOP ( 'NONE', ( #137346, #244851, #139743, #56344 ) ) ;
#9861 = VERTEX_POINT ( 'NONE', #67011 ) ;
#9862 = CIRCLE ( 'NONE', #243090, 0.09999999999998898659 ) ;
#9863 = LINE ( 'NONE', #46412, #182506 ) ;
#9864 = EDGE_CURVE ( 'NONE', #213961, #192664, #195889, .T. ) ;
#9865 = ADVANCED_FACE ( 'NONE', ( #226047 ), #210387, .F. ) ;
#9866 = CARTESIAN_POINT ( 'NONE',  ( 20.94999999999999929, 46.45388641681647357, -243.1520440498138385 ) ) ;
#9867 = CARTESIAN_POINT ( 'NONE',  ( -20.65000000000000568, 70.35000000001207354, -123.8731074845243398 ) ) ;
#9868 = CARTESIAN_POINT ( 'NONE',  ( -20.93975676684922504, 10.31104185824063002, -206.5204516983105236 ) ) ;
#9869 = VERTEX_POINT ( 'NONE', #209090 ) ;
#9870 = DIRECTION ( 'NONE',  ( 1.000000000000000000, 0.000000000000000000, 0.000000000000000000 ) ) ;
#9871 = FACE_OUTER_BOUND ( 'NONE', #123509, .T. ) ;
#9872 = ADVANCED_FACE ( 'NONE', ( #87833 ), #43, .F. ) ;
#9873 = FACE_OUTER_BOUND ( 'NONE', #132751, .T. ) ;
#9874 = DIRECTION ( 'NONE',  ( -1.000000000000000000, 0.000000000000000000, 0.000000000000000000 ) ) ;
#9876 = ORIENTED_EDGE ( 'NONE', *, *, #164398, .T. ) ;
#9875 = CIRCLE ( 'NONE', #110019, 11.74999999999999822 ) ;
#9877 = DIRECTION ( 'NONE',  ( -0.000000000000000000, 0.8814952561688430555, -0.4721928772777346239 ) ) ;
#9878 = AXIS2_PLACEMENT_3D ( 'NONE', #176923, #76496, #60780 ) ;
#9880 = ORIENTED_EDGE ( 'NONE', *, *, #43647, .T. ) ;
#9879 = LINE ( 'NONE', #103826, #200227 ) ;
#9881 = CARTESIAN_POINT ( 'NONE',  ( 23.25000000000000000, 87.65000000001195701, -103.0231074845242318 ) ) ;
#9882 = CARTESIAN_POINT ( 'NONE',  ( 18.49999999999999289, 43.35377423437995503, -245.1717807829448930 ) ) ;
#9883 = CARTESIAN_POINT ( 'NONE',  ( 18.59999999999999787, 60.94692742449272771, -251.5456325903398067 ) ) ;
#9884 = DIRECTION ( 'NONE',  ( 1.000000000000000000, 0.000000000000000000, 0.000000000000000000 ) ) ;
#9885 = CARTESIAN_POINT ( 'NONE',  ( -15.75000000000000355, 66.65000000001258229, -186.7731074845243882 ) ) ;
#9886 = ORIENTED_EDGE ( 'NONE', *, *, #46404, .F. ) ;
#9887 = EDGE_CURVE ( 'NONE', #36999, #102833, #212447, .T. ) ;
#9888 = FACE_OUTER_BOUND ( 'NONE', #185101, .T. ) ;
#9889 = CARTESIAN_POINT ( 'NONE',  ( -18.40000000000000213, 20.94763808724815846, -234.7254930126486556 ) ) ;
#9890 = DIRECTION ( 'NONE',  ( 1.000000000000000000, 0.000000000000000000, 0.000000000000000000 ) ) ;
#9891 = CARTESIAN_POINT ( 'NONE',  ( 21.87500000000000355, 66.25000000001257661, -191.1731074845244223 ) ) ;
#9892 = AXIS2_PLACEMENT_3D ( 'NONE', #164581, #105851, #201123 ) ;
#9893 = DIRECTION ( 'NONE',  ( 1.000000000000000000, 0.000000000000000000, 0.000000000000000000 ) ) ;
#9894 = CIRCLE ( 'NONE', #226354, 12.87499999999999822 ) ;
#9895 = DIRECTION ( 'NONE',  ( 1.000000000000000000, 0.000000000000000000, 0.000000000000000000 ) ) ;
#9897 = ORIENTED_EDGE ( 'NONE', *, *, #168915, .T. ) ;
#9896 = CIRCLE ( 'NONE', #5776, 0.1000000000000009492 ) ;
#9898 = ORIENTED_EDGE ( 'NONE', *, *, #85489, .T. ) ;
#9900 = CARTESIAN_POINT ( 'NONE',  ( -18.59999999999999787, 61.51025099401670104, -221.6110087929486951 ) ) ;
#9899 = CIRCLE ( 'NONE', #88993, 0.09999999999999939493 ) ;
#9901 = EDGE_CURVE ( 'NONE', #222414, #50332, #241652, .T. ) ;
#9902 = LINE ( 'NONE', #89434, #47405 ) ;
#9904 = EDGE_CURVE ( 'NONE', #58764, #231343, #8428, .T. ) ;
#9903 = DIRECTION ( 'NONE',  ( 1.000000000000000000, 0.000000000000000000, 0.000000000000000000 ) ) ;
#9905 = CARTESIAN_POINT ( 'NONE',  ( -20.94999999999999929, -4.756823075239758225, -233.1486023682345490 ) ) ;
#9906 = ADVANCED_FACE ( 'NONE', ( #92989 ), #212949, .F. ) ;
#9907 = ADVANCED_FACE ( 'NONE', ( #132127 ), #36914, .F. ) ;
#9908 = DIRECTION ( 'NONE',  ( 1.000000000000000000, 0.000000000000000000, 0.000000000000000000 ) ) ;
#9909 = AXIS2_PLACEMENT_3D ( 'NONE', #230148, #256068, #236556 ) ;
#9910 = AXIS2_PLACEMENT_3D ( 'NONE', #40254, #231072, #198002 ) ;
#9911 = CARTESIAN_POINT ( 'NONE',  ( -20.64999999999999858, 11.58468387039766512, -220.1227639117171861 ) ) ;
#9912 = AXIS2_PLACEMENT_3D ( 'NONE', #217765, #39182, #118713 ) ;
#9913 = FACE_OUTER_BOUND ( 'NONE', #111900, .T. ) ;
#9914 = CARTESIAN_POINT ( 'NONE',  ( -18.59999999999999787, 1.115600667400684642E-11, -100.5000000000000426 ) ) ;
#9915 = EDGE_CURVE ( 'NONE', #41586, #55172, #112572, .T. ) ;
#9917 = ADVANCED_FACE ( 'NONE', ( #33075 ), #91713, .F. ) ;
#9916 = ADVANCED_FACE ( 'NONE', ( #190850 ), #134663, .F. ) ;
#9918 = VERTEX_POINT ( 'NONE', #192120 ) ;
#9919 = LINE ( 'NONE', #185993, #23718 ) ;
#9920 = AXIS2_PLACEMENT_3D ( 'NONE', #86011, #165603, #245125 ) ;
#9921 = ORIENTED_EDGE ( 'NONE', *, *, #177886, .T. ) ;
#9922 = DIRECTION ( 'NONE',  ( 0.000000000000000000, 0.000000000000000000, -1.000000000000000000 ) ) ;
#9923 = LINE ( 'NONE', #71204, #78981 ) ;
#9925 = ADVANCED_FACE ( 'NONE', ( #253345 ), #151722, .F. ) ;
#9924 = CARTESIAN_POINT ( 'NONE',  ( 20.94999999999999929, -9.399999999988846611, -43.39396912265245021 ) ) ;
#9927 = VECTOR ( 'NONE', #220425, 1000.000000000000000 ) ;
#9926 = DIRECTION ( 'NONE',  ( 1.000000000000000000, 0.000000000000000000, 0.000000000000000000 ) ) ;
#9928 = CARTESIAN_POINT ( 'NONE',  ( 21.07199075132371746, 22.03847052870693091, -231.7647718156920575 ) ) ;
#9929 = FACE_OUTER_BOUND ( 'NONE', #64514, .T. ) ;
#9930 = VECTOR ( 'NONE', #169731, 1000.000000000000000 ) ;
#9931 = DIRECTION ( 'NONE',  ( 0.000000000000000000, -0.4088369013363280513, 0.9126074666063769270 ) ) ;
#9932 = ORIENTED_EDGE ( 'NONE', *, *, #147323, .T. ) ;
#9934 = CARTESIAN_POINT ( 'NONE',  ( -16.94062896051973865, 22.95638267382587117, -230.8749853720285898 ) ) ;
#9933 = CIRCLE ( 'NONE', #209864, 0.5000000000000004441 ) ;
#9935 = EDGE_CURVE ( 'NONE', #114377, #252254, #116752, .T. ) ;
#9936 = DIRECTION ( 'NONE',  ( 0.000000000000000000, -0.4088369013363281623, 0.9126074666063771490 ) ) ;
#9937 = CARTESIAN_POINT ( 'NONE',  ( -21.14999999999994174, 74.63923853664559260, -43.99645795275012006 ) ) ;
#9938 = CARTESIAN_POINT ( 'NONE',  ( -20.94999999999999929, 68.96868720525722551, -166.4139565462971007 ) ) ;
#9939 = EDGE_CURVE ( 'NONE', #4726, #211251, #45846, .T. ) ;
#9940 = EDGE_CURVE ( 'NONE', #154105, #203005, #112496, .T. ) ;
#9941 = CARTESIAN_POINT ( 'NONE',  ( -22.48660254037843131, 11.75000000001115374, -167.4499999999999886 ) ) ;
#9942 = ORIENTED_EDGE ( 'NONE', *, *, #135217, .T. ) ;
#9943 = CARTESIAN_POINT ( 'NONE',  ( -23.25000000000000000, 76.00000000001213607, -136.5231074845243313 ) ) ;
#9945 = ADVANCED_FACE ( 'NONE', ( #153009 ), #214234, .T. ) ;
#9944 = DIRECTION ( 'NONE',  ( 1.000000000000000000, 0.000000000000000000, 0.000000000000000000 ) ) ;
#9946 = ORIENTED_EDGE ( 'NONE', *, *, #239400, .F. ) ;
#9947 = ORIENTED_EDGE ( 'NONE', *, *, #139030, .T. ) ;
#9948 = LINE ( 'NONE', #68649, #151445 ) ;
#9949 = DIRECTION ( 'NONE',  ( 1.387778780781405791E-13, 0.9999176327611370985, 0.01283462868040226822 ) ) ;
#9950 = EDGE_CURVE ( 'NONE', #102830, #200535, #56416, .T. ) ;
#9951 = CIRCLE ( 'NONE', #34941, 0.1000000000000043493 ) ;
#9952 = ORIENTED_EDGE ( 'NONE', *, *, #48533, .T. ) ;
#9953 = DIRECTION ( 'NONE',  ( 1.000000000000000000, 0.000000000000000000, 0.000000000000000000 ) ) ;
#9954 = FACE_BOUND ( 'NONE', #177881, .T. ) ;
#9955 = ADVANCED_FACE ( 'NONE', ( #31775 ), #16816, .F. ) ;
#9957 = ORIENTED_EDGE ( 'NONE', *, *, #240631, .F. ) ;
#9956 = AXIS2_PLACEMENT_3D ( 'NONE', #46819, #87232, #166827 ) ;
#9959 = PLANE ( 'NONE',  #93854 ) ;
#9958 = CIRCLE ( 'NONE', #84755, 0.09999999999999939493 ) ;
#9960 = AXIS2_PLACEMENT_3D ( 'NONE', #187513, #182368, #3708 ) ;
#9961 = ORIENTED_EDGE ( 'NONE', *, *, #227998, .T. ) ;
#9962 = ADVANCED_FACE ( 'NONE', ( #124031 ), #158059, .T. ) ;
#9963 = DIRECTION ( 'NONE',  ( 0.7071067811865487940, 4.851104656540973741E-15, -0.7071067811865463515 ) ) ;
#9965 = ORIENTED_EDGE ( 'NONE', *, *, #102099, .T. ) ;
#9964 = CYLINDRICAL_SURFACE ( 'NONE', #54112, 11.80000000000000426 ) ;
#9966 = CARTESIAN_POINT ( 'NONE',  ( -20.54999999999999716, -9.499999999988848032, -110.3939691226524786 ) ) ;
#9968 = AXIS2_PLACEMENT_3D ( 'NONE', #214519, #231541, #111586 ) ;
#9967 = CARTESIAN_POINT ( 'NONE',  ( -22.50000000000000000, 11.64957080755595520, -133.9000000000000057 ) ) ;
#9969 = DIRECTION ( 'NONE',  ( 0.000000000000000000, 1.000000000000000000, 0.000000000000000000 ) ) ;
#9970 = CARTESIAN_POINT ( 'NONE',  ( -16.84793658983426923, 66.05000000001230376, -157.2894608067144304 ) ) ;
#9971 = FACE_OUTER_BOUND ( 'NONE', #31274, .T. ) ;
#9972 = AXIS2_PLACEMENT_3D ( 'NONE', #113067, #72683, #156074 ) ;
#9973 = FACE_OUTER_BOUND ( 'NONE', #244853, .T. ) ;
#9974 = DIRECTION ( 'NONE',  ( -0.000000000000000000, 0.8660254037844502539, 0.4999999999999799050 ) ) ;
#9975 = CIRCLE ( 'NONE', #238944, 0.09999999999999971412 ) ;
#9977 = ORIENTED_EDGE ( 'NONE', *, *, #187753, .T. ) ;
#9976 = CARTESIAN_POINT ( 'NONE',  ( -23.15000000000000213, 76.00000000001260503, -190.6481074845243597 ) ) ;
#9978 = EDGE_LOOP ( 'NONE', ( #42815, #8868, #194436, #92022 ) ) ;
#9980 = CARTESIAN_POINT ( 'NONE',  ( -14.77538296656415007, 9.436662931810239741, -85.32303673229492347 ) ) ;
#9979 = CARTESIAN_POINT ( 'NONE',  ( -22.39999999999999858, 68.20922040163824818, -69.52310748452437394 ) ) ;
#9981 = CIRCLE ( 'NONE', #255638, 12.97499999999999964 ) ;
#9983 = ORIENTED_EDGE ( 'NONE', *, *, #121954, .T. ) ;
#9982 = CARTESIAN_POINT ( 'NONE',  ( -18.59999999999999787, 6.982009704867601307, -137.6961521182563217 ) ) ;
#9984 = ORIENTED_EDGE ( 'NONE', *, *, #67063, .F. ) ;
#9985 = CARTESIAN_POINT ( 'NONE',  ( -21.93340585899525763, 0.6726324846117338607, -230.2742912564596054 ) ) ;
#9986 = DIRECTION ( 'NONE',  ( 0.000000000000000000, 6.982962677686266711E-15, -1.000000000000000000 ) ) ;
#9987 = AXIS2_PLACEMENT_3D ( 'NONE', #80568, #58442, #137985 ) ;
#9988 = DIRECTION ( 'NONE',  ( -0.000000000000000000, -0.9770955615653316162, -0.2128009952263604232 ) ) ;
#9989 = CARTESIAN_POINT ( 'NONE',  ( -20.94999027547553894, 10.29326151435327219, -172.9592822510415147 ) ) ;
#9990 = DIRECTION ( 'NONE',  ( -1.836970198721029934E-16, 1.000000000000000000, 0.000000000000000000 ) ) ;
#9991 = AXIS2_PLACEMENT_3D ( 'NONE', #226992, #167057, #246546 ) ;
#9992 = CARTESIAN_POINT ( 'NONE',  ( 18.39999999999997371, 11.47316190337362940, -158.2500000000000284 ) ) ;
#9993 = CARTESIAN_POINT ( 'NONE',  ( -18.59999999999999787, 77.83585931145498193, -24.51866831572578320 ) ) ;
#9994 = AXIS2_PLACEMENT_3D ( 'NONE', #152500, #247717, #35129 ) ;
#9996 = ORIENTED_EDGE ( 'NONE', *, *, #109292, .T. ) ;
#9995 = EDGE_CURVE ( 'NONE', #183962, #82856, #95893, .T. ) ;
#9997 = VERTEX_POINT ( 'NONE', #64045 ) ;
#9998 = DIRECTION ( 'NONE',  ( -6.938893903907222067E-15, -1.000000000000000000, -7.272083257015735086E-15 ) ) ;
#9999 = ADVANCED_FACE ( 'NONE', ( #62764 ), #5321, .F. ) ;
#10000 = ORIENTED_EDGE ( 'NONE', *, *, #12869, .F. ) ;
#10001 = CARTESIAN_POINT ( 'NONE',  ( -21.05000000000000071, 32.73471231533735448, -251.3091613769916535 ) ) ;
#10002 = VERTEX_POINT ( 'NONE', #138415 ) ;
#10004 = VECTOR ( 'NONE', #116567, 1000.000000000000000 ) ;
#10003 = CARTESIAN_POINT ( 'NONE',  ( -23.15000000000000213, 1.910280373842936141, -46.13136785519893834 ) ) ;
#10005 = AXIS2_PLACEMENT_3D ( 'NONE', #90717, #110282, #150706 ) ;
#10006 = DIRECTION ( 'NONE',  ( 0.000000000000000000, 0.000000000000000000, -1.000000000000000000 ) ) ;
#10007 = ADVANCED_FACE ( 'NONE', ( #142290 ), #217956, .F. ) ;
#10009 = EDGE_CURVE ( 'NONE', #211228, #68580, #120206, .T. ) ;
#10008 = DIRECTION ( 'NONE',  ( 0.000000000000000000, -0.000000000000000000, -1.000000000000000000 ) ) ;
#10010 = VERTEX_POINT ( 'NONE', #39381 ) ;
#10011 = CARTESIAN_POINT ( 'NONE',  ( -20.64999999999999858, -4.259020970815408091, -226.0869574510824123 ) ) ;
#10012 = EDGE_LOOP ( 'NONE', ( #172084, #112810, #153334 ) ) ;
#10013 = CARTESIAN_POINT ( 'NONE',  ( -16.87683809663752399, 21.23804903844422043, -180.1499999999999773 ) ) ;
#10014 = CARTESIAN_POINT ( 'NONE',  ( -2.995603634470829482E-16, -11.74999999998884448, -79.25000000000004263 ) ) ;
#10015 = CARTESIAN_POINT ( 'NONE',  ( 20.04142135623730070, 11.75000000001115907, -158.6500000000000057 ) ) ;
#10016 = ORIENTED_EDGE ( 'NONE', *, *, #131462, .F. ) ;
#10017 = B_SPLINE_CURVE_WITH_KNOTS ( 'NONE', 3,
 ( #206799, #162559, #225052, #184655 ),
 .UNSPECIFIED., .F., .F.,
 ( 4, 4 ),
 ( 0.000000000000000000, 0.0002118541922231869474 ),
 .UNSPECIFIED. ) ;
#10018 = DIRECTION ( 'NONE',  ( -1.000000000000000000, -0.000000000000000000, -0.000000000000000000 ) ) ;
#10019 = ORIENTED_EDGE ( 'NONE', *, *, #132475, .F. ) ;
#10022 = ORIENTED_EDGE ( 'NONE', *, *, #166909, .F. ) ;
#10021 = CARTESIAN_POINT ( 'NONE',  ( 18.49999999999999289, 46.32970330538243786, -243.0551226933711746 ) ) ;
#10020 = CARTESIAN_POINT ( 'NONE',  ( 18.43579564894488954, 46.91436734373925077, -255.3877619228566687 ) ) ;
#10023 = AXIS2_PLACEMENT_3D ( 'NONE', #137310, #133476, #257219 ) ;
#10024 = CARTESIAN_POINT ( 'NONE',  ( -18.79999999999999716, -11.65000000000000036, 33.00000000000000000 ) ) ;
#10025 = AXIS2_PLACEMENT_3D ( 'NONE', #22935, #243226, #123297 ) ;
#10026 = ORIENTED_EDGE ( 'NONE', *, *, #125080, .T. ) ;
#10027 = DIRECTION ( 'NONE',  ( 1.000000000000000000, 0.000000000000000000, 0.000000000000000000 ) ) ;
#10028 = ORIENTED_EDGE ( 'NONE', *, *, #149364, .F. ) ;
#10029 = CARTESIAN_POINT ( 'NONE',  ( -23.15000000000000213, -8.999999999988844479, -191.1060308773475356 ) ) ;
#10030 = DIRECTION ( 'NONE',  ( -1.000000000000000000, 0.000000000000000000, 0.000000000000000000 ) ) ;
#10031 = CARTESIAN_POINT ( 'NONE',  ( -17.22767730083556970, 52.63511723856208846, -231.0537232253000752 ) ) ;
#10032 = CARTESIAN_POINT ( 'NONE',  ( -16.92570016628985385, 66.04121104227219519, -123.9024568144853760 ) ) ;
#10033 = ORIENTED_EDGE ( 'NONE', *, *, #100506, .T. ) ;
#10034 = FACE_OUTER_BOUND ( 'NONE', #733, .T. ) ;
#10035 = CARTESIAN_POINT ( 'NONE',  ( -16.85939681242905408, 14.04926739942075997, -218.9616247998112328 ) ) ;
#10036 = CARTESIAN_POINT ( 'NONE',  ( 21.08134388332232234, 6.334680580529114202, -33.42418108249297859 ) ) ;
#10037 = ORIENTED_EDGE ( 'NONE', *, *, #42460, .F. ) ;
#10038 = ADVANCED_FACE ( 'NONE', ( #141026 ), #100565, .T. ) ;
#10039 = DIRECTION ( 'NONE',  ( 0.000000000000000000, 0.5273008465188219196, -0.8496786552930077896 ) ) ;
#10040 = ORIENTED_EDGE ( 'NONE', *, *, #4897, .T. ) ;
#10041 = DIRECTION ( 'NONE',  ( 1.000000000000000000, -0.000000000000000000, 0.000000000000000000 ) ) ;
#10042 = ORIENTED_EDGE ( 'NONE', *, *, #174392, .T. ) ;
#10043 = AXIS2_PLACEMENT_3D ( 'NONE', #169417, #248926, #205929 ) ;
#10044 = LINE ( 'NONE', #105252, #193348 ) ;
#10045 = DIRECTION ( 'NONE',  ( 0.000000000000000000, 0.000000000000000000, 1.000000000000000000 ) ) ;
#10047 = VERTEX_POINT ( 'NONE', #118902 ) ;
#10046 = SPHERICAL_SURFACE ( 'NONE', #152878, 0.1000000000000000056 ) ;
#10048 = CARTESIAN_POINT ( 'NONE',  ( -21.37071067811865532, 67.92928932189340685, -124.2731074845243597 ) ) ;
#10049 = EDGE_CURVE ( 'NONE', #235860, #47181, #198417, .T. ) ;
#10050 = CARTESIAN_POINT ( 'NONE',  ( -21.05000000000000071, 28.55432187084631224, -258.5393726171218418 ) ) ;
#10051 = CARTESIAN_POINT ( 'NONE',  ( -18.59999999999999787, -1.162701749926853712, -41.50000000000000000 ) ) ;
#10052 = EDGE_CURVE ( 'NONE', #245021, #45997, #175675, .T. ) ;
#10053 = VERTEX_POINT ( 'NONE', #207 ) ;
#10054 = CARTESIAN_POINT ( 'NONE',  ( 21.46681500593473402, 69.14248884062999423, -203.5231074845244166 ) ) ;
#10055 = CARTESIAN_POINT ( 'NONE',  ( 18.49999999999999645, 4.252251777740764460, -211.8999245327126744 ) ) ;
#10056 = VERTEX_POINT ( 'NONE', #121483 ) ;
#10058 = CARTESIAN_POINT ( 'NONE',  ( 21.05000000000000071, 1.618246818147480726, -230.7412754484373352 ) ) ;
#10057 = CIRCLE ( 'NONE', #205678, 0.1000000000000028644 ) ;
#10059 = VECTOR ( 'NONE', #242137, 1000.000000000000000 ) ;
#10060 = ORIENTED_EDGE ( 'NONE', *, *, #154410, .F. ) ;
#10061 = AXIS2_PLACEMENT_3D ( 'NONE', #44480, #180139, #198403 ) ;
#10062 = AXIS2_PLACEMENT_3D ( 'NONE', #145771, #3701, #87073 ) ;
#10063 = EDGE_CURVE ( 'NONE', #79373, #79923, #104426, .T. ) ;
#10064 = CARTESIAN_POINT ( 'NONE',  ( 15.74999999999999645, 9.350000000011133849, -117.3657431672739762 ) ) ;
#10065 = DIRECTION ( 'NONE',  ( -1.000000000000000000, 7.304098846218134667E-16, 5.100424963727255829E-30 ) ) ;
#10066 = EDGE_CURVE ( 'NONE', #128766, #216103, #104689, .T. ) ;
#10067 = ADVANCED_FACE ( 'NONE', ( #240125 ), #61481, .T. ) ;
#10070 = ORIENTED_EDGE ( 'NONE', *, *, #51696, .F. ) ;
#10069 = ORIENTED_EDGE ( 'NONE', *, *, #192635, .F. ) ;
#10068 = DIRECTION ( 'NONE',  ( 1.000000000000000000, 0.000000000000000000, 0.000000000000000000 ) ) ;
#10071 = FACE_BOUND ( 'NONE', #23826, .T. ) ;
#10072 = CARTESIAN_POINT ( 'NONE',  ( -22.44366136229477249, 0.009341569497225218552, -155.8502814425260397 ) ) ;
#10073 = CARTESIAN_POINT ( 'NONE',  ( -23.15000000000000213, 85.00000000001179501, -79.41707660717668205 ) ) ;
#10074 = TOROIDAL_SURFACE ( 'NONE', #159945, 0.2000000000000000111, 0.1000000000000000056 ) ;
#10075 = EDGE_CURVE ( 'NONE', #4154, #31295, #181444, .T. ) ;
#10077 = LINE ( 'NONE', #249975, #117067 ) ;
#10076 = DIRECTION ( 'NONE',  ( -0.000000000000000000, -0.8660254037844459241, -0.4999999999999873990 ) ) ;
#10078 = CARTESIAN_POINT ( 'NONE',  ( 23.25000000000000000, 87.65000000001202807, -114.7731074845242318 ) ) ;
#10079 = DIRECTION ( 'NONE',  ( 0.000000000000000000, 0.8814952561688438326, -0.4721928772777331806 ) ) ;
#10080 = CARTESIAN_POINT ( 'NONE',  ( -18.50000000000000000, 64.25000000001203659, -114.7731074845243882 ) ) ;
#10081 = AXIS2_PLACEMENT_3D ( 'NONE', #102528, #227640, #25610 ) ;
#10082 = CARTESIAN_POINT ( 'NONE',  ( -23.25000000000000000, 36.65892442174472876, -249.5511627012454596 ) ) ;
#10083 = AXIS2_PLACEMENT_3D ( 'NONE', #131895, #196987, #191903 ) ;
#10084 = ORIENTED_EDGE ( 'NONE', *, *, #71056, .F. ) ;
#10085 = VERTEX_POINT ( 'NONE', #44497 ) ;
#10086 = AXIS2_PLACEMENT_3D ( 'NONE', #146980, #25774, #230389 ) ;
#10087 = DIRECTION ( 'NONE',  ( 0.000000000000000000, 0.000000000000000000, 1.000000000000000000 ) ) ;
#10088 = VECTOR ( 'NONE', #50298, 1000.000000000000000 ) ;
#10090 = VERTEX_POINT ( 'NONE', #2768 ) ;
#10089 = DIRECTION ( 'NONE',  ( 0.000000000000000000, 0.2128009952263601179, -0.9770955615653315052 ) ) ;
#10091 = EDGE_LOOP ( 'NONE', ( #211173, #172407, #208181, #213723, #53390 ) ) ;
#10092 = EDGE_CURVE ( 'NONE', #67400, #2075, #647, .T. ) ;
#10093 = CARTESIAN_POINT ( 'NONE',  ( -20.54999999999999716, 66.65000000001253966, -182.2731074845244166 ) ) ;
#10094 = ORIENTED_EDGE ( 'NONE', *, *, #256177, .F. ) ;
#10095 = LINE ( 'NONE', #97288, #180120 ) ;
#10096 = VECTOR ( 'NONE', #125606, 1000.000000000000114 ) ;
#10097 = CIRCLE ( 'NONE', #172656, 0.09999999999999986677 ) ;
#10098 = ORIENTED_EDGE ( 'NONE', *, *, #209042, .T. ) ;
#10099 = TOROIDAL_SURFACE ( 'NONE', #122742, 12.97499999999999787, 0.1000000000000000056 ) ;
#10100 = DIRECTION ( 'NONE',  ( 1.000000000000000000, 0.000000000000000000, 0.000000000000000000 ) ) ;
#10101 = CARTESIAN_POINT ( 'NONE',  ( -14.00000000000000178, 9.850000000011133849, -83.75000000000004263 ) ) ;
#10102 = VECTOR ( 'NONE', #232610, 1000.000000000000000 ) ;
#10104 = ORIENTED_EDGE ( 'NONE', *, *, #4028, .T. ) ;
#10103 = ORIENTED_EDGE ( 'NONE', *, *, #224122, .T. ) ;
#10105 = EDGE_LOOP ( 'NONE', ( #90135, #149196, #205089 ) ) ;
#10106 = DIRECTION ( 'NONE',  ( 1.000000000000000000, -3.151514657663852580E-16, 8.547182517843351137E-17 ) ) ;
#10107 = ORIENTED_EDGE ( 'NONE', *, *, #25772, .T. ) ;
#10108 = ORIENTED_EDGE ( 'NONE', *, *, #18008, .T. ) ;
#10110 = DIRECTION ( 'NONE',  ( 0.000000000000000000, 1.000000000000000000, 6.853228547068871147E-15 ) ) ;
#10109 = VECTOR ( 'NONE', #178109, 1000.000000000000000 ) ;
#10111 = CARTESIAN_POINT ( 'NONE',  ( 21.07888907270776002, 43.42727287605945463, -234.7669095404490065 ) ) ;
#10112 = CARTESIAN_POINT ( 'NONE',  ( -12.60829076262180592, 9.389529397477895500, -185.3171079128936753 ) ) ;
#10114 = VERTEX_POINT ( 'NONE', #43205 ) ;
#10113 = CYLINDRICAL_SURFACE ( 'NONE', #151866, 0.09999999999999939493 ) ;
#10115 = DIRECTION ( 'NONE',  ( 1.000000000000000000, -0.000000000000000000, -0.000000000000000000 ) ) ;
#10116 = CARTESIAN_POINT ( 'NONE',  ( 21.04999999999999716, 12.04127962393059548, -206.0806704050589246 ) ) ;
#10118 = ORIENTED_EDGE ( 'NONE', *, *, #219431, .F. ) ;
#10117 = DIRECTION ( 'NONE',  ( 0.000000000000000000, 0.000000000000000000, 1.000000000000000000 ) ) ;
#10119 = DIRECTION ( 'NONE',  ( -1.000000000000000000, -0.000000000000000000, -0.000000000000000000 ) ) ;
#10120 = ORIENTED_EDGE ( 'NONE', *, *, #148917, .F. ) ;
#10121 = VECTOR ( 'NONE', #233569, 1000.000000000000114 ) ;
#10122 = DIRECTION ( 'NONE',  ( -1.000000000000000000, -0.000000000000000000, 0.000000000000000000 ) ) ;
#10123 = AXIS2_PLACEMENT_3D ( 'NONE', #127697, #110688, #247635 ) ;
#10124 = ORIENTED_EDGE ( 'NONE', *, *, #231711, .T. ) ;
#10125 = AXIS2_PLACEMENT_3D ( 'NONE', #80432, #256481, #239556 ) ;
#10126 = CARTESIAN_POINT ( 'NONE',  ( 22.32929514600007792, 68.42135243463590655, -170.1221831626383221 ) ) ;
#10127 = CARTESIAN_POINT ( 'NONE',  ( -16.92973740335347443, 30.27581433217048357, -234.7960487711081043 ) ) ;
#10128 = ORIENTED_EDGE ( 'NONE', *, *, #153797, .F. ) ;
#10130 = DIRECTION ( 'NONE',  ( 1.000000000000000000, -0.000000000000000000, -0.000000000000000000 ) ) ;
#10129 = CARTESIAN_POINT ( 'NONE',  ( -20.94999999999999929, 56.45527679911575802, -225.2871936083021467 ) ) ;
#10131 = LINE ( 'NONE', #12723, #214180 ) ;
#10132 = EDGE_CURVE ( 'NONE', #123224, #87130, #242274, .T. ) ;
#10133 = LINE ( 'NONE', #246176, #251331 ) ;
#10134 = SPHERICAL_SURFACE ( 'NONE', #230862, 0.1000000000000000056 ) ;
#10135 = ORIENTED_EDGE ( 'NONE', *, *, #219774, .T. ) ;
#10136 = ORIENTED_EDGE ( 'NONE', *, *, #19425, .T. ) ;
#10137 = CARTESIAN_POINT ( 'NONE',  ( -20.64999999999999858, 1.115600667400684642E-11, -79.87500000000004263 ) ) ;
#10138 = FACE_OUTER_BOUND ( 'NONE', #230829, .T. ) ;
#10139 = VERTEX_POINT ( 'NONE', #247820 ) ;
#10140 = CARTESIAN_POINT ( 'NONE',  ( -18.50000000000000000, 16.50669723772569952, -240.7258389668962479 ) ) ;
#10141 = ORIENTED_EDGE ( 'NONE', *, *, #196865, .T. ) ;
#10142 = FACE_OUTER_BOUND ( 'NONE', #252352, .T. ) ;
#10143 = EDGE_CURVE ( 'NONE', #85966, #181206, #254711, .T. ) ;
#10144 = CARTESIAN_POINT ( 'NONE',  ( -23.25000000000000000, 6.982009704856444898, -37.19615211825629331 ) ) ;
#10145 = CARTESIAN_POINT ( 'NONE',  ( -20.94999999999999929, 5.849999999999952571, -10.13249722427796762 ) ) ;
#10146 = AXIS2_PLACEMENT_3D ( 'NONE', #212663, #148840, #110983 ) ;
#10147 = ADVANCED_FACE ( 'NONE', ( #224390 ), #147435, .T. ) ;
#10148 = EDGE_CURVE ( 'NONE', #219738, #36888, #213057, .T. ) ;
#10149 = AXIS2_PLACEMENT_3D ( 'NONE', #196970, #220411, #41791 ) ;
#10150 = EDGE_LOOP ( 'NONE', ( #5241, #172101, #38586, #91828, #47018 ) ) ;
#10151 = CARTESIAN_POINT ( 'NONE',  ( -16.78493832629888161, 66.05416425680844839, -190.8591584654202506 ) ) ;
#10152 = AXIS2_PLACEMENT_3D ( 'NONE', #209448, #110348, #90773 ) ;
#10153 =( BOUNDED_CURVE ( )  B_SPLINE_CURVE ( 3, ( #55628, #137751, #120803, #36124 ),
 .UNSPECIFIED., .F., .T. ) 
 B_SPLINE_CURVE_WITH_KNOTS ( ( 4, 4 ),
 ( 1.570796326794895448, 3.141592653589791784 ),
 .UNSPECIFIED. ) 
 CURVE ( )  GEOMETRIC_REPRESENTATION_ITEM ( )  RATIONAL_B_SPLINE_CURVE ( ( 1.000000000000000000, 0.8047378541243650485, 0.8047378541243650485, 1.000000000000000000 ) ) 
 REPRESENTATION_ITEM ( '' )  );
#10154 = EDGE_LOOP ( 'NONE', ( #3676, #228797, #30575, #203755 ) ) ;
#10155 = ORIENTED_EDGE ( 'NONE', *, *, #9076, .T. ) ;
#10156 = VERTEX_POINT ( 'NONE', #108315 ) ;
#10157 = VECTOR ( 'NONE', #85979, 1000.000000000000000 ) ;
#10158 = DIRECTION ( 'NONE',  ( -2.252264143451594314E-15, -0.1298341882520124002, -0.9915357197604841577 ) ) ;
#10159 = DIRECTION ( 'NONE',  ( 0.000000000000000000, 0.000000000000000000, -1.000000000000000000 ) ) ;
#10160 = VECTOR ( 'NONE', #105027, 1000.000000000000000 ) ;
#10161 = LINE ( 'NONE', #171835, #104893 ) ;
#10162 = CARTESIAN_POINT ( 'NONE',  ( 18.49999999999998934, 19.85039924724470950, -69.28030305780140452 ) ) ;
#10163 = CYLINDRICAL_SURFACE ( 'NONE', #138508, 0.1000000000000013933 ) ;
#10164 = EDGE_CURVE ( 'NONE', #161970, #100003, #142324, .T. ) ;
#10166 = CARTESIAN_POINT ( 'NONE',  ( 21.08832698747859169, 8.775364393417216746, -12.22871746646415225 ) ) ;
#10165 = CARTESIAN_POINT ( 'NONE',  ( 21.05000000000000071, -0.09999999998884512298, -160.9593430482987344 ) ) ;
#10168 = ORIENTED_EDGE ( 'NONE', *, *, #253044, .T. ) ;
#10167 = CARTESIAN_POINT ( 'NONE',  ( 20.94999999999999574, 14.00000000001115730, -38.92709253038254502 ) ) ;
#10169 = CARTESIAN_POINT ( 'NONE',  ( -22.47071067811865319, 10.68684811775433374, -226.8807012965928038 ) ) ;
#10170 = ORIENTED_EDGE ( 'NONE', *, *, #172568, .T. ) ;
#10171 = AXIS2_PLACEMENT_3D ( 'NONE', #183124, #4460, #166155 ) ;
#10172 = EDGE_CURVE ( 'NONE', #252677, #188219, #58914, .T. ) ;
#10173 = FACE_OUTER_BOUND ( 'NONE', #76113, .T. ) ;
#10174 = ORIENTED_EDGE ( 'NONE', *, *, #3794, .F. ) ;
#10175 = ORIENTED_EDGE ( 'NONE', *, *, #185522, .F. ) ;
#10176 = DIRECTION ( 'NONE',  ( 0.000000000000000000, 0.000000000000000000, -1.000000000000000000 ) ) ;
#10177 = AXIS2_PLACEMENT_3D ( 'NONE', #65927, #145446, #224971 ) ;
#10178 = DIRECTION ( 'NONE',  ( -1.000000000000000000, 1.836970198721029934E-16, 1.282749433769087757E-30 ) ) ;
#10179 = LINE ( 'NONE', #109254, #246083 ) ;
#10180 = TOROIDAL_SURFACE ( 'NONE', #43484, 11.70000000000000639, 0.1000000000000000056 ) ;
#10181 = DIRECTION ( 'NONE',  ( 0.000000000000000000, -7.086529944415886769E-15, 1.000000000000000000 ) ) ;
#10182 = PRODUCT_RELATED_PRODUCT_CATEGORY ( 'part', '', ( #45061 ) ) ;
#10183 = AXIS2_PLACEMENT_3D ( 'NONE', #46356, #45092, #125899 ) ;
#10184 = VECTOR ( 'NONE', #236781, 1000.000000000000000 ) ;
#10185 = CARTESIAN_POINT ( 'NONE',  ( 20.85000000000000142, -1.835859311432481045, -212.5044391687984842 ) ) ;
#10186 = ORIENTED_EDGE ( 'NONE', *, *, #127665, .T. ) ;
#10187 = ORIENTED_EDGE ( 'NONE', *, *, #42101, .T. ) ;
#10188 = EDGE_CURVE ( 'NONE', #168738, #243465, #6631, .T. ) ;
#10189 = FACE_OUTER_BOUND ( 'NONE', #174082, .T. ) ;
#10191 = ORIENTED_EDGE ( 'NONE', *, *, #81204, .T. ) ;
#10190 = EDGE_CURVE ( 'NONE', #119379, #94181, #100601, .T. ) ;
#10192 = LINE ( 'NONE', #169295, #236204 ) ;
#10193 = CYLINDRICAL_SURFACE ( 'NONE', #82005, 4.000000000000003553 ) ;
#10194 = ORIENTED_EDGE ( 'NONE', *, *, #160872, .T. ) ;
#10195 = EDGE_CURVE ( 'NONE', #252537, #5245, #88131, .T. ) ;
#10196 = DIRECTION ( 'NONE',  ( -0.000000000000000000, 0.000000000000000000, 1.000000000000000000 ) ) ;
#10198 = VECTOR ( 'NONE', #164809, 1000.000000000000000 ) ;
#10197 = CARTESIAN_POINT ( 'NONE',  ( -18.34374000495059676, 54.09900352584866567, -229.1663746252470446 ) ) ;
#10199 = CARTESIAN_POINT ( 'NONE',  ( -11.60000000000000320, -12.25000000000000178, 15.00000000000000355 ) ) ;
#10200 = CARTESIAN_POINT ( 'NONE',  ( 20.94999999999999574, 14.77103648604101060, -236.4083752604501001 ) ) ;
#10201 = EDGE_LOOP ( 'NONE', ( #4654, #146788 ) ) ;
#10202 = DIRECTION ( 'NONE',  ( 0.000000000000000000, 0.000000000000000000, -1.000000000000000000 ) ) ;
#10203 = CARTESIAN_POINT ( 'NONE',  ( 20.85000000000000142, 77.83585931145600512, -158.5186683157258187 ) ) ;
#10204 = CARTESIAN_POINT ( 'NONE',  ( -18.59999999999999787, 77.36242903720570041, -162.1342262366031548 ) ) ;
#10205 = CARTESIAN_POINT ( 'NONE',  ( -18.59999999999999787, -1.851028230129704522, -179.1539132694224463 ) ) ;
#10206 = CIRCLE ( 'NONE', #26777, 0.09999999999999993616 ) ;
#10207 = CARTESIAN_POINT ( 'NONE',  ( 18.59999999999999787, 87.75000000001195133, -111.6731074845242233 ) ) ;
#10208 = EDGE_CURVE ( 'NONE', #143423, #33482, #246400, .T. ) ;
#10209 = DIRECTION ( 'NONE',  ( -1.000000000000000000, 0.000000000000000000, 0.000000000000000000 ) ) ;
#10210 = AXIS2_PLACEMENT_3D ( 'NONE', #76803, #74279, #32592 ) ;
#10211 = CIRCLE ( 'NONE', #89463, 0.09999999999999939493 ) ;
#10212 = ORIENTED_EDGE ( 'NONE', *, *, #76715, .T. ) ;
#10213 = AXIS2_PLACEMENT_3D ( 'NONE', #190848, #206522, #228674 ) ;
#10214 = CARTESIAN_POINT ( 'NONE',  ( -21.07094088545304444, 69.67983277809565834, -136.6220011870765632 ) ) ;
#10215 = ORIENTED_EDGE ( 'NONE', *, *, #128643, .F. ) ;
#10216 = SHAPE_REPRESENTATION ( 'Snap Open Cable Crossbars 12', ( #2425 ), #127326 ) ;
#10217 = DIRECTION ( 'NONE',  ( 1.000000000000000000, 0.000000000000000000, 0.000000000000000000 ) ) ;
#10218 = DIRECTION ( 'NONE',  ( -1.000000000000000000, 1.772924042024179204E-16, -4.808324575169892332E-17 ) ) ;
#10219 = CARTESIAN_POINT ( 'NONE',  ( 18.60000000000000497, 1.115600667400684642E-11, -134.0000000000000000 ) ) ;
#10220 = CARTESIAN_POINT ( 'NONE',  ( 23.25000000000000000, 87.65000000001246860, -173.1231074845242688 ) ) ;
#10221 = VERTEX_POINT ( 'NONE', #207426 ) ;
#10222 = EDGE_CURVE ( 'NONE', #74028, #30038, #204681, .T. ) ;
#10223 = LINE ( 'NONE', #89730, #175974 ) ;
#10224 = CARTESIAN_POINT ( 'NONE',  ( -5.999999999999938716, 64.65000000001120384, -25.92310748452479174 ) ) ;
#10225 = DIRECTION ( 'NONE',  ( 2.952720810173290591E-16, -0.4721928772777312933, -0.8814952561688448318 ) ) ;
#10226 = LINE ( 'NONE', #154884, #121532 ) ;
#10227 = CIRCLE ( 'NONE', #105857, 0.09999999999999939493 ) ;
#10228 = CARTESIAN_POINT ( 'NONE',  ( 18.59999999999999787, 7.567413955921498570, -241.6205176796878504 ) ) ;
#10229 = ORIENTED_EDGE ( 'NONE', *, *, #232167, .T. ) ;
#10230 = ORIENTED_EDGE ( 'NONE', *, *, #225434, .T. ) ;
#10231 = CARTESIAN_POINT ( 'NONE',  ( -20.90000000326035590, 6.338045365888075544, 12.02580456186802138 ) ) ;
#10233 = ADVANCED_FACE ( 'NONE', ( #69209 ), #63202, .T. ) ;
#10232 = CARTESIAN_POINT ( 'NONE',  ( 18.49999999999999289, 10.20857864377385127, -91.65000000000004832 ) ) ;
#10234 = CIRCLE ( 'NONE', #218863, 0.1000000000000032391 ) ;
#10235 = DIRECTION ( 'NONE',  ( 0.000000000000000000, 0.4999999999999689138, -0.8660254037844565822 ) ) ;
#10236 = B_SPLINE_CURVE_WITH_KNOTS ( 'NONE', 3,
 ( #68387, #168812, #86625, #8415, #9681, #247003 ),
 .UNSPECIFIED., .F., .F.,
 ( 4, 2, 4 ),
 ( 0.000000000000000000, 0.0001895189928937418447, 0.0003790379857874836894 ),
 .UNSPECIFIED. ) ;
#10237 = ORIENTED_EDGE ( 'NONE', *, *, #175533, .T. ) ;
#10238 = CARTESIAN_POINT ( 'NONE',  ( 23.15000000000000213, -12.41227409413852811, -97.40000000000004832 ) ) ;
#10239 = ADVANCED_FACE ( 'NONE', ( #168332 ), #129848, .T. ) ;
#10240 = LINE ( 'NONE', #191467, #225751 ) ;
#10241 = ORIENTED_EDGE ( 'NONE', *, *, #3645, .F. ) ;
#10242 = SPHERICAL_SURFACE ( 'NONE', #150511, 0.1000000000000000056 ) ;
#10243 = EDGE_CURVE ( 'NONE', #216369, #247118, #217131, .T. ) ;
#10244 = AXIS2_PLACEMENT_3D ( 'NONE', #220052, #239622, #41437 ) ;
#10245 = ADVANCED_FACE ( 'NONE', ( #228267 ), #187867, .T. ) ;
#10246 = ORIENTED_EDGE ( 'NONE', *, *, #89715, .F. ) ;
#10247 = ORIENTED_EDGE ( 'NONE', *, *, #217423, .T. ) ;
#10248 = VERTEX_POINT ( 'NONE', #70503 ) ;
#10249 = FACE_OUTER_BOUND ( 'NONE', #57648, .T. ) ;
#10250 = DIRECTION ( 'NONE',  ( 1.000000000000000000, 0.000000000000000000, 0.000000000000000000 ) ) ;
#10251 = CARTESIAN_POINT ( 'NONE',  ( 23.24999999999999289, 11.75000000001116263, -167.5999999999999659 ) ) ;
#10252 = CARTESIAN_POINT ( 'NONE',  ( -21.07928932188134041, 69.67148334361864670, -103.1220026301787414 ) ) ;
#10253 = CARTESIAN_POINT ( 'NONE',  ( -21.05000000000000071, 1.115600667400684642E-11, -167.4999999999999716 ) ) ;
#10254 = DIRECTION ( 'NONE',  ( 0.000000000000000000, 0.2128009952263601456, -0.9770955615653316162 ) ) ;
#10255 = CARTESIAN_POINT ( 'NONE',  ( -16.93226657140833069, 9.999543822724415776, -12.57871311097362188 ) ) ;
#10257 = DIRECTION ( 'NONE',  ( 1.000000000000000000, 0.000000000000000000, 0.000000000000000000 ) ) ;
#10256 = CARTESIAN_POINT ( 'NONE',  ( 21.14999999999999503, 7.128833340093095217, -233.7327013124392749 ) ) ;
#10258 = CARTESIAN_POINT ( 'NONE',  ( 21.15000000000005542, 64.35000000001120668, -3.023107484524792277 ) ) ;
#10259 = CARTESIAN_POINT ( 'NONE',  ( -21.14999999999994174, 77.25000000001119815, -43.92310748452479885 ) ) ;
#10260 = DIRECTION ( 'NONE',  ( -1.000000000000000000, -3.265361837132813093E-16, 0.000000000000000000 ) ) ;
#10262 = CARTESIAN_POINT ( 'NONE',  ( 20.95420533658165141, 18.77923608808111666, -228.0098942474668888 ) ) ;
#10261 = CIRCLE ( 'NONE', #231029, 11.65000000000001457 ) ;
#10263 = VERTEX_POINT ( 'NONE', #26220 ) ;
#10264 = AXIS2_PLACEMENT_3D ( 'NONE', #250504, #211393, #130558 ) ;
#10265 = EDGE_LOOP ( 'NONE', ( #226611, #68304, #10174, #13735 ) ) ;
#10266 = FACE_OUTER_BOUND ( 'NONE', #57926, .T. ) ;
#10267 = ADVANCED_FACE ( 'NONE', ( #88718 ), #129163, .F. ) ;
#10268 = CARTESIAN_POINT ( 'NONE',  ( -23.25000000000000000, 76.10000000001276987, -215.1726782920691505 ) ) ;
#10271 = PLANE ( 'NONE',  #186820 ) ;
#10270 = FACE_OUTER_BOUND ( 'NONE', #187, .T. ) ;
#10269 = CIRCLE ( 'NONE', #226723, 2.000000000000001776 ) ;
#10272 = CIRCLE ( 'NONE', #35416, 0.09999999999999939493 ) ;
#10274 = DIRECTION ( 'NONE',  ( 0.000000000000000000, -6.938893903907222067E-15, 1.000000000000000000 ) ) ;
#10273 = PRESENTATION_LAYER_ASSIGNMENT (  '', '', ( #248145 ) ) ;
#10276 = ADVANCED_FACE ( 'NONE', ( #249122 ), #150026, .F. ) ;
#10275 = CARTESIAN_POINT ( 'NONE',  ( 21.97500000000000497, 66.25000000001158185, -57.17310748452438673 ) ) ;
#10277 = DIRECTION ( 'NONE',  ( 0.000000000000000000, 1.897661533703519897E-16, -1.000000000000000000 ) ) ;
#10278 = ORIENTED_EDGE ( 'NONE', *, *, #112126, .F. ) ;
#10279 = ORIENTED_EDGE ( 'NONE', *, *, #59939, .T. ) ;
#10280 = EDGE_CURVE ( 'NONE', #223901, #101690, #11805, .T. ) ;
#10282 = VECTOR ( 'NONE', #105529, 1000.000000000000000 ) ;
#10281 = CARTESIAN_POINT ( 'NONE',  ( -15.51798037960205257, 9.376659938533535410, -17.62819254821728876 ) ) ;
#10283 = VERTEX_POINT ( 'NONE', #71771 ) ;
#10284 = CARTESIAN_POINT ( 'NONE',  ( 23.14999999999999147, 4.150000000011154988, -67.00000000000004263 ) ) ;
#10285 = EDGE_CURVE ( 'NONE', #109096, #198292, #233912, .T. ) ;
#10286 = CIRCLE ( 'NONE', #110207, 0.1000000000000124678 ) ;
#10288 = LINE ( 'NONE', #188913, #121578 ) ;
#10287 = AXIS2_PLACEMENT_3D ( 'NONE', #186442, #104300, #69069 ) ;
#10289 = AXIS2_PLACEMENT_3D ( 'NONE', #161807, #45682, #204742 ) ;
#10290 = CIRCLE ( 'NONE', #47846, 0.09999999999998898659 ) ;
#10291 = ORIENTED_EDGE ( 'NONE', *, *, #128877, .F. ) ;
#10292 = CARTESIAN_POINT ( 'NONE',  ( -2.995603634470829482E-16, 28.91254064196106910, -237.8576372133405528 ) ) ;
#10293 = EDGE_LOOP ( 'NONE', ( #212810, #38345, #235393, #94777 ) ) ;
#10294 = EDGE_CURVE ( 'NONE', #213256, #179078, #237994, .T. ) ;
#10295 = DIRECTION ( 'NONE',  ( 0.000000000000000000, 0.9915357197604837136, -0.1298341882520134827 ) ) ;
#10296 = ADVANCED_FACE ( 'NONE', ( #194293 ), #192237, .F. ) ;
#10297 = DIRECTION ( 'NONE',  ( 1.000000000000000000, 0.000000000000000000, 0.000000000000000000 ) ) ;
#10299 = AXIS2_PLACEMENT_3D ( 'NONE', #68331, #151743, #172611 ) ;
#10298 = DIRECTION ( 'NONE',  ( 0.000000000000000000, -0.9876197685951265681, -0.1568667991644790149 ) ) ;
#10301 = DIRECTION ( 'NONE',  ( 1.000000000000000000, 0.000000000000000000, 0.000000000000000000 ) ) ;
#10300 = AXIS2_PLACEMENT_3D ( 'NONE', #195355, #80469, #156230 ) ;
#10302 = DIRECTION ( 'NONE',  ( -0.000000000000000000, 1.000000000000000000, 6.982962677686266711E-15 ) ) ;
#10304 = CIRCLE ( 'NONE', #156057, 0.1000000000000013933 ) ;
#10303 = DIRECTION ( 'NONE',  ( -0.000000000000000000, -0.9770955615653316162, -0.2128009952263604232 ) ) ;
#10305 = CYLINDRICAL_SURFACE ( 'NONE', #1065, 0.09999999999999939493 ) ;
#10306 = CYLINDRICAL_SURFACE ( 'NONE', #145434, 0.1000000000000124678 ) ;
#10308 = EDGE_LOOP ( 'NONE', ( #230650, #214838, #47259, #48492 ) ) ;
#10307 = DIRECTION ( 'NONE',  ( 1.000000000000000000, 0.000000000000000000, -0.000000000000000000 ) ) ;
#10310 = CARTESIAN_POINT ( 'NONE',  ( -23.15000000000000213, 76.00000000001267608, -203.5231074845243597 ) ) ;
#10309 = CARTESIAN_POINT ( 'NONE',  ( -16.77683809663752257, 66.05416425680785153, -115.6870565036285683 ) ) ;
#10311 = AXIS2_PLACEMENT_3D ( 'NONE', #247977, #108476, #186748 ) ;
#10312 = ORIENTED_EDGE ( 'NONE', *, *, #76677, .T. ) ;
#10314 = EDGE_LOOP ( 'NONE', ( #635, #229159, #146735, #174698 ) ) ;
#10313 = CARTESIAN_POINT ( 'NONE',  ( 21.05000000000000071, 67.22371710472015138, -194.9644784893834810 ) ) ;
#10315 = ORIENTED_EDGE ( 'NONE', *, *, #249936, .T. ) ;
#10316 = DIRECTION ( 'NONE',  ( 0.000000000000000000, -0.2128009952263604232, 0.9770955615653316162 ) ) ;
#10317 = CIRCLE ( 'NONE', #185268, 0.1000000000000028644 ) ;
#10318 = CARTESIAN_POINT ( 'NONE',  ( 22.49066049874202022, 75.94365674847951198, -81.17311972204143444 ) ) ;
#10319 = FACE_OUTER_BOUND ( 'NONE', #68803, .T. ) ;
#10320 = CARTESIAN_POINT ( 'NONE',  ( 23.15000000000000213, -4.756823075239758225, -233.1486023682345490 ) ) ;
#10321 = AXIS2_PLACEMENT_3D ( 'NONE', #7460, #30917, #204371 ) ;
#10322 = DIRECTION ( 'NONE',  ( 1.000000000000000000, -0.000000000000000000, -0.000000000000000000 ) ) ;
#10323 = AXIS2_PLACEMENT_3D ( 'NONE', #156268, #216187, #137934 ) ;
#10324 = CARTESIAN_POINT ( 'NONE',  ( -18.41431012584568805, 13.18782249248739369, -207.5708846587602920 ) ) ;
#10325 = DIRECTION ( 'NONE',  ( -1.000000000000000000, 0.000000000000000000, -0.000000000000000000 ) ) ;
#10326 = CARTESIAN_POINT ( 'NONE',  ( 20.94999999999999929, 67.85909929089923764, -227.8797997985275856 ) ) ;
#10327 = EDGE_LOOP ( 'NONE', ( #47152, #78985, #215056 ) ) ;
#10328 = VERTEX_POINT ( 'NONE', #92579 ) ;
#10329 = CARTESIAN_POINT ( 'NONE',  ( 19.75857864376268935, 64.35000000001220144, -145.1731074845244507 ) ) ;
#10330 = ADVANCED_FACE ( 'NONE', ( #91320 ), #95162, .F. ) ;
#10331 = ORIENTED_EDGE ( 'NONE', *, *, #149458, .F. ) ;
#10332 = CARTESIAN_POINT ( 'NONE',  ( -18.40000000000000213, 64.66825945288707089, -149.1731074845244507 ) ) ;
#10333 = ORIENTED_EDGE ( 'NONE', *, *, #160485, .F. ) ;
#10334 = CARTESIAN_POINT ( 'NONE',  ( 18.40000000000000213, -9.500000000000000000, -40.42214984933045940 ) ) ;
#10335 = CARTESIAN_POINT ( 'NONE',  ( 19.96984138294294908, 11.75000000000005862, -24.72457207120111988 ) ) ;
#10336 = CARTESIAN_POINT ( 'NONE',  ( -22.39999999999999858, -2.479040261793999722, -189.6172560698084624 ) ) ;
#10337 = CARTESIAN_POINT ( 'NONE',  ( -21.05000000000000426, 1.372110199356192384, -230.7624259250305556 ) ) ;
#10338 = CARTESIAN_POINT ( 'NONE',  ( -23.15000000000000213, -4.356730526971941408, -226.1082375506050539 ) ) ;
#10339 = VERTEX_POINT ( 'NONE', #134267 ) ;
#10340 = CARTESIAN_POINT ( 'NONE',  ( 22.88900146558018989, 67.29609520889877672, -60.27310748452438816 ) ) ;
#10341 = CIRCLE ( 'NONE', #122774, 0.1000000000000124678 ) ;
#10342 = LINE ( 'NONE', #182892, #197938 ) ;
#10343 = TOROIDAL_SURFACE ( 'NONE', #51998, 4.149999999999999467, 0.1000000000000000056 ) ;
#10344 = CARTESIAN_POINT ( 'NONE',  ( 21.05000000000000071, 20.02733907826963033, -235.1395327601354666 ) ) ;
#10345 = CARTESIAN_POINT ( 'NONE',  ( -21.14999999999999858, 1.115600667400684642E-11, -26.95934304829875927 ) ) ;
#10347 = EDGE_CURVE ( 'NONE', #162149, #208880, #233416, .T. ) ;
#10346 = DIRECTION ( 'NONE',  ( 1.000000000000000000, -3.448943450116723568E-16, -6.438528483529607644E-16 ) ) ;
#10348 = AXIS2_PLACEMENT_3D ( 'NONE', #231308, #55177, #171365 ) ;
#10349 = EDGE_LOOP ( 'NONE', ( #1724, #177786, #186299, #7133 ) ) ;
#10351 = CARTESIAN_POINT ( 'NONE',  ( -23.39999999999994529, 79.78873604695631627, -7.297728304630792806 ) ) ;
#10350 = CARTESIAN_POINT ( 'NONE',  ( -23.25000000000000000, 4.250000000011156409, -88.15000000000004832 ) ) ;
#10352 = ORIENTED_EDGE ( 'NONE', *, *, #141677, .T. ) ;
#10355 = ORIENTED_EDGE ( 'NONE', *, *, #41256, .T. ) ;
#10354 = CARTESIAN_POINT ( 'NONE',  ( 22.59080734064468388, 64.25000000001215028, -136.5538571926214502 ) ) ;
#10353 = DIRECTION ( 'NONE',  ( 0.000000000000000000, -0.8814952561688439436, 0.4721928772777331806 ) ) ;
#10356 = CARTESIAN_POINT ( 'NONE',  ( 23.15000000000000213, 87.48912529308798014, -106.1231074845242262 ) ) ;
#10357 = AXIS2_PLACEMENT_3D ( 'NONE', #110072, #113923, #53950 ) ;
#10358 = PLANE ( 'NONE',  #111275 ) ;
#10359 = LINE ( 'NONE', #29930, #20961 ) ;
#10360 = CIRCLE ( 'NONE', #39593, 0.09999999999999939493 ) ;
#10361 = VERTEX_POINT ( 'NONE', #216386 ) ;
#10362 = CARTESIAN_POINT ( 'NONE',  ( -23.25000000000000000, -1.249999999988843369, -108.3004807544151191 ) ) ;
#10363 = DIRECTION ( 'NONE',  ( 0.000000000000000000, 1.000000000000000000, 6.982962677686266711E-15 ) ) ;
#10365 = CYLINDRICAL_SURFACE ( 'NONE', #167494, 4.049999999999998046 ) ;
#10364 = SPHERICAL_SURFACE ( 'NONE', #151715, 0.1000000000000000056 ) ;
#10367 = ORIENTED_EDGE ( 'NONE', *, *, #16329, .T. ) ;
#10366 = CARTESIAN_POINT ( 'NONE',  ( -20.94999999999999929, 70.22659352830977753, -197.9852579278363578 ) ) ;
#10368 = CIRCLE ( 'NONE', #156128, 0.09999999999999939493 ) ;
#10369 = CIRCLE ( 'NONE', #68039, 0.1000000000000028644 ) ;
#10370 = TOROIDAL_SURFACE ( 'NONE', #39611, 0.4000000000000003553, 0.1000000000000000056 ) ;
#10371 = ORIENTED_EDGE ( 'NONE', *, *, #232165, .T. ) ;
#10372 = CARTESIAN_POINT ( 'NONE',  ( -17.29838795458690015, 10.37154985796052920, -111.8952587173832427 ) ) ;
#10373 = CARTESIAN_POINT ( 'NONE',  ( 21.05000000000000071, -1.849084418615859926, -179.1560105214470866 ) ) ;
#10374 = DIRECTION ( 'NONE',  ( 1.000000000000000000, 0.000000000000000000, 0.000000000000000000 ) ) ;
#10375 = ORIENTED_EDGE ( 'NONE', *, *, #228913, .F. ) ;
#10376 = CARTESIAN_POINT ( 'NONE',  ( -16.77683809663752257, 9.945835743215303282, -188.3360509808957488 ) ) ;
#10377 = LINE ( 'NONE', #44677, #118131 ) ;
#10378 = CARTESIAN_POINT ( 'NONE',  ( -20.85000000000000142, 77.83585931145570669, -124.9186683157258244 ) ) ;
#10379 = AXIS2_PLACEMENT_3D ( 'NONE', #110944, #247885, #208774 ) ;
#10380 = VERTEX_POINT ( 'NONE', #211264 ) ;
#10381 = DIRECTION ( 'NONE',  ( 3.469446951953635015E-14, -0.000000000000000000, 1.000000000000000000 ) ) ;
#10382 = EDGE_CURVE ( 'NONE', #248456, #219674, #191730, .T. ) ;
#10383 = ORIENTED_EDGE ( 'NONE', *, *, #242915, .T. ) ;
#10384 = DIRECTION ( 'NONE',  ( 0.000000000000000000, 0.9126074666063813678, 0.4088369013363182813 ) ) ;
#10385 = CARTESIAN_POINT ( 'NONE',  ( -20.54999999999999716, 76.00000000001142553, -36.02310748452432421 ) ) ;
#10386 = AXIS2_PLACEMENT_3D ( 'NONE', #120163, #38043, #39326 ) ;
#10387 = ORIENTED_EDGE ( 'NONE', *, *, #241945, .F. ) ;
#10388 = ORIENTED_EDGE ( 'NONE', *, *, #110095, .T. ) ;
#10389 = EDGE_CURVE ( 'NONE', #64792, #189058, #200594, .T. ) ;
#10390 = ORIENTED_EDGE ( 'NONE', *, *, #120368, .T. ) ;
#10392 = ORIENTED_EDGE ( 'NONE', *, *, #185297, .F. ) ;
#10391 = FACE_OUTER_BOUND ( 'NONE', #232579, .T. ) ;
#10393 = ADVANCED_FACE ( 'NONE', ( #117298 ), #154839, .T. ) ;
#10394 = ORIENTED_EDGE ( 'NONE', *, *, #15881, .T. ) ;
#10397 = ORIENTED_EDGE ( 'NONE', *, *, #56143, .T. ) ;
#10396 = ORIENTED_EDGE ( 'NONE', *, *, #181239, .T. ) ;
#10395 = CARTESIAN_POINT ( 'NONE',  ( -21.14999999999999858, 11.65000000001115588, -134.1000000000000227 ) ) ;
#10398 = LINE ( 'NONE', #89908, #206368 ) ;
#10400 = EDGE_CURVE ( 'NONE', #155399, #104681, #196494, .T. ) ;
#10399 = ORIENTED_EDGE ( 'NONE', *, *, #32685, .F. ) ;
#10401 = FACE_OUTER_BOUND ( 'NONE', #93182, .T. ) ;
#10402 = DIRECTION ( 'NONE',  ( -1.000000000000000000, 0.000000000000000000, 0.000000000000000000 ) ) ;
#10403 = AXIS2_PLACEMENT_3D ( 'NONE', #191981, #212812, #95419 ) ;
#10404 = CARTESIAN_POINT ( 'NONE',  ( 23.14999999999998437, 1.115600667400684642E-11, -33.50000000000000000 ) ) ;
#10405 = CARTESIAN_POINT ( 'NONE',  ( -22.50875500270930019, 25.97741616883209659, -254.4468630028325435 ) ) ;
#10406 = ORIENTED_EDGE ( 'NONE', *, *, #146075, .F. ) ;
#10407 = EDGE_LOOP ( 'NONE', ( #105848, #211786, #79026, #81256 ) ) ;
#10408 = DIRECTION ( 'NONE',  ( 0.000000000000000000, 0.000000000000000000, -1.000000000000000000 ) ) ;
#10409 = AXIS2_PLACEMENT_3D ( 'NONE', #57363, #97761, #93937 ) ;
#10411 = ORIENTED_EDGE ( 'NONE', *, *, #225642, .F. ) ;
#10410 = CARTESIAN_POINT ( 'NONE',  ( 23.14999999999999858, 36.65892442174935439, -249.5511627012433848 ) ) ;
#10412 = CARTESIAN_POINT ( 'NONE',  ( -21.14999999999999858, 11.75000000001115552, -134.1000000000000227 ) ) ;
#10414 = ORIENTED_EDGE ( 'NONE', *, *, #1280, .F. ) ;
#10413 = DIRECTION ( 'NONE',  ( 0.000000000000000000, 0.8371762388950346745, 0.5469332180710581026 ) ) ;
#10415 = EDGE_CURVE ( 'NONE', #56261, #106243, #251666, .T. ) ;
#10416 = VERTEX_POINT ( 'NONE', #153909 ) ;
#10417 = CYLINDRICAL_SURFACE ( 'NONE', #33560, 0.1000000000000028644 ) ;
#10418 = ORIENTED_EDGE ( 'NONE', *, *, #159810, .F. ) ;
#10419 = CARTESIAN_POINT ( 'NONE',  ( -16.88783316861821859, 9.950000000011137047, -180.2522640419797426 ) ) ;
#10420 = CARTESIAN_POINT ( 'NONE',  ( 23.14999999999999858, 11.65000000001116298, -93.48519422934610645 ) ) ;
#10423 = VERTEX_POINT ( 'NONE', #133020 ) ;
#10422 = EDGE_LOOP ( 'NONE', ( #62459, #224548, #132059, #170278 ) ) ;
#10421 = CIRCLE ( 'NONE', #210339, 0.09999999999999939493 ) ;
#10424 = AXIS2_PLACEMENT_3D ( 'NONE', #193460, #14836, #108768 ) ;
#10425 = ORIENTED_EDGE ( 'NONE', *, *, #189400, .T. ) ;
#10426 = CARTESIAN_POINT ( 'NONE',  ( -18.37160782347004329, 13.18118307098499820, -207.5961113505749438 ) ) ;
#10427 = VERTEX_POINT ( 'NONE', #35226 ) ;
#10428 = ORIENTED_EDGE ( 'NONE', *, *, #90569, .T. ) ;
#10429 = DIRECTION ( 'NONE',  ( 1.000000000000000000, 0.000000000000000000, 0.000000000000000000 ) ) ;
#10431 = VERTEX_POINT ( 'NONE', #212560 ) ;
#10430 = CARTESIAN_POINT ( 'NONE',  ( 20.84999999999998721, 10.33248238083634440, -206.5948465439131496 ) ) ;
#10432 = CARTESIAN_POINT ( 'NONE',  ( -18.40000000000000213, 67.17743825834622839, -194.2731074845244166 ) ) ;
#10434 = DIRECTION ( 'NONE',  ( -3.469446951953635015E-14, -1.000000000000000000, 0.000000000000000000 ) ) ;
#10433 = DIRECTION ( 'NONE',  ( 0.000000000000000000, -6.608470384673558123E-15, 1.000000000000000000 ) ) ;
#10435 = DIRECTION ( 'NONE',  ( 1.000000000000000000, -7.304098846218134667E-16, -5.100424963727256530E-30 ) ) ;
#10436 = CARTESIAN_POINT ( 'NONE',  ( -14.77738660682463134, 62.09660346237241413, -218.7363060264989087 ) ) ;
#10437 = ORIENTED_EDGE ( 'NONE', *, *, #93816, .F. ) ;
#10438 = ORIENTED_EDGE ( 'NONE', *, *, #9019, .T. ) ;
#10439 = CARTESIAN_POINT ( 'NONE',  ( 23.15000000000000213, -8.596261682231828516, -57.54987248284972168 ) ) ;
#10440 = DIRECTION ( 'NONE',  ( 0.000000000000000000, -0.9229812358756199764, 0.3848449534832346086 ) ) ;
#10441 = CIRCLE ( 'NONE', #39680, 0.09999999999999939493 ) ;
#10442 = ORIENTED_EDGE ( 'NONE', *, *, #199545, .T. ) ;
#10443 = CIRCLE ( 'NONE', #247759, 0.1000000000000070832 ) ;
#10444 = AXIS2_PLACEMENT_3D ( 'NONE', #79101, #218616, #40034 ) ;
#10445 = VECTOR ( 'NONE', #9643, 1000.000000000000000 ) ;
#10446 = ADVANCED_FACE ( 'NONE', ( #93875 ), #114732, .F. ) ;
#10447 = DIRECTION ( 'NONE',  ( 1.000000000000000000, 0.000000000000000000, 0.000000000000000000 ) ) ;
#10448 = ORIENTED_EDGE ( 'NONE', *, *, #61513, .F. ) ;
#10449 = ORIENTED_EDGE ( 'NONE', *, *, #228397, .T. ) ;
#10450 = CARTESIAN_POINT ( 'NONE',  ( -23.25000000000000000, 64.35000000001195986, -103.0231074845244024 ) ) ;
#10451 = DIRECTION ( 'NONE',  ( 0.000000000000000000, -0.1568667991644863147, -0.9876197685951252359 ) ) ;
#10452 = ORIENTED_EDGE ( 'NONE', *, *, #172169, .F. ) ;
#10453 = CARTESIAN_POINT ( 'NONE',  ( -16.97683809663752186, 9.950000000011138823, -87.09763598180373378 ) ) ;
#10454 = ORIENTED_EDGE ( 'NONE', *, *, #177305, .T. ) ;
#10455 = CARTESIAN_POINT ( 'NONE',  ( -21.04999999999999361, 6.307425219576554554, -100.5168198683856957 ) ) ;
#10457 = EDGE_CURVE ( 'NONE', #24438, #60871, #113441, .T. ) ;
#10456 = DIRECTION ( 'NONE',  ( -0.000000000000000000, 1.000000000000000000, 6.982962677686266711E-15 ) ) ;
#10459 = CARTESIAN_POINT ( 'NONE',  ( 23.14999999999999503, 62.92003201576280702, -207.2439188921395612 ) ) ;
#10458 = CARTESIAN_POINT ( 'NONE',  ( -20.64999999999999858, 2.500000000011154633, -87.27537807723794572 ) ) ;
#10460 = CARTESIAN_POINT ( 'NONE',  ( 21.05000000000000071, 7.128833340094563376, -233.7327013124401276 ) ) ;
#10461 = CARTESIAN_POINT ( 'NONE',  ( -23.25000000000000000, 8.882751598337867094, -187.0399955572217721 ) ) ;
#10462 = DIRECTION ( 'NONE',  ( -1.000000000000000000, 0.000000000000000000, 0.000000000000000000 ) ) ;
#10463 = ADVANCED_FACE ( 'NONE', ( #252939 ), #16922, .F. ) ;
#10464 = ORIENTED_EDGE ( 'NONE', *, *, #42281, .F. ) ;
#10465 = AXIS2_PLACEMENT_3D ( 'NONE', #85688, #165266, #145689 ) ;
#10466 = AXIS2_PLACEMENT_3D ( 'NONE', #88634, #67811, #50792 ) ;
#10468 = ORIENTED_EDGE ( 'NONE', *, *, #240463, .F. ) ;
#10467 = ORIENTED_EDGE ( 'NONE', *, *, #101947, .F. ) ;
#10469 = ORIENTED_EDGE ( 'NONE', *, *, #86991, .T. ) ;
#10470 = AXIS2_PLACEMENT_3D ( 'NONE', #43935, #47765, #8662 ) ;
#10471 = LINE ( 'NONE', #226942, #57164 ) ;
#10472 = EDGE_CURVE ( 'NONE', #135828, #188180, #198113, .T. ) ;
#10473 = CARTESIAN_POINT ( 'NONE',  ( 18.59999999999999432, 1.162701749949165642, -108.6000000000000227 ) ) ;
#10475 = CARTESIAN_POINT ( 'NONE',  ( -22.48660254037843487, 11.75000000001115730, -33.45000000000001705 ) ) ;
#10474 = CARTESIAN_POINT ( 'NONE',  ( 20.94999999999999929, 70.60000000001200249, -115.4283735034374274 ) ) ;
#10476 = CARTESIAN_POINT ( 'NONE',  ( -20.85000000000000142, 7.128833340094563376, -233.7327013124401276 ) ) ;
#10477 = VERTEX_POINT ( 'NONE', #218952 ) ;
#10478 = AXIS2_PLACEMENT_3D ( 'NONE', #116448, #39507, #154332 ) ;
#10479 = EDGE_CURVE ( 'NONE', #46675, #12212, #101545, .T. ) ;
#10480 = DIRECTION ( 'NONE',  ( 0.000000000000000000, 0.9126074666063660468, 0.4088369013363524762 ) ) ;
#10481 = AXIS2_PLACEMENT_3D ( 'NONE', #23807, #241535, #158196 ) ;
#10482 = AXIS2_PLACEMENT_3D ( 'NONE', #113974, #130983, #248364 ) ;
#10483 = ORIENTED_EDGE ( 'NONE', *, *, #16578, .F. ) ;
#10484 = FACE_OUTER_BOUND ( 'NONE', #49736, .T. ) ;
#10485 = CARTESIAN_POINT ( 'NONE',  ( -22.50000000000000000, 0.09263750062063533242, -88.85030279295926903 ) ) ;
#10486 = DIRECTION ( 'NONE',  ( 0.000000000000000000, 1.000000000000000000, 0.000000000000000000 ) ) ;
#10487 = ORIENTED_EDGE ( 'NONE', *, *, #171813, .T. ) ;
#10488 = LINE ( 'NONE', #110861, #152418 ) ;
#10489 = EDGE_CURVE ( 'NONE', #48255, #43270, #67494, .T. ) ;
#10490 = CIRCLE ( 'NONE', #164608, 0.1000000000000124678 ) ;
#10491 = DIRECTION ( 'NONE',  ( -1.000000000000000000, -0.000000000000000000, -0.000000000000000000 ) ) ;
#10492 = ORIENTED_EDGE ( 'NONE', *, *, #165815, .F. ) ;
#10493 = ORIENTED_EDGE ( 'NONE', *, *, #117634, .F. ) ;
#10494 = CARTESIAN_POINT ( 'NONE',  ( -16.87665923198281348, 9.950000000011138823, -54.35000000000000142 ) ) ;
#10495 = AXIS2_PLACEMENT_3D ( 'NONE', #120614, #99710, #159724 ) ;
#10496 = CARTESIAN_POINT ( 'NONE',  ( -16.89318236219976299, 9.951535257886286345, -54.35512963210585724 ) ) ;
#10497 = CARTESIAN_POINT ( 'NONE',  ( 23.24999999999999289, 64.35000000001186038, -90.87310748452438247 ) ) ;
#10498 = EDGE_CURVE ( 'NONE', #83068, #94181, #118599, .T. ) ;
#10499 = CARTESIAN_POINT ( 'NONE',  ( -21.14999999999999858, -0.09999999998884338825, -60.75000000000004974 ) ) ;
#10500 = CARTESIAN_POINT ( 'NONE',  ( -21.05000000000000071, 40.58313652815211015, -247.7931640254992658 ) ) ;
#10501 = EDGE_CURVE ( 'NONE', #197779, #144144, #159111, .T. ) ;
#10502 = AXIS2_PLACEMENT_3D ( 'NONE', #71961, #8133, #129353 ) ;
#10503 = CARTESIAN_POINT ( 'NONE',  ( -18.40000000000000213, 11.47316190336247388, -12.65000000000000213 ) ) ;
#10505 = ORIENTED_EDGE ( 'NONE', *, *, #102097, .T. ) ;
#10504 = AXIS2_PLACEMENT_3D ( 'NONE', #225161, #68689, #46533 ) ;
#10506 = DIRECTION ( 'NONE',  ( 0.000000000000000000, 0.000000000000000000, -1.000000000000000000 ) ) ;
#10507 = CARTESIAN_POINT ( 'NONE',  ( -20.64999999999999858, -4.161311414658873886, -226.0656773515597706 ) ) ;
#10509 = FACE_OUTER_BOUND ( 'NONE', #170313, .T. ) ;
#10508 = DIRECTION ( 'NONE',  ( 0.000000000000000000, -0.9908441862701605762, 0.1350103645451835310 ) ) ;
#10510 = DIRECTION ( 'NONE',  ( 1.000000000000000000, -0.000000000000000000, 0.000000000000000000 ) ) ;
#10511 = CARTESIAN_POINT ( 'NONE',  ( -18.50000000000000000, -9.400000000000005684, -7.297259759663287326 ) ) ;
#10512 = CYLINDRICAL_SURFACE ( 'NONE', #249566, 0.09999999999999939493 ) ;
#10513 = DIRECTION ( 'NONE',  ( 0.000000000000000000, -0.9876197685951265681, -0.1568667991644790149 ) ) ;
#10515 = ORIENTED_EDGE ( 'NONE', *, *, #132208, .F. ) ;
#10514 = CARTESIAN_POINT ( 'NONE',  ( 21.07016717457009847, 30.89038661691666121, -252.1353965670249977 ) ) ;
#10516 = B_SPLINE_CURVE_WITH_KNOTS ( 'NONE', 3,
 ( #138293, #255649, #57476, #159194 ),
 .UNSPECIFIED., .F., .F.,
 ( 4, 4 ),
 ( 0.000000000000000000, 0.001767853679387106471 ),
 .UNSPECIFIED. ) ;
#10517 = EDGE_CURVE ( 'NONE', #189423, #109416, #184197, .T. ) ;
#10518 = EDGE_CURVE ( 'NONE', #235552, #246027, #79430, .T. ) ;
#10520 = CIRCLE ( 'NONE', #43828, 2.099999999999990763 ) ;
#10519 = CARTESIAN_POINT ( 'NONE',  ( -6.000000000000002665, -11.65000000000000036, 13.90000000000000213 ) ) ;
#10521 = CIRCLE ( 'NONE', #131299, 4.099999999999986322 ) ;
#10522 = EDGE_CURVE ( 'NONE', #103860, #242379, #88313, .T. ) ;
#10523 = FACE_OUTER_BOUND ( 'NONE', #84759, .T. ) ;
#10524 = AXIS2_PLACEMENT_3D ( 'NONE', #231963, #248951, #70336 ) ;
#10525 = CYLINDRICAL_SURFACE ( 'NONE', #200423, 0.09999999999999939493 ) ;
#10526 = ORIENTED_EDGE ( 'NONE', *, *, #29726, .F. ) ;
#10527 = FACE_OUTER_BOUND ( 'NONE', #60589, .T. ) ;
#10528 = DIRECTION ( 'NONE',  ( -1.000000000000000000, 0.000000000000000000, 0.000000000000000000 ) ) ;
#10529 = LINE ( 'NONE', #164464, #181981 ) ;
#10530 = AXIS2_PLACEMENT_3D ( 'NONE', #14551, #54916, #130617 ) ;
#10531 = AXIS2_PLACEMENT_3D ( 'NONE', #107999, #243653, #225355 ) ;
#10532 = ORIENTED_EDGE ( 'NONE', *, *, #18022, .F. ) ;
#10533 = CARTESIAN_POINT ( 'NONE',  ( -16.93388492042258875, 66.01145817749568323, -56.92365260771056512 ) ) ;
#10535 = ORIENTED_EDGE ( 'NONE', *, *, #241272, .T. ) ;
#10534 = CARTESIAN_POINT ( 'NONE',  ( 21.33487959338958717, 69.27444184810119054, -170.0231074845243882 ) ) ;
#10536 = CARTESIAN_POINT ( 'NONE',  ( 21.05000000000000071, 1.115600667400684642E-11, -134.0000000000000284 ) ) ;
#10537 =( BOUNDED_SURFACE ( )  B_SPLINE_SURFACE ( 3, 2, ( 
 ( #56585, #158328, #116599 ),
 ( #196136, #17489, #137425 ),
 ( #237829, #96990, #179170 ),
 ( #176593, #256046, #198699 ) ),
 .UNSPECIFIED., .F., .F., .F. ) 
 B_SPLINE_SURFACE_WITH_KNOTS ( ( 4, 4 ),
 ( 3, 3 ),
 ( 0.0008258556059633759532, 0.0009616864997632702718 ),
 ( 0.000000000000000000, 1.000000000000000000 ),
 .UNSPECIFIED. ) 
 GEOMETRIC_REPRESENTATION_ITEM ( )  RATIONAL_B_SPLINE_SURFACE ( (
 ( 1.000000000000000000, 0.9152888060719485130, 1.000000000000000000),
 ( 1.000000000000000000, 0.9327727094138529296, 1.000000000000000000),
 ( 1.000000000000000000, 0.9369023509257985438, 1.000000000000000000),
 ( 1.000000000000000000, 0.9246339933864583527, 1.000000000000000000) ) ) 
 REPRESENTATION_ITEM ( '' )  SURFACE ( )  );
#10538 = CARTESIAN_POINT ( 'NONE',  ( -18.59999999999999787, 43.30036367478129478, -245.0872390055602352 ) ) ;
#10539 = ORIENTED_EDGE ( 'NONE', *, *, #17937, .T. ) ;
#10540 = DIRECTION ( 'NONE',  ( -0.000000000000000000, 0.000000000000000000, 1.000000000000000000 ) ) ;
#10541 = VECTOR ( 'NONE', #246208, 1000.000000000000000 ) ;
#10542 = EDGE_CURVE ( 'NONE', #19242, #9008, #21728, .T. ) ;
#10543 = APPLICATION_PROTOCOL_DEFINITION ( 'draft international standard', 'automotive_design', 1998, #43997 ) ;
#10544 = DIRECTION ( 'NONE',  ( 0.000000000000000000, 0.9915357197604971473, -0.1298341882519111479 ) ) ;
#10545 = LINE ( 'NONE', #47071, #135740 ) ;
#10546 = FACE_OUTER_BOUND ( 'NONE', #53696, .T. ) ;
#10547 = VECTOR ( 'NONE', #14070, 1000.000000000000000 ) ;
#10548 = EDGE_LOOP ( 'NONE', ( #74657, #89380, #187565, #217233 ) ) ;
#10550 = ADVANCED_FACE ( 'NONE', ( #39064 ), #163375, .T. ) ;
#10549 = DIRECTION ( 'NONE',  ( 1.000000000000000000, 0.000000000000000000, 0.000000000000000000 ) ) ;
#10551 = CARTESIAN_POINT ( 'NONE',  ( 21.05000000000000071, 87.48912529308798014, -106.1231074845242262 ) ) ;
#10552 = EDGE_CURVE ( 'NONE', #17815, #161815, #1301, .T. ) ;
#10553 = EDGE_CURVE ( 'NONE', #71337, #28028, #71806, .T. ) ;
#10554 = CARTESIAN_POINT ( 'NONE',  ( 23.15000000000000213, 69.09936979046463534, -247.6075824278584605 ) ) ;
#10555 = ORIENTED_EDGE ( 'NONE', *, *, #237569, .T. ) ;
#10556 = AXIS2_PLACEMENT_3D ( 'NONE', #112687, #51384, #150532 ) ;
#10557 = ORIENTED_EDGE ( 'NONE', *, *, #81410, .T. ) ;
#10558 = EDGE_CURVE ( 'NONE', #81073, #127304, #80712, .T. ) ;
#10559 = CARTESIAN_POINT ( 'NONE',  ( -23.15000000000000213, 5.354661166737471056, -213.3684367965233832 ) ) ;
#10560 = CARTESIAN_POINT ( 'NONE',  ( -22.24259225415828567, 68.50806212944651463, -103.1221733679771972 ) ) ;
#10561 = FACE_OUTER_BOUND ( 'NONE', #203084, .T. ) ;
#10562 = B_SPLINE_CURVE_WITH_KNOTS ( 'NONE', 3,
 ( #188506, #206791, #28186, #247187, #148105, #244622, #88090, #9868, #227623, #48992, #128537, #110247, #134918, #51527, #91968, #33327, #189798, #11157, #90679 ),
 .UNSPECIFIED., .F., .F.,
 ( 4, 3, 3, 3, 3, 3, 4 ),
 ( -2.000416914645579387E-06, 4.235164736271501695E-22, 4.714008503743245793E-05, 9.979203887776031420E-05, 0.0001372215519229365321, 0.0001635031576220883785, 0.0001900083748504048946 ),
 .UNSPECIFIED. ) ;
#10563 = DIRECTION ( 'NONE',  ( 1.000000000000000000, 0.000000000000000000, 0.000000000000000000 ) ) ;
#10565 = DIRECTION ( 'NONE',  ( -1.000000000000000000, 0.000000000000000000, 0.000000000000000000 ) ) ;
#10564 = PLANE ( 'NONE',  #144981 ) ;
#10566 = CARTESIAN_POINT ( 'NONE',  ( -21.11101077989000174, 75.98471473109815122, -176.4467922192504830 ) ) ;
#10567 = DIRECTION ( 'NONE',  ( -0.000000000000000000, -6.982962677686266711E-15, 1.000000000000000000 ) ) ;
#10568 = ORIENTED_EDGE ( 'NONE', *, *, #116948, .F. ) ;
#10569 = AXIS2_PLACEMENT_3D ( 'NONE', #141584, #2057, #222374 ) ;
#10570 = EDGE_CURVE ( 'NONE', #120408, #214743, #197125, .T. ) ;
#10572 = EDGE_LOOP ( 'NONE', ( #235321, #69640, #203389 ) ) ;
#10571 = CARTESIAN_POINT ( 'NONE',  ( 12.26145404764308644, 62.65055472571233253, -217.0190438104122279 ) ) ;
#10573 = AXIS2_PLACEMENT_3D ( 'NONE', #124463, #149175, #170049 ) ;
#10574 = EDGE_CURVE ( 'NONE', #153112, #123515, #3765, .T. ) ;
#10575 = DIRECTION ( 'NONE',  ( 0.000000000000000000, 0.2617529984165031243, 0.9651348961777157509 ) ) ;
#10577 = DIRECTION ( 'NONE',  ( -0.000000000000000000, 1.000000000000000000, 6.982962677686266711E-15 ) ) ;
#10576 = DIRECTION ( 'NONE',  ( -1.000000000000000000, 0.000000000000000000, 0.000000000000000000 ) ) ;
#10578 = ORIENTED_EDGE ( 'NONE', *, *, #72708, .F. ) ;
#10579 = CARTESIAN_POINT ( 'NONE',  ( -23.25000000000000000, 2.000000000011154189, -154.2753780772379173 ) ) ;
#10581 = EDGE_CURVE ( 'NONE', #216036, #53024, #100773, .T. ) ;
#10580 = DIRECTION ( 'NONE',  ( -1.000000000000000000, -0.000000000000000000, -0.000000000000000000 ) ) ;
#10582 = CARTESIAN_POINT ( 'NONE',  ( -21.13435531349793450, 69.50627893641963340, -103.0231074845243597 ) ) ;
#10583 = CARTESIAN_POINT ( 'NONE',  ( 20.94999999999999929, 1.148907358139439339E-11, -201.0000000000015064 ) ) ;
#10584 = ORIENTED_EDGE ( 'NONE', *, *, #25542, .F. ) ;
#10585 = ORIENTED_EDGE ( 'NONE', *, *, #93281, .T. ) ;
#10586 = PLANE ( 'NONE',  #92765 ) ;
#10587 = ORIENTED_EDGE ( 'NONE', *, *, #253546, .T. ) ;
#10588 = DIRECTION ( 'NONE',  ( 1.000000000000000000, 0.000000000000000000, -0.000000000000000000 ) ) ;
#10589 = EDGE_CURVE ( 'NONE', #6520, #156141, #46630, .T. ) ;
#10590 = CIRCLE ( 'NONE', #14703, 0.1000000000000028644 ) ;
#10591 = FACE_OUTER_BOUND ( 'NONE', #68698, .T. ) ;
#10592 = CARTESIAN_POINT ( 'NONE',  ( 20.94999999999999929, 61.95000000001146390, -41.53680255528533394 ) ) ;
#10593 = ADVANCED_FACE ( 'NONE', ( #108005 ), #238183, .F. ) ;
#10594 = AXIS2_PLACEMENT_3D ( 'NONE', #92345, #75385, #117054 ) ;
#10595 = DIRECTION ( 'NONE',  ( 1.000000000000000000, 0.000000000000000000, 0.000000000000000000 ) ) ;
#10596 = ORIENTED_EDGE ( 'NONE', *, *, #98462, .F. ) ;
#10597 = EDGE_CURVE ( 'NONE', #156110, #57467, #144544, .T. ) ;
#10598 = DIRECTION ( 'NONE',  ( 0.000000000000000000, 0.000000000000000000, 1.000000000000000000 ) ) ;
#10599 = ADVANCED_FACE ( 'NONE', ( #207112 ), #169302, .F. ) ;
#10600 = CARTESIAN_POINT ( 'NONE',  ( 21.05000000000000071, -3.770473190032740174, -225.9805569534692324 ) ) ;
#10601 = DIRECTION ( 'NONE',  ( 0.000000000000000000, 0.000000000000000000, -1.000000000000000000 ) ) ;
#10602 = DIRECTION ( 'NONE',  ( -2.561896900575096011E-15, 0.5907332058517336115, -0.8068669527896984439 ) ) ;
#10603 = DIRECTION ( 'NONE',  ( -1.000000000000000000, 0.000000000000000000, 0.000000000000000000 ) ) ;
#10604 = CARTESIAN_POINT ( 'NONE',  ( -16.92280123533733871, 66.05000000001224691, -149.3737397986104725 ) ) ;
#10605 = VERTEX_POINT ( 'NONE', #5019 ) ;
#10607 = CARTESIAN_POINT ( 'NONE',  ( -22.59999999999999787, 12.54152817314149715, -223.4164406214577241 ) ) ;
#10606 = CARTESIAN_POINT ( 'NONE',  ( -17.11825945287482753, 10.04999999999998295, -12.65000000000000213 ) ) ;
#10608 = ORIENTED_EDGE ( 'NONE', *, *, #98569, .F. ) ;
#10610 = EDGE_LOOP ( 'NONE', ( #69076, #190839, #236443, #253146 ) ) ;
#10609 = CARTESIAN_POINT ( 'NONE',  ( -21.05000000000000071, 76.00000000001210765, -132.2231074845243199 ) ) ;
#10611 = CIRCLE ( 'NONE', #252014, 11.65000000000000036 ) ;
#10612 = EDGE_LOOP ( 'NONE', ( #250563, #91895, #37354, #185187 ) ) ;
#10613 = CIRCLE ( 'NONE', #156377, 12.87500000000000000 ) ;
#10614 = DIRECTION ( 'NONE',  ( -0.000000000000000000, -0.000000000000000000, 1.000000000000000000 ) ) ;
#10615 = LINE ( 'NONE', #190552, #18106 ) ;
#10616 = CARTESIAN_POINT ( 'NONE',  ( -23.15000000000000213, 68.76258920191057200, -222.5680764032308048 ) ) ;
#10617 = ORIENTED_EDGE ( 'NONE', *, *, #69149, .F. ) ;
#10618 = EDGE_CURVE ( 'NONE', #126382, #71039, #25909, .T. ) ;
#10619 = DIRECTION ( 'NONE',  ( 0.000000000000000000, 0.000000000000000000, 1.000000000000000000 ) ) ;
#10620 = CARTESIAN_POINT ( 'NONE',  ( 23.14999999999999858, 1.115600667400684642E-11, -134.0000000000000284 ) ) ;
#10621 = ORIENTED_EDGE ( 'NONE', *, *, #251969, .F. ) ;
#10622 = CARTESIAN_POINT ( 'NONE',  ( 18.39999999999999858, -9.519327731081279609, -174.4729763765593020 ) ) ;
#10623 = EDGE_CURVE ( 'NONE', #118177, #66589, #162983, .T. ) ;
#10625 = CIRCLE ( 'NONE', #214605, 0.09999999999999868716 ) ;
#10624 = CARTESIAN_POINT ( 'NONE',  ( 21.05000000000000071, 76.00000000001165290, -69.52310748452431710 ) ) ;
#10626 = ORIENTED_EDGE ( 'NONE', *, *, #175711, .T. ) ;
#10628 = FACE_OUTER_BOUND ( 'NONE', #51728, .T. ) ;
#10627 = AXIS2_PLACEMENT_3D ( 'NONE', #102644, #3567, #123528 ) ;
#10629 = TOROIDAL_SURFACE ( 'NONE', #131417, 0.2000000000000000111, 0.1000000000000000056 ) ;
#10630 = ORIENTED_EDGE ( 'NONE', *, *, #85599, .T. ) ;
#10631 = FACE_OUTER_BOUND ( 'NONE', #104856, .T. ) ;
#10632 = VERTEX_POINT ( 'NONE', #225361 ) ;
#10633 = CARTESIAN_POINT ( 'NONE',  ( -23.25000000000000000, 74.93036000061670165, -233.6816308724374949 ) ) ;
#10634 =( BOUNDED_SURFACE ( )  B_SPLINE_SURFACE ( 3, 2, ( 
 ( #77020, #156607, #9674 ),
 ( #236099, #155317, #188308 ),
 ( #56163, #74507, #136999 ),
 ( #216535, #248290, #69673 ),
 ( #213979, #129628, #212701 ),
 ( #34092, #15805, #95309 ) ),
 .UNSPECIFIED., .F., .F., .F. ) 
 B_SPLINE_SURFACE_WITH_KNOTS ( ( 4, 2, 4 ),
 ( 3, 3 ),
 ( 0.0001342700090130055928, 0.0002909192928057414561, 0.0004475685765984773194 ),
 ( 0.000000000000000000, 1.000000000000000000 ),
 .UNSPECIFIED. ) 
 GEOMETRIC_REPRESENTATION_ITEM ( )  RATIONAL_B_SPLINE_SURFACE ( (
 ( 1.000000000000000000, 0.7250110520819893489, 1.000000000000000000),
 ( 1.000000000000000000, 0.7257599279128809089, 1.000000000000000000),
 ( 1.000000000000000000, 0.7137594617291853627, 1.000000000000000000),
 ( 1.000000000000000000, 0.6959270178800760487, 1.000000000000000000),
 ( 1.000000000000000000, 0.6919879549345794301, 1.000000000000000000),
 ( 1.000000000000000000, 0.7071067811865708874, 1.000000000000000000) ) ) 
 REPRESENTATION_ITEM ( '' )  SURFACE ( )  );
#10635 = EDGE_CURVE ( 'NONE', #116446, #205515, #839, .T. ) ;
#10636 = CARTESIAN_POINT ( 'NONE',  ( -20.94999999999999929, 87.24382154048164750, -206.5725299160771726 ) ) ;
#10637 = DIRECTION ( 'NONE',  ( 0.000000000000000000, 0.000000000000000000, 1.000000000000000000 ) ) ;
#10638 = DIRECTION ( 'NONE',  ( 0.000000000000000000, 1.000000000000000000, 0.000000000000000000 ) ) ;
#10639 = CARTESIAN_POINT ( 'NONE',  ( -18.50000000000000000, 77.86671491006937629, -124.7704322382422788 ) ) ;
#10641 = EDGE_CURVE ( 'NONE', #121863, #251542, #184971, .T. ) ;
#10640 = PLANE ( 'NONE',  #230559 ) ;
#10642 = EDGE_LOOP ( 'NONE', ( #36682, #37007, #14049, #89140 ) ) ;
#10643 = DIRECTION ( 'NONE',  ( -1.000000000000000000, -0.000000000000000000, 0.000000000000000000 ) ) ;
#10644 = AXIS2_PLACEMENT_3D ( 'NONE', #107855, #44040, #205663 ) ;
#10645 = ORIENTED_EDGE ( 'NONE', *, *, #85169, .T. ) ;
#10647 = CARTESIAN_POINT ( 'NONE',  ( 21.14999999999999858, 31.98723526783714988, -238.8784020251475511 ) ) ;
#10646 = CARTESIAN_POINT ( 'NONE',  ( -21.05000000000000071, 36.65892442174472876, -249.5511627012454596 ) ) ;
#10648 = STYLED_ITEM ( 'NONE', ( #72664 ), #85670 ) ;
#10649 = ORIENTED_EDGE ( 'NONE', *, *, #257353, .F. ) ;
#10650 = DIRECTION ( 'NONE',  ( 1.000000000000000000, 2.952720810173289112E-16, -0.000000000000000000 ) ) ;
#10651 = AXIS2_PLACEMENT_3D ( 'NONE', #132849, #69031, #11622 ) ;
#10652 = CARTESIAN_POINT ( 'NONE',  ( -23.25000000000000000, 2.600000000011156054, -180.7246219227620543 ) ) ;
#10653 = FACE_OUTER_BOUND ( 'NONE', #241380, .T. ) ;
#10654 = ORIENTED_EDGE ( 'NONE', *, *, #169233, .T. ) ;
#10656 = ORIENTED_EDGE ( 'NONE', *, *, #117554, .F. ) ;
#10655 = LINE ( 'NONE', #90162, #187155 ) ;
#10657 = CIRCLE ( 'NONE', #189708, 0.1000000000000043771 ) ;
#10658 = DIRECTION ( 'NONE',  ( 0.000000000000000000, 0.2617529984165152257, 0.9651348961777124202 ) ) ;
#10659 = VECTOR ( 'NONE', #122565, 1000.000000000000000 ) ;
#10661 = CARTESIAN_POINT ( 'NONE',  ( 20.94999999999999574, 44.55458850188623643, -247.3966190010231969 ) ) ;
#10660 = CARTESIAN_POINT ( 'NONE',  ( -21.05000000000000071, 76.10000000001222986, -148.1731074845243086 ) ) ;
#10662 = VECTOR ( 'NONE', #83402, 1000.000000000000000 ) ;
#10663 = CIRCLE ( 'NONE', #52326, 0.09999999999999942268 ) ;
#10665 = ORIENTED_EDGE ( 'NONE', *, *, #66559, .F. ) ;
#10664 = CARTESIAN_POINT ( 'NONE',  ( -20.54999999999999716, 71.65000000001151648, -48.27310748452435263 ) ) ;
#10666 = ORIENTED_EDGE ( 'NONE', *, *, #188114, .T. ) ;
#10667 = CARTESIAN_POINT ( 'NONE',  ( -20.05000000000000426, 66.75000000001151079, -48.37310748452438247 ) ) ;
#10668 = AXIS2_PLACEMENT_3D ( 'NONE', #27103, #244820, #66201 ) ;
#10669 = CARTESIAN_POINT ( 'NONE',  ( 23.14999999999999503, 6.650000000011155876, -54.65000000000000568 ) ) ;
#10670 = ORIENTED_EDGE ( 'NONE', *, *, #249757, .F. ) ;
#10671 = CARTESIAN_POINT ( 'NONE',  ( 21.00000000000000000, 8.000000000000000000, 1.212568896937007867 ) ) ;
#10672 = ORIENTED_EDGE ( 'NONE', *, *, #144014, .T. ) ;
#10673 = AXIS2_PLACEMENT_3D ( 'NONE', #42148, #121689, #201201 ) ;
#10674 = CARTESIAN_POINT ( 'NONE',  ( 23.14999999999998437, 63.32247822353865985, -234.7950268628915467 ) ) ;
#10675 = LINE ( 'NONE', #13251, #147443 ) ;
#10676 = AXIS2_PLACEMENT_3D ( 'NONE', #98726, #217413, #235703 ) ;
#10678 = EDGE_LOOP ( 'NONE', ( #225231, #146612, #68127, #21308 ) ) ;
#10677 = AXIS2_PLACEMENT_3D ( 'NONE', #159787, #121940, #60652 ) ;
#10679 = FACE_OUTER_BOUND ( 'NONE', #136746, .T. ) ;
#10680 = EDGE_CURVE ( 'NONE', #237092, #170195, #221597, .T. ) ;
#10681 = VERTEX_POINT ( 'NONE', #148423 ) ;
#10682 = CARTESIAN_POINT ( 'NONE',  ( 21.07933241753356768, 6.163820597116702160, -199.5620170604115344 ) ) ;
#10683 = ORIENTED_EDGE ( 'NONE', *, *, #128582, .F. ) ;
#10684 = ORIENTED_EDGE ( 'NONE', *, *, #9405, .T. ) ;
#10685 = CARTESIAN_POINT ( 'NONE',  ( -21.05000000000001847, 61.10390814609986165, -234.2085808482629261 ) ) ;
#10686 = VERTEX_POINT ( 'NONE', #128861 ) ;
#10687 = EDGE_CURVE ( 'NONE', #31646, #120408, #204860, .T. ) ;
#10688 = LINE ( 'NONE', #249310, #242045 ) ;
#10689 = VERTEX_POINT ( 'NONE', #208408 ) ;
#10691 = EDGE_LOOP ( 'NONE', ( #194173, #209080, #62755, #235627 ) ) ;
#10690 = DIRECTION ( 'NONE',  ( 1.000000000000000000, 0.000000000000000000, 0.000000000000000000 ) ) ;
#10692 = EDGE_CURVE ( 'NONE', #239952, #144728, #246559, .T. ) ;
#10693 = ORIENTED_EDGE ( 'NONE', *, *, #3630, .F. ) ;
#10694 = VECTOR ( 'NONE', #156608, 1000.000000000000000 ) ;
#10695 = DIRECTION ( 'NONE',  ( 0.000000000000000000, 1.000000000000000000, 7.116814260417668513E-15 ) ) ;
#10696 = ORIENTED_EDGE ( 'NONE', *, *, #22250, .T. ) ;
#10697 = CIRCLE ( 'NONE', #177326, 0.1000000000000070832 ) ;
#10700 = ORIENTED_EDGE ( 'NONE', *, *, #28842, .F. ) ;
#10699 = ORIENTED_EDGE ( 'NONE', *, *, #10821, .T. ) ;
#10698 = DIRECTION ( 'NONE',  ( 0.000000000000000000, 0.2128009952263609783, -0.9770955615653315052 ) ) ;
#10701 = LINE ( 'NONE', #69403, #173796 ) ;
#10702 = AXIS2_PLACEMENT_3D ( 'NONE', #109098, #170426, #249911 ) ;
#10703 = CARTESIAN_POINT ( 'NONE',  ( 21.05000000000000071, 13.50240476722978933, -238.5648941131444474 ) ) ;
#10705 = EDGE_CURVE ( 'NONE', #56702, #126714, #27215, .T. ) ;
#10704 = VERTEX_POINT ( 'NONE', #66312 ) ;
#10706 = CIRCLE ( 'NONE', #231293, 0.09999999999998898659 ) ;
#10707 = EDGE_CURVE ( 'NONE', #72992, #4098, #146587, .T. ) ;
#10708 = ORIENTED_EDGE ( 'NONE', *, *, #89086, .T. ) ;
#10709 = FACE_OUTER_BOUND ( 'NONE', #214046, .T. ) ;
#10711 = ORIENTED_EDGE ( 'NONE', *, *, #194735, .F. ) ;
#10710 = CARTESIAN_POINT ( 'NONE',  ( 23.14999999999999858, 5.000000000011153745, -155.0947339810869323 ) ) ;
#10712 = DIRECTION ( 'NONE',  ( 0.000000000000000000, -0.8814952561688431665, 0.4721928772777346794 ) ) ;
#10713 = VERTEX_POINT ( 'NONE', #203247 ) ;
#10714 = EDGE_CURVE ( 'NONE', #22319, #203751, #192406, .T. ) ;
#10715 = FACE_OUTER_BOUND ( 'NONE', #170032, .T. ) ;
#10716 = DIRECTION ( 'NONE',  ( 2.952720810173289605E-16, -0.9770955615653318382, -0.2128009952263588411 ) ) ;
#10717 = AXIS2_PLACEMENT_3D ( 'NONE', #34891, #111837, #15314 ) ;
#10718 = VERTEX_POINT ( 'NONE', #246233 ) ;
#10719 = DIRECTION ( 'NONE',  ( 2.952720810173289112E-16, -1.000000000000000000, 0.000000000000000000 ) ) ;
#10720 = DIRECTION ( 'NONE',  ( -1.000000000000000000, 2.952720810173289112E-16, 2.061873921506763405E-30 ) ) ;
#10721 = EDGE_CURVE ( 'NONE', #137100, #132943, #226651, .T. ) ;
#10722 = AXIS2_PLACEMENT_3D ( 'NONE', #97401, #238224, #15355 ) ;
#10723 = ORIENTED_EDGE ( 'NONE', *, *, #192563, .F. ) ;
#10725 = ORIENTED_EDGE ( 'NONE', *, *, #255545, .F. ) ;
#10724 = CARTESIAN_POINT ( 'NONE',  ( 19.83283456528358002, 54.53338637568176495, -228.6684279706500433 ) ) ;
#10726 = DIRECTION ( 'NONE',  ( -0.000000000000000000, 0.8700118002898356018, -0.4930308989875170078 ) ) ;
#10728 = ORIENTED_EDGE ( 'NONE', *, *, #60768, .T. ) ;
#10727 = ORIENTED_EDGE ( 'NONE', *, *, #5967, .T. ) ;
#10729 = ORIENTED_EDGE ( 'NONE', *, *, #175671, .T. ) ;
#10730 = DIRECTION ( 'NONE',  ( 1.000000000000000000, 0.000000000000000000, 0.000000000000000000 ) ) ;
#10731 = ORIENTED_EDGE ( 'NONE', *, *, #15932, .T. ) ;
#10732 = EDGE_LOOP ( 'NONE', ( #38691, #25118, #57792, #84019 ) ) ;
#10733 = LINE ( 'NONE', #71998, #225700 ) ;
#10734 = AXIS2_PLACEMENT_3D ( 'NONE', #195469, #156349, #234563 ) ;
#10735 = VERTEX_POINT ( 'NONE', #193971 ) ;
#10736 = DIRECTION ( 'NONE',  ( 0.000000000000000000, 0.000000000000000000, -1.000000000000000000 ) ) ;
#10737 = LINE ( 'NONE', #88963, #239933 ) ;
#10738 = EDGE_CURVE ( 'NONE', #207975, #40042, #179945, .T. ) ;
#10739 = ORIENTED_EDGE ( 'NONE', *, *, #7213, .F. ) ;
#10740 = ORIENTED_EDGE ( 'NONE', *, *, #158069, .F. ) ;
#10741 = DIRECTION ( 'NONE',  ( -1.000000000000000000, -1.836970198721029934E-16, -3.186635328391151676E-31 ) ) ;
#10742 = EDGE_LOOP ( 'NONE', ( #73469, #51688, #92656, #252088 ) ) ;
#10743 = CIRCLE ( 'NONE', #256371, 0.8750000000000007772 ) ;
#10744 = AXIS2_PLACEMENT_3D ( 'NONE', #257988, #97658, #41590 ) ;
#10745 = AXIS2_PLACEMENT_3D ( 'NONE', #101978, #179022, #2893 ) ;
#10746 = AXIS2_PLACEMENT_3D ( 'NONE', #152283, #191418, #231811 ) ;
#10747 = EDGE_CURVE ( 'NONE', #51386, #142612, #234085, .T. ) ;
#10748 = DIRECTION ( 'NONE',  ( 1.000000000000000000, 0.000000000000000000, -0.000000000000000000 ) ) ;
#10749 = ORIENTED_EDGE ( 'NONE', *, *, #187916, .F. ) ;
#10750 = CARTESIAN_POINT ( 'NONE',  ( 22.57856590037848932, -0.004128330053175053270, -122.2499415373245739 ) ) ;
#10751 = VERTEX_POINT ( 'NONE', #153600 ) ;
#10752 = DIRECTION ( 'NONE',  ( 0.000000000000000000, -8.267618268485210697E-15, 1.000000000000000000 ) ) ;
#10753 = CARTESIAN_POINT ( 'NONE',  ( 15.48841904831874849, 29.55072697483408817, -236.0309298094674944 ) ) ;
#10754 = CARTESIAN_POINT ( 'NONE',  ( 18.52928932188134326, 33.71149860592453251, -236.3111109633100000 ) ) ;
#10755 = CARTESIAN_POINT ( 'NONE',  ( -22.50000000000000000, 7.790779598384560245, -167.3999999999999773 ) ) ;
#10756 = CARTESIAN_POINT ( 'NONE',  ( -16.87851181299898684, 66.04995707600456001, -157.3732509998913258 ) ) ;
#10757 = CARTESIAN_POINT ( 'NONE',  ( -23.25000000000000000, 1.115600667400684642E-11, -167.4999999999999716 ) ) ;
#10758 = DIRECTION ( 'NONE',  ( -1.000000000000000000, -0.000000000000000000, -0.000000000000000000 ) ) ;
#10759 = CARTESIAN_POINT ( 'NONE',  ( 18.41815437325366389, 37.99504821466788229, -261.0425665635218593 ) ) ;
#10760 = CARTESIAN_POINT ( 'NONE',  ( -18.59999999999999787, 5.341242990002807112, -90.69334979351201298 ) ) ;
#10761 = ADVANCED_FACE ( 'NONE', ( #14053 ), #254610, .F. ) ;
#10762 = AXIS2_PLACEMENT_3D ( 'NONE', #8231, #68196, #107311 ) ;
#10763 = ORIENTED_EDGE ( 'NONE', *, *, #214149, .F. ) ;
#10764 = EDGE_CURVE ( 'NONE', #162495, #94704, #171867, .T. ) ;
#10765 = ORIENTED_EDGE ( 'NONE', *, *, #27840, .T. ) ;
#10766 = AXIS2_PLACEMENT_3D ( 'NONE', #66050, #88154, #247249 ) ;
#10768 = ORIENTED_EDGE ( 'NONE', *, *, #29607, .T. ) ;
#10767 = CARTESIAN_POINT ( 'NONE',  ( -20.54999999999999716, 23.68770167995059595, -252.8127582590406348 ) ) ;
#10769 = ORIENTED_EDGE ( 'NONE', *, *, #3527, .F. ) ;
#10770 = B_SPLINE_CURVE_WITH_KNOTS ( 'NONE', 3,
 ( #205307, #167516, #26716, #226137, #166238, #127077 ),
 .UNSPECIFIED., .F., .F.,
 ( 4, 2, 4 ),
 ( 1.138412281109779656E-18, 0.0001569047307838639517, 0.0003138094615677267650 ),
 .UNSPECIFIED. ) ;
#10771 = CARTESIAN_POINT ( 'NONE',  ( 18.79999999999999716, 5.488301202077012775, 16.40000000000000213 ) ) ;
#10772 = EDGE_CURVE ( 'NONE', #149860, #136295, #5107, .T. ) ;
#10773 = DIRECTION ( 'NONE',  ( -2.342056488767301376E-15, -0.1290532225515364506, -0.9916376685811525427 ) ) ;
#10775 = CARTESIAN_POINT ( 'NONE',  ( 21.08479644141222664, 1.563360853806263107, -230.6850037888585234 ) ) ;
#10774 = CARTESIAN_POINT ( 'NONE',  ( 20.04142135623730070, 11.75000000001115907, -58.15000000000000568 ) ) ;
#10776 = ORIENTED_EDGE ( 'NONE', *, *, #141546, .F. ) ;
#10777 = ORIENTED_EDGE ( 'NONE', *, *, #81403, .F. ) ;
#10778 = ADVANCED_FACE ( 'NONE', ( #156145 ), #131406, .F. ) ;
#10779 = ADVANCED_FACE ( 'NONE', ( #190116 ), #115706, .F. ) ;
#10780 = CARTESIAN_POINT ( 'NONE',  ( 18.54147908293611735, -9.463261657916959280, -40.54894889675577474 ) ) ;
#10781 = CARTESIAN_POINT ( 'NONE',  ( -23.25000000000000000, 76.00000000001213607, -136.5231074845243313 ) ) ;
#10782 = ORIENTED_EDGE ( 'NONE', *, *, #154940, .F. ) ;
#10783 = ORIENTED_EDGE ( 'NONE', *, *, #134751, .F. ) ;
#10784 = CIRCLE ( 'NONE', #23276, 7.800000000000001599 ) ;
#10785 = DIRECTION ( 'NONE',  ( 0.000000000000000000, -0.9654727137038715545, -0.2605042016806676242 ) ) ;
#10786 = CARTESIAN_POINT ( 'NONE',  ( -22.39999999999999858, 36.61804073161109585, -249.4599019545848364 ) ) ;
#10787 = CARTESIAN_POINT ( 'NONE',  ( -20.09999999999999787, 3.362550747017865493, 28.82623795144604983 ) ) ;
#10788 = EDGE_CURVE ( 'NONE', #116826, #122253, #212254, .T. ) ;
#10789 = DIRECTION ( 'NONE',  ( -0.7071067811865463515, -0.7071067811865487940, 7.587431340288849180E-16 ) ) ;
#10791 = VERTEX_POINT ( 'NONE', #210959 ) ;
#10790 = PLANE ( 'NONE',  #168615 ) ;
#10792 = CARTESIAN_POINT ( 'NONE',  ( 21.30000000000002558, 76.00000000001195133, -103.0231074845243171 ) ) ;
#10793 = DIRECTION ( 'NONE',  ( 0.000000000000000000, 0.000000000000000000, -1.000000000000000000 ) ) ;
#10794 = CARTESIAN_POINT ( 'NONE',  ( -18.59999999999999787, 77.63717271298224887, -91.44095411905229298 ) ) ;
#10795 = CARTESIAN_POINT ( 'NONE',  ( -23.25000000000000000, 64.25000000001237765, -170.0231074845244166 ) ) ;
#10796 = ORIENTED_EDGE ( 'NONE', *, *, #230927, .F. ) ;
#10797 = CARTESIAN_POINT ( 'NONE',  ( -18.40000000000000213, 11.47316190337364183, -124.6740539331920843 ) ) ;
#10798 = FACE_OUTER_BOUND ( 'NONE', #3361, .T. ) ;
#10800 = FACE_OUTER_BOUND ( 'NONE', #175281, .T. ) ;
#10799 = CARTESIAN_POINT ( 'NONE',  ( -21.05000000000000071, 31.98723526783714988, -238.8784020251475511 ) ) ;
#10801 = CARTESIAN_POINT ( 'NONE',  ( 21.14999999999999858, 23.07408735703284464, -230.1204787304871502 ) ) ;
#10802 = CARTESIAN_POINT ( 'NONE',  ( -16.87333278164147288, 9.882609784590036028, -53.86683219384699584 ) ) ;
#10803 = AXIS2_PLACEMENT_3D ( 'NONE', #189874, #90751, #230272 ) ;
#10804 = CARTESIAN_POINT ( 'NONE',  ( -23.15000000000000213, 4.150000000011156764, -121.6500000000000341 ) ) ;
#10805 = CARTESIAN_POINT ( 'NONE',  ( -16.77683809663752257, 66.05416425680736836, -48.68705650362859672 ) ) ;
#10806 = CARTESIAN_POINT ( 'NONE',  ( -18.50000000000000000, 11.75000000001115197, -55.25000000000004974 ) ) ;
#10807 = CIRCLE ( 'NONE', #23299, 0.09999999999999489853 ) ;
#10808 = CARTESIAN_POINT ( 'NONE',  ( -21.10257677756356642, 69.60161825747941577, -136.5480582340923661 ) ) ;
#10809 = AXIS2_PLACEMENT_3D ( 'NONE', #250107, #45481, #151010 ) ;
#10810 = VERTEX_POINT ( 'NONE', #32349 ) ;
#10811 = VECTOR ( 'NONE', #230408, 1000.000000000000000 ) ;
#10812 = ORIENTED_EDGE ( 'NONE', *, *, #185618, .T. ) ;
#10814 = EDGE_LOOP ( 'NONE', ( #232329, #22052, #45587, #225074, #73174 ) ) ;
#10813 = COLOUR_RGB ( '', 0.72549020, 0.75294118, 0.79215686) ;
#10815 = FACE_OUTER_BOUND ( 'NONE', #217541, .T. ) ;
#10816 = DIRECTION ( 'NONE',  ( 1.000000000000000000, 0.000000000000000000, 0.000000000000000000 ) ) ;
#10817 = EDGE_CURVE ( 'NONE', #214648, #224952, #111861, .T. ) ;
#10818 = VERTEX_POINT ( 'NONE', #213510 ) ;
#10819 = ADVANCED_FACE ( 'NONE', ( #93569 ), #130017, .F. ) ;
#10820 = ORIENTED_EDGE ( 'NONE', *, *, #234795, .F. ) ;
#10821 = EDGE_CURVE ( 'NONE', #5154, #102599, #191423, .T. ) ;
#10822 = ORIENTED_EDGE ( 'NONE', *, *, #137517, .F. ) ;
#10823 = CARTESIAN_POINT ( 'NONE',  ( -23.15000000000000213, 76.00000000001186606, -90.24810748452431142 ) ) ;
#10824 = CIRCLE ( 'NONE', #243857, 4.049999999999998046 ) ;
#10825 = ORIENTED_EDGE ( 'NONE', *, *, #22648, .T. ) ;
#10826 = COLOUR_RGB ( '', 0.66274510, 0.83137255, 0.94901961) ;
#10827 = CARTESIAN_POINT ( 'NONE',  ( -22.50000000000000000, 11.38316329224760359, -198.5208684056144079 ) ) ;
#10828 = AXIS2_PLACEMENT_3D ( 'NONE', #71289, #148229, #10008 ) ;
#10829 = FACE_OUTER_BOUND ( 'NONE', #233283, .T. ) ;
#10830 = CARTESIAN_POINT ( 'NONE',  ( -21.14999999999999858, 1.363275264940686293, -230.6442496871288483 ) ) ;
#10831 = CARTESIAN_POINT ( 'NONE',  ( -23.25000000000000355, 5.650000000011139001, -87.85000000000003695 ) ) ;
#10832 = DIRECTION ( 'NONE',  ( -1.000000000000000000, 0.000000000000000000, 0.000000000000000000 ) ) ;
#10835 = VERTEX_POINT ( 'NONE', #253915 ) ;
#10834 = CARTESIAN_POINT ( 'NONE',  ( -16.87998658237768623, 30.01800629463564363, -234.7061659226108929 ) ) ;
#10833 = VECTOR ( 'NONE', #82096, 1000.000000000000000 ) ;
#10837 = CARTESIAN_POINT ( 'NONE',  ( 21.05000000000000071, 33.07085611758234478, -241.5418614019517065 ) ) ;
#10836 = CARTESIAN_POINT ( 'NONE',  ( 20.94999999999999574, 18.65488991999774271, -228.0822300706204544 ) ) ;
#10838 = CARTESIAN_POINT ( 'NONE',  ( -16.86733706339143168, 9.965990529650822438, -154.9031153019987244 ) ) ;
#10839 = VERTEX_POINT ( 'NONE', #75323 ) ;
#10840 = CYLINDRICAL_SURFACE ( 'NONE', #139892, 0.09999999999999939493 ) ;
#10841 = AXIS2_PLACEMENT_3D ( 'NONE', #194095, #15453, #94962 ) ;
#10842 = CARTESIAN_POINT ( 'NONE',  ( 23.14999999999999858, 70.40000000001199965, -115.4283735034374274 ) ) ;
#10843 = DIRECTION ( 'NONE',  ( 1.000000000000000000, 7.304098846218135653E-16, 5.100424963727256530E-30 ) ) ;
#10845 = ORIENTED_EDGE ( 'NONE', *, *, #227484, .F. ) ;
#10844 = AXIS2_PLACEMENT_3D ( 'NONE', #48261, #89947, #132952 ) ;
#10846 = SHAPE_REPRESENTATION_RELATIONSHIP ( 'NONE' , 'NONE' ,  #90142, #181958 ) ;
#10847 = ADVANCED_FACE ( 'NONE', ( #236930 ), #56981, .F. ) ;
#10848 = DIRECTION ( 'NONE',  ( 0.000000000000000000, 0.000000000000000000, 1.000000000000000000 ) ) ;
#10849 = VERTEX_POINT ( 'NONE', #80387 ) ;
#10850 = AXIS2_PLACEMENT_3D ( 'NONE', #243544, #186146, #105284 ) ;
#10851 = FACE_OUTER_BOUND ( 'NONE', #184599, .T. ) ;
#10852 = CIRCLE ( 'NONE', #173211, 7.900000000000003908 ) ;
#10853 = CARTESIAN_POINT ( 'NONE',  ( 23.14999999999999858, 11.65000000001116298, -193.9851942293460070 ) ) ;
#10854 = ADVANCED_FACE ( 'NONE', ( #99958 ), #20473, .F. ) ;
#10855 = FACE_OUTER_BOUND ( 'NONE', #95417, .T. ) ;
#10856 = ORIENTED_EDGE ( 'NONE', *, *, #131843, .T. ) ;
#10857 = AXIS2_PLACEMENT_3D ( 'NONE', #56051, #141699, #101244 ) ;
#10858 = EDGE_LOOP ( 'NONE', ( #217082, #226134, #52695, #225958 ) ) ;
#10859 = EDGE_CURVE ( 'NONE', #93645, #145277, #62152, .T. ) ;
#10860 = DIRECTION ( 'NONE',  ( 0.000000000000000000, -0.01562499999999307672, 0.9998779222360100194 ) ) ;
#10861 = DIRECTION ( 'NONE',  ( 0.000000000000000000, -0.07893460099012301889, 0.9968797965484754720 ) ) ;
#10862 = CARTESIAN_POINT ( 'NONE',  ( 20.86777300164944648, 65.66799936921584901, -164.4299399888601556 ) ) ;
#10863 = DIRECTION ( 'NONE',  ( 0.000000000000000000, 6.982962677686266711E-15, -1.000000000000000000 ) ) ;
#10864 = EDGE_CURVE ( 'NONE', #124815, #143703, #188488, .T. ) ;
#10866 = DIRECTION ( 'NONE',  ( 1.000000000000000000, -0.000000000000000000, -0.000000000000000000 ) ) ;
#10865 = CYLINDRICAL_SURFACE ( 'NONE', #26037, 0.09999999999998898659 ) ;
#10867 = DIRECTION ( 'NONE',  ( 0.000000000000000000, 0.2128009952263601456, -0.9770955615653316162 ) ) ;
#10868 = CARTESIAN_POINT ( 'NONE',  ( -22.60000000000094289, 0.1008583690985001419, 11.74956712348940790 ) ) ;
#10869 = FACE_OUTER_BOUND ( 'NONE', #206312, .T. ) ;
#10870 = ORIENTED_EDGE ( 'NONE', *, *, #196952, .T. ) ;
#10871 = DIRECTION ( 'NONE',  ( 0.000000000000000000, -6.982962677686266711E-15, 1.000000000000000000 ) ) ;
#10872 = EDGE_CURVE ( 'NONE', #251277, #178255, #30287, .T. ) ;
#10874 = ORIENTED_EDGE ( 'NONE', *, *, #243078, .T. ) ;
#10873 = CARTESIAN_POINT ( 'NONE',  ( 18.39999999999997371, 11.47316190337362940, -57.75000000000000711 ) ) ;
#10875 = CARTESIAN_POINT ( 'NONE',  ( 22.47071067811864609, 68.27992525551434255, -170.1221999392270448 ) ) ;
#10877 = ADVANCED_FACE ( 'NONE', ( #182102 ), #46817, .T. ) ;
#10876 = ADVANCED_FACE ( 'NONE', ( #59541 ), #77845, .T. ) ;
#10878 = DIRECTION ( 'NONE',  ( -1.000000000000000000, 0.000000000000000000, 0.000000000000000000 ) ) ;
#10879 = CARTESIAN_POINT ( 'NONE',  ( -23.25000000000000000, 62.42744096235649920, -225.1319887738535499 ) ) ;
#10880 = CARTESIAN_POINT ( 'NONE',  ( -16.85722902420150149, 66.05000000001206217, -123.7575600107535934 ) ) ;
#10881 = CARTESIAN_POINT ( 'NONE',  ( 23.14999999999999503, 64.35000000001186038, -90.87310748452438247 ) ) ;
#10883 = ORIENTED_EDGE ( 'NONE', *, *, #101940, .F. ) ;
#10882 = CARTESIAN_POINT ( 'NONE',  ( -22.48660254037843487, 64.35000000001214460, -136.5731074845243711 ) ) ;
#10885 = DIRECTION ( 'NONE',  ( 1.000000000000000000, 0.000000000000000000, 0.000000000000000000 ) ) ;
#10884 = APPLICATION_CONTEXT ( 'automotive_design' ) ;
#10886 = FACE_OUTER_BOUND ( 'NONE', #22043, .T. ) ;
#10887 = CARTESIAN_POINT ( 'NONE',  ( 22.59066674512258643, 11.75000000001115552, -66.96949587636957801 ) ) ;
#10888 = PLANE ( 'NONE',  #186697 ) ;
#10889 = ORIENTED_EDGE ( 'NONE', *, *, #57731, .T. ) ;
#10890 = CARTESIAN_POINT ( 'NONE',  ( 18.52165635395192211, -7.769097849577835113, -209.8815359301855494 ) ) ;
#10891 = VECTOR ( 'NONE', #43048, 1000.000000000000000 ) ;
#10892 = VERTEX_POINT ( 'NONE', #120868 ) ;
#10893 = CIRCLE ( 'NONE', #2485, 1.500000000000001332 ) ;
#10894 = TOROIDAL_SURFACE ( 'NONE', #77479, 2.100000000000002309, 0.1000000000000000056 ) ;
#10895 = SPHERICAL_SURFACE ( 'NONE', #175816, 0.1000000000000000056 ) ;
#10896 = ORIENTED_EDGE ( 'NONE', *, *, #192111, .T. ) ;
#10897 = DIRECTION ( 'NONE',  ( 0.000000000000000000, -6.982962677686266711E-15, 1.000000000000000000 ) ) ;
#10898 = ADVANCED_FACE ( 'NONE', ( #101220 ), #23127, .T. ) ;
#10899 = EDGE_CURVE ( 'NONE', #216617, #26389, #255055, .T. ) ;
#10900 = ORIENTED_EDGE ( 'NONE', *, *, #197435, .F. ) ;
#10901 = AXIS2_PLACEMENT_3D ( 'NONE', #184833, #162730, #101402 ) ;
#10902 = DIRECTION ( 'NONE',  ( -1.000000000000000000, -0.000000000000000000, -0.000000000000000000 ) ) ;
#10903 = CYLINDRICAL_SURFACE ( 'NONE', #37668, 12.87499999999999822 ) ;
#10904 = EDGE_CURVE ( 'NONE', #128875, #66482, #122127, .T. ) ;
#10905 = CARTESIAN_POINT ( 'NONE',  ( -18.50000000000000000, 11.75000000001115197, -155.7499999999999716 ) ) ;
#10906 = ORIENTED_EDGE ( 'NONE', *, *, #160337, .T. ) ;
#10907 = VECTOR ( 'NONE', #76189, 1000.000000000000000 ) ;
#10909 = AXIS2_PLACEMENT_3D ( 'NONE', #241768, #158422, #200087 ) ;
#10908 = CARTESIAN_POINT ( 'NONE',  ( -16.81744102076749314, 9.950000000011142376, -180.1499999999999773 ) ) ;
#10910 = EDGE_CURVE ( 'NONE', #160216, #209723, #51081, .T. ) ;
#10911 = CARTESIAN_POINT ( 'NONE',  ( -20.65000000000000568, 7.250000000011138646, -180.1499999999999773 ) ) ;
#10912 = AXIS2_PLACEMENT_3D ( 'NONE', #34003, #112235, #230903 ) ;
#10913 = DIRECTION ( 'NONE',  ( -1.000000000000000000, -0.000000000000000000, -0.000000000000000000 ) ) ;
#10914 = ADVANCED_FACE ( 'NONE', ( #136526 ), #98660, .F. ) ;
#10915 = CARTESIAN_POINT ( 'NONE',  ( -23.39999999999994529, 76.00000000001119815, -36.02310748452479316 ) ) ;
#10916 = CARTESIAN_POINT ( 'NONE',  ( 20.94999999999999929, 11.65000000001115943, -160.7161343370219129 ) ) ;
#10917 = FACE_OUTER_BOUND ( 'NONE', #55184, .T. ) ;
#10918 = ORIENTED_EDGE ( 'NONE', *, *, #158365, .F. ) ;
#10920 = EDGE_LOOP ( 'NONE', ( #101886, #176267, #81248, #194910 ) ) ;
#10919 = CARTESIAN_POINT ( 'NONE',  ( -21.46681500593269121, 6.857511159395801137, -167.4999999999999432 ) ) ;
#10921 = ORIENTED_EDGE ( 'NONE', *, *, #247804, .T. ) ;
#10922 = DIRECTION ( 'NONE',  ( 0.000000000000000000, 0.000000000000000000, -1.000000000000000000 ) ) ;
#10923 = EDGE_LOOP ( 'NONE', ( #87844, #163578, #3709, #196370 ) ) ;
#10924 = CARTESIAN_POINT ( 'NONE',  ( 20.46382478191414833, 65.40137955871470865, -128.8452930151789531 ) ) ;
#10925 = DIRECTION ( 'NONE',  ( -1.000000000000000000, -0.000000000000000000, -0.000000000000000000 ) ) ;
#10926 = DIRECTION ( 'NONE',  ( 1.000000000000000000, 0.000000000000000000, 0.000000000000000000 ) ) ;
#10928 = ORIENTED_EDGE ( 'NONE', *, *, #116491, .T. ) ;
#10927 = VECTOR ( 'NONE', #147000, 1000.000000000000000 ) ;
#10929 = EDGE_CURVE ( 'NONE', #4741, #222996, #158711, .T. ) ;
#10930 = CARTESIAN_POINT ( 'NONE',  ( 20.94999999999999929, 85.00000000001149658, -45.91707660717670336 ) ) ;
#10931 = FACE_OUTER_BOUND ( 'NONE', #27384, .T. ) ;
#10932 = CARTESIAN_POINT ( 'NONE',  ( 18.59999999999999076, 69.35000000001200249, -115.2731074845243455 ) ) ;
#10933 = ORIENTED_EDGE ( 'NONE', *, *, #22271, .F. ) ;
#10935 = VERTEX_POINT ( 'NONE', #40048 ) ;
#10934 = DIRECTION ( 'NONE',  ( 1.000000000000000000, 0.000000000000000000, 0.000000000000000000 ) ) ;
#10936 = CARTESIAN_POINT ( 'NONE',  ( 21.15000000000005542, 83.97335046823651794, -37.38386894789040582 ) ) ;
#10937 = DIRECTION ( 'NONE',  ( 1.000000000000000000, 0.000000000000000000, -1.020425574104004196E-15 ) ) ;
#10938 = EDGE_CURVE ( 'NONE', #37547, #185637, #176993, .T. ) ;
#10939 = VECTOR ( 'NONE', #23021, 1000.000000000000114 ) ;
#10940 = CIRCLE ( 'NONE', #44255, 0.09999999999999939493 ) ;
#10941 = AXIS2_PLACEMENT_3D ( 'NONE', #142106, #27, #159139 ) ;
#10942 = AXIS2_PLACEMENT_3D ( 'NONE', #77212, #118937, #245 ) ;
#10943 = ORIENTED_EDGE ( 'NONE', *, *, #12046, .T. ) ;
#10944 = DIRECTION ( 'NONE',  ( -1.000000000000000000, 0.000000000000000000, 0.000000000000000000 ) ) ;
#10945 = CARTESIAN_POINT ( 'NONE',  ( -17.80356949364745489, 41.60004162723406296, -235.4193010670205979 ) ) ;
#10946 = CARTESIAN_POINT ( 'NONE',  ( -20.94788355080264353, 18.36312997293286031, -236.9042258689303821 ) ) ;
#10947 = ORIENTED_EDGE ( 'NONE', *, *, #103447, .F. ) ;
#10948 = DIRECTION ( 'NONE',  ( 0.000000000000000000, 0.000000000000000000, -1.000000000000000000 ) ) ;
#10949 = EDGE_CURVE ( 'NONE', #241979, #58292, #26900, .T. ) ;
#10950 = CARTESIAN_POINT ( 'NONE',  ( -22.45354308602712123, -2.500503598582757281, -189.5187041294708479 ) ) ;
#10951 = CARTESIAN_POINT ( 'NONE',  ( 23.24999999999999645, 5.600000000011153389, -55.25000000000004974 ) ) ;
#10952 = ORIENTED_EDGE ( 'NONE', *, *, #40129, .F. ) ;
#10953 = EDGE_LOOP ( 'NONE', ( #30709, #197639, #46562, #126034, #60747 ) ) ;
#10954 = DIRECTION ( 'NONE',  ( 0.000000000000000000, 1.734723475976817507E-14, -1.000000000000000000 ) ) ;
#10955 = AXIS2_PLACEMENT_3D ( 'NONE', #127020, #227396, #205252 ) ;
#10956 = ORIENTED_EDGE ( 'NONE', *, *, #77388, .F. ) ;
#10957 = CYLINDRICAL_SURFACE ( 'NONE', #187351, 0.09999999999998898659 ) ;
#10959 = ORIENTED_EDGE ( 'NONE', *, *, #249561, .F. ) ;
#10958 = CARTESIAN_POINT ( 'NONE',  ( 18.59999999999999432, 1.162701749949165642, -108.5000000000000426 ) ) ;
#10960 = CARTESIAN_POINT ( 'NONE',  ( -21.05000000000000071, -1.162701749926853712, -41.50000000000000000 ) ) ;
#10961 = DIRECTION ( 'NONE',  ( 1.000000000000000000, 0.000000000000000000, 0.000000000000000000 ) ) ;
#10962 = CARTESIAN_POINT ( 'NONE',  ( -16.86133551771149541, 9.949999999999983302, -20.80134343454665213 ) ) ;
#10963 = PLANE ( 'NONE',  #26927 ) ;
#10964 = DIRECTION ( 'NONE',  ( 1.000000000000000000, -0.000000000000000000, 0.000000000000000000 ) ) ;
#10965 = DIRECTION ( 'NONE',  ( 1.000000000000000000, 0.000000000000000000, -0.000000000000000000 ) ) ;
#10967 = ORIENTED_EDGE ( 'NONE', *, *, #145010, .T. ) ;
#10966 = DIRECTION ( 'NONE',  ( 0.000000000000000000, 1.000000000000000000, 0.000000000000000000 ) ) ;
#10968 = AXIS2_PLACEMENT_3D ( 'NONE', #256681, #57224, #212492 ) ;
#10969 = DIRECTION ( 'NONE',  ( 0.000000000000000000, 0.9126074666063770380, 0.4088369013363281068 ) ) ;
#10970 = DIRECTION ( 'NONE',  ( 0.7071067811865487940, 0.000000000000000000, -0.7071067811865463515 ) ) ;
#10971 = DIRECTION ( 'NONE',  ( 0.000000000000000000, 0.000000000000000000, -1.000000000000000000 ) ) ;
#10972 = LINE ( 'NONE', #91792, #130675 ) ;
#10973 = ORIENTED_EDGE ( 'NONE', *, *, #144379, .T. ) ;
#10974 = ADVANCED_FACE ( 'NONE', ( #243340 ), #204212, .T. ) ;
#10975 = SPHERICAL_SURFACE ( 'NONE', #110747, 0.1000000000000000056 ) ;
#10976 = DIRECTION ( 'NONE',  ( 2.952720810173289112E-16, 1.000000000000000000, 6.467318590049456648E-15 ) ) ;
#10977 = VECTOR ( 'NONE', #23732, 999.9999999999998863 ) ;
#10978 = ORIENTED_EDGE ( 'NONE', *, *, #1268, .F. ) ;
#10979 = CIRCLE ( 'NONE', #185952, 0.09999999999998898659 ) ;
#10980 = DIRECTION ( 'NONE',  ( 0.000000000000000000, -0.2128009952263604510, 0.9770955615653315052 ) ) ;
#10981 = STYLED_ITEM ( 'NONE', ( #147766 ), #88633 ) ;
#10982 = EDGE_LOOP ( 'NONE', ( #67471, #42334, #246857, #1716 ) ) ;
#10983 = CARTESIAN_POINT ( 'NONE',  ( 18.49999999999998934, 69.55000000001261640, -193.5060803140843859 ) ) ;
#10984 = ORIENTED_EDGE ( 'NONE', *, *, #163631, .F. ) ;
#10985 = ADVANCED_FACE ( 'NONE', ( #7298 ), #26003, .T. ) ;
#10987 = ORIENTED_EDGE ( 'NONE', *, *, #81364, .T. ) ;
#10986 = FACE_OUTER_BOUND ( 'NONE', #105795, .T. ) ;
#10989 = EDGE_CURVE ( 'NONE', #205142, #2443, #38648, .T. ) ;
#10988 = CARTESIAN_POINT ( 'NONE',  ( 18.59999999999999432, -1.135018845910178431, -41.21697688343231647 ) ) ;
#10990 = ORIENTED_EDGE ( 'NONE', *, *, #185402, .T. ) ;
#10991 = CARTESIAN_POINT ( 'NONE',  ( -18.59999999999999787, 74.86109765932731364, -233.8067614591677454 ) ) ;
#10992 = EDGE_LOOP ( 'NONE', ( #95386, #85100, #215684, #195435 ) ) ;
#10993 = EDGE_LOOP ( 'NONE', ( #167230, #119676, #164749, #16639 ) ) ;
#10994 = DIRECTION ( 'NONE',  ( 0.000000000000000000, 0.000000000000000000, 1.000000000000000000 ) ) ;
#10996 = ORIENTED_EDGE ( 'NONE', *, *, #257115, .T. ) ;
#10995 = LINE ( 'NONE', #184483, #101367 ) ;
#10997 = DIRECTION ( 'NONE',  ( -1.073024830501117923E-15, -0.9126074666063771490, -0.4088369013363281623 ) ) ;
#10999 = ORIENTED_EDGE ( 'NONE', *, *, #160129, .T. ) ;
#10998 = CIRCLE ( 'NONE', #2616, 1.500000000000001332 ) ;
#11000 = AXIS2_PLACEMENT_3D ( 'NONE', #206616, #164923, #145348 ) ;
#11001 = ADVANCED_FACE ( 'NONE', ( #85519 ), #245924, .T. ) ;
#11002 = ADVANCED_FACE ( 'NONE', ( #125955 ), #117755, .F. ) ;
#11003 = ORIENTED_EDGE ( 'NONE', *, *, #205832, .F. ) ;
#11004 = COLOUR_RGB ( '', 0.40784314, 0.44705882, 0.49803922) ;
#11005 = DIRECTION ( 'NONE',  ( -0.000000000000000000, -1.156482317317873105E-15, 1.000000000000000000 ) ) ;
#11006 = DIRECTION ( 'NONE',  ( 2.978066053179067751E-16, -1.000000000000000000, 0.000000000000000000 ) ) ;
#11007 = DIRECTION ( 'NONE',  ( -1.000000000000000000, 0.000000000000000000, 0.000000000000000000 ) ) ;
#11008 = VERTEX_POINT ( 'NONE', #167690 ) ;
#11009 = CIRCLE ( 'NONE', #15318, 0.1000000000000028644 ) ;
#11010 = ADVANCED_FACE ( 'NONE', ( #68570 ), #13536, .F. ) ;
#11011 = FACE_OUTER_BOUND ( 'NONE', #200026, .T. ) ;
#11012 = AXIS2_PLACEMENT_3D ( 'NONE', #168903, #107594, #24236 ) ;
#11013 = DIRECTION ( 'NONE',  ( 0.000000000000000000, -0.9908441862701782288, -0.1350103645450542456 ) ) ;
#11014 = CARTESIAN_POINT ( 'NONE',  ( 20.95512820512820440, 8.876151316288115822, -12.15000000000000036 ) ) ;
#11015 = VERTEX_POINT ( 'NONE', #142938 ) ;
#11016 = CARTESIAN_POINT ( 'NONE',  ( -17.11825945287482753, 66.05000000001261640, -190.7731074845244166 ) ) ;
#11017 = CARTESIAN_POINT ( 'NONE',  ( -21.05000000000000071, -0.2561057920810652089, -100.4651035583277405 ) ) ;
#11018 = DIRECTION ( 'NONE',  ( 1.186688945009009831E-16, -1.000000000000000000, 0.000000000000000000 ) ) ;
#11019 = EDGE_CURVE ( 'NONE', #173065, #76314, #100949, .T. ) ;
#11020 = DIRECTION ( 'NONE',  ( -0.000000000000000000, 0.2617529984165031243, 0.9651348961777157509 ) ) ;
#11021 = ORIENTED_EDGE ( 'NONE', *, *, #81067, .T. ) ;
#11022 = DIRECTION ( 'NONE',  ( 2.557131231893036985E-16, 0.7049548389605068133, -0.7092521942342977503 ) ) ;
#11023 = ORIENTED_EDGE ( 'NONE', *, *, #203096, .T. ) ;
#11024 = CARTESIAN_POINT ( 'NONE',  ( -18.54159361262937722, -7.746324184985851069, -209.9014299668642138 ) ) ;
#11025 = EDGE_LOOP ( 'NONE', ( #48008, #194421, #184946, #10947 ) ) ;
#11026 = AXIS2_PLACEMENT_3D ( 'NONE', #198977, #136403, #159877 ) ;
#11027 = STYLED_ITEM ( 'NONE', ( #144184 ), #108017 ) ;
#11028 = EDGE_CURVE ( 'NONE', #88364, #144144, #225871, .T. ) ;
#11029 = CIRCLE ( 'NONE', #35986, 0.09999999999999484301 ) ;
#11030 = CARTESIAN_POINT ( 'NONE',  ( -21.05000000000000071, 72.02722222756958104, -225.1832529173024398 ) ) ;
#11031 = DIRECTION ( 'NONE',  ( 1.000000000000000000, 2.952720810173289112E-16, -0.000000000000000000 ) ) ;
#11032 = ORIENTED_EDGE ( 'NONE', *, *, #62228, .T. ) ;
#11033 = ORIENTED_EDGE ( 'NONE', *, *, #165153, .T. ) ;
#11034 = DIRECTION ( 'NONE',  ( 0.000000000000000000, 0.000000000000000000, -1.000000000000000000 ) ) ;
#11035 = CARTESIAN_POINT ( 'NONE',  ( 18.59999999999999076, 1.835341550235567887, -78.55515129256302487 ) ) ;
#11036 = VERTEX_POINT ( 'NONE', #225044 ) ;
#11037 = AXIS2_PLACEMENT_3D ( 'NONE', #236788, #121994, #56843 ) ;
#11038 = DIRECTION ( 'NONE',  ( 0.000000000000000000, 0.000000000000000000, 1.000000000000000000 ) ) ;
#11039 = CARTESIAN_POINT ( 'NONE',  ( -20.94999999999999929, -1.835341550213255957, -78.55515129256302487 ) ) ;
#11040 = EDGE_CURVE ( 'NONE', #40351, #146933, #63413, .T. ) ;
#11041 = ORIENTED_EDGE ( 'NONE', *, *, #144141, .T. ) ;
#11042 = DIRECTION ( 'NONE',  ( 0.000000000000000000, 0.000000000000000000, 1.000000000000000000 ) ) ;
#11043 = CIRCLE ( 'NONE', #98470, 0.1000000000000016293 ) ;
#11044 = ORIENTED_EDGE ( 'NONE', *, *, #61052, .F. ) ;
#11045 = CARTESIAN_POINT ( 'NONE',  ( 20.94999999999999929, -11.48912529306489994, -164.5000000000000000 ) ) ;
#11046 = CARTESIAN_POINT ( 'NONE',  ( -16.77902162784673834, 22.98694688306329326, -230.9438819989467220 ) ) ;
#11047 = DIRECTION ( 'NONE',  ( 0.000000000000000000, 0.000000000000000000, -1.000000000000000000 ) ) ;
#11049 = ORIENTED_EDGE ( 'NONE', *, *, #251731, .T. ) ;
#11048 = FACE_OUTER_BOUND ( 'NONE', #175054, .T. ) ;
#11050 = AXIS2_PLACEMENT_3D ( 'NONE', #187387, #90819, #206939 ) ;
#11051 = CARTESIAN_POINT ( 'NONE',  ( -21.55000000000000071, 7.350000000011155166, -146.2500000000000284 ) ) ;
#11052 = DIRECTION ( 'NONE',  ( 1.734723475976817823E-14, 1.000000000000000000, -0.000000000000000000 ) ) ;
#11053 = VECTOR ( 'NONE', #5859, 999.9999999999998863 ) ;
#11054 = DIRECTION ( 'NONE',  ( 0.000000000000000000, 0.8814952561688476074, -0.4721928772777262417 ) ) ;
#11056 = CARTESIAN_POINT ( 'NONE',  ( 20.04142135623730070, 64.25000000001220712, -145.3731074845244393 ) ) ;
#11055 = CARTESIAN_POINT ( 'NONE',  ( 18.49999999999999289, 11.75000000001115907, -155.7499999999999716 ) ) ;
#11058 = VECTOR ( 'NONE', #234981, 1000.000000000000000 ) ;
#11057 = CARTESIAN_POINT ( 'NONE',  ( 20.94999999999999929, 10.47338541492406172, -108.0786544642485723 ) ) ;
#11059 = CIRCLE ( 'NONE', #165181, 11.80000000000000426 ) ;
#11060 = CARTESIAN_POINT ( 'NONE',  ( -20.94999999999999929, -11.39257802169451672, -70.07394957983198935 ) ) ;
#11061 = CYLINDRICAL_SURFACE ( 'NONE', #1963, 0.09999999999999939493 ) ;
#11062 = CARTESIAN_POINT ( 'NONE',  ( 20.95512820512820440, 60.90483797576754910, -225.2715357783924333 ) ) ;
#11064 = EDGE_LOOP ( 'NONE', ( #31607, #53064, #253982, #251293 ) ) ;
#11063 = CIRCLE ( 'NONE', #215073, 0.1000000000000055844 ) ;
#11065 = EDGE_CURVE ( 'NONE', #39843, #242585, #226324, .T. ) ;
#11066 = EDGE_LOOP ( 'NONE', ( #5934, #146113, #81108 ) ) ;
#11067 = ORIENTED_EDGE ( 'NONE', *, *, #243931, .T. ) ;
#11068 = ADVANCED_FACE ( 'NONE', ( #202934 ), #127255, .T. ) ;
#11070 = EDGE_CURVE ( 'NONE', #249855, #181739, #10562, .T. ) ;
#11069 = AXIS2_PLACEMENT_3D ( 'NONE', #193297, #231153, #94169 ) ;
#11071 = CARTESIAN_POINT ( 'NONE',  ( -18.59999999999999787, 77.83585931145498193, -24.51866831572578675 ) ) ;
#11072 = AXIS2_PLACEMENT_3D ( 'NONE', #75032, #196221, #114114 ) ;
#11073 = DIRECTION ( 'NONE',  ( -1.000000000000000000, -0.000000000000000000, -0.000000000000000000 ) ) ;
#11074 = VERTEX_POINT ( 'NONE', #112824 ) ;
#11075 = AXIS2_PLACEMENT_3D ( 'NONE', #104478, #49672, #47082 ) ;
#11076 = EDGE_CURVE ( 'NONE', #180338, #85330, #171545, .T. ) ;
#11077 = SURFACE_STYLE_USAGE ( .BOTH. , #7201 ) ;
#11079 = EDGE_CURVE ( 'NONE', #123690, #59708, #213415, .T. ) ;
#11078 = LINE ( 'NONE', #69784, #3214 ) ;
#11080 = CARTESIAN_POINT ( 'NONE',  ( -22.39999999999999858, 0.09999999999999939493, 7.790779598373403836 ) ) ;
#11081 = EDGE_CURVE ( 'NONE', #80528, #16882, #191457, .T. ) ;
#11082 = CARTESIAN_POINT ( 'NONE',  ( 20.90000000000000213, 0.000000000000000000, 0.000000000000000000 ) ) ;
#11083 = ORIENTED_EDGE ( 'NONE', *, *, #110781, .F. ) ;
#11084 = EDGE_CURVE ( 'NONE', #202894, #71736, #130209, .T. ) ;
#11085 = VERTEX_POINT ( 'NONE', #211936 ) ;
#11086 = DIRECTION ( 'NONE',  ( 0.000000000000000000, 0.000000000000000000, 1.000000000000000000 ) ) ;
#11087 = CARTESIAN_POINT ( 'NONE',  ( -20.94999999999999929, 61.95000000001191154, -97.50941241376341395 ) ) ;
#11088 = VERTEX_POINT ( 'NONE', #251029 ) ;
#11089 = EDGE_CURVE ( 'NONE', #184113, #60702, #193651, .T. ) ;
#11090 = AXIS2_PLACEMENT_3D ( 'NONE', #33539, #213395, #253804 ) ;
#11091 = CARTESIAN_POINT ( 'NONE',  ( 21.12642695952774119, 0.09890328320052040045, -94.12434007796485957 ) ) ;
#11093 = ORIENTED_EDGE ( 'NONE', *, *, #257916, .T. ) ;
#11092 = CARTESIAN_POINT ( 'NONE',  ( -2.995603634470829482E-16, 6.650000000011155876, -88.15000000000004832 ) ) ;
#11094 = DIRECTION ( 'NONE',  ( 7.304098846218134667E-16, -1.000000000000000000, 0.000000000000000000 ) ) ;
#11095 = CARTESIAN_POINT ( 'NONE',  ( -20.94999999999999929, 67.23127455305841238, -235.8551265064783991 ) ) ;
#11097 = ORIENTED_EDGE ( 'NONE', *, *, #14494, .F. ) ;
#11096 = DIRECTION ( 'NONE',  ( 0.000000000000000000, 0.000000000000000000, 1.000000000000000000 ) ) ;
#11098 = DIRECTION ( 'NONE',  ( 1.000000000000000000, 1.394253735153569469E-16, 2.602809386958778209E-16 ) ) ;
#11099 = DIRECTION ( 'NONE',  ( -1.000000000000000000, 0.000000000000000000, -0.000000000000000000 ) ) ;
#11100 = CYLINDRICAL_SURFACE ( 'NONE', #203103, 0.09999999999999939493 ) ;
#11101 = CARTESIAN_POINT ( 'NONE',  ( 20.94999999999999929, 71.00000000001180922, -81.92837350343744163 ) ) ;
#11103 = CARTESIAN_POINT ( 'NONE',  ( 21.12400222705959507, 8.778511907088271116, -179.7500000000000000 ) ) ;
#11102 = CARTESIAN_POINT ( 'NONE',  ( -23.25000000000000000, 85.00000000001197975, -112.3170766071766735 ) ) ;
#11104 = CARTESIAN_POINT ( 'NONE',  ( -20.05000000000000426, 66.75000000001223555, -148.7731074845244166 ) ) ;
#11105 = DIRECTION ( 'NONE',  ( -1.000000000000000000, 0.000000000000000000, 0.000000000000000000 ) ) ;
#11106 = AXIS2_PLACEMENT_3D ( 'NONE', #203879, #121798, #60504 ) ;
#11107 = CIRCLE ( 'NONE', #177557, 11.70000000000000284 ) ;
#11108 = CARTESIAN_POINT ( 'NONE',  ( 23.15000000000000213, 78.98983215084128062, -228.7927651294584450 ) ) ;
#11109 = VECTOR ( 'NONE', #240581, 1000.000000000000114 ) ;
#11111 = DIRECTION ( 'NONE',  ( 0.000000000000000000, 1.000000000000000000, 6.982962677686266711E-15 ) ) ;
#11110 = AXIS2_PLACEMENT_3D ( 'NONE', #208370, #70150, #14007 ) ;
#11112 = VERTEX_POINT ( 'NONE', #72433 ) ;
#11113 = EDGE_CURVE ( 'NONE', #14211, #236891, #191101, .T. ) ;
#11114 = CARTESIAN_POINT ( 'NONE',  ( -1.739115166359751170E-14, 15.92646454033038594, -219.3818586450342707 ) ) ;
#11115 = ORIENTED_EDGE ( 'NONE', *, *, #124542, .T. ) ;
#11116 = CARTESIAN_POINT ( 'NONE',  ( 20.94999999999999574, 10.47338541492405994, -74.57865446424858646 ) ) ;
#11117 = VERTEX_POINT ( 'NONE', #131098 ) ;
#11118 = DIRECTION ( 'NONE',  ( -0.000000000000000000, 1.000000000000000000, 0.000000000000000000 ) ) ;
#11119 = DIRECTION ( 'NONE',  ( 1.000000000000000000, 0.000000000000000000, 0.000000000000000000 ) ) ;
#11120 = ADVANCED_FACE ( 'NONE', ( #249768 ), #21905, .F. ) ;
#11121 = ADVANCED_FACE ( 'NONE', ( #231501 ), #69868, .T. ) ;
#11122 = ORIENTED_EDGE ( 'NONE', *, *, #127272, .T. ) ;
#11123 = CIRCLE ( 'NONE', #106787, 0.1000000000000028644 ) ;
#11124 = CARTESIAN_POINT ( 'NONE',  ( 18.49999999999996803, 7.070967871809997973, -70.74656422186831151 ) ) ;
#11125 = FILL_AREA_STYLE ('',( #89351 ) ) ;
#11126 = AXIS2_PLACEMENT_3D ( 'NONE', #242528, #161740, #40524 ) ;
#11127 = ORIENTED_EDGE ( 'NONE', *, *, #132367, .F. ) ;
#11128 = ORIENTED_EDGE ( 'NONE', *, *, #97652, .F. ) ;
#11129 = CARTESIAN_POINT ( 'NONE',  ( -20.54999999999999716, 68.85000000001156195, -57.17310748452437252 ) ) ;
#11130 = LINE ( 'NONE', #90645, #240907 ) ;
#11131 = CIRCLE ( 'NONE', #94321, 0.1000000000000028644 ) ;
#11132 = DIRECTION ( 'NONE',  ( 1.000000000000000000, -3.151514657663852580E-16, 8.547182517843351137E-17 ) ) ;
#11133 = DIRECTION ( 'NONE',  ( 1.000000000000000000, 0.000000000000000000, 0.000000000000000000 ) ) ;
#11134 = CYLINDRICAL_SURFACE ( 'NONE', #239886, 0.09999999999999939493 ) ;
#11136 = DIRECTION ( 'NONE',  ( 0.000000000000000000, 0.8814952561688444987, -0.4721928772777320149 ) ) ;
#11135 = DIRECTION ( 'NONE',  ( 0.000000000000000000, -0.9654727137038715545, 0.2605042016806676242 ) ) ;
#11137 = CARTESIAN_POINT ( 'NONE',  ( -15.15766958671844300, 9.410538608540024441, -82.43268799714094541 ) ) ;
#11139 = VERTEX_POINT ( 'NONE', #55373 ) ;
#11138 = CARTESIAN_POINT ( 'NONE',  ( -20.64999999999999858, 4.250000000011156409, -146.3500000000000227 ) ) ;
#11141 = CYLINDRICAL_SURFACE ( 'NONE', #49979, 0.09999999999999939493 ) ;
#11140 = CARTESIAN_POINT ( 'NONE',  ( 20.97438252431638972, 8.925423506087151182, -75.47237068901085877 ) ) ;
#11142 = CARTESIAN_POINT ( 'NONE',  ( 21.05000000000000071, -8.730841121484171907, -143.5980747189843783 ) ) ;
#11143 = ORIENTED_EDGE ( 'NONE', *, *, #138214, .T. ) ;
#11144 = CARTESIAN_POINT ( 'NONE',  ( -22.39999999999999858, 11.65000000001115588, -167.5999999999999659 ) ) ;
#11145 = CYLINDRICAL_SURFACE ( 'NONE', #172793, 0.1999999999999987899 ) ;
#11146 = DIRECTION ( 'NONE',  ( -1.000000000000000000, 0.000000000000000000, 0.000000000000000000 ) ) ;
#11147 = ORIENTED_EDGE ( 'NONE', *, *, #86433, .T. ) ;
#11148 = DIRECTION ( 'NONE',  ( -1.020425574104004196E-15, -6.982962677686266711E-15, 1.000000000000000000 ) ) ;
#11149 = AXIS2_PLACEMENT_3D ( 'NONE', #115300, #252237, #114008 ) ;
#11150 = CARTESIAN_POINT ( 'NONE',  ( -21.29999999999995808, 0.000000000000000000, 0.000000000000000000 ) ) ;
#11151 = CARTESIAN_POINT ( 'NONE',  ( 13.54556439290363556, 66.54940788787816075, -87.96691916571599279 ) ) ;
#11152 = EDGE_LOOP ( 'NONE', ( #50765, #68084, #109767, #210658 ) ) ;
#11153 = VERTEX_POINT ( 'NONE', #12458 ) ;
#11154 = CARTESIAN_POINT ( 'NONE',  ( -17.11825945287481332, 51.52760218553060412, -231.9873527057832234 ) ) ;
#11155 = DIRECTION ( 'NONE',  ( 0.000000000000000000, 0.9651348961777158619, -0.2617529984165031243 ) ) ;
#11156 = CARTESIAN_POINT ( 'NONE',  ( -23.25000000000000000, -1.249999999988843369, -175.3004807544151049 ) ) ;
#11157 = CARTESIAN_POINT ( 'NONE',  ( -20.85882249326303040, 10.33248238083634796, -206.5948465439131496 ) ) ;
#11158 = VERTEX_POINT ( 'NONE', #30747 ) ;
#11159 = CIRCLE ( 'NONE', #123585, 1.999999999999994893 ) ;
#11160 = CARTESIAN_POINT ( 'NONE',  ( 18.39999999999999147, 8.822561741677553471, -109.7500000000000426 ) ) ;
#11161 = EDGE_CURVE ( 'NONE', #213303, #199626, #93250, .T. ) ;
#11162 = CARTESIAN_POINT ( 'NONE',  ( 20.04142135623730070, 11.75000000000000355, 11.75000000000000000 ) ) ;
#11163 = AXIS2_PLACEMENT_3D ( 'NONE', #236012, #57360, #237311 ) ;
#11164 = CYLINDRICAL_SURFACE ( 'NONE', #116341, 0.5000000000000004441 ) ;
#11165 = DIRECTION ( 'NONE',  ( -3.469446951953515108E-14, 0.000000000000000000, -1.000000000000000000 ) ) ;
#11166 = EDGE_CURVE ( 'NONE', #177338, #244896, #9415, .T. ) ;
#11167 = AXIS2_PLACEMENT_3D ( 'NONE', #206063, #26160, #149962 ) ;
#11168 = AXIS2_PLACEMENT_3D ( 'NONE', #240381, #121731, #43459 ) ;
#11169 = ORIENTED_EDGE ( 'NONE', *, *, #195611, .F. ) ;
#11170 = CARTESIAN_POINT ( 'NONE',  ( -18.50000000000000000, 11.65000000001115232, -45.75000000000000000 ) ) ;
#11171 = AXIS2_PLACEMENT_3D ( 'NONE', #86185, #26256, #242709 ) ;
#11172 = ADVANCED_FACE ( 'NONE', ( #132388 ), #155212, .T. ) ;
#11174 = VERTEX_POINT ( 'NONE', #228925 ) ;
#11173 = CARTESIAN_POINT ( 'NONE',  ( -16.93344882324368683, 66.00341123272393418, -82.11008178971945881 ) ) ;
#11175 = EDGE_CURVE ( 'NONE', #147363, #246499, #76062, .T. ) ;
#11176 = CARTESIAN_POINT ( 'NONE',  ( 22.49231231312463208, 31.84026337202740820, -238.9442601656825786 ) ) ;
#11177 = CARTESIAN_POINT ( 'NONE',  ( 18.59999999999999076, 62.96704557978079464, -212.5773704035085814 ) ) ;
#11178 = LINE ( 'NONE', #69885, #101275 ) ;
#11179 = AXIS2_PLACEMENT_3D ( 'NONE', #216066, #196506, #217341 ) ;
#11180 = CARTESIAN_POINT ( 'NONE',  ( 20.94999999999999574, 1.750000000011155743, -179.1695115579016147 ) ) ;
#11181 = ORIENTED_EDGE ( 'NONE', *, *, #105509, .T. ) ;
#11182 = CARTESIAN_POINT ( 'NONE',  ( -20.54999999999999716, -8.999999999988846255, -110.3939691226524786 ) ) ;
#11183 = CARTESIAN_POINT ( 'NONE',  ( 18.59999999999999076, 1.835341550235567887, -78.55515129256302487 ) ) ;
#11184 = CARTESIAN_POINT ( 'NONE',  ( 20.84999999999998721, 67.49222854868494892, -195.4187676019683693 ) ) ;
#11185 = ORIENTED_EDGE ( 'NONE', *, *, #114312, .F. ) ;
#11186 = DIRECTION ( 'NONE',  ( -0.000000000000000000, -0.1335171055202867274, -0.9910465087640865089 ) ) ;
#11187 = CARTESIAN_POINT ( 'NONE',  ( -23.25000000000000000, -1.835859311432481045, -145.5044391687985694 ) ) ;
#11188 = DIRECTION ( 'NONE',  ( 0.000000000000000000, 0.000000000000000000, 1.000000000000000000 ) ) ;
#11189 = CARTESIAN_POINT ( 'NONE',  ( 21.13422380239053311, 6.493326514816903483, -167.4999999999999716 ) ) ;
#11190 = AXIS2_PLACEMENT_3D ( 'NONE', #74722, #154262, #16014 ) ;
#11191 = DIRECTION ( 'NONE',  ( 0.000000000000000000, 1.000000000000000000, 6.608470384673536824E-15 ) ) ;
#11192 = EDGE_CURVE ( 'NONE', #223637, #92778, #209330, .T. ) ;
#11194 = EDGE_CURVE ( 'NONE', #203901, #201185, #57959, .T. ) ;
#11193 = AXIS2_PLACEMENT_3D ( 'NONE', #30261, #245455, #25129 ) ;
#11195 = ORIENTED_EDGE ( 'NONE', *, *, #189624, .T. ) ;
#11196 = EDGE_LOOP ( 'NONE', ( #133586, #58926 ) ) ;
#11197 = DIRECTION ( 'NONE',  ( 0.000000000000000000, -6.982962677686266711E-15, 1.000000000000000000 ) ) ;
#11198 = CIRCLE ( 'NONE', #119537, 0.09999999999998898659 ) ;
#11199 = CARTESIAN_POINT ( 'NONE',  ( -12.25000000000000178, 66.65000000001185754, -86.27310748452437394 ) ) ;
#11200 = CARTESIAN_POINT ( 'NONE',  ( -20.54999999999999716, 1.925233644870967487, -154.7697564668738721 ) ) ;
#11201 = CIRCLE ( 'NONE', #36153, 11.74999999999999645 ) ;
#11202 = CARTESIAN_POINT ( 'NONE',  ( -21.14999999893415250, 38.10142838669770526, -236.0297427011622631 ) ) ;
#11203 = CARTESIAN_POINT ( 'NONE',  ( -21.40925344232282512, 6.658518859401606704, -133.9010498113803749 ) ) ;
#11204 = VECTOR ( 'NONE', #101706, 1000.000000000000000 ) ;
#11205 = CIRCLE ( 'NONE', #156970, 0.1000000000000028644 ) ;
#11206 = CARTESIAN_POINT ( 'NONE',  ( 23.14999999999999858, 1.115600667400684642E-11, -134.0000000000000284 ) ) ;
#11207 = FACE_OUTER_BOUND ( 'NONE', #19427, .T. ) ;
#11208 = ADVANCED_FACE ( 'NONE', ( #78803 ), #179241, .F. ) ;
#11209 = CARTESIAN_POINT ( 'NONE',  ( 23.14999999999999858, 5.600000000011153389, -112.9052660189131245 ) ) ;
#11210 = EDGE_CURVE ( 'NONE', #2322, #221912, #105234, .T. ) ;
#11211 = DIRECTION ( 'NONE',  ( 0.000000000000000000, 1.000000000000000000, 6.982962677686266711E-15 ) ) ;
#11212 = AXIS2_PLACEMENT_3D ( 'NONE', #128138, #109834, #129411 ) ;
#11213 = ORIENTED_EDGE ( 'NONE', *, *, #220478, .T. ) ;
#11215 = DIRECTION ( 'NONE',  ( -3.787827842127535236E-15, 0.7397360091702777085, 0.6728971962616808744 ) ) ;
#11214 = AXIS2_PLACEMENT_3D ( 'NONE', #54172, #155880, #134975 ) ;
#11216 = ORIENTED_EDGE ( 'NONE', *, *, #178228, .F. ) ;
#11217 = CYLINDRICAL_SURFACE ( 'NONE', #159993, 0.09999999999999939493 ) ;
#11218 = CARTESIAN_POINT ( 'NONE',  ( 21.07964655665547937, 8.774889614989714204, -79.22191658296409855 ) ) ;
#11219 = EDGE_CURVE ( 'NONE', #190309, #177816, #24983, .T. ) ;
#11220 = CARTESIAN_POINT ( 'NONE',  ( 22.39999999999999858, 75.90000000001242597, -177.8138870828977360 ) ) ;
#11221 = DIRECTION ( 'NONE',  ( 0.000000000000000000, 0.3488585713686159218, 0.9371753822965306346 ) ) ;
#11222 = DIRECTION ( 'NONE',  ( 0.000000000000000000, -1.000000000000000000, -6.982962677686265922E-15 ) ) ;
#11223 = CARTESIAN_POINT ( 'NONE',  ( -13.40000000000000213, -11.65000000000000036, 17.60000000000000497 ) ) ;
#11224 = EDGE_CURVE ( 'NONE', #254838, #62456, #38343, .T. ) ;
#11225 = EDGE_LOOP ( 'NONE', ( #80746, #87691, #73403, #172849 ) ) ;
#11226 = DIRECTION ( 'NONE',  ( 6.938893903907224433E-15, 1.000000000000000000, 7.272083257015735086E-15 ) ) ;
#11227 = CARTESIAN_POINT ( 'NONE',  ( 21.05000000000005400, 76.00000000001119815, -36.02310748452479316 ) ) ;
#11228 = LINE ( 'NONE', #214548, #60812 ) ;
#11229 = CIRCLE ( 'NONE', #23730, 0.1000000000000076938 ) ;
#11230 = LINE ( 'NONE', #9938, #72949 ) ;
#11231 = EDGE_CURVE ( 'NONE', #49193, #147247, #254837, .T. ) ;
#11232 = EDGE_LOOP ( 'NONE', ( #219877, #236880, #124474, #208634 ) ) ;
#11233 = DIRECTION ( 'NONE',  ( 0.000000000000000000, 1.000000000000000000, 0.000000000000000000 ) ) ;
#11234 = CARTESIAN_POINT ( 'NONE',  ( -23.25000000000000000, 1.115626384983466744E-11, -198.8999999999999773 ) ) ;
#11235 = EDGE_LOOP ( 'NONE', ( #41089, #161365, #49130, #67436 ) ) ;
#11236 = EDGE_CURVE ( 'NONE', #127492, #197068, #256114, .T. ) ;
#11237 = ORIENTED_EDGE ( 'NONE', *, *, #84950, .F. ) ;
#11238 = CYLINDRICAL_SURFACE ( 'NONE', #43289, 0.09999999999999939493 ) ;
#11239 = CARTESIAN_POINT ( 'NONE',  ( 21.05000000000000071, 6.256349259666485807, -229.7266095100222572 ) ) ;
#11240 = AXIS2_PLACEMENT_3D ( 'NONE', #12020, #151536, #165964 ) ;
#11241 = EDGE_CURVE ( 'NONE', #138871, #79373, #234447, .T. ) ;
#11242 = EDGE_LOOP ( 'NONE', ( #150410, #150793, #243849, #188723 ) ) ;
#11244 = VECTOR ( 'NONE', #14672, 1000.000000000000000 ) ;
#11243 = CARTESIAN_POINT ( 'NONE',  ( 18.50000000000000355, -9.399999999988841282, -174.3820418481727188 ) ) ;
#11245 = CARTESIAN_POINT ( 'NONE',  ( -21.05000000000000071, 18.62343931468261360, -223.9512205031617498 ) ) ;
#11246 = VECTOR ( 'NONE', #220234, 1000.000000000000000 ) ;
#11247 = ORIENTED_EDGE ( 'NONE', *, *, #153362, .T. ) ;
#11248 = AXIS2_PLACEMENT_3D ( 'NONE', #122677, #182646, #153826 ) ;
#11249 = DIRECTION ( 'NONE',  ( -0.000000000000000000, -0.000000000000000000, 1.000000000000000000 ) ) ;
#11250 =( BOUNDED_SURFACE ( )  B_SPLINE_SURFACE ( 3, 2, ( 
 ( #101006, #120649, #163611 ),
 ( #200168, #1936, #81460 ),
 ( #3223, #162339, #123196 ),
 ( #64507, #85319, #68364 ),
 ( #9665, #224849, #86606 ),
 ( #145308, #128344, #69660 ) ),
 .UNSPECIFIED., .F., .F., .F. ) 
 B_SPLINE_SURFACE_WITH_KNOTS ( ( 4, 2, 4 ),
 ( 3, 3 ),
 ( -1.776356839400250465E-15, 0.7853981633974468357, 1.570796326794895448 ),
 ( 0.000000000000000000, 1.000000000000000000 ),
 .UNSPECIFIED. ) 
 GEOMETRIC_REPRESENTATION_ITEM ( )  RATIONAL_B_SPLINE_SURFACE ( (
 ( 1.000000000000000000, 0.5000000000000260902, 1.000000000000000000),
 ( 1.000000000000000000, 0.4993418825329626332, 1.000000000000000000),
 ( 1.000000000000000000, 0.5278258667064184007, 1.000000000000000000),
 ( 1.000000000000000000, 0.6092287576689454642, 1.000000000000000000),
 ( 1.000000000000000000, 0.6611148371783867050, 1.000000000000000000),
 ( 1.000000000000000000, 0.7071067811865597852, 1.000000000000000000) ) ) 
 REPRESENTATION_ITEM ( '' )  SURFACE ( )  );
#11251 = VERTEX_POINT ( 'NONE', #117950 ) ;
#11252 = CARTESIAN_POINT ( 'NONE',  ( 20.95512820512820440, 10.62384868372303615, -79.15000000000004832 ) ) ;
#11253 = DIRECTION ( 'NONE',  ( -1.000000000000000000, 0.000000000000000000, -0.000000000000000000 ) ) ;
#11255 = ORIENTED_EDGE ( 'NONE', *, *, #236033, .T. ) ;
#11254 = LINE ( 'NONE', #90767, #133233 ) ;
#11256 = FACE_OUTER_BOUND ( 'NONE', #45772, .T. ) ;
#11258 = UNCERTAINTY_MEASURE_WITH_UNIT (LENGTH_MEASURE( 1.000000000000000082E-05 ), #33384, 'distance_accuracy_value', 'NONE');
#11257 = DIRECTION ( 'NONE',  ( 0.000000000000000000, -1.000000000000000000, -6.982962677686266711E-15 ) ) ;
#11259 = CARTESIAN_POINT ( 'NONE',  ( -20.86777300164945004, 65.66799936921553638, -130.9299399888601272 ) ) ;
#11260 = AXIS2_PLACEMENT_3D ( 'NONE', #192098, #211660, #33056 ) ;
#11261 = DIRECTION ( 'NONE',  ( 0.7071067811865487940, 4.851104656540973741E-15, -0.7071067811865463515 ) ) ;
#11262 = DIRECTION ( 'NONE',  ( -0.7071067811865456854, 0.7071067811865493491, 0.000000000000000000 ) ) ;
#11263 = CIRCLE ( 'NONE', #148651, 12.97500000000000320 ) ;
#11264 = CARTESIAN_POINT ( 'NONE',  ( -20.54999999999999716, 1.115600667400684642E-11, -167.5000000000000284 ) ) ;
#11265 = CARTESIAN_POINT ( 'NONE',  ( 20.94999999999999929, 8.876614585098254295, -108.8850804788447135 ) ) ;
#11267 = ORIENTED_EDGE ( 'NONE', *, *, #48514, .F. ) ;
#11266 = DIRECTION ( 'NONE',  ( 0.000000000000000000, 6.982962677686266711E-15, -1.000000000000000000 ) ) ;
#11268 = ORIENTED_EDGE ( 'NONE', *, *, #50104, .T. ) ;
#11270 = CARTESIAN_POINT ( 'NONE',  ( -15.39126916658602973, 9.389571634557565716, -84.81764071236919733 ) ) ;
#11269 = CYLINDRICAL_SURFACE ( 'NONE', #16345, 0.09999999999999939493 ) ;
#11272 = VERTEX_POINT ( 'NONE', #197480 ) ;
#11271 = DIRECTION ( 'NONE',  ( 0.000000000000000000, 0.000000000000000000, -1.000000000000000000 ) ) ;
#11273 = ORIENTED_EDGE ( 'NONE', *, *, #158800, .T. ) ;
#11274 = CARTESIAN_POINT ( 'NONE',  ( -16.80939487329394666, 66.05000000001255955, -182.6731074845235412 ) ) ;
#11275 = DIRECTION ( 'NONE',  ( -0.000000000000000000, 6.982962677686266711E-15, -1.000000000000000000 ) ) ;
#11276 = CIRCLE ( 'NONE', #52953, 0.09999999999999950595 ) ;
#11277 = CARTESIAN_POINT ( 'NONE',  ( -16.94107738177414291, 10.01423928514777373, -188.4499999999999886 ) ) ;
#11278 = FACE_OUTER_BOUND ( 'NONE', #199997, .T. ) ;
#11279 = DIRECTION ( 'NONE',  ( 0.000000000000000000, 0.000000000000000000, -1.000000000000000000 ) ) ;
#11280 = CARTESIAN_POINT ( 'NONE',  ( -20.00857864376270001, 30.09302283515540211, -235.6538990729184491 ) ) ;
#11281 = DIRECTION ( 'NONE',  ( 0.000000000000000000, -1.000000000000000000, -6.982962677686266711E-15 ) ) ;
#11282 = VERTEX_POINT ( 'NONE', #77514 ) ;
#11283 = ORIENTED_EDGE ( 'NONE', *, *, #164400, .F. ) ;
#11284 = EDGE_CURVE ( 'NONE', #180654, #214033, #38841, .T. ) ;
#11285 = DIRECTION ( 'NONE',  ( 0.000000000000000000, 1.000000000000000000, 0.000000000000000000 ) ) ;
#11286 = AXIS2_PLACEMENT_3D ( 'NONE', #185304, #45789, #204847 ) ;
#11287 = AXIS2_PLACEMENT_3D ( 'NONE', #184298, #83876, #60489 ) ;
#11288 = ORIENTED_EDGE ( 'NONE', *, *, #25162, .F. ) ;
#11289 = AXIS2_PLACEMENT_3D ( 'NONE', #171369, #132194, #33139 ) ;
#11291 = DIRECTION ( 'NONE',  ( 1.000000000000000000, 0.000000000000000000, 0.000000000000000000 ) ) ;
#11290 = AXIS2_PLACEMENT_3D ( 'NONE', #66628, #84860, #243971 ) ;
#11292 = EDGE_LOOP ( 'NONE', ( #127477, #154441, #2937, #23887 ) ) ;
#11293 = DIRECTION ( 'NONE',  ( -0.000000000000000000, 0.1350103645451876666, 0.9908441862701600211 ) ) ;
#11294 = CARTESIAN_POINT ( 'NONE',  ( -16.92132318717937522, 9.966070024017081863, -79.62240663035211696 ) ) ;
#11295 = ADVANCED_FACE ( 'NONE', ( #155823 ), #16312, .F. ) ;
#11296 = CARTESIAN_POINT ( 'NONE',  ( -40.23850191057533010, 67.65000000001118963, -25.49719488170504533 ) ) ;
#11297 = VERTEX_POINT ( 'NONE', #215755 ) ;
#11298 = CARTESIAN_POINT ( 'NONE',  ( -23.25000000000000000, -13.88357498613435936, -191.9982587459959689 ) ) ;
#11299 = ORIENTED_EDGE ( 'NONE', *, *, #100753, .F. ) ;
#11300 = ADVANCED_FACE ( 'NONE', ( #144886 ), #137497, .T. ) ;
#11301 = ADVANCED_FACE ( 'NONE', ( #243993 ), #217035, .F. ) ;
#11302 = CARTESIAN_POINT ( 'NONE',  ( -14.00000000000000178, 26.54497872210690090, -232.9592037335782209 ) ) ;
#11303 = CARTESIAN_POINT ( 'NONE',  ( 20.94999999999999929, 8.926614585098253229, -108.9716830192231498 ) ) ;
#11304 = VERTEX_POINT ( 'NONE', #158403 ) ;
#11305 = CARTESIAN_POINT ( 'NONE',  ( -18.40000000000000213, 67.17743825834520521, -60.27310748452438816 ) ) ;
#11306 = ORIENTED_EDGE ( 'NONE', *, *, #140522, .F. ) ;
#11309 = ORIENTED_EDGE ( 'NONE', *, *, #60034, .T. ) ;
#11308 = DIRECTION ( 'NONE',  ( 1.000000000000000000, 0.000000000000000000, 0.000000000000000000 ) ) ;
#11307 = FACE_OUTER_BOUND ( 'NONE', #229209, .T. ) ;
#11310 = DIRECTION ( 'NONE',  ( 0.000000000000000000, -1.000000000000000000, -6.982962677686266711E-15 ) ) ;
#11311 = ORIENTED_EDGE ( 'NONE', *, *, #87543, .T. ) ;
#11312 = CARTESIAN_POINT ( 'NONE',  ( -18.59999999999999787, 5.900000000011102586, -177.7190997646563915 ) ) ;
#11313 = AXIS2_PLACEMENT_3D ( 'NONE', #55480, #97162, #213298 ) ;
#11314 = EDGE_LOOP ( 'NONE', ( #165044, #47569, #149053, #3511 ) ) ;
#11315 = EDGE_CURVE ( 'NONE', #162811, #248722, #167853, .T. ) ;
#11316 = CARTESIAN_POINT ( 'NONE',  ( 18.49999999999999289, 10.20857864377385127, -155.7499999999999716 ) ) ;
#11317 = ORIENTED_EDGE ( 'NONE', *, *, #55809, .T. ) ;
#11318 = CARTESIAN_POINT ( 'NONE',  ( -20.94999999999999929, 76.00000000001244871, -170.0231074845243597 ) ) ;
#11319 = DIRECTION ( 'NONE',  ( 0.000000000000000000, 0.000000000000000000, -1.000000000000000000 ) ) ;
#11320 =( BOUNDED_CURVE ( )  B_SPLINE_CURVE ( 3, ( #54864, #250506, #148868, #151437 ),
 .UNSPECIFIED., .F., .F. ) 
 B_SPLINE_CURVE_WITH_KNOTS ( ( 4, 4 ),
 ( 5.733388419619901200, 5.983100554402347449 ),
 .UNSPECIFIED. ) 
 CURVE ( )  GEOMETRIC_REPRESENTATION_ITEM ( )  RATIONAL_B_SPLINE_CURVE ( ( 1.000000000000000000, 0.9948104011409417691, 0.9948104011409417691, 1.000000000000000000 ) ) 
 REPRESENTATION_ITEM ( '' )  );
#11321 = LINE ( 'NONE', #171710, #147862 ) ;
#11322 = VERTEX_POINT ( 'NONE', #116669 ) ;
#11323 = DIRECTION ( 'NONE',  ( 0.000000000000000000, 6.982962677686266711E-15, -1.000000000000000000 ) ) ;
#11324 = CARTESIAN_POINT ( 'NONE',  ( -16.87683809663752044, 13.94271038643071670, -218.6617923402251336 ) ) ;
#11325 = CARTESIAN_POINT ( 'NONE',  ( 21.14250536705908345, 6.518172176891880554, -33.50000000000000000 ) ) ;
#11326 = AXIS2_PLACEMENT_3D ( 'NONE', #176584, #215670, #17485 ) ;
#11327 = ORIENTED_EDGE ( 'NONE', *, *, #69183, .F. ) ;
#11328 = DIRECTION ( 'NONE',  ( 1.000000000000000000, 0.000000000000000000, 0.000000000000000000 ) ) ;
#11329 = ORIENTED_EDGE ( 'NONE', *, *, #56060, .F. ) ;
#11330 = LINE ( 'NONE', #32199, #214820 ) ;
#11331 = VERTEX_POINT ( 'NONE', #39734 ) ;
#11332 = EDGE_CURVE ( 'NONE', #41600, #206025, #125346, .T. ) ;
#11333 = CARTESIAN_POINT ( 'NONE',  ( -21.05000000000000071, 11.75000000001115552, -193.9851942293460070 ) ) ;
#11334 = DIRECTION ( 'NONE',  ( -0.000000000000000000, 1.000000000000000000, 0.000000000000000000 ) ) ;
#11336 = EDGE_LOOP ( 'NONE', ( #112706, #8203, #144502, #111341, #218854, #64929, #153358, #145469, #85290, #153751 ) ) ;
#11335 = CARTESIAN_POINT ( 'NONE',  ( -16.84981964351489125, 44.34925329055300836, -235.2389759867866417 ) ) ;
#11337 = CARTESIAN_POINT ( 'NONE',  ( -20.85000000000000142, 42.94477010600543565, -254.3363632230312703 ) ) ;
#11338 = ORIENTED_EDGE ( 'NONE', *, *, #5955, .F. ) ;
#11339 = AXIS2_PLACEMENT_3D ( 'NONE', #8617, #145541, #84235 ) ;
#11340 = CARTESIAN_POINT ( 'NONE',  ( -20.96077737575309996, 36.10128815642492839, -236.0658802525699400 ) ) ;
#11341 = FACE_OUTER_BOUND ( 'NONE', #53203, .T. ) ;
#11343 = EDGE_CURVE ( 'NONE', #22150, #56972, #80298, .T. ) ;
#11342 = ORIENTED_EDGE ( 'NONE', *, *, #132614, .T. ) ;
#11344 = CIRCLE ( 'NONE', #165481, 0.5000000000000001110 ) ;
#11345 = DIRECTION ( 'NONE',  ( -1.000000000000000000, 0.000000000000000000, -0.000000000000000000 ) ) ;
#11346 = DIRECTION ( 'NONE',  ( 0.000000000000000000, 0.000000000000000000, -1.000000000000000000 ) ) ;
#11347 = ORIENTED_EDGE ( 'NONE', *, *, #32657, .T. ) ;
#11348 = CARTESIAN_POINT ( 'NONE',  ( 21.05000000000000071, 1.316055977212909456, -230.7323992127457473 ) ) ;
#11349 = VECTOR ( 'NONE', #64822, 1000.000000000000000 ) ;
#11350 = VECTOR ( 'NONE', #242001, 1000.000000000000000 ) ;
#11351 = ORIENTED_EDGE ( 'NONE', *, *, #5219, .T. ) ;
#11352 =( BOUNDED_CURVE ( )  B_SPLINE_CURVE ( 3, ( #200043, #138732, #44816, #124360 ),
 .UNSPECIFIED., .F., .F. ) 
 B_SPLINE_CURVE_WITH_KNOTS ( ( 4, 4 ),
 ( 5.733388419619902088, 5.983100554402347449 ),
 .UNSPECIFIED. ) 
 CURVE ( )  GEOMETRIC_REPRESENTATION_ITEM ( )  RATIONAL_B_SPLINE_CURVE ( ( 1.000000000000000000, 0.9948104011409417691, 0.9948104011409417691, 1.000000000000000000 ) ) 
 REPRESENTATION_ITEM ( '' )  );
#11353 = PRODUCT_DEFINITION_FORMATION_WITH_SPECIFIED_SOURCE ( 'ANY', '', #151478, .NOT_KNOWN. ) ;
#11354 = DIRECTION ( 'NONE',  ( -0.000000000000000000, 1.000000000000000000, 8.717686153663073805E-15 ) ) ;
#11356 = DIRECTION ( 'NONE',  ( 1.000000000000000000, 0.000000000000000000, 0.000000000000000000 ) ) ;
#11355 = VECTOR ( 'NONE', #177222, 1000.000000000000000 ) ;
#11357 = CIRCLE ( 'NONE', #186140, 0.09999999999999939493 ) ;
#11360 = ORIENTED_EDGE ( 'NONE', *, *, #231316, .F. ) ;
#11359 = ORIENTED_EDGE ( 'NONE', *, *, #257859, .T. ) ;
#11358 = CARTESIAN_POINT ( 'NONE',  ( -20.64999999999999858, 7.250000000011155521, -155.2500000000000284 ) ) ;
#11361 = EDGE_CURVE ( 'NONE', #41121, #256883, #140063, .T. ) ;
#11362 = DIRECTION ( 'NONE',  ( 0.000000000000000000, 1.000000000000000000, -6.308085367188393199E-16 ) ) ;
#11363 = CARTESIAN_POINT ( 'NONE',  ( -21.05000000000000071, -0.09999999998884338825, -88.85000000000003695 ) ) ;
#11364 = DIRECTION ( 'NONE',  ( 1.000000000000000000, 3.265361837132813093E-16, -0.000000000000000000 ) ) ;
#11366 = DIRECTION ( 'NONE',  ( 0.5932847527679310229, -0.8049926720990042694, 0.000000000000000000 ) ) ;
#11365 = DIRECTION ( 'NONE',  ( 0.000000000000000000, 0.000000000000000000, -1.000000000000000000 ) ) ;
#11367 = DIRECTION ( 'NONE',  ( 2.840903330521633255E-16, 0.8700118002898357128, -0.4930308989875171188 ) ) ;
#11368 = AXIS2_PLACEMENT_3D ( 'NONE', #125364, #203609, #121539 ) ;
#11369 = CARTESIAN_POINT ( 'NONE',  ( -20.64999999999999858, 55.48145342050125350, -241.1189016111836736 ) ) ;
#11370 = CARTESIAN_POINT ( 'NONE',  ( -23.15000000000000213, -9.499999999988848032, -143.8939691226524644 ) ) ;
#11371 = AXIS2_PLACEMENT_3D ( 'NONE', #214657, #56839, #156002 ) ;
#11372 = ORIENTED_EDGE ( 'NONE', *, *, #75310, .T. ) ;
#11373 = ORIENTED_EDGE ( 'NONE', *, *, #105586, .T. ) ;
#11374 = EDGE_CURVE ( 'NONE', #181858, #184831, #188667, .T. ) ;
#11376 = FACE_OUTER_BOUND ( 'NONE', #234231, .T. ) ;
#11375 = AXIS2_PLACEMENT_3D ( 'NONE', #30016, #109508, #172107 ) ;
#11377 = EDGE_CURVE ( 'NONE', #228673, #165186, #206165, .T. ) ;
#11379 = EDGE_LOOP ( 'NONE', ( #145302, #221518, #255487 ) ) ;
#11378 = FACE_OUTER_BOUND ( 'NONE', #34326, .T. ) ;
#11380 = CIRCLE ( 'NONE', #115420, 0.09999999999999489853 ) ;
#11381 = VERTEX_POINT ( 'NONE', #26255 ) ;
#11382 = CARTESIAN_POINT ( 'NONE',  ( 20.85000000000000142, 1.115600667400684642E-11, -74.90000000000000568 ) ) ;
#11383 = VERTEX_POINT ( 'NONE', #228304 ) ;
#11384 = DIRECTION ( 'NONE',  ( 1.000000000000000000, 0.000000000000000000, 0.000000000000000000 ) ) ;
#11385 = AXIS2_PLACEMENT_3D ( 'NONE', #225510, #208568, #29934 ) ;
#11386 = ADVANCED_FACE ( 'NONE', ( #146177 ), #251009, .F. ) ;
#11387 = EDGE_CURVE ( 'NONE', #167725, #242093, #247854, .T. ) ;
#11388 = EDGE_LOOP ( 'NONE', ( #167822, #95945, #183853, #2575 ) ) ;
#11389 = EDGE_CURVE ( 'NONE', #245795, #68761, #210029, .T. ) ;
#11390 = CARTESIAN_POINT ( 'NONE',  ( -16.89268316805465986, 66.04827818676963602, -82.16735500597883401 ) ) ;
#11391 = DIRECTION ( 'NONE',  ( 2.952720810173289112E-16, 1.000000000000000000, 6.308085367188367561E-15 ) ) ;
#11392 = EDGE_CURVE ( 'NONE', #242599, #20178, #76231, .T. ) ;
#11395 = VERTEX_POINT ( 'NONE', #11842 ) ;
#11394 = EDGE_LOOP ( 'NONE', ( #95040, #186441, #44680, #181427 ) ) ;
#11393 = VECTOR ( 'NONE', #4022, 1000.000000000000227 ) ;
#11396 = ORIENTED_EDGE ( 'NONE', *, *, #153924, .F. ) ;
#11399 = EDGE_CURVE ( 'NONE', #206042, #58070, #86184, .T. ) ;
#11398 = ADVANCED_FACE ( 'NONE', ( #148772 ), #190480, .F. ) ;
#11397 = AXIS2_PLACEMENT_3D ( 'NONE', #23737, #4131, #246591 ) ;
#11400 = CIRCLE ( 'NONE', #211312, 0.1000000000000028644 ) ;
#11401 = ORIENTED_EDGE ( 'NONE', *, *, #87162, .T. ) ;
#11402 = ORIENTED_EDGE ( 'NONE', *, *, #98664, .F. ) ;
#11403 = DIRECTION ( 'NONE',  ( 0.000000000000000000, 0.8814952561688430555, -0.4721928772777346239 ) ) ;
#11404 = DIRECTION ( 'NONE',  ( 0.000000000000000000, 1.000000000000000000, 0.000000000000000000 ) ) ;
#11405 = CARTESIAN_POINT ( 'NONE',  ( -14.11361717019515538, 9.457426452500055092, -186.0000418683999612 ) ) ;
#11407 = ORIENTED_EDGE ( 'NONE', *, *, #195968, .T. ) ;
#11406 = DIRECTION ( 'NONE',  ( -0.000000000000000000, 0.9876197685951276783, 0.1568667991644721316 ) ) ;
#11408 = CARTESIAN_POINT ( 'NONE',  ( 21.05000000000000071, 8.776282895303632259, -179.6499999999999773 ) ) ;
#11409 = CARTESIAN_POINT ( 'NONE',  ( 22.47071067811865319, 7.720074744509197728, -167.4009075452973434 ) ) ;
#11411 = VERTEX_POINT ( 'NONE', #170943 ) ;
#11410 = CARTESIAN_POINT ( 'NONE',  ( 18.39999999999999503, 11.75000000001113953, -91.25000000000005684 ) ) ;
#11412 = LINE ( 'NONE', #88106, #217658 ) ;
#11413 = ORIENTED_EDGE ( 'NONE', *, *, #131848, .F. ) ;
#11414 = FACE_OUTER_BOUND ( 'NONE', #129602, .T. ) ;
#11415 = ORIENTED_EDGE ( 'NONE', *, *, #190407, .F. ) ;
#11416 = VECTOR ( 'NONE', #214106, 1000.000000000000000 ) ;
#11417 = CARTESIAN_POINT ( 'NONE',  ( 18.39999999999999503, 61.61567564761062243, -212.7289293916498991 ) ) ;
#11419 = EDGE_CURVE ( 'NONE', #97541, #73948, #251191, .T. ) ;
#11418 = FACE_OUTER_BOUND ( 'NONE', #252579, .T. ) ;
#11420 = CIRCLE ( 'NONE', #157182, 0.09999999999999939493 ) ;
#11421 = ORIENTED_EDGE ( 'NONE', *, *, #200652, .F. ) ;
#11423 = DIRECTION ( 'NONE',  ( 1.000000000000000000, 0.000000000000000000, 9.486769009248220990E-16 ) ) ;
#11422 = DIRECTION ( 'NONE',  ( 0.000000000000000000, -0.9651348961777157509, 0.2617529984165031243 ) ) ;
#11424 = EDGE_CURVE ( 'NONE', #108480, #142601, #6668, .T. ) ;
#11425 = EDGE_CURVE ( 'NONE', #256760, #54689, #17967, .T. ) ;
#11426 = DIRECTION ( 'NONE',  ( -1.000000000000000000, -1.836970198721029934E-16, 0.000000000000000000 ) ) ;
#11427 = CARTESIAN_POINT ( 'NONE',  ( -18.40000000000000213, 5.650000000011139001, -121.3500000000000369 ) ) ;
#11428 = CARTESIAN_POINT ( 'NONE',  ( 20.85000000000000142, 68.87972903831409610, -65.86354444268503983 ) ) ;
#11429 = EDGE_LOOP ( 'NONE', ( #206593, #215876, #53054, #191035 ) ) ;
#11430 = ORIENTED_EDGE ( 'NONE', *, *, #60269, .F. ) ;
#11431 = AXIS2_PLACEMENT_3D ( 'NONE', #136407, #197686, #60738 ) ;
#11432 = ADVANCED_FACE ( 'NONE', ( #28861 ), #121396, .F. ) ;
#11433 = CARTESIAN_POINT ( 'NONE',  ( -18.50000000000000000, 1.162701749949165642, -142.1000000000000227 ) ) ;
#11434 = CARTESIAN_POINT ( 'NONE',  ( 18.57071067811864040, 10.17928932189250091, -121.7500000000000426 ) ) ;
#11435 = ORIENTED_EDGE ( 'NONE', *, *, #100356, .T. ) ;
#11436 = DIRECTION ( 'NONE',  ( 0.000000000000000000, 0.2128009952263485993, -0.9770955615653341697 ) ) ;
#11437 = ORIENTED_EDGE ( 'NONE', *, *, #106782, .F. ) ;
#11438 = DIRECTION ( 'NONE',  ( 1.000000000000000000, 0.000000000000000000, 0.000000000000000000 ) ) ;
#11439 = FACE_OUTER_BOUND ( 'NONE', #227749, .T. ) ;
#11440 = EDGE_CURVE ( 'NONE', #252850, #201612, #67870, .T. ) ;
#11441 = AXIS2_PLACEMENT_3D ( 'NONE', #44698, #244153, #240329 ) ;
#11442 = CARTESIAN_POINT ( 'NONE',  ( 23.15000000000000213, 87.48912529308852015, -173.1231074845242688 ) ) ;
#11443 = CIRCLE ( 'NONE', #115463, 0.09999999999999982514 ) ;
#11444 = CIRCLE ( 'NONE', #32303, 0.09999999999999939493 ) ;
#11445 = CIRCLE ( 'NONE', #90516, 11.80000000000000426 ) ;
#11446 = ORIENTED_EDGE ( 'NONE', *, *, #143150, .F. ) ;
#11447 = DIRECTION ( 'NONE',  ( 0.000000000000000000, 0.1568667991644863147, 0.9876197685951252359 ) ) ;
#11448 = CIRCLE ( 'NONE', #169702, 0.2000000000000057288 ) ;
#11449 = EDGE_LOOP ( 'NONE', ( #19580, #48397, #140121, #34171, #246481 ) ) ;
#11450 = ORIENTED_EDGE ( 'NONE', *, *, #66730, .T. ) ;
#11451 = VERTEX_POINT ( 'NONE', #131757 ) ;
#11452 = DIRECTION ( 'NONE',  ( -0.8660254037843391206, 0.1308764992082676881, 0.4825674480890321805 ) ) ;
#11453 = CARTESIAN_POINT ( 'NONE',  ( -20.54999999999999716, 73.50000000001229239, -156.7984855617622770 ) ) ;
#11454 = DIRECTION ( 'NONE',  ( -0.000000000000000000, 0.000000000000000000, -1.000000000000000000 ) ) ;
#11455 = LINE ( 'NONE', #70158, #57004 ) ;
#11456 = LINE ( 'NONE', #250052, #192519 ) ;
#11458 = CYLINDRICAL_SURFACE ( 'NONE', #190796, 0.09999999999999939493 ) ;
#11457 = CARTESIAN_POINT ( 'NONE',  ( -21.05000000000000071, 16.53615870702968138, -240.8540256063542984 ) ) ;
#11460 = EDGE_LOOP ( 'NONE', ( #140001, #110418, #188061, #219472 ) ) ;
#11459 = DIRECTION ( 'NONE',  ( 0.000000000000000000, -0.8660254037844411501, -0.4999999999999956146 ) ) ;
#11461 = CARTESIAN_POINT ( 'NONE',  ( -21.40925344232282157, 10.18571439685150004, -227.8165249505043448 ) ) ;
#11462 = VERTEX_POINT ( 'NONE', #256785 ) ;
#11463 = LINE ( 'NONE', #56957, #69824 ) ;
#11464 = ORIENTED_EDGE ( 'NONE', *, *, #189871, .T. ) ;
#11465 = ORIENTED_EDGE ( 'NONE', *, *, #10522, .T. ) ;
#11466 = FACE_OUTER_BOUND ( 'NONE', #221769, .T. ) ;
#11467 = AXIS2_PLACEMENT_3D ( 'NONE', #37519, #21804, #180875 ) ;
#11468 = CARTESIAN_POINT ( 'NONE',  ( 23.14999999999999858, 76.00000000001213607, -136.5231074845243313 ) ) ;
#11469 = CARTESIAN_POINT ( 'NONE',  ( -16.94333152882356330, 66.00965798855385458, -48.63107595342290779 ) ) ;
#11470 = DIRECTION ( 'NONE',  ( 0.000000000000000000, -6.467318590049456648E-15, 1.000000000000000000 ) ) ;
#11471 = AXIS2_PLACEMENT_3D ( 'NONE', #199841, #81137, #181561 ) ;
#11472 = CARTESIAN_POINT ( 'NONE',  ( 20.94403535211772294, 18.37039103902859694, -236.9176190769588857 ) ) ;
#11473 = ORIENTED_EDGE ( 'NONE', *, *, #137043, .F. ) ;
#11474 = ORIENTED_EDGE ( 'NONE', *, *, #134225, .F. ) ;
#11475 = CYLINDRICAL_SURFACE ( 'NONE', #219699, 0.09999999999999939493 ) ;
#11476 = ORIENTED_EDGE ( 'NONE', *, *, #31096, .F. ) ;
#11477 = DIRECTION ( 'NONE',  ( 1.000000000000000000, 7.304098846218134667E-16, -0.000000000000000000 ) ) ;
#11478 = CARTESIAN_POINT ( 'NONE',  ( 20.94999999999999929, 9.374458193048763377, -220.5475659691911119 ) ) ;
#11479 = ORIENTED_EDGE ( 'NONE', *, *, #131217, .T. ) ;
#11480 = CARTESIAN_POINT ( 'NONE',  ( 19.90000000000000924, 1.249999999999999334, 22.00000000000000355 ) ) ;
#11481 = CARTESIAN_POINT ( 'NONE',  ( -20.99749315643149217, 11.75000000001115197, -59.98519423124096761 ) ) ;
#11482 = CARTESIAN_POINT ( 'NONE',  ( -33.72168855820451938, 14.15900158805616726, -219.2550725561364686 ) ) ;
#11483 = CARTESIAN_POINT ( 'NONE',  ( -23.25000000000000000, 7.128833340093095217, -233.7327013124392749 ) ) ;
#11484 = ORIENTED_EDGE ( 'NONE', *, *, #203124, .T. ) ;
#11485 = DIRECTION ( 'NONE',  ( 0.000000000000000000, 0.000000000000000000, -1.000000000000000000 ) ) ;
#11486 = DIRECTION ( 'NONE',  ( 0.000000000000000000, -0.9868171638914228216, 0.1618390714546044939 ) ) ;
#11487 = CARTESIAN_POINT ( 'NONE',  ( -22.94999999999999929, 1.885425182446134107, -11.49641995933507843 ) ) ;
#11488 = CARTESIAN_POINT ( 'NONE',  ( 23.40000000000005542, 87.50449464844290048, -37.85861909827351468 ) ) ;
#11489 = EDGE_CURVE ( 'NONE', #73311, #238735, #133058, .T. ) ;
#11490 = CARTESIAN_POINT ( 'NONE',  ( -18.59999999999999787, 3.912899247244609580, -178.9818229730109351 ) ) ;
#11491 = VECTOR ( 'NONE', #32700, 1000.000000000000000 ) ;
#11493 = AXIS2_PLACEMENT_3D ( 'NONE', #173160, #128858, #74042 ) ;
#11492 = CARTESIAN_POINT ( 'NONE',  ( -22.39999999999999858, 0.1000000000111554016, -25.70922040162659883 ) ) ;
#11494 = EDGE_CURVE ( 'NONE', #202163, #11913, #54779, .T. ) ;
#11495 = AXIS2_PLACEMENT_3D ( 'NONE', #244947, #66324, #145839 ) ;
#11496 = ORIENTED_EDGE ( 'NONE', *, *, #221361, .F. ) ;
#11497 = ADVANCED_FACE ( 'NONE', ( #216426 ), #36551, .T. ) ;
#11498 = CARTESIAN_POINT ( 'NONE',  ( -16.97092634996621641, 65.99911103366444820, -157.3929647182265228 ) ) ;
#11499 = EDGE_CURVE ( 'NONE', #163909, #126285, #78194, .T. ) ;
#11500 = ORIENTED_EDGE ( 'NONE', *, *, #139581, .F. ) ;
#11501 = FACE_BOUND ( 'NONE', #14365, .T. ) ;
#11502 = CARTESIAN_POINT ( 'NONE',  ( -18.50000000000000000, 1.006414599850381730, -224.3937905772586703 ) ) ;
#11503 = LINE ( 'NONE', #144883, #8656 ) ;
#11504 = FACE_OUTER_BOUND ( 'NONE', #183244, .T. ) ;
#11505 = DIRECTION ( 'NONE',  ( -7.304098846218134667E-16, -1.000000000000000000, -6.982962677686267499E-15 ) ) ;
#11506 = CARTESIAN_POINT ( 'NONE',  ( 20.02499999999999858, 9.750000000011153745, -88.25000000000005684 ) ) ;
#11507 = ORIENTED_EDGE ( 'NONE', *, *, #29484, .F. ) ;
#11508 = CARTESIAN_POINT ( 'NONE',  ( 18.59999999999998721, 6.846123162363745074, -137.7377262668498759 ) ) ;
#11509 = CIRCLE ( 'NONE', #215497, 0.09999999999999907574 ) ;
#11510 = CARTESIAN_POINT ( 'NONE',  ( 22.47007471830798409, 10.77449791745510232, -226.9269314985139374 ) ) ;
#11511 = CARTESIAN_POINT ( 'NONE',  ( -23.15000000000000213, 84.66355140188177586, -193.9990063664569959 ) ) ;
#11512 = VECTOR ( 'NONE', #122509, 1000.000000000000000 ) ;
#11513 = SPHERICAL_SURFACE ( 'NONE', #98921, 0.1000000000000000056 ) ;
#11514 = EDGE_CURVE ( 'NONE', #94156, #135298, #122031, .T. ) ;
#11515 = AXIS2_PLACEMENT_3D ( 'NONE', #150484, #193467, #132192 ) ;
#11516 = ORIENTED_EDGE ( 'NONE', *, *, #90347, .F. ) ;
#11517 = ORIENTED_EDGE ( 'NONE', *, *, #6604, .F. ) ;
#11518 = CARTESIAN_POINT ( 'NONE',  ( 20.94999999999999929, 69.45000000001259366, -191.3731074845244109 ) ) ;
#11519 = DIRECTION ( 'NONE',  ( 0.000000000000000000, 0.000000000000000000, -1.000000000000000000 ) ) ;
#11520 = DIRECTION ( 'NONE',  ( 0.000000000000000000, -0.1350103645451876666, 0.9908441862701600211 ) ) ;
#11521 = CARTESIAN_POINT ( 'NONE',  ( -16.86379686415369861, 44.04906952004396459, -235.3100105550803960 ) ) ;
#11522 = ORIENTED_EDGE ( 'NONE', *, *, #115315, .T. ) ;
#11523 = DIRECTION ( 'NONE',  ( 0.000000000000000000, 0.2128009952263403282, -0.9770955615653358350 ) ) ;
#11524 = CONTEXT_DEPENDENT_SHAPE_REPRESENTATION ( #220694, #120481 ) ;
#11525 = CARTESIAN_POINT ( 'NONE',  ( 19.90000000000000568, 5.488301202077012775, 16.40000000000000213 ) ) ;
#11526 = ORIENTED_EDGE ( 'NONE', *, *, #206611, .F. ) ;
#11527 = CARTESIAN_POINT ( 'NONE',  ( 18.59999999999999076, 15.53922597307775000, -223.0482397989536025 ) ) ;
#11528 = AXIS2_PLACEMENT_3D ( 'NONE', #177590, #100544, #240100 ) ;
#11529 = EDGE_CURVE ( 'NONE', #20074, #156872, #13701, .T. ) ;
#11530 = AXIS2_PLACEMENT_3D ( 'NONE', #65836, #86658, #67127 ) ;
#11531 = ORIENTED_EDGE ( 'NONE', *, *, #94855, .T. ) ;
#11532 = ORIENTED_EDGE ( 'NONE', *, *, #21790, .F. ) ;
#11533 = ORIENTED_EDGE ( 'NONE', *, *, #177179, .T. ) ;
#11534 = DIRECTION ( 'NONE',  ( 0.000000000000000000, 1.000000000000000000, 0.000000000000000000 ) ) ;
#11535 = CARTESIAN_POINT ( 'NONE',  ( 21.05000000000000071, 70.65782965956557859, -228.4198064469268559 ) ) ;
#11536 = AXIS2_PLACEMENT_3D ( 'NONE', #106094, #44870, #185663 ) ;
#11537 = CARTESIAN_POINT ( 'NONE',  ( -16.77683809663752257, 66.05416425680770942, -90.35915846542016538 ) ) ;
#11538 = EDGE_CURVE ( 'NONE', #169297, #132306, #116065, .T. ) ;
#11539 = DIRECTION ( 'NONE',  ( -0.000000000000000000, 0.1480365673253065117, -0.9889818879709273425 ) ) ;
#11540 = DIRECTION ( 'NONE',  ( 1.000000000000000000, 0.000000000000000000, 0.000000000000000000 ) ) ;
#11541 = SPHERICAL_SURFACE ( 'NONE', #32995, 0.1000000000000000056 ) ;
#11542 = CARTESIAN_POINT ( 'NONE',  ( -21.05000000000000071, -10.74476030654554393, -206.4104182790846096 ) ) ;
#11543 = EDGE_CURVE ( 'NONE', #117385, #194152, #151282, .T. ) ;
#11546 = CARTESIAN_POINT ( 'NONE',  ( -20.94999999999999929, 42.92545512184477730, -254.1955779480491344 ) ) ;
#11545 = AXIS2_PLACEMENT_3D ( 'NONE', #254318, #34049, #154011 ) ;
#11544 = CARTESIAN_POINT ( 'NONE',  ( -18.59999999999999787, 11.75000000001115197, -55.25000000000004974 ) ) ;
#11547 = CARTESIAN_POINT ( 'NONE',  ( -21.05000000000000071, 77.16270174995064224, -195.6231074845243540 ) ) ;
#11548 = CARTESIAN_POINT ( 'NONE',  ( -18.50000000000000000, 11.65000000001115232, -188.8499999999999659 ) ) ;
#11549 = CARTESIAN_POINT ( 'NONE',  ( 21.05000000000000071, 11.65000000000000746, -12.15000000000000036 ) ) ;
#11550 = DIRECTION ( 'NONE',  ( 1.000000000000000000, -0.000000000000000000, -0.000000000000000000 ) ) ;
#11551 = AXIS2_PLACEMENT_3D ( 'NONE', #77641, #137618, #116793 ) ;
#11552 = ORIENTED_EDGE ( 'NONE', *, *, #55832, .T. ) ;
#11553 = CIRCLE ( 'NONE', #69812, 4.049999999999998046 ) ;
#11554 = ORIENTED_EDGE ( 'NONE', *, *, #147138, .F. ) ;
#11555 = CYLINDRICAL_SURFACE ( 'NONE', #236126, 0.09999999999999939493 ) ;
#11556 = CIRCLE ( 'NONE', #15845, 0.09999999999999982514 ) ;
#11557 = DIRECTION ( 'NONE',  ( 0.000000000000000000, 0.000000000000000000, 1.000000000000000000 ) ) ;
#11558 = DIRECTION ( 'NONE',  ( 0.000000000000000000, -6.454785026890489601E-15, 1.000000000000000000 ) ) ;
#11559 = DIRECTION ( 'NONE',  ( 0.000000000000000000, 0.000000000000000000, -1.000000000000000000 ) ) ;
#11560 = EDGE_CURVE ( 'NONE', #221017, #128093, #49765, .T. ) ;
#11561 = CIRCLE ( 'NONE', #169796, 11.70000000000000284 ) ;
#11562 = CARTESIAN_POINT ( 'NONE',  ( -23.25000000000000000, -1.164121893230052995, -208.9148480855715775 ) ) ;
#11563 = DIRECTION ( 'NONE',  ( 1.000000000000000000, 0.000000000000000000, 0.000000000000000000 ) ) ;
#11564 = VECTOR ( 'NONE', #48974, 1000.000000000000000 ) ;
#11565 = DIRECTION ( 'NONE',  ( 1.000000000000000000, -0.000000000000000000, -0.000000000000000000 ) ) ;
#11566 = EDGE_CURVE ( 'NONE', #9918, #56583, #22104, .T. ) ;
#11567 = EDGE_LOOP ( 'NONE', ( #240657, #216875, #83798, #192037 ) ) ;
#11568 = EDGE_LOOP ( 'NONE', ( #245553, #102926, #146628, #24602 ) ) ;
#11569 = DIRECTION ( 'NONE',  ( -1.000000000000000000, 6.938893903907270030E-14, 0.000000000000000000 ) ) ;
#11570 = EDGE_CURVE ( 'NONE', #155056, #142179, #209513, .T. ) ;
#11571 = EDGE_LOOP ( 'NONE', ( #33582, #7621, #131263, #90824 ) ) ;
#11572 = CARTESIAN_POINT ( 'NONE',  ( -22.59999999999999787, 31.76322370622491320, -238.8696546380523671 ) ) ;
#11573 = AXIS2_PLACEMENT_3D ( 'NONE', #19546, #3820, #242417 ) ;
#11574 = CIRCLE ( 'NONE', #44880, 0.09999999999999939493 ) ;
#11575 = AXIS2_PLACEMENT_3D ( 'NONE', #167935, #110488, #32270 ) ;
#11576 = TOROIDAL_SURFACE ( 'NONE', #53253, 4.099999999999999645, 0.1000000000000000056 ) ;
#11577 = VERTEX_POINT ( 'NONE', #156500 ) ;
#11578 = DIRECTION ( 'NONE',  ( 0.1538461538461510236, 0.9880948137434718559, 0.000000000000000000 ) ) ;
#11579 = ADVANCED_FACE ( 'NONE', ( #57337 ), #37825, .F. ) ;
#11580 = EDGE_LOOP ( 'NONE', ( #63865, #9542, #128841, #112694, #46605, #161713, #246046, #167279, #50674 ) ) ;
#11581 = AXIS2_PLACEMENT_3D ( 'NONE', #249927, #227786, #85674 ) ;
#11582 = DIRECTION ( 'NONE',  ( 0.000000000000000000, -6.982962677686266711E-15, 1.000000000000000000 ) ) ;
#11583 = CARTESIAN_POINT ( 'NONE',  ( -21.05000000000000071, 1.261786168576181755, -175.5864989635454378 ) ) ;
#11584 = CARTESIAN_POINT ( 'NONE',  ( 20.94999999999999929, 74.16465844978787914, -158.4679561919613775 ) ) ;
#11585 = CARTESIAN_POINT ( 'NONE',  ( -20.54999999999999716, 11.48697431424113446, -220.1440440112397994 ) ) ;
#11586 = CARTESIAN_POINT ( 'NONE',  ( 21.00000000000000000, 9.749999999999998224, -21.25000000000000000 ) ) ;
#11587 = CARTESIAN_POINT ( 'NONE',  ( -20.94999999999999929, 70.10000000001220144, -146.7422072491807796 ) ) ;
#11588 = CARTESIAN_POINT ( 'NONE',  ( -20.95000000000000284, 35.97645343225767789, -235.9694016464868298 ) ) ;
#11590 = VERTEX_POINT ( 'NONE', #112220 ) ;
#11589 = CARTESIAN_POINT ( 'NONE',  ( 18.36493879433278309, -0.6805351584761402117, -242.5179116711672407 ) ) ;
#11592 = DIRECTION ( 'NONE',  ( 0.000000000000000000, 1.000000000000000000, 0.000000000000000000 ) ) ;
#11591 = DIRECTION ( 'NONE',  ( 6.938893903907499746E-14, -0.9126074666063545004, -0.4088369013363783999 ) ) ;
#11593 = VERTEX_POINT ( 'NONE', #191771 ) ;
#11594 = ORIENTED_EDGE ( 'NONE', *, *, #119400, .F. ) ;
#11595 = VECTOR ( 'NONE', #22016, 1000.000000000000000 ) ;
#11596 = ORIENTED_EDGE ( 'NONE', *, *, #68975, .T. ) ;
#11597 = DIRECTION ( 'NONE',  ( -1.000000000000000000, 0.000000000000000000, 0.000000000000000000 ) ) ;
#11598 = AXIS2_PLACEMENT_3D ( 'NONE', #215582, #177776, #117775 ) ;
#11599 = AXIS2_PLACEMENT_3D ( 'NONE', #24323, #244621, #86819 ) ;
#11600 = DIRECTION ( 'NONE',  ( 1.000000000000000000, -7.304098846218134667E-16, -5.100424963727255829E-30 ) ) ;
#11601 = CARTESIAN_POINT ( 'NONE',  ( 20.99551997958404215, 62.86709121503483999, -207.0570825002670006 ) ) ;
#11602 = FACE_OUTER_BOUND ( 'NONE', #19079, .T. ) ;
#11603 = DIRECTION ( 'NONE',  ( 0.000000000000000000, 1.000000000000000000, 0.000000000000000000 ) ) ;
#11604 = DIRECTION ( 'NONE',  ( 1.000000000000000000, 0.000000000000000000, 0.000000000000000000 ) ) ;
#11605 = CARTESIAN_POINT ( 'NONE',  ( -18.44085059012131822, 13.22076274678546248, -207.5974132564758747 ) ) ;
#11606 = FACE_OUTER_BOUND ( 'NONE', #10992, .T. ) ;
#11607 = AXIS2_PLACEMENT_3D ( 'NONE', #182387, #63700, #218915 ) ;
#11608 = VECTOR ( 'NONE', #121140, 1000.000000000000000 ) ;
#11609 = DIRECTION ( 'NONE',  ( 0.000000000000000000, 0.000000000000000000, -1.000000000000000000 ) ) ;
#11610 = VERTEX_POINT ( 'NONE', #194333 ) ;
#11611 = ORIENTED_EDGE ( 'NONE', *, *, #189723, .T. ) ;
#11612 = LINE ( 'NONE', #229372, #206257 ) ;
#11613 = CIRCLE ( 'NONE', #65760, 4.149999999999999467 ) ;
#11614 = VERTEX_POINT ( 'NONE', #117337 ) ;
#11615 = CARTESIAN_POINT ( 'NONE',  ( 20.84999999999998721, -11.74999999998884448, -167.5000000000000000 ) ) ;
#11616 = ORIENTED_EDGE ( 'NONE', *, *, #208146, .F. ) ;
#11617 = DIRECTION ( 'NONE',  ( -1.000000000000000000, 0.000000000000000000, 0.000000000000000000 ) ) ;
#11618 = CIRCLE ( 'NONE', #53101, 0.2000000000000057288 ) ;
#11619 = FACE_BOUND ( 'NONE', #36314, .T. ) ;
#11620 = DIRECTION ( 'NONE',  ( 0.000000000000000000, 0.000000000000000000, -1.000000000000000000 ) ) ;
#11621 = EDGE_CURVE ( 'NONE', #244761, #207287, #196856, .T. ) ;
#11622 = DIRECTION ( 'NONE',  ( 2.952720810173289112E-16, 0.9651348961777158619, -0.2617529984165024026 ) ) ;
#11623 = DIRECTION ( 'NONE',  ( 1.000000000000000000, 2.952720810173289112E-16, -0.000000000000000000 ) ) ;
#11624 = VERTEX_POINT ( 'NONE', #19533 ) ;
#11625 = CIRCLE ( 'NONE', #7495, 0.3999999999999975797 ) ;
#11626 = DIRECTION ( 'NONE',  ( -3.265361837132813093E-16, 1.000000000000000000, 0.000000000000000000 ) ) ;
#11627 = EDGE_CURVE ( 'NONE', #14807, #4697, #42936, .T. ) ;
#11629 = EDGE_CURVE ( 'NONE', #145638, #210448, #242839, .T. ) ;
#11628 = AXIS2_PLACEMENT_3D ( 'NONE', #116980, #253905, #97375 ) ;
#11631 = CARTESIAN_POINT ( 'NONE',  ( 21.14999999999999858, 67.25744985290005218, -235.7586130168606076 ) ) ;
#11630 = CIRCLE ( 'NONE', #86593, 0.09999999999999954758 ) ;
#11632 = DIRECTION ( 'NONE',  ( 1.000000000000000000, 0.000000000000000000, 0.000000000000000000 ) ) ;
#11633 = AXIS2_PLACEMENT_3D ( 'NONE', #31394, #109597, #130452 ) ;
#11634 = DIRECTION ( 'NONE',  ( -1.000000000000000000, 0.000000000000000000, -0.000000000000000000 ) ) ;
#11635 = DIRECTION ( 'NONE',  ( 0.000000000000000000, 1.000000000000000000, 6.688090509790097607E-15 ) ) ;
#11636 = VERTEX_POINT ( 'NONE', #5054 ) ;
#11638 = CARTESIAN_POINT ( 'NONE',  ( -5.899999999999938183, 64.65000000001120384, -26.02310748452479316 ) ) ;
#11637 = CARTESIAN_POINT ( 'NONE',  ( -17.11825945287482753, 60.84284427644114146, -221.0155524357444392 ) ) ;
#11639 = ORIENTED_EDGE ( 'NONE', *, *, #158767, .F. ) ;
#11642 = ORIENTED_EDGE ( 'NONE', *, *, #171607, .T. ) ;
#11641 = CARTESIAN_POINT ( 'NONE',  ( 20.95512820512820440, 67.12384868372420499, -161.4644784893834810 ) ) ;
#11640 = CARTESIAN_POINT ( 'NONE',  ( -20.94999999999999929, 43.08613539620618837, -254.3146655184800409 ) ) ;
#11643 = CIRCLE ( 'NONE', #40872, 0.09999999999999939493 ) ;
#11644 = CARTESIAN_POINT ( 'NONE',  ( -20.64999999999999858, 73.50000000001254818, -183.2477294072864709 ) ) ;
#11645 = DIRECTION ( 'NONE',  ( 0.000000000000000000, 0.7397360091702755991, -0.6728971962616832059 ) ) ;
#11646 = CARTESIAN_POINT ( 'NONE',  ( -18.45140287520618116, 85.48607773954142885, -96.38258435783812672 ) ) ;
#11647 = ORIENTED_EDGE ( 'NONE', *, *, #134734, .F. ) ;
#11648 = LINE ( 'NONE', #71619, #217742 ) ;
#11649 = EDGE_CURVE ( 'NONE', #59470, #125487, #163731, .T. ) ;
#11650 = DIRECTION ( 'NONE',  ( -1.000000000000000000, -0.000000000000000000, -0.000000000000000000 ) ) ;
#11652 = DIRECTION ( 'NONE',  ( 0.000000000000000000, -1.000000000000000000, 0.000000000000000000 ) ) ;
#11651 = DIRECTION ( 'NONE',  ( 0.000000000000000000, -1.000000000000000000, -1.734723475976757554E-14 ) ) ;
#11654 = ORIENTED_EDGE ( 'NONE', *, *, #5008, .F. ) ;
#11653 = CARTESIAN_POINT ( 'NONE',  ( 21.05315837424256031, 11.75000000154545177, -93.65835600266693461 ) ) ;
#11655 = AXIS2_PLACEMENT_3D ( 'NONE', #136265, #94591, #116730 ) ;
#11656 = ORIENTED_EDGE ( 'NONE', *, *, #215097, .F. ) ;
#11657 = CARTESIAN_POINT ( 'NONE',  ( -17.22767730082994575, 10.34924421247850468, -111.8575713094296162 ) ) ;
#11658 = CARTESIAN_POINT ( 'NONE',  ( 20.94999999999999574, -11.41227409413852989, -170.3999999999999773 ) ) ;
#11659 = DIRECTION ( 'NONE',  ( 0.000000000000000000, -0.4999999999999943379, -0.8660254037844420383 ) ) ;
#11660 = ORIENTED_EDGE ( 'NONE', *, *, #58865, .T. ) ;
#11661 = CYLINDRICAL_SURFACE ( 'NONE', #118626, 0.09999999999999939493 ) ;
#11662 = ADVANCED_FACE ( 'NONE', ( #83308 ), #162909, .F. ) ;
#11663 = DIRECTION ( 'NONE',  ( -1.000000000000000000, 0.000000000000000000, 0.000000000000000000 ) ) ;
#11664 = DIRECTION ( 'NONE',  ( -1.000000000000000000, -0.000000000000000000, -0.000000000000000000 ) ) ;
#11665 = EDGE_CURVE ( 'NONE', #175343, #160781, #183735, .T. ) ;
#11666 = EDGE_LOOP ( 'NONE', ( #237404, #79063, #224062, #25503, #213283 ) ) ;
#11667 = CARTESIAN_POINT ( 'NONE',  ( 20.52683494730034397, 60.79012627653062850, -225.2957294340843930 ) ) ;
#11668 = CARTESIAN_POINT ( 'NONE',  ( 20.99999999999999645, 66.25000000001153921, -48.67310748452440095 ) ) ;
#11670 = EDGE_CURVE ( 'NONE', #201690, #224268, #184558, .T. ) ;
#11669 = ORIENTED_EDGE ( 'NONE', *, *, #61107, .F. ) ;
#11671 = VECTOR ( 'NONE', #45174, 1000.000000000000000 ) ;
#11672 = CIRCLE ( 'NONE', #65811, 0.1000000000000124678 ) ;
#11673 = CARTESIAN_POINT ( 'NONE',  ( 20.85000000000000142, -1.149570369564537842, -108.3159124845020074 ) ) ;
#11674 = CARTESIAN_POINT ( 'NONE',  ( 23.14999999999999503, 6.550000000011156231, -146.3500000000000227 ) ) ;
#11675 = AXIS2_PLACEMENT_3D ( 'NONE', #226330, #88098, #163827 ) ;
#11676 = EDGE_LOOP ( 'NONE', ( #112299, #8926, #158428 ) ) ;
#11677 = EDGE_LOOP ( 'NONE', ( #209741, #35220, #4895, #39981 ) ) ;
#11678 = ORIENTED_EDGE ( 'NONE', *, *, #36566, .T. ) ;
#11679 = VERTEX_POINT ( 'NONE', #199461 ) ;
#11680 = ORIENTED_EDGE ( 'NONE', *, *, #146304, .F. ) ;
#11684 = ADVANCED_FACE ( 'NONE', ( #102879 ), #123762, .F. ) ;
#11683 = ORIENTED_EDGE ( 'NONE', *, *, #128956, .F. ) ;
#11682 = EDGE_LOOP ( 'NONE', ( #197009, #165294, #137426 ) ) ;
#11681 = CARTESIAN_POINT ( 'NONE',  ( 22.47071067811865319, 76.00000000001267608, -203.5231074845243597 ) ) ;
#11685 = AXIS2_PLACEMENT_3D ( 'NONE', #112015, #110710, #170743 ) ;
#11686 = FACE_OUTER_BOUND ( 'NONE', #26406, .T. ) ;
#11687 = AXIS2_PLACEMENT_3D ( 'NONE', #56431, #193413, #154319 ) ;
#11688 = ORIENTED_EDGE ( 'NONE', *, *, #84971, .T. ) ;
#11689 = FACE_OUTER_BOUND ( 'NONE', #231774, .T. ) ;
#11690 = CARTESIAN_POINT ( 'NONE',  ( -21.14999999999999858, -0.09999999998884338825, -88.85042919245522341 ) ) ;
#11691 = DIRECTION ( 'NONE',  ( 1.000000000000000000, -3.151514657663852580E-16, 8.547182517843351137E-17 ) ) ;
#11692 =( BOUNDED_CURVE ( )  B_SPLINE_CURVE ( 3, ( #76179, #172774, #33254, #155764 ),
 .UNSPECIFIED., .F., .T. ) 
 B_SPLINE_CURVE_WITH_KNOTS ( ( 4, 4 ),
 ( 3.432212674861197410, 3.693332928900581624 ),
 .UNSPECIFIED. ) 
 CURVE ( )  GEOMETRIC_REPRESENTATION_ITEM ( )  RATIONAL_B_SPLINE_CURVE ( ( 1.000000000000000000, 0.9943260843901261525, 0.9943260843901261525, 1.000000000000000000 ) ) 
 REPRESENTATION_ITEM ( '' )  );
#11693 = AXIS2_PLACEMENT_3D ( 'NONE', #120454, #179139, #451 ) ;
#11694 = CARTESIAN_POINT ( 'NONE',  ( -18.59999999999999787, 1.148907358139439339E-11, -201.0000000000015064 ) ) ;
#11695 = ORIENTED_EDGE ( 'NONE', *, *, #239344, .F. ) ;
#11696 = ORIENTED_EDGE ( 'NONE', *, *, #3514, .F. ) ;
#11697 = ORIENTED_EDGE ( 'NONE', *, *, #33819, .T. ) ;
#11698 = EDGE_CURVE ( 'NONE', #161314, #256777, #197232, .T. ) ;
#11699 = DIRECTION ( 'NONE',  ( 1.000000000000000000, 0.000000000000000000, 0.000000000000000000 ) ) ;
#11701 = ORIENTED_EDGE ( 'NONE', *, *, #205800, .T. ) ;
#11700 = CARTESIAN_POINT ( 'NONE',  ( -21.14999999999999858, 1.115600667400684642E-11, -21.85042919245520210 ) ) ;
#11702 = CYLINDRICAL_SURFACE ( 'NONE', #34214, 0.09999999999998898659 ) ;
#11704 = ORIENTED_EDGE ( 'NONE', *, *, #140585, .T. ) ;
#11703 = CARTESIAN_POINT ( 'NONE',  ( -20.94999999999999929, 76.00000000001126921, -203.5231074845248997 ) ) ;
#11705 = VERTEX_POINT ( 'NONE', #63776 ) ;
#11706 = LINE ( 'NONE', #32576, #8757 ) ;
#11707 = EDGE_CURVE ( 'NONE', #104346, #64710, #192969, .T. ) ;
#11708 = EDGE_CURVE ( 'NONE', #154018, #76954, #25767, .T. ) ;
#11709 = ORIENTED_EDGE ( 'NONE', *, *, #202258, .F. ) ;
#11710 = DIRECTION ( 'NONE',  ( 0.000000000000000000, 1.000000000000000000, 0.000000000000000000 ) ) ;
#11711 = CARTESIAN_POINT ( 'NONE',  ( -21.05000000000000426, 76.02103547655254090, -176.3275633064720296 ) ) ;
#11712 = AXIS2_PLACEMENT_3D ( 'NONE', #104097, #144514, #1148 ) ;
#11713 = VECTOR ( 'NONE', #29030, 1000.000000000000000 ) ;
#11714 = CIRCLE ( 'NONE', #178318, 0.09999999999998898659 ) ;
#11716 = EDGE_CURVE ( 'NONE', #63679, #222677, #5666, .T. ) ;
#11715 = EDGE_CURVE ( 'NONE', #2987, #33556, #176411, .T. ) ;
#11718 = VERTEX_POINT ( 'NONE', #118640 ) ;
#11717 = ORIENTED_EDGE ( 'NONE', *, *, #152190, .F. ) ;
#11719 = ORIENTED_EDGE ( 'NONE', *, *, #4230, .T. ) ;
#11721 = ADVANCED_FACE ( 'NONE', ( #198149 ), #76394, .T. ) ;
#11720 = DIRECTION ( 'NONE',  ( -1.000000000000000000, 1.652117596168391700E-15, 0.000000000000000000 ) ) ;
#11722 = VERTEX_POINT ( 'NONE', #243697 ) ;
#11723 = EDGE_LOOP ( 'NONE', ( #233672, #80326, #174766, #217559 ) ) ;
#11724 = CARTESIAN_POINT ( 'NONE',  ( 18.60000000000000497, 36.65892442174472876, -249.5511627012454596 ) ) ;
#11726 = ORIENTED_EDGE ( 'NONE', *, *, #17567, .F. ) ;
#11725 = FACE_OUTER_BOUND ( 'NONE', #56959, .T. ) ;
#11727 = DIRECTION ( 'NONE',  ( 1.000000000000000000, 0.000000000000000000, 0.000000000000000000 ) ) ;
#11728 = AXIS2_PLACEMENT_3D ( 'NONE', #86225, #207507, #186656 ) ;
#11729 = ADVANCED_FACE ( 'NONE', ( #229282 ), #145869, .T. ) ;
#11731 = LINE ( 'NONE', #130357, #40214 ) ;
#11730 = CARTESIAN_POINT ( 'NONE',  ( 20.94999999999999929, 71.00000000001180922, -81.92837350343744163 ) ) ;
#11732 = DIRECTION ( 'NONE',  ( 0.000000000000000000, -6.982962677686266711E-15, 1.000000000000000000 ) ) ;
#11733 = CARTESIAN_POINT ( 'NONE',  ( -14.00000000000000178, 13.18880795147152440, -215.2702608532411830 ) ) ;
#11734 = VERTEX_POINT ( 'NONE', #87174 ) ;
#11735 = EDGE_LOOP ( 'NONE', ( #169451, #189621, #12126, #38704, #220882 ) ) ;
#11736 = CARTESIAN_POINT ( 'NONE',  ( -18.40000000000000213, 64.51332499825382172, -45.27310748452440947 ) ) ;
#11738 = EDGE_CURVE ( 'NONE', #199264, #115602, #169341, .T. ) ;
#11737 = CARTESIAN_POINT ( 'NONE',  ( -23.25000000000000000, 78.57744179526842743, -232.8011145694030972 ) ) ;
#11739 = ORIENTED_EDGE ( 'NONE', *, *, #20313, .F. ) ;
#11740 = AXIS2_PLACEMENT_3D ( 'NONE', #38244, #201156, #102033 ) ;
#11741 = AXIS2_PLACEMENT_3D ( 'NONE', #168935, #248426, #189738 ) ;
#11742 = EDGE_CURVE ( 'NONE', #172479, #171479, #144581, .T. ) ;
#11743 = EDGE_CURVE ( 'NONE', #87179, #240058, #185012, .T. ) ;
#11744 = VECTOR ( 'NONE', #87888, 1000.000000000000000 ) ;
#11745 = DIRECTION ( 'NONE',  ( 1.000000000000000000, -0.000000000000000000, 0.000000000000000000 ) ) ;
#11746 = DIRECTION ( 'NONE',  ( -1.000000000000000000, 0.000000000000000000, 0.000000000000000000 ) ) ;
#11747 = VECTOR ( 'NONE', #5382, 1000.000000000000000 ) ;
#11748 = ORIENTED_EDGE ( 'NONE', *, *, #235926, .T. ) ;
#11749 = EDGE_LOOP ( 'NONE', ( #254561, #92901, #49364, #38719 ) ) ;
#11750 = EDGE_CURVE ( 'NONE', #12745, #187441, #50613, .T. ) ;
#11751 = CARTESIAN_POINT ( 'NONE',  ( -23.15000000000000213, 11.65000000001115588, -59.98519422934606382 ) ) ;
#11752 = DIRECTION ( 'NONE',  ( 1.000000000000000000, 0.000000000000000000, 0.000000000000000000 ) ) ;
#11753 = ORIENTED_EDGE ( 'NONE', *, *, #97434, .T. ) ;
#11754 = DIRECTION ( 'NONE',  ( 1.000000000000000000, 1.832422279913646096E-16, 3.990820347355631841E-17 ) ) ;
#11755 = ORIENTED_EDGE ( 'NONE', *, *, #7623, .F. ) ;
#11756 = DIRECTION ( 'NONE',  ( 1.000000000000000000, 0.000000000000000000, 0.000000000000000000 ) ) ;
#11758 = DIRECTION ( 'NONE',  ( -0.000000000000000000, 0.2128009952263603677, -0.9770955615653313941 ) ) ;
#11757 =( BOUNDED_SURFACE ( )  B_SPLINE_SURFACE ( 3, 2, ( 
 ( #202544, #145122, #207701 ),
 ( #224667, #46032, #66888 ),
 ( #125574, #205092, #105987 ),
 ( #186853, #206402, #162159 ),
 ( #47297, #146399, #225925 ),
 ( #29092, #8215, #27799 ),
 ( #167301, #68174, #48601 ),
 ( #147715, #128158, #188122 ),
 ( #241673, #63023, #142558 ),
 ( #222074, #4328, #43476 ),
 ( #123021, #83835, #112453 ),
 ( #210267, #35505, #90283 ) ),
 .UNSPECIFIED., .F., .F., .F. ) 
 B_SPLINE_SURFACE_WITH_KNOTS ( ( 4, 2, 2, 2, 2, 4 ),
 ( 3, 3 ),
 ( 3.174653483277205090, 3.943930578431714018, 4.713207673586222946, 5.482484768740731873, 5.867123316317986337, 6.251761863895240801 ),
 ( 0.000000000000000000, 1.000000000000000000 ),
 .UNSPECIFIED. ) 
 GEOMETRIC_REPRESENTATION_ITEM ( )  RATIONAL_B_SPLINE_SURFACE ( (
 ( 1.000000000000000000, 0.8659465255642228021, 1.000000000000000000),
 ( 1.000000000000000000, 0.8648614068488691409, 1.000000000000000000),
 ( 1.000000000000000000, 0.8489031841323105843, 1.000000000000000000),
 ( 1.000000000000000000, 0.7927507630162217156, 1.000000000000000000),
 ( 1.000000000000000000, 0.7523013859014273663, 1.000000000000000000),
 ( 1.000000000000000000, 0.6616226951191639394, 1.000000000000000000),
 ( 1.000000000000000000, 0.6112214368725639169, 1.000000000000000000),
 ( 1.000000000000000000, 0.5507684314497727218, 1.000000000000000000),
 ( 1.000000000000000000, 0.5333267243152293169, 1.000000000000000000),
 ( 1.000000000000000000, 0.5084565446480597828, 1.000000000000000000),
 ( 1.000000000000000000, 0.5010722703450565252, 1.000000000000000000),
 ( 1.000000000000000000, 0.5001234037138694299, 1.000000000000000000) ) ) 
 REPRESENTATION_ITEM ( '' )  SURFACE ( )  );
#11760 = CARTESIAN_POINT ( 'NONE',  ( -21.05000000000000071, -1.236118717437888259, -194.8647072476926212 ) ) ;
#11759 = FACE_OUTER_BOUND ( 'NONE', #147428, .T. ) ;
#11761 = CARTESIAN_POINT ( 'NONE',  ( 20.94999999999999929, 0.000000000000000000, -37.50000000000000000 ) ) ;
#11762 = ADVANCED_FACE ( 'NONE', ( #45498 ), #46767, .T. ) ;
#11763 = DIRECTION ( 'NONE',  ( -1.000000000000000000, 0.000000000000000000, 0.000000000000000000 ) ) ;
#11765 = EDGE_CURVE ( 'NONE', #188452, #227951, #101308, .T. ) ;
#11764 = DIRECTION ( 'NONE',  ( 1.000000000000000000, -0.000000000000000000, -0.000000000000000000 ) ) ;
#11766 = CARTESIAN_POINT ( 'NONE',  ( -21.55000000000000426, 65.28755502419014078, -213.4139377145917820 ) ) ;
#11767 = EDGE_CURVE ( 'NONE', #234183, #176065, #39039, .T. ) ;
#11769 = ORIENTED_EDGE ( 'NONE', *, *, #68276, .F. ) ;
#11768 = DIRECTION ( 'NONE',  ( 0.000000000000000000, 0.000000000000000000, -1.000000000000000000 ) ) ;
#11770 = AXIS2_PLACEMENT_3D ( 'NONE', #109810, #189371, #10730 ) ;
#11773 = ORIENTED_EDGE ( 'NONE', *, *, #119032, .T. ) ;
#11772 = EDGE_LOOP ( 'NONE', ( #96842, #86600, #221750, #122432 ) ) ;
#11771 = CIRCLE ( 'NONE', #157524, 0.09999999999999939493 ) ;
#11774 = ORIENTED_EDGE ( 'NONE', *, *, #70752, .T. ) ;
#11775 = AXIS2_PLACEMENT_3D ( 'NONE', #139768, #77234, #254571 ) ;
#11776 = CARTESIAN_POINT ( 'NONE',  ( 22.47110162079220785, 0.02879741280269312517, 11.64993593668433469 ) ) ;
#11777 = LINE ( 'NONE', #191706, #116105 ) ;
#11778 = EDGE_CURVE ( 'NONE', #244896, #34405, #213805, .T. ) ;
#11779 = CIRCLE ( 'NONE', #174110, 2.699999999999999289 ) ;
#11781 = CARTESIAN_POINT ( 'NONE',  ( 21.14999999999999858, 64.35000000001228670, -157.7731074845244450 ) ) ;
#11780 = CARTESIAN_POINT ( 'NONE',  ( 23.24999999999999645, 4.775700934590591196, -88.65123189595408348 ) ) ;
#11782 = ADVANCED_FACE ( 'NONE', ( #209712 ), #7669, .T. ) ;
#11783 = FACE_OUTER_BOUND ( 'NONE', #78743, .T. ) ;
#11784 = ORIENTED_EDGE ( 'NONE', *, *, #65565, .T. ) ;
#11785 = CARTESIAN_POINT ( 'NONE',  ( -22.50000000000000000, 11.64957080755595520, -100.4000000000000483 ) ) ;
#11786 = ORIENTED_EDGE ( 'NONE', *, *, #250558, .T. ) ;
#11787 = ORIENTED_EDGE ( 'NONE', *, *, #179376, .T. ) ;
#11788 = CARTESIAN_POINT ( 'NONE',  ( -21.05000000000000071, 0.09779029130878996723, 6.257814610476121864 ) ) ;
#11789 = DIRECTION ( 'NONE',  ( 1.000000000000000000, 0.000000000000000000, 0.000000000000000000 ) ) ;
#11790 = CARTESIAN_POINT ( 'NONE',  ( -20.94999999999999929, 76.00000000001213607, -136.5231074845243313 ) ) ;
#11791 = ORIENTED_EDGE ( 'NONE', *, *, #182521, .F. ) ;
#11792 = AXIS2_PLACEMENT_3D ( 'NONE', #47207, #146317, #126764 ) ;
#11793 = AXIS2_PLACEMENT_3D ( 'NONE', #9553, #192072, #92940 ) ;
#11794 = DIRECTION ( 'NONE',  ( 0.000000000000000000, -1.000000000000000000, -6.860497997771531562E-15 ) ) ;
#11795 = CARTESIAN_POINT ( 'NONE',  ( -23.25000000000000000, 11.75000000001115552, -167.5000000000000284 ) ) ;
#11796 = ORIENTED_EDGE ( 'NONE', *, *, #252109, .T. ) ;
#11797 = VERTEX_POINT ( 'NONE', #226692 ) ;
#11798 = CARTESIAN_POINT ( 'NONE',  ( -18.37160782347004329, 64.52438358520949180, -93.77310748452438816 ) ) ;
#11799 = CARTESIAN_POINT ( 'NONE',  ( 22.39999999999999503, 0.1000000000111554016, -92.70922040162665212 ) ) ;
#11800 = CARTESIAN_POINT ( 'NONE',  ( -21.44999999999999929, 68.85000000001254250, -182.3731074845244109 ) ) ;
#11801 = CARTESIAN_POINT ( 'NONE',  ( 20.94999999999999929, -11.48912529306489994, -130.9000000000000341 ) ) ;
#11802 = LINE ( 'NONE', #10500, #65105 ) ;
#11803 = CARTESIAN_POINT ( 'NONE',  ( -20.94999999999999929, -11.75000000000000000, -2.900000000000003464 ) ) ;
#11804 = ORIENTED_EDGE ( 'NONE', *, *, #53149, .T. ) ;
#11805 = LINE ( 'NONE', #235945, #250474 ) ;
#11806 = CARTESIAN_POINT ( 'NONE',  ( -21.93340585971692747, 7.324147022868200629, -33.50000000000000711 ) ) ;
#11807 = VECTOR ( 'NONE', #142907, 1000.000000000000000 ) ;
#11809 = DIRECTION ( 'NONE',  ( 0.000000000000000000, -0.9915357197604882655, 0.1298341882519793711 ) ) ;
#11808 = CARTESIAN_POINT ( 'NONE',  ( -18.59999999999999787, 1.115600667400684642E-11, -167.5000000000000284 ) ) ;
#11810 = CARTESIAN_POINT ( 'NONE',  ( 18.49999999999999289, 65.50857864377465489, -111.6731074845243796 ) ) ;
#11811 = AXIS2_PLACEMENT_3D ( 'NONE', #70802, #171206, #150323 ) ;
#11812 = DIRECTION ( 'NONE',  ( 0.000000000000000000, 0.4088369013363281068, -0.9126074666063770380 ) ) ;
#11813 = EDGE_CURVE ( 'NONE', #223255, #168502, #166768, .T. ) ;
#11814 = CARTESIAN_POINT ( 'NONE',  ( 20.04142135623730070, 11.65000000000000391, -21.35000000000000142 ) ) ;
#11816 = FACE_OUTER_BOUND ( 'NONE', #66334, .T. ) ;
#11815 = AXIS2_PLACEMENT_3D ( 'NONE', #146208, #220629, #42007 ) ;
#11818 = EDGE_LOOP ( 'NONE', ( #183940, #128384, #54975, #15645, #61088, #243622, #248529, #45614, #171333, #147569, #140384, #222147, #248137, #189034, #194791, #225580, #33771, #12019 ) ) ;
#11817 = CARTESIAN_POINT ( 'NONE',  ( 23.25000000000000000, 85.60000000001188880, -93.12913836187179584 ) ) ;
#11819 = ADVANCED_FACE ( 'NONE', ( #48060 ), #127610, .F. ) ;
#11820 = CIRCLE ( 'NONE', #82473, 11.75000000000000533 ) ;
#11821 = CARTESIAN_POINT ( 'NONE',  ( -20.94999999999999929, 64.35000000001245724, -170.0231074845244166 ) ) ;
#11822 = AXIS2_PLACEMENT_3D ( 'NONE', #63021, #81281, #184260 ) ;
#11823 = AXIS2_PLACEMENT_3D ( 'NONE', #252310, #114090, #94523 ) ;
#11824 = AXIS2_PLACEMENT_3D ( 'NONE', #82317, #241436, #4093 ) ;
#11825 = B_SPLINE_CURVE_WITH_KNOTS ( 'NONE', 3,
 ( #253895, #76544, #156124, #75301, #31050, #154835, #234334, #110540, #179527, #37448 ),
 .UNSPECIFIED., .F., .F.,
 ( 4, 3, 3, 4 ),
 ( 0.000000000000000000, 4.874959354402468362E-05, 9.785140065121357639E-05, 0.0001360444631936129551 ),
 .UNSPECIFIED. ) ;
#11826 = SPHERICAL_SURFACE ( 'NONE', #154749, 0.1000000000000000056 ) ;
#11827 = AXIS2_PLACEMENT_3D ( 'NONE', #37801, #96439, #254234 ) ;
#11828 = EDGE_CURVE ( 'NONE', #35026, #145808, #188859, .T. ) ;
#11829 = CARTESIAN_POINT ( 'NONE',  ( 22.47071067811865319, 68.27992525551361780, -69.62219993922698791 ) ) ;
#11830 = DIRECTION ( 'NONE',  ( 1.000000000000000000, -0.000000000000000000, -0.000000000000000000 ) ) ;
#11831 = TOROIDAL_SURFACE ( 'NONE', #45113, 0.4000000000000017431, 0.1000000000000000056 ) ;
#11832 = DIRECTION ( 'NONE',  ( -0.000000000000000000, -6.982962677686266711E-15, 1.000000000000000000 ) ) ;
#11833 = DIRECTION ( 'NONE',  ( 0.7071067811865487940, -0.7071067811865462405, -4.216150419019403701E-15 ) ) ;
#11834 = CARTESIAN_POINT ( 'NONE',  ( -16.97048326478264713, 66.05000000001157900, -56.38200060439721284 ) ) ;
#11835 = EDGE_LOOP ( 'NONE', ( #100292, #96571, #66921, #137758, #190948 ) ) ;
#11836 = CARTESIAN_POINT ( 'NONE',  ( -20.00857864376270001, 66.85000000001180354, -81.87310748452438247 ) ) ;
#11838 = EDGE_LOOP ( 'NONE', ( #238963, #7524, #256693, #75065, #254393, #132251, #133087, #131625, #219176, #231638, #73102, #181645, #248350, #18936 ) ) ;
#11837 = CYLINDRICAL_SURFACE ( 'NONE', #246760, 0.1000000000000124678 ) ;
#11839 = LINE ( 'NONE', #91359, #225702 ) ;
#11840 = DIRECTION ( 'NONE',  ( -1.000000000000000000, -2.952720810173289112E-16, 0.000000000000000000 ) ) ;
#11841 = ORIENTED_EDGE ( 'NONE', *, *, #33972, .F. ) ;
#11842 = CARTESIAN_POINT ( 'NONE',  ( 23.24999999999999289, 11.65000000001116298, -134.0000000000000000 ) ) ;
#11843 = CIRCLE ( 'NONE', #53327, 0.5000000000000004441 ) ;
#11844 = PRODUCT_CONTEXT ( 'NONE', #168951, 'mechanical' ) ;
#11845 = CARTESIAN_POINT ( 'NONE',  ( 21.30000000000002558, 1.115600667400684642E-11, -71.05000000000003979 ) ) ;
#11846 = DIRECTION ( 'NONE',  ( 0.000000000000000000, 2.775557561562812086E-13, 1.000000000000000000 ) ) ;
#11847 = CARTESIAN_POINT ( 'NONE',  ( -18.46093223321785359, 85.48068296828637358, -95.93855697059757404 ) ) ;
#11848 = ORIENTED_EDGE ( 'NONE', *, *, #101714, .T. ) ;
#11849 = DIRECTION ( 'NONE',  ( 0.000000000000000000, 0.9998779222360100194, 0.01562499999998606150 ) ) ;
#11850 = FACE_OUTER_BOUND ( 'NONE', #80631, .T. ) ;
#11851 = CARTESIAN_POINT ( 'NONE',  ( -20.54999999999999716, 9.614325556249161409, -211.5456030694648746 ) ) ;
#11852 = ORIENTED_EDGE ( 'NONE', *, *, #191270, .T. ) ;
#11853 = ORIENTED_EDGE ( 'NONE', *, *, #5514, .F. ) ;
#11854 = FACE_OUTER_BOUND ( 'NONE', #136239, .T. ) ;
#11855 = EDGE_CURVE ( 'NONE', #24047, #241077, #63962, .T. ) ;
#11856 = CARTESIAN_POINT ( 'NONE',  ( -23.24999999999999645, -9.599999999988845900, -174.1001893912220737 ) ) ;
#11857 = CARTESIAN_POINT ( 'NONE',  ( 18.59999999999999076, 64.35000000001177511, -78.17310748452437963 ) ) ;
#11858 = FACE_OUTER_BOUND ( 'NONE', #139824, .T. ) ;
#11859 = EDGE_CURVE ( 'NONE', #196416, #119125, #91046, .T. ) ;
#11861 = DIRECTION ( 'NONE',  ( 1.000000000000000000, 0.000000000000000000, 0.000000000000000000 ) ) ;
#11860 = CARTESIAN_POINT ( 'NONE',  ( -20.94999999999999929, 74.16465844978765176, -124.9679561919613207 ) ) ;
#11862 = CIRCLE ( 'NONE', #3446, 2.000000000000001776 ) ;
#11863 = AXIS2_PLACEMENT_3D ( 'NONE', #195923, #99342, #178946 ) ;
#11865 = DIRECTION ( 'NONE',  ( 1.000000000000000000, 0.000000000000000000, 0.000000000000000000 ) ) ;
#11864 = AXIS2_PLACEMENT_3D ( 'NONE', #225907, #104670, #5581 ) ;
#11866 = CARTESIAN_POINT ( 'NONE',  ( -17.80356949363585528, 65.12326860301367049, -113.3100344602850953 ) ) ;
#11867 = AXIS2_PLACEMENT_3D ( 'NONE', #165105, #189804, #132395 ) ;
#11868 = CARTESIAN_POINT ( 'NONE',  ( -17.71734398241073905, 12.78051993042367585, -208.7322573998702353 ) ) ;
#11869 = VERTEX_POINT ( 'NONE', #53199 ) ;
#11871 = EDGE_LOOP ( 'NONE', ( #61285, #212405, #117586, #30097, #106841, #7890 ) ) ;
#11870 = CARTESIAN_POINT ( 'NONE',  ( 13.12229106158771685, 62.91120958565417709, -215.7552931531716638 ) ) ;
#11872 = SPHERICAL_SURFACE ( 'NONE', #60234, 0.1000000000000000056 ) ;
#11873 = DIRECTION ( 'NONE',  ( 1.836970198721029934E-16, 1.000000000000000000, 6.982962677686266711E-15 ) ) ;
#11875 = CARTESIAN_POINT ( 'NONE',  ( -18.40000000000000213, 43.47495547423554996, -233.9258172596817076 ) ) ;
#11874 = DIRECTION ( 'NONE',  ( 0.000000000000000000, 0.000000000000000000, -1.000000000000000000 ) ) ;
#11876 = EDGE_CURVE ( 'NONE', #89611, #174523, #154900, .T. ) ;
#11877 = ORIENTED_EDGE ( 'NONE', *, *, #146118, .F. ) ;
#11878 = CARTESIAN_POINT ( 'NONE',  ( -21.44999999999999929, 53.08776555244186568, -234.2469744149522626 ) ) ;
#11879 = CARTESIAN_POINT ( 'NONE',  ( 19.75857864376268935, 64.25000000001196554, -111.7731074845243882 ) ) ;
#11880 = LINE ( 'NONE', #247893, #153596 ) ;
#11881 = FACE_OUTER_BOUND ( 'NONE', #94670, .T. ) ;
#11882 = EDGE_CURVE ( 'NONE', #201448, #252440, #195309, .T. ) ;
#11883 = ORIENTED_EDGE ( 'NONE', *, *, #16699, .F. ) ;
#11884 = ORIENTED_EDGE ( 'NONE', *, *, #54620, .T. ) ;
#11885 = AXIS2_PLACEMENT_3D ( 'NONE', #109948, #13437, #12169 ) ;
#11887 = CIRCLE ( 'NONE', #166011, 0.09999999999999939493 ) ;
#11886 = CARTESIAN_POINT ( 'NONE',  ( 20.94999999999999574, 74.75000000001189449, -95.02310748452431710 ) ) ;
#11888 = EDGE_CURVE ( 'NONE', #221991, #217842, #16657, .T. ) ;
#11889 = VERTEX_POINT ( 'NONE', #171903 ) ;
#11890 = FACE_OUTER_BOUND ( 'NONE', #218314, .T. ) ;
#11892 = CARTESIAN_POINT ( 'NONE',  ( 20.94999999999999929, -8.999999999988842703, -124.1060308773475924 ) ) ;
#11891 = CIRCLE ( 'NONE', #207517, 0.09999999999999939493 ) ;
#11893 = CARTESIAN_POINT ( 'NONE',  ( 18.52928932188133970, 10.27928932189250411, -91.65000000000004832 ) ) ;
#11894 = FACE_OUTER_BOUND ( 'NONE', #36096, .T. ) ;
#11895 = ORIENTED_EDGE ( 'NONE', *, *, #124581, .T. ) ;
#11896 = DIRECTION ( 'NONE',  ( -1.000000000000000000, 0.000000000000000000, 0.000000000000000000 ) ) ;
#11897 = EDGE_CURVE ( 'NONE', #181640, #179663, #47186, .T. ) ;
#11898 = FACE_OUTER_BOUND ( 'NONE', #133737, .T. ) ;
#11899 = DIRECTION ( 'NONE',  ( 0.000000000000000000, -0.9999631594459056361, -0.008583690987124413183 ) ) ;
#11900 = CARTESIAN_POINT ( 'NONE',  ( -21.05000000000000071, 1.115600667400684642E-11, -167.5000000000000284 ) ) ;
#11901 = LINE ( 'NONE', #189239, #247679 ) ;
#11902 = CARTESIAN_POINT ( 'NONE',  ( -18.59999999999999787, 77.16270174995064224, -195.5231074845243313 ) ) ;
#11903 = CARTESIAN_POINT ( 'NONE',  ( 20.94999999999999574, 69.45000000001188312, -93.17928539484123007 ) ) ;
#11904 = CIRCLE ( 'NONE', #49480, 0.9750000000000036415 ) ;
#11905 = ORIENTED_EDGE ( 'NONE', *, *, #114747, .T. ) ;
#11907 = CARTESIAN_POINT ( 'NONE',  ( 18.59999999999999076, 11.65000000001115943, -158.8500000000000227 ) ) ;
#11906 = CARTESIAN_POINT ( 'NONE',  ( -23.25000000000000000, 76.10000000001203091, -114.6726782920691079 ) ) ;
#11909 = ORIENTED_EDGE ( 'NONE', *, *, #61557, .F. ) ;
#11908 = AXIS2_PLACEMENT_3D ( 'NONE', #41848, #161796, #122663 ) ;
#11911 = ORIENTED_EDGE ( 'NONE', *, *, #248792, .F. ) ;
#11910 = CARTESIAN_POINT ( 'NONE',  ( 20.94999999999999574, -1.851028230129704522, -145.6539132694225032 ) ) ;
#11912 = TOROIDAL_SURFACE ( 'NONE', #7801, 0.6000000000000015321, 0.1000000000000000056 ) ;
#11913 = VERTEX_POINT ( 'NONE', #96156 ) ;
#11914 = CARTESIAN_POINT ( 'NONE',  ( -16.94878442675512531, 9.991729103002162660, -146.6117804243621379 ) ) ;
#11915 = CARTESIAN_POINT ( 'NONE',  ( 15.07585980824112326, 66.58236703690597835, -151.8741590187921986 ) ) ;
#11916 = LINE ( 'NONE', #169724, #118260 ) ;
#11917 = CARTESIAN_POINT ( 'NONE',  ( 21.05000000000000071, 1.115600667400684642E-11, -134.0000000000000284 ) ) ;
#11918 = ORIENTED_EDGE ( 'NONE', *, *, #79808, .T. ) ;
#11919 = CARTESIAN_POINT ( 'NONE',  ( 21.05000000000000426, 69.74118280533120640, -203.5567402198580567 ) ) ;
#11920 = VECTOR ( 'NONE', #183628, 1000.000000000000000 ) ;
#11921 = CYLINDRICAL_SURFACE ( 'NONE', #168739, 0.09999999999999939493 ) ;
#11922 = VERTEX_POINT ( 'NONE', #74083 ) ;
#11923 = SPHERICAL_SURFACE ( 'NONE', #160622, 0.1000000000000000056 ) ;
#11924 = DIRECTION ( 'NONE',  ( 0.000000000000000000, 1.000000000000000000, 6.982962677686266711E-15 ) ) ;
#11925 = AXIS2_PLACEMENT_3D ( 'NONE', #48197, #126453, #143448 ) ;
#11926 = ORIENTED_EDGE ( 'NONE', *, *, #161545, .T. ) ;
#11927 = DIRECTION ( 'NONE',  ( 0.000000000000000000, -6.982962677686266711E-15, 1.000000000000000000 ) ) ;
#11928 = TOROIDAL_SURFACE ( 'NONE', #57849, 0.4000000000000012990, 0.1000000000000000056 ) ;
#11929 = EDGE_CURVE ( 'NONE', #183157, #67224, #163913, .T. ) ;
#11930 = EDGE_LOOP ( 'NONE', ( #37031, #81659, #142316, #75237 ) ) ;
#11932 = ORIENTED_EDGE ( 'NONE', *, *, #15096, .T. ) ;
#11931 = CIRCLE ( 'NONE', #178528, 0.8750000000000007772 ) ;
#11933 = CARTESIAN_POINT ( 'NONE',  ( 21.14999999999998082, -11.75000000000000000, 3.469446951953614189E-15 ) ) ;
#11934 = DIRECTION ( 'NONE',  ( 0.000000000000000000, 0.000000000000000000, -1.000000000000000000 ) ) ;
#11935 = DIRECTION ( 'NONE',  ( 0.000000000000000000, -1.000000000000000000, -6.982962677686266711E-15 ) ) ;
#11936 = EDGE_CURVE ( 'NONE', #172629, #99187, #72798, .T. ) ;
#11937 = FACE_OUTER_BOUND ( 'NONE', #18043, .T. ) ;
#11938 = CIRCLE ( 'NONE', #57692, 0.1000000000000055844 ) ;
#11939 = ADVANCED_FACE ( 'NONE', ( #94884 ), #147161, .T. ) ;
#11940 = ADVANCED_FACE ( 'NONE', ( #255189 ), #9778, .T. ) ;
#11941 = DIRECTION ( 'NONE',  ( 0.000000000000000000, 0.000000000000000000, 1.000000000000000000 ) ) ;
#11942 = AXIS2_PLACEMENT_3D ( 'NONE', #236050, #36607, #135652 ) ;
#11943 = DIRECTION ( 'NONE',  ( 0.000000000000000000, -0.4088369013363783999, 0.9126074666063545004 ) ) ;
#11944 = ORIENTED_EDGE ( 'NONE', *, *, #39954, .F. ) ;
#11945 = CARTESIAN_POINT ( 'NONE',  ( 20.94999999999999574, 1.261786168576181755, -41.58649896354548048 ) ) ;
#11946 = ORIENTED_EDGE ( 'NONE', *, *, #17270, .T. ) ;
#11948 = CARTESIAN_POINT ( 'NONE',  ( 20.94999999999999574, -1.249999999999999334, -8.000000000000000000 ) ) ;
#11947 = CARTESIAN_POINT ( 'NONE',  ( 18.54999999999999716, 12.98648691417778167, -219.5104337504080263 ) ) ;
#11949 = CIRCLE ( 'NONE', #220222, 0.1000000000000117045 ) ;
#11950 = EDGE_LOOP ( 'NONE', ( #231355, #130360, #170042, #70727 ) ) ;
#11951 = DIRECTION ( 'NONE',  ( 0.000000000000000000, 0.000000000000000000, 1.000000000000000000 ) ) ;
#11952 = AXIS2_PLACEMENT_3D ( 'NONE', #236318, #57665, #160670 ) ;
#11953 = VECTOR ( 'NONE', #31341, 1000.000000000000000 ) ;
#11954 = AXIS2_PLACEMENT_3D ( 'NONE', #255715, #38030, #60115 ) ;
#11955 = DIRECTION ( 'NONE',  ( 0.000000000000000000, 0.9916376685811618685, -0.1290532225514649800 ) ) ;
#11956 = CARTESIAN_POINT ( 'NONE',  ( -20.94999999999999929, 74.25000000001259082, -191.8535959266227451 ) ) ;
#11957 = ORIENTED_EDGE ( 'NONE', *, *, #200757, .F. ) ;
#11959 = ORIENTED_EDGE ( 'NONE', *, *, #84250, .F. ) ;
#11958 = DIRECTION ( 'NONE',  ( -1.000000000000000000, -0.000000000000000000, -0.000000000000000000 ) ) ;
#11960 = ADVANCED_FACE ( 'NONE', ( #156180 ), #55723, .F. ) ;
#11961 = CIRCLE ( 'NONE', #191016, 0.1000000000000013933 ) ;
#11962 = EDGE_CURVE ( 'NONE', #189515, #193526, #138922, .T. ) ;
#11964 = CARTESIAN_POINT ( 'NONE',  ( -20.64999999999999858, 7.128833340094563376, -233.7327013124401276 ) ) ;
#11963 = CARTESIAN_POINT ( 'NONE',  ( 21.56666275994539816, -1.480534921131848591, -194.2019862094512064 ) ) ;
#11966 = ORIENTED_EDGE ( 'NONE', *, *, #58445, .F. ) ;
#11965 = CARTESIAN_POINT ( 'NONE',  ( -23.15000000000000213, 11.65000000001115588, -126.9851942293460922 ) ) ;
#11967 = ORIENTED_EDGE ( 'NONE', *, *, #245641, .T. ) ;
#11968 = VECTOR ( 'NONE', #200230, 1000.000000000000114 ) ;
#11969 = AXIS2_PLACEMENT_3D ( 'NONE', #11851, #232177, #151358 ) ;
#11970 = SPHERICAL_SURFACE ( 'NONE', #10311, 0.1000000000000000056 ) ;
#11971 = DIRECTION ( 'NONE',  ( 1.000000000000000000, 2.952720810173289112E-16, -0.000000000000000000 ) ) ;
#11972 = VERTEX_POINT ( 'NONE', #174491 ) ;
#11973 = VERTEX_POINT ( 'NONE', #14091 ) ;
#11974 = EDGE_CURVE ( 'NONE', #16838, #54351, #180489, .T. ) ;
#11976 = EDGE_CURVE ( 'NONE', #163656, #254080, #252670, .T. ) ;
#11975 = DIRECTION ( 'NONE',  ( 7.304098846218134667E-16, 0.4088369013363281068, -0.9126074666063770380 ) ) ;
#11977 = CARTESIAN_POINT ( 'NONE',  ( 21.72449340488910252, 10.28395627750227703, -146.6500000000000341 ) ) ;
#11978 = ADVANCED_FACE ( 'NONE', ( #92320 ), #131451, .F. ) ;
#11979 = ORIENTED_EDGE ( 'NONE', *, *, #34248, .F. ) ;
#11980 = CARTESIAN_POINT ( 'NONE',  ( -20.94999999999999929, 68.11887992016828264, -227.8068560890360175 ) ) ;
#11981 = VECTOR ( 'NONE', #93219, 1000.000000000000000 ) ;
#11982 = CIRCLE ( 'NONE', #241120, 0.09999999999999938105 ) ;
#11984 = EDGE_LOOP ( 'NONE', ( #34816, #148366, #187214, #80304 ) ) ;
#11983 = AXIS2_PLACEMENT_3D ( 'NONE', #173543, #59932, #139479 ) ;
#11985 = LINE ( 'NONE', #211444, #197766 ) ;
#11986 = CIRCLE ( 'NONE', #45280, 0.1000000000000028644 ) ;
#11987 = EDGE_LOOP ( 'NONE', ( #236841, #230235, #218852, #15222 ) ) ;
#11988 = EDGE_LOOP ( 'NONE', ( #31961, #10312, #232108, #36964 ) ) ;
#11989 = DIRECTION ( 'NONE',  ( 0.000000000000000000, -1.000000000000000000, -0.000000000000000000 ) ) ;
#11990 = VERTEX_POINT ( 'NONE', #196552 ) ;
#11991 = DIRECTION ( 'NONE',  ( 0.000000000000000000, 0.000000000000000000, -1.000000000000000000 ) ) ;
#11992 = ORIENTED_EDGE ( 'NONE', *, *, #151471, .T. ) ;
#11994 = EDGE_LOOP ( 'NONE', ( #32153, #171502, #64550, #256901 ) ) ;
#11993 = DIRECTION ( 'NONE',  ( -1.000000000000000000, -1.541880601228652843E-16, -2.878400969107353907E-16 ) ) ;
#11995 = AXIS2_PLACEMENT_3D ( 'NONE', #94146, #254481, #172453 ) ;
#11996 = VERTEX_POINT ( 'NONE', #17911 ) ;
#11997 = CARTESIAN_POINT ( 'NONE',  ( 23.24999999999999289, 69.35000000001205933, -124.3731074845243540 ) ) ;
#11998 = AXIS2_PLACEMENT_3D ( 'NONE', #41659, #200714, #167706 ) ;
#11999 = ORIENTED_EDGE ( 'NONE', *, *, #134145, .F. ) ;
#12003 = ADVANCED_FACE ( 'NONE', ( #71508 ), #54476, .T. ) ;
#12002 = ORIENTED_EDGE ( 'NONE', *, *, #44587, .T. ) ;
#12001 = EDGE_LOOP ( 'NONE', ( #198106, #195753, #84223, #137689 ) ) ;
#12000 = FACE_OUTER_BOUND ( 'NONE', #240551, .T. ) ;
#12004 = AXIS2_PLACEMENT_3D ( 'NONE', #81226, #121683, #198623 ) ;
#12005 = CARTESIAN_POINT ( 'NONE',  ( 23.14999999999999503, 64.35000000001186038, -90.77310748452438816 ) ) ;
#12006 = ORIENTED_EDGE ( 'NONE', *, *, #100552, .F. ) ;
#12007 = DIRECTION ( 'NONE',  ( 1.000000000000000000, -0.000000000000000000, -0.000000000000000000 ) ) ;
#12008 = VERTEX_POINT ( 'NONE', #111910 ) ;
#12009 = ADVANCED_FACE ( 'NONE', ( #256465 ), #119611, .F. ) ;
#12010 = DIRECTION ( 'NONE',  ( 1.000000000000000000, -4.851622311275597861E-17, 1.082981191754466620E-16 ) ) ;
#12012 = VERTEX_POINT ( 'NONE', #219971 ) ;
#12011 = DIRECTION ( 'NONE',  ( -1.836970198721029934E-16, 1.000000000000000000, 0.000000000000000000 ) ) ;
#12013 = DIRECTION ( 'NONE',  ( 1.000000000000000000, 0.000000000000000000, 0.000000000000000000 ) ) ;
#12014 = ORIENTED_EDGE ( 'NONE', *, *, #130601, .T. ) ;
#12015 = CARTESIAN_POINT ( 'NONE',  ( 21.05000000000000071, 65.31570632562468859, -95.49643354588684474 ) ) ;
#12016 = LINE ( 'NONE', #69418, #173208 ) ;
#12017 = AXIS2_PLACEMENT_3D ( 'NONE', #83044, #4804, #106467 ) ;
#12019 = ORIENTED_EDGE ( 'NONE', *, *, #66794, .T. ) ;
#12018 = EDGE_CURVE ( 'NONE', #231216, #4559, #188860, .T. ) ;
#12020 = CARTESIAN_POINT ( 'NONE',  ( 23.14999999999999503, 42.98415524044398950, -233.9519173640447889 ) ) ;
#12021 = CARTESIAN_POINT ( 'NONE',  ( -20.94999999999999929, 77.83534155023670564, -158.4679561919613491 ) ) ;
#12022 = EDGE_CURVE ( 'NONE', #39510, #43703, #109734, .T. ) ;
#12023 = ORIENTED_EDGE ( 'NONE', *, *, #245277, .F. ) ;
#12025 = EDGE_LOOP ( 'NONE', ( #138536, #106594, #133117, #116553 ) ) ;
#12024 = CARTESIAN_POINT ( 'NONE',  ( 18.79999999999999716, -1.311673547813416718, -7.986648289447971116 ) ) ;
#12026 = CARTESIAN_POINT ( 'NONE',  ( -23.15000000000000213, 6.268811756569107274, -220.3853799378769622 ) ) ;
#12027 = ADVANCED_FACE ( 'NONE', ( #218674 ), #161305, .T. ) ;
#12029 = ORIENTED_EDGE ( 'NONE', *, *, #152628, .F. ) ;
#12028 = VERTEX_POINT ( 'NONE', #41368 ) ;
#12030 = ORIENTED_EDGE ( 'NONE', *, *, #238390, .F. ) ;
#12032 = EDGE_CURVE ( 'NONE', #160190, #141186, #42619, .T. ) ;
#12031 = DIRECTION ( 'NONE',  ( 1.000000000000000000, 0.000000000000000000, 0.000000000000000000 ) ) ;
#12033 = EDGE_LOOP ( 'NONE', ( #83231, #95866, #190917, #69683 ) ) ;
#12034 = EDGE_LOOP ( 'NONE', ( #45854, #190011, #234382, #60658, #57954, #130703, #178062, #200215, #222279, #72952, #48247, #168573, #231722, #169549 ) ) ;
#12035 = DIRECTION ( 'NONE',  ( 1.000000000000000000, 0.000000000000000000, 0.000000000000000000 ) ) ;
#12036 = ORIENTED_EDGE ( 'NONE', *, *, #42241, .F. ) ;
#12037 = CARTESIAN_POINT ( 'NONE',  ( -23.25000000000000000, 7.128833340094563376, -233.7327013124401276 ) ) ;
#12038 = CARTESIAN_POINT ( 'NONE',  ( -23.25000000000000000, 7.128833340094563376, -233.7327013124401276 ) ) ;
#12039 = ORIENTED_EDGE ( 'NONE', *, *, #175617, .F. ) ;
#12040 = VERTEX_POINT ( 'NONE', #21789 ) ;
#12041 = AXIS2_PLACEMENT_3D ( 'NONE', #152676, #53544, #174824 ) ;
#12042 = LINE ( 'NONE', #91557, #13207 ) ;
#12043 = CIRCLE ( 'NONE', #195389, 0.1000000000000028644 ) ;
#12044 = VECTOR ( 'NONE', #43566, 1000.000000000000000 ) ;
#12045 = ORIENTED_EDGE ( 'NONE', *, *, #117720, .T. ) ;
#12046 = EDGE_CURVE ( 'NONE', #9522, #110542, #38249, .T. ) ;
#12047 = EDGE_CURVE ( 'NONE', #169411, #11593, #893, .T. ) ;
#12048 = AXIS2_PLACEMENT_3D ( 'NONE', #21430, #100888, #141347 ) ;
#12049 = LINE ( 'NONE', #236199, #234659 ) ;
#12050 = VERTEX_POINT ( 'NONE', #160026 ) ;
#12051 = ADVANCED_FACE ( 'NONE', ( #120906 ), #239544, .F. ) ;
#12052 = CARTESIAN_POINT ( 'NONE',  ( -20.00857864376270001, 66.85000000001156195, -57.17310748452438673 ) ) ;
#12054 = ORIENTED_EDGE ( 'NONE', *, *, #229318, .T. ) ;
#12053 = CARTESIAN_POINT ( 'NONE',  ( -22.16821283564876666, 68.44102665923159634, -170.0231074845243882 ) ) ;
#12055 = DIRECTION ( 'NONE',  ( 1.836970198721029934E-16, -1.000000000000000000, -0.000000000000000000 ) ) ;
#12056 = LINE ( 'NONE', #168591, #55975 ) ;
#12057 = CARTESIAN_POINT ( 'NONE',  ( 21.05000000000005400, 87.75000000001119815, -43.82310748452479743 ) ) ;
#12058 = DIRECTION ( 'NONE',  ( 0.000000000000000000, 0.9651348961777157509, -0.2617529984165031243 ) ) ;
#12059 = DIRECTION ( 'NONE',  ( 0.000000000000000000, -1.000000000000000000, -6.982962677686266711E-15 ) ) ;
#12060 = DIRECTION ( 'NONE',  ( 1.000000000000000000, 0.000000000000000000, 0.000000000000000000 ) ) ;
#12062 = DIRECTION ( 'NONE',  ( 1.000000000000000000, 0.000000000000000000, 0.000000000000000000 ) ) ;
#12061 = AXIS2_PLACEMENT_3D ( 'NONE', #107238, #128095, #224610 ) ;
#12064 = CARTESIAN_POINT ( 'NONE',  ( 23.25000000000000355, 2.513905990859601314, -256.7358755158824692 ) ) ;
#12063 = CIRCLE ( 'NONE', #37004, 0.09999999999999939493 ) ;
#12066 = EDGE_CURVE ( 'NONE', #109393, #256406, #178309, .T. ) ;
#12065 = CARTESIAN_POINT ( 'NONE',  ( 18.46932045258611765, 37.97547201091887814, -261.2271751612549906 ) ) ;
#12067 = CIRCLE ( 'NONE', #174406, 0.09999999999998898659 ) ;
#12068 = CARTESIAN_POINT ( 'NONE',  ( -20.54999999999999716, 2.499999999999998668, -20.27537807723789953 ) ) ;
#12069 = EDGE_CURVE ( 'NONE', #248870, #107706, #234839, .T. ) ;
#12070 = ORIENTED_EDGE ( 'NONE', *, *, #76404, .T. ) ;
#12071 = AXIS2_PLACEMENT_3D ( 'NONE', #91897, #72363, #29404 ) ;
#12072 = EDGE_CURVE ( 'NONE', #56619, #67927, #38778, .T. ) ;
#12074 = ORIENTED_EDGE ( 'NONE', *, *, #243016, .T. ) ;
#12073 = EDGE_LOOP ( 'NONE', ( #30455, #46079, #213745, #154993 ) ) ;
#12075 = ORIENTED_EDGE ( 'NONE', *, *, #239776, .T. ) ;
#12076 = LINE ( 'NONE', #206401, #78413 ) ;
#12077 =( BOUNDED_SURFACE ( )  B_SPLINE_SURFACE ( 3, 2, ( 
 ( #85502, #2141, #82939 ),
 ( #3422, #45134, #26884 ),
 ( #125938, #43858, #81654 ),
 ( #103796, #141662, #144214 ),
 ( #124679, #165080, #106367 ),
 ( #219919, #185925, #86808 ) ),
 .UNSPECIFIED., .F., .F., .F. ) 
 B_SPLINE_SURFACE_WITH_KNOTS ( ( 4, 2, 4 ),
 ( 3, 3 ),
 ( 4.712388980384689674, 5.497787143782137953, 6.283185307179586232 ),
 ( 0.000000000000000000, 1.000000000000000000 ),
 .UNSPECIFIED. ) 
 GEOMETRIC_REPRESENTATION_ITEM ( )  RATIONAL_B_SPLINE_SURFACE ( (
 ( 1.000000000000000000, 0.7071067811865475727, 1.000000000000000000),
 ( 1.000000000000000000, 0.7727932973491635771, 1.000000000000000000),
 ( 1.000000000000000000, 0.8282379607649708042, 1.000000000000000000),
 ( 1.000000000000000000, 0.9038128468039490215, 1.000000000000000000),
 ( 1.000000000000000000, 0.9240297172243560064, 1.000000000000000000),
 ( 1.000000000000000000, 0.9238795325112961754, 1.000000000000000000) ) ) 
 REPRESENTATION_ITEM ( '' )  SURFACE ( )  );
#12078 = CARTESIAN_POINT ( 'NONE',  ( -20.64999999999999858, -8.999999999988846255, -143.8939691226524644 ) ) ;
#12079 = LINE ( 'NONE', #152886, #16054 ) ;
#12080 = EDGE_CURVE ( 'NONE', #53606, #250417, #164761, .T. ) ;
#12081 = B_SPLINE_CURVE_WITH_KNOTS ( 'NONE', 3,
 ( #160857, #46017, #20059, #143826, #85112, #223364, #220806, #460, #42187, #121732, #102114, #181693, #3027, #164696, #44753, #65586, #99546, #63011, #82547 ),
 .UNSPECIFIED., .F., .F.,
 ( 4, 3, 3, 3, 3, 3, 4 ),
 ( 0.000000000000000000, 7.110282409889913185E-05, 0.0001508797727291427476, 0.0002027344179858411031, 0.0002343294522349015981, 0.0002454816334821165657, 0.0002619873080085518072 ),
 .UNSPECIFIED. ) ;
#12082 = ORIENTED_EDGE ( 'NONE', *, *, #208396, .T. ) ;
#12083 = EDGE_LOOP ( 'NONE', ( #234998, #83510, #151972 ) ) ;
#12084 = SHAPE_REPRESENTATION_RELATIONSHIP ( 'NONE' , 'NONE' ,  #106899, #154111 ) ;
#12085 = LINE ( 'NONE', #171182, #37493 ) ;
#12086 = CARTESIAN_POINT ( 'NONE',  ( 18.58222699835054570, 10.33200063080772324, -173.0931674956643178 ) ) ;
#12087 = LINE ( 'NONE', #172467, #141427 ) ;
#12088 = VERTEX_POINT ( 'NONE', #140423 ) ;
#12089 = ORIENTED_EDGE ( 'NONE', *, *, #95848, .T. ) ;
#12090 = CIRCLE ( 'NONE', #150118, 0.1000000000000028644 ) ;
#12091 = VECTOR ( 'NONE', #253039, 1000.000000000000000 ) ;
#12092 = DIRECTION ( 'NONE',  ( 0.000000000000000000, -0.2605042016806740079, 0.9654727137038698892 ) ) ;
#12093 = LINE ( 'NONE', #32959, #142833 ) ;
#12094 = CARTESIAN_POINT ( 'NONE',  ( -20.07928932188135107, 9.220710678129810489, -45.85000000000000142 ) ) ;
#12096 = ORIENTED_EDGE ( 'NONE', *, *, #119972, .F. ) ;
#12095 = CARTESIAN_POINT ( 'NONE',  ( 20.94999999999999929, 7.128833340094563376, -233.7327013124401276 ) ) ;
#12097 = CIRCLE ( 'NONE', #199543, 11.64999999999999325 ) ;
#12098 = FACE_OUTER_BOUND ( 'NONE', #224572, .T. ) ;
#12099 = CARTESIAN_POINT ( 'NONE',  ( -20.94999999999999929, 7.070967871809997973, -70.74656422186831151 ) ) ;
#12100 = DIRECTION ( 'NONE',  ( 0.000000000000000000, 0.2605042016806715099, 0.9654727137038706664 ) ) ;
#12101 = PLANE ( 'NONE',  #4357 ) ;
#12102 = ORIENTED_EDGE ( 'NONE', *, *, #216926, .T. ) ;
#12103 = CARTESIAN_POINT ( 'NONE',  ( 13.43663047529820709, 66.55335465531658201, -84.61230102842419853 ) ) ;
#12104 = FACE_BOUND ( 'NONE', #141237, .T. ) ;
#12106 = DIRECTION ( 'NONE',  ( 0.000000000000000000, 1.000000000000000000, 0.000000000000000000 ) ) ;
#12105 = LINE ( 'NONE', #89036, #49317 ) ;
#12107 = CARTESIAN_POINT ( 'NONE',  ( -18.59999999999999787, -1.835341550213255957, -179.1551512925629197 ) ) ;
#12108 = LINE ( 'NONE', #250681, #99234 ) ;
#12109 = DIRECTION ( 'NONE',  ( -1.000000000000000000, 0.000000000000000000, 0.000000000000000000 ) ) ;
#12110 = CARTESIAN_POINT ( 'NONE',  ( -16.77732147262506146, 66.05403306739287927, -48.68661624124851528 ) ) ;
#12111 = CIRCLE ( 'NONE', #57847, 0.09999999999999939493 ) ;
#12112 = CIRCLE ( 'NONE', #220386, 4.049999999999998934 ) ;
#12113 = LINE ( 'NONE', #90321, #616 ) ;
#12114 = DIRECTION ( 'NONE',  ( 1.000000000000000000, 0.000000000000000000, 0.000000000000000000 ) ) ;
#12115 = AXIS2_PLACEMENT_3D ( 'NONE', #203398, #204657, #168161 ) ;
#12116 = VERTEX_POINT ( 'NONE', #141712 ) ;
#12117 = CIRCLE ( 'NONE', #45402, 4.049999999999998046 ) ;
#12118 = ORIENTED_EDGE ( 'NONE', *, *, #242706, .T. ) ;
#12119 = ORIENTED_EDGE ( 'NONE', *, *, #192141, .F. ) ;
#12120 = ADVANCED_FACE ( 'NONE', ( #221238 ), #3482, .F. ) ;
#12121 = DIRECTION ( 'NONE',  ( -2.342056488767301376E-15, -0.1350103645451904977, 0.9908441862701596881 ) ) ;
#12122 = LINE ( 'NONE', #212871, #123644 ) ;
#12123 = ORIENTED_EDGE ( 'NONE', *, *, #150110, .F. ) ;
#12124 = TOROIDAL_SURFACE ( 'NONE', #220398, 11.70000000000000107, 0.1000000000000000056 ) ;
#12125 = AXIS2_PLACEMENT_3D ( 'NONE', #246292, #67644, #10254 ) ;
#12126 = ORIENTED_EDGE ( 'NONE', *, *, #183866, .F. ) ;
#12127 = EDGE_CURVE ( 'NONE', #146487, #130685, #182140, .T. ) ;
#12128 = ORIENTED_EDGE ( 'NONE', *, *, #219778, .T. ) ;
#12129 = CARTESIAN_POINT ( 'NONE',  ( 21.53551880898956838, 6.784797761427480367, -66.90103026542837483 ) ) ;
#12130 = VERTEX_POINT ( 'NONE', #163860 ) ;
#12131 = AXIS2_PLACEMENT_3D ( 'NONE', #118242, #154829, #55658 ) ;
#12132 = DIRECTION ( 'NONE',  ( -0.000000000000000000, -0.000000000000000000, 1.000000000000000000 ) ) ;
#12133 = AXIS2_PLACEMENT_3D ( 'NONE', #176075, #239881, #75681 ) ;
#12134 = CIRCLE ( 'NONE', #195299, 0.4000000000000114575 ) ;
#12135 = DIRECTION ( 'NONE',  ( 0.000000000000000000, 0.000000000000000000, -1.000000000000000000 ) ) ;
#12136 = CARTESIAN_POINT ( 'NONE',  ( 23.14999999999999858, 76.00000000001142553, -36.02310748452432421 ) ) ;
#12137 = CIRCLE ( 'NONE', #257754, 0.09999999999999935330 ) ;
#12138 = DIRECTION ( 'NONE',  ( 0.000000000000000000, 0.000000000000000000, 1.000000000000000000 ) ) ;
#12139 = PLANE ( 'NONE',  #254002 ) ;
#12141 = ORIENTED_EDGE ( 'NONE', *, *, #145311, .T. ) ;
#12140 = CARTESIAN_POINT ( 'NONE',  ( -16.77180007708460963, 30.21900964602406248, -234.8138379153629387 ) ) ;
#12143 = CARTESIAN_POINT ( 'NONE',  ( 19.86930884467607328, 11.68691006698174739, -192.2392226389382301 ) ) ;
#12142 = DIRECTION ( 'NONE',  ( 0.000000000000000000, 0.000000000000000000, -1.000000000000000000 ) ) ;
#12144 = VECTOR ( 'NONE', #205078, 1000.000000000000000 ) ;
#12145 = CARTESIAN_POINT ( 'NONE',  ( -16.86420534634261514, 9.970615445602874161, -154.9183365492374094 ) ) ;
#12146 = DIRECTION ( 'NONE',  ( 1.073024830501117725E-15, -0.000000000000000000, -1.000000000000000000 ) ) ;
#12147 = CARTESIAN_POINT ( 'NONE',  ( -16.90138253750126651, 66.05000000001180638, -82.31154477661976898 ) ) ;
#12148 = CARTESIAN_POINT ( 'NONE',  ( 18.59999999999999787, 11.75000000000000000, 30.09999999999999787 ) ) ;
#12149 = ORIENTED_EDGE ( 'NONE', *, *, #181360, .F. ) ;
#12150 = PRESENTATION_STYLE_ASSIGNMENT (( #193341 ) ) ;
#12151 = DIRECTION ( 'NONE',  ( 0.000000000000000000, 0.2617529984165046231, 0.9651348961777154178 ) ) ;
#12152 = DIRECTION ( 'NONE',  ( 1.000000000000000000, 0.000000000000000000, 0.000000000000000000 ) ) ;
#12154 = ORIENTED_EDGE ( 'NONE', *, *, #175616, .T. ) ;
#12153 = MECHANICAL_DESIGN_GEOMETRIC_PRESENTATION_REPRESENTATION (  '', ( #191221 ), #257769 ) ;
#12155 = DIRECTION ( 'NONE',  ( 0.000000000000000000, -0.9999631594459053030, -0.008583690987162452199 ) ) ;
#12156 = FACE_OUTER_BOUND ( 'NONE', #116191, .T. ) ;
#12157 = CARTESIAN_POINT ( 'NONE',  ( 0.8999999999999995781, -9.650000000000003908, 23.40000000000000213 ) ) ;
#12158 = EDGE_LOOP ( 'NONE', ( #62416, #136439, #88320, #191658, #154857, #215888, #77129, #33848, #98345, #223296, #5565, #47566, #1520, #253492 ) ) ;
#12159 = ORIENTED_EDGE ( 'NONE', *, *, #131217, .F. ) ;
#12160 = AXIS2_PLACEMENT_3D ( 'NONE', #97395, #182113, #239519 ) ;
#12161 = EDGE_CURVE ( 'NONE', #104349, #149025, #230753, .T. ) ;
#12162 = CIRCLE ( 'NONE', #212061, 0.09999999999999939493 ) ;
#12163 = FACE_OUTER_BOUND ( 'NONE', #111676, .T. ) ;
#12164 = LINE ( 'NONE', #214195, #89805 ) ;
#12165 = CARTESIAN_POINT ( 'NONE',  ( 20.94999999999999929, 65.70729864261056719, -164.5657455973725121 ) ) ;
#12166 = PLANE ( 'NONE',  #52983 ) ;
#12167 = ADVANCED_FACE ( 'NONE', ( #225081 ), #4748, .F. ) ;
#12168 = DIRECTION ( 'NONE',  ( 0.000000000000000000, -6.997203936713171069E-15, 1.000000000000000000 ) ) ;
#12169 = DIRECTION ( 'NONE',  ( 0.000000000000000000, 0.2128009952263603122, -0.9770955615653315052 ) ) ;
#12170 = CARTESIAN_POINT ( 'NONE',  ( -23.25000000000000000, 79.19526988099229925, -196.1889237952725296 ) ) ;
#12171 = ORIENTED_EDGE ( 'NONE', *, *, #223484, .F. ) ;
#12172 = CARTESIAN_POINT ( 'NONE',  ( -23.49999999999994316, 76.00000000001119815, -31.87310748452479459 ) ) ;
#12173 = AXIS2_PLACEMENT_3D ( 'NONE', #155777, #76192, #131041 ) ;
#12175 = ORIENTED_EDGE ( 'NONE', *, *, #39512, .F. ) ;
#12174 = LINE ( 'NONE', #91686, #117030 ) ;
#12176 = FACE_OUTER_BOUND ( 'NONE', #167046, .T. ) ;
#12177 = DIRECTION ( 'NONE',  ( -1.000000000000000000, 0.000000000000000000, 0.000000000000000000 ) ) ;
#12178 = DIRECTION ( 'NONE',  ( 1.000000000000000000, -0.000000000000000000, -0.000000000000000000 ) ) ;
#12179 =( BOUNDED_CURVE ( )  B_SPLINE_CURVE ( 3, ( #253467, #111406, #110112, #74881 ),
 .UNSPECIFIED., .F., .T. ) 
 B_SPLINE_CURVE_WITH_KNOTS ( ( 4, 4 ),
 ( 0.3000847527772381174, 0.5497968875596821459 ),
 .UNSPECIFIED. ) 
 CURVE ( )  GEOMETRIC_REPRESENTATION_ITEM ( )  RATIONAL_B_SPLINE_CURVE ( ( 1.000000000000000000, 0.9948104011409419911, 0.9948104011409419911, 1.000000000000000000 ) ) 
 REPRESENTATION_ITEM ( '' )  );
#12180 = CARTESIAN_POINT ( 'NONE',  ( -18.59999999999999787, 77.83585931145570669, -125.0186683157258045 ) ) ;
#12181 = ADVANCED_FACE ( 'NONE', ( #25629 ), #139115, .F. ) ;
#12182 = CARTESIAN_POINT ( 'NONE',  ( 18.49999999999999289, 11.65000000001115943, -58.35000000000000142 ) ) ;
#12184 = ORIENTED_EDGE ( 'NONE', *, *, #60814, .F. ) ;
#12183 = CARTESIAN_POINT ( 'NONE',  ( 21.46681500593474112, 69.14248884062944001, -136.5231074845243597 ) ) ;
#12185 = FACE_OUTER_BOUND ( 'NONE', #244064, .T. ) ;
#12186 = CARTESIAN_POINT ( 'NONE',  ( -20.07928932188135107, 9.220710678129810489, -88.15000000000004832 ) ) ;
#12187 = CARTESIAN_POINT ( 'NONE',  ( 22.49544290803770608, 11.74987023786810880, -66.93468804074250045 ) ) ;
#12188 = DIRECTION ( 'NONE',  ( -1.000000000000000000, 0.000000000000000000, 0.000000000000000000 ) ) ;
#12189 = ADVANCED_FACE ( 'NONE', ( #29513 ), #49034, .T. ) ;
#12190 = VERTEX_POINT ( 'NONE', #204249 ) ;
#12191 = DIRECTION ( 'NONE',  ( -1.000000000000000000, 0.000000000000000000, 0.000000000000000000 ) ) ;
#12193 = EDGE_LOOP ( 'NONE', ( #166943, #71719, #227277 ) ) ;
#12192 = CIRCLE ( 'NONE', #203865, 0.09999999999998898659 ) ;
#12194 = AXIS2_PLACEMENT_3D ( 'NONE', #242576, #219155, #2678 ) ;
#12195 = CARTESIAN_POINT ( 'NONE',  ( -16.92507428761699018, 9.950000000011140600, -121.2866025403784960 ) ) ;
#12196 = EDGE_CURVE ( 'NONE', #54663, #61007, #206829, .T. ) ;
#12197 = VERTEX_POINT ( 'NONE', #88129 ) ;
#12198 = FACE_OUTER_BOUND ( 'NONE', #22720, .T. ) ;
#12199 = CIRCLE ( 'NONE', #157960, 0.09999999999998898659 ) ;
#12200 = ORIENTED_EDGE ( 'NONE', *, *, #47264, .T. ) ;
#12201 = DIRECTION ( 'NONE',  ( -1.000000000000000000, 0.000000000000000000, -0.000000000000000000 ) ) ;
#12202 = DIRECTION ( 'NONE',  ( 0.000000000000000000, 0.000000000000000000, -1.000000000000000000 ) ) ;
#12203 = CARTESIAN_POINT ( 'NONE',  ( -5.900000000000002132, -11.65000000000000036, 14.00000000000000178 ) ) ;
#12204 = ORIENTED_EDGE ( 'NONE', *, *, #236920, .F. ) ;
#12205 = EDGE_CURVE ( 'NONE', #139895, #220391, #129846, .T. ) ;
#12206 = CARTESIAN_POINT ( 'NONE',  ( -21.05000000000000071, 1.162701749949165642, -41.60000000000000142 ) ) ;
#12207 = DIRECTION ( 'NONE',  ( 0.000000000000000000, 1.000000000000000000, 0.000000000000000000 ) ) ;
#12208 = CARTESIAN_POINT ( 'NONE',  ( 21.05000000000000071, 28.55432187084631934, -258.5393726171218418 ) ) ;
#12210 = VECTOR ( 'NONE', #29880, 1000.000000000000114 ) ;
#12209 = CARTESIAN_POINT ( 'NONE',  ( 13.22461703343584638, 9.436662931799084220, -18.32303673229488794 ) ) ;
#12211 = CARTESIAN_POINT ( 'NONE',  ( -23.25000000000000000, 70.05000000001196270, -113.3288097895591591 ) ) ;
#12212 = VERTEX_POINT ( 'NONE', #6044 ) ;
#12213 = CARTESIAN_POINT ( 'NONE',  ( -18.33682934331526226, 85.51118559110554429, -129.6174527158510728 ) ) ;
#12214 = VERTEX_POINT ( 'NONE', #105117 ) ;
#12216 = ORIENTED_EDGE ( 'NONE', *, *, #144821, .T. ) ;
#12215 = CARTESIAN_POINT ( 'NONE',  ( -23.25000000000000000, 7.021664781911246322, -70.83356540189728889 ) ) ;
#12217 = ORIENTED_EDGE ( 'NONE', *, *, #12374, .T. ) ;
#12218 = CARTESIAN_POINT ( 'NONE',  ( -21.05000000000000071, 9.997527148596390134, -228.1702915402975691 ) ) ;
#12219 = VERTEX_POINT ( 'NONE', #124733 ) ;
#12220 = CARTESIAN_POINT ( 'NONE',  ( -16.87851181299898684, 66.04995707600485844, -190.8732509998913258 ) ) ;
#12221 = CARTESIAN_POINT ( 'NONE',  ( -20.64999999999999858, 76.00000000001172396, -71.42310748452430857 ) ) ;
#12222 = DIRECTION ( 'NONE',  ( -0.000000000000000000, -0.000000000000000000, 1.000000000000000000 ) ) ;
#12223 = VERTEX_POINT ( 'NONE', #26938 ) ;
#12224 = CARTESIAN_POINT ( 'NONE',  ( -16.87036670365548474, 66.01058118070987746, -48.54354736722234520 ) ) ;
#12225 = LINE ( 'NONE', #130860, #239602 ) ;
#12226 = EDGE_LOOP ( 'NONE', ( #62080, #241108, #191770, #165333, #241458, #101221, #189690, #151306, #3079, #147383, #79872 ) ) ;
#12227 = EDGE_CURVE ( 'NONE', #140520, #228310, #64745, .T. ) ;
#12229 = EDGE_LOOP ( 'NONE', ( #768, #80937, #233887, #99345 ) ) ;
#12228 = CYLINDRICAL_SURFACE ( 'NONE', #171827, 0.1000000000000008105 ) ;
#12230 = CARTESIAN_POINT ( 'NONE',  ( -23.15000000000000213, -11.65000000000000036, -30.39999999999999503 ) ) ;
#12231 = FACE_OUTER_BOUND ( 'NONE', #198653, .T. ) ;
#12232 = AXIS2_PLACEMENT_3D ( 'NONE', #47761, #28257, #107752 ) ;
#12233 = AXIS2_PLACEMENT_3D ( 'NONE', #204778, #247772, #27490 ) ;
#12234 = AXIS2_PLACEMENT_3D ( 'NONE', #186632, #63461, #80427 ) ;
#12235 = CIRCLE ( 'NONE', #212128, 12.87499999999999822 ) ;
#12236 = ORIENTED_EDGE ( 'NONE', *, *, #53846, .T. ) ;
#12237 = DIRECTION ( 'NONE',  ( 0.000000000000000000, 6.308085367183347448E-16, 1.000000000000000000 ) ) ;
#12239 = EDGE_CURVE ( 'NONE', #35839, #74847, #89074, .T. ) ;
#12238 = CARTESIAN_POINT ( 'NONE',  ( -18.59999999999999787, 11.65000000001115232, -40.51480577065400013 ) ) ;
#12240 = AXIS2_PLACEMENT_3D ( 'NONE', #105737, #223138, #44522 ) ;
#12241 = CARTESIAN_POINT ( 'NONE',  ( -20.92356734117541706, 18.39335631088232503, -236.9600537807593241 ) ) ;
#12242 = ORIENTED_EDGE ( 'NONE', *, *, #145880, .F. ) ;
#12243 = DIRECTION ( 'NONE',  ( 0.000000000000000000, -0.2617529984165030132, -0.9651348961777157509 ) ) ;
#12244 = DIRECTION ( 'NONE',  ( -2.812466655313719426E-14, -0.1350103645451835865, -0.9908441862701605762 ) ) ;
#12245 = EDGE_CURVE ( 'NONE', #137004, #78394, #30843, .T. ) ;
#12246 = DIRECTION ( 'NONE',  ( 0.000000000000000000, 0.3848449534832868446, 0.9229812358755982160 ) ) ;
#12247 = AXIS2_PLACEMENT_3D ( 'NONE', #206994, #49194, #230404 ) ;
#12248 = AXIS2_PLACEMENT_3D ( 'NONE', #32677, #56010, #213834 ) ;
#12249 = AXIS2_PLACEMENT_3D ( 'NONE', #215857, #39841, #195057 ) ;
#12250 = EDGE_CURVE ( 'NONE', #159544, #162125, #183424, .T. ) ;
#12251 = CIRCLE ( 'NONE', #199699, 0.09999999999999939493 ) ;
#12252 = ORIENTED_EDGE ( 'NONE', *, *, #240226, .F. ) ;
#12253 = DIRECTION ( 'NONE',  ( -0.000000000000000000, -6.982962677686266711E-15, 1.000000000000000000 ) ) ;
#12254 = ORIENTED_EDGE ( 'NONE', *, *, #224934, .F. ) ;
#12255 = CARTESIAN_POINT ( 'NONE',  ( 20.94999999999999574, 87.48912529308769592, -66.62310748452424036 ) ) ;
#12256 = DIRECTION ( 'NONE',  ( 0.000000000000000000, 0.000000000000000000, -1.000000000000000000 ) ) ;
#12259 = EDGE_CURVE ( 'NONE', #244686, #64807, #176583, .T. ) ;
#12258 = ORIENTED_EDGE ( 'NONE', *, *, #204317, .T. ) ;
#12257 = CARTESIAN_POINT ( 'NONE',  ( 12.60053434924910576, 25.37977472455730776, -232.8574044443169271 ) ) ;
#12260 = FACE_OUTER_BOUND ( 'NONE', #157446, .T. ) ;
#12261 = DIRECTION ( 'NONE',  ( -1.000000000000000000, 0.000000000000000000, 0.000000000000000000 ) ) ;
#12262 = DIRECTION ( 'NONE',  ( -1.000000000000000000, -0.000000000000000000, 0.000000000000000000 ) ) ;
#12263 = DIRECTION ( 'NONE',  ( -2.561896900575096011E-15, -0.5907332058517279494, 0.8068669527897025517 ) ) ;
#12264 = DIRECTION ( 'NONE',  ( 0.000000000000000000, 0.000000000000000000, -1.000000000000000000 ) ) ;
#12265 = EDGE_CURVE ( 'NONE', #2981, #155807, #86856, .T. ) ;
#12266 = CARTESIAN_POINT ( 'NONE',  ( -20.94999999999999929, 76.00000000001190870, -103.0231074845243029 ) ) ;
#12267 = EDGE_CURVE ( 'NONE', #148565, #142261, #39231, .T. ) ;
#12268 = LINE ( 'NONE', #70969, #7192 ) ;
#12270 = EDGE_LOOP ( 'NONE', ( #166422, #21867, #81165, #114694 ) ) ;
#12269 = CARTESIAN_POINT ( 'NONE',  ( 20.94999999999999929, 68.97833521811233481, -166.1895420826271277 ) ) ;
#12271 = VECTOR ( 'NONE', #165517, 1000.000000000000000 ) ;
#12273 = EDGE_CURVE ( 'NONE', #168786, #85846, #130776, .T. ) ;
#12272 = DIRECTION ( 'NONE',  ( -0.000000000000000000, 0.2617529984165031243, 0.9651348961777157509 ) ) ;
#12274 = CARTESIAN_POINT ( 'NONE',  ( 21.14999999999999858, 0.09779029131994770863, -127.7421853895238968 ) ) ;
#12275 = CIRCLE ( 'NONE', #249765, 0.4000000000000114575 ) ;
#12277 = EDGE_CURVE ( 'NONE', #17623, #252254, #255631, .T. ) ;
#12276 = DIRECTION ( 'NONE',  ( 0.000000000000000000, 0.000000000000000000, 1.000000000000000000 ) ) ;
#12278 = CARTESIAN_POINT ( 'NONE',  ( 20.94999999999999574, 18.14639373905162145, -237.6648341169113792 ) ) ;
#12279 = EDGE_CURVE ( 'NONE', #235449, #101287, #3274, .T. ) ;
#12280 = ORIENTED_EDGE ( 'NONE', *, *, #103050, .F. ) ;
#12281 = PLANE ( 'NONE',  #68683 ) ;
#12282 = DIRECTION ( 'NONE',  ( 0.000000000000000000, 0.000000000000000000, -1.000000000000000000 ) ) ;
#12283 = VECTOR ( 'NONE', #82632, 1000.000000000000000 ) ;
#12284 = ORIENTED_EDGE ( 'NONE', *, *, #222592, .F. ) ;
#12285 = AXIS2_PLACEMENT_3D ( 'NONE', #17310, #117675, #159387 ) ;
#12286 = DIRECTION ( 'NONE',  ( 1.000000000000000000, 0.000000000000000000, 0.000000000000000000 ) ) ;
#12287 = VECTOR ( 'NONE', #254620, 1000.000000000000000 ) ;
#12288 = CARTESIAN_POINT ( 'NONE',  ( -16.93583594267724024, 10.00862343506335783, -79.55939083932079825 ) ) ;
#12289 = VERTEX_POINT ( 'NONE', #169028 ) ;
#12290 = CARTESIAN_POINT ( 'NONE',  ( -18.40000000000000213, 11.48667500176882861, -124.7500000000000284 ) ) ;
#12291 = ADVANCED_FACE ( 'NONE', ( #171585 ), #143244, .T. ) ;
#12292 = VERTEX_POINT ( 'NONE', #251075 ) ;
#12293 = EDGE_CURVE ( 'NONE', #176232, #95340, #131139, .T. ) ;
#12294 = CARTESIAN_POINT ( 'NONE',  ( 18.39999999999999503, 11.74999999999998224, -12.65000000000000213 ) ) ;
#12296 = ORIENTED_EDGE ( 'NONE', *, *, #238093, .F. ) ;
#12295 = CARTESIAN_POINT ( 'NONE',  ( 21.93340585900768858, 76.00000000001219291, -143.8472545066313728 ) ) ;
#12297 = AXIS2_PLACEMENT_3D ( 'NONE', #212563, #135561, #53476 ) ;
#12298 = CIRCLE ( 'NONE', #120634, 7.900000000000013678 ) ;
#12299 = DIRECTION ( 'NONE',  ( -1.000000000000000000, -0.000000000000000000, -0.000000000000000000 ) ) ;
#12300 = ORIENTED_EDGE ( 'NONE', *, *, #51111, .F. ) ;
#12301 = CARTESIAN_POINT ( 'NONE',  ( -20.94999999999999929, 76.00000000001170974, -69.52310748452431710 ) ) ;
#12302 = EDGE_LOOP ( 'NONE', ( #167125, #159282, #1504, #216157 ) ) ;
#12305 = ADVANCED_FACE ( 'NONE', ( #52877 ), #105805, .T. ) ;
#12304 = ORIENTED_EDGE ( 'NONE', *, *, #217181, .F. ) ;
#12303 = EDGE_LOOP ( 'NONE', ( #174671, #76672, #112137, #113608 ) ) ;
#12306 = CARTESIAN_POINT ( 'NONE',  ( -23.25000000000000000, 2.600000000011156054, -113.7246219227621395 ) ) ;
#12308 = ORIENTED_EDGE ( 'NONE', *, *, #154348, .F. ) ;
#12307 = CARTESIAN_POINT ( 'NONE',  ( 21.07888907270776002, 10.72506921352637654, -146.2211935868332091 ) ) ;
#12309 = DIRECTION ( 'NONE',  ( 0.000000000000000000, -0.2617529984165152257, -0.9651348961777124202 ) ) ;
#12310 = ORIENTED_EDGE ( 'NONE', *, *, #73318, .F. ) ;
#12311 = AXIS2_PLACEMENT_3D ( 'NONE', #200663, #161551, #239794 ) ;
#12312 = AXIS2_PLACEMENT_3D ( 'NONE', #51592, #148155, #49053 ) ;
#12313 = TOROIDAL_SURFACE ( 'NONE', #187094, 0.4000000000000015210, 0.1000000000000000056 ) ;
#12314 = AXIS2_PLACEMENT_3D ( 'NONE', #40301, #136784, #196758 ) ;
#12315 = ORIENTED_EDGE ( 'NONE', *, *, #24174, .T. ) ;
#12317 = AXIS2_PLACEMENT_3D ( 'NONE', #217916, #145768, #186203 ) ;
#12316 = FACE_OUTER_BOUND ( 'NONE', #80816, .T. ) ;
#12318 = CARTESIAN_POINT ( 'NONE',  ( 20.12500000000000355, 10.24195072708267240, -7.860203727086118697 ) ) ;
#12319 = ORIENTED_EDGE ( 'NONE', *, *, #117934, .F. ) ;
#12320 = LINE ( 'NONE', #33187, #37003 ) ;
#12321 = CARTESIAN_POINT ( 'NONE',  ( 21.14999999999999858, 65.28660755661168480, -57.27310748452440237 ) ) ;
#12322 = DIRECTION ( 'NONE',  ( -0.000000000000000000, -1.265107689135680095E-16, 1.000000000000000000 ) ) ;
#12324 = EDGE_LOOP ( 'NONE', ( #69127, #202779, #176505, #35667, #176251 ) ) ;
#12323 = ADVANCED_FACE ( 'NONE', ( #193694 ), #211981, .T. ) ;
#12325 = DIRECTION ( 'NONE',  ( 0.000000000000000000, 0.000000000000000000, -1.000000000000000000 ) ) ;
#12326 = DIRECTION ( 'NONE',  ( 0.000000000000000000, -6.982962677686267499E-15, 1.000000000000000000 ) ) ;
#12327 = FACE_OUTER_BOUND ( 'NONE', #95956, .T. ) ;
#12328 = FACE_OUTER_BOUND ( 'NONE', #114326, .T. ) ;
#12329 = EDGE_CURVE ( 'NONE', #161528, #15766, #155751, .T. ) ;
#12330 = ORIENTED_EDGE ( 'NONE', *, *, #112389, .T. ) ;
#12331 = CARTESIAN_POINT ( 'NONE',  ( -16.87242674293849731, 14.15923359356921729, -219.2561378310278144 ) ) ;
#12332 = EDGE_LOOP ( 'NONE', ( #75777, #98915, #15644, #228792 ) ) ;
#12334 = PRESENTATION_LAYER_ASSIGNMENT (  '', '', ( #178941 ) ) ;
#12333 = CARTESIAN_POINT ( 'NONE',  ( -18.52186455168988388, -7.768930579343111376, -209.8816825891055373 ) ) ;
#12335 = ORIENTED_EDGE ( 'NONE', *, *, #113986, .F. ) ;
#12336 = CARTESIAN_POINT ( 'NONE',  ( -13.54795643572458275, 24.86276468521554506, -232.5111033352153811 ) ) ;
#12337 = DIRECTION ( 'NONE',  ( 0.000000000000000000, 0.000000000000000000, -1.000000000000000000 ) ) ;
#12338 = ORIENTED_EDGE ( 'NONE', *, *, #38942, .F. ) ;
#12339 = VERTEX_POINT ( 'NONE', #155868 ) ;
#12341 = ADVANCED_FACE ( 'NONE', ( #95846 ), #33371, .F. ) ;
#12340 = DIRECTION ( 'NONE',  ( 1.000000000000000000, 0.000000000000000000, 0.000000000000000000 ) ) ;
#12342 = CARTESIAN_POINT ( 'NONE',  ( -21.64999999999999858, 7.250000000011148416, -179.7499999999999716 ) ) ;
#12343 = ORIENTED_EDGE ( 'NONE', *, *, #149750, .F. ) ;
#12344 = CARTESIAN_POINT ( 'NONE',  ( 20.27550659511088682, 9.216043722520002035, -113.1500000000000483 ) ) ;
#12345 = EDGE_CURVE ( 'NONE', #14142, #214434, #90720, .T. ) ;
#12346 = DIRECTION ( 'NONE',  ( 1.000000000000000000, -0.000000000000000000, -0.000000000000000000 ) ) ;
#12347 = AXIS2_PLACEMENT_3D ( 'NONE', #381, #98174, #121650 ) ;
#12348 = ORIENTED_EDGE ( 'NONE', *, *, #46754, .T. ) ;
#12349 = EDGE_CURVE ( 'NONE', #100003, #91601, #121827, .T. ) ;
#12350 = CIRCLE ( 'NONE', #95523, 11.80000000000001670 ) ;
#12351 = ORIENTED_EDGE ( 'NONE', *, *, #13041, .F. ) ;
#12352 = TOROIDAL_SURFACE ( 'NONE', #87148, 12.97499999999999609, 0.1000000000000000056 ) ;
#12353 = EDGE_CURVE ( 'NONE', #105545, #257429, #134963, .T. ) ;
#12356 = ADVANCED_FACE ( 'NONE', ( #210678 ), #12506, .T. ) ;
#12355 = EDGE_CURVE ( 'NONE', #95915, #128122, #60035, .T. ) ;
#12354 = LINE ( 'NONE', #35768, #114238 ) ;
#12357 = DIRECTION ( 'NONE',  ( 0.7071067811865463515, -0.7071067811865487940, 0.000000000000000000 ) ) ;
#12358 = DIRECTION ( 'NONE',  ( -2.978066053179066765E-16, -0.9651348961777157509, 0.2617529984165031243 ) ) ;
#12360 = EDGE_LOOP ( 'NONE', ( #119536, #155518, #179823 ) ) ;
#12359 = CARTESIAN_POINT ( 'NONE',  ( 23.14999999999999503, 69.35000000001180354, -81.77310748452435973 ) ) ;
#12361 = DIRECTION ( 'NONE',  ( 0.000000000000000000, -1.000000000000000000, -0.000000000000000000 ) ) ;
#12362 = AXIS2_PLACEMENT_3D ( 'NONE', #193692, #141404, #180548 ) ;
#12363 = CARTESIAN_POINT ( 'NONE',  ( 23.24999999999999645, 1.115600667400684642E-11, -167.5000000000000284 ) ) ;
#12364 = PLANE ( 'NONE',  #60579 ) ;
#12365 = CIRCLE ( 'NONE', #74911, 0.09999999999999939493 ) ;
#12367 = FACE_OUTER_BOUND ( 'NONE', #52133, .T. ) ;
#12366 = LINE ( 'NONE', #7182, #31856 ) ;
#12368 = CARTESIAN_POINT ( 'NONE',  ( 18.59999999999999076, 69.45000000001222418, -148.8731074845244109 ) ) ;
#12369 = CARTESIAN_POINT ( 'NONE',  ( 18.41356215285961895, -9.499999999988869348, -107.5320693966996544 ) ) ;
#12370 = DIRECTION ( 'NONE',  ( 0.000000000000000000, 0.2128009952263611726, -0.9770955615653312831 ) ) ;
#12371 = CARTESIAN_POINT ( 'NONE',  ( -21.09096482362057046, 75.96055172123814714, -176.3866518499285121 ) ) ;
#12372 = ADVANCED_FACE ( 'NONE', ( #192404 ), #73766, .F. ) ;
#12374 = EDGE_CURVE ( 'NONE', #46505, #67969, #126499, .T. ) ;
#12373 = AXIS2_PLACEMENT_3D ( 'NONE', #26817, #185855, #178517 ) ;
#12375 = VERTEX_POINT ( 'NONE', #75057 ) ;
#12376 = EDGE_CURVE ( 'NONE', #126912, #231604, #141407, .T. ) ;
#12377 = ORIENTED_EDGE ( 'NONE', *, *, #186952, .T. ) ;
#12378 = ADVANCED_FACE ( 'NONE', ( #256155 ), #60577, .T. ) ;
#12379 = CARTESIAN_POINT ( 'NONE',  ( 20.85000000000000142, -0.3238857010591806307, -200.9575895893139545 ) ) ;
#12380 = DIRECTION ( 'NONE',  ( 0.000000000000000000, 0.1298341882519953583, 0.9915357197604862671 ) ) ;
#12381 = EDGE_CURVE ( 'NONE', #178010, #58070, #14092, .T. ) ;
#12382 = ORIENTED_EDGE ( 'NONE', *, *, #241375, .F. ) ;
#12383 = LINE ( 'NONE', #189714, #74011 ) ;
#12385 = CARTESIAN_POINT ( 'NONE',  ( 20.93975676684922504, 10.31104185824063002, -206.5204516983105236 ) ) ;
#12384 = AXIS2_PLACEMENT_3D ( 'NONE', #47793, #84315, #62248 ) ;
#12386 = VERTEX_POINT ( 'NONE', #120589 ) ;
#12387 = ORIENTED_EDGE ( 'NONE', *, *, #216333, .F. ) ;
#12388 = DIRECTION ( 'NONE',  ( -1.000000000000000000, 0.000000000000000000, 0.000000000000000000 ) ) ;
#12389 = DIRECTION ( 'NONE',  ( 0.000000000000000000, 0.000000000000000000, -1.000000000000000000 ) ) ;
#12390 = ORIENTED_EDGE ( 'NONE', *, *, #209788, .T. ) ;
#12391 = ADVANCED_FACE ( 'NONE', ( #181827 ), #240516, .T. ) ;
#12392 = CARTESIAN_POINT ( 'NONE',  ( 18.49999999999998934, 45.21086124044690280, -238.4331873168094091 ) ) ;
#12394 = VERTEX_POINT ( 'NONE', #22777 ) ;
#12393 = DIRECTION ( 'NONE',  ( -1.652117596168391700E-15, 1.000000000000000000, 6.982962677686266711E-15 ) ) ;
#12395 = DIRECTION ( 'NONE',  ( 0.000000000000000000, 1.000000000000000000, 0.000000000000000000 ) ) ;
#12397 = ORIENTED_EDGE ( 'NONE', *, *, #45122, .T. ) ;
#12396 = DIRECTION ( 'NONE',  ( 0.000000000000000000, -0.4721928772777346239, -0.8814952561688430555 ) ) ;
#12398 = CARTESIAN_POINT ( 'NONE',  ( -22.39999999999999858, 33.47376623175146904, -242.4412390690852703 ) ) ;
#12399 = CARTESIAN_POINT ( 'NONE',  ( -16.87331047859651179, 9.950000000011142376, -46.15000000000000568 ) ) ;
#12400 = CARTESIAN_POINT ( 'NONE',  ( 23.15000000000000213, -11.74999999998883737, -88.35000000000003695 ) ) ;
#12401 = CARTESIAN_POINT ( 'NONE',  ( 20.12500000000000000, 9.750000000011153745, -175.6117712821142618 ) ) ;
#12402 = B_SPLINE_CURVE_WITH_KNOTS ( 'NONE', 3,
 ( #129198, #148767, #104460, #164473, #49648, #105740, #206160, #208744 ),
 .UNSPECIFIED., .F., .F.,
 ( 4, 2, 2, 4 ),
 ( 0.000000000000000000, 0.0001306511400391696253, 0.0001959767100587203668, 0.0002613022800782711084 ),
 .UNSPECIFIED. ) ;
#12403 = EDGE_CURVE ( 'NONE', #77802, #223637, #80691, .T. ) ;
#12406 = CARTESIAN_POINT ( 'NONE',  ( 20.84451136049448294, 10.62014191482269965, -107.9939245595242170 ) ) ;
#12405 = AXIS2_PLACEMENT_3D ( 'NONE', #44782, #184281, #5620 ) ;
#12404 = CARTESIAN_POINT ( 'NONE',  ( 23.25000000000000000, 84.59626168225486254, -93.57297996737396772 ) ) ;
#12407 = CARTESIAN_POINT ( 'NONE',  ( 21.05000000000000071, 10.47809638650343622, -198.7179823275938020 ) ) ;
#12408 = AXIS2_PLACEMENT_3D ( 'NONE', #83961, #243080, #25350 ) ;
#12409 = AXIS2_PLACEMENT_3D ( 'NONE', #129138, #208692, #32644 ) ;
#12410 = CARTESIAN_POINT ( 'NONE',  ( -18.54260524012575928, 85.62421939008640948, -163.2823344387538498 ) ) ;
#12411 = CARTESIAN_POINT ( 'NONE',  ( 21.05000000000000071, 1.626809808086280951, -230.7491004397056145 ) ) ;
#12412 = DIRECTION ( 'NONE',  ( 0.000000000000000000, 2.891205793294679805E-16, -1.000000000000000000 ) ) ;
#12413 = VERTEX_POINT ( 'NONE', #42317 ) ;
#12414 = CARTESIAN_POINT ( 'NONE',  ( 18.59999999999997655, 76.00000000001244871, -170.0231074845243597 ) ) ;
#12415 = VECTOR ( 'NONE', #125040, 1000.000000000000000 ) ;
#12416 = EDGE_LOOP ( 'NONE', ( #157603, #56927, #56875, #117432 ) ) ;
#12417 = CARTESIAN_POINT ( 'NONE',  ( 18.59999999999999076, 19.00443933019177223, -232.7770257915295531 ) ) ;
#12418 = ORIENTED_EDGE ( 'NONE', *, *, #2486, .F. ) ;
#12419 = EDGE_CURVE ( 'NONE', #131400, #75618, #68243, .T. ) ;
#12420 = CARTESIAN_POINT ( 'NONE',  ( 21.05000000000000071, 76.00000000001126921, -203.5231074845248997 ) ) ;
#12421 = CARTESIAN_POINT ( 'NONE',  ( -23.15000000000000213, 76.00000000001126921, -203.5231074845248997 ) ) ;
#12422 = APPLICATION_CONTEXT ( 'automotive_design' ) ;
#12423 = CIRCLE ( 'NONE', #158200, 0.1000000000000008937 ) ;
#12424 = ORIENTED_EDGE ( 'NONE', *, *, #13202, .F. ) ;
#12425 = VECTOR ( 'NONE', #2614, 1000.000000000000000 ) ;
#12426 = DIRECTION ( 'NONE',  ( 0.000000000000000000, 0.9915357197604862671, -0.1298341882519953583 ) ) ;
#12427 =( NAMED_UNIT ( * ) PLANE_ANGLE_UNIT ( ) SI_UNIT ( $, .RADIAN. ) );
#12428 = EDGE_CURVE ( 'NONE', #222155, #196636, #22473, .T. ) ;
#12429 = ORIENTED_EDGE ( 'NONE', *, *, #105891, .T. ) ;
#12430 = AXIS2_PLACEMENT_3D ( 'NONE', #60820, #199067, #99933 ) ;
#12431 = VERTEX_POINT ( 'NONE', #159704 ) ;
#12432 = CARTESIAN_POINT ( 'NONE',  ( -23.15000000000000213, 64.35000000001146248, -43.03791325517834565 ) ) ;
#12433 = DIRECTION ( 'NONE',  ( 0.000000000000000000, 0.000000000000000000, -1.000000000000000000 ) ) ;
#12434 = FACE_OUTER_BOUND ( 'NONE', #157664, .T. ) ;
#12435 = CARTESIAN_POINT ( 'NONE',  ( 13.77030915526558452, 27.89153536508384335, -234.1274767587460133 ) ) ;
#12436 = DIRECTION ( 'NONE',  ( -1.000000000000000000, -0.000000000000000000, -0.000000000000000000 ) ) ;
#12438 = DIRECTION ( 'NONE',  ( -1.000000000000000000, 2.670994536826046953E-16, 9.848483305199541222E-16 ) ) ;
#12437 = CARTESIAN_POINT ( 'NONE',  ( 18.59999999999999787, -11.65000000000000036, 6.100000000000001421 ) ) ;
#12439 = CARTESIAN_POINT ( 'NONE',  ( -14.11697426661281440, 9.457410944778569473, -82.00008397379009750 ) ) ;
#12441 = ORIENTED_EDGE ( 'NONE', *, *, #127715, .F. ) ;
#12440 = CARTESIAN_POINT ( 'NONE',  ( -23.15000000000000213, 70.73902226565648732, -215.2805781460175467 ) ) ;
#12443 = DIRECTION ( 'NONE',  ( 0.000000000000000000, -6.982962677686266711E-15, 1.000000000000000000 ) ) ;
#12442 = CARTESIAN_POINT ( 'NONE',  ( 20.59588692710267921, 10.36872342117990975, -74.63908109451070061 ) ) ;
#12444 = DIRECTION ( 'NONE',  ( 0.000000000000000000, 0.9770955615653559301, 0.2128009952262481796 ) ) ;
#12445 = VERTEX_POINT ( 'NONE', #17596 ) ;
#12446 = CARTESIAN_POINT ( 'NONE',  ( -18.50000000000001066, -9.421308209727696337, -174.7423632140504708 ) ) ;
#12447 = DIRECTION ( 'NONE',  ( 0.000000000000000000, 1.000000000000000000, 6.982962677686266711E-15 ) ) ;
#12448 = VERTEX_POINT ( 'NONE', #179286 ) ;
#12449 = CARTESIAN_POINT ( 'NONE',  ( 21.05000000000000071, -11.29603075032412640, -63.95210084033612929 ) ) ;
#12450 = CIRCLE ( 'NONE', #212365, 3.899999999999987033 ) ;
#12451 = DIRECTION ( 'NONE',  ( 1.000000000000000000, -7.304098846218134667E-16, -0.000000000000000000 ) ) ;
#12452 = CARTESIAN_POINT ( 'NONE',  ( -23.24999999999999645, -9.600000000000003197, -40.20018939122204671 ) ) ;
#12453 = ORIENTED_EDGE ( 'NONE', *, *, #169798, .T. ) ;
#12454 = ORIENTED_EDGE ( 'NONE', *, *, #11315, .F. ) ;
#12455 = CARTESIAN_POINT ( 'NONE',  ( 22.49999999999999289, 64.13768741198656187, -247.0874927502468381 ) ) ;
#12456 = CIRCLE ( 'NONE', #208265, 0.1999999999999884925 ) ;
#12457 = FACE_OUTER_BOUND ( 'NONE', #63915, .T. ) ;
#12458 = CARTESIAN_POINT ( 'NONE',  ( -22.39999999999999858, 64.25313205997782973, -247.2214437328673853 ) ) ;
#12459 = ORIENTED_EDGE ( 'NONE', *, *, #62305, .F. ) ;
#12460 = VECTOR ( 'NONE', #238326, 1000.000000000000000 ) ;
#12461 = CARTESIAN_POINT ( 'NONE',  ( 23.15000000000000213, 62.12148660976905745, -247.5636999539406133 ) ) ;
#12463 = EDGE_CURVE ( 'NONE', #166675, #233701, #35145, .T. ) ;
#12462 = DIRECTION ( 'NONE',  ( 0.000000000000000000, -1.000000000000000000, 0.000000000000000000 ) ) ;
#12464 = CARTESIAN_POINT ( 'NONE',  ( 21.07928932188134397, 0.09889514566555242248, -127.6714833436067238 ) ) ;
#12465 = DIRECTION ( 'NONE',  ( 0.000000000000000000, 0.4088369013363280513, -0.9126074666063769270 ) ) ;
#12466 = CIRCLE ( 'NONE', #145527, 0.9000000000000014655 ) ;
#12467 = ORIENTED_EDGE ( 'NONE', *, *, #4048, .F. ) ;
#12469 = CARTESIAN_POINT ( 'NONE',  ( -21.05000000000000071, 44.05869416168422958, -258.6139110589941197 ) ) ;
#12468 = VECTOR ( 'NONE', #218728, 1000.000000000000000 ) ;
#12471 = EDGE_LOOP ( 'NONE', ( #105180, #117829, #50180 ) ) ;
#12470 = CARTESIAN_POINT ( 'NONE',  ( -16.94132844910801339, 66.00756324483145931, -82.12690572854207005 ) ) ;
#12472 = LINE ( 'NONE', #105419, #109938 ) ;
#12473 = CARTESIAN_POINT ( 'NONE',  ( 20.94999999999999929, 76.00000000001170974, -69.52310748452431710 ) ) ;
#12474 = DIRECTION ( 'NONE',  ( -1.000000000000000000, 0.000000000000000000, -0.000000000000000000 ) ) ;
#12475 = CIRCLE ( 'NONE', #199912, 0.09999999999999939493 ) ;
#12476 = DIRECTION ( 'NONE',  ( -1.000000000000000000, 9.012599976028471648E-15, 6.882867235861662930E-14 ) ) ;
#12477 = EDGE_CURVE ( 'NONE', #204085, #74763, #97610, .T. ) ;
#12478 = DIRECTION ( 'NONE',  ( 1.000000000000000000, 1.794895427898102820E-16, 3.909090864890033875E-17 ) ) ;
#12479 = ORIENTED_EDGE ( 'NONE', *, *, #179070, .F. ) ;
#12480 = DIRECTION ( 'NONE',  ( 0.000000000000000000, 1.000000000000000000, -1.224646799147353207E-16 ) ) ;
#12481 = AXIS2_PLACEMENT_3D ( 'NONE', #37147, #137486, #191427 ) ;
#12482 = CARTESIAN_POINT ( 'NONE',  ( -21.05000000000000071, 70.15000000001192859, -92.89061026024637613 ) ) ;
#12483 = FACE_OUTER_BOUND ( 'NONE', #67885, .T. ) ;
#12484 = VECTOR ( 'NONE', #250475, 1000.000000000000000 ) ;
#12485 = EDGE_CURVE ( 'NONE', #230941, #203487, #180551, .T. ) ;
#12486 = EDGE_LOOP ( 'NONE', ( #61567, #186808, #7031, #168361 ) ) ;
#12487 = DIRECTION ( 'NONE',  ( 0.000000000000000000, -0.9908441862701596881, -0.1350103645451904977 ) ) ;
#12488 = CYLINDRICAL_SURFACE ( 'NONE', #102521, 0.09999999999999939493 ) ;
#12489 =( NAMED_UNIT ( * ) PLANE_ANGLE_UNIT ( ) SI_UNIT ( $, .RADIAN. ) );
#12490 = CARTESIAN_POINT ( 'NONE',  ( -16.94445028196808778, 9.992063609708889516, -46.10733017841845793 ) ) ;
#12491 = EDGE_CURVE ( 'NONE', #171236, #117217, #136246, .T. ) ;
#12493 = CARTESIAN_POINT ( 'NONE',  ( 12.26145404764308822, 9.351413679112544841, -184.4803435675489993 ) ) ;
#12492 = TOROIDAL_SURFACE ( 'NONE', #257929, 0.2000000000000000111, 0.1000000000000000056 ) ;
#12494 = AXIS2_PLACEMENT_3D ( 'NONE', #177402, #256848, #18294 ) ;
#12496 = ORIENTED_EDGE ( 'NONE', *, *, #212160, .T. ) ;
#12495 = VECTOR ( 'NONE', #154214, 1000.000000000000000 ) ;
#12497 = EDGE_LOOP ( 'NONE', ( #173993, #29341, #244810, #162677 ) ) ;
#12498 = PRESENTATION_LAYER_ASSIGNMENT (  '', '', ( #220586 ) ) ;
#12499 = VECTOR ( 'NONE', #183493, 1000.000000000000000 ) ;
#12500 = EDGE_CURVE ( 'NONE', #61933, #187354, #147531, .T. ) ;
#12501 = DIRECTION ( 'NONE',  ( 1.000000000000000000, 0.000000000000000000, -0.000000000000000000 ) ) ;
#12502 = DIRECTION ( 'NONE',  ( 1.000000000000000000, 0.000000000000000000, 0.000000000000000000 ) ) ;
#12503 = EDGE_CURVE ( 'NONE', #92492, #256102, #241795, .T. ) ;
#12504 = AXIS2_PLACEMENT_3D ( 'NONE', #88035, #149351, #30691 ) ;
#12505 = CARTESIAN_POINT ( 'NONE',  ( -21.64999999999999858, 65.95000000001201101, -115.7731074845243597 ) ) ;
#12506 = PLANE ( 'NONE',  #1586 ) ;
#12507 = EDGE_CURVE ( 'NONE', #247920, #94393, #22651, .T. ) ;
#12508 = CARTESIAN_POINT ( 'NONE',  ( 18.49999999999999645, 14.81796439977981272, -236.5325475414793743 ) ) ;
#12509 = CARTESIAN_POINT ( 'NONE',  ( -20.85000000000000142, -1.851617760457748618, -112.1031897196037050 ) ) ;
#12510 = EDGE_CURVE ( 'NONE', #365, #19404, #164299, .T. ) ;
#12511 = CARTESIAN_POINT ( 'NONE',  ( -18.39999999999999858, 11.47867410001043886, -109.7746932163407081 ) ) ;
#12512 = LINE ( 'NONE', #215800, #102707 ) ;
#12513 = EDGE_LOOP ( 'NONE', ( #154372, #131344, #178907 ) ) ;
#12514 = DIRECTION ( 'NONE',  ( 0.000000000000000000, 0.000000000000000000, -1.000000000000000000 ) ) ;
#12515 = EDGE_LOOP ( 'NONE', ( #15578, #22661, #237739, #126733 ) ) ;
#12516 = DIRECTION ( 'NONE',  ( 1.000000000000000000, 0.000000000000000000, 0.000000000000000000 ) ) ;
#12518 = ADVANCED_FACE ( 'NONE', ( #257446 ), #68419, .T. ) ;
#12517 = CARTESIAN_POINT ( 'NONE',  ( 23.14999999999999858, 76.00000000001195133, -103.0231074845243171 ) ) ;
#12519 = FACE_OUTER_BOUND ( 'NONE', #1501, .T. ) ;
#12520 = LINE ( 'NONE', #192424, #248789 ) ;
#12521 = DIRECTION ( 'NONE',  ( 1.000000000000000000, 0.000000000000000000, 0.000000000000000000 ) ) ;
#12522 = CARTESIAN_POINT ( 'NONE',  ( 18.59999999999999076, 79.15532900748003442, -196.2806010913881778 ) ) ;
#12523 = DIRECTION ( 'NONE',  ( 0.000000000000000000, 1.000000000000000000, 6.853228547068871147E-15 ) ) ;
#12525 = ORIENTED_EDGE ( 'NONE', *, *, #212637, .T. ) ;
#12524 = CIRCLE ( 'NONE', #245736, 0.09999999999999939493 ) ;
#12526 = ADVANCED_FACE ( 'NONE', ( #138801 ), #214172, .T. ) ;
#12527 = CARTESIAN_POINT ( 'NONE',  ( -16.94107738177415712, 22.92025126680846725, -230.8312174982872591 ) ) ;
#12528 = DIRECTION ( 'NONE',  ( 0.000000000000000000, 1.000000000000000000, 0.000000000000000000 ) ) ;
#12529 = AXIS2_PLACEMENT_3D ( 'NONE', #92469, #74238, #250270 ) ;
#12530 = CARTESIAN_POINT ( 'NONE',  ( 22.39999999999999503, 11.65000000001116298, -100.5000000000000284 ) ) ;
#12531 = DIRECTION ( 'NONE',  ( 0.000000000000000000, 0.9915357197604794948, -0.1298341882520470392 ) ) ;
#12532 = CARTESIAN_POINT ( 'NONE',  ( 18.39999999999999858, 85.68240343348826116, -96.36626410711143365 ) ) ;
#12533 = VECTOR ( 'NONE', #190441, 1000.000000000000000 ) ;
#12534 = ORIENTED_EDGE ( 'NONE', *, *, #126671, .T. ) ;
#12535 = DIRECTION ( 'NONE',  ( 0.000000000000000000, 0.000000000000000000, -1.000000000000000000 ) ) ;
#12537 = EDGE_CURVE ( 'NONE', #239010, #59872, #20195, .T. ) ;
#12536 = DIRECTION ( 'NONE',  ( 0.000000000000000000, 0.2617529984165031243, 0.9651348961777157509 ) ) ;
#12538 = ORIENTED_EDGE ( 'NONE', *, *, #111371, .T. ) ;
#12539 = VERTEX_POINT ( 'NONE', #87836 ) ;
#12540 = CARTESIAN_POINT ( 'NONE',  ( 22.59999985501178799, 55.87389454177473169, -232.8428744225223284 ) ) ;
#12541 = DIRECTION ( 'NONE',  ( 0.000000000000000000, -0.2128009952263485993, 0.9770955615653341697 ) ) ;
#12542 = TOROIDAL_SURFACE ( 'NONE', #116574, 0.2000000000000000111, 0.1000000000000000056 ) ;
#12543 = AXIS2_PLACEMENT_3D ( 'NONE', #171762, #249987, #174348 ) ;
#12544 = ORIENTED_EDGE ( 'NONE', *, *, #89907, .T. ) ;
#12545 = CARTESIAN_POINT ( 'NONE',  ( 18.59999996954842771, -9.523204137847015360, -174.3830417119173433 ) ) ;
#12546 = CARTESIAN_POINT ( 'NONE',  ( 21.04999999999999716, 8.894723818389001835, -41.98708432314988670 ) ) ;
#12547 = EDGE_LOOP ( 'NONE', ( #31027, #167974, #31048, #2302 ) ) ;
#12548 = VECTOR ( 'NONE', #184267, 999.9999999999998863 ) ;
#12549 = ADVANCED_FACE ( 'NONE', ( #9597 ), #247487, .T. ) ;
#12550 = AXIS2_PLACEMENT_3D ( 'NONE', #252289, #21112, #73701 ) ;
#12551 = DIRECTION ( 'NONE',  ( 0.000000000000000000, 0.000000000000000000, 1.000000000000000000 ) ) ;
#12552 = VERTEX_POINT ( 'NONE', #167425 ) ;
#12553 = FACE_OUTER_BOUND ( 'NONE', #114936, .T. ) ;
#12554 = CARTESIAN_POINT ( 'NONE',  ( 20.94999999999999574, 63.67931791018308019, -224.6923787560153301 ) ) ;
#12557 = EDGE_CURVE ( 'NONE', #61933, #45948, #55920, .T. ) ;
#12556 = ORIENTED_EDGE ( 'NONE', *, *, #172456, .F. ) ;
#12555 = CARTESIAN_POINT ( 'NONE',  ( 18.54999999999999716, 8.750000000011182166, -109.7500000000000426 ) ) ;
#12558 = CARTESIAN_POINT ( 'NONE',  ( -16.87331047859649757, 51.61886293219124155, -231.9464690156495692 ) ) ;
#12559 = SPHERICAL_SURFACE ( 'NONE', #245241, 0.1000000000000000056 ) ;
#12560 = DIRECTION ( 'NONE',  ( 1.000000000000000000, 3.265361837132813093E-16, -0.000000000000000000 ) ) ;
#12561 = DIRECTION ( 'NONE',  ( -1.000000000000000000, 0.000000000000000000, 0.000000000000000000 ) ) ;
#12562 = CARTESIAN_POINT ( 'NONE',  ( -16.77732147278574715, 66.05403306743916403, -190.8595987276486312 ) ) ;
#12563 = EDGE_CURVE ( 'NONE', #131456, #168999, #134270, .T. ) ;
#12564 = DIRECTION ( 'NONE',  ( 1.000000000000000000, 3.469446951953704435E-14, -2.003086131649669752E-14 ) ) ;
#12565 = DIRECTION ( 'NONE',  ( 1.000000000000000000, 0.000000000000000000, 0.000000000000000000 ) ) ;
#12566 = EDGE_CURVE ( 'NONE', #26218, #137088, #201691, .T. ) ;
#12568 = VERTEX_POINT ( 'NONE', #106113 ) ;
#12567 = CARTESIAN_POINT ( 'NONE',  ( 20.04142135623730070, 15.90518444080776383, -219.2841490888777116 ) ) ;
#12569 = VERTEX_POINT ( 'NONE', #163547 ) ;
#12572 = CARTESIAN_POINT ( 'NONE',  ( -18.39999999999999858, 58.59238382117401756, -223.8764022407665379 ) ) ;
#12571 = CARTESIAN_POINT ( 'NONE',  ( 23.14999999999999858, 1.115600667400684642E-11, -100.5000000000000426 ) ) ;
#12570 = AXIS2_PLACEMENT_3D ( 'NONE', #152218, #231737, #153523 ) ;
#12573 = AXIS2_PLACEMENT_3D ( 'NONE', #225812, #43362, #126739 ) ;
#12575 = ORIENTED_EDGE ( 'NONE', *, *, #208067, .F. ) ;
#12574 = CARTESIAN_POINT ( 'NONE',  ( -20.94999999999999929, 74.25000000001229239, -158.3535959266227451 ) ) ;
#12576 = ORIENTED_EDGE ( 'NONE', *, *, #210341, .F. ) ;
#12577 = CARTESIAN_POINT ( 'NONE',  ( -20.64999999999999858, 9.690755012883057518, -211.4266134137857023 ) ) ;
#12578 = EDGE_CURVE ( 'NONE', #19158, #134779, #89248, .T. ) ;
#12579 = LINE ( 'NONE', #28303, #213719 ) ;
#12581 = EDGE_CURVE ( 'NONE', #78560, #242161, #118511, .T. ) ;
#12580 = DIRECTION ( 'NONE',  ( 1.000000000000000000, 0.000000000000000000, 0.000000000000000000 ) ) ;
#12582 = DIRECTION ( 'NONE',  ( -1.000000000000000000, 0.000000000000000000, 0.000000000000000000 ) ) ;
#12583 = CARTESIAN_POINT ( 'NONE',  ( -21.44999999999999929, 11.68239342655420110, -220.1014838121945161 ) ) ;
#12584 = DIRECTION ( 'NONE',  ( -0.5932847527679298016, 0.8049926720990051576, 0.000000000000000000 ) ) ;
#12585 = CARTESIAN_POINT ( 'NONE',  ( -18.39999999999999858, 78.24072131640578220, -231.5548844243369047 ) ) ;
#12586 = AXIS2_PLACEMENT_3D ( 'NONE', #21218, #218079, #100684 ) ;
#12587 = EDGE_LOOP ( 'NONE', ( #206396, #79602, #111325, #34296 ) ) ;
#12588 = VERTEX_POINT ( 'NONE', #47432 ) ;
#12589 = AXIS2_PLACEMENT_3D ( 'NONE', #94165, #18502, #231148 ) ;
#12590 = DIRECTION ( 'NONE',  ( 0.000000000000000000, 1.000000000000000000, 6.352154140967427193E-15 ) ) ;
#12591 = TOROIDAL_SURFACE ( 'NONE', #166735, 0.4000000000000012990, 0.1000000000000000056 ) ;
#12592 = VECTOR ( 'NONE', #15316, 1000.000000000000000 ) ;
#12593 = ORIENTED_EDGE ( 'NONE', *, *, #119754, .F. ) ;
#12594 = CARTESIAN_POINT ( 'NONE',  ( -16.87683809663752399, 9.850000000011144508, -113.9023640181963373 ) ) ;
#12595 = ORIENTED_EDGE ( 'NONE', *, *, #23555, .F. ) ;
#12596 = DIRECTION ( 'NONE',  ( 0.000000000000000000, 0.9908441862701782288, 0.1350103645450542456 ) ) ;
#12597 = EDGE_CURVE ( 'NONE', #100605, #205408, #207843, .T. ) ;
#12598 = CIRCLE ( 'NONE', #249902, 0.09999999999998898659 ) ;
#12599 = DIRECTION ( 'NONE',  ( 0.000000000000000000, -0.3848449534832868446, -0.9229812358755983270 ) ) ;
#12600 = CARTESIAN_POINT ( 'NONE',  ( 18.50000000000000000, 65.50857864377418593, -44.77310748452439526 ) ) ;
#12601 = ADVANCED_FACE ( 'NONE', ( #143969 ), #108713, .F. ) ;
#12602 = ORIENTED_EDGE ( 'NONE', *, *, #159796, .F. ) ;
#12603 = EDGE_CURVE ( 'NONE', #161501, #108803, #176206, .T. ) ;
#12604 = DIRECTION ( 'NONE',  ( 0.000000000000000000, -1.000000000000000000, 0.000000000000000000 ) ) ;
#12605 = ORIENTED_EDGE ( 'NONE', *, *, #69057, .T. ) ;
#12606 = TOROIDAL_SURFACE ( 'NONE', #145849, 12.77500000000000036, 0.1000000000000000056 ) ;
#12607 = CARTESIAN_POINT ( 'NONE',  ( 20.94999999999999929, 1.115625160336667635E-11, -98.50000000000004263 ) ) ;
#12609 = CONICAL_SURFACE ( 'NONE', #195779, 4.299999999999953637, 0.7853981633974466137 ) ;
#12608 = CARTESIAN_POINT ( 'NONE',  ( -18.50000000000000000, 11.75000000001115197, -100.6000000000000369 ) ) ;
#12610 = ORIENTED_EDGE ( 'NONE', *, *, #209729, .F. ) ;
#12611 = DIRECTION ( 'NONE',  ( 0.000000000000000000, -2.775557561562888827E-14, 1.000000000000000000 ) ) ;
#12612 = VERTEX_POINT ( 'NONE', #83956 ) ;
#12615 = VERTEX_POINT ( 'NONE', #245655 ) ;
#12614 = DIRECTION ( 'NONE',  ( -0.000000000000000000, 0.08413937888703756918, -0.9964539953858901900 ) ) ;
#12613 = CARTESIAN_POINT ( 'NONE',  ( -16.27683809663750480, 9.350000000011133849, -54.44999999999999574 ) ) ;
#12616 = CARTESIAN_POINT ( 'NONE',  ( -21.05000000000000071, 0.03363273534480175353, -27.24118280531852321 ) ) ;
#12617 = ORIENTED_EDGE ( 'NONE', *, *, #125244, .T. ) ;
#12618 = EDGE_LOOP ( 'NONE', ( #229654, #45752, #54759, #204208 ) ) ;
#12619 = DIRECTION ( 'NONE',  ( 0.000000000000000000, 6.982962677686266711E-15, -1.000000000000000000 ) ) ;
#12620 = ORIENTED_EDGE ( 'NONE', *, *, #232181, .T. ) ;
#12621 = FACE_OUTER_BOUND ( 'NONE', #172055, .T. ) ;
#12622 = DIRECTION ( 'NONE',  ( 0.000000000000000000, -6.982962677686267499E-15, 1.000000000000000000 ) ) ;
#12623 = CARTESIAN_POINT ( 'NONE',  ( -22.50000000000000000, 64.35042919246758686, -170.1231074845244393 ) ) ;
#12624 = DIRECTION ( 'NONE',  ( 0.000000000000000000, 0.000000000000000000, 1.000000000000000000 ) ) ;
#12625 = DIRECTION ( 'NONE',  ( -1.836970198721029934E-16, 1.000000000000000000, 0.000000000000000000 ) ) ;
#12626 = EDGE_CURVE ( 'NONE', #153145, #206536, #243381, .T. ) ;
#12627 = ORIENTED_EDGE ( 'NONE', *, *, #175654, .F. ) ;
#12628 = CARTESIAN_POINT ( 'NONE',  ( -16.93440969289731157, 44.06337821721247394, -235.2817209114844275 ) ) ;
#12629 = CARTESIAN_POINT ( 'NONE',  ( 23.15000000000000213, 11.36448785225375424, -246.7787679937655980 ) ) ;
#12630 = CARTESIAN_POINT ( 'NONE',  ( 20.94999999999999929, 11.43341603104965110, -245.8667934851861787 ) ) ;
#12631 = CIRCLE ( 'NONE', #62689, 0.1000000000000013933 ) ;
#12632 = ORIENTED_EDGE ( 'NONE', *, *, #130354, .F. ) ;
#12633 = LINE ( 'NONE', #229096, #201087 ) ;
#12634 = ORIENTED_EDGE ( 'NONE', *, *, #33176, .T. ) ;
#12635 = DIRECTION ( 'NONE',  ( 1.000000000000000000, 0.000000000000000000, 0.000000000000000000 ) ) ;
#12636 = ORIENTED_EDGE ( 'NONE', *, *, #146302, .T. ) ;
#12637 = CARTESIAN_POINT ( 'NONE',  ( 18.49999999999999645, 74.16465844978787914, -158.4679561919613775 ) ) ;
#12638 = CARTESIAN_POINT ( 'NONE',  ( 18.49999999999999289, 8.433899723187009201, -209.4150263691077782 ) ) ;
#12639 = VECTOR ( 'NONE', #183048, 1000.000000000000114 ) ;
#12641 = ORIENTED_EDGE ( 'NONE', *, *, #60307, .T. ) ;
#12640 = DIRECTION ( 'NONE',  ( 0.000000000000000000, -0.8660254037844411501, -0.4999999999999956146 ) ) ;
#12642 = LINE ( 'NONE', #13911, #95851 ) ;
#12643 = EDGE_LOOP ( 'NONE', ( #151097, #52115, #105909, #239456 ) ) ;
#12644 = DIRECTION ( 'NONE',  ( 0.000000000000000000, 0.000000000000000000, -1.000000000000000000 ) ) ;
#12645 = ADVANCED_FACE ( 'NONE', ( #226052 ), #130958, .T. ) ;
#12646 = CARTESIAN_POINT ( 'NONE',  ( -20.94999999999999929, 80.78317333349157536, -192.9003134612048882 ) ) ;
#12647 = EDGE_LOOP ( 'NONE', ( #76373, #126403, #48830, #42174 ) ) ;
#12648 = DIRECTION ( 'NONE',  ( 1.000000000000000000, 0.000000000000000000, 0.000000000000000000 ) ) ;
#12650 = EDGE_CURVE ( 'NONE', #160579, #234175, #63143, .T. ) ;
#12649 = CARTESIAN_POINT ( 'NONE',  ( 18.39999999999999858, 85.51932773110476660, -163.0501311079649440 ) ) ;
#12651 = ORIENTED_EDGE ( 'NONE', *, *, #122018, .T. ) ;
#12652 = CARTESIAN_POINT ( 'NONE',  ( 21.05000000000000071, 1.560925708358002373, -230.7692066839898359 ) ) ;
#12653 = AXIS2_PLACEMENT_3D ( 'NONE', #251437, #187632, #231896 ) ;
#12654 = AXIS2_PLACEMENT_3D ( 'NONE', #167792, #132488, #247283 ) ;
#12655 = VERTEX_POINT ( 'NONE', #125699 ) ;
#12656 = EDGE_CURVE ( 'NONE', #8831, #199802, #14281, .T. ) ;
#12657 = CARTESIAN_POINT ( 'NONE',  ( -23.25000000000000000, 2.600000000011156054, -147.2246219227621111 ) ) ;
#12659 = EDGE_CURVE ( 'NONE', #17064, #88829, #105988, .T. ) ;
#12658 = CARTESIAN_POINT ( 'NONE',  ( -18.44448725179913851, -9.490081715472173940, -73.62896029406249454 ) ) ;
#12660 = CIRCLE ( 'NONE', #20864, 0.1000000000000008799 ) ;
#12661 = AXIS2_PLACEMENT_3D ( 'NONE', #24985, #121521, #43244 ) ;
#12662 = AXIS2_PLACEMENT_3D ( 'NONE', #27321, #67685, #168122 ) ;
#12665 = ORIENTED_EDGE ( 'NONE', *, *, #236566, .F. ) ;
#12664 = ORIENTED_EDGE ( 'NONE', *, *, #6604, .T. ) ;
#12663 = CARTESIAN_POINT ( 'NONE',  ( 22.50000000000000000, 75.90000000001172964, -81.27310748452431710 ) ) ;
#12666 = CARTESIAN_POINT ( 'NONE',  ( -20.94999999999999929, -11.64999999998884483, -67.00000000000000000 ) ) ;
#12667 = DIRECTION ( 'NONE',  ( -1.000000000000000000, 0.000000000000000000, 0.000000000000000000 ) ) ;
#12668 = DIRECTION ( 'NONE',  ( -0.7071067811865487940, 0.7071067811865463515, -7.215498431451184074E-16 ) ) ;
#12670 = FACE_OUTER_BOUND ( 'NONE', #169729, .T. ) ;
#12669 = CARTESIAN_POINT ( 'NONE',  ( 23.14999999999999858, 76.00000000001193712, -107.0231074845243029 ) ) ;
#12671 = CARTESIAN_POINT ( 'NONE',  ( -18.59999999999999787, 52.22920805963557456, -232.3304987350788906 ) ) ;
#12672 = CARTESIAN_POINT ( 'NONE',  ( 23.25000000000000000, -11.64999999998884483, -100.5000000000000284 ) ) ;
#12673 = CARTESIAN_POINT ( 'NONE',  ( 18.39999999999999858, 8.794517532467700960, -245.5155488533044945 ) ) ;
#12674 = AXIS2_PLACEMENT_3D ( 'NONE', #121801, #22713, #102181 ) ;
#12675 = DIRECTION ( 'NONE',  ( -0.000000000000000000, -6.982962677686266711E-15, 1.000000000000000000 ) ) ;
#12676 = ADVANCED_FACE ( 'NONE', ( #214237 ), #85129, .T. ) ;
#12677 = ADVANCED_FACE ( 'NONE', ( #134666 ), #222518, .T. ) ;
#12678 = CIRCLE ( 'NONE', #37623, 0.1000000000000028644 ) ;
#12679 = ORIENTED_EDGE ( 'NONE', *, *, #224280, .T. ) ;
#12680 = AXIS2_PLACEMENT_3D ( 'NONE', #47321, #126888, #65616 ) ;
#12682 = ORIENTED_EDGE ( 'NONE', *, *, #24841, .T. ) ;
#12681 = VECTOR ( 'NONE', #209, 1000.000000000000114 ) ;
#12683 = DIRECTION ( 'NONE',  ( 0.000000000000000000, -0.1350103645451876666, -0.9908441862701600211 ) ) ;
#12685 = ORIENTED_EDGE ( 'NONE', *, *, #217316, .F. ) ;
#12684 = DIRECTION ( 'NONE',  ( 0.000000000000000000, 6.997203936713167125E-15, -1.000000000000000000 ) ) ;
#12686 = EDGE_LOOP ( 'NONE', ( #188067, #235958, #244957 ) ) ;
#12687 = FACE_OUTER_BOUND ( 'NONE', #68965, .T. ) ;
#12688 = EDGE_LOOP ( 'NONE', ( #178491, #83741, #225508, #254335, #130102, #116298, #135066, #166249, #155602, #6417, #62670, #229536, #209261, #213371, #243772, #8124, #60667, #44797, #179157, #251132, #7852, #35044, #117291 ) ) ;
#12689 = FACE_OUTER_BOUND ( 'NONE', #244722, .T. ) ;
#12690 = EDGE_CURVE ( 'NONE', #197777, #154965, #52573, .T. ) ;
#12691 = CONICAL_SURFACE ( 'NONE', #133478, 4.299999999999970512, 0.7853981633974466137 ) ;
#12692 = ORIENTED_EDGE ( 'NONE', *, *, #49968, .F. ) ;
#12693 = CARTESIAN_POINT ( 'NONE',  ( -16.88328101497759448, 66.04964716579338813, -149.1719279695951457 ) ) ;
#12694 = CARTESIAN_POINT ( 'NONE',  ( 21.05000000000000071, 85.40000000001178648, -79.41707660717668205 ) ) ;
#12695 = ADVANCED_FACE ( 'NONE', ( #248225 ), #229940, .T. ) ;
#12697 = ORIENTED_EDGE ( 'NONE', *, *, #183127, .T. ) ;
#12696 = ORIENTED_EDGE ( 'NONE', *, *, #248754, .F. ) ;
#12698 = VERTEX_POINT ( 'NONE', #113841 ) ;
#12699 = ORIENTED_EDGE ( 'NONE', *, *, #234019, .F. ) ;
#12700 = EDGE_LOOP ( 'NONE', ( #220085, #47729, #135777, #225300 ) ) ;
#12701 = DIRECTION ( 'NONE',  ( 0.000000000000000000, 6.982962677686266711E-15, -1.000000000000000000 ) ) ;
#12702 = DIRECTION ( 'NONE',  ( -1.000000000000000000, 0.000000000000000000, 0.000000000000000000 ) ) ;
#12703 = CARTESIAN_POINT ( 'NONE',  ( -14.87770893841224940, 9.430637101707896264, -185.7682606180609355 ) ) ;
#12705 = ORIENTED_EDGE ( 'NONE', *, *, #186171, .F. ) ;
#12704 = DIRECTION ( 'NONE',  ( 0.000000000000000000, 0.000000000000000000, 1.000000000000000000 ) ) ;
#12706 = CARTESIAN_POINT ( 'NONE',  ( 23.14999999999999503, 64.25000000001220712, -148.2731074845243882 ) ) ;
#12707 = ADVANCED_FACE ( 'NONE', ( #133415 ), #30464, .F. ) ;
#12708 = FACE_OUTER_BOUND ( 'NONE', #755, .T. ) ;
#12710 = ORIENTED_EDGE ( 'NONE', *, *, #247654, .F. ) ;
#12709 = FACE_BOUND ( 'NONE', #159419, .T. ) ;
#12711 = SPHERICAL_SURFACE ( 'NONE', #84339, 0.1000000000000000056 ) ;
#12712 = EDGE_LOOP ( 'NONE', ( #54838, #188745, #160254, #179121 ) ) ;
#12713 = DIRECTION ( 'NONE',  ( -4.239556034732056743E-17, 0.1298341882520022694, 0.9915357197604853789 ) ) ;
#12714 = CIRCLE ( 'NONE', #237726, 0.5000000000000008882 ) ;
#12715 = EDGE_LOOP ( 'NONE', ( #234551, #161143, #37177, #142301 ) ) ;
#12716 = DIRECTION ( 'NONE',  ( -1.836970198721029934E-16, -1.000000000000000000, -6.982962677686266711E-15 ) ) ;
#12717 = DIRECTION ( 'NONE',  ( 2.952720810173289112E-16, -1.000000000000000000, -0.000000000000000000 ) ) ;
#12718 = CIRCLE ( 'NONE', #214, 0.1000000000000098310 ) ;
#12720 = ADVANCED_FACE ( 'NONE', ( #70898 ), #35628, .F. ) ;
#12719 = VERTEX_POINT ( 'NONE', #51268 ) ;
#12722 = SPHERICAL_SURFACE ( 'NONE', #103852, 0.1000000000000000056 ) ;
#12721 = CARTESIAN_POINT ( 'NONE',  ( 18.49999999999996803, 14.83511725869332132, -235.8887435844146978 ) ) ;
#12723 = CARTESIAN_POINT ( 'NONE',  ( -20.94999999999999929, 87.48912529308798014, -106.0231074845242176 ) ) ;
#12724 = AXIS2_PLACEMENT_3D ( 'NONE', #226654, #12780, #247518 ) ;
#12725 = DIRECTION ( 'NONE',  ( 0.000000000000000000, 0.1575844902526560010, 0.9875055080513781558 ) ) ;
#12726 = DIRECTION ( 'NONE',  ( 1.000000000000000000, 0.000000000000000000, 0.000000000000000000 ) ) ;
#12727 = ORIENTED_EDGE ( 'NONE', *, *, #40912, .T. ) ;
#12728 = VERTEX_POINT ( 'NONE', #12203 ) ;
#12730 = AXIS2_PLACEMENT_3D ( 'NONE', #214761, #210920, #36150 ) ;
#12729 = CARTESIAN_POINT ( 'NONE',  ( -21.07954763557624744, 0.06587591862980950175, -127.6707090099604471 ) ) ;
#12731 = CARTESIAN_POINT ( 'NONE',  ( 18.59999999999999076, 11.65000000001115943, -192.3499999999999659 ) ) ;
#12732 = ORIENTED_EDGE ( 'NONE', *, *, #33193, .F. ) ;
#12733 = DIRECTION ( 'NONE',  ( 0.000000000000000000, -0.2128009952263604232, 0.9770955615653316162 ) ) ;
#12734 = VERTEX_POINT ( 'NONE', #212950 ) ;
#12735 = ADVANCED_FACE ( 'NONE', ( #233807 ), #210389, .F. ) ;
#12736 = CARTESIAN_POINT ( 'NONE',  ( 20.04142135623730070, 51.33926024308902925, -230.0993571250899379 ) ) ;
#12737 = DIRECTION ( 'NONE',  ( 0.000000000000000000, 0.000000000000000000, 1.000000000000000000 ) ) ;
#12738 = FACE_OUTER_BOUND ( 'NONE', #51082, .T. ) ;
#12739 = AXIS2_PLACEMENT_3D ( 'NONE', #114321, #109168, #193867 ) ;
#12740 = VERTEX_POINT ( 'NONE', #172590 ) ;
#12741 = CARTESIAN_POINT ( 'NONE',  ( -20.94999999999994600, 64.35000000001120668, -30.02310748452479316 ) ) ;
#12742 = AXIS2_PLACEMENT_3D ( 'NONE', #178880, #84834, #125293 ) ;
#12744 = ORIENTED_EDGE ( 'NONE', *, *, #162371, .T. ) ;
#12743 = VECTOR ( 'NONE', #199278, 1000.000000000000114 ) ;
#12745 = VERTEX_POINT ( 'NONE', #50016 ) ;
#12746 = ORIENTED_EDGE ( 'NONE', *, *, #77368, .F. ) ;
#12747 = CARTESIAN_POINT ( 'NONE',  ( 21.05000000000000071, -1.162701749926853712, -75.10000000000003695 ) ) ;
#12748 = CARTESIAN_POINT ( 'NONE',  ( 12.29592348164039528, 66.64419340838141181, -53.23200495297823664 ) ) ;
#12749 = DIRECTION ( 'NONE',  ( -1.000000000000000000, -0.000000000000000000, -0.000000000000000000 ) ) ;
#12750 = LINE ( 'NONE', #92244, #48829 ) ;
#12752 = DIRECTION ( 'NONE',  ( 1.000000000000000000, 0.000000000000000000, 0.000000000000000000 ) ) ;
#12751 = CARTESIAN_POINT ( 'NONE',  ( -23.25000000000000000, 76.00000000001165290, -69.52310748452431710 ) ) ;
#12754 = VERTEX_POINT ( 'NONE', #253348 ) ;
#12753 = CYLINDRICAL_SURFACE ( 'NONE', #160589, 0.09999999999998898659 ) ;
#12755 = LINE ( 'NONE', #210930, #212322 ) ;
#12756 = VERTEX_POINT ( 'NONE', #211683 ) ;
#12757 = CARTESIAN_POINT ( 'NONE',  ( 20.85000000000000142, 77.85161776048127535, -158.4199177649206831 ) ) ;
#12758 = EDGE_LOOP ( 'NONE', ( #235315, #113092, #226535 ) ) ;
#12759 = ORIENTED_EDGE ( 'NONE', *, *, #102553, .F. ) ;
#12760 = CARTESIAN_POINT ( 'NONE',  ( 18.59999999999999076, 67.65998959290219261, -227.8609496483021530 ) ) ;
#12761 = DIRECTION ( 'NONE',  ( -1.000000000000000000, 0.000000000000000000, 0.000000000000000000 ) ) ;
#12762 = DIRECTION ( 'NONE',  ( 0.000000000000000000, -0.4721928772777346239, -0.8814952561688430555 ) ) ;
#12763 = CARTESIAN_POINT ( 'NONE',  ( -18.59999999999999787, 7.120270961708750512, -204.6595630418393057 ) ) ;
#12764 = CIRCLE ( 'NONE', #183430, 0.1000000000000028644 ) ;
#12765 = DIRECTION ( 'NONE',  ( 1.000000000000000000, 0.000000000000000000, 0.000000000000000000 ) ) ;
#12766 = ORIENTED_EDGE ( 'NONE', *, *, #130555, .F. ) ;
#12767 = VERTEX_POINT ( 'NONE', #149142 ) ;
#12768 = CYLINDRICAL_SURFACE ( 'NONE', #140794, 0.1000000000000052097 ) ;
#12769 = EDGE_LOOP ( 'NONE', ( #85709, #157379, #210149 ) ) ;
#12770 = LINE ( 'NONE', #190108, #173725 ) ;
#12771 = CARTESIAN_POINT ( 'NONE',  ( 5.900000000000060751, 64.35000000001120668, -22.02310748452479316 ) ) ;
#12772 = ORIENTED_EDGE ( 'NONE', *, *, #257916, .F. ) ;
#12773 = LINE ( 'NONE', #14050, #7169 ) ;
#12774 = CARTESIAN_POINT ( 'NONE',  ( -23.25000000000000000, 69.01799029515544248, -99.32695536626806643 ) ) ;
#12775 = DIRECTION ( 'NONE',  ( 1.000000000000000000, 0.000000000000000000, 0.000000000000000000 ) ) ;
#12776 = DIRECTION ( 'NONE',  ( -3.787827842127535236E-15, -0.8900778951570268438, -0.4558084472153153266 ) ) ;
#12777 = VERTEX_POINT ( 'NONE', #91715 ) ;
#12778 = FACE_OUTER_BOUND ( 'NONE', #233232, .T. ) ;
#12779 = DIRECTION ( 'NONE',  ( -1.000000000000000000, 0.000000000000000000, 0.000000000000000000 ) ) ;
#12780 = DIRECTION ( 'NONE',  ( 0.000000000000000000, 0.000000000000000000, 1.000000000000000000 ) ) ;
#12781 = CARTESIAN_POINT ( 'NONE',  ( -21.05000000000000071, 87.75000000001173817, -72.52310748452423184 ) ) ;
#12782 = CIRCLE ( 'NONE', #212678, 0.5000000000000004441 ) ;
#12783 = CIRCLE ( 'NONE', #91858, 0.09999999999999939493 ) ;
#12785 = ADVANCED_FACE ( 'NONE', ( #171307 ), #230943, .T. ) ;
#12784 = DIRECTION ( 'NONE',  ( 1.000000000000000000, 0.000000000000000000, 0.000000000000000000 ) ) ;
#12786 = CIRCLE ( 'NONE', #50151, 0.09999999999999939493 ) ;
#12787 = DIRECTION ( 'NONE',  ( 0.000000000000000000, 0.000000000000000000, -1.000000000000000000 ) ) ;
#12788 = ORIENTED_EDGE ( 'NONE', *, *, #242862, .F. ) ;
#12789 = AXIS2_PLACEMENT_3D ( 'NONE', #64739, #33055, #13449 ) ;
#12790 = DIRECTION ( 'NONE',  ( -1.000000000000000000, -2.885090398161910739E-16, -6.283419270304611573E-17 ) ) ;
#12791 = EDGE_CURVE ( 'NONE', #153790, #121700, #39415, .T. ) ;
#12792 = ORIENTED_EDGE ( 'NONE', *, *, #169314, .T. ) ;
#12793 = DIRECTION ( 'NONE',  ( -0.7071067811865389130, -5.024295867788141276E-15, 0.7071067811865561215 ) ) ;
#12794 = CARTESIAN_POINT ( 'NONE',  ( -23.25000000000000000, -1.249999999988843369, -74.80048075441509070 ) ) ;
#12795 = CYLINDRICAL_SURFACE ( 'NONE', #33833, 0.1000000000000101918 ) ;
#12796 = CARTESIAN_POINT ( 'NONE',  ( 21.14999999999999858, 10.71339244341104013, -179.7499999999999716 ) ) ;
#12797 = DIRECTION ( 'NONE',  ( 1.000000000000000000, -0.000000000000000000, 0.000000000000000000 ) ) ;
#12798 = DIRECTION ( 'NONE',  ( -4.701977403289178058E-30, -2.433019743745433765E-14, 1.000000000000000000 ) ) ;
#12800 = EDGE_CURVE ( 'NONE', #17738, #106574, #218415, .T. ) ;
#12799 = VECTOR ( 'NONE', #134315, 1000.000000000000000 ) ;
#12801 = EDGE_LOOP ( 'NONE', ( #25673, #80183, #180954, #10776, #157881 ) ) ;
#12802 = CARTESIAN_POINT ( 'NONE',  ( -16.91049119928362643, 66.05000000001223270, -149.1413870913335415 ) ) ;
#12803 = DIRECTION ( 'NONE',  ( 7.304098846218134667E-16, 1.000000000000000000, 6.982962677686267499E-15 ) ) ;
#12804 = DIRECTION ( 'NONE',  ( -1.000000000000000000, 1.652117596168391700E-15, 0.000000000000000000 ) ) ;
#12805 = DIRECTION ( 'NONE',  ( 0.000000000000000000, 1.000000000000000000, 0.000000000000000000 ) ) ;
#12806 = DIRECTION ( 'NONE',  ( 0.000000000000000000, 0.000000000000000000, -1.000000000000000000 ) ) ;
#12807 = ORIENTED_EDGE ( 'NONE', *, *, #45837, .T. ) ;
#12808 = ORIENTED_EDGE ( 'NONE', *, *, #80041, .F. ) ;
#12809 = DIRECTION ( 'NONE',  ( -1.646408749285562691E-14, -1.000000000000000000, -6.982962677686266711E-15 ) ) ;
#12811 = ADVANCED_FACE ( 'NONE', ( #30475 ), #189543, .F. ) ;
#12810 = CARTESIAN_POINT ( 'NONE',  ( -18.59999999999999787, -9.321008403350132809, -107.7359382490779183 ) ) ;
#12812 =( BOUNDED_SURFACE ( )  B_SPLINE_SURFACE ( 3, 2, ( 
 ( #85535, #4730, #8612 ),
 ( #145537, #47716, #225061 ),
 ( #64725, #46436, #88108 ),
 ( #162567, #122143, #141687 ) ),
 .UNSPECIFIED., .F., .F., .F. ) 
 B_SPLINE_SURFACE_WITH_KNOTS ( ( 4, 4 ),
 ( 3, 3 ),
 ( 0.0008258556059633754111, 0.0009616864997632845833 ),
 ( 0.000000000000000000, 1.000000000000000000 ),
 .UNSPECIFIED. ) 
 GEOMETRIC_REPRESENTATION_ITEM ( )  RATIONAL_B_SPLINE_SURFACE ( (
 ( 1.000000000000000000, 0.9152888060719349683, 1.000000000000000000),
 ( 1.000000000000000000, 0.9327727094138200670, 1.000000000000000000),
 ( 1.000000000000000000, 0.9369023509258446181, 1.000000000000000000),
 ( 1.000000000000000000, 0.9246339933864486937, 1.000000000000000000) ) ) 
 REPRESENTATION_ITEM ( '' )  SURFACE ( )  );
#12813 = CARTESIAN_POINT ( 'NONE',  ( -20.94999999999999929, 44.00266445878927613, -258.8505972146074896 ) ) ;
#12814 = EDGE_CURVE ( 'NONE', #214618, #65824, #97027, .T. ) ;
#12815 = AXIS2_PLACEMENT_3D ( 'NONE', #196230, #52863, #15052 ) ;
#12816 = ORIENTED_EDGE ( 'NONE', *, *, #126816, .F. ) ;
#12817 = EDGE_CURVE ( 'NONE', #155744, #213386, #100663, .T. ) ;
#12818 = CONTEXT_DEPENDENT_SHAPE_REPRESENTATION ( #82428, #3935 ) ;
#12819 = CARTESIAN_POINT ( 'NONE',  ( 23.15000000000000213, -8.596261682231828516, -158.0498724828497359 ) ) ;
#12820 = VECTOR ( 'NONE', #125973, 1000.000000000000000 ) ;
#12821 = EDGE_LOOP ( 'NONE', ( #182378, #214334, #185204 ) ) ;
#12822 = CARTESIAN_POINT ( 'NONE',  ( 23.24999999999999289, 6.450000000011156587, -155.7499999999999716 ) ) ;
#12823 = EDGE_CURVE ( 'NONE', #17520, #53190, #99392, .T. ) ;
#12824 = ORIENTED_EDGE ( 'NONE', *, *, #158539, .T. ) ;
#12826 = ORIENTED_EDGE ( 'NONE', *, *, #2935, .T. ) ;
#12825 = CARTESIAN_POINT ( 'NONE',  ( 18.59999999999999076, 76.00000000001170974, -69.52310748452431710 ) ) ;
#12827 = VECTOR ( 'NONE', #197145, 1000.000000000000000 ) ;
#12828 = ORIENTED_EDGE ( 'NONE', *, *, #46792, .T. ) ;
#12829 = DIRECTION ( 'NONE',  ( 1.000000000000000000, 0.000000000000000000, -0.000000000000000000 ) ) ;
#12830 = CARTESIAN_POINT ( 'NONE',  ( -23.25000000000000000, 0.000000000000000000, 0.000000000000000000 ) ) ;
#12831 = DIRECTION ( 'NONE',  ( 0.000000000000000000, 0.000000000000000000, -1.000000000000000000 ) ) ;
#12832 = DIRECTION ( 'NONE',  ( 0.000000000000000000, -6.982962677686266711E-15, 1.000000000000000000 ) ) ;
#12833 = DIRECTION ( 'NONE',  ( 1.000000000000000000, 0.000000000000000000, 0.000000000000000000 ) ) ;
#12834 = CARTESIAN_POINT ( 'NONE',  ( 20.94999999999999929, -4.254329952141541860, -236.2118329068272260 ) ) ;
#12835 = ADVANCED_FACE ( 'NONE', ( #135959 ), #175154, .F. ) ;
#12837 = DIRECTION ( 'NONE',  ( 1.000000000000000000, 0.000000000000000000, -0.000000000000000000 ) ) ;
#12836 = DIRECTION ( 'NONE',  ( 7.589415207398576792E-15, -1.000000000000000000, -0.000000000000000000 ) ) ;
#12838 = CARTESIAN_POINT ( 'NONE',  ( -16.27683809663750480, 9.350000000011133849, -176.7499999999999716 ) ) ;
#12839 = CARTESIAN_POINT ( 'NONE',  ( 23.25000000000000000, -11.48912529307605546, -30.39999999999999503 ) ) ;
#12840 = CARTESIAN_POINT ( 'NONE',  ( -18.59999999999999787, 11.65000000001115232, -21.75000000000000355 ) ) ;
#12841 = DIRECTION ( 'NONE',  ( 0.000000000000000000, 0.000000000000000000, 1.000000000000000000 ) ) ;
#12842 = VECTOR ( 'NONE', #79195, 1000.000000000000000 ) ;
#12843 = ORIENTED_EDGE ( 'NONE', *, *, #26272, .T. ) ;
#12844 = CIRCLE ( 'NONE', #96189, 2.000000000000001776 ) ;
#12845 = LINE ( 'NONE', #171938, #170411 ) ;
#12846 = CARTESIAN_POINT ( 'NONE',  ( 23.15000000000000213, -8.663551401869158397, -9.524101118067305194 ) ) ;
#12847 = VECTOR ( 'NONE', #137286, 1000.000000000000000 ) ;
#12848 = AXIS2_PLACEMENT_3D ( 'NONE', #194638, #212893, #255815 ) ;
#12849 = DIRECTION ( 'NONE',  ( 0.000000000000000000, 0.8814952561688428334, -0.4721928772777349570 ) ) ;
#12850 = DIRECTION ( 'NONE',  ( -1.652117596168391700E-15, 1.000000000000000000, 6.982962677686266711E-15 ) ) ;
#12851 = AXIS2_PLACEMENT_3D ( 'NONE', #70539, #127920, #228307 ) ;
#12852 = EDGE_LOOP ( 'NONE', ( #218466, #149517, #9819 ) ) ;
#12853 = AXIS2_PLACEMENT_3D ( 'NONE', #139184, #222573, #177083 ) ;
#12854 = ORIENTED_EDGE ( 'NONE', *, *, #93490, .T. ) ;
#12855 = CARTESIAN_POINT ( 'NONE',  ( -22.50000000000000000, 76.00000000001203659, -114.6726782920691221 ) ) ;
#12856 = VERTEX_POINT ( 'NONE', #254614 ) ;
#12857 = CARTESIAN_POINT ( 'NONE',  ( 20.94999999999999574, 10.47338541492405994, -141.5786544642485580 ) ) ;
#12858 = FACE_OUTER_BOUND ( 'NONE', #151456, .T. ) ;
#12859 = VECTOR ( 'NONE', #213521, 1000.000000000000000 ) ;
#12860 = AXIS2_PLACEMENT_3D ( 'NONE', #95313, #118747, #215262 ) ;
#12861 = AXIS2_PLACEMENT_3D ( 'NONE', #244943, #165423, #46734 ) ;
#12862 = AXIS2_PLACEMENT_3D ( 'NONE', #107988, #68878, #150967 ) ;
#12863 = VECTOR ( 'NONE', #126270, 1000.000000000000000 ) ;
#12864 = EDGE_CURVE ( 'NONE', #74720, #52643, #47164, .T. ) ;
#12865 = ADVANCED_FACE ( 'NONE', ( #199823 ), #113829, .T. ) ;
#12866 = ORIENTED_EDGE ( 'NONE', *, *, #163109, .F. ) ;
#12867 = DIRECTION ( 'NONE',  ( 0.7071067811865487940, 0.000000000000000000, -0.7071067811865463515 ) ) ;
#12868 = ORIENTED_EDGE ( 'NONE', *, *, #45600, .T. ) ;
#12869 = EDGE_CURVE ( 'NONE', #81561, #82525, #192952, .T. ) ;
#12872 = EDGE_CURVE ( 'NONE', #79646, #183531, #96814, .T. ) ;
#12871 =( BOUNDED_SURFACE ( )  B_SPLINE_SURFACE ( 3, 2, ( 
 ( #198280, #40540, #97867 ),
 ( #140888, #239991, #116205 ),
 ( #159189, #156634, #254380 ),
 ( #19662, #178766, #155344 ) ),
 .UNSPECIFIED., .F., .F., .F. ) 
 B_SPLINE_SURFACE_WITH_KNOTS ( ( 4, 4 ),
 ( 3, 3 ),
 ( 0.0008258556059633782300, 0.0009616864997632838244 ),
 ( 0.000000000000000000, 1.000000000000000000 ),
 .UNSPECIFIED. ) 
 GEOMETRIC_REPRESENTATION_ITEM ( )  RATIONAL_B_SPLINE_SURFACE ( (
 ( 1.000000000000000000, 0.9152888060719127639, 1.000000000000000000),
 ( 1.000000000000000000, 0.9327727094137693298, 1.000000000000000000),
 ( 1.000000000000000000, 0.9369023509258749272, 1.000000000000000000),
 ( 1.000000000000000000, 0.9246339933864399230, 1.000000000000000000) ) ) 
 REPRESENTATION_ITEM ( '' )  SURFACE ( )  );
#12870 = CARTESIAN_POINT ( 'NONE',  ( 23.14999999999999503, 28.81810206650552075, -238.0339362645743222 ) ) ;
#12873 = DIRECTION ( 'NONE',  ( 0.000000000000000000, -6.982962677686266711E-15, 1.000000000000000000 ) ) ;
#12874 = CARTESIAN_POINT ( 'NONE',  ( 23.24999999999999289, 52.91185528119409298, -244.1460391050142675 ) ) ;
#12875 = CYLINDRICAL_SURFACE ( 'NONE', #121006, 0.1000000000000076522 ) ;
#12876 = FACE_OUTER_BOUND ( 'NONE', #82724, .T. ) ;
#12877 = VECTOR ( 'NONE', #209583, 1000.000000000000000 ) ;
#12878 = FACE_OUTER_BOUND ( 'NONE', #157671, .T. ) ;
#12879 = ADVANCED_FACE ( 'NONE', ( #139808 ), #195966, .F. ) ;
#12880 = FACE_OUTER_BOUND ( 'NONE', #98271, .T. ) ;
#12881 = CARTESIAN_POINT ( 'NONE',  ( -20.54999999999999716, 85.00000000001261924, -194.1291383618718385 ) ) ;
#12883 = ORIENTED_EDGE ( 'NONE', *, *, #219270, .T. ) ;
#12882 = CARTESIAN_POINT ( 'NONE',  ( -1.739115166359751801E-14, 11.65000000001114699, -192.3499999999999659 ) ) ;
#12885 = CARTESIAN_POINT ( 'NONE',  ( -18.50000000000000000, 9.350000000011156942, -146.1500000000000341 ) ) ;
#12884 = CARTESIAN_POINT ( 'NONE',  ( -20.54999999999999716, 25.27005795345702666, -235.3392409252341224 ) ) ;
#12886 = ORIENTED_EDGE ( 'NONE', *, *, #199779, .T. ) ;
#12888 = ORIENTED_EDGE ( 'NONE', *, *, #103593, .T. ) ;
#12887 = LINE ( 'NONE', #115812, #106862 ) ;
#12889 = ADVANCED_FACE ( 'NONE', ( #120307 ), #17327, .T. ) ;
#12890 = EDGE_LOOP ( 'NONE', ( #242595, #237755, #172582, #251650 ) ) ;
#12891 = CARTESIAN_POINT ( 'NONE',  ( 20.90000000000000213, 8.000000000000000000, 1.212568896937007867 ) ) ;
#12893 = EDGE_CURVE ( 'NONE', #20901, #66550, #81116, .T. ) ;
#12892 = EDGE_CURVE ( 'NONE', #210898, #21362, #21196, .T. ) ;
#12894 = DIRECTION ( 'NONE',  ( -1.000000000000000000, 0.000000000000000000, 0.000000000000000000 ) ) ;
#12895 = CARTESIAN_POINT ( 'NONE',  ( -21.45000000000000284, 7.708578643773852157, -188.6499999999999488 ) ) ;
#12896 = CARTESIAN_POINT ( 'NONE',  ( 18.52165635395184751, -9.481150711282177568, -7.024837582862474505 ) ) ;
#12897 = CARTESIAN_POINT ( 'NONE',  ( -23.15000000000000213, 85.00000000001149658, -45.31707660717669484 ) ) ;
#12898 = LINE ( 'NONE', #151105, #91054 ) ;
#12899 = DIRECTION ( 'NONE',  ( -0.000000000000000000, -6.982962677686266711E-15, 1.000000000000000000 ) ) ;
#12900 = CIRCLE ( 'NONE', #46181, 0.09999999999999939493 ) ;
#12901 = ADVANCED_FACE ( 'NONE', ( #160708 ), #216785, .T. ) ;
#12902 = DIRECTION ( 'NONE',  ( 1.000000000000000000, 0.000000000000000000, 0.000000000000000000 ) ) ;
#12903 = ORIENTED_EDGE ( 'NONE', *, *, #79470, .T. ) ;
#12904 = ORIENTED_EDGE ( 'NONE', *, *, #147687, .F. ) ;
#12905 = DIRECTION ( 'NONE',  ( 1.000000000000000000, -1.207181226542539700E-16, 2.694675058168174199E-16 ) ) ;
#12906 = EDGE_CURVE ( 'NONE', #91084, #84620, #197015, .T. ) ;
#12907 = ADVANCED_FACE ( 'NONE', ( #197229 ), #36917, .F. ) ;
#12908 = AXIS2_PLACEMENT_3D ( 'NONE', #149264, #13596, #12325 ) ;
#12909 = ORIENTED_EDGE ( 'NONE', *, *, #142449, .F. ) ;
#12910 = LINE ( 'NONE', #131543, #179910 ) ;
#12911 = ORIENTED_EDGE ( 'NONE', *, *, #148424, .F. ) ;
#12912 = DIRECTION ( 'NONE',  ( 4.336808689942017736E-16, -0.000000000000000000, 1.000000000000000000 ) ) ;
#12913 =( BOUNDED_CURVE ( )  B_SPLINE_CURVE ( 3, ( #237953, #97121, #116728, #115437 ),
 .UNSPECIFIED., .F., .F. ) 
 B_SPLINE_CURVE_WITH_KNOTS ( ( 4, 4 ),
 ( 0.5235987755982449698, 1.570796326794896558 ),
 .UNSPECIFIED. ) 
 CURVE ( )  GEOMETRIC_REPRESENTATION_ITEM ( )  RATIONAL_B_SPLINE_CURVE ( ( 1.000000000000000000, 0.9106836025229499976, 0.9106836025229499976, 1.000000000000000000 ) ) 
 REPRESENTATION_ITEM ( '' )  );
#12914 = EDGE_CURVE ( 'NONE', #48943, #73041, #172140, .T. ) ;
#12915 = AXIS2_PLACEMENT_3D ( 'NONE', #226295, #168961, #64673 ) ;
#12916 = DIRECTION ( 'NONE',  ( 1.000000000000000000, 0.000000000000000000, 0.000000000000000000 ) ) ;
#12917 = CARTESIAN_POINT ( 'NONE',  ( -21.07016717456947319, 69.67905916191169524, -103.0231074845243455 ) ) ;
#12918 = CARTESIAN_POINT ( 'NONE',  ( -20.94999999999999929, 74.83729825007462466, -195.4231074845243654 ) ) ;
#12919 = CARTESIAN_POINT ( 'NONE',  ( 18.59999999999999432, 77.63717271298224887, -91.44095411905229298 ) ) ;
#12920 = VERTEX_POINT ( 'NONE', #158155 ) ;
#12921 = EDGE_CURVE ( 'NONE', #140349, #205600, #226207, .T. ) ;
#12922 = FACE_OUTER_BOUND ( 'NONE', #71384, .T. ) ;
#12923 = LINE ( 'NONE', #247650, #28701 ) ;
#12924 = VECTOR ( 'NONE', #223058, 1000.000000000000000 ) ;
#12925 = DIRECTION ( 'NONE',  ( 0.000000000000000000, -0.9651348961777156399, 0.2617529984165037349 ) ) ;
#12926 = CARTESIAN_POINT ( 'NONE',  ( -16.92507428761699018, 66.05000000001255955, -182.7365049441459917 ) ) ;
#12927 = DIRECTION ( 'NONE',  ( 1.000000000000000000, 7.304098846218133681E-16, -4.217023435051677501E-16 ) ) ;
#12928 = ORIENTED_EDGE ( 'NONE', *, *, #87763, .F. ) ;
#12931 = DIRECTION ( 'NONE',  ( 0.000000000000000000, 0.9908441862701782288, -0.1350103645450542456 ) ) ;
#12930 = CARTESIAN_POINT ( 'NONE',  ( -17.11825945287482753, 60.96553306590055854, -220.9452142459683159 ) ) ;
#12929 = CIRCLE ( 'NONE', #62965, 0.3999999999999975797 ) ;
#12932 = ORIENTED_EDGE ( 'NONE', *, *, #87980, .T. ) ;
#12935 = ORIENTED_EDGE ( 'NONE', *, *, #108880, .T. ) ;
#12934 = CARTESIAN_POINT ( 'NONE',  ( 22.57320508075687115, 64.25000000001215028, -136.5231074845243597 ) ) ;
#12933 = CYLINDRICAL_SURFACE ( 'NONE', #82443, 0.1000000000000028644 ) ;
#12936 = AXIS2_PLACEMENT_3D ( 'NONE', #190065, #90955, #170556 ) ;
#12937 = DIRECTION ( 'NONE',  ( 0.000000000000000000, -0.2617529984164506107, -0.9651348961777299618 ) ) ;
#12938 = AXIS2_PLACEMENT_3D ( 'NONE', #117163, #155029, #137979 ) ;
#12939 = FACE_OUTER_BOUND ( 'NONE', #45957, .T. ) ;
#12940 = VERTEX_POINT ( 'NONE', #198512 ) ;
#12941 = DIRECTION ( 'NONE',  ( -0.000000000000000000, 1.000000000000000000, 6.982962677686266711E-15 ) ) ;
#12942 = CARTESIAN_POINT ( 'NONE',  ( -23.25000000000000000, 71.65000000001199965, -115.3731074845243256 ) ) ;
#12943 = FACE_OUTER_BOUND ( 'NONE', #81070, .T. ) ;
#12945 = ORIENTED_EDGE ( 'NONE', *, *, #133328, .T. ) ;
#12944 = LINE ( 'NONE', #52019, #72687 ) ;
#12946 = ORIENTED_EDGE ( 'NONE', *, *, #198662, .T. ) ;
#12947 = DIRECTION ( 'NONE',  ( 0.000000000000000000, 1.000000000000000000, 0.000000000000000000 ) ) ;
#12948 = CARTESIAN_POINT ( 'NONE',  ( -23.15000000000000213, 74.00000000001151079, -49.24772940728643533 ) ) ;
#12949 = DIRECTION ( 'NONE',  ( 0.000000000000000000, 6.982962677686266711E-15, -1.000000000000000000 ) ) ;
#12950 = DIRECTION ( 'NONE',  ( 0.000000000000000000, 0.000000000000000000, 1.000000000000000000 ) ) ;
#12951 = ORIENTED_EDGE ( 'NONE', *, *, #152942, .T. ) ;
#12952 = CARTESIAN_POINT ( 'NONE',  ( 20.94999999999999929, 77.83534155023701828, -191.9679561919613491 ) ) ;
#12953 = CARTESIAN_POINT ( 'NONE',  ( -22.59999999999999787, 7.128833340093095217, -233.7327013124392749 ) ) ;
#12954 = LINE ( 'NONE', #151168, #105889 ) ;
#12955 = ORIENTED_EDGE ( 'NONE', *, *, #222690, .T. ) ;
#12956 = CARTESIAN_POINT ( 'NONE',  ( 20.22516295850462598, 59.74753603935580060, -225.6296577699291106 ) ) ;
#12957 = DIRECTION ( 'NONE',  ( 1.000000000000000000, 0.000000000000000000, 0.000000000000000000 ) ) ;
#12958 = AXIS2_PLACEMENT_3D ( 'NONE', #42367, #121918, #102299 ) ;
#12959 = EDGE_CURVE ( 'NONE', #142529, #16905, #27618, .T. ) ;
#12960 = VECTOR ( 'NONE', #52169, 1000.000000000000000 ) ;
#12961 = AXIS2_PLACEMENT_3D ( 'NONE', #113845, #170020, #193407 ) ;
#12962 = EDGE_LOOP ( 'NONE', ( #71923, #163572, #246862, #52313 ) ) ;
#12963 = AXIS2_PLACEMENT_3D ( 'NONE', #230542, #251372, #212270 ) ;
#12964 = DIRECTION ( 'NONE',  ( 1.000000000000000000, 0.000000000000000000, 0.000000000000000000 ) ) ;
#12966 = ADVANCED_FACE ( 'NONE', ( #104515 ), #105802, .T. ) ;
#12965 = CARTESIAN_POINT ( 'NONE',  ( 21.72449340488910252, 10.28395627750227703, -46.15000000000001279 ) ) ;
#12967 = VERTEX_POINT ( 'NONE', #122846 ) ;
#12968 = AXIS2_PLACEMENT_3D ( 'NONE', #133393, #192094, #190827 ) ;
#12969 = EDGE_LOOP ( 'NONE', ( #230743, #140518, #181105, #205359 ) ) ;
#12970 = EDGE_CURVE ( 'NONE', #128733, #78948, #155566, .T. ) ;
#12971 = DIRECTION ( 'NONE',  ( 1.000000000000000000, 0.000000000000000000, 0.000000000000000000 ) ) ;
#12972 = EDGE_LOOP ( 'NONE', ( #63437, #213151, #126932, #256855 ) ) ;
#12975 = EDGE_CURVE ( 'NONE', #54257, #242821, #130391, .T. ) ;
#12974 = ORIENTED_EDGE ( 'NONE', *, *, #37276, .T. ) ;
#12973 = DIRECTION ( 'NONE',  ( 1.000000000000000000, 0.000000000000000000, 0.000000000000000000 ) ) ;
#12976 = ORIENTED_EDGE ( 'NONE', *, *, #6135, .F. ) ;
#12977 = AXIS2_PLACEMENT_3D ( 'NONE', #8948, #147166, #227996 ) ;
#12980 = ORIENTED_EDGE ( 'NONE', *, *, #240302, .F. ) ;
#12979 = ORIENTED_EDGE ( 'NONE', *, *, #31337, .T. ) ;
#12978 = DIRECTION ( 'NONE',  ( 0.000000000000000000, 0.000000000000000000, -1.000000000000000000 ) ) ;
#12981 = CARTESIAN_POINT ( 'NONE',  ( -20.94999999999994245, 67.85000000001119247, -51.02310748452479316 ) ) ;
#12982 = ORIENTED_EDGE ( 'NONE', *, *, #243795, .T. ) ;
#12983 = CARTESIAN_POINT ( 'NONE',  ( 20.94999999999999929, 24.04029978241812060, -253.0016354099517457 ) ) ;
#12984 = LINE ( 'NONE', #74251, #199254 ) ;
#12985 = FACE_OUTER_BOUND ( 'NONE', #94350, .T. ) ;
#12986 = EDGE_CURVE ( 'NONE', #147651, #236113, #205380, .T. ) ;
#12987 = DIRECTION ( 'NONE',  ( -3.265361837132813093E-16, -0.4088369013363280513, 0.9126074666063769270 ) ) ;
#12988 = LINE ( 'NONE', #153810, #92804 ) ;
#12990 = EDGE_CURVE ( 'NONE', #82525, #112448, #17953, .T. ) ;
#12989 = VERTEX_POINT ( 'NONE', #227055 ) ;
#12991 = ORIENTED_EDGE ( 'NONE', *, *, #172799, .F. ) ;
#12992 = ORIENTED_EDGE ( 'NONE', *, *, #31476, .F. ) ;
#12993 = CARTESIAN_POINT ( 'NONE',  ( 20.94999999999999929, 76.00000000001193712, -107.0231074845243029 ) ) ;
#12995 = ORIENTED_EDGE ( 'NONE', *, *, #87188, .F. ) ;
#12994 = CARTESIAN_POINT ( 'NONE',  ( 21.05000000000000071, 64.35000000001267040, -203.5231074845244166 ) ) ;
#12996 = EDGE_LOOP ( 'NONE', ( #33480, #208453, #194883, #57495 ) ) ;
#12997 = AXIS2_PLACEMENT_3D ( 'NONE', #56075, #15725, #39128 ) ;
#12998 = ORIENTED_EDGE ( 'NONE', *, *, #59736, .T. ) ;
#12999 = DIRECTION ( 'NONE',  ( -0.000000000000000000, -0.000000000000000000, 1.000000000000000000 ) ) ;
#13000 = CIRCLE ( 'NONE', #17269, 0.09999999999998898659 ) ;
#13001 = EDGE_CURVE ( 'NONE', #42929, #63249, #213789, .T. ) ;
#13002 = ORIENTED_EDGE ( 'NONE', *, *, #201292, .F. ) ;
#13004 = VECTOR ( 'NONE', #256247, 1000.000000000000114 ) ;
#13003 = LINE ( 'NONE', #151218, #6347 ) ;
#13005 = FACE_OUTER_BOUND ( 'NONE', #154818, .T. ) ;
#13006 = ADVANCED_FACE ( 'NONE', ( #221900 ), #8032, .F. ) ;
#13008 = VERTEX_POINT ( 'NONE', #43301 ) ;
#13007 = ORIENTED_EDGE ( 'NONE', *, *, #157994, .F. ) ;
#13009 = ORIENTED_EDGE ( 'NONE', *, *, #204131, .F. ) ;
#13010 = VECTOR ( 'NONE', #145188, 1000.000000000000000 ) ;
#13011 = VERTEX_POINT ( 'NONE', #67988 ) ;
#13012 = ORIENTED_EDGE ( 'NONE', *, *, #16454, .F. ) ;
#13013 = DIRECTION ( 'NONE',  ( 0.000000000000000000, 0.000000000000000000, -1.000000000000000000 ) ) ;
#13014 = VECTOR ( 'NONE', #78477, 1000.000000000000000 ) ;
#13016 = VERTEX_POINT ( 'NONE', #62852 ) ;
#13015 = DIRECTION ( 'NONE',  ( 0.000000000000000000, -0.1332476588733448597, -0.9910827722268067408 ) ) ;
#13017 = CYLINDRICAL_SURFACE ( 'NONE', #214835, 0.5000000000000014433 ) ;
#13019 = DIRECTION ( 'NONE',  ( -1.000000000000000000, -0.000000000000000000, -0.000000000000000000 ) ) ;
#13018 = DIRECTION ( 'NONE',  ( 1.000000000000000000, 0.000000000000000000, 0.000000000000000000 ) ) ;
#13020 = EDGE_CURVE ( 'NONE', #33881, #237173, #25040, .T. ) ;
#13021 = CARTESIAN_POINT ( 'NONE',  ( -18.39999999999999858, 11.47316190337362585, -42.79982924846601122 ) ) ;
#13022 = ORIENTED_EDGE ( 'NONE', *, *, #115843, .F. ) ;
#13023 = ADVANCED_FACE ( 'NONE', ( #202365 ), #103241, .F. ) ;
#13024 = ORIENTED_EDGE ( 'NONE', *, *, #192089, .T. ) ;
#13025 = CARTESIAN_POINT ( 'NONE',  ( 18.48413544395646113, 85.66430403363958135, -96.34000249148589035 ) ) ;
#13026 = SPHERICAL_SURFACE ( 'NONE', #251690, 0.1000000000000000056 ) ;
#13027 = LINE ( 'NONE', #252885, #49526 ) ;
#13030 = ADVANCED_FACE ( 'NONE', ( #48416 ), #56571, .T. ) ;
#13029 = ORIENTED_EDGE ( 'NONE', *, *, #6043, .T. ) ;
#13028 = AXIS2_PLACEMENT_3D ( 'NONE', #86582, #166188, #67055 ) ;
#13031 = VECTOR ( 'NONE', #158846, 1000.000000000000114 ) ;
#13032 = CARTESIAN_POINT ( 'NONE',  ( -16.93589915522259304, 51.67754058831158659, -231.8559428553618318 ) ) ;
#13033 = CARTESIAN_POINT ( 'NONE',  ( -21.05000000000000071, 1.115600667400684642E-11, -33.50000000000000000 ) ) ;
#13034 = ORIENTED_EDGE ( 'NONE', *, *, #91404, .F. ) ;
#13035 = ORIENTED_EDGE ( 'NONE', *, *, #41844, .T. ) ;
#13036 = CARTESIAN_POINT ( 'NONE',  ( -23.15000000000000213, 59.19392724319018129, -220.9828015967491126 ) ) ;
#13037 = CARTESIAN_POINT ( 'NONE',  ( -16.78569801330232281, 66.05206626689856364, -123.8661945791768630 ) ) ;
#13038 = VERTEX_POINT ( 'NONE', #65418 ) ;
#13039 = DIRECTION ( 'NONE',  ( 1.000000000000000000, 0.000000000000000000, 0.000000000000000000 ) ) ;
#13040 = EDGE_LOOP ( 'NONE', ( #185620, #9150, #193775, #47801, #69019, #142300, #89579, #227387, #45635, #199314, #58093, #75285 ) ) ;
#13041 = EDGE_CURVE ( 'NONE', #246033, #1104, #43100, .T. ) ;
#13042 = CARTESIAN_POINT ( 'NONE',  ( 18.41832399655374886, -9.682403266662264585, -140.6568436200283543 ) ) ;
#13044 = VECTOR ( 'NONE', #162342, 1000.000000000000000 ) ;
#13043 = CARTESIAN_POINT ( 'NONE',  ( -16.94107738177415712, 10.01423928514777728, -146.5500000000000114 ) ) ;
#13046 = CARTESIAN_POINT ( 'NONE',  ( -16.87036670365548474, 66.01058118070987746, -48.54354736722234520 ) ) ;
#13045 = DIRECTION ( 'NONE',  ( -1.000000000000000000, 0.000000000000000000, 0.000000000000000000 ) ) ;
#13047 = SPHERICAL_SURFACE ( 'NONE', #107630, 0.1000000000000000056 ) ;
#13048 = DIRECTION ( 'NONE',  ( -0.000000000000000000, 1.000000000000000000, -0.000000000000000000 ) ) ;
#13050 = ADVANCED_FACE ( 'NONE', ( #230939 ), #101291, .F. ) ;
#13049 = CARTESIAN_POINT ( 'NONE',  ( 21.14999999999999858, 65.28660755661196902, -90.77310748452438816 ) ) ;
#13052 = ORIENTED_EDGE ( 'NONE', *, *, #119274, .T. ) ;
#13051 = DIRECTION ( 'NONE',  ( 0.000000000000000000, -6.688090509790120484E-15, 1.000000000000000000 ) ) ;
#13053 = AXIS2_PLACEMENT_3D ( 'NONE', #105099, #244638, #67293 ) ;
#13054 = AXIS2_PLACEMENT_3D ( 'NONE', #140867, #101695, #82139 ) ;
#13055 = VECTOR ( 'NONE', #77517, 1000.000000000000227 ) ;
#13056 = AXIS2_PLACEMENT_3D ( 'NONE', #106764, #186326, #87193 ) ;
#13058 = ORIENTED_EDGE ( 'NONE', *, *, #175695, .T. ) ;
#13057 = ORIENTED_EDGE ( 'NONE', *, *, #227183, .T. ) ;
#13059 = ORIENTED_EDGE ( 'NONE', *, *, #13784, .T. ) ;
#13060 = CARTESIAN_POINT ( 'NONE',  ( 20.94999999999999574, 8.926614585098251453, -175.9716830192230930 ) ) ;
#13062 = CARTESIAN_POINT ( 'NONE',  ( 21.93642651522410603, 7.327166239325793029, -1.462266042833915125E-16 ) ) ;
#13061 = CARTESIAN_POINT ( 'NONE',  ( -16.81453563122428108, 66.06089979457560446, -182.7348488238791901 ) ) ;
#13063 = DIRECTION ( 'NONE',  ( -0.000000000000000000, 0.1298341882519735979, 0.9915357197604890427 ) ) ;
#13064 = ORIENTED_EDGE ( 'NONE', *, *, #56105, .T. ) ;
#13065 = DIRECTION ( 'NONE',  ( 0.000000000000000000, -6.982962677686267499E-15, 1.000000000000000000 ) ) ;
#13066 = EDGE_LOOP ( 'NONE', ( #3740, #247955, #119586, #220087 ) ) ;
#13067 = ORIENTED_EDGE ( 'NONE', *, *, #198514, .T. ) ;
#13068 = CARTESIAN_POINT ( 'NONE',  ( 20.85000000000000142, -11.74999999998883560, -64.00000000000000000 ) ) ;
#13069 = DIRECTION ( 'NONE',  ( -0.000000000000000000, 1.000000000000000000, 6.982962677686266711E-15 ) ) ;
#13070 = DIRECTION ( 'NONE',  ( 2.978066053179066765E-16, -0.4721928772777322925, -0.8814952561688443877 ) ) ;
#13071 = CARTESIAN_POINT ( 'NONE',  ( -23.15000000000000213, 1.115625160336667635E-11, -136.0000000000000284 ) ) ;
#13072 = DIRECTION ( 'NONE',  ( 0.000000000000000000, 0.000000000000000000, 1.000000000000000000 ) ) ;
#13073 = VERTEX_POINT ( 'NONE', #28918 ) ;
#13074 = EDGE_LOOP ( 'NONE', ( #91816, #201390, #55241, #223903 ) ) ;
#13075 = DIRECTION ( 'NONE',  ( 0.000000000000000000, 0.000000000000000000, 1.000000000000000000 ) ) ;
#13076 = CARTESIAN_POINT ( 'NONE',  ( -16.94878442675511820, 9.991729103002159107, -54.38821957563787635 ) ) ;
#13077 = DIRECTION ( 'NONE',  ( 0.000000000000000000, 1.000000000000000000, 0.000000000000000000 ) ) ;
#13078 = FACE_OUTER_BOUND ( 'NONE', #21071, .T. ) ;
#13079 = DIRECTION ( 'NONE',  ( 0.000000000000000000, -0.9910465087640866200, -0.1335171055202867274 ) ) ;
#13080 = CARTESIAN_POINT ( 'NONE',  ( -16.92989507731676113, 9.950000000011138823, -188.1174989306101395 ) ) ;
#13081 = ORIENTED_EDGE ( 'NONE', *, *, #157752, .T. ) ;
#13082 = DIRECTION ( 'NONE',  ( 0.000000000000000000, 0.8814952561688437216, -0.4721928772777334582 ) ) ;
#13083 = VECTOR ( 'NONE', #54298, 1000.000000000000000 ) ;
#13084 = DIRECTION ( 'NONE',  ( 0.000000000000000000, -6.853228547068871147E-15, 1.000000000000000000 ) ) ;
#13085 = DIRECTION ( 'NONE',  ( -0.000000000000000000, 1.000000000000000000, 6.982962677686266711E-15 ) ) ;
#13086 = DIRECTION ( 'NONE',  ( 0.000000000000000000, 1.000000000000000000, 0.000000000000000000 ) ) ;
#13087 = DIRECTION ( 'NONE',  ( -1.000000000000000000, 0.000000000000000000, 0.000000000000000000 ) ) ;
#13088 = LINE ( 'NONE', #15668, #128748 ) ;
#13089 = FACE_OUTER_BOUND ( 'NONE', #225380, .T. ) ;
#13091 = ORIENTED_EDGE ( 'NONE', *, *, #169488, .F. ) ;
#13090 = DIRECTION ( 'NONE',  ( 0.000000000000000000, -1.000000000000000000, -6.352154140967427193E-15 ) ) ;
#13092 = DIRECTION ( 'NONE',  ( 1.000000000000000000, -0.000000000000000000, 0.000000000000000000 ) ) ;
#13093 = ADVANCED_FACE ( 'NONE', ( #211361 ), #70591, .F. ) ;
#13094 = CARTESIAN_POINT ( 'NONE',  ( 21.00000000000000000, 14.02742277431099538, -219.5907614236512870 ) ) ;
#13095 = ADVANCED_FACE ( 'NONE', ( #11894 ), #30171, .F. ) ;
#13096 = ADVANCED_FACE ( 'NONE', ( #108409 ), #55517, .T. ) ;
#13097 = DIRECTION ( 'NONE',  ( 1.000000000000000000, 0.000000000000000000, 0.000000000000000000 ) ) ;
#13098 = CARTESIAN_POINT ( 'NONE',  ( 15.66039659514495774, 9.360749169926259938, -84.31457014060728739 ) ) ;
#13099 = FACE_OUTER_BOUND ( 'NONE', #180748, .T. ) ;
#13100 = CIRCLE ( 'NONE', #71361, 0.1000000000000124678 ) ;
#13101 = PLANE ( 'NONE',  #189063 ) ;
#13102 = LINE ( 'NONE', #207449, #107642 ) ;
#13104 = DIRECTION ( 'NONE',  ( 0.000000000000000000, -0.2617529984165031243, -0.9651348961777157509 ) ) ;
#13103 = AXIS2_PLACEMENT_3D ( 'NONE', #236664, #80129, #181847 ) ;
#13105 = ORIENTED_EDGE ( 'NONE', *, *, #174275, .F. ) ;
#13106 = DIRECTION ( 'NONE',  ( -1.000000000000000000, 0.000000000000000000, 0.000000000000000000 ) ) ;
#13108 = ORIENTED_EDGE ( 'NONE', *, *, #164199, .T. ) ;
#13107 = DIRECTION ( 'NONE',  ( 0.000000000000000000, 0.000000000000000000, 1.000000000000000000 ) ) ;
#13109 = CARTESIAN_POINT ( 'NONE',  ( -18.59999999999999787, -1.249999999988843369, -142.0000000000000284 ) ) ;
#13110 = EDGE_CURVE ( 'NONE', #176594, #85588, #156219, .T. ) ;
#13111 = VERTEX_POINT ( 'NONE', #58342 ) ;
#13112 = DIRECTION ( 'NONE',  ( 0.000000000000000000, 0.000000000000000000, -1.000000000000000000 ) ) ;
#13113 = APPLICATION_PROTOCOL_DEFINITION ( 'draft international standard', 'automotive_design', 1998, #100702 ) ;
#13114 = CARTESIAN_POINT ( 'NONE',  ( 22.48660254037843842, 11.37252324248628632, -198.4720136275361710 ) ) ;
#13115 = CARTESIAN_POINT ( 'NONE',  ( -22.48660254037843487, 11.65000000001115588, -33.45000000000002416 ) ) ;
#13116 = EDGE_LOOP ( 'NONE', ( #75548, #222357, #1869, #171818, #134555, #54438, #55987, #148, #18985, #180811, #151187, #125310 ) ) ;
#13117 = DIRECTION ( 'NONE',  ( 0.000000000000000000, 0.000000000000000000, 1.000000000000000000 ) ) ;
#13118 = CARTESIAN_POINT ( 'NONE',  ( 20.94999999999999929, -11.48912529306489994, -198.0999999999999659 ) ) ;
#13119 = CARTESIAN_POINT ( 'NONE',  ( -23.15000000000000213, -8.999999999988844479, -191.1060308773475356 ) ) ;
#13120 = EDGE_CURVE ( 'NONE', #21635, #149328, #34738, .T. ) ;
#13121 = ORIENTED_EDGE ( 'NONE', *, *, #248982, .F. ) ;
#13122 = ADVANCED_FACE ( 'NONE', ( #9297 ), #50966, .T. ) ;
#13123 = VERTEX_POINT ( 'NONE', #151399 ) ;
#13124 = DIRECTION ( 'NONE',  ( 0.000000000000000000, 0.000000000000000000, 1.000000000000000000 ) ) ;
#13125 = CARTESIAN_POINT ( 'NONE',  ( -22.59999999999999787, 75.90000000001245439, -181.6726782920691505 ) ) ;
#13126 = CARTESIAN_POINT ( 'NONE',  ( 20.94999999999999929, 20.93186404871370598, -233.6960508434578401 ) ) ;
#13128 = CARTESIAN_POINT ( 'NONE',  ( -21.14999999999999858, 69.45934304831071415, -103.0231074845243597 ) ) ;
#13127 = VECTOR ( 'NONE', #129671, 1000.000000000000000 ) ;
#13129 = CIRCLE ( 'NONE', #33831, 0.1000000000000033362 ) ;
#13130 = EDGE_CURVE ( 'NONE', #224814, #153656, #217852, .T. ) ;
#13133 = CARTESIAN_POINT ( 'NONE',  ( 22.49066049874202022, -2.424081457535128159, -189.6048348505414083 ) ) ;
#13132 = CIRCLE ( 'NONE', #204641, 0.1000000000000002554 ) ;
#13131 = FACE_OUTER_BOUND ( 'NONE', #77065, .T. ) ;
#13134 = DIRECTION ( 'NONE',  ( 0.000000000000000000, -6.938893903907222067E-15, 1.000000000000000000 ) ) ;
#13135 = CARTESIAN_POINT ( 'NONE',  ( -23.15000000000000213, 7.128833340094563376, -233.7327013124401276 ) ) ;
#13136 = CARTESIAN_POINT ( 'NONE',  ( -22.39999999999999858, 1.115600667400684642E-11, -33.39999999999999858 ) ) ;
#13137 = DIRECTION ( 'NONE',  ( 1.000000000000000000, 0.000000000000000000, 0.000000000000000000 ) ) ;
#13138 = ORIENTED_EDGE ( 'NONE', *, *, #182288, .F. ) ;
#13140 = VERTEX_POINT ( 'NONE', #228357 ) ;
#13139 = DIRECTION ( 'NONE',  ( 0.000000000000000000, -0.9770955615653316162, -0.2128009952263604232 ) ) ;
#13141 = CARTESIAN_POINT ( 'NONE',  ( -18.59999999999999787, 9.150000000000002132, 11.75000000000000000 ) ) ;
#13142 = CARTESIAN_POINT ( 'NONE',  ( -23.15000000000000213, 87.65000000001144542, -39.12310748452424747 ) ) ;
#13144 = CARTESIAN_POINT ( 'NONE',  ( 21.05000000000000071, 76.00000000001126921, -203.5231074845248997 ) ) ;
#13143 = CARTESIAN_POINT ( 'NONE',  ( 20.94999999999999929, 53.86595165227826243, -236.3638196928718855 ) ) ;
#13145 = ORIENTED_EDGE ( 'NONE', *, *, #94052, .F. ) ;
#13146 = LINE ( 'NONE', #153981, #101631 ) ;
#13147 = CARTESIAN_POINT ( 'NONE',  ( 19.99999999738052736, 64.25000000001196554, -111.8359355348916893 ) ) ;
#13148 = CYLINDRICAL_SURFACE ( 'NONE', #232670, 0.09999999999999939493 ) ;
#13149 = CARTESIAN_POINT ( 'NONE',  ( 15.66039659514496130, 12.83090422469976488, -215.9260128953783351 ) ) ;
#13150 = ORIENTED_EDGE ( 'NONE', *, *, #180459, .T. ) ;
#13152 = VERTEX_POINT ( 'NONE', #37542 ) ;
#13151 = VECTOR ( 'NONE', #45502, 1000.000000000000000 ) ;
#13153 = EDGE_CURVE ( 'NONE', #71883, #191690, #122205, .T. ) ;
#13154 = DIRECTION ( 'NONE',  ( 0.000000000000000000, -0.7203564749500614983, 0.6936040289657504632 ) ) ;
#13155 = ORIENTED_EDGE ( 'NONE', *, *, #223882, .F. ) ;
#13156 = LINE ( 'NONE', #90095, #67961 ) ;
#13157 = LINE ( 'NONE', #129251, #52045 ) ;
#13158 = CARTESIAN_POINT ( 'NONE',  ( 21.05000000000000071, 8.876614585098257848, -142.3850804788446851 ) ) ;
#13159 = EDGE_CURVE ( 'NONE', #205114, #30110, #88858, .T. ) ;
#13160 = ADVANCED_FACE ( 'NONE', ( #16697 ), #64977, .T. ) ;
#13161 = ORIENTED_EDGE ( 'NONE', *, *, #223629, .F. ) ;
#13162 = CARTESIAN_POINT ( 'NONE',  ( 20.94999999999999574, 36.09166453643263850, -236.0643439437599511 ) ) ;
#13163 = AXIS2_PLACEMENT_3D ( 'NONE', #125874, #123328, #82867 ) ;
#13164 = EDGE_CURVE ( 'NONE', #9191, #63552, #188840, .T. ) ;
#13166 = ADVANCED_FACE ( 'NONE', ( #170994 ), #220008, .T. ) ;
#13165 = CARTESIAN_POINT ( 'NONE',  ( -21.65000000000000213, 68.29142135624991283, -191.1731074845243938 ) ) ;
#13167 = VECTOR ( 'NONE', #238833, 1000.000000000000000 ) ;
#13168 = CARTESIAN_POINT ( 'NONE',  ( -20.94999999999999929, 0.000000000000000000, 0.000000000000000000 ) ) ;
#13169 = CARTESIAN_POINT ( 'NONE',  ( 23.24999999999999289, 10.99842653345846699, -220.2504445088529792 ) ) ;
#13171 = CARTESIAN_POINT ( 'NONE',  ( 23.15000000000000213, -11.48912529306489994, -130.9000000000000341 ) ) ;
#13170 = LINE ( 'NONE', #228366, #220567 ) ;
#13173 = DIRECTION ( 'NONE',  ( 1.000000000000000000, 0.000000000000000000, 0.000000000000000000 ) ) ;
#13172 = AXIS2_PLACEMENT_3D ( 'NONE', #20296, #59364, #18984 ) ;
#13174 = ORIENTED_EDGE ( 'NONE', *, *, #169537, .T. ) ;
#13176 = CARTESIAN_POINT ( 'NONE',  ( -20.64999999999999858, 1.115600667400684642E-11, -200.9999999999999432 ) ) ;
#13175 = DIRECTION ( 'NONE',  ( -2.840903330521632269E-16, 0.9550021345545507412, -0.2965989261549202838 ) ) ;
#13177 = ORIENTED_EDGE ( 'NONE', *, *, #235593, .F. ) ;
#13179 = ORIENTED_EDGE ( 'NONE', *, *, #51733, .F. ) ;
#13178 = CARTESIAN_POINT ( 'NONE',  ( 18.59999999999998721, 69.15387683765879956, -32.28538121767450519 ) ) ;
#13180 = ADVANCED_FACE ( 'NONE', ( #62226 ), #255429, .T. ) ;
#13181 = ORIENTED_EDGE ( 'NONE', *, *, #247520, .T. ) ;
#13182 = CARTESIAN_POINT ( 'NONE',  ( -16.89318236219976299, 9.951535257886295227, -146.6448703678941285 ) ) ;
#13184 = ADVANCED_FACE ( 'NONE', ( #222555 ), #178347, .F. ) ;
#13183 = VECTOR ( 'NONE', #103183, 1000.000000000000000 ) ;
#13185 = DIRECTION ( 'NONE',  ( -0.000000000000000000, -0.000000000000000000, -1.000000000000000000 ) ) ;
#13186 = FACE_OUTER_BOUND ( 'NONE', #198283, .T. ) ;
#13187 = CARTESIAN_POINT ( 'NONE',  ( 21.04999999999999716, 65.45624872451648457, -128.9667196758603041 ) ) ;
#13188 = AXIS2_PLACEMENT_3D ( 'NONE', #16948, #217673, #93896 ) ;
#13189 = ORIENTED_EDGE ( 'NONE', *, *, #216933, .F. ) ;
#13190 = DIRECTION ( 'NONE',  ( 0.000000000000000000, -1.000000000000000000, -0.000000000000000000 ) ) ;
#13192 = EDGE_CURVE ( 'NONE', #148530, #113184, #151266, .T. ) ;
#13191 = FACE_OUTER_BOUND ( 'NONE', #141931, .T. ) ;
#13193 = ORIENTED_EDGE ( 'NONE', *, *, #4198, .T. ) ;
#13194 = TOROIDAL_SURFACE ( 'NONE', #196321, 0.2000000000000000111, 0.1000000000000000056 ) ;
#13195 = LINE ( 'NONE', #151430, #81613 ) ;
#13196 = EDGE_CURVE ( 'NONE', #41142, #14901, #101494, .T. ) ;
#13197 = DIRECTION ( 'NONE',  ( 0.000000000000000000, 1.000000000000000000, -1.224646799147353207E-16 ) ) ;
#13198 = AXIS2_PLACEMENT_3D ( 'NONE', #104241, #125128, #67704 ) ;
#13199 = VERTEX_POINT ( 'NONE', #2227 ) ;
#13200 = EDGE_CURVE ( 'NONE', #197466, #94008, #64133, .T. ) ;
#13202 = EDGE_CURVE ( 'NONE', #89853, #18191, #174513, .T. ) ;
#13201 = CIRCLE ( 'NONE', #121551, 0.1000000000000002554 ) ;
#13203 = EDGE_LOOP ( 'NONE', ( #198259, #227829, #188806, #145960, #121496 ) ) ;
#13204 = CARTESIAN_POINT ( 'NONE',  ( 18.46858270002952906, -9.474202674699409243, -141.1020219347038847 ) ) ;
#13205 = ORIENTED_EDGE ( 'NONE', *, *, #248751, .F. ) ;
#13206 = DIRECTION ( 'NONE',  ( 0.000000000000000000, 0.8700118002898321601, -0.4930308989875230030 ) ) ;
#13207 = VECTOR ( 'NONE', #248058, 1000.000000000000000 ) ;
#13208 = EDGE_CURVE ( 'NONE', #97170, #46680, #23118, .T. ) ;
#13209 = DIRECTION ( 'NONE',  ( 0.000000000000000000, 0.000000000000000000, 1.000000000000000000 ) ) ;
#13210 = DIRECTION ( 'NONE',  ( 1.000000000000000000, -0.000000000000000000, 0.000000000000000000 ) ) ;
#13211 = AXIS2_PLACEMENT_3D ( 'NONE', #85019, #203720, #2932 ) ;
#13212 = DIRECTION ( 'NONE',  ( 0.000000000000000000, 0.000000000000000000, -1.000000000000000000 ) ) ;
#13213 = EDGE_CURVE ( 'NONE', #134581, #203424, #102593, .T. ) ;
#13214 = EDGE_CURVE ( 'NONE', #178378, #154754, #162617, .T. ) ;
#13215 = ADVANCED_FACE ( 'NONE', ( #4784 ), #240867, .T. ) ;
#13216 = DIRECTION ( 'NONE',  ( 0.000000000000000000, 0.000000000000000000, -1.000000000000000000 ) ) ;
#13217 = CARTESIAN_POINT ( 'NONE',  ( 21.98333005346336932, 76.00000000001200817, -110.3971828135809830 ) ) ;
#13218 = DIRECTION ( 'NONE',  ( -0.5932847527679310229, 0.8049926720990042694, -6.366092712777067056E-16 ) ) ;
#13219 = CIRCLE ( 'NONE', #29814, 0.09999999999999939493 ) ;
#13220 = ORIENTED_EDGE ( 'NONE', *, *, #179587, .F. ) ;
#13221 = DIRECTION ( 'NONE',  ( 0.000000000000000000, 1.000000000000000000, 0.000000000000000000 ) ) ;
#13222 = AXIS2_PLACEMENT_3D ( 'NONE', #161628, #241153, #187601 ) ;
#13223 = ORIENTED_EDGE ( 'NONE', *, *, #78836, .F. ) ;
#13227 = VERTEX_POINT ( 'NONE', #163897 ) ;
#13226 =( BOUNDED_SURFACE ( )  B_SPLINE_SURFACE ( 3, 2, ( 
 ( #69361, #133174, #90168 ),
 ( #129318, #109736, #193158 ),
 ( #14534, #151473, #211424 ),
 ( #189301, #169770, #150181 ) ),
 .UNSPECIFIED., .F., .F., .T. ) 
 B_SPLINE_SURFACE_WITH_KNOTS ( ( 4, 4 ),
 ( 3, 3 ),
 ( 0.0008258556059633759532, 0.0009616864997632701634 ),
 ( 0.000000000000000000, 1.000000000000000000 ),
 .UNSPECIFIED. ) 
 GEOMETRIC_REPRESENTATION_ITEM ( )  RATIONAL_B_SPLINE_SURFACE ( (
 ( 1.000000000000000000, 0.9152888060719485130, 1.000000000000000000),
 ( 1.000000000000000000, 0.9327727094138390518, 1.000000000000000000),
 ( 1.000000000000000000, 0.9369023509257937699, 1.000000000000000000),
 ( 1.000000000000000000, 0.9246339933864583527, 1.000000000000000000) ) ) 
 REPRESENTATION_ITEM ( '' )  SURFACE ( )  );
#13225 = DIRECTION ( 'NONE',  ( 0.000000000000000000, 0.9908441862701420355, 0.1350103645453197554 ) ) ;
#13224 = CARTESIAN_POINT ( 'NONE',  ( -13.39999999999994351, 66.35000000001119247, -23.62310748452479103 ) ) ;
#13228 = CIRCLE ( 'NONE', #100658, 0.6000000000000015321 ) ;
#13229 = ORIENTED_EDGE ( 'NONE', *, *, #54044, .F. ) ;
#13230 = DIRECTION ( 'NONE',  ( -1.000000000000000000, 0.000000000000000000, 0.000000000000000000 ) ) ;
#13231 = CIRCLE ( 'NONE', #72048, 0.5000000000000004441 ) ;
#13232 = LINE ( 'NONE', #73219, #134775 ) ;
#13233 = LINE ( 'NONE', #189292, #239421 ) ;
#13234 = CARTESIAN_POINT ( 'NONE',  ( 20.94999999999999574, 14.83422855357708414, -203.3235740904736417 ) ) ;
#13235 = ORIENTED_EDGE ( 'NONE', *, *, #45099, .T. ) ;
#13237 = EDGE_LOOP ( 'NONE', ( #236838, #214454, #160225, #164478, #113729 ) ) ;
#13236 = FACE_OUTER_BOUND ( 'NONE', #12515, .T. ) ;
#13238 = ADVANCED_FACE ( 'NONE', ( #38820 ), #98738, .F. ) ;
#13240 = FACE_OUTER_BOUND ( 'NONE', #158831, .T. ) ;
#13239 = CARTESIAN_POINT ( 'NONE',  ( 21.15000000000005187, 82.84256550613280012, -26.34830530078816935 ) ) ;
#13242 = VERTEX_POINT ( 'NONE', #119645 ) ;
#13241 = CARTESIAN_POINT ( 'NONE',  ( -18.50000000000000000, 18.18127959618848166, -237.5711165786817389 ) ) ;
#13243 = ORIENTED_EDGE ( 'NONE', *, *, #101678, .F. ) ;
#13244 = AXIS2_PLACEMENT_3D ( 'NONE', #82882, #209280, #188433 ) ;
#13245 = FACE_OUTER_BOUND ( 'NONE', #163392, .T. ) ;
#13246 = CARTESIAN_POINT ( 'NONE',  ( -18.40000000000000213, 5.650000000011139001, -154.8500000000000227 ) ) ;
#13247 = ORIENTED_EDGE ( 'NONE', *, *, #190321, .T. ) ;
#13248 = DIRECTION ( 'NONE',  ( 0.000000000000000000, -0.5868805631290353597, -0.8096735173027127530 ) ) ;
#13249 = EDGE_LOOP ( 'NONE', ( #88311, #232927, #40668, #50470 ) ) ;
#13250 = CARTESIAN_POINT ( 'NONE',  ( -18.44448725179913851, -9.490081715472175716, -107.1289602940625372 ) ) ;
#13251 = CARTESIAN_POINT ( 'NONE',  ( -23.25000000000000000, -11.74999999998884448, -134.0000000000000284 ) ) ;
#13252 = EDGE_LOOP ( 'NONE', ( #218592, #215534, #95883, #132333 ) ) ;
#13253 = CARTESIAN_POINT ( 'NONE',  ( 18.59999999999999076, -1.249999999999999334, -7.999999999999998224 ) ) ;
#13254 = ADVANCED_FACE ( 'NONE', ( #199167 ), #20552, .F. ) ;
#13256 = EDGE_CURVE ( 'NONE', #127698, #177453, #22461, .T. ) ;
#13255 = CARTESIAN_POINT ( 'NONE',  ( 21.07971444708685738, 6.166122833947518700, -199.5672020556278028 ) ) ;
#13258 = ORIENTED_EDGE ( 'NONE', *, *, #85587, .F. ) ;
#13257 = AXIS2_PLACEMENT_3D ( 'NONE', #237295, #252991, #92627 ) ;
#13259 = ORIENTED_EDGE ( 'NONE', *, *, #253384, .T. ) ;
#13260 = CARTESIAN_POINT ( 'NONE',  ( 20.21567752745113111, 18.89280262299452318, -228.4652292927793269 ) ) ;
#13261 = ORIENTED_EDGE ( 'NONE', *, *, #104862, .T. ) ;
#13262 = EDGE_CURVE ( 'NONE', #131609, #40304, #68221, .T. ) ;
#13263 = CARTESIAN_POINT ( 'NONE',  ( 20.94999999999999929, 71.00000000001180922, -81.92837350343744163 ) ) ;
#13264 = ORIENTED_EDGE ( 'NONE', *, *, #147746, .F. ) ;
#13267 = EDGE_CURVE ( 'NONE', #231005, #97895, #26539, .T. ) ;
#13266 = ORIENTED_EDGE ( 'NONE', *, *, #194452, .T. ) ;
#13265 = CARTESIAN_POINT ( 'NONE',  ( 21.40925344232283223, 75.90104981139234042, -109.6816263439147576 ) ) ;
#13268 =( BOUNDED_SURFACE ( )  B_SPLINE_SURFACE ( 3, 2, ( 
 ( #30466, #129555, #212940 ),
 ( #34329, #72159, #68297 ),
 ( #48716, #188238, #91708 ),
 ( #252059, #128271, #190840 ) ),
 .UNSPECIFIED., .F., .F., .F. ) 
 B_SPLINE_SURFACE_WITH_KNOTS ( ( 4, 4 ),
 ( 3, 3 ),
 ( 4.712388980384689674, 5.765869716888531116 ),
 ( 0.000000000000000000, 1.000000000000000000 ),
 .UNSPECIFIED. ) 
 GEOMETRIC_REPRESENTATION_ITEM ( )  RATIONAL_B_SPLINE_SURFACE ( (
 ( 1.000000000000000000, 0.7071067811865475727, 1.000000000000000000),
 ( 1.000000000000000000, 0.7953136715913721178, 1.000000000000000000),
 ( 1.000000000000000000, 0.8646876308615152329, 1.000000000000000000),
 ( 1.000000000000000000, 0.8984936768950676500, 1.000000000000000000) ) ) 
 REPRESENTATION_ITEM ( '' )  SURFACE ( )  );
#13269 = VERTEX_POINT ( 'NONE', #247260 ) ;
#13270 = DIRECTION ( 'NONE',  ( 0.000000000000000000, -0.2128009952263485993, 0.9770955615653341697 ) ) ;
#13271 = ORIENTED_EDGE ( 'NONE', *, *, #23112, .T. ) ;
#13273 = ORIENTED_EDGE ( 'NONE', *, *, #122809, .T. ) ;
#13272 = ORIENTED_EDGE ( 'NONE', *, *, #229152, .T. ) ;
#13274 = VECTOR ( 'NONE', #235965, 1000.000000000000000 ) ;
#13275 = ORIENTED_EDGE ( 'NONE', *, *, #229800, .F. ) ;
#13276 = AXIS2_PLACEMENT_3D ( 'NONE', #211867, #71074, #150598 ) ;
#13277 = AXIS2_PLACEMENT_3D ( 'NONE', #18618, #177721, #254629 ) ;
#13278 = CARTESIAN_POINT ( 'NONE',  ( 21.05543885634738643, 8.775771046858691804, -45.68438447071469000 ) ) ;
#13279 = ORIENTED_EDGE ( 'NONE', *, *, #60657, .T. ) ;
#13280 = CARTESIAN_POINT ( 'NONE',  ( -16.93294127766158752, 10.00328010296601988, -154.9299072658292573 ) ) ;
#13282 = ORIENTED_EDGE ( 'NONE', *, *, #247520, .F. ) ;
#13281 = FACE_OUTER_BOUND ( 'NONE', #90176, .T. ) ;
#13283 = DIRECTION ( 'NONE',  ( -1.000000000000000000, -0.000000000000000000, -0.000000000000000000 ) ) ;
#13284 = EDGE_LOOP ( 'NONE', ( #28475, #250576, #238204, #188342, #176312 ) ) ;
#13285 = CARTESIAN_POINT ( 'NONE',  ( -21.08621493067320429, 0.05619483948720607747, -161.1507057088280419 ) ) ;
#13286 = VERTEX_POINT ( 'NONE', #244691 ) ;
#13287 = DIRECTION ( 'NONE',  ( 0.000000000000000000, -0.9550021345545530727, 0.2965989261549131228 ) ) ;
#13288 = CARTESIAN_POINT ( 'NONE',  ( 18.57399277249656322, 18.41291479239798790, -236.9963116028434058 ) ) ;
#13289 = VECTOR ( 'NONE', #57030, 1000.000000000000000 ) ;
#13290 = VERTEX_POINT ( 'NONE', #245999 ) ;
#13292 = ORIENTED_EDGE ( 'NONE', *, *, #198169, .T. ) ;
#13291 = FACE_OUTER_BOUND ( 'NONE', #187765, .T. ) ;
#13293 = DIRECTION ( 'NONE',  ( -0.000000000000000000, -0.8660254037844459241, -0.4999999999999873990 ) ) ;
#13294 = ADVANCED_FACE ( 'NONE', ( #29546 ), #11238, .T. ) ;
#13296 = EDGE_LOOP ( 'NONE', ( #196236, #110209, #202151, #58024 ) ) ;
#13295 = EDGE_LOOP ( 'NONE', ( #252546, #212376, #100208, #53276 ) ) ;
#13297 = EDGE_LOOP ( 'NONE', ( #120657, #78355, #68704, #47370 ) ) ;
#13298 = DIRECTION ( 'NONE',  ( 0.000000000000000000, 0.000000000000000000, 1.000000000000000000 ) ) ;
#13299 = VERTEX_POINT ( 'NONE', #124770 ) ;
#13300 = ORIENTED_EDGE ( 'NONE', *, *, #221020, .T. ) ;
#13301 = CARTESIAN_POINT ( 'NONE',  ( 20.85000000000000142, -1.835859311432481045, -78.50443916879852679 ) ) ;
#13302 = ORIENTED_EDGE ( 'NONE', *, *, #36304, .F. ) ;
#13303 = CARTESIAN_POINT ( 'NONE',  ( -23.25000000000000000, 2.000000000011154189, -120.7753780772379315 ) ) ;
#13304 = DIRECTION ( 'NONE',  ( -1.020425574104004196E-15, 0.000000000000000000, -1.000000000000000000 ) ) ;
#13305 = EDGE_CURVE ( 'NONE', #172414, #89589, #69946, .T. ) ;
#13306 = ORIENTED_EDGE ( 'NONE', *, *, #237566, .F. ) ;
#13307 = AXIS2_PLACEMENT_3D ( 'NONE', #179032, #219385, #159443 ) ;
#13308 = AXIS2_PLACEMENT_3D ( 'NONE', #132425, #15056, #172879 ) ;
#13309 = EDGE_CURVE ( 'NONE', #43158, #70322, #51430, .T. ) ;
#13310 = ORIENTED_EDGE ( 'NONE', *, *, #181262, .T. ) ;
#13311 = CIRCLE ( 'NONE', #46592, 0.09999999999999993616 ) ;
#13312 = DIRECTION ( 'NONE',  ( 0.000000000000000000, -0.1335171055202870327, 0.9910465087640865089 ) ) ;
#13313 = VERTEX_POINT ( 'NONE', #165172 ) ;
#13314 = EDGE_CURVE ( 'NONE', #136330, #46709, #9948, .T. ) ;
#13315 = DIRECTION ( 'NONE',  ( -1.000000000000000000, -0.000000000000000000, -0.000000000000000000 ) ) ;
#13316 = VERTEX_POINT ( 'NONE', #169065 ) ;
#13317 = ORIENTED_EDGE ( 'NONE', *, *, #83640, .F. ) ;
#13318 = FACE_OUTER_BOUND ( 'NONE', #186627, .T. ) ;
#13321 = ADVANCED_FACE ( 'NONE', ( #46491 ), #248553, .T. ) ;
#13320 = ORIENTED_EDGE ( 'NONE', *, *, #227151, .T. ) ;
#13319 = CARTESIAN_POINT ( 'NONE',  ( 18.59999994388910238, 85.36356618708374810, -162.8419902477237144 ) ) ;
#13322 = CARTESIAN_POINT ( 'NONE',  ( 21.07946286933444568, 0.07668384326755511848, -127.6709626809923179 ) ) ;
#13323 = FACE_OUTER_BOUND ( 'NONE', #64912, .T. ) ;
#13324 = ADVANCED_FACE ( 'NONE', ( #7374 ), #149484, .F. ) ;
#13325 = CARTESIAN_POINT ( 'NONE',  ( 20.95561247346651967, 65.40499263480853642, -128.9293247175427268 ) ) ;
#13326 = CARTESIAN_POINT ( 'NONE',  ( 18.58143601961928582, 33.87351802927719291, -236.2204290509960458 ) ) ;
#13327 = AXIS2_PLACEMENT_3D ( 'NONE', #92014, #90722, #171589 ) ;
#13328 = FACE_OUTER_BOUND ( 'NONE', #184886, .T. ) ;
#13329 = DIRECTION ( 'NONE',  ( -2.952720810173289112E-16, 1.000000000000000000, 0.000000000000000000 ) ) ;
#13330 = CARTESIAN_POINT ( 'NONE',  ( -20.54999999999999716, -9.000000000000003553, -9.893969122652444881 ) ) ;
#13331 = CARTESIAN_POINT ( 'NONE',  ( 21.53551880898956838, 10.24532516527459158, -227.7052014679549927 ) ) ;
#13332 = CYLINDRICAL_SURFACE ( 'NONE', #227690, 0.09999999999998898659 ) ;
#13334 = EDGE_CURVE ( 'NONE', #212682, #162878, #333, .T. ) ;
#13333 = CARTESIAN_POINT ( 'NONE',  ( 22.49806830649814060, 75.92253568368671779, -148.1729971393633889 ) ) ;
#13335 = CARTESIAN_POINT ( 'NONE',  ( -21.52071067811865746, 68.22071067813051570, -90.67310748452436542 ) ) ;
#13336 = ORIENTED_EDGE ( 'NONE', *, *, #126090, .T. ) ;
#13338 = ORIENTED_EDGE ( 'NONE', *, *, #22075, .T. ) ;
#13337 = ORIENTED_EDGE ( 'NONE', *, *, #14973, .F. ) ;
#13339 = VERTEX_POINT ( 'NONE', #8667 ) ;
#13341 = EDGE_CURVE ( 'NONE', #83495, #109956, #9951, .T. ) ;
#13340 = CARTESIAN_POINT ( 'NONE',  ( 21.07928932188134397, 75.90110485435833709, -209.8516241409176928 ) ) ;
#13342 = AXIS2_PLACEMENT_3D ( 'NONE', #134185, #194195, #32571 ) ;
#13343 = LINE ( 'NONE', #212833, #73768 ) ;
#13345 = CARTESIAN_POINT ( 'NONE',  ( -20.94999999999999929, 5.900000000000005684, -23.28090023534362629 ) ) ;
#13344 = CARTESIAN_POINT ( 'NONE',  ( 21.05000000000000071, 74.63912941282028157, -161.9501095574334215 ) ) ;
#13346 = VERTEX_POINT ( 'NONE', #28266 ) ;
#13347 = VERTEX_POINT ( 'NONE', #107760 ) ;
#13348 = VECTOR ( 'NONE', #18195, 1000.000000000000000 ) ;
#13349 =( NAMED_UNIT ( * ) SI_UNIT ( $, .STERADIAN. ) SOLID_ANGLE_UNIT ( ) );
#13350 = AXIS2_PLACEMENT_3D ( 'NONE', #247675, #248973, #172030 ) ;
#13351 = DIRECTION ( 'NONE',  ( 0.000000000000000000, 0.000000000000000000, 1.000000000000000000 ) ) ;
#13352 = TOROIDAL_SURFACE ( 'NONE', #50733, 11.65000000000000036, 0.1000000000000000056 ) ;
#13353 = AXIS2_PLACEMENT_3D ( 'NONE', #66850, #87676, #248049 ) ;
#13354 = DIRECTION ( 'NONE',  ( -1.000000000000000000, 0.000000000000000000, 0.000000000000000000 ) ) ;
#13355 = ORIENTED_EDGE ( 'NONE', *, *, #50686, .F. ) ;
#13356 = ORIENTED_EDGE ( 'NONE', *, *, #10164, .F. ) ;
#13357 = DIRECTION ( 'NONE',  ( 0.000000000000000000, -0.9856811345164744331, -0.1686199900910800020 ) ) ;
#13358 = AXIS2_PLACEMENT_3D ( 'NONE', #128893, #88439, #247548 ) ;
#13359 = DIRECTION ( 'NONE',  ( 0.000000000000000000, 0.000000000000000000, 1.000000000000000000 ) ) ;
#13360 = VECTOR ( 'NONE', #74071, 1000.000000000000000 ) ;
#13361 = CARTESIAN_POINT ( 'NONE',  ( 21.05000000000000071, 5.000000000011153745, -112.9052660189131245 ) ) ;
#13363 = VERTEX_POINT ( 'NONE', #170358 ) ;
#13362 = CARTESIAN_POINT ( 'NONE',  ( 20.94999999999999929, -11.29603075033528548, -3.047899159663867152 ) ) ;
#13364 = CARTESIAN_POINT ( 'NONE',  ( 21.05000000000000071, 36.65892442174472876, -249.5511627012454596 ) ) ;
#13365 = DIRECTION ( 'NONE',  ( 0.000000000000000000, 1.000000000000000000, 6.982962677686266711E-15 ) ) ;
#13367 = CIRCLE ( 'NONE', #163211, 0.1000000000000028644 ) ;
#13366 = CARTESIAN_POINT ( 'NONE',  ( -18.59999999999999787, 14.83511725869332132, -235.8887435844146978 ) ) ;
#13368 = VERTEX_POINT ( 'NONE', #187320 ) ;
#13369 = CARTESIAN_POINT ( 'NONE',  ( 15.66039659514496130, 66.63925083009672790, -85.70853734391710077 ) ) ;
#13370 = DIRECTION ( 'NONE',  ( 0.000000000000000000, 0.8814952561688476074, -0.4721928772777262417 ) ) ;
#13371 = CARTESIAN_POINT ( 'NONE',  ( -20.85000000000000142, -11.74999999998884448, -134.0000000000000284 ) ) ;
#13372 = VECTOR ( 'NONE', #34567, 1000.000000000000000 ) ;
#13374 = CARTESIAN_POINT ( 'NONE',  ( -22.94999999999999929, 5.488301202077012775, 16.40000000000000213 ) ) ;
#13373 = CARTESIAN_POINT ( 'NONE',  ( -23.15000000000000213, 11.65000000001115588, -59.98519422934604961 ) ) ;
#13375 = CYLINDRICAL_SURFACE ( 'NONE', #162195, 0.09999999999999939493 ) ;
#13376 = CARTESIAN_POINT ( 'NONE',  ( -21.14999999999994174, 83.97335046823651794, -37.38386894789040582 ) ) ;
#13377 = B_SPLINE_CURVE_WITH_KNOTS ( 'NONE', 3,
 ( #82567, #46040, #205098, #206406, #81286, #240404, #141298, #123026 ),
 .UNSPECIFIED., .F., .F.,
 ( 4, 2, 2, 4 ),
 ( 0.000000000000000000, 0.0001881495939909292280, 0.0002822243909863938419, 0.0003762991879818584559 ),
 .UNSPECIFIED. ) ;
#13378 = DIRECTION ( 'NONE',  ( 1.000000000000000000, 0.000000000000000000, 0.000000000000000000 ) ) ;
#13379 = DIRECTION ( 'NONE',  ( 0.000000000000000000, 0.000000000000000000, -1.000000000000000000 ) ) ;
#13380 = CARTESIAN_POINT ( 'NONE',  ( -21.05000000000000071, 85.51932773110506503, -196.5501311079649724 ) ) ;
#13381 = AXIS2_PLACEMENT_3D ( 'NONE', #46553, #226469, #242198 ) ;
#13382 = ORIENTED_EDGE ( 'NONE', *, *, #11343, .T. ) ;
#13383 = ADVANCED_FACE ( 'NONE', ( #249847 ), #112905, .F. ) ;
#13384 = VERTEX_POINT ( 'NONE', #171627 ) ;
#13385 = CIRCLE ( 'NONE', #96555, 0.1000000000000013933 ) ;
#13386 = ORIENTED_EDGE ( 'NONE', *, *, #147687, .T. ) ;
#13387 = CARTESIAN_POINT ( 'NONE',  ( -21.37071067811865532, 21.73808232493841075, -232.4027708824187073 ) ) ;
#13388 = CARTESIAN_POINT ( 'NONE',  ( -23.15000000000000213, 71.65000000001155911, -57.27310748452435263 ) ) ;
#13389 = ORIENTED_EDGE ( 'NONE', *, *, #202066, .T. ) ;
#13391 = EDGE_CURVE ( 'NONE', #123588, #123054, #113993, .T. ) ;
#13390 = CIRCLE ( 'NONE', #146622, 0.09999999999999963085 ) ;
#13392 = CARTESIAN_POINT ( 'NONE',  ( -21.05000000000000071, 86.10439672154322466, -209.4215112426525138 ) ) ;
#13393 = ORIENTED_EDGE ( 'NONE', *, *, #158154, .T. ) ;
#13394 = EDGE_CURVE ( 'NONE', #209282, #152492, #222298, .T. ) ;
#13395 = EDGE_CURVE ( 'NONE', #120974, #205644, #126477, .T. ) ;
#13396 = ORIENTED_EDGE ( 'NONE', *, *, #149417, .T. ) ;
#13397 = CARTESIAN_POINT ( 'NONE',  ( 21.05000000000000071, 76.10000000001198828, -109.5637644362255543 ) ) ;
#13398 = CIRCLE ( 'NONE', #42421, 0.09999999999999939493 ) ;
#13399 = ORIENTED_EDGE ( 'NONE', *, *, #114358, .F. ) ;
#13400 = AXIS2_PLACEMENT_3D ( 'NONE', #125723, #104839, #248249 ) ;
#13402 = CARTESIAN_POINT ( 'NONE',  ( 18.60000000000000142, -7.567701079425715349, -210.0537230116848946 ) ) ;
#13401 = TOROIDAL_SURFACE ( 'NONE', #134178, 11.89999999999999858, 0.1000000000000000056 ) ;
#13403 = DIRECTION ( 'NONE',  ( 0.000000000000000000, 0.2617529984165083423, 0.9651348961777143076 ) ) ;
#13404 = DIRECTION ( 'NONE',  ( 0.000000000000000000, 0.9875055080513743810, -0.1575844902526802316 ) ) ;
#13405 = CARTESIAN_POINT ( 'NONE',  ( -20.94999999999999929, 74.25000000001186606, -91.35359592662267403 ) ) ;
#13406 = DIRECTION ( 'NONE',  ( 0.000000000000000000, -0.9876197685951265681, -0.1568667991644790149 ) ) ;
#13408 = ORIENTED_EDGE ( 'NONE', *, *, #183145, .T. ) ;
#13407 = DIRECTION ( 'NONE',  ( 6.938893903907030216E-14, 0.000000000000000000, 1.000000000000000000 ) ) ;
#13410 = FACE_OUTER_BOUND ( 'NONE', #208805, .T. ) ;
#13409 = CARTESIAN_POINT ( 'NONE',  ( 21.09096482362019387, 6.209396322289256531, -199.6072866877750300 ) ) ;
#13411 = EDGE_CURVE ( 'NONE', #93357, #218820, #230548, .T. ) ;
#13412 = CARTESIAN_POINT ( 'NONE',  ( -22.50000000000000000, 12.62988036037869755, -223.4632815780722694 ) ) ;
#13413 = CARTESIAN_POINT ( 'NONE',  ( -21.05000000000000071, 36.02918351690955490, -236.0543695120161374 ) ) ;
#13414 = CARTESIAN_POINT ( 'NONE',  ( -16.89021194854739250, 66.05000000001180638, -82.28053935292003018 ) ) ;
#13416 = EDGE_CURVE ( 'NONE', #62401, #76270, #92047, .T. ) ;
#13415 = CARTESIAN_POINT ( 'NONE',  ( -20.85000000000000142, 28.60154115857408641, -258.4512230915049713 ) ) ;
#13417 = VERTEX_POINT ( 'NONE', #133739 ) ;
#13418 = DIRECTION ( 'NONE',  ( 0.000000000000000000, 0.000000000000000000, -1.000000000000000000 ) ) ;
#13419 = PRODUCT_RELATED_PRODUCT_CATEGORY ( 'part', '', ( #70236 ) ) ;
#13420 = ORIENTED_EDGE ( 'NONE', *, *, #26719, .F. ) ;
#13421 = DIRECTION ( 'NONE',  ( 1.000000000000000000, -0.000000000000000000, -0.000000000000000000 ) ) ;
#13422 = VECTOR ( 'NONE', #102819, 1000.000000000000000 ) ;
#13423 = ORIENTED_EDGE ( 'NONE', *, *, #154756, .F. ) ;
#13424 = EDGE_CURVE ( 'NONE', #134210, #179995, #172324, .T. ) ;
#13425 = CARTESIAN_POINT ( 'NONE',  ( 20.73486653747088582, 7.250000000011182166, -46.15000000000000568 ) ) ;
#13426 = DIRECTION ( 'NONE',  ( 1.000000000000000000, -2.952720810173289112E-16, -2.061873921506763405E-30 ) ) ;
#13427 = ADVANCED_FACE ( 'NONE', ( #34672 ), #29986, .T. ) ;
#13428 = ORIENTED_EDGE ( 'NONE', *, *, #206863, .T. ) ;
#13429 = EDGE_CURVE ( 'NONE', #153815, #242609, #155734, .T. ) ;
#13430 = VERTEX_POINT ( 'NONE', #54200 ) ;
#13431 = LINE ( 'NONE', #172548, #31876 ) ;
#13432 = DIRECTION ( 'NONE',  ( -0.000000000000000000, 3.469446951953635015E-14, 1.000000000000000000 ) ) ;
#13433 = DIRECTION ( 'NONE',  ( 1.000000000000000000, 0.000000000000000000, 0.000000000000000000 ) ) ;
#13434 = DIRECTION ( 'NONE',  ( 1.000000000000000000, -1.335000415235278971E-16, 2.979993593738921214E-16 ) ) ;
#13436 = DIRECTION ( 'NONE',  ( 1.000000000000000000, 0.000000000000000000, -0.000000000000000000 ) ) ;
#13435 = FACE_OUTER_BOUND ( 'NONE', #237299, .T. ) ;
#13437 = DIRECTION ( 'NONE',  ( 1.000000000000000000, 0.000000000000000000, 0.000000000000000000 ) ) ;
#13438 = CARTESIAN_POINT ( 'NONE',  ( 12.60873083341396494, 9.389571634557560387, -51.31764071236915470 ) ) ;
#13439 = DIRECTION ( 'NONE',  ( 0.000000000000000000, -0.8814952561688430555, 0.4721928772777346239 ) ) ;
#13440 = ORIENTED_EDGE ( 'NONE', *, *, #136531, .T. ) ;
#13441 = DIRECTION ( 'NONE',  ( 0.000000000000000000, -0.1022405907414166287, -0.9947597004326452774 ) ) ;
#13442 = AXIS2_PLACEMENT_3D ( 'NONE', #217066, #38452, #117990 ) ;
#13444 = ORIENTED_EDGE ( 'NONE', *, *, #109609, .F. ) ;
#13443 = CARTESIAN_POINT ( 'NONE',  ( -18.34374000495060386, 64.52683809664961245, -127.2731074845243882 ) ) ;
#13445 = CARTESIAN_POINT ( 'NONE',  ( 16.87683809663749557, 9.950000000011131718, -188.3499999999999659 ) ) ;
#13446 = DIRECTION ( 'NONE',  ( -0.000000000000000000, 0.1350103645451626311, 0.9908441862701635738 ) ) ;
#13448 = CARTESIAN_POINT ( 'NONE',  ( -18.58735405345342784, -0.7666499927750894949, -242.4349016823527734 ) ) ;
#13447 = CARTESIAN_POINT ( 'NONE',  ( -20.94999999999999929, 74.95298800634525094, -207.3836470692357636 ) ) ;
#13449 = DIRECTION ( 'NONE',  ( 0.000000000000000000, 0.000000000000000000, 1.000000000000000000 ) ) ;
#13451 = ORIENTED_EDGE ( 'NONE', *, *, #181874, .T. ) ;
#13450 = CARTESIAN_POINT ( 'NONE',  ( 21.05000000000000071, -9.000000000000000000, -24.10603087734755690 ) ) ;
#13452 = CARTESIAN_POINT ( 'NONE',  ( -20.07928932188135107, 66.77928932189314537, -81.87310748452438247 ) ) ;
#13453 = CARTESIAN_POINT ( 'NONE',  ( 23.24999999999999289, 11.65000000001116298, -146.1500000000000341 ) ) ;
#13454 = DIRECTION ( 'NONE',  ( 0.000000000000000000, -0.5000000000000004441, -0.8660254037844384856 ) ) ;
#13455 = FACE_OUTER_BOUND ( 'NONE', #120093, .T. ) ;
#13456 = CARTESIAN_POINT ( 'NONE',  ( -18.47140463609787986, 85.67147468523276643, -96.35034702625016223 ) ) ;
#13457 = EDGE_LOOP ( 'NONE', ( #142674, #89468, #92268, #136773 ) ) ;
#13458 = DIRECTION ( 'NONE',  ( 1.000000000000000000, 0.000000000000000000, 0.000000000000000000 ) ) ;
#13459 = ORIENTED_EDGE ( 'NONE', *, *, #199176, .T. ) ;
#13460 = ADVANCED_FACE ( 'NONE', ( #73803 ), #135003, .F. ) ;
#13462 = CIRCLE ( 'NONE', #117685, 0.09999999999999982514 ) ;
#13461 = CARTESIAN_POINT ( 'NONE',  ( -21.05000000000000071, 14.05000000001115623, -106.0136950707610310 ) ) ;
#13463 = ORIENTED_EDGE ( 'NONE', *, *, #175310, .F. ) ;
#13464 = DIRECTION ( 'NONE',  ( 0.000000000000000000, -0.2617529984165853363, -0.9651348961776934354 ) ) ;
#13465 = EDGE_LOOP ( 'NONE', ( #198865, #48955, #17121, #240866 ) ) ;
#13466 = AXIS2_PLACEMENT_3D ( 'NONE', #246637, #27642, #83679 ) ;
#13467 = CYLINDRICAL_SURFACE ( 'NONE', #80904, 0.1000000000000064587 ) ;
#13468 = DIRECTION ( 'NONE',  ( 0.000000000000000000, 0.5378121776619166905, -0.8430646840892739302 ) ) ;
#13469 = AXIS2_PLACEMENT_3D ( 'NONE', #236899, #238170, #79088 ) ;
#13470 = ADVANCED_FACE ( 'NONE', ( #210718 ), #59819, .T. ) ;
#13471 = DIRECTION ( 'NONE',  ( 0.000000000000000000, -6.982962677686266711E-15, 1.000000000000000000 ) ) ;
#13472 = VERTEX_POINT ( 'NONE', #254917 ) ;
#13473 = EDGE_CURVE ( 'NONE', #38996, #153545, #164089, .T. ) ;
#13474 = CARTESIAN_POINT ( 'NONE',  ( -16.77431908686106610, 9.945805754517978770, -12.66416078234975373 ) ) ;
#13475 = DIRECTION ( 'NONE',  ( 1.000000000000000000, -0.000000000000000000, -0.000000000000000000 ) ) ;
#13476 = AXIS2_PLACEMENT_3D ( 'NONE', #208301, #165307, #45357 ) ;
#13477 = DIRECTION ( 'NONE',  ( -1.000000000000000000, 0.000000000000000000, -0.000000000000000000 ) ) ;
#13478 = VECTOR ( 'NONE', #179711, 1000.000000000000000 ) ;
#13479 = EDGE_CURVE ( 'NONE', #157348, #70815, #168218, .T. ) ;
#13480 = B_SPLINE_CURVE_WITH_KNOTS ( 'NONE', 3,
 ( #130562, #14507, #92715, #93999, #91454, #113576 ),
 .UNSPECIFIED., .F., .F.,
 ( 4, 2, 4 ),
 ( 0.000000000000000000, 0.0001568709654583423218, 0.0003137419309166846436 ),
 .UNSPECIFIED. ) ;
#13481 = CARTESIAN_POINT ( 'NONE',  ( 13.12229106158772929, 9.430637101696738966, -18.26826061806094614 ) ) ;
#13482 = CARTESIAN_POINT ( 'NONE',  ( -16.93935632781549572, 66.01526950028690521, -115.6334467358140614 ) ) ;
#13483 = ORIENTED_EDGE ( 'NONE', *, *, #127764, .T. ) ;
#13484 = CARTESIAN_POINT ( 'NONE',  ( -18.58744394320938298, 85.56638515456030802, -129.7002594306477761 ) ) ;
#13485 = ORIENTED_EDGE ( 'NONE', *, *, #88917, .T. ) ;
#13487 = ORIENTED_EDGE ( 'NONE', *, *, #185958, .T. ) ;
#13486 = CARTESIAN_POINT ( 'NONE',  ( -21.14999999999999858, 64.35000000001166143, -69.52310748452440237 ) ) ;
#13488 = EDGE_CURVE ( 'NONE', #207394, #77841, #212018, .T. ) ;
#13489 = ORIENTED_EDGE ( 'NONE', *, *, #237504, .T. ) ;
#13490 = DIRECTION ( 'NONE',  ( 0.000000000000000000, 0.01283462868040404978, 0.9999176327611370985 ) ) ;
#13491 = EDGE_CURVE ( 'NONE', #211904, #90469, #111621, .T. ) ;
#13492 = CARTESIAN_POINT ( 'NONE',  ( -16.89268316805466341, 66.04827818677041762, -190.8788599630699707 ) ) ;
#13493 = DIRECTION ( 'NONE',  ( 1.000000000000000000, 0.000000000000000000, 0.000000000000000000 ) ) ;
#13494 = DIRECTION ( 'NONE',  ( 1.000000000000000000, 0.000000000000000000, 0.000000000000000000 ) ) ;
#13495 = ORIENTED_EDGE ( 'NONE', *, *, #27452, .T. ) ;
#13496 = CARTESIAN_POINT ( 'NONE',  ( -21.64999999999999858, 30.16539832223782369, -234.6716761914553899 ) ) ;
#13497 = DIRECTION ( 'NONE',  ( 0.000000000000000000, 0.000000000000000000, -1.000000000000000000 ) ) ;
#13498 = ORIENTED_EDGE ( 'NONE', *, *, #65681, .F. ) ;
#13500 = ORIENTED_EDGE ( 'NONE', *, *, #145036, .T. ) ;
#13499 = CARTESIAN_POINT ( 'NONE',  ( 23.24999999999999289, 64.35000000001213039, -136.5231074845243597 ) ) ;
#13501 = AXIS2_PLACEMENT_3D ( 'NONE', #52864, #252349, #133696 ) ;
#13502 = DIRECTION ( 'NONE',  ( 0.000000000000000000, 7.056502275159890043E-15, -1.000000000000000000 ) ) ;
#13503 = CARTESIAN_POINT ( 'NONE',  ( 21.05000000000000071, 11.60000000000000675, -26.57179676972450011 ) ) ;
#13504 = CIRCLE ( 'NONE', #117538, 0.1999999999999987899 ) ;
#13505 = CARTESIAN_POINT ( 'NONE',  ( 20.12499999999999645, 60.48513714662838225, -225.3600541895200138 ) ) ;
#13506 = ORIENTED_EDGE ( 'NONE', *, *, #7245, .T. ) ;
#13507 = EDGE_CURVE ( 'NONE', #109222, #175428, #60616, .T. ) ;
#13508 = ADVANCED_FACE ( 'NONE', ( #98426 ), #77599, .F. ) ;
#13509 = VERTEX_POINT ( 'NONE', #41098 ) ;
#13510 = DIRECTION ( 'NONE',  ( 1.000000000000000000, 2.952720810173289112E-16, -0.000000000000000000 ) ) ;
#13511 = DIRECTION ( 'NONE',  ( 1.000000000000000000, -0.000000000000000000, 0.000000000000000000 ) ) ;
#13512 = EDGE_LOOP ( 'NONE', ( #242495, #24555, #80316, #144767 ) ) ;
#13513 = CARTESIAN_POINT ( 'NONE',  ( 23.15000000000000213, 28.51339163295720525, -258.4040038037771865 ) ) ;
#13514 = EDGE_CURVE ( 'NONE', #8349, #95988, #51605, .T. ) ;
#13515 = CARTESIAN_POINT ( 'NONE',  ( -22.45437739390954590, -2.479040262656531546, -189.6172560658480677 ) ) ;
#13516 = DIRECTION ( 'NONE',  ( 0.000000000000000000, 0.000000000000000000, -1.000000000000000000 ) ) ;
#13517 = EDGE_CURVE ( 'NONE', #253585, #207953, #120631, .T. ) ;
#13518 = EDGE_CURVE ( 'NONE', #75024, #172022, #99582, .T. ) ;
#13519 = CIRCLE ( 'NONE', #76045, 11.65000000000000746 ) ;
#13520 = EDGE_LOOP ( 'NONE', ( #9154, #249941, #201130 ) ) ;
#13521 = DIRECTION ( 'NONE',  ( -1.000000000000000000, -3.265361837132813093E-16, 0.000000000000000000 ) ) ;
#13522 = ORIENTED_EDGE ( 'NONE', *, *, #238565, .F. ) ;
#13524 = FACE_OUTER_BOUND ( 'NONE', #125122, .T. ) ;
#13523 = B_SPLINE_CURVE_WITH_KNOTS ( 'NONE', 3,
 ( #218489, #121987, #119428, #102383, #219788, #200239, #180684, #2016, #81538, #202801, #161122, #84084, #3297, #159846, #82818, #162413, #163686, #243203, #241920 ),
 .UNSPECIFIED., .F., .F.,
 ( 4, 3, 3, 3, 3, 3, 4 ),
 ( -2.000416914658901521E-06, 0.000000000000000000, 4.714008503744565809E-05, 9.979203887777271477E-05, 0.0001372215519229478891, 0.0001635031576220937453, 0.0001900083748504128364 ),
 .UNSPECIFIED. ) ;
#13525 = DIRECTION ( 'NONE',  ( 0.000000000000000000, 0.000000000000000000, -1.000000000000000000 ) ) ;
#13526 = VECTOR ( 'NONE', #58486, 999.9999999999998863 ) ;
#13528 = ORIENTED_EDGE ( 'NONE', *, *, #10498, .F. ) ;
#13527 = FACE_OUTER_BOUND ( 'NONE', #67741, .T. ) ;
#13530 = EDGE_CURVE ( 'NONE', #161497, #196101, #30825, .T. ) ;
#13529 = CARTESIAN_POINT ( 'NONE',  ( -20.54999999999999716, 2.000000000011154189, -87.27537807723794572 ) ) ;
#13531 = CARTESIAN_POINT ( 'NONE',  ( 18.49999999999999645, 77.83534155023670564, -158.4679561919613491 ) ) ;
#13532 = DIRECTION ( 'NONE',  ( 0.000000000000000000, 0.9126074666063660468, 0.4088369013363524762 ) ) ;
#13533 = CARTESIAN_POINT ( 'NONE',  ( 23.14999999999999503, 64.35000000001150511, -48.17310748452440095 ) ) ;
#13534 = CARTESIAN_POINT ( 'NONE',  ( 20.27550659511088682, 66.78395627750275310, -60.27310748452438816 ) ) ;
#13535 = EDGE_CURVE ( 'NONE', #25250, #160733, #239276, .T. ) ;
#13536 = TOROIDAL_SURFACE ( 'NONE', #159292, 7.791421356237335338, 0.1000000000000000056 ) ;
#13537 = LINE ( 'NONE', #252127, #189098 ) ;
#13538 = DIRECTION ( 'NONE',  ( 1.000000000000000000, -0.000000000000000000, -0.000000000000000000 ) ) ;
#13540 = ORIENTED_EDGE ( 'NONE', *, *, #189760, .T. ) ;
#13539 = CARTESIAN_POINT ( 'NONE',  ( -21.17356465864818560, 69.57719687377041851, -136.6220187255381973 ) ) ;
#13541 = VECTOR ( 'NONE', #208249, 1000.000000000000000 ) ;
#13542 = AXIS2_PLACEMENT_3D ( 'NONE', #18251, #76930, #219005 ) ;
#13543 = AXIS2_PLACEMENT_3D ( 'NONE', #96349, #152532, #175939 ) ;
#13544 = AXIS2_PLACEMENT_3D ( 'NONE', #100406, #159154, #19624 ) ;
#13545 = CARTESIAN_POINT ( 'NONE',  ( -18.50000000000000000, 64.35000000001234355, -163.0083017138704236 ) ) ;
#13546 = CARTESIAN_POINT ( 'NONE',  ( 22.39999999999999858, 7.790779598384538929, -33.39999999999999858 ) ) ;
#13547 = CARTESIAN_POINT ( 'NONE',  ( 21.05000000000000071, 67.17357026049489832, -128.1090527715806502 ) ) ;
#13548 = AXIS2_PLACEMENT_3D ( 'NONE', #65966, #25568, #163795 ) ;
#13549 = VERTEX_POINT ( 'NONE', #121908 ) ;
#13550 = CYLINDRICAL_SURFACE ( 'NONE', #58078, 0.09999999999999939493 ) ;
#13551 = AXIS2_PLACEMENT_3D ( 'NONE', #181474, #60210, #180187 ) ;
#13552 = DIRECTION ( 'NONE',  ( 1.000000000000000000, 0.000000000000000000, 0.000000000000000000 ) ) ;
#13553 = CARTESIAN_POINT ( 'NONE',  ( -20.54999999999999716, -9.399999999988848387, -76.89396912265249284 ) ) ;
#13554 = AXIS2_PLACEMENT_3D ( 'NONE', #75127, #119369, #78915 ) ;
#13555 = VECTOR ( 'NONE', #181087, 1000.000000000000000 ) ;
#13556 = ORIENTED_EDGE ( 'NONE', *, *, #252807, .T. ) ;
#13557 = CIRCLE ( 'NONE', #71833, 0.3999999999999975797 ) ;
#13559 = EDGE_CURVE ( 'NONE', #126194, #38036, #82727, .T. ) ;
#13558 = LINE ( 'NONE', #74841, #172697 ) ;
#13560 = AXIS2_PLACEMENT_3D ( 'NONE', #77363, #164630, #143761 ) ;
#13561 = AXIS2_PLACEMENT_3D ( 'NONE', #218339, #15046, #197505 ) ;
#13562 = CARTESIAN_POINT ( 'NONE',  ( -16.93772744219066340, 9.993541108763510650, -79.59806197196974153 ) ) ;
#13563 = ORIENTED_EDGE ( 'NONE', *, *, #85972, .F. ) ;
#13564 = CARTESIAN_POINT ( 'NONE',  ( 20.94999999999999929, 7.128833340094563376, -233.7327013124401276 ) ) ;
#13565 = VERTEX_POINT ( 'NONE', #234987 ) ;
#13567 = VECTOR ( 'NONE', #19083, 1000.000000000000000 ) ;
#13566 = CARTESIAN_POINT ( 'NONE',  ( -23.15000000000000213, 5.950000000011163692, -157.1942976949652007 ) ) ;
#13569 = ORIENTED_EDGE ( 'NONE', *, *, #144421, .T. ) ;
#13568 = DIRECTION ( 'NONE',  ( 1.000000000000000000, -0.000000000000000000, 0.000000000000000000 ) ) ;
#13570 = DIRECTION ( 'NONE',  ( 0.000000000000000000, 0.000000000000000000, -1.000000000000000000 ) ) ;
#13571 = ORIENTED_EDGE ( 'NONE', *, *, #125718, .F. ) ;
#13572 = CYLINDRICAL_SURFACE ( 'NONE', #1622, 0.09999999999999939493 ) ;
#13573 = ORIENTED_EDGE ( 'NONE', *, *, #99699, .T. ) ;
#13575 = EDGE_LOOP ( 'NONE', ( #152146, #84790, #56330, #38003 ) ) ;
#13574 = ORIENTED_EDGE ( 'NONE', *, *, #205213, .T. ) ;
#13576 = DIRECTION ( 'NONE',  ( 0.000000000000000000, 0.9908441862701605762, 0.1350103645451835310 ) ) ;
#13577 = B_SPLINE_CURVE_WITH_KNOTS ( 'NONE', 3,
 ( #72530, #35969, #215849, #37258, #92066, #97158, #176766, #93349, #256207, #77617 ),
 .UNSPECIFIED., .F., .F.,
 ( 4, 2, 2, 2, 4 ),
 ( 0.000000000000000000, 4.221631689687584354E-05, 8.443263379375168709E-05, 0.0001688652675875033742, 0.0003377305351749930332 ),
 .UNSPECIFIED. ) ;
#13579 = EDGE_LOOP ( 'NONE', ( #19021, #178547, #89918, #87849 ) ) ;
#13578 = CARTESIAN_POINT ( 'NONE',  ( 21.05000000000000071, 10.72371710471867701, -146.1500000000000341 ) ) ;
#13580 = ADVANCED_FACE ( 'NONE', ( #95461 ), #156756, .F. ) ;
#13581 = CARTESIAN_POINT ( 'NONE',  ( 20.87600722750343252, 65.66887361445314752, -63.93298459182691573 ) ) ;
#13583 = EDGE_LOOP ( 'NONE', ( #151559, #63017, #251659 ) ) ;
#13582 = AXIS2_PLACEMENT_3D ( 'NONE', #116715, #191145, #256158 ) ;
#13584 = AXIS2_PLACEMENT_3D ( 'NONE', #46822, #106803, #158182 ) ;
#13585 = CIRCLE ( 'NONE', #88572, 0.2000000000000057288 ) ;
#13586 = ORIENTED_EDGE ( 'NONE', *, *, #39696, .F. ) ;
#13587 = DIRECTION ( 'NONE',  ( 2.952720810173289112E-16, 1.000000000000000000, -6.088138035986627436E-46 ) ) ;
#13588 = DIRECTION ( 'NONE',  ( 0.000000000000000000, 7.086529944415886769E-15, -1.000000000000000000 ) ) ;
#13589 =( BOUNDED_SURFACE ( )  B_SPLINE_SURFACE ( 3, 2, ( 
 ( #186224, #244898, #66274 ),
 ( #145790, #144498, #242330 ),
 ( #227913, #49266, #224043 ),
 ( #204480, #147070, #187523 ),
 ( #25873, #63691, #183661 ),
 ( #3720, #64974, #201932 ),
 ( #225317, #27179, #102800 ),
 ( #143223, #226608, #126230 ),
 ( #105351, #222758, #205770 ),
 ( #87092, #246194, #47976 ) ),
 .UNSPECIFIED., .F., .F., .F. ) 
 B_SPLINE_SURFACE_WITH_KNOTS ( ( 4, 2, 2, 2, 4 ),
 ( 3, 3 ),
 ( 0.0001701955120502393333, 0.0002247052511886148682, 0.0002792149903269904032, 0.0003882344686037414189, 0.0006062734251572434504 ),
 ( 0.000000000000000000, 1.000000000000000000 ),
 .UNSPECIFIED. ) 
 GEOMETRIC_REPRESENTATION_ITEM ( )  RATIONAL_B_SPLINE_SURFACE ( (
 ( 1.000000000000000000, 0.2966190024560962923, 1.000000000000000000),
 ( 1.000000000000000000, 0.2964522492697523326, 1.000000000000000000),
 ( 1.000000000000000000, 0.3059923531903553373, 1.000000000000000000),
 ( 1.000000000000000000, 0.3355751146924953465, 1.000000000000000000),
 ( 1.000000000000000000, 0.3550672384964631556, 1.000000000000000000),
 ( 1.000000000000000000, 0.4157034672184506396, 1.000000000000000000),
 ( 1.000000000000000000, 0.4588031877630285860, 1.000000000000000000),
 ( 1.000000000000000000, 0.5771441759709375896, 1.000000000000000000),
 ( 1.000000000000000000, 0.6469377121736774594, 1.000000000000000000),
 ( 1.000000000000000000, 0.7071067811865192621, 1.000000000000000000) ) ) 
 REPRESENTATION_ITEM ( '' )  SURFACE ( )  );
#13590 = DIRECTION ( 'NONE',  ( -2.952720810173289112E-16, -0.9651348961777157509, 0.2617529984165031243 ) ) ;
#13591 = ORIENTED_EDGE ( 'NONE', *, *, #245510, .T. ) ;
#13592 = LINE ( 'NONE', #172705, #216026 ) ;
#13593 = DIRECTION ( 'NONE',  ( -1.000000000000000000, 0.000000000000000000, -0.000000000000000000 ) ) ;
#13594 = CARTESIAN_POINT ( 'NONE',  ( -18.59999999999999787, -1.362429037193310988, -41.38888124792119783 ) ) ;
#13595 = ORIENTED_EDGE ( 'NONE', *, *, #242690, .T. ) ;
#13596 = DIRECTION ( 'NONE',  ( -1.000000000000000000, -0.000000000000000000, 0.000000000000000000 ) ) ;
#13597 = DIRECTION ( 'NONE',  ( -1.000000000000000000, -0.000000000000000000, -0.000000000000000000 ) ) ;
#13598 = EDGE_LOOP ( 'NONE', ( #125478, #242850, #227325, #52218 ) ) ;
#13599 = CARTESIAN_POINT ( 'NONE',  ( -16.93388492042257809, 14.20741668428894222, -219.2962582334711499 ) ) ;
#13600 = ORIENTED_EDGE ( 'NONE', *, *, #243476, .F. ) ;
#13601 = CARTESIAN_POINT ( 'NONE',  ( -18.47079683080344026, -7.741948359812542257, -209.9616156304373931 ) ) ;
#13602 = ORIENTED_EDGE ( 'NONE', *, *, #254777, .F. ) ;
#13603 = DIRECTION ( 'NONE',  ( 3.469446951953498700E-14, -0.7899159663865300551, -0.6132151058540831201 ) ) ;
#13604 = ORIENTED_EDGE ( 'NONE', *, *, #15503, .F. ) ;
#13605 = CIRCLE ( 'NONE', #92701, 0.09999999999998898659 ) ;
#13606 = ORIENTED_EDGE ( 'NONE', *, *, #95705, .F. ) ;
#13607 = CARTESIAN_POINT ( 'NONE',  ( 23.14999999999999858, 1.115600667400684642E-11, -100.5000000000000426 ) ) ;
#13608 = CARTESIAN_POINT ( 'NONE',  ( 20.85000000000000142, 64.25000000001195133, -109.8069731475024753 ) ) ;
#13609 = VERTEX_POINT ( 'NONE', #14677 ) ;
#13610 = EDGE_LOOP ( 'NONE', ( #58308, #146378, #226141, #11877 ) ) ;
#13611 = DIRECTION ( 'NONE',  ( 0.000000000000000000, 1.000000000000000000, 0.000000000000000000 ) ) ;
#13612 = DIRECTION ( 'NONE',  ( 0.000000000000000000, -6.982962677686266711E-15, 1.000000000000000000 ) ) ;
#13613 = ORIENTED_EDGE ( 'NONE', *, *, #39357, .T. ) ;
#13614 = EDGE_CURVE ( 'NONE', #2322, #80091, #60007, .T. ) ;
#13615 = EDGE_LOOP ( 'NONE', ( #239543, #218644, #141888, #110763 ) ) ;
#13616 = CIRCLE ( 'NONE', #126024, 0.09999999999998568367 ) ;
#13617 = CARTESIAN_POINT ( 'NONE',  ( 20.94999999999999574, -11.39257802169451672, -103.5739495798319751 ) ) ;
#13618 = EDGE_CURVE ( 'NONE', #125420, #132220, #15963, .T. ) ;
#13619 = CYLINDRICAL_SURFACE ( 'NONE', #138748, 0.09999999999998898659 ) ;
#13620 = ADVANCED_FACE ( 'NONE', ( #152907 ), #92885, .T. ) ;
#13621 = PLANE ( 'NONE',  #76053 ) ;
#13623 = ORIENTED_EDGE ( 'NONE', *, *, #56156, .F. ) ;
#13622 = CARTESIAN_POINT ( 'NONE',  ( 23.14999999999999503, 51.38014393322265505, -230.1906178717505327 ) ) ;
#13624 = LINE ( 'NONE', #235231, #136719 ) ;
#13625 = CARTESIAN_POINT ( 'NONE',  ( -22.50000000000000000, 12.55707850971102069, -223.4244300710886648 ) ) ;
#13626 = FACE_OUTER_BOUND ( 'NONE', #23249, .T. ) ;
#13628 = DIRECTION ( 'NONE',  ( 1.000000000000000000, -0.000000000000000000, -0.000000000000000000 ) ) ;
#13627 = DIRECTION ( 'NONE',  ( -1.000000000000000000, 0.000000000000000000, 0.000000000000000000 ) ) ;
#13629 = DIRECTION ( 'NONE',  ( 0.000000000000000000, 1.776356839400277286E-15, -1.000000000000000000 ) ) ;
#13630 = CARTESIAN_POINT ( 'NONE',  ( -23.15000000000000213, 64.35000000001176090, -76.53791325517833855 ) ) ;
#13631 = AXIS2_PLACEMENT_3D ( 'NONE', #120575, #98369, #162267 ) ;
#13632 = EDGE_CURVE ( 'NONE', #130829, #135164, #235006, .T. ) ;
#13633 = CARTESIAN_POINT ( 'NONE',  ( -20.85000000000000142, 43.35377423437995503, -245.1717807829448930 ) ) ;
#13634 = CARTESIAN_POINT ( 'NONE',  ( -21.07928932188134041, 75.90110485435803866, -176.3516241409176644 ) ) ;
#13635 = CIRCLE ( 'NONE', #155319, 0.5000000000000004441 ) ;
#13636 = ORIENTED_EDGE ( 'NONE', *, *, #82816, .F. ) ;
#13637 = VECTOR ( 'NONE', #96737, 1000.000000000000000 ) ;
#13638 = ORIENTED_EDGE ( 'NONE', *, *, #226393, .F. ) ;
#13639 = EDGE_CURVE ( 'NONE', #66482, #193487, #64304, .T. ) ;
#13640 = DIRECTION ( 'NONE',  ( 1.000000000000000000, 0.000000000000000000, 0.000000000000000000 ) ) ;
#13641 = CARTESIAN_POINT ( 'NONE',  ( -23.25000000000000000, 77.25000000001136868, -28.22262673010923351 ) ) ;
#13642 = EDGE_LOOP ( 'NONE', ( #3874, #147045, #45689, #134579 ) ) ;
#13643 = CIRCLE ( 'NONE', #51029, 0.2000000000000057288 ) ;
#13644 = AXIS2_PLACEMENT_3D ( 'NONE', #30924, #227797, #110420 ) ;
#13645 = FACE_OUTER_BOUND ( 'NONE', #104840, .T. ) ;
#13646 = FACE_OUTER_BOUND ( 'NONE', #243621, .T. ) ;
#13647 = EDGE_LOOP ( 'NONE', ( #64917, #4448, #244259 ) ) ;
#13648 = VERTEX_POINT ( 'NONE', #57606 ) ;
#13649 = LINE ( 'NONE', #172769, #104810 ) ;
#13650 = CARTESIAN_POINT ( 'NONE',  ( -23.25000000000000000, 36.65892442174472876, -249.5511627012454596 ) ) ;
#13651 = CIRCLE ( 'NONE', #121822, 0.09999999999999939493 ) ;
#13652 = CARTESIAN_POINT ( 'NONE',  ( -18.40000000000000213, 8.822561741677553471, -57.75000000000000000 ) ) ;
#13654 = ORIENTED_EDGE ( 'NONE', *, *, #227439, .F. ) ;
#13653 = CARTESIAN_POINT ( 'NONE',  ( -20.94999999999999929, 74.16465844978819177, -191.9679561919613775 ) ) ;
#13655 = DIRECTION ( 'NONE',  ( 3.469446951953635015E-14, 6.982962677686266711E-15, -1.000000000000000000 ) ) ;
#13657 = ORIENTED_EDGE ( 'NONE', *, *, #20605, .T. ) ;
#13656 = CARTESIAN_POINT ( 'NONE',  ( -18.59999999999999787, 59.16775194334852728, -221.0793150863668473 ) ) ;
#13658 = VECTOR ( 'NONE', #193858, 1000.000000000000114 ) ;
#13659 = DIRECTION ( 'NONE',  ( 0.000000000000000000, 7.086529944415894657E-15, -1.000000000000000000 ) ) ;
#13661 = CARTESIAN_POINT ( 'NONE',  ( -21.05000000000000071, 0.000000000000000000, 0.000000000000000000 ) ) ;
#13660 = CIRCLE ( 'NONE', #46966, 0.09999999999999939493 ) ;
#13662 = DIRECTION ( 'NONE',  ( 0.000000000000000000, 0.000000000000000000, 1.000000000000000000 ) ) ;
#13663 = DIRECTION ( 'NONE',  ( 0.000000000000000000, 7.116814260417676401E-15, -1.000000000000000000 ) ) ;
#13664 = AXIS2_PLACEMENT_3D ( 'NONE', #215044, #156390, #36437 ) ;
#13666 = CARTESIAN_POINT ( 'NONE',  ( 20.51284917709620359, 10.31088662285602275, -108.1724731855920538 ) ) ;
#13665 = DIRECTION ( 'NONE',  ( 1.000000000000000000, 0.000000000000000000, 0.000000000000000000 ) ) ;
#13667 = LINE ( 'NONE', #232733, #178783 ) ;
#13668 = CARTESIAN_POINT ( 'NONE',  ( 20.94999999999999574, 68.51069317435826633, -224.1259271199053842 ) ) ;
#13669 = CARTESIAN_POINT ( 'NONE',  ( 21.05000000000000071, 70.15000000001235492, -159.8906102602464330 ) ) ;
#13670 = VERTEX_POINT ( 'NONE', #254510 ) ;
#13671 = EDGE_CURVE ( 'NONE', #235869, #248947, #135856, .T. ) ;
#13672 = CARTESIAN_POINT ( 'NONE',  ( 13.40000000000005898, 64.35000000001120668, -21.02310748452479316 ) ) ;
#13673 = ORIENTED_EDGE ( 'NONE', *, *, #185696, .T. ) ;
#13674 = ORIENTED_EDGE ( 'NONE', *, *, #139438, .T. ) ;
#13675 = LINE ( 'NONE', #227586, #248432 ) ;
#13676 = DIRECTION ( 'NONE',  ( 0.000000000000000000, -0.8096735173027302945, 0.5868805631290110458 ) ) ;
#13677 = ADVANCED_FACE ( 'NONE', ( #134568 ), #98005, .F. ) ;
#13678 = ORIENTED_EDGE ( 'NONE', *, *, #240009, .T. ) ;
#13680 = B_SPLINE_CURVE_WITH_KNOTS ( 'NONE', 3,
 ( #13686, #31995, #134891, #110214, #72404, #54094, #132350, #91941, #194919, #231473, #252284, #192335, #133637 ),
 .UNSPECIFIED., .F., .F.,
 ( 4, 3, 3, 3, 4 ),
 ( 1.084445006577768218E-16, 1.946463881814412345E-05, 3.922356109944399394E-05, 4.215060953238735362E-05, 4.415117091092665805E-05 ),
 .UNSPECIFIED. ) ;
#13679 = CARTESIAN_POINT ( 'NONE',  ( -21.05000000000000071, 30.78834561061718489, -252.2906857787774015 ) ) ;
#13681 = EDGE_CURVE ( 'NONE', #53624, #227815, #118301, .T. ) ;
#13682 = CIRCLE ( 'NONE', #55163, 0.1000000000000028644 ) ;
#13683 = ORIENTED_EDGE ( 'NONE', *, *, #12463, .F. ) ;
#13684 = VERTEX_POINT ( 'NONE', #231151 ) ;
#13685 = DIRECTION ( 'NONE',  ( 3.469446951953728416E-14, 0.8660254037844343777, -0.5000000000000074385 ) ) ;
#13686 = CARTESIAN_POINT ( 'NONE',  ( -16.81744102076749314, 66.05000000001157900, -56.87310748452438958 ) ) ;
#13687 = DIRECTION ( 'NONE',  ( 1.000000000000000000, 0.000000000000000000, 0.000000000000000000 ) ) ;
#13688 = PLANE ( 'NONE',  #140588 ) ;
#13689 = CARTESIAN_POINT ( 'NONE',  ( 12.25000000000000000, 9.349999999999983658, -16.74999999999999645 ) ) ;
#13690 = EDGE_CURVE ( 'NONE', #189000, #67768, #226412, .T. ) ;
#13692 = FACE_OUTER_BOUND ( 'NONE', #103862, .T. ) ;
#13691 = CARTESIAN_POINT ( 'NONE',  ( -20.64999999999999858, 76.00000000001244871, -170.0231074845243597 ) ) ;
#13693 = CARTESIAN_POINT ( 'NONE',  ( -23.15000000000000213, 76.00000000001213607, -136.5231074845242745 ) ) ;
#13695 = ORIENTED_EDGE ( 'NONE', *, *, #198332, .T. ) ;
#13694 = DIRECTION ( 'NONE',  ( 0.000000000000000000, -0.1298341882519953860, -0.9915357197604862671 ) ) ;
#13697 = DIRECTION ( 'NONE',  ( 1.000000000000000000, 0.000000000000000000, 0.000000000000000000 ) ) ;
#13696 = CYLINDRICAL_SURFACE ( 'NONE', #142159, 0.4999999999999944489 ) ;
#13698 = CARTESIAN_POINT ( 'NONE',  ( -20.94999999999999929, -11.41227409413852811, -198.0999999999999659 ) ) ;
#13699 = ORIENTED_EDGE ( 'NONE', *, *, #208678, .T. ) ;
#13700 = CARTESIAN_POINT ( 'NONE',  ( -18.50000000000000000, 11.65000000001115232, -21.75000000000000355 ) ) ;
#13701 = CIRCLE ( 'NONE', #159462, 0.09999999999999939493 ) ;
#13702 = CARTESIAN_POINT ( 'NONE',  ( 21.08832698747859169, 8.775364393428372267, -146.2287174664641896 ) ) ;
#13704 = ADVANCED_FACE ( 'NONE', ( #38082 ), #75907, .F. ) ;
#13703 = DIRECTION ( 'NONE',  ( 0.000000000000000000, 0.000000000000000000, -1.000000000000000000 ) ) ;
#13706 = EDGE_CURVE ( 'NONE', #51386, #94361, #116331, .T. ) ;
#13705 = ORIENTED_EDGE ( 'NONE', *, *, #155750, .T. ) ;
#13708 = CARTESIAN_POINT ( 'NONE',  ( -18.40000000000000213, 70.35000000001230092, -157.3731074845244109 ) ) ;
#13707 = AXIS2_PLACEMENT_3D ( 'NONE', #143477, #108217, #63951 ) ;
#13709 = VECTOR ( 'NONE', #50487, 1000.000000000000000 ) ;
#13710 = DIRECTION ( 'NONE',  ( 0.000000000000000000, 0.000000000000000000, 1.000000000000000000 ) ) ;
#13711 = CARTESIAN_POINT ( 'NONE',  ( 19.99999999999998934, 11.75000000001115907, -192.3499999999999659 ) ) ;
#13712 = VERTEX_POINT ( 'NONE', #137159 ) ;
#13713 = ORIENTED_EDGE ( 'NONE', *, *, #167967, .T. ) ;
#13714 = CIRCLE ( 'NONE', #88706, 2.000000000000001776 ) ;
#13715 = ADVANCED_FACE ( 'NONE', ( #115031 ), #255797, .T. ) ;
#13716 = FACE_OUTER_BOUND ( 'NONE', #41760, .T. ) ;
#13717 = CARTESIAN_POINT ( 'NONE',  ( -18.51697539158857353, 10.31565961587945957, -173.0364194119178478 ) ) ;
#13718 = CARTESIAN_POINT ( 'NONE',  ( 18.59999999999998721, 43.18640298906419162, -245.2812653309023574 ) ) ;
#13720 = EDGE_CURVE ( 'NONE', #90111, #138795, #47525, .T. ) ;
#13719 = CARTESIAN_POINT ( 'NONE',  ( 17.74533788810831325, 65.18150020854152160, -159.7094848095768498 ) ) ;
#13721 = ORIENTED_EDGE ( 'NONE', *, *, #252009, .F. ) ;
#13722 = EDGE_CURVE ( 'NONE', #97044, #196423, #14258, .T. ) ;
#13723 = TOROIDAL_SURFACE ( 'NONE', #1228, 0.9750000000000019762, 0.1000000000000000056 ) ;
#13725 = VECTOR ( 'NONE', #185006, 1000.000000000000114 ) ;
#13724 = DIRECTION ( 'NONE',  ( 0.000000000000000000, 6.982962677686266711E-15, -1.000000000000000000 ) ) ;
#13726 = CARTESIAN_POINT ( 'NONE',  ( -22.48660254037843131, 64.25000000001236344, -170.0731074845244279 ) ) ;
#13727 = CARTESIAN_POINT ( 'NONE',  ( 18.59999999999999076, -1.149570369564537842, -74.81591248450196474 ) ) ;
#13728 = VECTOR ( 'NONE', #116842, 1000.000000000000000 ) ;
#13729 = DIRECTION ( 'NONE',  ( 0.000000000000000000, -1.000000000000000000, 0.000000000000000000 ) ) ;
#13730 = CARTESIAN_POINT ( 'NONE',  ( -20.64999999999999858, 76.00000000001244871, -170.0231074845243597 ) ) ;
#13731 = AXIS2_PLACEMENT_3D ( 'NONE', #191618, #12973, #152486 ) ;
#13732 = AXIS2_PLACEMENT_3D ( 'NONE', #5708, #83937, #240496 ) ;
#13733 = VECTOR ( 'NONE', #239984, 1000.000000000000000 ) ;
#13735 = ORIENTED_EDGE ( 'NONE', *, *, #241866, .F. ) ;
#13734 = CARTESIAN_POINT ( 'NONE',  ( -16.93415306273742260, 66.00437773999929902, -82.11305054216397536 ) ) ;
#13736 = TOROIDAL_SURFACE ( 'NONE', #105276, 0.2000000000000000111, 0.1000000000000000056 ) ;
#13737 = DIRECTION ( 'NONE',  ( 1.000000000000000000, 0.000000000000000000, 0.000000000000000000 ) ) ;
#13739 = ADVANCED_FACE ( 'NONE', ( #127985 ), #169716, .T. ) ;
#13738 = DIRECTION ( 'NONE',  ( 0.000000000000000000, -0.7071067811865472397, -0.7071067811865479058 ) ) ;
#13740 = CARTESIAN_POINT ( 'NONE',  ( 20.94999999999999929, 1.115600667400684642E-11, -134.0000000000000284 ) ) ;
#13741 = DIRECTION ( 'NONE',  ( -1.000000000000000000, -1.541880601228652843E-16, -2.878400969107353907E-16 ) ) ;
#13742 = ADVANCED_FACE ( 'NONE', ( #109683 ), #93973, .T. ) ;
#13743 = CARTESIAN_POINT ( 'NONE',  ( -23.15000000000000213, -9.499999999988848032, -177.3939691226524076 ) ) ;
#13745 = ORIENTED_EDGE ( 'NONE', *, *, #179559, .F. ) ;
#13744 = LINE ( 'NONE', #253614, #169343 ) ;
#13746 = CARTESIAN_POINT ( 'NONE',  ( 21.09546886439535029, 8.878553113014918452, -12.23709385055535925 ) ) ;
#13747 = DIRECTION ( 'NONE',  ( 1.000000000000000000, 0.000000000000000000, 0.000000000000000000 ) ) ;
#13748 = DIRECTION ( 'NONE',  ( 2.557131231893037478E-16, 0.8660254037844420383, -0.4999999999999943379 ) ) ;
#13749 = ORIENTED_EDGE ( 'NONE', *, *, #15855, .T. ) ;
#13750 = CARTESIAN_POINT ( 'NONE',  ( 22.59999999999999787, 11.64957080755595520, -33.40000000000000568 ) ) ;
#13751 = DIRECTION ( 'NONE',  ( 0.000000000000000000, 0.000000000000000000, 1.000000000000000000 ) ) ;
#13752 = DIRECTION ( 'NONE',  ( 1.000000000000000000, 0.000000000000000000, 0.000000000000000000 ) ) ;
#13753 = EDGE_CURVE ( 'NONE', #171694, #6394, #51810, .T. ) ;
#13754 = FACE_OUTER_BOUND ( 'NONE', #208246, .T. ) ;
#13755 = VECTOR ( 'NONE', #127735, 1000.000000000000000 ) ;
#13756 = VECTOR ( 'NONE', #184747, 1000.000000000000000 ) ;
#13757 = CARTESIAN_POINT ( 'NONE',  ( 21.05000000000000071, 4.850467289730776344, -188.9657325909983001 ) ) ;
#13758 = CONICAL_SURFACE ( 'NONE', #197090, 4.049999999999998046, 0.7853981633974604915 ) ;
#13759 = AXIS2_PLACEMENT_3D ( 'NONE', #251549, #232016, #53358 ) ;
#13760 = ORIENTED_EDGE ( 'NONE', *, *, #218439, .T. ) ;
#13761 = VERTEX_POINT ( 'NONE', #92692 ) ;
#13762 = CARTESIAN_POINT ( 'NONE',  ( 18.59999999999999787, 36.65892442174472876, -249.5511627012454596 ) ) ;
#13763 = DIRECTION ( 'NONE',  ( -1.000000000000000000, 0.000000000000000000, 0.000000000000000000 ) ) ;
#13764 = CARTESIAN_POINT ( 'NONE',  ( 18.42636655943170609, -0.7441698762049262506, -242.2113638065491728 ) ) ;
#13765 = DIRECTION ( 'NONE',  ( 1.000000000000000000, -0.000000000000000000, -0.000000000000000000 ) ) ;
#13766 = FACE_OUTER_BOUND ( 'NONE', #91373, .T. ) ;
#13767 = ADVANCED_FACE ( 'NONE', ( #187961 ), #70604, .T. ) ;
#13768 = DIRECTION ( 'NONE',  ( 0.000000000000000000, 0.2128009952264354188, -0.9770955615653151849 ) ) ;
#13769 = CARTESIAN_POINT ( 'NONE',  ( 21.05000000000000071, 0.000000000000000000, -33.50000000000000000 ) ) ;
#13770 = EDGE_CURVE ( 'NONE', #78926, #151026, #143413, .T. ) ;
#13771 = VECTOR ( 'NONE', #61471, 1000.000000000000000 ) ;
#13772 = CARTESIAN_POINT ( 'NONE',  ( 20.94999999999999574, 77.83534155023627932, -91.46795619196132066 ) ) ;
#13773 = ORIENTED_EDGE ( 'NONE', *, *, #162189, .F. ) ;
#13774 = CARTESIAN_POINT ( 'NONE',  ( 13.40000000000005720, 64.25000000001119815, -18.32310748452480098 ) ) ;
#13775 = EDGE_CURVE ( 'NONE', #163086, #37503, #135005, .T. ) ;
#13776 = ADVANCED_FACE ( 'NONE', ( #230956 ), #31025, .T. ) ;
#13777 = ORIENTED_EDGE ( 'NONE', *, *, #70749, .T. ) ;
#13778 = FACE_OUTER_BOUND ( 'NONE', #117729, .T. ) ;
#13779 = DIRECTION ( 'NONE',  ( 0.000000000000000000, 0.8814952561688476074, -0.4721928772777262417 ) ) ;
#13781 = ORIENTED_EDGE ( 'NONE', *, *, #218386, .F. ) ;
#13780 = CARTESIAN_POINT ( 'NONE',  ( 20.99999999999997868, 1.148907358139439339E-11, -201.0000000000015064 ) ) ;
#13782 = CARTESIAN_POINT ( 'NONE',  ( -22.39999999999999858, -3.275978944802467652, -228.2735455795363748 ) ) ;
#13784 = EDGE_CURVE ( 'NONE', #129693, #248393, #80645, .T. ) ;
#13783 = SURFACE_STYLE_USAGE ( .BOTH. , #208151 ) ;
#13785 = DIRECTION ( 'NONE',  ( 0.000000000000000000, 0.000000000000000000, 1.000000000000000000 ) ) ;
#13786 = DIRECTION ( 'NONE',  ( -0.000000000000000000, 0.9876197685951241256, 0.1568667991644932258 ) ) ;
#13787 = EDGE_LOOP ( 'NONE', ( #214229, #209524, #30269, #191254 ) ) ;
#13788 = DIRECTION ( 'NONE',  ( 0.000000000000000000, 0.000000000000000000, -1.000000000000000000 ) ) ;
#13789 = CARTESIAN_POINT ( 'NONE',  ( 13.40000000000005898, 64.35000000001120668, -21.02310748452479316 ) ) ;
#13790 = DIRECTION ( 'NONE',  ( 8.673617379884087537E-15, 6.982962677686266711E-15, -1.000000000000000000 ) ) ;
#13791 = DIRECTION ( 'NONE',  ( 1.000000000000000000, 0.000000000000000000, 0.000000000000000000 ) ) ;
#13792 = LINE ( 'NONE', #78578, #124757 ) ;
#13793 = EDGE_CURVE ( 'NONE', #204622, #50484, #85110, .T. ) ;
#13794 = AXIS2_PLACEMENT_3D ( 'NONE', #110960, #32752, #49705 ) ;
#13795 = EDGE_CURVE ( 'NONE', #49052, #40449, #55897, .T. ) ;
#13796 = ORIENTED_EDGE ( 'NONE', *, *, #138506, .T. ) ;
#13797 = CARTESIAN_POINT ( 'NONE',  ( 18.59999999999999076, 28.95347087985017609, -237.9930060266852081 ) ) ;
#13798 = FACE_OUTER_BOUND ( 'NONE', #96112, .T. ) ;
#13799 = VERTEX_POINT ( 'NONE', #30184 ) ;
#13800 = EDGE_CURVE ( 'NONE', #55017, #233370, #189219, .T. ) ;
#13801 = ORIENTED_EDGE ( 'NONE', *, *, #136665, .T. ) ;
#13802 = DIRECTION ( 'NONE',  ( 1.073024830501117725E-15, 6.982962677686266711E-15, -1.000000000000000000 ) ) ;
#13803 = CARTESIAN_POINT ( 'NONE',  ( -18.59999999999999787, -1.164121893230052995, -175.2148480855716173 ) ) ;
#13804 = ORIENTED_EDGE ( 'NONE', *, *, #247270, .T. ) ;
#13805 = CARTESIAN_POINT ( 'NONE',  ( -20.54999999999999716, 74.00000000001223555, -149.7477294072864709 ) ) ;
#13806 = DIRECTION ( 'NONE',  ( 1.000000000000000000, 0.000000000000000000, 0.000000000000000000 ) ) ;
#13807 = TOROIDAL_SURFACE ( 'NONE', #151391, 7.791421356237335338, 0.1000000000000000056 ) ;
#13808 = VERTEX_POINT ( 'NONE', #210101 ) ;
#13809 = EDGE_CURVE ( 'NONE', #124544, #167594, #34052, .T. ) ;
#13810 = ADVANCED_FACE ( 'NONE', ( #190544 ), #14478, .T. ) ;
#13811 = CIRCLE ( 'NONE', #109841, 0.09999999999999939493 ) ;
#13812 = CIRCLE ( 'NONE', #242941, 0.1000000000000027534 ) ;
#13813 = ADVANCED_FACE ( 'NONE', ( #234781 ), #236059, .T. ) ;
#13814 = ORIENTED_EDGE ( 'NONE', *, *, #126606, .T. ) ;
#13815 = CARTESIAN_POINT ( 'NONE',  ( -23.25000000000000000, 30.69873658968802488, -264.9868732779115703 ) ) ;
#13816 = DIRECTION ( 'NONE',  ( 2.840903330521633255E-16, -0.8700118002898322711, 0.4930308989875231696 ) ) ;
#13818 = VERTEX_POINT ( 'NONE', #155280 ) ;
#13817 = DIRECTION ( 'NONE',  ( 0.000000000000000000, 0.2617529984165034018, 0.9651348961777157509 ) ) ;
#13819 = ADVANCED_FACE ( 'NONE', ( #138224 ), #79535, .T. ) ;
#13820 = CARTESIAN_POINT ( 'NONE',  ( -20.54999999999999716, 4.250000000011156409, -179.8499999999999943 ) ) ;
#13822 = CARTESIAN_POINT ( 'NONE',  ( -22.50000000000000000, 11.64976291804307884, -133.9111900236131021 ) ) ;
#13821 = UNCERTAINTY_MEASURE_WITH_UNIT (LENGTH_MEASURE( 1.000000000000000082E-05 ), #120776, 'distance_accuracy_value', 'NONE');
#13823 = LINE ( 'NONE', #150766, #16940 ) ;
#13824 = CARTESIAN_POINT ( 'NONE',  ( -20.54999999999999716, 11.60058429089262333, -246.3380203656811887 ) ) ;
#13825 = EDGE_CURVE ( 'NONE', #233908, #143318, #26725, .T. ) ;
#13826 = CARTESIAN_POINT ( 'NONE',  ( 20.94999999999999929, 11.65000000001115943, -160.7161343370219129 ) ) ;
#13827 = CIRCLE ( 'NONE', #151212, 0.09999999999999986677 ) ;
#13828 = CYLINDRICAL_SURFACE ( 'NONE', #18031, 11.74999999999999645 ) ;
#13830 = DIRECTION ( 'NONE',  ( 0.000000000000000000, 0.9910827722268055195, 0.1332476588733540468 ) ) ;
#13829 = VECTOR ( 'NONE', #213065, 1000.000000000000000 ) ;
#13832 = EDGE_LOOP ( 'NONE', ( #195697, #171558, #7045, #23130 ) ) ;
#13831 = DIRECTION ( 'NONE',  ( 0.000000000000000000, 0.4930308989875575865, 0.8700118002898125091 ) ) ;
#13833 = ORIENTED_EDGE ( 'NONE', *, *, #188288, .T. ) ;
#13836 = CARTESIAN_POINT ( 'NONE',  ( -16.87683809663752399, 51.08978195134977796, -232.2756554297758953 ) ) ;
#13835 = LINE ( 'NONE', #73836, #153931 ) ;
#13834 = AXIS2_PLACEMENT_3D ( 'NONE', #82703, #46175, #162297 ) ;
#13838 = ORIENTED_EDGE ( 'NONE', *, *, #115623, .T. ) ;
#13837 = DIRECTION ( 'NONE',  ( 1.000000000000000000, 0.000000000000000000, 0.000000000000000000 ) ) ;
#13839 = ADVANCED_BREP_SHAPE_REPRESENTATION ( '', ( #193773, #2425 ), #147622 ) ;
#13840 = EDGE_LOOP ( 'NONE', ( #76855, #236453, #216190, #31231 ) ) ;
#13841 = CARTESIAN_POINT ( 'NONE',  ( -16.80117486205003630, 66.05034273170022630, -182.6742526115989449 ) ) ;
#13842 = CARTESIAN_POINT ( 'NONE',  ( 18.79999999999999716, 11.59510167572422112, 1.901609089591594470 ) ) ;
#13843 = DIRECTION ( 'NONE',  ( -1.000000000000000000, 0.000000000000000000, -0.000000000000000000 ) ) ;
#13844 = AXIS2_PLACEMENT_3D ( 'NONE', #196460, #161206, #80341 ) ;
#13845 = CARTESIAN_POINT ( 'NONE',  ( 19.75857864376269291, 11.75000000001116440, -58.25000000000000711 ) ) ;
#13846 = EDGE_CURVE ( 'NONE', #197595, #201532, #199528, .T. ) ;
#13847 = LINE ( 'NONE', #175507, #184028 ) ;
#13848 = PLANE ( 'NONE',  #73921 ) ;
#13849 = AXIS2_PLACEMENT_3D ( 'NONE', #81369, #159669, #82654 ) ;
#13850 = AXIS2_PLACEMENT_3D ( 'NONE', #86311, #128047, #200198 ) ;
#13851 = VECTOR ( 'NONE', #65101, 1000.000000000000000 ) ;
#13853 = AXIS2_PLACEMENT_3D ( 'NONE', #244330, #203927, #104792 ) ;
#13852 = CARTESIAN_POINT ( 'NONE',  ( 20.94999999999999929, 5.850000000000004086, -23.36750277572207679 ) ) ;
#13854 = EDGE_CURVE ( 'NONE', #45747, #161618, #179956, .T. ) ;
#13855 = ORIENTED_EDGE ( 'NONE', *, *, #119576, .T. ) ;
#13856 = ORIENTED_EDGE ( 'NONE', *, *, #157775, .T. ) ;
#13857 = CARTESIAN_POINT ( 'NONE',  ( 21.11825140030044423, 30.77385224628299198, -252.1797090801663046 ) ) ;
#13858 = VERTEX_POINT ( 'NONE', #97804 ) ;
#13859 = CARTESIAN_POINT ( 'NONE',  ( -23.15000000000000213, -11.74999999998884448, -67.00000000000004263 ) ) ;
#13860 = VERTEX_POINT ( 'NONE', #76983 ) ;
#13861 = DIRECTION ( 'NONE',  ( 0.000000000000000000, -7.086529944415894657E-15, 1.000000000000000000 ) ) ;
#13862 = CARTESIAN_POINT ( 'NONE',  ( -23.15000000000000213, 1.115600667400684642E-11, -100.5000000000000284 ) ) ;
#13863 = EDGE_CURVE ( 'NONE', #212706, #30748, #118076, .T. ) ;
#13864 = CARTESIAN_POINT ( 'NONE',  ( -20.64999999999999858, 2.500000000011154633, -120.7753780772379315 ) ) ;
#13865 = ORIENTED_EDGE ( 'NONE', *, *, #185215, .F. ) ;
#13866 = DIRECTION ( 'NONE',  ( 0.000000000000000000, 0.2617529984164915779, 0.9651348961777187485 ) ) ;
#13867 = EDGE_LOOP ( 'NONE', ( #33172, #224063, #143466, #200363 ) ) ;
#13868 = DIRECTION ( 'NONE',  ( 1.000000000000000000, 0.000000000000000000, 0.000000000000000000 ) ) ;
#13869 = CARTESIAN_POINT ( 'NONE',  ( 18.49713797159812145, 8.901728458076256345, -245.3988228286745823 ) ) ;
#13870 = AXIS2_PLACEMENT_3D ( 'NONE', #130521, #117070, #90100 ) ;
#13871 = VERTEX_POINT ( 'NONE', #117402 ) ;
#13872 = VECTOR ( 'NONE', #253233, 1000.000000000000000 ) ;
#13873 = CYLINDRICAL_SURFACE ( 'NONE', #215067, 0.1000000000000072220 ) ;
#13874 = ORIENTED_EDGE ( 'NONE', *, *, #97856, .F. ) ;
#13877 = VERTEX_POINT ( 'NONE', #95268 ) ;
#13876 = DIRECTION ( 'NONE',  ( 0.000000000000000000, -1.000000000000000000, 0.000000000000000000 ) ) ;
#13875 = DIRECTION ( 'NONE',  ( 0.000000000000000000, 1.000000000000000000, 6.982962677686266711E-15 ) ) ;
#13878 = EDGE_CURVE ( 'NONE', #168134, #39096, #59970, .T. ) ;
#13879 = DIRECTION ( 'NONE',  ( 0.000000000000000000, 0.000000000000000000, 1.000000000000000000 ) ) ;
#13880 = ORIENTED_EDGE ( 'NONE', *, *, #46792, .F. ) ;
#13881 = ORIENTED_EDGE ( 'NONE', *, *, #116126, .T. ) ;
#13882 = VECTOR ( 'NONE', #129686, 1000.000000000000000 ) ;
#13883 = CIRCLE ( 'NONE', #43111, 0.1000000000000008799 ) ;
#13884 = CARTESIAN_POINT ( 'NONE',  ( 22.39999999999999503, -5.963111948670274387E-16, 7.790779598373379855 ) ) ;
#13885 = VERTEX_POINT ( 'NONE', #20899 ) ;
#13886 = LINE ( 'NONE', #157269, #234977 ) ;
#13887 = PLANE ( 'NONE',  #5492 ) ;
#13888 = CARTESIAN_POINT ( 'NONE',  ( 21.14999999999999858, 11.75000000001116263, -33.60000000000000142 ) ) ;
#13889 = FACE_OUTER_BOUND ( 'NONE', #183758, .T. ) ;
#13890 = AXIS2_PLACEMENT_3D ( 'NONE', #242404, #182461, #59901 ) ;
#13891 = B_SPLINE_CURVE_WITH_KNOTS ( 'NONE', 3,
 ( #45735, #249096, #130401, #146116 ),
 .UNSPECIFIED., .F., .F.,
 ( 4, 4 ),
 ( 0.000000000000000000, 0.001767853679387101484 ),
 .UNSPECIFIED. ) ;
#13892 = CARTESIAN_POINT ( 'NONE',  ( 20.94999999999999574, -11.64999999998883595, -36.39999999999999858 ) ) ;
#13893 = AXIS2_PLACEMENT_3D ( 'NONE', #148949, #49826, #44707 ) ;
#13894 = ORIENTED_EDGE ( 'NONE', *, *, #25148, .F. ) ;
#13895 = AXIS2_PLACEMENT_3D ( 'NONE', #112720, #154449, #232680 ) ;
#13896 = VECTOR ( 'NONE', #22126, 1000.000000000000000 ) ;
#13897 = CARTESIAN_POINT ( 'NONE',  ( -16.93970660449832621, 44.02061140864920930, -235.2815329157306508 ) ) ;
#13898 = DIRECTION ( 'NONE',  ( 1.000000000000000000, 0.000000000000000000, 0.000000000000000000 ) ) ;
#13900 = CARTESIAN_POINT ( 'NONE',  ( 21.05000000000000071, 1.115625160336667635E-11, -65.00000000000000000 ) ) ;
#13899 = AXIS2_PLACEMENT_3D ( 'NONE', #13633, #256029, #38339 ) ;
#13901 = ORIENTED_EDGE ( 'NONE', *, *, #175378, .F. ) ;
#13902 = CARTESIAN_POINT ( 'NONE',  ( -21.65000000000000213, 44.22674245267958781, -235.2580479164738279 ) ) ;
#13903 = ORIENTED_EDGE ( 'NONE', *, *, #44385, .F. ) ;
#13904 = CARTESIAN_POINT ( 'NONE',  ( 23.15000000000000213, -4.735542975717121905, -233.2463119243910796 ) ) ;
#13906 = ORIENTED_EDGE ( 'NONE', *, *, #19128, .F. ) ;
#13905 = AXIS2_PLACEMENT_3D ( 'NONE', #122932, #88592, #202463 ) ;
#13907 = DIRECTION ( 'NONE',  ( 0.000000000000000000, -1.000000000000000000, 0.000000000000000000 ) ) ;
#13908 = DIRECTION ( 'NONE',  ( 1.000000000000000000, 0.000000000000000000, 0.000000000000000000 ) ) ;
#13910 = ORIENTED_EDGE ( 'NONE', *, *, #84486, .T. ) ;
#13909 = DIRECTION ( 'NONE',  ( 0.000000000000000000, 0.000000000000000000, -1.000000000000000000 ) ) ;
#13911 = CARTESIAN_POINT ( 'NONE',  ( 20.27550659511088682, 66.78395627750275310, -60.27310748452438816 ) ) ;
#13912 = VERTEX_POINT ( 'NONE', #194396 ) ;
#13913 = VECTOR ( 'NONE', #11832, 1000.000000000000000 ) ;
#13914 = CARTESIAN_POINT ( 'NONE',  ( 20.94999999999999929, 74.16465844978745281, -91.46795619196133487 ) ) ;
#13915 = CIRCLE ( 'NONE', #72195, 0.09999999999998898659 ) ;
#13916 = EDGE_CURVE ( 'NONE', #16660, #90469, #93331, .T. ) ;
#13917 = CYLINDRICAL_SURFACE ( 'NONE', #2013, 0.09999999999999939493 ) ;
#13918 = ORIENTED_EDGE ( 'NONE', *, *, #193548, .T. ) ;
#13919 = CIRCLE ( 'NONE', #159665, 0.1000000000000013933 ) ;
#13920 = LINE ( 'NONE', #94720, #159953 ) ;
#13921 = CARTESIAN_POINT ( 'NONE',  ( -12.25000000000000178, 9.850000000011133849, -50.25000000000000711 ) ) ;
#13922 = ORIENTED_EDGE ( 'NONE', *, *, #93140, .T. ) ;
#13923 = CYLINDRICAL_SURFACE ( 'NONE', #94986, 0.1000000000000052097 ) ;
#13924 = CIRCLE ( 'NONE', #26403, 0.09999999999998898659 ) ;
#13925 = EDGE_LOOP ( 'NONE', ( #12075, #85767, #208517, #83066 ) ) ;
#13926 = AXIS2_PLACEMENT_3D ( 'NONE', #234408, #134027, #86224 ) ;
#13927 = AXIS2_PLACEMENT_3D ( 'NONE', #46887, #147286, #126439 ) ;
#13928 = CARTESIAN_POINT ( 'NONE',  ( 18.59999999999999432, -1.162701749938011453, -8.099999999999999645 ) ) ;
#13929 = CIRCLE ( 'NONE', #59873, 0.09999999999999939493 ) ;
#13930 = DIRECTION ( 'NONE',  ( 0.000000000000000000, 0.000000000000000000, -1.000000000000000000 ) ) ;
#13931 = EDGE_CURVE ( 'NONE', #168616, #129923, #101685, .T. ) ;
#13932 = EDGE_CURVE ( 'NONE', #156170, #142842, #75720, .T. ) ;
#13934 = VERTEX_POINT ( 'NONE', #80818 ) ;
#13933 = DIRECTION ( 'NONE',  ( -0.000000000000000000, 0.000000000000000000, 1.000000000000000000 ) ) ;
#13935 = CARTESIAN_POINT ( 'NONE',  ( -21.05000000000000071, 1.115600667400684642E-11, -167.5000000000000284 ) ) ;
#13936 = DIRECTION ( 'NONE',  ( 0.000000000000000000, -1.000000000000000000, 0.000000000000000000 ) ) ;
#13937 = DIRECTION ( 'NONE',  ( -1.000000000000000000, 0.000000000000000000, 0.000000000000000000 ) ) ;
#13939 = CARTESIAN_POINT ( 'NONE',  ( -15.06720934482788010, 66.58230930894843880, -51.38150678775980396 ) ) ;
#13938 = DIRECTION ( 'NONE',  ( 1.836970198721029934E-16, -1.000000000000000000, -0.000000000000000000 ) ) ;
#13940 = DIRECTION ( 'NONE',  ( 0.000000000000000000, 0.000000000000000000, -1.000000000000000000 ) ) ;
#13941 = DIRECTION ( 'NONE',  ( -2.915501640297154283E-16, 0.9770955615653317272, 0.2128009952263596460 ) ) ;
#13943 = EDGE_CURVE ( 'NONE', #46904, #1689, #218212, .T. ) ;
#13942 = AXIS2_PLACEMENT_3D ( 'NONE', #57140, #118440, #218791 ) ;
#13944 = DIRECTION ( 'NONE',  ( 0.000000000000000000, 0.000000000000000000, -1.000000000000000000 ) ) ;
#13945 = CONICAL_SURFACE ( 'NONE', #176281, 7.750000000000034639, 0.7853981633974531640 ) ;
#13946 = CARTESIAN_POINT ( 'NONE',  ( -23.25000000000000000, 52.91185528119410009, -244.1460391050142960 ) ) ;
#13947 = AXIS2_PLACEMENT_3D ( 'NONE', #171696, #214623, #116825 ) ;
#13948 = AXIS2_PLACEMENT_3D ( 'NONE', #98544, #115583, #94734 ) ;
#13949 = ORIENTED_EDGE ( 'NONE', *, *, #164570, .F. ) ;
#13950 = ORIENTED_EDGE ( 'NONE', *, *, #252491, .F. ) ;
#13951 = EDGE_CURVE ( 'NONE', #43638, #54225, #251552, .T. ) ;
#13952 = DIRECTION ( 'NONE',  ( 0.000000000000000000, 0.9651348961777157509, -0.2617529984165031243 ) ) ;
#13955 = EDGE_LOOP ( 'NONE', ( #62810, #164642, #41602, #51287 ) ) ;
#13954 = EDGE_CURVE ( 'NONE', #88476, #128875, #226604, .T. ) ;
#13953 = LINE ( 'NONE', #249988, #154408 ) ;
#13956 = ORIENTED_EDGE ( 'NONE', *, *, #69339, .T. ) ;
#13957 = CARTESIAN_POINT ( 'NONE',  ( -18.59999999999999787, 77.83585931145498193, -24.51866831572578320 ) ) ;
#13958 = ORIENTED_EDGE ( 'NONE', *, *, #226682, .F. ) ;
#13959 = SPHERICAL_SURFACE ( 'NONE', #80100, 0.1000000000000000056 ) ;
#13960 = EDGE_CURVE ( 'NONE', #224235, #92271, #196928, .T. ) ;
#13961 = VERTEX_POINT ( 'NONE', #161686 ) ;
#13962 = EDGE_CURVE ( 'NONE', #142512, #204451, #243542, .T. ) ;
#13963 = CARTESIAN_POINT ( 'NONE',  ( 23.14999999999999858, 76.00000000001190870, -103.0231074845243029 ) ) ;
#13965 = ORIENTED_EDGE ( 'NONE', *, *, #196357, .T. ) ;
#13964 = EDGE_LOOP ( 'NONE', ( #3704, #39307, #23126, #102271 ) ) ;
#13966 = EDGE_LOOP ( 'NONE', ( #217262, #248498, #200725 ) ) ;
#13967 = ORIENTED_EDGE ( 'NONE', *, *, #247179, .F. ) ;
#13968 = VERTEX_POINT ( 'NONE', #106808 ) ;
#13969 = DIRECTION ( 'NONE',  ( 0.000000000000000000, 0.000000000000000000, -1.000000000000000000 ) ) ;
#13970 = CARTESIAN_POINT ( 'NONE',  ( 21.05933563467872105, 43.40235695101777225, -234.7786682115255985 ) ) ;
#13971 = CIRCLE ( 'NONE', #5560, 0.09999999999999939493 ) ;
#13972 = CARTESIAN_POINT ( 'NONE',  ( -15.39126916658603150, 9.389571634557567492, -185.3176407123691547 ) ) ;
#13974 = ORIENTED_EDGE ( 'NONE', *, *, #95592, .T. ) ;
#13973 = PLANE ( 'NONE',  #141716 ) ;
#13975 = CARTESIAN_POINT ( 'NONE',  ( -18.40000000000000213, 16.35463830854640932, -222.1788605317357224 ) ) ;
#13976 = DIRECTION ( 'NONE',  ( 0.000000000000000000, -1.000000000000000000, 0.000000000000000000 ) ) ;
#13978 = ORIENTED_EDGE ( 'NONE', *, *, #65378, .T. ) ;
#13977 = CARTESIAN_POINT ( 'NONE',  ( -21.14999999999999858, 0.000000000000000000, 6.540656951701240729 ) ) ;
#13979 = DIRECTION ( 'NONE',  ( -1.000000000000000000, 0.000000000000000000, 0.000000000000000000 ) ) ;
#13980 = ORIENTED_EDGE ( 'NONE', *, *, #65709, .T. ) ;
#13983 = EDGE_CURVE ( 'NONE', #248236, #192885, #135201, .T. ) ;
#13982 = VERTEX_POINT ( 'NONE', #6432 ) ;
#13981 = DIRECTION ( 'NONE',  ( 0.000000000000000000, 0.000000000000000000, -1.000000000000000000 ) ) ;
#13984 = CARTESIAN_POINT ( 'NONE',  ( 20.94999999999999929, 76.00000000001142553, -36.02310748452432421 ) ) ;
#13985 = CARTESIAN_POINT ( 'NONE',  ( -16.89318236219976654, 9.951535257886286345, -113.1448703678941854 ) ) ;
#13986 = ORIENTED_EDGE ( 'NONE', *, *, #131058, .F. ) ;
#13988 = CARTESIAN_POINT ( 'NONE',  ( -18.44448725179913851, -9.490081715472173940, -140.6289602940625514 ) ) ;
#13987 = CARTESIAN_POINT ( 'NONE',  ( 23.14999999999999858, 76.00000000001156764, -56.64810748452432421 ) ) ;
#13989 = CYLINDRICAL_SURFACE ( 'NONE', #184957, 0.09999999999999939493 ) ;
#13990 = AXIS2_PLACEMENT_3D ( 'NONE', #123806, #139494, #144627 ) ;
#13991 = FACE_OUTER_BOUND ( 'NONE', #202479, .T. ) ;
#13992 = CARTESIAN_POINT ( 'NONE',  ( 20.95512820512820440, 10.62384868372303615, -41.16491356908760935 ) ) ;
#13993 = VERTEX_POINT ( 'NONE', #205917 ) ;
#13995 = ORIENTED_EDGE ( 'NONE', *, *, #15006, .T. ) ;
#13994 = AXIS2_PLACEMENT_3D ( 'NONE', #58863, #113726, #39360 ) ;
#13996 = EDGE_CURVE ( 'NONE', #205, #123531, #202080, .T. ) ;
#13997 = DIRECTION ( 'NONE',  ( 1.186688945009010077E-16, 0.4088369013363281068, -0.9126074666063770380 ) ) ;
#13998 = DIRECTION ( 'NONE',  ( 0.000000000000000000, -0.5273008465187821736, 0.8496786552930323255 ) ) ;
#13999 = ORIENTED_EDGE ( 'NONE', *, *, #107347, .T. ) ;
#14000 = CARTESIAN_POINT ( 'NONE',  ( 23.15000000000000213, -8.999999999988842703, -191.6060308773475072 ) ) ;
#14001 = EDGE_LOOP ( 'NONE', ( #201575, #62425, #67462 ) ) ;
#14002 = CARTESIAN_POINT ( 'NONE',  ( -22.60000000000094289, 0.1008583691096561347, -55.25043287651063650 ) ) ;
#14003 = DIRECTION ( 'NONE',  ( 0.000000000000000000, -0.1455152366551522025, -0.9893560106964505163 ) ) ;
#14004 = CARTESIAN_POINT ( 'NONE',  ( -22.39999999999999858, 0.1000000000111554016, -92.70922040162662370 ) ) ;
#14005 = VERTEX_POINT ( 'NONE', #126384 ) ;
#14006 = CIRCLE ( 'NONE', #72460, 11.90000000000000036 ) ;
#14007 = DIRECTION ( 'NONE',  ( 1.000000000000000000, 0.000000000000000000, 0.000000000000000000 ) ) ;
#14008 =( LENGTH_UNIT ( ) NAMED_UNIT ( * ) SI_UNIT ( .MILLI., .METRE. ) );
#14009 = EDGE_CURVE ( 'NONE', #205018, #971, #81033, .T. ) ;
#14010 = AXIS2_PLACEMENT_3D ( 'NONE', #72777, #251370, #34934 ) ;
#14011 = EDGE_CURVE ( 'NONE', #151221, #34916, #255966, .T. ) ;
#14012 = ORIENTED_EDGE ( 'NONE', *, *, #169781, .F. ) ;
#14013 = VERTEX_POINT ( 'NONE', #105501 ) ;
#14014 = AXIS2_PLACEMENT_3D ( 'NONE', #139716, #161895, #4071 ) ;
#14015 = ORIENTED_EDGE ( 'NONE', *, *, #123473, .T. ) ;
#14016 = CIRCLE ( 'NONE', #172641, 0.09999999999999939493 ) ;
#14017 = DIRECTION ( 'NONE',  ( 1.000000000000000000, 0.000000000000000000, 0.000000000000000000 ) ) ;
#14018 = FACE_OUTER_BOUND ( 'NONE', #46852, .T. ) ;
#14019 = CARTESIAN_POINT ( 'NONE',  ( 20.04142135623730070, 64.35000000001150511, -48.17310748452440095 ) ) ;
#14020 = CARTESIAN_POINT ( 'NONE',  ( 13.54577453029515688, 66.54939790392350574, -118.0792115214276947 ) ) ;
#14021 = EDGE_CURVE ( 'NONE', #98769, #89222, #87239, .T. ) ;
#14023 = CARTESIAN_POINT ( 'NONE',  ( -21.14999999999994174, 74.94272479589878344, -3.023107484524792277 ) ) ;
#14022 = DIRECTION ( 'NONE',  ( 0.000000000000000000, 1.776356839400155604E-15, 1.000000000000000000 ) ) ;
#14025 = VERTEX_POINT ( 'NONE', #182532 ) ;
#14024 = CARTESIAN_POINT ( 'NONE',  ( -18.40000000000000213, 16.64129698264336099, -222.1941556740511032 ) ) ;
#14026 = DIRECTION ( 'NONE',  ( 0.000000000000000000, -0.4088369013363281623, 0.9126074666063771490 ) ) ;
#14027 = ORIENTED_EDGE ( 'NONE', *, *, #233482, .F. ) ;
#14028 = CARTESIAN_POINT ( 'NONE',  ( -15.06774609480955363, 9.417651958852161442, -149.3587873924404619 ) ) ;
#14029 = ORIENTED_EDGE ( 'NONE', *, *, #104167, .T. ) ;
#14030 = ORIENTED_EDGE ( 'NONE', *, *, #60971, .F. ) ;
#14031 = DIRECTION ( 'NONE',  ( -0.000000000000000000, 0.9876197685951279004, -0.1568667991644694115 ) ) ;
#14033 = AXIS2_PLACEMENT_3D ( 'NONE', #115648, #76507, #12725 ) ;
#14032 = FACE_OUTER_BOUND ( 'NONE', #121052, .T. ) ;
#14035 = EDGE_CURVE ( 'NONE', #114879, #227981, #139288, .T. ) ;
#14034 = CARTESIAN_POINT ( 'NONE',  ( -16.86337532320262156, 66.02003279578721617, -56.97203195350720506 ) ) ;
#14036 = AXIS2_PLACEMENT_3D ( 'NONE', #160201, #98879, #251884 ) ;
#14037 = EDGE_CURVE ( 'NONE', #230288, #101170, #160191, .T. ) ;
#14038 = CARTESIAN_POINT ( 'NONE',  ( -20.94999999999999929, 87.39257802171779588, -133.4491579046922709 ) ) ;
#14039 = CIRCLE ( 'NONE', #197167, 0.09999999999999939493 ) ;
#14040 = CARTESIAN_POINT ( 'NONE',  ( 20.89878130938411616, 18.40663661316795441, -236.9846611508999388 ) ) ;
#14041 = ORIENTED_EDGE ( 'NONE', *, *, #100464, .F. ) ;
#14042 = ORIENTED_EDGE ( 'NONE', *, *, #90504, .F. ) ;
#14043 = ADVANCED_FACE ( 'NONE', ( #3871 ), #45568, .T. ) ;
#14044 = CIRCLE ( 'NONE', #159779, 0.1000000000000026007 ) ;
#14045 = DIRECTION ( 'NONE',  ( 0.000000000000000000, -0.8814952561688428334, 0.4721928772777350680 ) ) ;
#14046 = ORIENTED_EDGE ( 'NONE', *, *, #174401, .F. ) ;
#14047 = LINE ( 'NONE', #70181, #144414 ) ;
#14048 = CARTESIAN_POINT ( 'NONE',  ( -21.44999999999999929, 7.249999999999999112, -21.15000000000000213 ) ) ;
#14049 = ORIENTED_EDGE ( 'NONE', *, *, #10415, .F. ) ;
#14050 = CARTESIAN_POINT ( 'NONE',  ( 21.05000000000000071, 16.53042682864194290, -240.8665456014163624 ) ) ;
#14051 = CARTESIAN_POINT ( 'NONE',  ( 20.90000000000000213, 7.973296578895943121, -1.410778198689825347 ) ) ;
#14052 = CARTESIAN_POINT ( 'NONE',  ( -18.43707690579161351, -9.682403433465239573, -207.6568433774127129 ) ) ;
#14053 = FACE_OUTER_BOUND ( 'NONE', #92197, .T. ) ;
#14054 = ORIENTED_EDGE ( 'NONE', *, *, #75636, .F. ) ;
#14055 = AXIS2_PLACEMENT_3D ( 'NONE', #134334, #135623, #211329 ) ;
#14056 = AXIS2_PLACEMENT_3D ( 'NONE', #77047, #222973, #204686 ) ;
#14057 = AXIS2_PLACEMENT_3D ( 'NONE', #196592, #214877, #97468 ) ;
#14058 = TOROIDAL_SURFACE ( 'NONE', #159788, 12.77500000000000036, 0.1000000000000000056 ) ;
#14059 = CYLINDRICAL_SURFACE ( 'NONE', #141824, 0.09999999999998898659 ) ;
#14060 = DIRECTION ( 'NONE',  ( 1.186688945009010077E-16, 1.000000000000000000, 6.982962677686266711E-15 ) ) ;
#14061 = CARTESIAN_POINT ( 'NONE',  ( -20.94999999999999929, 43.44873802792533724, -245.1397081572968659 ) ) ;
#14062 = ORIENTED_EDGE ( 'NONE', *, *, #23509, .F. ) ;
#14063 = CARTESIAN_POINT ( 'NONE',  ( -23.15000000000000213, 64.35000000001150511, -48.17310748452440095 ) ) ;
#14064 = ORIENTED_EDGE ( 'NONE', *, *, #27094, .F. ) ;
#14065 = ADVANCED_FACE ( 'NONE', ( #22173 ), #43009, .T. ) ;
#14066 = DIRECTION ( 'NONE',  ( 0.000000000000000000, 0.8814952561688476074, -0.4721928772777262417 ) ) ;
#14067 = EDGE_CURVE ( 'NONE', #212843, #46813, #143377, .T. ) ;
#14068 = CYLINDRICAL_SURFACE ( 'NONE', #41907, 4.049999999999994493 ) ;
#14069 = CARTESIAN_POINT ( 'NONE',  ( -23.15000000000000213, -8.999999999988844479, -158.1060308773475924 ) ) ;
#14070 = DIRECTION ( 'NONE',  ( -1.000000000000000000, -0.000000000000000000, -0.000000000000000000 ) ) ;
#14071 = DIRECTION ( 'NONE',  ( 0.000000000000000000, 0.8814952561688430555, -0.4721928772777346239 ) ) ;
#14072 = LINE ( 'NONE', #191446, #115381 ) ;
#14073 = EDGE_LOOP ( 'NONE', ( #160139, #57208, #110758, #102427, #124497 ) ) ;
#14074 = CARTESIAN_POINT ( 'NONE',  ( -16.93658211146646408, 66.00589133767087446, -123.9274025544800537 ) ) ;
#14075 = DIRECTION ( 'NONE',  ( -0.000000000000000000, -1.000000000000000000, -6.982962677686266711E-15 ) ) ;
#14076 = CARTESIAN_POINT ( 'NONE',  ( -21.05000000000000071, -11.48912529306490349, -103.5000000000000426 ) ) ;
#14078 = TOROIDAL_SURFACE ( 'NONE', #88859, 0.2000000000000000111, 0.1000000000000000056 ) ;
#14077 = LINE ( 'NONE', #93597, #13360 ) ;
#14079 = EDGE_CURVE ( 'NONE', #190074, #48902, #230928, .T. ) ;
#14080 = CIRCLE ( 'NONE', #118107, 0.09999999999999817368 ) ;
#14081 = CARTESIAN_POINT ( 'NONE',  ( -13.39999999999994529, 67.75000000001118394, -16.98168612828748181 ) ) ;
#14082 = VERTEX_POINT ( 'NONE', #104233 ) ;
#14083 = VERTEX_POINT ( 'NONE', #5118 ) ;
#14084 = DIRECTION ( 'NONE',  ( -1.000000000000000000, -0.000000000000000000, 0.000000000000000000 ) ) ;
#14085 = CIRCLE ( 'NONE', #101506, 0.09999999999999939493 ) ;
#14086 = DIRECTION ( 'NONE',  ( 1.000000000000000000, 0.000000000000000000, 0.000000000000000000 ) ) ;
#14087 = CYLINDRICAL_SURFACE ( 'NONE', #1887, 0.1000000000000001443 ) ;
#14088 = DIRECTION ( 'NONE',  ( 1.000000000000000000, 0.000000000000000000, 0.000000000000000000 ) ) ;
#14089 = CARTESIAN_POINT ( 'NONE',  ( 18.54999999999999716, 22.97806745954237329, -230.9350634111225986 ) ) ;
#14090 = ORIENTED_EDGE ( 'NONE', *, *, #88674, .T. ) ;
#14091 = CARTESIAN_POINT ( 'NONE',  ( -18.59999999999999787, 64.25000000001260503, -191.3731074845244393 ) ) ;
#14092 = CIRCLE ( 'NONE', #159829, 0.09999999999999883982 ) ;
#14093 = CONTEXT_DEPENDENT_SHAPE_REPRESENTATION ( #135754, #118328 ) ;
#14095 = VECTOR ( 'NONE', #105923, 999.9999999999998863 ) ;
#14094 = CARTESIAN_POINT ( 'NONE',  ( -20.54999999999999716, 68.28002175382172823, -222.4371999040225774 ) ) ;
#14096 = ORIENTED_EDGE ( 'NONE', *, *, #108087, .T. ) ;
#14097 = DIRECTION ( 'NONE',  ( 1.000000000000000000, 0.000000000000000000, 0.000000000000000000 ) ) ;
#14098 = CIRCLE ( 'NONE', #47379, 0.09999999999998464284 ) ;
#14099 = AXIS2_PLACEMENT_3D ( 'NONE', #88988, #166012, #168599 ) ;
#14100 = PRODUCT ( 'Injection Molded Chain Links 14', 'Injection Molded Chain Links 14', '', ( #218994 ) ) ;
#14101 = DIRECTION ( 'NONE',  ( -0.000000000000000000, -0.8660254037844459241, -0.4999999999999873990 ) ) ;
#14102 = EDGE_CURVE ( 'NONE', #176594, #360, #168594, .T. ) ;
#14103 = CIRCLE ( 'NONE', #130784, 0.09999999999998898659 ) ;
#14104 = ORIENTED_EDGE ( 'NONE', *, *, #134158, .T. ) ;
#14105 = DIRECTION ( 'NONE',  ( -1.000000000000000000, 3.151514657663852580E-16, -8.547182517843351137E-17 ) ) ;
#14106 = EDGE_CURVE ( 'NONE', #73243, #14224, #161510, .T. ) ;
#14107 = ORIENTED_EDGE ( 'NONE', *, *, #9217, .T. ) ;
#14108 = DIRECTION ( 'NONE',  ( 0.000000000000000000, 6.982962677686266711E-15, -1.000000000000000000 ) ) ;
#14109 = FACE_OUTER_BOUND ( 'NONE', #16819, .T. ) ;
#14111 = AXIS2_PLACEMENT_3D ( 'NONE', #18227, #97722, #256773 ) ;
#14110 = DIRECTION ( 'NONE',  ( 1.000000000000000000, 0.000000000000000000, 0.000000000000000000 ) ) ;
#14112 = DIRECTION ( 'NONE',  ( 0.000000000000000000, -0.9579639084728132081, -0.2868887416116073230 ) ) ;
#14113 = CYLINDRICAL_SURFACE ( 'NONE', #90535, 0.1000000000000028644 ) ;
#14115 = EDGE_CURVE ( 'NONE', #16570, #207709, #193496, .T. ) ;
#14114 = DIRECTION ( 'NONE',  ( 1.000000000000000000, 0.000000000000000000, 0.000000000000000000 ) ) ;
#14116 = DIRECTION ( 'NONE',  ( 0.000000000000000000, 0.000000000000000000, 1.000000000000000000 ) ) ;
#14117 = CARTESIAN_POINT ( 'NONE',  ( -21.14999999999999858, 0.09779029131994770863, -27.24218538952388613 ) ) ;
#14119 = DIRECTION ( 'NONE',  ( -1.000000000000000000, 0.000000000000000000, 0.000000000000000000 ) ) ;
#14118 = DIRECTION ( 'NONE',  ( 0.000000000000000000, -0.8741572761215355980, 0.4856429311786357172 ) ) ;
#14120 = CIRCLE ( 'NONE', #155774, 0.09999999999998898659 ) ;
#14121 = DIRECTION ( 'NONE',  ( 0.000000000000000000, 1.000000000000000000, 0.000000000000000000 ) ) ;
#14122 = EDGE_CURVE ( 'NONE', #139949, #25924, #245051, .T. ) ;
#14123 = CARTESIAN_POINT ( 'NONE',  ( 21.13461538461537614, 22.12278086513518005, -231.6846110910352081 ) ) ;
#14124 = CARTESIAN_POINT ( 'NONE',  ( -21.64999999999999858, 7.250000000011148416, -188.6499999999999488 ) ) ;
#14125 = ORIENTED_EDGE ( 'NONE', *, *, #73612, .F. ) ;
#14126 = DIRECTION ( 'NONE',  ( 0.000000000000000000, -0.9910827722268055195, -0.1332476588733540468 ) ) ;
#14127 = VECTOR ( 'NONE', #221090, 1000.000000000000000 ) ;
#14128 = DIRECTION ( 'NONE',  ( -1.000000000000000000, 0.000000000000000000, 0.000000000000000000 ) ) ;
#14129 = DIRECTION ( 'NONE',  ( -1.000000000000000000, 0.000000000000000000, 0.000000000000000000 ) ) ;
#14130 = CIRCLE ( 'NONE', #184781, 0.8750000000000007772 ) ;
#14131 = EDGE_CURVE ( 'NONE', #11411, #229722, #225463, .T. ) ;
#14132 = CIRCLE ( 'NONE', #22507, 11.79999999999999716 ) ;
#14134 = EDGE_CURVE ( 'NONE', #37415, #232829, #85303, .T. ) ;
#14133 = ADVANCED_FACE ( 'NONE', ( #88517 ), #250190, .T. ) ;
#14135 = ORIENTED_EDGE ( 'NONE', *, *, #253187, .T. ) ;
#14136 = DIRECTION ( 'NONE',  ( -0.000000000000000000, 0.8660254037844411501, 0.4999999999999956146 ) ) ;
#14137 = DIRECTION ( 'NONE',  ( -4.408576920032447355E-17, 0.1290532225515392262, 0.9916376685811520986 ) ) ;
#14138 = DIRECTION ( 'NONE',  ( 1.000000000000000000, 0.000000000000000000, 0.000000000000000000 ) ) ;
#14139 = ORIENTED_EDGE ( 'NONE', *, *, #3310, .T. ) ;
#14140 = B_SPLINE_CURVE_WITH_KNOTS ( 'NONE', 3,
 ( #107693, #206803, #106391, #28198, #249778, #89408, #189811, #131107, #49003, #67287, #228936, #187257, #248496, #69879, #146805, #128549, #85528, #208105, #230209 ),
 .UNSPECIFIED., .F., .F.,
 ( 4, 3, 3, 3, 3, 3, 4 ),
 ( 1.387778780781445676E-17, 2.646747978908994698E-05, 5.271166642128863382E-05, 9.008788829885137981E-05, 0.0001426648776561022008, 0.0001897378458659801945, 0.0001917382627806380965 ),
 .UNSPECIFIED. ) ;
#14141 = CARTESIAN_POINT ( 'NONE',  ( -18.50000000000000000, 77.83534155023670564, -158.4679561919613491 ) ) ;
#14142 = VERTEX_POINT ( 'NONE', #12885 ) ;
#14143 = CARTESIAN_POINT ( 'NONE',  ( 21.05000000000000426, 6.285166956194035315, -199.7189084715529361 ) ) ;
#14144 = DIRECTION ( 'NONE',  ( -0.000000000000000000, 0.1350103645451876666, 0.9908441862701600211 ) ) ;
#14145 = AXIS2_PLACEMENT_3D ( 'NONE', #96872, #38237, #255933 ) ;
#14147 = ADVANCED_FACE ( 'NONE', ( #128964 ), #147229, .T. ) ;
#14146 =( GEOMETRIC_REPRESENTATION_CONTEXT ( 3 ) GLOBAL_UNCERTAINTY_ASSIGNED_CONTEXT ( ( #255317 ) ) GLOBAL_UNIT_ASSIGNED_CONTEXT ( ( #124534, #146630, #168834 ) ) REPRESENTATION_CONTEXT ( 'NONE', 'WORKASPACE' ) );
#14148 = AXIS2_PLACEMENT_3D ( 'NONE', #51423, #228825, #69759 ) ;
#14149 = ADVANCED_FACE ( 'NONE', ( #226763 ), #49419, .F. ) ;
#14150 = ADVANCED_BREP_SHAPE_REPRESENTATION ( '', ( #189925, #2425 ), #156768 ) ;
#14151 = ORIENTED_EDGE ( 'NONE', *, *, #242061, .F. ) ;
#14152 = CARTESIAN_POINT ( 'NONE',  ( -23.15000000000000213, 21.17283678855157802, -243.7231193059830332 ) ) ;
#14153 = ADVANCED_FACE ( 'NONE', ( #91109 ), #35314, .T. ) ;
#14154 = ORIENTED_EDGE ( 'NONE', *, *, #192563, .T. ) ;
#14155 = LINE ( 'NONE', #254007, #53938 ) ;
#14156 = DIRECTION ( 'NONE',  ( 1.000000000000000000, 0.000000000000000000, 0.000000000000000000 ) ) ;
#14158 = CARTESIAN_POINT ( 'NONE',  ( -18.39999999999999858, 85.60000000001210196, -129.4910380878245633 ) ) ;
#14157 = PRODUCT_DEFINITION_CONTEXT ( 'detailed design', #179206, 'design' ) ;
#14159 = DIRECTION ( 'NONE',  ( -0.000000000000000000, -1.156482317317873105E-15, 1.000000000000000000 ) ) ;
#14160 = DIRECTION ( 'NONE',  ( 0.000000000000000000, 0.9126074666063765939, 0.4088369013363291060 ) ) ;
#14161 = ADVANCED_FACE ( 'NONE', ( #251461 ), #9007, .T. ) ;
#14162 = DIRECTION ( 'NONE',  ( 1.000000000000000000, 0.000000000000000000, 0.000000000000000000 ) ) ;
#14163 = LINE ( 'NONE', #113231, #217553 ) ;
#14164 = DIRECTION ( 'NONE',  ( 0.7071067811865456854, -0.7071067811865493491, -0.000000000000000000 ) ) ;
#14167 = VERTEX_POINT ( 'NONE', #69005 ) ;
#14166 = EDGE_CURVE ( 'NONE', #49960, #235552, #97777, .T. ) ;
#14165 = CARTESIAN_POINT ( 'NONE',  ( 21.04999999999953886, 69.55891531154068730, -103.0053880512149789 ) ) ;
#14169 = CARTESIAN_POINT ( 'NONE',  ( 18.39999999999999503, 61.34848953995435039, -212.6564661897791098 ) ) ;
#14168 = LINE ( 'NONE', #114527, #199504 ) ;
#14170 = ORIENTED_EDGE ( 'NONE', *, *, #139728, .F. ) ;
#14172 = VERTEX_POINT ( 'NONE', #51960 ) ;
#14171 = CARTESIAN_POINT ( 'NONE',  ( -18.59999999999999787, 64.35000000001230092, -157.8731074845244393 ) ) ;
#14173 = ORIENTED_EDGE ( 'NONE', *, *, #57886, .F. ) ;
#14174 = CARTESIAN_POINT ( 'NONE',  ( -16.87036670365549895, 9.989418819312803066, -79.52043988269799968 ) ) ;
#14175 = DIRECTION ( 'NONE',  ( 0.000000000000000000, -1.000000000000000000, 0.000000000000000000 ) ) ;
#14176 = AXIS2_PLACEMENT_3D ( 'NONE', #104242, #24763, #100386 ) ;
#14178 = FACE_OUTER_BOUND ( 'NONE', #104305, .T. ) ;
#14177 = B_SPLINE_CURVE_WITH_KNOTS ( 'NONE', 3,
 ( #199815, #21190, #100652, #180241, #1575, #81107, #160700, #170985, #127963, #147519 ),
 .UNSPECIFIED., .F., .F.,
 ( 4, 3, 3, 4 ),
 ( -2.000561356210515597E-06, 0.000000000000000000, 1.787822682428821068E-05, 4.206475347089863842E-05 ),
 .UNSPECIFIED. ) ;
#14179 = CARTESIAN_POINT ( 'NONE',  ( 18.51997666896852124, -9.392332131518996263, -7.143406187483815728 ) ) ;
#14180 = DIRECTION ( 'NONE',  ( 1.000000000000000000, 0.000000000000000000, 0.000000000000000000 ) ) ;
#14181 = EDGE_CURVE ( 'NONE', #223514, #411, #93522, .T. ) ;
#14182 = FACE_OUTER_BOUND ( 'NONE', #103693, .T. ) ;
#14183 = DIRECTION ( 'NONE',  ( -1.000000000000000000, 0.000000000000000000, -0.000000000000000000 ) ) ;
#14184 = FACE_OUTER_BOUND ( 'NONE', #240436, .T. ) ;
#14185 = EDGE_CURVE ( 'NONE', #109416, #174607, #131120, .T. ) ;
#14186 = VERTEX_POINT ( 'NONE', #229353 ) ;
#14187 = ORIENTED_EDGE ( 'NONE', *, *, #29971, .T. ) ;
#14188 = CARTESIAN_POINT ( 'NONE',  ( 20.94999999999999929, 6.550000000011156231, -79.25000000000004263 ) ) ;
#14189 = AXIS2_PLACEMENT_3D ( 'NONE', #254385, #154080, #178772 ) ;
#14190 = AXIS2_PLACEMENT_3D ( 'NONE', #140799, #121276, #41711 ) ;
#14191 = ORIENTED_EDGE ( 'NONE', *, *, #107034, .T. ) ;
#14192 = CARTESIAN_POINT ( 'NONE',  ( -18.59999999999999787, 6.266619843005246437, -211.3861694115776402 ) ) ;
#14193 = ORIENTED_EDGE ( 'NONE', *, *, #32389, .F. ) ;
#14194 = CARTESIAN_POINT ( 'NONE',  ( 18.37172112093847787, -9.570961652243262563, -40.31673445348319973 ) ) ;
#14195 = CIRCLE ( 'NONE', #26661, 0.2000000000000057288 ) ;
#14196 = FACE_BOUND ( 'NONE', #164128, .T. ) ;
#14197 = DIRECTION ( 'NONE',  ( 0.000000000000000000, 1.156482317317873105E-15, -1.000000000000000000 ) ) ;
#14198 = EDGE_CURVE ( 'NONE', #59994, #152240, #207223, .T. ) ;
#14199 = CARTESIAN_POINT ( 'NONE',  ( -14.00000000000000178, 13.18880795147152440, -215.2702608532411830 ) ) ;
#14200 = CARTESIAN_POINT ( 'NONE',  ( -20.94999999999999929, 79.03091752131670944, -235.9469187808398942 ) ) ;
#14201 = ORIENTED_EDGE ( 'NONE', *, *, #133144, .F. ) ;
#14202 = DIRECTION ( 'NONE',  ( 0.000000000000000000, 0.2617529984164938539, 0.9651348961777183044 ) ) ;
#14203 = DIRECTION ( 'NONE',  ( 1.000000000000000000, 0.000000000000000000, 0.000000000000000000 ) ) ;
#14205 = AXIS2_PLACEMENT_3D ( 'NONE', #78289, #255602, #198242 ) ;
#14204 = CARTESIAN_POINT ( 'NONE',  ( 18.69999999999999929, 2.524878688533307880, -16.24283924587617989 ) ) ;
#14206 = CARTESIAN_POINT ( 'NONE',  ( 20.73486653747090003, 7.250000000000026645, -20.85000000000000142 ) ) ;
#14207 = ORIENTED_EDGE ( 'NONE', *, *, #84055, .T. ) ;
#14209 = CARTESIAN_POINT ( 'NONE',  ( 18.39999999999998082, 11.47316190337362585, -109.7500000000000284 ) ) ;
#14208 = DIRECTION ( 'NONE',  ( 1.000000000000000000, 0.000000000000000000, 0.000000000000000000 ) ) ;
#14211 = VERTEX_POINT ( 'NONE', #14169 ) ;
#14210 = AXIS2_PLACEMENT_3D ( 'NONE', #67291, #146812, #226342 ) ;
#14214 = ORIENTED_EDGE ( 'NONE', *, *, #18917, .T. ) ;
#14213 = CARTESIAN_POINT ( 'NONE',  ( -20.94999999999999929, 1.851028230152016674, -145.6539132694225032 ) ) ;
#14212 = DIRECTION ( 'NONE',  ( -1.000000000000000000, 0.000000000000000000, -0.000000000000000000 ) ) ;
#14215 = CARTESIAN_POINT ( 'NONE',  ( -20.85000000000000142, -1.164121893230052995, -74.71484808557160306 ) ) ;
#14216 = AXIS2_PLACEMENT_3D ( 'NONE', #30884, #50384, #32162 ) ;
#14217 = CIRCLE ( 'NONE', #180594, 0.1999999999999999833 ) ;
#14218 = CARTESIAN_POINT ( 'NONE',  ( -22.48660254037843131, 64.25000000001163869, -69.57310748452438531 ) ) ;
#14219 = VERTEX_POINT ( 'NONE', #211062 ) ;
#14220 = DIRECTION ( 'NONE',  ( -1.000000000000000000, -0.000000000000000000, 0.000000000000000000 ) ) ;
#14221 = DIRECTION ( 'NONE',  ( -1.000000000000000000, 0.000000000000000000, 0.000000000000000000 ) ) ;
#14222 = FACE_OUTER_BOUND ( 'NONE', #103721, .T. ) ;
#14224 = VERTEX_POINT ( 'NONE', #209780 ) ;
#14223 = CARTESIAN_POINT ( 'NONE',  ( -18.59999999999999787, 64.35000000001161879, -62.50830171387039513 ) ) ;
#14225 = AXIS2_PLACEMENT_3D ( 'NONE', #48936, #188450, #124638 ) ;
#14226 = AXIS2_PLACEMENT_3D ( 'NONE', #218396, #181869, #21522 ) ;
#14227 = AXIS2_PLACEMENT_3D ( 'NONE', #112290, #113557, #251782 ) ;
#14228 = ORIENTED_EDGE ( 'NONE', *, *, #67657, .F. ) ;
#14229 = DIRECTION ( 'NONE',  ( 1.000000000000000000, 0.000000000000000000, 0.000000000000000000 ) ) ;
#14230 = CARTESIAN_POINT ( 'NONE',  ( 18.39999999999999858, -9.519327731081279609, -73.97297637655938729 ) ) ;
#14231 = CARTESIAN_POINT ( 'NONE',  ( -23.15000000000000213, 1.115600667400684642E-11, -100.5000000000000426 ) ) ;
#14232 = DIRECTION ( 'NONE',  ( 6.938893903906854773E-14, -0.5273008465188072647, 0.8496786552930167824 ) ) ;
#14233 = ORIENTED_EDGE ( 'NONE', *, *, #143097, .F. ) ;
#14234 = CARTESIAN_POINT ( 'NONE',  ( -23.15000000000000213, -4.756823075239758225, -233.1486023682345490 ) ) ;
#14235 = DIRECTION ( 'NONE',  ( 0.000000000000000000, 0.000000000000000000, -1.000000000000000000 ) ) ;
#14236 = DIRECTION ( 'NONE',  ( 1.000000000000000000, 0.000000000000000000, 0.000000000000000000 ) ) ;
#14237 = VERTEX_POINT ( 'NONE', #31181 ) ;
#14238 = CARTESIAN_POINT ( 'NONE',  ( 20.58091095332318332, 60.73084122572070243, -225.3693818331944669 ) ) ;
#14239 = AXIS2_PLACEMENT_3D ( 'NONE', #196980, #95329, #236120 ) ;
#14240 = AXIS2_PLACEMENT_3D ( 'NONE', #121610, #240257, #23795 ) ;
#14242 = TOROIDAL_SURFACE ( 'NONE', #230712, 0.4000000000000005773, 0.1000000000000000056 ) ;
#14241 = CARTESIAN_POINT ( 'NONE',  ( -21.44999999999999929, 7.150000000000000355, -21.25000000000000000 ) ) ;
#14243 = EDGE_CURVE ( 'NONE', #63364, #229182, #93131, .T. ) ;
#14244 = ORIENTED_EDGE ( 'NONE', *, *, #39434, .T. ) ;
#14245 = CARTESIAN_POINT ( 'NONE',  ( -18.59999999999999787, 11.65000000001115232, -40.51480577065400013 ) ) ;
#14246 = DIRECTION ( 'NONE',  ( 0.000000000000000000, 6.982962677686266711E-15, -1.000000000000000000 ) ) ;
#14247 = ORIENTED_EDGE ( 'NONE', *, *, #129134, .T. ) ;
#14248 = ORIENTED_EDGE ( 'NONE', *, *, #172282, .T. ) ;
#14249 = LINE ( 'NONE', #232008, #237371 ) ;
#14250 = ORIENTED_EDGE ( 'NONE', *, *, #51312, .F. ) ;
#14252 = EDGE_LOOP ( 'NONE', ( #214428, #94687, #23233, #234168 ) ) ;
#14251 = DIRECTION ( 'NONE',  ( 2.952720810173289112E-16, 0.4088369013363278848, -0.9126074666063770380 ) ) ;
#14253 = ADVANCED_FACE ( 'NONE', ( #190221 ), #185112, .T. ) ;
#14254 = EDGE_CURVE ( 'NONE', #20178, #33168, #247651, .T. ) ;
#14257 = ORIENTED_EDGE ( 'NONE', *, *, #42522, .T. ) ;
#14256 = VERTEX_POINT ( 'NONE', #137918 ) ;
#14255 = CARTESIAN_POINT ( 'NONE',  ( 21.51976009735019346, 60.56174996242723552, -234.0462932889414560 ) ) ;
#14258 = CIRCLE ( 'NONE', #222497, 0.09999999999999022171 ) ;
#14259 = AXIS2_PLACEMENT_3D ( 'NONE', #1953, #5802, #222272 ) ;
#14260 = DIRECTION ( 'NONE',  ( 0.000000000000000000, -0.01562499999999307672, 0.9998779222360100194 ) ) ;
#14261 = CARTESIAN_POINT ( 'NONE',  ( -21.05000000000000071, -1.835341550213257733, -45.05515129256298223 ) ) ;
#14262 = CARTESIAN_POINT ( 'NONE',  ( -18.50000000000000000, 63.79568978998910467, -212.8021059378898485 ) ) ;
#14263 = CIRCLE ( 'NONE', #189225, 0.09999999999998898659 ) ;
#14264 = DIRECTION ( 'NONE',  ( 0.000000000000000000, 0.000000000000000000, 1.000000000000000000 ) ) ;
#14265 = DIRECTION ( 'NONE',  ( 0.000000000000000000, 0.000000000000000000, 1.000000000000000000 ) ) ;
#14266 = CARTESIAN_POINT ( 'NONE',  ( -22.39999999999999858, 26.02743912001966464, -254.3139371321002216 ) ) ;
#14267 = ORIENTED_EDGE ( 'NONE', *, *, #36215, .F. ) ;
#14268 = ORIENTED_EDGE ( 'NONE', *, *, #223551, .T. ) ;
#14270 = VERTEX_POINT ( 'NONE', #255261 ) ;
#14269 = AXIS2_PLACEMENT_3D ( 'NONE', #97839, #219088, #254354 ) ;
#14271 = EDGE_CURVE ( 'NONE', #62919, #95570, #1922, .T. ) ;
#14272 = DIRECTION ( 'NONE',  ( 0.000000000000000000, -0.2617529984165031243, -0.9651348961777157509 ) ) ;
#14273 = VECTOR ( 'NONE', #85469, 1000.000000000000000 ) ;
#14276 = EDGE_LOOP ( 'NONE', ( #26876, #245073, #195279, #202181, #216253, #153486, #480, #82340 ) ) ;
#14275 = ADVANCED_FACE ( 'NONE', ( #93675 ), #103052, .T. ) ;
#14274 = DIRECTION ( 'NONE',  ( 1.000000000000000000, 0.000000000000000000, 0.000000000000000000 ) ) ;
#14277 = LINE ( 'NONE', #54648, #184189 ) ;
#14278 = ORIENTED_EDGE ( 'NONE', *, *, #121390, .F. ) ;
#14279 = ORIENTED_EDGE ( 'NONE', *, *, #116769, .T. ) ;
#14280 = DIRECTION ( 'NONE',  ( 0.000000000000000000, 0.2128009952263587856, -0.9770955615653318382 ) ) ;
#14281 = CIRCLE ( 'NONE', #43477, 0.09999999999998898659 ) ;
#14282 = EDGE_CURVE ( 'NONE', #224282, #148469, #178375, .T. ) ;
#14283 = CIRCLE ( 'NONE', #193343, 0.1000000000000028644 ) ;
#14284 = ORIENTED_EDGE ( 'NONE', *, *, #11929, .F. ) ;
#14285 = EDGE_CURVE ( 'NONE', #53093, #60702, #235180, .T. ) ;
#14286 = TOROIDAL_SURFACE ( 'NONE', #47554, 0.2000000000000000111, 0.1000000000000000056 ) ;
#14287 = CARTESIAN_POINT ( 'NONE',  ( -23.25000000000000000, 4.150000000011156764, -146.3500000000000227 ) ) ;
#14288 = CARTESIAN_POINT ( 'NONE',  ( -21.04999999999999716, 76.08574093704584129, -176.4369337733373584 ) ) ;
#14289 = AXIS2_PLACEMENT_3D ( 'NONE', #2015, #39910, #136373 ) ;
#14291 = VERTEX_POINT ( 'NONE', #74149 ) ;
#14290 = ORIENTED_EDGE ( 'NONE', *, *, #103134, .F. ) ;
#14292 = ORIENTED_EDGE ( 'NONE', *, *, #18581, .T. ) ;
#14293 = CYLINDRICAL_SURFACE ( 'NONE', #69639, 0.09999999999999982514 ) ;
#14295 = VERTEX_POINT ( 'NONE', #15443 ) ;
#14294 = EDGE_CURVE ( 'NONE', #190824, #95434, #252734, .T. ) ;
#14296 = ORIENTED_EDGE ( 'NONE', *, *, #192718, .T. ) ;
#14297 = FACE_OUTER_BOUND ( 'NONE', #178465, .T. ) ;
#14299 = ORIENTED_EDGE ( 'NONE', *, *, #51999, .F. ) ;
#14298 = CARTESIAN_POINT ( 'NONE',  ( 18.49999999999999289, 10.49142135623730709, -24.85000000000000142 ) ) ;
#14300 = CARTESIAN_POINT ( 'NONE',  ( 20.94999999999999929, 1.115600667400684642E-11, -108.3000000000000540 ) ) ;
#14301 = VECTOR ( 'NONE', #97079, 1000.000000000000000 ) ;
#14303 = DIRECTION ( 'NONE',  ( 0.000000000000000000, 0.000000000000000000, -1.000000000000000000 ) ) ;
#14302 = CARTESIAN_POINT ( 'NONE',  ( -20.94999999999999929, -1.835341550224411922, -11.55515129256298046 ) ) ;
#14304 = CARTESIAN_POINT ( 'NONE',  ( 20.94999999999999929, 62.98048128140160173, -207.0210305352945568 ) ) ;
#14305 = DIRECTION ( 'NONE',  ( 0.000000000000000000, 0.000000000000000000, 1.000000000000000000 ) ) ;
#14306 = LINE ( 'NONE', #158950, #242611 ) ;
#14307 = ORIENTED_EDGE ( 'NONE', *, *, #164273, .T. ) ;
#14309 = EDGE_CURVE ( 'NONE', #47209, #106650, #235744, .T. ) ;
#14308 = VERTEX_POINT ( 'NONE', #157547 ) ;
#14310 = PLANE ( 'NONE',  #203705 ) ;
#14311 = AXIS2_PLACEMENT_3D ( 'NONE', #252529, #190008, #68777 ) ;
#14312 = DIRECTION ( 'NONE',  ( 1.000000000000000000, -0.000000000000000000, 0.000000000000000000 ) ) ;
#14313 = DIRECTION ( 'NONE',  ( 1.000000000000000000, 0.000000000000000000, 0.000000000000000000 ) ) ;
#14314 = ORIENTED_EDGE ( 'NONE', *, *, #225104, .T. ) ;
#14315 = CYLINDRICAL_SURFACE ( 'NONE', #2954, 0.09999999999999939493 ) ;
#14316 = CIRCLE ( 'NONE', #214205, 7.800000000000000711 ) ;
#14317 = AXIS2_PLACEMENT_3D ( 'NONE', #214032, #212754, #116230 ) ;
#14318 = CARTESIAN_POINT ( 'NONE',  ( -18.79999999999999716, -1.885425182446133885, -11.49641995933507843 ) ) ;
#14319 = TOROIDAL_SURFACE ( 'NONE', #135062, 11.65000000000000036, 0.1000000000000000056 ) ;
#14320 = CARTESIAN_POINT ( 'NONE',  ( -23.15000000000000213, 85.50000000001207923, -126.6291383618717816 ) ) ;
#14321 = ORIENTED_EDGE ( 'NONE', *, *, #213390, .F. ) ;
#14322 = ORIENTED_EDGE ( 'NONE', *, *, #165214, .F. ) ;
#14323 = DIRECTION ( 'NONE',  ( -1.000000000000000000, -2.952720810173289112E-16, 0.000000000000000000 ) ) ;
#14324 = CARTESIAN_POINT ( 'NONE',  ( 18.39999999999999858, 85.68240343348777799, -29.36626410711146562 ) ) ;
#14325 = ORIENTED_EDGE ( 'NONE', *, *, #68806, .T. ) ;
#14326 = CARTESIAN_POINT ( 'NONE',  ( 20.94999999999999929, 10.72371710471868056, -79.15000000000004832 ) ) ;
#14328 = ORIENTED_EDGE ( 'NONE', *, *, #81937, .F. ) ;
#14327 =( REPRESENTATION_RELATIONSHIP ('NONE','NONE', #36900, #10216 ) REPRESENTATION_RELATIONSHIP_WITH_TRANSFORMATION ( #227993 )SHAPE_REPRESENTATION_RELATIONSHIP( ) );
#14329 = CARTESIAN_POINT ( 'NONE',  ( -23.15000000000000213, 1.115626384983466744E-11, -165.4000000000000341 ) ) ;
#14330 = CYLINDRICAL_SURFACE ( 'NONE', #95591, 0.1000000000000028644 ) ;
#14332 = DIRECTION ( 'NONE',  ( 1.734723475976817823E-14, 0.4088369013363281623, -0.9126074666063771490 ) ) ;
#14331 = CARTESIAN_POINT ( 'NONE',  ( 19.97071067811864609, 15.99555563007541004, -219.3668113423574653 ) ) ;
#14333 = DIRECTION ( 'NONE',  ( 0.000000000000000000, 0.8777080977375072424, -0.4791956752371691608 ) ) ;
#14334 = CARTESIAN_POINT ( 'NONE',  ( 18.57399277249656322, 65.66887361445387228, -164.4329845918269655 ) ) ;
#14335 = DIRECTION ( 'NONE',  ( 0.000000000000000000, -7.429790795770647916E-15, 1.000000000000000000 ) ) ;
#14337 = ORIENTED_EDGE ( 'NONE', *, *, #230648, .F. ) ;
#14336 = DIRECTION ( 'NONE',  ( 0.000000000000000000, 0.000000000000000000, 1.000000000000000000 ) ) ;
#14338 = CIRCLE ( 'NONE', #222563, 0.1000000000000001305 ) ;
#14339 = EDGE_CURVE ( 'NONE', #158643, #186519, #10341, .T. ) ;
#14341 = VERTEX_POINT ( 'NONE', #158814 ) ;
#14340 = ORIENTED_EDGE ( 'NONE', *, *, #213756, .T. ) ;
#14342 = ORIENTED_EDGE ( 'NONE', *, *, #87234, .F. ) ;
#14343 = ADVANCED_FACE ( 'NONE', ( #153712 ), #238312, .F. ) ;
#14344 = CARTESIAN_POINT ( 'NONE',  ( -20.85000000000000142, 7.021664781911246322, -70.63356540189728605 ) ) ;
#14345 = CARTESIAN_POINT ( 'NONE',  ( -20.07928932188135107, 9.220710678129810489, -54.65000000000000568 ) ) ;
#14346 =( BOUNDED_SURFACE ( )  B_SPLINE_SURFACE ( 3, 2, ( 
 ( #102732, #4913, #242259 ),
 ( #243552, #240997, #144426 ),
 ( #64908, #45356, #165305 ),
 ( #205701, #25792, #244829 ) ),
 .UNSPECIFIED., .F., .F., .F. ) 
 B_SPLINE_SURFACE_WITH_KNOTS ( ( 4, 4 ),
 ( 3, 3 ),
 ( 5.727910411845712702, 5.983100554402349225 ),
 ( 0.000000000000000000, 1.000000000000000000 ),
 .UNSPECIFIED. ) 
 GEOMETRIC_REPRESENTATION_ITEM ( )  RATIONAL_B_SPLINE_SURFACE ( (
 ( 1.000000000000000000, 0.8946697475932264831, 1.000000000000000000),
 ( 1.000000000000000000, 0.9035312726220544599, 1.000000000000000000),
 ( 1.000000000000000000, 0.9104333467450480555, 1.000000000000000000),
 ( 1.000000000000000000, 0.9152888060719390761, 1.000000000000000000) ) ) 
 REPRESENTATION_ITEM ( '' )  SURFACE ( )  );
#14347 = CARTESIAN_POINT ( 'NONE',  ( -23.15000000000000213, 4.350000000011156054, -155.1500000000000057 ) ) ;
#14348 = ADVANCED_FACE ( 'NONE', ( #97493 ), #154964, .T. ) ;
#14349 = EDGE_CURVE ( 'NONE', #217380, #167762, #72712, .T. ) ;
#14351 = CARTESIAN_POINT ( 'NONE',  ( -22.48660254037843487, 11.65000000001115588, -33.45000000000001705 ) ) ;
#14350 = CARTESIAN_POINT ( 'NONE',  ( -20.64999999999999858, 1.115623935689868526E-11, -132.1000000000000227 ) ) ;
#14352 = EDGE_LOOP ( 'NONE', ( #125740, #113749, #143247, #142152, #42841 ) ) ;
#14353 = CARTESIAN_POINT ( 'NONE',  ( 20.12500000000000355, 10.24195072709382970, -74.86020372708617288 ) ) ;
#14354 = EDGE_LOOP ( 'NONE', ( #58600, #57235, #249519, #116451 ) ) ;
#14355 = VERTEX_POINT ( 'NONE', #234460 ) ;
#14356 = CARTESIAN_POINT ( 'NONE',  ( -21.07928932188134041, 69.67148334361296236, -69.62200263017901136 ) ) ;
#14357 = CARTESIAN_POINT ( 'NONE',  ( 13.99999999999999822, 62.10905854918434699, -217.1108499610991203 ) ) ;
#14358 = EDGE_CURVE ( 'NONE', #212829, #169291, #164456, .T. ) ;
#14359 = CARTESIAN_POINT ( 'NONE',  ( 18.59999999999999076, -1.835859311432481045, -112.0044391687985694 ) ) ;
#14360 = EDGE_CURVE ( 'NONE', #252532, #212201, #147891, .T. ) ;
#14361 = ADVANCED_FACE ( 'NONE', ( #143052 ), #225149, .T. ) ;
#14362 = SPHERICAL_SURFACE ( 'NONE', #160791, 0.1000000000000000056 ) ;
#14363 = CIRCLE ( 'NONE', #231019, 11.70000000000000284 ) ;
#14364 = DIRECTION ( 'NONE',  ( 1.224646799147353207E-16, -0.4088369013363281623, 0.9126074666063771490 ) ) ;
#14365 = EDGE_LOOP ( 'NONE', ( #91977, #104907 ) ) ;
#14366 = VERTEX_POINT ( 'NONE', #20579 ) ;
#14367 = CARTESIAN_POINT ( 'NONE',  ( 22.39999999999999503, -0.1008583690875579364, -88.75043287651064361 ) ) ;
#14368 = ADVANCED_FACE ( 'NONE', ( #46520 ), #242164, .T. ) ;
#14369 = CARTESIAN_POINT ( 'NONE',  ( -18.60000000000001208, -9.364240527579751117, -40.68024858184076464 ) ) ;
#14370 = DIRECTION ( 'NONE',  ( -0.000000000000000000, -0.000000000000000000, -1.000000000000000000 ) ) ;
#14371 = DIRECTION ( 'NONE',  ( 0.000000000000000000, -0.9126074666063773710, -0.4088369013363272741 ) ) ;
#14372 = FACE_OUTER_BOUND ( 'NONE', #159211, .T. ) ;
#14373 = DIRECTION ( 'NONE',  ( 0.000000000000000000, -6.853228547068871147E-15, 1.000000000000000000 ) ) ;
#14374 = CARTESIAN_POINT ( 'NONE',  ( -21.07094088545304089, 6.320167221927643020, -33.40110629744778237 ) ) ;
#14375 = EDGE_CURVE ( 'NONE', #202242, #180038, #239464, .T. ) ;
#14377 = CARTESIAN_POINT ( 'NONE',  ( 20.95512820512820440, 8.876151316299271343, -45.65000000000000568 ) ) ;
#14376 = CARTESIAN_POINT ( 'NONE',  ( 20.95512820512820440, 10.62384868372303615, -45.65000000000000568 ) ) ;
#14378 = DIRECTION ( 'NONE',  ( 0.000000000000000000, 0.000000000000000000, -1.000000000000000000 ) ) ;
#14379 = FACE_OUTER_BOUND ( 'NONE', #184773, .T. ) ;
#14380 = DIRECTION ( 'NONE',  ( 0.000000000000000000, -0.8814952561688430555, 0.4721928772777346239 ) ) ;
#14381 = DIRECTION ( 'NONE',  ( -1.000000000000000000, 0.000000000000000000, -0.000000000000000000 ) ) ;
#14382 = EDGE_CURVE ( 'NONE', #243571, #125503, #220042, .T. ) ;
#14383 = VECTOR ( 'NONE', #242227, 1000.000000000000000 ) ;
#14385 = VERTEX_POINT ( 'NONE', #144323 ) ;
#14384 = CYLINDRICAL_SURFACE ( 'NONE', #107146, 0.09999999999999939493 ) ;
#14386 = VECTOR ( 'NONE', #14144, 1000.000000000000000 ) ;
#14387 = AXIS2_PLACEMENT_3D ( 'NONE', #11428, #132652, #250024 ) ;
#14388 = ADVANCED_FACE ( 'NONE', ( #200483 ), #179649, .T. ) ;
#14389 = DIRECTION ( 'NONE',  ( 1.000000000000000000, 0.000000000000000000, 0.000000000000000000 ) ) ;
#14390 = EDGE_CURVE ( 'NONE', #212939, #128108, #135387, .T. ) ;
#14391 = EDGE_CURVE ( 'NONE', #158124, #229990, #243739, .T. ) ;
#14392 = CARTESIAN_POINT ( 'NONE',  ( 23.15000000000000213, -8.999999999988842703, -157.6060308773475640 ) ) ;
#14393 = CARTESIAN_POINT ( 'NONE',  ( 21.30000000000002558, 36.65892442174472876, -249.5511627012454596 ) ) ;
#14394 = DIRECTION ( 'NONE',  ( -1.000000000000000000, 0.000000000000000000, -0.000000000000000000 ) ) ;
#14395 = DIRECTION ( 'NONE',  ( 0.000000000000000000, -0.4088369013363280513, 0.9126074666063769270 ) ) ;
#14396 = VECTOR ( 'NONE', #233357, 1000.000000000000114 ) ;
#14397 = DIRECTION ( 'NONE',  ( 0.000000000000000000, 0.8660254037844383745, -0.5000000000000003331 ) ) ;
#14398 = AXIS2_PLACEMENT_3D ( 'NONE', #167204, #208865, #30244 ) ;
#14399 = CARTESIAN_POINT ( 'NONE',  ( 18.49999999999998934, 10.25000000261906941, -24.68717194963243600 ) ) ;
#14400 = DIRECTION ( 'NONE',  ( -3.265361837132813093E-16, -1.000000000000000000, -6.982962677686266711E-15 ) ) ;
#14401 = AXIS2_PLACEMENT_3D ( 'NONE', #140571, #242238, #220125 ) ;
#14402 = AXIS2_PLACEMENT_3D ( 'NONE', #146213, #129236, #185353 ) ;
#14403 = ORIENTED_EDGE ( 'NONE', *, *, #59677, .F. ) ;
#14404 = DIRECTION ( 'NONE',  ( -3.265361837132813093E-16, 1.000000000000000000, 0.000000000000000000 ) ) ;
#14406 = VERTEX_POINT ( 'NONE', #201754 ) ;
#14405 = CARTESIAN_POINT ( 'NONE',  ( 21.05000000000000071, 64.35000000001218723, -143.5379132551784096 ) ) ;
#14407 = DIRECTION ( 'NONE',  ( -0.000000000000000000, 0.1350103645451876666, 0.9908441862701600211 ) ) ;
#14408 = DIRECTION ( 'NONE',  ( 0.000000000000000000, 0.2128009952263650861, -0.9770955615653305060 ) ) ;
#14409 = ORIENTED_EDGE ( 'NONE', *, *, #239585, .T. ) ;
#14410 = DIRECTION ( 'NONE',  ( 0.000000000000000000, 0.000000000000000000, 1.000000000000000000 ) ) ;
#14411 = CIRCLE ( 'NONE', #131081, 12.97500000000000320 ) ;
#14412 = AXIS2_PLACEMENT_3D ( 'NONE', #115040, #212865, #253253 ) ;
#14413 = SHAPE_DEFINITION_REPRESENTATION ( #109742, #53611 ) ;
#14414 = VECTOR ( 'NONE', #9647, 1000.000000000000000 ) ;
#14416 = AXIS2_PLACEMENT_3D ( 'NONE', #205276, #127041, #103597 ) ;
#14415 = CARTESIAN_POINT ( 'NONE',  ( -18.50000000000000000, 52.36135249642984490, -232.3808757916058880 ) ) ;
#14417 = CARTESIAN_POINT ( 'NONE',  ( 22.59999954896768770, -2.509145966787972526, -189.5205087850422956 ) ) ;
#14418 = VERTEX_POINT ( 'NONE', #161367 ) ;
#14419 = SPHERICAL_SURFACE ( 'NONE', #54630, 0.1000000000000000056 ) ;
#14420 = DIRECTION ( 'NONE',  ( -1.000000000000000000, -0.000000000000000000, -0.000000000000000000 ) ) ;
#14421 = AXIS2_PLACEMENT_3D ( 'NONE', #68066, #126752, #105876 ) ;
#14422 = CARTESIAN_POINT ( 'NONE',  ( -16.79363873026997922, 9.948850229429586634, -121.3461537814455085 ) ) ;
#14423 = EDGE_LOOP ( 'NONE', ( #195186, #65745, #216533, #196968, #119983 ) ) ;
#14424 = EDGE_LOOP ( 'NONE', ( #214815, #115077, #248360, #133082 ) ) ;
#14425 = AXIS2_PLACEMENT_3D ( 'NONE', #246091, #128708, #208250 ) ;
#14426 = DIRECTION ( 'NONE',  ( -1.000000000000000000, 0.000000000000000000, -0.000000000000000000 ) ) ;
#14427 = CIRCLE ( 'NONE', #197549, 11.70000000000001172 ) ;
#14428 = DIRECTION ( 'NONE',  ( 1.000000000000000000, 0.000000000000000000, 0.000000000000000000 ) ) ;
#14429 = DIRECTION ( 'NONE',  ( 1.000000000000000000, 0.000000000000000000, 0.000000000000000000 ) ) ;
#14430 = EDGE_CURVE ( 'NONE', #88314, #243325, #118859, .T. ) ;
#14431 = CARTESIAN_POINT ( 'NONE',  ( -21.33487959338958362, 69.27444184810076422, -103.0231074845243597 ) ) ;
#14433 = CARTESIAN_POINT ( 'NONE',  ( -23.15000000000000213, 76.00000000001162448, -65.47310748452431994 ) ) ;
#14432 = CARTESIAN_POINT ( 'NONE',  ( -20.64999999999999858, 68.85000000001228670, -157.6731074845243938 ) ) ;
#14434 = CARTESIAN_POINT ( 'NONE',  ( -21.08198257630413508, 75.92735667622784490, -176.3597042185394059 ) ) ;
#14435 = EDGE_CURVE ( 'NONE', #217189, #22276, #3548, .T. ) ;
#14436 = CYLINDRICAL_SURFACE ( 'NONE', #64384, 0.1000000000000008105 ) ;
#14437 = CARTESIAN_POINT ( 'NONE',  ( 20.94999999999999574, 43.48442877397276618, -245.2193771921251084 ) ) ;
#14438 = CARTESIAN_POINT ( 'NONE',  ( 21.05000000000000071, 76.00000000001267608, -203.5231074845243597 ) ) ;
#14439 = ORIENTED_EDGE ( 'NONE', *, *, #170689, .T. ) ;
#14440 = VERTEX_POINT ( 'NONE', #103915 ) ;
#14441 = CYLINDRICAL_SURFACE ( 'NONE', #160423, 0.09999999999999939493 ) ;
#14442 = CARTESIAN_POINT ( 'NONE',  ( 22.39999999999999503, -0.1008583690875579364, -55.25043287651065782 ) ) ;
#14443 = CARTESIAN_POINT ( 'NONE',  ( 18.49999999999998934, 65.75000000001251976, -178.8731074845244109 ) ) ;
#14444 =( BOUNDED_SURFACE ( )  B_SPLINE_SURFACE ( 3, 2, ( 
 ( #166993, #64000, #6586 ),
 ( #84809, #7900, #46981 ),
 ( #164393, #67846, #185235 ),
 ( #104381, #143528, #4020 ),
 ( #83527, #163120, #26172 ),
 ( #146095, #242626, #224352 ) ),
 .UNSPECIFIED., .F., .F., .F. ) 
 B_SPLINE_SURFACE_WITH_KNOTS ( ( 4, 2, 4 ),
 ( 3, 3 ),
 ( 4.712388980384689674, 5.497787143782137953, 6.283185307179586232 ),
 ( 0.000000000000000000, 1.000000000000000000 ),
 .UNSPECIFIED. ) 
 GEOMETRIC_REPRESENTATION_ITEM ( )  RATIONAL_B_SPLINE_SURFACE ( (
 ( 1.000000000000000000, 0.7071067811865475727, 1.000000000000000000),
 ( 1.000000000000000000, 0.7727932973488792490, 1.000000000000000000),
 ( 1.000000000000000000, 0.8282379607653241882, 1.000000000000000000),
 ( 1.000000000000000000, 0.9038128468035547813, 1.000000000000000000),
 ( 1.000000000000000000, 0.9240297172246445534, 1.000000000000000000),
 ( 1.000000000000000000, 0.9238795325112961754, 1.000000000000000000) ) ) 
 REPRESENTATION_ITEM ( '' )  SURFACE ( )  );
#14445 = ADVANCED_FACE ( 'NONE', ( #221301 ), #85623, .F. ) ;
#14446 = EDGE_CURVE ( 'NONE', #244526, #202111, #97963, .T. ) ;
#14447 = EDGE_LOOP ( 'NONE', ( #73022, #247290, #42877 ) ) ;
#14448 = CARTESIAN_POINT ( 'NONE',  ( 21.05000000000000071, 67.23127455305841238, -235.8551265064783991 ) ) ;
#14449 = CARTESIAN_POINT ( 'NONE',  ( 21.05000000000000071, 67.23127455305835554, -235.8551265064784559 ) ) ;
#14450 = LINE ( 'NONE', #172260, #245128 ) ;
#14451 = LINE ( 'NONE', #254295, #164794 ) ;
#14452 = ORIENTED_EDGE ( 'NONE', *, *, #201907, .T. ) ;
#14453 = ORIENTED_EDGE ( 'NONE', *, *, #107012, .T. ) ;
#14454 = AXIS2_PLACEMENT_3D ( 'NONE', #208513, #11592, #130222 ) ;
#14455 = AXIS2_PLACEMENT_3D ( 'NONE', #160458, #239975, #61330 ) ;
#14456 = CARTESIAN_POINT ( 'NONE',  ( -21.05000000000000071, 64.35000000001190301, -96.23924182154622997 ) ) ;
#14457 = EDGE_LOOP ( 'NONE', ( #108721, #95228, #4348, #10355 ) ) ;
#14458 = CARTESIAN_POINT ( 'NONE',  ( -21.05000000000000071, -11.48912529306489994, -63.89999999999999858 ) ) ;
#14459 = FACE_OUTER_BOUND ( 'NONE', #191373, .T. ) ;
#14460 = EDGE_CURVE ( 'NONE', #73708, #209135, #39580, .T. ) ;
#14461 = AXIS2_PLACEMENT_3D ( 'NONE', #84041, #87921, #26715 ) ;
#14462 = CIRCLE ( 'NONE', #176754, 0.09999999999999395484 ) ;
#14463 = VERTEX_POINT ( 'NONE', #101321 ) ;
#14464 = CARTESIAN_POINT ( 'NONE',  ( 21.05000000000000071, 36.02918351690956200, -236.0543695120161090 ) ) ;
#14465 = CARTESIAN_POINT ( 'NONE',  ( -21.14999999999999858, 76.00000000001213607, -136.5231074845242745 ) ) ;
#14467 = CIRCLE ( 'NONE', #139314, 0.09999999999998304689 ) ;
#14466 = DIRECTION ( 'NONE',  ( 1.000000000000000000, 0.000000000000000000, 0.000000000000000000 ) ) ;
#14468 = DIRECTION ( 'NONE',  ( 0.000000000000000000, -1.000000000000000000, 0.000000000000000000 ) ) ;
#14470 = CIRCLE ( 'NONE', #160215, 0.09999999999998898659 ) ;
#14469 = CARTESIAN_POINT ( 'NONE',  ( 21.00000000000000000, 9.750000000011153745, -88.25000000000005684 ) ) ;
#14471 = EDGE_CURVE ( 'NONE', #119208, #214056, #139489, .T. ) ;
#14472 = CARTESIAN_POINT ( 'NONE',  ( -23.39999999999994529, 74.83745509109094485, -43.92310748452479885 ) ) ;
#14473 = AXIS2_PLACEMENT_3D ( 'NONE', #243275, #21689, #145464 ) ;
#14474 = CARTESIAN_POINT ( 'NONE',  ( 21.00000000000000000, 9.750000000011153745, -121.7500000000000426 ) ) ;
#14476 = ORIENTED_EDGE ( 'NONE', *, *, #157233, .T. ) ;
#14475 = ADVANCED_FACE ( 'NONE', ( #141773 ), #63520, .F. ) ;
#14478 = PLANE ( 'NONE',  #155907 ) ;
#14477 = DIRECTION ( 'NONE',  ( 1.000000000000000000, 0.000000000000000000, 0.000000000000000000 ) ) ;
#14479 = EDGE_LOOP ( 'NONE', ( #254199, #155879, #118725, #222268 ) ) ;
#14481 = ORIENTED_EDGE ( 'NONE', *, *, #412, .T. ) ;
#14480 = DIRECTION ( 'NONE',  ( 0.000000000000000000, 0.000000000000000000, -1.000000000000000000 ) ) ;
#14482 = AXIS2_PLACEMENT_3D ( 'NONE', #28638, #208523, #108124 ) ;
#14483 = ORIENTED_EDGE ( 'NONE', *, *, #119180, .F. ) ;
#14484 = CARTESIAN_POINT ( 'NONE',  ( -18.34374000495059676, 11.47316190337362940, -91.25000000000005684 ) ) ;
#14485 = CARTESIAN_POINT ( 'NONE',  ( 14.22916352759893499, 66.54258906972209786, -151.5231915757781849 ) ) ;
#14486 = DIRECTION ( 'NONE',  ( -1.000000000000000000, 0.000000000000000000, 0.000000000000000000 ) ) ;
#14487 = DIRECTION ( 'NONE',  ( -1.000000000000000000, -0.000000000000000000, -0.000000000000000000 ) ) ;
#14488 = EDGE_LOOP ( 'NONE', ( #18435, #61405, #137047, #257905 ) ) ;
#14489 = CARTESIAN_POINT ( 'NONE',  ( 21.06086055315988759, 8.774707514967413857, -112.7023221551541070 ) ) ;
#14491 = CARTESIAN_POINT ( 'NONE',  ( 21.05000000000000071, 1.115600667400684642E-11, -67.00000000000004263 ) ) ;
#14490 = CIRCLE ( 'NONE', #6062, 0.09999999999998898659 ) ;
#14492 = ADVANCED_FACE ( 'NONE', ( #163925 ), #162646, .F. ) ;
#14493 = ORIENTED_EDGE ( 'NONE', *, *, #90762, .F. ) ;
#14494 = EDGE_CURVE ( 'NONE', #28335, #6807, #32137, .T. ) ;
#14495 = CARTESIAN_POINT ( 'NONE',  ( 18.49999999999998934, 19.85039924723355398, -2.280303057801358335 ) ) ;
#14496 = AXIS2_PLACEMENT_3D ( 'NONE', #220809, #159566, #239101 ) ;
#14497 = CARTESIAN_POINT ( 'NONE',  ( 23.24999999999999289, 64.35000000001173248, -81.27310748452440237 ) ) ;
#14498 = EDGE_CURVE ( 'NONE', #4495, #33688, #77139, .T. ) ;
#14499 = ORIENTED_EDGE ( 'NONE', *, *, #214017, .T. ) ;
#14500 = DIRECTION ( 'NONE',  ( 0.000000000000000000, -0.8814952561683926380, 0.4721928772785753958 ) ) ;
#14501 = AXIS2_PLACEMENT_3D ( 'NONE', #196749, #54672, #153835 ) ;
#14502 = VECTOR ( 'NONE', #184870, 1000.000000000000000 ) ;
#14503 = EDGE_LOOP ( 'NONE', ( #225605, #195805, #159133, #98854 ) ) ;
#14504 = AXIS2_PLACEMENT_3D ( 'NONE', #92036, #226392, #206856 ) ;
#14505 = CARTESIAN_POINT ( 'NONE',  ( 18.49999999999998934, 65.70711192142361767, -97.56510546851221477 ) ) ;
#14506 = VERTEX_POINT ( 'NONE', #68677 ) ;
#14507 = CARTESIAN_POINT ( 'NONE',  ( -22.45305610364635385, 76.10085836911117951, -181.7726746080137445 ) ) ;
#14508 = CARTESIAN_POINT ( 'NONE',  ( 18.39999999999999858, -9.519327731081283162, -107.4729763765593589 ) ) ;
#14509 = FACE_OUTER_BOUND ( 'NONE', #94682, .T. ) ;
#14510 = EDGE_CURVE ( 'NONE', #200641, #69752, #164636, .T. ) ;
#14511 = CARTESIAN_POINT ( 'NONE',  ( 18.49999999999999289, 10.49142135624846439, -58.35000000000000142 ) ) ;
#14512 = EDGE_CURVE ( 'NONE', #111850, #235746, #109068, .T. ) ;
#14513 = LINE ( 'NONE', #253080, #241938 ) ;
#14514 = CARTESIAN_POINT ( 'NONE',  ( 18.33683296300444709, -9.511149971121596991, -73.90570741271007194 ) ) ;
#14515 = FACE_OUTER_BOUND ( 'NONE', #36131, .T. ) ;
#14516 = VERTEX_POINT ( 'NONE', #187350 ) ;
#14517 = CIRCLE ( 'NONE', #185177, 0.09999999999998898659 ) ;
#14519 = CARTESIAN_POINT ( 'NONE',  ( -16.94445028196808778, 9.992063609708889516, -113.1073301784184792 ) ) ;
#14518 = CARTESIAN_POINT ( 'NONE',  ( 20.94999999999999574, 7.128833340093095217, -233.7327013124392749 ) ) ;
#14520 = ORIENTED_EDGE ( 'NONE', *, *, #137999, .F. ) ;
#14523 = ORIENTED_EDGE ( 'NONE', *, *, #50472, .T. ) ;
#14522 = CARTESIAN_POINT ( 'NONE',  ( -20.85000000000000142, 6.933893972126341509, -37.28564583437357527 ) ) ;
#14521 = CARTESIAN_POINT ( 'NONE',  ( -23.15000000000000213, -2.001034438968700258, -225.8925473383868905 ) ) ;
#14524 = ORIENTED_EDGE ( 'NONE', *, *, #66572, .T. ) ;
#14525 = CARTESIAN_POINT ( 'NONE',  ( -23.25000000000000000, 77.14957036958705316, -28.20719500002235236 ) ) ;
#14526 = DIRECTION ( 'NONE',  ( -0.000000000000000000, 0.9770955615653313941, 0.2128009952263603954 ) ) ;
#14527 = CARTESIAN_POINT ( 'NONE',  ( 20.95512820512820440, 65.37615131630066401, -182.2731074845244450 ) ) ;
#14528 = CARTESIAN_POINT ( 'NONE',  ( 20.95035502843362707, 59.10205934002117090, -225.8004220253184258 ) ) ;
#14529 = VECTOR ( 'NONE', #148793, 1000.000000000000227 ) ;
#14530 = ORIENTED_EDGE ( 'NONE', *, *, #138525, .T. ) ;
#14532 = EDGE_LOOP ( 'NONE', ( #14452, #55263, #55021, #5058 ) ) ;
#14531 = LINE ( 'NONE', #17091, #34624 ) ;
#14534 = CARTESIAN_POINT ( 'NONE',  ( -16.92973740335405708, 66.00749618554552001, -190.9291665197260386 ) ) ;
#14533 = CARTESIAN_POINT ( 'NONE',  ( -21.05000000000000071, 63.58084468663284383, -237.4904741118237723 ) ) ;
#14536 = ORIENTED_EDGE ( 'NONE', *, *, #142536, .T. ) ;
#14535 = DIRECTION ( 'NONE',  ( -1.000000000000000000, 0.000000000000000000, 0.000000000000000000 ) ) ;
#14537 = ORIENTED_EDGE ( 'NONE', *, *, #192046, .T. ) ;
#14538 = DIRECTION ( 'NONE',  ( 1.000000000000000000, 0.000000000000000000, -0.000000000000000000 ) ) ;
#14539 = VECTOR ( 'NONE', #189980, 1000.000000000000000 ) ;
#14540 = AXIS2_PLACEMENT_3D ( 'NONE', #175216, #36973, #116480 ) ;
#14541 = CARTESIAN_POINT ( 'NONE',  ( 23.25000000000000000, 6.550000000011156231, -146.3500000000000227 ) ) ;
#14542 = VERTEX_POINT ( 'NONE', #72540 ) ;
#14543 = CARTESIAN_POINT ( 'NONE',  ( -23.15000000000000213, 70.76519756549814133, -215.1840646563997836 ) ) ;
#14544 = ORIENTED_EDGE ( 'NONE', *, *, #53617, .F. ) ;
#14545 = FACE_OUTER_BOUND ( 'NONE', #239805, .T. ) ;
#14546 = CARTESIAN_POINT ( 'NONE',  ( -23.15000000000000213, 69.16514130714681130, -247.7543978865853660 ) ) ;
#14547 = ORIENTED_EDGE ( 'NONE', *, *, #235614, .F. ) ;
#14548 = DIRECTION ( 'NONE',  ( -1.000000000000000000, 0.000000000000000000, -0.000000000000000000 ) ) ;
#14549 = EDGE_CURVE ( 'NONE', #102764, #67043, #71255, .T. ) ;
#14550 = AXIS2_PLACEMENT_3D ( 'NONE', #101078, #144094, #222335 ) ;
#14551 = CARTESIAN_POINT ( 'NONE',  ( 23.14999999999999858, 78.10000000001141984, -36.02310748452431000 ) ) ;
#14552 = AXIS2_PLACEMENT_3D ( 'NONE', #4190, #81151, #2899 ) ;
#14553 = CIRCLE ( 'NONE', #160311, 0.6000000000000033085 ) ;
#14554 = VECTOR ( 'NONE', #141441, 1000.000000000000227 ) ;
#14555 = ORIENTED_EDGE ( 'NONE', *, *, #24193, .F. ) ;
#14556 = ORIENTED_EDGE ( 'NONE', *, *, #59806, .T. ) ;
#14557 = CYLINDRICAL_SURFACE ( 'NONE', #82072, 0.09999999999999939493 ) ;
#14558 = VERTEX_POINT ( 'NONE', #150775 ) ;
#14559 = PRESENTATION_LAYER_ASSIGNMENT (  '', '', ( #43754 ) ) ;
#14560 = CARTESIAN_POINT ( 'NONE',  ( -21.05000000000000071, -11.74999999998884448, -164.6000000000000227 ) ) ;
#14562 = EDGE_CURVE ( 'NONE', #151973, #8323, #52186, .T. ) ;
#14561 = ORIENTED_EDGE ( 'NONE', *, *, #182169, .T. ) ;
#14564 = VERTEX_POINT ( 'NONE', #90781 ) ;
#14563 = CARTESIAN_POINT ( 'NONE',  ( -18.50000000000000000, 77.36242903720540198, -128.6342262366031548 ) ) ;
#14565 = VERTEX_POINT ( 'NONE', #51640 ) ;
#14566 = ADVANCED_FACE ( 'NONE', ( #229039 ), #56281, .F. ) ;
#14567 = CARTESIAN_POINT ( 'NONE',  ( -21.05000000000000071, 78.24390740893981899, -231.6169762517609172 ) ) ;
#14568 = EDGE_CURVE ( 'NONE', #66070, #136892, #155040, .T. ) ;
#14569 = ORIENTED_EDGE ( 'NONE', *, *, #79494, .T. ) ;
#14573 = ORIENTED_EDGE ( 'NONE', *, *, #129445, .F. ) ;
#14572 = ORIENTED_EDGE ( 'NONE', *, *, #71480, .F. ) ;
#14571 = DIRECTION ( 'NONE',  ( 0.000000000000000000, -6.789366196018718420E-15, 1.000000000000000000 ) ) ;
#14570 = B_SPLINE_CURVE_WITH_KNOTS ( 'NONE', 3,
 ( #31712, #53810, #111216, #228612, #10838, #12145, #89070, #90354, #154243, #192060 ),
 .UNSPECIFIED., .F., .F.,
 ( 4, 3, 3, 4 ),
 ( 7.632826238681696029E-06, 4.756916949875625587E-05, 9.484459048152062838E-05, 0.0001435500935100044199 ),
 .UNSPECIFIED. ) ;
#14574 = ORIENTED_EDGE ( 'NONE', *, *, #233913, .T. ) ;
#14575 = B_SPLINE_CURVE_WITH_KNOTS ( 'NONE', 3,
 ( #141301, #104697, #60462, #39664, #4340, #223385, #202556 ),
 .UNSPECIFIED., .F., .F.,
 ( 4, 3, 4 ),
 ( 0.000000000000000000, 0.0007844235214594318627, 0.001767853679404347454 ),
 .UNSPECIFIED. ) ;
#14576 = AXIS2_PLACEMENT_3D ( 'NONE', #100440, #2641, #41809 ) ;
#14577 = AXIS2_PLACEMENT_3D ( 'NONE', #178816, #19718, #238755 ) ;
#14578 = CARTESIAN_POINT ( 'NONE',  ( 21.07964655665547582, 8.774889614989714204, -45.72191658296406302 ) ) ;
#14579 = AXIS2_PLACEMENT_3D ( 'NONE', #91079, #31150, #33721 ) ;
#14580 = ORIENTED_EDGE ( 'NONE', *, *, #39894, .T. ) ;
#14581 = EDGE_CURVE ( 'NONE', #156376, #247484, #127031, .T. ) ;
#14582 = FACE_OUTER_BOUND ( 'NONE', #59442, .T. ) ;
#14584 = ORIENTED_EDGE ( 'NONE', *, *, #232883, .T. ) ;
#14583 = CARTESIAN_POINT ( 'NONE',  ( 20.94999999999999574, 87.65000000001192859, -100.1231074845242262 ) ) ;
#14585 = LINE ( 'NONE', #253159, #84005 ) ;
#14586 = ORIENTED_EDGE ( 'NONE', *, *, #159863, .T. ) ;
#14587 = VERTEX_POINT ( 'NONE', #254943 ) ;
#14588 = AXIS2_PLACEMENT_3D ( 'NONE', #256503, #85285, #77920 ) ;
#14589 = AXIS2_PLACEMENT_3D ( 'NONE', #76655, #36279, #57072 ) ;
#14590 = CARTESIAN_POINT ( 'NONE',  ( 22.47007471830798764, 1.115784134737059924E-11, -159.7792893480734904 ) ) ;
#14591 = CARTESIAN_POINT ( 'NONE',  ( 18.50016250449482413, 18.35558276679035572, -236.8903279188155864 ) ) ;
#14592 = AXIS2_PLACEMENT_3D ( 'NONE', #227111, #131877, #210144 ) ;
#14593 = EDGE_LOOP ( 'NONE', ( #37242, #15404, #132835, #91312 ) ) ;
#14594 = VERTEX_POINT ( 'NONE', #135035 ) ;
#14595 = PLANE ( 'NONE',  #6787 ) ;
#14598 = ORIENTED_EDGE ( 'NONE', *, *, #102448, .F. ) ;
#14597 = ORIENTED_EDGE ( 'NONE', *, *, #35919, .T. ) ;
#14596 = AXIS2_PLACEMENT_3D ( 'NONE', #244781, #183546, #162705 ) ;
#14599 = ORIENTED_EDGE ( 'NONE', *, *, #200446, .T. ) ;
#14601 = EDGE_LOOP ( 'NONE', ( #47038, #174680, #215860, #23375 ) ) ;
#14600 = EDGE_CURVE ( 'NONE', #206482, #222414, #76352, .T. ) ;
#14602 = VECTOR ( 'NONE', #88146, 1000.000000000000114 ) ;
#14603 = VERTEX_POINT ( 'NONE', #157224 ) ;
#14604 = EDGE_CURVE ( 'NONE', #177733, #79556, #2111, .T. ) ;
#14605 = CARTESIAN_POINT ( 'NONE',  ( 20.95512820512820440, 18.86447962780959386, -229.9497396848627204 ) ) ;
#14606 = VERTEX_POINT ( 'NONE', #82436 ) ;
#14607 = FACE_OUTER_BOUND ( 'NONE', #207161, .T. ) ;
#14608 = AXIS2_PLACEMENT_3D ( 'NONE', #96612, #217849, #39269 ) ;
#14609 = AXIS2_PLACEMENT_3D ( 'NONE', #9993, #149530, #210759 ) ;
#14610 = LINE ( 'NONE', #168578, #198406 ) ;
#14611 = VERTEX_POINT ( 'NONE', #174232 ) ;
#14613 = EDGE_CURVE ( 'NONE', #152534, #4741, #47901, .T. ) ;
#14612 = VERTEX_POINT ( 'NONE', #33436 ) ;
#14614 = LINE ( 'NONE', #30315, #225540 ) ;
#14615 = VERTEX_POINT ( 'NONE', #34702 ) ;
#14616 = CARTESIAN_POINT ( 'NONE',  ( 22.88900146558018989, 62.14200773611577233, -221.3678968928247457 ) ) ;
#14617 = EDGE_LOOP ( 'NONE', ( #12692, #159466, #160875, #86077 ) ) ;
#14618 = ORIENTED_EDGE ( 'NONE', *, *, #192808, .F. ) ;
#14619 = CARTESIAN_POINT ( 'NONE',  ( 20.94999999999999929, 1.115600667400684642E-11, -167.4999999999999716 ) ) ;
#14621 = VERTEX_POINT ( 'NONE', #38535 ) ;
#14620 = CARTESIAN_POINT ( 'NONE',  ( -21.64999999999999858, 65.95000000001232365, -157.3731074845244393 ) ) ;
#14622 = DIRECTION ( 'NONE',  ( 0.000000000000000000, 0.9126074666063772600, 0.4088369013363273852 ) ) ;
#14623 = CARTESIAN_POINT ( 'NONE',  ( -18.59999999999999787, -9.749999999999943157, -15.00000000000002309 ) ) ;
#14624 = FACE_OUTER_BOUND ( 'NONE', #212236, .T. ) ;
#14625 = DIRECTION ( 'NONE',  ( 0.000000000000000000, -2.775557561563196798E-13, -1.000000000000000000 ) ) ;
#14626 = CARTESIAN_POINT ( 'NONE',  ( 20.02499999999999858, 9.750000000011153745, -54.65000000000000568 ) ) ;
#14627 = LINE ( 'NONE', #253205, #231484 ) ;
#14628 = VECTOR ( 'NONE', #146285, 1000.000000000000000 ) ;
#14629 = DIRECTION ( 'NONE',  ( -1.000000000000000000, 0.000000000000000000, 0.000000000000000000 ) ) ;
#14630 = DIRECTION ( 'NONE',  ( -1.000000000000000000, 0.000000000000000000, 0.000000000000000000 ) ) ;
#14631 = CARTESIAN_POINT ( 'NONE',  ( 20.94999999999999929, -8.663551401869154844, -23.97589888193268948 ) ) ;
#14632 = AXIS2_PLACEMENT_3D ( 'NONE', #221346, #199255, #58417 ) ;
#14633 = CARTESIAN_POINT ( 'NONE',  ( 18.43565242384934422, -9.519327731081284938, -73.97297637655937308 ) ) ;
#14634 = CARTESIAN_POINT ( 'NONE',  ( 21.05000000000000071, 87.48912529308871910, -200.6231074845242688 ) ) ;
#14635 = AXIS2_PLACEMENT_3D ( 'NONE', #43369, #82453, #162045 ) ;
#14636 = ORIENTED_EDGE ( 'NONE', *, *, #119180, .T. ) ;
#14637 = AXIS2_PLACEMENT_3D ( 'NONE', #62941, #223286, #43382 ) ;
#14638 = EDGE_CURVE ( 'NONE', #1255, #104063, #241544, .T. ) ;
#14640 = VERTEX_POINT ( 'NONE', #75119 ) ;
#14639 = ORIENTED_EDGE ( 'NONE', *, *, #67051, .T. ) ;
#14641 = AXIS2_PLACEMENT_3D ( 'NONE', #255775, #167638, #247139 ) ;
#14643 = ORIENTED_EDGE ( 'NONE', *, *, #41774, .F. ) ;
#14642 = ADVANCED_FACE ( 'NONE', ( #217138 ), #84750, .F. ) ;
#14644 = CYLINDRICAL_SURFACE ( 'NONE', #98845, 0.09999999999999983902 ) ;
#14645 = DIRECTION ( 'NONE',  ( -0.000000000000000000, -0.000000000000000000, -1.000000000000000000 ) ) ;
#14646 = EDGE_CURVE ( 'NONE', #221039, #86050, #251927, .T. ) ;
#14647 = EDGE_CURVE ( 'NONE', #55017, #12777, #222882, .T. ) ;
#14649 = DIRECTION ( 'NONE',  ( -3.265361837132813093E-16, -0.9651348961777146407, 0.2617529984165072321 ) ) ;
#14648 = CARTESIAN_POINT ( 'NONE',  ( -23.15000000000000213, 87.48912529308822172, -139.6231074845242688 ) ) ;
#14650 = ORIENTED_EDGE ( 'NONE', *, *, #170640, .F. ) ;
#14652 = ORIENTED_EDGE ( 'NONE', *, *, #248556, .F. ) ;
#14651 = CIRCLE ( 'NONE', #60401, 12.77500000000000036 ) ;
#14653 = CARTESIAN_POINT ( 'NONE',  ( 21.13461538461538325, 67.11458296203710461, -57.17310748452437963 ) ) ;
#14654 = AXIS2_PLACEMENT_3D ( 'NONE', #122623, #242540, #5187 ) ;
#14655 = DIRECTION ( 'NONE',  ( 1.000000000000000000, 0.000000000000000000, 0.000000000000000000 ) ) ;
#14656 = EDGE_CURVE ( 'NONE', #253488, #147289, #142519, .T. ) ;
#14657 = CARTESIAN_POINT ( 'NONE',  ( -21.45000000000000284, 7.708578643773852157, -155.1500000000000057 ) ) ;
#14658 = EDGE_LOOP ( 'NONE', ( #256327, #254797, #49243, #3953 ) ) ;
#14659 = ORIENTED_EDGE ( 'NONE', *, *, #240347, .F. ) ;
#14660 = AXIS2_PLACEMENT_3D ( 'NONE', #235754, #19286, #57100 ) ;
#14661 = EDGE_CURVE ( 'NONE', #170158, #21653, #245407, .T. ) ;
#14662 = LINE ( 'NONE', #61140, #63222 ) ;
#14664 = EDGE_CURVE ( 'NONE', #162415, #75205, #81211, .T. ) ;
#14663 = EDGE_CURVE ( 'NONE', #1729, #176334, #28969, .T. ) ;
#14665 = DIRECTION ( 'NONE',  ( 1.000000000000000000, 0.000000000000000000, 0.000000000000000000 ) ) ;
#14666 = ORIENTED_EDGE ( 'NONE', *, *, #24736, .F. ) ;
#14667 = CARTESIAN_POINT ( 'NONE',  ( 18.59999999999998721, 30.62437029989165893, -230.5032680968432715 ) ) ;
#14669 = ORIENTED_EDGE ( 'NONE', *, *, #179698, .F. ) ;
#14668 = CARTESIAN_POINT ( 'NONE',  ( 23.14999999999999858, 1.115600667400684642E-11, -134.0000000000000000 ) ) ;
#14671 = EDGE_CURVE ( 'NONE', #129212, #144252, #163302, .T. ) ;
#14670 = TOROIDAL_SURFACE ( 'NONE', #56315, 0.2000000000000000111, 0.1000000000000000056 ) ;
#14672 = DIRECTION ( 'NONE',  ( -0.000000000000000000, -0.8814952561688430555, 0.4721928772777346239 ) ) ;
#14673 = DIRECTION ( 'NONE',  ( -1.000000000000000000, -0.000000000000000000, 0.000000000000000000 ) ) ;
#14674 = CARTESIAN_POINT ( 'NONE',  ( 18.60000000000000142, -9.321008403350125704, -174.7359382490778614 ) ) ;
#14675 = ORIENTED_EDGE ( 'NONE', *, *, #150073, .T. ) ;
#14676 = CARTESIAN_POINT ( 'NONE',  ( 12.25000000000000000, 66.65000000001185754, -86.27310748452437394 ) ) ;
#14677 = CARTESIAN_POINT ( 'NONE',  ( -18.50000000000000000, 43.63140573099096287, -239.9077968784524444 ) ) ;
#14678 = CYLINDRICAL_SURFACE ( 'NONE', #19460, 0.09999999999998898659 ) ;
#14679 = EDGE_CURVE ( 'NONE', #45216, #17064, #85007, .T. ) ;
#14681 = DIRECTION ( 'NONE',  ( 1.000000000000000000, 0.000000000000000000, 0.000000000000000000 ) ) ;
#14680 = DIRECTION ( 'NONE',  ( 0.000000000000000000, 6.982962677686266711E-15, -1.000000000000000000 ) ) ;
#14682 = FACE_OUTER_BOUND ( 'NONE', #142517, .T. ) ;
#14683 = DIRECTION ( 'NONE',  ( 0.000000000000000000, 0.000000000000000000, -1.000000000000000000 ) ) ;
#14684 = DIRECTION ( 'NONE',  ( 0.000000000000000000, 0.1575844902526835067, 0.9875055080513738259 ) ) ;
#14685 = CARTESIAN_POINT ( 'NONE',  ( 21.51976009735019346, 6.910458441670357388, -33.50000000000000000 ) ) ;
#14686 = EDGE_CURVE ( 'NONE', #100546, #124483, #235349, .T. ) ;
#14687 = ADVANCED_FACE ( 'NONE', ( #202416 ), #23816, .T. ) ;
#14689 = ORIENTED_EDGE ( 'NONE', *, *, #57593, .T. ) ;
#14688 = AXIS2_PLACEMENT_3D ( 'NONE', #223675, #183286, #63320 ) ;
#14690 = VECTOR ( 'NONE', #236674, 1000.000000000000000 ) ;
#14691 = ORIENTED_EDGE ( 'NONE', *, *, #178030, .F. ) ;
#14692 = EDGE_CURVE ( 'NONE', #70987, #134912, #223617, .T. ) ;
#14693 = DIRECTION ( 'NONE',  ( 1.000000000000000000, 0.000000000000000000, -0.000000000000000000 ) ) ;
#14694 = SPHERICAL_SURFACE ( 'NONE', #98839, 0.1000000000000000056 ) ;
#14695 = ORIENTED_EDGE ( 'NONE', *, *, #241057, .T. ) ;
#14696 = CARTESIAN_POINT ( 'NONE',  ( -23.15000000000000213, -9.599999999988845900, -124.1060308773475924 ) ) ;
#14697 = EDGE_CURVE ( 'NONE', #17092, #120951, #10520, .T. ) ;
#14698 = ORIENTED_EDGE ( 'NONE', *, *, #23138, .T. ) ;
#14699 = FILL_AREA_STYLE_COLOUR ( '', #15089 ) ;
#14700 = EDGE_CURVE ( 'NONE', #142940, #226886, #125459, .T. ) ;
#14701 = ORIENTED_EDGE ( 'NONE', *, *, #49751, .T. ) ;
#14702 = CARTESIAN_POINT ( 'NONE',  ( 21.07954640115298162, 75.93399229287234675, -109.3523951805481573 ) ) ;
#14703 = AXIS2_PLACEMENT_3D ( 'NONE', #73660, #29409, #153202 ) ;
#14704 = VERTEX_POINT ( 'NONE', #182881 ) ;
#14705 = DIRECTION ( 'NONE',  ( -0.000000000000000000, -1.897661533703519897E-16, 1.000000000000000000 ) ) ;
#14706 = CYLINDRICAL_SURFACE ( 'NONE', #111746, 0.09999999999999939493 ) ;
#14707 = DIRECTION ( 'NONE',  ( 1.000000000000000000, 0.000000000000000000, 0.000000000000000000 ) ) ;
#14708 = AXIS2_PLACEMENT_3D ( 'NONE', #147187, #149785, #25972 ) ;
#14709 = CARTESIAN_POINT ( 'NONE',  ( 18.44364597020196328, 85.49048731717437022, -129.4651295948404197 ) ) ;
#14710 = CARTESIAN_POINT ( 'NONE',  ( 18.49999999999999289, 10.20857864377384239, -192.2671572875252934 ) ) ;
#14712 = ORIENTED_EDGE ( 'NONE', *, *, #252639, .T. ) ;
#14711 = CARTESIAN_POINT ( 'NONE',  ( -16.79270642812319991, 30.19479984366789438, -234.8051300827147259 ) ) ;
#14713 = FACE_OUTER_BOUND ( 'NONE', #211737, .T. ) ;
#14714 = EDGE_CURVE ( 'NONE', #32098, #62912, #143765, .T. ) ;
#14715 = CARTESIAN_POINT ( 'NONE',  ( 0.9000000000000547562, 64.35000000001120668, -10.02310748452479139 ) ) ;
#14716 = DIRECTION ( 'NONE',  ( 0.000000000000000000, 0.9126074666063770380, 0.4088369013363281068 ) ) ;
#14717 = DIRECTION ( 'NONE',  ( -0.000000000000000000, 0.1350103645451807555, 0.9908441862701610203 ) ) ;
#14718 = FACE_OUTER_BOUND ( 'NONE', #145533, .T. ) ;
#14719 = ORIENTED_EDGE ( 'NONE', *, *, #173317, .T. ) ;
#14720 = FACE_OUTER_BOUND ( 'NONE', #156973, .T. ) ;
#14721 = ORIENTED_EDGE ( 'NONE', *, *, #250746, .T. ) ;
#14722 = CARTESIAN_POINT ( 'NONE',  ( -20.64999999999999858, 19.73066058418984170, -238.2142830767208466 ) ) ;
#14723 = EDGE_LOOP ( 'NONE', ( #184292, #87683, #51984, #57120, #229485 ) ) ;
#14724 = CIRCLE ( 'NONE', #181310, 0.2000000000000076994 ) ;
#14726 = CARTESIAN_POINT ( 'NONE',  ( -21.05000000000000071, 2.953700692300310848, -208.6327728934509764 ) ) ;
#14725 = CIRCLE ( 'NONE', #123030, 0.1000000000000028644 ) ;
#14727 = CARTESIAN_POINT ( 'NONE',  ( -16.94275863006528482, 9.989496048667513506, -20.89169738207657900 ) ) ;
#14728 = CARTESIAN_POINT ( 'NONE',  ( 21.30000000000002558, 76.00000000001267608, -203.5231074845243597 ) ) ;
#14729 = VERTEX_POINT ( 'NONE', #227102 ) ;
#14730 = EDGE_LOOP ( 'NONE', ( #769, #143049, #150264 ) ) ;
#14731 = CARTESIAN_POINT ( 'NONE',  ( -18.59999999999999787, 78.45218979564165807, -232.7313097695096076 ) ) ;
#14732 = CARTESIAN_POINT ( 'NONE',  ( 18.59999999999999076, 65.50857864377465489, -111.7731074845243739 ) ) ;
#14733 = ADVANCED_FACE ( 'NONE', ( #65468 ), #85653, .T. ) ;
#14734 = DIRECTION ( 'NONE',  ( 1.000000000000000000, 0.000000000000000000, 0.000000000000000000 ) ) ;
#14735 = CARTESIAN_POINT ( 'NONE',  ( -16.77683809663752257, 23.65833333333332433, -16.75000000000000000 ) ) ;
#14738 = DIRECTION ( 'NONE',  ( 0.000000000000000000, -3.339342691255721203E-13, 1.000000000000000000 ) ) ;
#14737 = CIRCLE ( 'NONE', #156397, 0.09999999999999939493 ) ;
#14736 = CARTESIAN_POINT ( 'NONE',  ( -23.25000000000000000, 76.00000000001142553, -36.02310748452432421 ) ) ;
#14739 = LINE ( 'NONE', #35588, #249197 ) ;
#14740 = EDGE_CURVE ( 'NONE', #198528, #176003, #9342, .T. ) ;
#14741 = CIRCLE ( 'NONE', #201983, 0.09999999999999939493 ) ;
#14742 = CARTESIAN_POINT ( 'NONE',  ( 13.43663047529820176, 9.446645344706402270, -51.91080645610020383 ) ) ;
#14743 = DIRECTION ( 'NONE',  ( -1.000000000000000000, 0.000000000000000000, -0.000000000000000000 ) ) ;
#14745 = EDGE_LOOP ( 'NONE', ( #41555, #192487, #233042, #230766 ) ) ;
#14744 = VECTOR ( 'NONE', #168678, 1000.000000000000114 ) ;
#14746 = DIRECTION ( 'NONE',  ( 0.000000000000000000, 6.982962677686266711E-15, -1.000000000000000000 ) ) ;
#14747 = AXIS2_PLACEMENT_3D ( 'NONE', #67888, #223100, #163153 ) ;
#14749 = VERTEX_POINT ( 'NONE', #128028 ) ;
#14748 = CARTESIAN_POINT ( 'NONE',  ( 18.39999999999999503, 64.25000000001179501, -78.77310748452438816 ) ) ;
#14750 = CARTESIAN_POINT ( 'NONE',  ( 20.95265033839679347, 65.48774916754547348, -195.9573437284944646 ) ) ;
#14751 = CARTESIAN_POINT ( 'NONE',  ( 23.15000000000000213, 84.59626168225530307, -160.5729799673740104 ) ) ;
#14753 = DIRECTION ( 'NONE',  ( 0.000000000000000000, -1.000000000000000000, 0.000000000000000000 ) ) ;
#14752 = CARTESIAN_POINT ( 'NONE',  ( -21.14999999999999858, 67.23127455305841238, -235.8551265064783991 ) ) ;
#14754 = EDGE_CURVE ( 'NONE', #132210, #157237, #218772, .T. ) ;
#14755 = EDGE_CURVE ( 'NONE', #35113, #201330, #231463, .T. ) ;
#14757 = VERTEX_POINT ( 'NONE', #54881 ) ;
#14756 = DIRECTION ( 'NONE',  ( 1.000000000000000000, -0.000000000000000000, 0.000000000000000000 ) ) ;
#14758 = DIRECTION ( 'NONE',  ( 1.000000000000000000, 0.000000000000000000, 0.000000000000000000 ) ) ;
#14759 = CYLINDRICAL_SURFACE ( 'NONE', #237124, 0.09999999999999939493 ) ;
#14760 = DIRECTION ( 'NONE',  ( 1.000000000000000000, 0.000000000000000000, -0.000000000000000000 ) ) ;
#14761 = DIRECTION ( 'NONE',  ( 0.000000000000000000, -0.4088369013363282733, 0.9126074666063771490 ) ) ;
#14762 = CARTESIAN_POINT ( 'NONE',  ( -18.59999999999999787, 10.33248238083634440, -139.5948465439131780 ) ) ;
#14763 = ORIENTED_EDGE ( 'NONE', *, *, #180906, .F. ) ;
#14764 = CARTESIAN_POINT ( 'NONE',  ( -21.04999999999994387, 64.35000000001120668, -30.12310748452479103 ) ) ;
#14765 = EDGE_CURVE ( 'NONE', #221732, #47300, #194435, .T. ) ;
#14766 = ORIENTED_EDGE ( 'NONE', *, *, #26669, .T. ) ;
#14767 = CARTESIAN_POINT ( 'NONE',  ( 22.59999954896768770, 76.00882823225521179, -215.2736161585923469 ) ) ;
#14768 = ORIENTED_EDGE ( 'NONE', *, *, #169629, .T. ) ;
#14769 = CARTESIAN_POINT ( 'NONE',  ( -17.11825945287481332, 9.950000000011138823, -154.7500000000000284 ) ) ;
#14770 = VECTOR ( 'NONE', #217522, 1000.000000000000000 ) ;
#14771 = VERTEX_POINT ( 'NONE', #11945 ) ;
#14772 = AXIS2_PLACEMENT_3D ( 'NONE', #246451, #147351, #207341 ) ;
#14773 = EDGE_CURVE ( 'NONE', #186539, #144523, #169752, .T. ) ;
#14774 = DIRECTION ( 'NONE',  ( 1.713247197920696616E-14, 0.9876197685951252359, -0.1568667991644863424 ) ) ;
#14776 = CARTESIAN_POINT ( 'NONE',  ( 20.94999999999999929, 71.00000000001253397, -182.4283735034374843 ) ) ;
#14775 = TOROIDAL_SURFACE ( 'NONE', #10470, 7.800000000000000711, 0.1000000000000000056 ) ;
#14777 = ORIENTED_EDGE ( 'NONE', *, *, #43192, .T. ) ;
#14778 = CIRCLE ( 'NONE', #110410, 0.8750000000000007772 ) ;
#14779 = AXIS2_PLACEMENT_3D ( 'NONE', #182193, #225131, #68658 ) ;
#14781 = FACE_OUTER_BOUND ( 'NONE', #43905, .T. ) ;
#14780 = CIRCLE ( 'NONE', #181180, 4.049999999999990941 ) ;
#14782 = LINE ( 'NONE', #144272, #7441 ) ;
#14783 = CARTESIAN_POINT ( 'NONE',  ( -23.15000000000000213, 2.500000000011154633, -187.7753780772378889 ) ) ;
#14784 = CARTESIAN_POINT ( 'NONE',  ( 21.30000000000002558, 76.00000000001195133, -103.0231074845243171 ) ) ;
#14785 = CARTESIAN_POINT ( 'NONE',  ( -16.94165728009537020, 66.01213024408822605, -115.6320524760141666 ) ) ;
#14787 = ORIENTED_EDGE ( 'NONE', *, *, #45292, .T. ) ;
#14786 = ADVANCED_FACE ( 'NONE', ( #173620 ), #106335, .T. ) ;
#14788 = CARTESIAN_POINT ( 'NONE',  ( -18.50000000000000000, 85.40000000001209912, -129.6410656363516125 ) ) ;
#14789 = VERTEX_POINT ( 'NONE', #114872 ) ;
#14791 = ORIENTED_EDGE ( 'NONE', *, *, #114109, .F. ) ;
#14790 = CARTESIAN_POINT ( 'NONE',  ( 21.06600267594171783, 67.22483393081196823, -90.81884470214961880 ) ) ;
#14792 = VECTOR ( 'NONE', #155691, 1000.000000000000000 ) ;
#14793 = ORIENTED_EDGE ( 'NONE', *, *, #4582, .T. ) ;
#14794 = CARTESIAN_POINT ( 'NONE',  ( 20.94999999999999929, 85.40000000001252545, -179.9170766071767389 ) ) ;
#14795 = CARTESIAN_POINT ( 'NONE',  ( 20.12500000000000355, 65.75804927292941215, -128.6629037574382721 ) ) ;
#14796 = AXIS2_PLACEMENT_3D ( 'NONE', #66833, #104631, #47243 ) ;
#14797 = CARTESIAN_POINT ( 'NONE',  ( -23.25000000000000000, 2.000000000011154189, -80.22462192276213955 ) ) ;
#14798 = FACE_OUTER_BOUND ( 'NONE', #41506, .T. ) ;
#14799 = VERTEX_POINT ( 'NONE', #251811 ) ;
#14800 = CIRCLE ( 'NONE', #160539, 0.09999999999999939493 ) ;
#14801 = CARTESIAN_POINT ( 'NONE',  ( -23.25000000000000000, 64.25000000001173817, -81.27310748452440237 ) ) ;
#14802 = FACE_OUTER_BOUND ( 'NONE', #142238, .T. ) ;
#14803 = AXIS2_PLACEMENT_3D ( 'NONE', #181910, #123218, #64524 ) ;
#14804 = EDGE_CURVE ( 'NONE', #14945, #8661, #119037, .T. ) ;
#14805 = VERTEX_POINT ( 'NONE', #247953 ) ;
#14807 = VERTEX_POINT ( 'NONE', #109720 ) ;
#14806 = DIRECTION ( 'NONE',  ( -1.000000000000000000, -0.000000000000000000, 0.000000000000000000 ) ) ;
#14809 = EDGE_CURVE ( 'NONE', #255868, #192876, #102229, .T. ) ;
#14808 = CARTESIAN_POINT ( 'NONE',  ( 18.49999999999999289, 64.25000000001173817, -81.27310748452440237 ) ) ;
#14810 = DIRECTION ( 'NONE',  ( 0.000000000000000000, 0.4859085964047519801, 0.8740096314915323239 ) ) ;
#14811 = CARTESIAN_POINT ( 'NONE',  ( -23.15000000000000213, 87.48912529308779540, -72.62310748452422615 ) ) ;
#14812 = ORIENTED_EDGE ( 'NONE', *, *, #53096, .T. ) ;
#14813 = ADVANCED_FACE ( 'NONE', ( #250522 ), #249257, .T. ) ;
#14814 = DIRECTION ( 'NONE',  ( 0.000000000000000000, 0.4088369013362748716, -0.9126074666064009078 ) ) ;
#14815 = ORIENTED_EDGE ( 'NONE', *, *, #39161, .T. ) ;
#14816 = CARTESIAN_POINT ( 'NONE',  ( 23.24999999999999289, 64.23880400315596262, -222.2474036988971307 ) ) ;
#14817 = ADVANCED_FACE ( 'NONE', ( #53619 ), #95310, .T. ) ;
#14818 = CARTESIAN_POINT ( 'NONE',  ( 21.05315837477245111, 64.25000000001249134, -176.8647514783818906 ) ) ;
#14819 = EDGE_CURVE ( 'NONE', #226285, #41654, #39932, .T. ) ;
#14820 = DIRECTION ( 'NONE',  ( 0.000000000000000000, 1.000000000000000000, 6.982962677686266711E-15 ) ) ;
#14821 = AXIS2_PLACEMENT_3D ( 'NONE', #176155, #155318, #40515 ) ;
#14822 = AXIS2_PLACEMENT_3D ( 'NONE', #84367, #223914, #13879 ) ;
#14823 = EDGE_CURVE ( 'NONE', #167915, #213068, #68979, .T. ) ;
#14824 = CIRCLE ( 'NONE', #85659, 2.000000000000001776 ) ;
#14825 = ORIENTED_EDGE ( 'NONE', *, *, #231444, .F. ) ;
#14826 = CARTESIAN_POINT ( 'NONE',  ( 20.84999999999999787, 11.75000000001116085, -60.08085275404130243 ) ) ;
#14827 = VECTOR ( 'NONE', #118774, 1000.000000000000000 ) ;
#14828 = CIRCLE ( 'NONE', #60574, 0.1999999999999987899 ) ;
#14829 = VERTEX_POINT ( 'NONE', #30214 ) ;
#14830 = DIRECTION ( 'NONE',  ( 0.000000000000000000, 0.8814952561688476074, -0.4721928772777262417 ) ) ;
#14831 = EDGE_CURVE ( 'NONE', #159614, #253024, #256312, .T. ) ;
#14833 = VERTEX_POINT ( 'NONE', #51010 ) ;
#14832 = DIRECTION ( 'NONE',  ( 0.000000000000000000, 0.1568667991644355497, -0.9876197685951332295 ) ) ;
#14834 = DIRECTION ( 'NONE',  ( 0.000000000000000000, 0.000000000000000000, 1.000000000000000000 ) ) ;
#14835 = DIRECTION ( 'NONE',  ( -0.000000000000000000, -0.000000000000000000, -1.000000000000000000 ) ) ;
#14836 = DIRECTION ( 'NONE',  ( 1.000000000000000000, 0.000000000000000000, 0.000000000000000000 ) ) ;
#14838 = DIRECTION ( 'NONE',  ( 0.000000000000000000, 0.000000000000000000, 1.000000000000000000 ) ) ;
#14837 = CIRCLE ( 'NONE', #152779, 0.1000000000000029060 ) ;
#14839 = LINE ( 'NONE', #116484, #168601 ) ;
#14840 = AXIS2_PLACEMENT_3D ( 'NONE', #210928, #184944, #165390 ) ;
#14841 = DIRECTION ( 'NONE',  ( -1.000000000000000000, 0.000000000000000000, 0.000000000000000000 ) ) ;
#14842 = CARTESIAN_POINT ( 'NONE',  ( -16.77683809663752257, 66.05416425680813575, -157.3591584654202222 ) ) ;
#14844 = ORIENTED_EDGE ( 'NONE', *, *, #87761, .F. ) ;
#14843 = DIRECTION ( 'NONE',  ( 0.000000000000000000, 0.000000000000000000, 1.000000000000000000 ) ) ;
#14845 = AXIS2_PLACEMENT_3D ( 'NONE', #6336, #183716, #102855 ) ;
#14846 = CARTESIAN_POINT ( 'NONE',  ( -21.05000000000000071, 41.42187432231295219, -260.1830396872097140 ) ) ;
#14847 = TOROIDAL_SURFACE ( 'NONE', #160602, 4.099999999999999645, 0.1000000000000000056 ) ;
#14848 = CARTESIAN_POINT ( 'NONE',  ( -20.54999999999999716, -9.000000000000001776, -23.60603087734756045 ) ) ;
#14849 = LINE ( 'NONE', #209161, #97324 ) ;
#14850 = EDGE_LOOP ( 'NONE', ( #189057, #86213, #43522, #238866 ) ) ;
#14851 = CARTESIAN_POINT ( 'NONE',  ( 20.94999999999999574, 74.83729825007408465, -128.4231074845243086 ) ) ;
#14852 = CYLINDRICAL_SURFACE ( 'NONE', #160291, 0.1000000000000013656 ) ;
#14853 = ORIENTED_EDGE ( 'NONE', *, *, #148042, .T. ) ;
#14854 = AXIS2_PLACEMENT_3D ( 'NONE', #49959, #227313, #188198 ) ;
#14855 = CIRCLE ( 'NONE', #77188, 0.09999999999999939493 ) ;
#14856 = EDGE_CURVE ( 'NONE', #118580, #93087, #191875, .T. ) ;
#14857 = AXIS2_PLACEMENT_3D ( 'NONE', #109700, #245387, #47148 ) ;
#14858 = CARTESIAN_POINT ( 'NONE',  ( -21.07016717456946608, 61.13071397353302672, -234.2006012892922513 ) ) ;
#14859 = ORIENTED_EDGE ( 'NONE', *, *, #114447, .F. ) ;
#14860 = DIRECTION ( 'NONE',  ( 0.000000000000000000, -0.2128009952263403282, 0.9770955615653358350 ) ) ;
#14861 = ORIENTED_EDGE ( 'NONE', *, *, #141473, .F. ) ;
#14862 = EDGE_CURVE ( 'NONE', #251548, #1294, #135572, .T. ) ;
#14864 = ORIENTED_EDGE ( 'NONE', *, *, #112067, .T. ) ;
#14863 = CARTESIAN_POINT ( 'NONE',  ( -20.85000000000000142, 1.115600667400684642E-11, -67.00000000000000000 ) ) ;
#14865 = DIRECTION ( 'NONE',  ( 6.938893903907030216E-14, 0.000000000000000000, 1.000000000000000000 ) ) ;
#14866 = VERTEX_POINT ( 'NONE', #230991 ) ;
#14867 = EDGE_CURVE ( 'NONE', #101132, #179727, #148063, .T. ) ;
#14868 = DIRECTION ( 'NONE',  ( 0.000000000000000000, 0.9126074666063769270, 0.4088369013363280513 ) ) ;
#14869 = EDGE_CURVE ( 'NONE', #61048, #224619, #212702, .T. ) ;
#14870 = VERTEX_POINT ( 'NONE', #14519 ) ;
#14872 = VERTEX_POINT ( 'NONE', #94010 ) ;
#14871 = ORIENTED_EDGE ( 'NONE', *, *, #41436, .F. ) ;
#14873 = DIRECTION ( 'NONE',  ( -2.978066053179069723E-16, -1.000000000000000000, -7.742971738265580590E-15 ) ) ;
#14875 = VERTEX_POINT ( 'NONE', #74508 ) ;
#14874 = DIRECTION ( 'NONE',  ( 0.7071359030027322135, 0.3338770338705078222, 0.6232856014206827888 ) ) ;
#14876 = LINE ( 'NONE', #249622, #248009 ) ;
#14877 = VECTOR ( 'NONE', #103440, 1000.000000000000000 ) ;
#14878 = ORIENTED_EDGE ( 'NONE', *, *, #157064, .T. ) ;
#14879 = VECTOR ( 'NONE', #222544, 1000.000000000000000 ) ;
#14880 = VERTEX_POINT ( 'NONE', #154054 ) ;
#14881 = EDGE_CURVE ( 'NONE', #192091, #112369, #95870, .T. ) ;
#14882 = DIRECTION ( 'NONE',  ( -0.000000000000000000, 0.9910827722268049644, -0.1332476588733589318 ) ) ;
#14883 = CARTESIAN_POINT ( 'NONE',  ( 21.22070241538126467, 75.90108096947668059, -75.99305375739393753 ) ) ;
#14884 = DIRECTION ( 'NONE',  ( -2.840903330521632269E-16, -0.8700118002898356018, 0.4930308989875170078 ) ) ;
#14885 = EDGE_LOOP ( 'NONE', ( #240958, #256390, #132223, #26538 ) ) ;
#14886 = DIRECTION ( 'NONE',  ( -1.000000000000000000, 0.000000000000000000, -0.000000000000000000 ) ) ;
#14887 = CARTESIAN_POINT ( 'NONE',  ( -18.60000000000000142, -9.321008403350123928, -74.23593824907794669 ) ) ;
#14888 = FACE_OUTER_BOUND ( 'NONE', #11749, .T. ) ;
#14889 = VERTEX_POINT ( 'NONE', #116174 ) ;
#14890 = CARTESIAN_POINT ( 'NONE',  ( -21.14999999999999858, 11.75000000001115552, -40.22613063605918882 ) ) ;
#14891 = CARTESIAN_POINT ( 'NONE',  ( -18.43459694179580310, 38.00868472153695876, -261.0447666131053097 ) ) ;
#14892 = PLANE ( 'NONE',  #199409 ) ;
#14893 = EDGE_LOOP ( 'NONE', ( #61675, #142377, #175182, #100694 ) ) ;
#14894 = CARTESIAN_POINT ( 'NONE',  ( -16.92209698673895701, 14.14609827904097017, -219.1958258126950909 ) ) ;
#14895 = VERTEX_POINT ( 'NONE', #20939 ) ;
#14896 = ORIENTED_EDGE ( 'NONE', *, *, #201184, .T. ) ;
#14897 = AXIS2_PLACEMENT_3D ( 'NONE', #249356, #32907, #227205 ) ;
#14898 = AXIS2_PLACEMENT_3D ( 'NONE', #59563, #23070, #120892 ) ;
#14899 = CARTESIAN_POINT ( 'NONE',  ( 18.60000000000000142, -9.399999999988782662, -107.7972597596633193 ) ) ;
#14900 = EDGE_LOOP ( 'NONE', ( #26759, #70682, #2680, #111596 ) ) ;
#14901 = VERTEX_POINT ( 'NONE', #99138 ) ;
#14902 = CARTESIAN_POINT ( 'NONE',  ( -22.50000000000000000, 11.36146383068193444, -198.4232501820394816 ) ) ;
#14903 = ADVANCED_FACE ( 'NONE', ( #254358 ), #252108, .F. ) ;
#14904 = DIRECTION ( 'NONE',  ( 0.000000000000000000, 0.000000000000000000, 1.000000000000000000 ) ) ;
#14905 = ORIENTED_EDGE ( 'NONE', *, *, #211785, .T. ) ;
#14906 = ADVANCED_FACE ( 'NONE', ( #220405 ), #77021, .F. ) ;
#14907 = EDGE_LOOP ( 'NONE', ( #76843, #221871, #29608, #2864 ) ) ;
#14908 = FACE_OUTER_BOUND ( 'NONE', #59589, .T. ) ;
#14909 = CARTESIAN_POINT ( 'NONE',  ( -18.51024323315077424, 65.68895814178220860, -64.00265578621379348 ) ) ;
#14910 = EDGE_LOOP ( 'NONE', ( #198925, #75826, #165276, #72603 ) ) ;
#14911 = ADVANCED_FACE ( 'NONE', ( #22212 ), #138264, .T. ) ;
#14912 = CIRCLE ( 'NONE', #119135, 0.09999999999999939493 ) ;
#14913 = ORIENTED_EDGE ( 'NONE', *, *, #248103, .F. ) ;
#14914 = AXIS2_PLACEMENT_3D ( 'NONE', #72784, #37489, #132741 ) ;
#14915 = AXIS2_PLACEMENT_3D ( 'NONE', #163071, #143474, #165629 ) ;
#14916 = CARTESIAN_POINT ( 'NONE',  ( 21.14999999999999858, 69.45934304831143891, -203.5231074845243882 ) ) ;
#14917 =( GEOMETRIC_REPRESENTATION_CONTEXT ( 3 ) GLOBAL_UNCERTAINTY_ASSIGNED_CONTEXT ( ( #16711 ) ) GLOBAL_UNIT_ASSIGNED_CONTEXT ( ( #218277, #123066, #200034 ) ) REPRESENTATION_CONTEXT ( 'NONE', 'WORKASPACE' ) );
#14918 = DIRECTION ( 'NONE',  ( 1.000000000000000000, -3.265361837132813093E-16, -2.280189983783949500E-30 ) ) ;
#14919 = DIRECTION ( 'NONE',  ( -1.000000000000000000, -0.000000000000000000, -0.000000000000000000 ) ) ;
#14920 = FACE_OUTER_BOUND ( 'NONE', #206615, .T. ) ;
#14921 = CARTESIAN_POINT ( 'NONE',  ( -18.39999999999999858, 11.47316190337362762, -76.32594606680801519 ) ) ;
#14923 = ADVANCED_FACE ( 'NONE', ( #137000 ), #36654, .T. ) ;
#14922 = CARTESIAN_POINT ( 'NONE',  ( -18.59999999999999787, 66.65000000001180069, -81.77310748452437394 ) ) ;
#14925 = CARTESIAN_POINT ( 'NONE',  ( 23.14999999999999858, 1.115625160336667635E-11, -65.00000000000000000 ) ) ;
#14924 = DIRECTION ( 'NONE',  ( 0.000000000000000000, -8.267618268485201230E-15, 1.000000000000000000 ) ) ;
#14926 = CARTESIAN_POINT ( 'NONE',  ( 23.24999999999999289, 64.25000000001185185, -90.87310748452438247 ) ) ;
#14927 = CARTESIAN_POINT ( 'NONE',  ( 18.59999999999998366, 1.115600667400684642E-11, -67.00000000000000000 ) ) ;
#14928 = FACE_OUTER_BOUND ( 'NONE', #16453, .T. ) ;
#14929 = DIRECTION ( 'NONE',  ( -1.000000000000000000, 0.000000000000000000, 0.000000000000000000 ) ) ;
#14930 = AXIS2_PLACEMENT_3D ( 'NONE', #166278, #124561, #145385 ) ;
#14931 = ORIENTED_EDGE ( 'NONE', *, *, #132450, .F. ) ;
#14932 = VECTOR ( 'NONE', #156281, 1000.000000000000000 ) ;
#14933 = EDGE_CURVE ( 'NONE', #232638, #155954, #51, .T. ) ;
#14935 = VERTEX_POINT ( 'NONE', #79574 ) ;
#14934 = DIRECTION ( 'NONE',  ( 0.000000000000000000, -7.116814260417668513E-15, 1.000000000000000000 ) ) ;
#14936 = AXIS2_PLACEMENT_3D ( 'NONE', #67706, #209792, #66428 ) ;
#14937 = EDGE_CURVE ( 'NONE', #246752, #198869, #89786, .T. ) ;
#14939 = ADVANCED_FACE ( 'NONE', ( #159164 ), #219090, .F. ) ;
#14938 = VECTOR ( 'NONE', #155306, 1000.000000000000000 ) ;
#14940 = AXIS2_PLACEMENT_3D ( 'NONE', #190681, #250611, #168575 ) ;
#14941 = DIRECTION ( 'NONE',  ( 0.000000000000000000, 0.9126074666063753726, 0.4088369013363316040 ) ) ;
#14942 = EDGE_LOOP ( 'NONE', ( #5541, #160162, #141582, #98498 ) ) ;
#14943 = DIRECTION ( 'NONE',  ( 0.000000000000000000, 0.2128009952263604232, -0.9770955615653316162 ) ) ;
#14944 = SPHERICAL_SURFACE ( 'NONE', #220378, 0.1000000000000000056 ) ;
#14945 = VERTEX_POINT ( 'NONE', #174906 ) ;
#14946 = EDGE_CURVE ( 'NONE', #38206, #244808, #135702, .T. ) ;
#14948 = CARTESIAN_POINT ( 'NONE',  ( 21.11701782572533048, 60.08865071491936760, -221.2306002442901729 ) ) ;
#14947 = VECTOR ( 'NONE', #166614, 1000.000000000000000 ) ;
#14949 = DIRECTION ( 'NONE',  ( -1.000000000000000000, 0.000000000000000000, 0.000000000000000000 ) ) ;
#14950 = ADVANCED_FACE ( 'NONE', ( #120041 ), #238672, .T. ) ;
#14951 = CIRCLE ( 'NONE', #160730, 0.09999999999998898659 ) ;
#14952 = CARTESIAN_POINT ( 'NONE',  ( -21.12230431290520727, 10.17345785877508391, -228.0379268863081847 ) ) ;
#14954 = ORIENTED_EDGE ( 'NONE', *, *, #92215, .T. ) ;
#14953 = DIRECTION ( 'NONE',  ( 1.000000000000000000, 0.000000000000000000, 0.000000000000000000 ) ) ;
#14955 = CARTESIAN_POINT ( 'NONE',  ( 20.94999999999999929, 1.360870587203197646, -108.5729979270909951 ) ) ;
#14956 = AXIS2_PLACEMENT_3D ( 'NONE', #173550, #52243, #17006 ) ;
#14957 = CIRCLE ( 'NONE', #119021, 0.1000000000000028644 ) ;
#14959 = ORIENTED_EDGE ( 'NONE', *, *, #91830, .T. ) ;
#14958 = CARTESIAN_POINT ( 'NONE',  ( -18.41817142474038960, 85.49870306661395603, -96.41914199688721965 ) ) ;
#14960 = LINE ( 'NONE', #174061, #91767 ) ;
#14961 = DIRECTION ( 'NONE',  ( -0.000000000000000000, 0.4721928772777346239, 0.8814952561688430555 ) ) ;
#14962 = FACE_OUTER_BOUND ( 'NONE', #146804, .T. ) ;
#14963 = DIRECTION ( 'NONE',  ( 0.000000000000000000, 0.000000000000000000, -1.000000000000000000 ) ) ;
#14964 = EDGE_CURVE ( 'NONE', #257328, #53042, #96566, .T. ) ;
#14966 = CARTESIAN_POINT ( 'NONE',  ( 20.94999999999999574, 1.750000000011155743, -112.1695115579016857 ) ) ;
#14965 = CARTESIAN_POINT ( 'NONE',  ( -21.05000000000000071, 77.16270174994990327, -94.92310748452430857 ) ) ;
#14967 = CARTESIAN_POINT ( 'NONE',  ( -23.25000000000000000, 1.910280373842930812, -188.3686321448010403 ) ) ;
#14968 = FACE_OUTER_BOUND ( 'NONE', #254370, .T. ) ;
#14969 = CARTESIAN_POINT ( 'NONE',  ( -20.94999999999999929, 44.47083028126616000, -247.4212268238128161 ) ) ;
#14970 = CYLINDRICAL_SURFACE ( 'NONE', #234771, 0.09999999999999939493 ) ;
#14971 = EDGE_CURVE ( 'NONE', #68121, #85685, #156476, .T. ) ;
#14972 = DIRECTION ( 'NONE',  ( 1.000000000000000000, 0.000000000000000000, 0.000000000000000000 ) ) ;
#14973 = EDGE_CURVE ( 'NONE', #162457, #14005, #248297, .T. ) ;
#14974 = ORIENTED_EDGE ( 'NONE', *, *, #93525, .F. ) ;
#14975 = DIRECTION ( 'NONE',  ( -0.5932847527679298016, -0.8049926720990051576, -5.621233785078291429E-15 ) ) ;
#14976 = ORIENTED_EDGE ( 'NONE', *, *, #94324, .F. ) ;
#14977 = ORIENTED_EDGE ( 'NONE', *, *, #200593, .F. ) ;
#14978 = EDGE_CURVE ( 'NONE', #172545, #89486, #63888, .T. ) ;
#14979 = DIRECTION ( 'NONE',  ( 0.000000000000000000, 1.000000000000000000, -6.938893903907270030E-14 ) ) ;
#14980 = CARTESIAN_POINT ( 'NONE',  ( -18.59999999999999787, -1.835859311432481045, -145.5044391687985694 ) ) ;
#14981 = ORIENTED_EDGE ( 'NONE', *, *, #193069, .F. ) ;
#14982 = ADVANCED_FACE ( 'NONE', ( #143420 ), #98138, .T. ) ;
#14983 = CIRCLE ( 'NONE', #160753, 0.09999999999999907574 ) ;
#14984 = EDGE_CURVE ( 'NONE', #116632, #69997, #87281, .T. ) ;
#14985 = TOROIDAL_SURFACE ( 'NONE', #235527, 0.4000000000000012990, 0.1000000000000000056 ) ;
#14986 = ORIENTED_EDGE ( 'NONE', *, *, #176207, .F. ) ;
#14987 = CARTESIAN_POINT ( 'NONE',  ( -21.05000000000000071, 30.84055724867796044, -252.2517348665298016 ) ) ;
#14988 = VECTOR ( 'NONE', #78104, 1000.000000000000000 ) ;
#14989 = CIRCLE ( 'NONE', #223247, 11.65000000000000391 ) ;
#14990 = EDGE_CURVE ( 'NONE', #49647, #242990, #185666, .T. ) ;
#14991 = ORIENTED_EDGE ( 'NONE', *, *, #168902, .F. ) ;
#14992 = EDGE_LOOP ( 'NONE', ( #74267, #112887, #59412 ) ) ;
#14993 = TOROIDAL_SURFACE ( 'NONE', #227363, 0.2000000000000000111, 0.1000000000000000056 ) ;
#14994 = DIRECTION ( 'NONE',  ( 0.000000000000000000, 0.000000000000000000, 1.000000000000000000 ) ) ;
#14995 = DIRECTION ( 'NONE',  ( 1.000000000000000000, 0.000000000000000000, 0.000000000000000000 ) ) ;
#14996 = DIRECTION ( 'NONE',  ( 0.000000000000000000, -1.000000000000000000, -6.982962677686265922E-15 ) ) ;
#14997 = CARTESIAN_POINT ( 'NONE',  ( 12.93279065517212700, 27.56753475832528011, -233.9973862756306744 ) ) ;
#14998 = DIRECTION ( 'NONE',  ( 1.000000000000000000, -7.136802563874200093E-16, -1.554319503706925554E-16 ) ) ;
#15000 = FACE_OUTER_BOUND ( 'NONE', #11152, .T. ) ;
#14999 = DIRECTION ( 'NONE',  ( -0.000000000000000000, 6.982962677686266711E-15, -1.000000000000000000 ) ) ;
#15001 = CARTESIAN_POINT ( 'NONE',  ( 18.49999999999999289, 10.49142135624846617, -58.25000000000000711 ) ) ;
#15003 = EDGE_LOOP ( 'NONE', ( #204643, #13386, #175038, #139051 ) ) ;
#15002 = LINE ( 'NONE', #95783, #71641 ) ;
#15005 = CARTESIAN_POINT ( 'NONE',  ( 22.39999999999999858, 75.90000000001199965, -110.8138870828976934 ) ) ;
#15004 = CARTESIAN_POINT ( 'NONE',  ( -22.59999999999999787, 0.1008583690987122083, 11.74956712348939192 ) ) ;
#15006 = EDGE_CURVE ( 'NONE', #148274, #90674, #224234, .T. ) ;
#15007 = DIRECTION ( 'NONE',  ( 0.000000000000000000, -6.982962677686266711E-15, 1.000000000000000000 ) ) ;
#15008 = AXIS2_PLACEMENT_3D ( 'NONE', #151579, #169875, #251926 ) ;
#15009 = EDGE_CURVE ( 'NONE', #147541, #166406, #48099, .T. ) ;
#15010 = ORIENTED_EDGE ( 'NONE', *, *, #55691, .F. ) ;
#15011 = DIRECTION ( 'NONE',  ( 0.000000000000000000, -6.982962677686266711E-15, 1.000000000000000000 ) ) ;
#15012 = CARTESIAN_POINT ( 'NONE',  ( -18.59999999999999787, 11.64999999999999680, -12.14999999999999858 ) ) ;
#15013 = ORIENTED_EDGE ( 'NONE', *, *, #160659, .F. ) ;
#15014 = AXIS2_PLACEMENT_3D ( 'NONE', #250738, #73425, #74723 ) ;
#15015 = FACE_OUTER_BOUND ( 'NONE', #110839, .T. ) ;
#15016 = DIRECTION ( 'NONE',  ( 1.000000000000000000, 0.000000000000000000, 0.000000000000000000 ) ) ;
#15017 = PLANE ( 'NONE',  #55231 ) ;
#15018 = ORIENTED_EDGE ( 'NONE', *, *, #89160, .F. ) ;
#15019 = ORIENTED_EDGE ( 'NONE', *, *, #167949, .T. ) ;
#15020 = CARTESIAN_POINT ( 'NONE',  ( 23.24999999999999645, 1.115600667400684642E-11, -67.00000000000004263 ) ) ;
#15021 = CARTESIAN_POINT ( 'NONE',  ( -18.59999994787167310, -0.7120786659332111190, -242.4841517841200869 ) ) ;
#15022 = AXIS2_PLACEMENT_3D ( 'NONE', #41526, #201856, #40247 ) ;
#15023 = DIRECTION ( 'NONE',  ( 0.000000000000000000, 0.000000000000000000, 1.000000000000000000 ) ) ;
#15024 = CARTESIAN_POINT ( 'NONE',  ( 23.14999999999999503, 69.35000000001151932, -48.37310748452436826 ) ) ;
#15025 = EDGE_LOOP ( 'NONE', ( #231027, #216368, #167552, #55140 ) ) ;
#15026 = DIRECTION ( 'NONE',  ( 1.000000000000000000, 0.000000000000000000, 0.000000000000000000 ) ) ;
#15027 = CARTESIAN_POINT ( 'NONE',  ( -22.49533356619869195, 64.34999999370828050, -170.0882300648472949 ) ) ;
#15028 = DIRECTION ( 'NONE',  ( 1.000000000000000000, -7.304098846218134667E-16, -5.100424963727255829E-30 ) ) ;
#15029 = EDGE_CURVE ( 'NONE', #89321, #183814, #93891, .T. ) ;
#15030 = DIRECTION ( 'NONE',  ( 0.000000000000000000, 0.2617529984165152257, 0.9651348961777124202 ) ) ;
#15031 = VECTOR ( 'NONE', #131070, 1000.000000000000000 ) ;
#15032 = CIRCLE ( 'NONE', #181622, 0.09999999999998898659 ) ;
#15033 = EDGE_CURVE ( 'NONE', #173882, #62202, #26059, .T. ) ;
#15034 = AXIS2_PLACEMENT_3D ( 'NONE', #136973, #112297, #54854 ) ;
#15035 = CIRCLE ( 'NONE', #114974, 0.1000000000000028644 ) ;
#15036 = DIRECTION ( 'NONE',  ( 0.000000000000000000, 0.000000000000000000, 1.000000000000000000 ) ) ;
#15038 = VERTEX_POINT ( 'NONE', #165571 ) ;
#15037 = DIRECTION ( 'NONE',  ( 0.7071067811865474617, -0.7071067811865474617, -4.937700262164531476E-15 ) ) ;
#15039 = PLANE ( 'NONE',  #178602 ) ;
#15040 = CARTESIAN_POINT ( 'NONE',  ( 20.94999999999999574, 44.18518595211054389, -258.7688298343402380 ) ) ;
#15041 = CARTESIAN_POINT ( 'NONE',  ( -22.60000000000080789, 0.04781698047652390565, -122.2499775688472567 ) ) ;
#15042 = CARTESIAN_POINT ( 'NONE',  ( -18.50000000000000000, 70.37092869010230345, -198.1237041667535550 ) ) ;
#15044 = ORIENTED_EDGE ( 'NONE', *, *, #18388, .T. ) ;
#15043 = FACE_OUTER_BOUND ( 'NONE', #176238, .T. ) ;
#15045 = CYLINDRICAL_SURFACE ( 'NONE', #4891, 0.1000000000000013656 ) ;
#15046 = DIRECTION ( 'NONE',  ( 0.000000000000000000, -0.5000000000000016653, 0.8660254037844377084 ) ) ;
#15047 = CARTESIAN_POINT ( 'NONE',  ( -18.35235881385853318, 11.47341900771289502, -9.250000000000001776 ) ) ;
#15048 = ORIENTED_EDGE ( 'NONE', *, *, #178913, .T. ) ;
#15049 = DIRECTION ( 'NONE',  ( 0.000000000000000000, -0.1350103645451904977, 0.9908441862701596881 ) ) ;
#15050 = CARTESIAN_POINT ( 'NONE',  ( -20.94999999999999929, 68.58368164137472434, -224.2353459317783120 ) ) ;
#15051 = CARTESIAN_POINT ( 'NONE',  ( 18.59999999999999076, 63.62814136979439184, -224.4990371885399441 ) ) ;
#15052 = DIRECTION ( 'NONE',  ( 0.000000000000000000, 0.000000000000000000, -1.000000000000000000 ) ) ;
#15053 = CIRCLE ( 'NONE', #115179, 0.09999999999999939493 ) ;
#15054 = EDGE_CURVE ( 'NONE', #191859, #75372, #81385, .T. ) ;
#15055 = AXIS2_PLACEMENT_3D ( 'NONE', #112179, #249119, #191727 ) ;
#15056 = DIRECTION ( 'NONE',  ( -1.000000000000000000, 0.000000000000000000, 0.000000000000000000 ) ) ;
#15057 = LINE ( 'NONE', #94563, #17689 ) ;
#15058 = VERTEX_POINT ( 'NONE', #24794 ) ;
#15059 = ORIENTED_EDGE ( 'NONE', *, *, #219723, .F. ) ;
#15060 = CARTESIAN_POINT ( 'NONE',  ( 23.14999999999999503, 11.65000000001116298, -112.6500000000000341 ) ) ;
#15061 = DIRECTION ( 'NONE',  ( 1.000000000000000000, 0.000000000000000000, 0.000000000000000000 ) ) ;
#15062 = CARTESIAN_POINT ( 'NONE',  ( -16.92507428761701505, 66.05000000001157900, -56.80971002490283439 ) ) ;
#15063 = CARTESIAN_POINT ( 'NONE',  ( -20.85000000000000142, 1.115600667400684642E-11, -200.9999999999999432 ) ) ;
#15064 = DIRECTION ( 'NONE',  ( -1.000000000000000000, 0.000000000000000000, 0.000000000000000000 ) ) ;
#15065 = DIRECTION ( 'NONE',  ( 0.000000000000000000, 0.8700118002898321601, -0.4930308989875230030 ) ) ;
#15066 = CARTESIAN_POINT ( 'NONE',  ( 21.00000000000000000, 7.973296578895943121, 1.410778198689825347 ) ) ;
#15067 = ORIENTED_EDGE ( 'NONE', *, *, #186875, .F. ) ;
#15068 = CARTESIAN_POINT ( 'NONE',  ( -33.72168855820452649, 33.06517536918362055, -220.7872234046467952 ) ) ;
#15069 = ORIENTED_EDGE ( 'NONE', *, *, #197200, .F. ) ;
#15070 = CARTESIAN_POINT ( 'NONE',  ( 18.49999999999999289, 65.79142135624879018, -44.87310748452438958 ) ) ;
#15071 = FACE_OUTER_BOUND ( 'NONE', #149802, .T. ) ;
#15072 = DIRECTION ( 'NONE',  ( -1.000000000000000000, 2.952720810173289112E-16, 2.061873921506763405E-30 ) ) ;
#15073 = EDGE_LOOP ( 'NONE', ( #113178, #56437, #18692, #169849 ) ) ;
#15074 = DIRECTION ( 'NONE',  ( -0.000000000000000000, -1.000000000000000000, 6.308085367188393199E-16 ) ) ;
#15075 = DIRECTION ( 'NONE',  ( -1.000000000000000000, -0.000000000000000000, -0.000000000000000000 ) ) ;
#15076 = CARTESIAN_POINT ( 'NONE',  ( 18.46932045258648714, 85.67068520027744682, -62.84924711152763166 ) ) ;
#15077 = ADVANCED_FACE ( 'NONE', ( #126423 ), #204664, .T. ) ;
#15078 = ORIENTED_EDGE ( 'NONE', *, *, #206989, .T. ) ;
#15079 = DIRECTION ( 'NONE',  ( 0.000000000000000000, 0.000000000000000000, 1.000000000000000000 ) ) ;
#15080 = DIRECTION ( 'NONE',  ( 1.020425574104004196E-15, -6.982962677686266711E-15, 1.000000000000000000 ) ) ;
#15082 = EDGE_CURVE ( 'NONE', #4416, #62328, #189937, .T. ) ;
#15081 = DIRECTION ( 'NONE',  ( 0.000000000000000000, -7.056502275159890832E-15, 1.000000000000000000 ) ) ;
#15083 = CARTESIAN_POINT ( 'NONE',  ( -18.48550754432080012, 85.46339977857178383, -162.9743177321096539 ) ) ;
#15084 = AXIS2_PLACEMENT_3D ( 'NONE', #21161, #201048, #107075 ) ;
#15085 = DIRECTION ( 'NONE',  ( 0.000000000000000000, 1.000000000000000000, 6.853228547068871147E-15 ) ) ;
#15086 = AXIS2_PLACEMENT_3D ( 'NONE', #248507, #37183, #249795 ) ;
#15087 = AXIS2_PLACEMENT_3D ( 'NONE', #96320, #138014, #175906 ) ;
#15088 = ORIENTED_EDGE ( 'NONE', *, *, #21799, .T. ) ;
#15090 = FACE_OUTER_BOUND ( 'NONE', #255646, .T. ) ;
#15089 = COLOUR_RGB ( '', 0.09019608, 0.27058824, 0.51372549) ;
#15092 = EDGE_CURVE ( 'NONE', #117519, #204559, #27374, .T. ) ;
#15091 = CARTESIAN_POINT ( 'NONE',  ( -16.81453046979148880, 66.06089771857094206, -90.31138096092139733 ) ) ;
#15093 = ORIENTED_EDGE ( 'NONE', *, *, #219532, .F. ) ;
#15094 = DIRECTION ( 'NONE',  ( 0.000000000000000000, 7.056502275159890043E-15, -1.000000000000000000 ) ) ;
#15096 = EDGE_CURVE ( 'NONE', #250894, #162196, #186420, .T. ) ;
#15095 = DIRECTION ( 'NONE',  ( 0.000000000000000000, 0.000000000000000000, -1.000000000000000000 ) ) ;
#15097 = CARTESIAN_POINT ( 'NONE',  ( 20.95512820512820440, 11.25838014693915845, -210.9828572391343755 ) ) ;
#15098 = VERTEX_POINT ( 'NONE', #147271 ) ;
#15099 = CARTESIAN_POINT ( 'NONE',  ( 18.31572054635715574, -9.548475435767818098, -174.3505701647482624 ) ) ;
#15100 = CARTESIAN_POINT ( 'NONE',  ( 20.95429402530547591, 8.876194151113343977, -42.02308669793784901 ) ) ;
#15101 = EDGE_CURVE ( 'NONE', #159653, #154400, #256506, .T. ) ;
#15102 = ORIENTED_EDGE ( 'NONE', *, *, #160438, .T. ) ;
#15103 = AXIS2_PLACEMENT_3D ( 'NONE', #80076, #16316, #158406 ) ;
#15104 = ORIENTED_EDGE ( 'NONE', *, *, #162087, .T. ) ;
#15105 = AXIS2_PLACEMENT_3D ( 'NONE', #179958, #102953, #196930 ) ;
#15106 = DIRECTION ( 'NONE',  ( -1.000000000000000000, 0.000000000000000000, 0.000000000000000000 ) ) ;
#15108 = EDGE_CURVE ( 'NONE', #171525, #8827, #14983, .T. ) ;
#15107 = DIRECTION ( 'NONE',  ( -1.000000000000000000, 0.000000000000000000, 0.000000000000000000 ) ) ;
#15111 = ORIENTED_EDGE ( 'NONE', *, *, #153417, .T. ) ;
#15110 = DIRECTION ( 'NONE',  ( 0.000000000000000000, 1.000000000000000000, -0.000000000000000000 ) ) ;
#15109 =( BOUNDED_CURVE ( )  B_SPLINE_CURVE ( 3, ( #57258, #178545, #42856, #216349 ),
 .UNSPECIFIED., .F., .F. ) 
 B_SPLINE_CURVE_WITH_KNOTS ( ( 4, 4 ),
 ( 3.141592653589793116, 4.712388980384692339 ),
 .UNSPECIFIED. ) 
 CURVE ( )  GEOMETRIC_REPRESENTATION_ITEM ( )  RATIONAL_B_SPLINE_CURVE ( ( 1.000000000000000000, 0.8047378541243643824, 0.8047378541243643824, 1.000000000000000000 ) ) 
 REPRESENTATION_ITEM ( '' )  );
#15112 = DIRECTION ( 'NONE',  ( 0.000000000000000000, 0.8814952561688436106, -0.4721928772777334027 ) ) ;
#15114 = AXIS2_PLACEMENT_3D ( 'NONE', #51973, #75439, #135365 ) ;
#15113 = DIRECTION ( 'NONE',  ( 1.000000000000000000, 0.000000000000000000, 0.000000000000000000 ) ) ;
#15115 = CARTESIAN_POINT ( 'NONE',  ( -20.94788355080264353, 65.69792220476342948, -131.0335554128461979 ) ) ;
#15116 = CARTESIAN_POINT ( 'NONE',  ( -23.25000000000000000, 1.148907358139439339E-11, -201.0000000000015064 ) ) ;
#15117 = CARTESIAN_POINT ( 'NONE',  ( 21.05000000000000071, -8.663551401857999323, -157.9758988819327215 ) ) ;
#15118 = LINE ( 'NONE', #35971, #193014 ) ;
#15119 = DIRECTION ( 'NONE',  ( 0.000000000000000000, 6.982962677686267499E-15, -1.000000000000000000 ) ) ;
#15121 = ORIENTED_EDGE ( 'NONE', *, *, #206515, .F. ) ;
#15120 = LINE ( 'NONE', #112932, #157071 ) ;
#15122 = ORIENTED_EDGE ( 'NONE', *, *, #209530, .F. ) ;
#15124 = CARTESIAN_POINT ( 'NONE',  ( -16.97683810757273193, 51.05890824306432307, -232.1973218175039051 ) ) ;
#15123 = FACE_OUTER_BOUND ( 'NONE', #200358, .T. ) ;
#15126 = ORIENTED_EDGE ( 'NONE', *, *, #118529, .T. ) ;
#15125 = CARTESIAN_POINT ( 'NONE',  ( 21.05000000000000071, 8.815201804578357780, -75.42053749668541229 ) ) ;
#15127 = EDGE_LOOP ( 'NONE', ( #3955, #20582, #243279, #245828 ) ) ;
#15128 = CARTESIAN_POINT ( 'NONE',  ( -16.97683809663752186, 9.950000000011138823, -76.25000000000004263 ) ) ;
#15129 = LINE ( 'NONE', #196315, #188778 ) ;
#15130 = CIRCLE ( 'NONE', #194209, 0.09999999999999939493 ) ;
#15132 =( BOUNDED_SURFACE ( )  B_SPLINE_SURFACE ( 3, 2, ( 
 ( #182559, #243794, #123859 ),
 ( #104262, #144679, #203393 ),
 ( #183819, #65147, #186405 ),
 ( #208538, #12917, #191553 ) ),
 .UNSPECIFIED., .F., .F., .F. ) 
 B_SPLINE_SURFACE_WITH_KNOTS ( ( 4, 4 ),
 ( 3, 3 ),
 ( 0.04058434257139457990, 0.04256401539001584966 ),
 ( 0.000000000000000000, 1.000000000000000000 ),
 .UNSPECIFIED. ) 
 GEOMETRIC_REPRESENTATION_ITEM ( )  RATIONAL_B_SPLINE_SURFACE ( (
 ( 1.000000000000000000, 0.7103081912008383236, 1.000000000000000000),
 ( 1.000000000000000000, 0.7104998333555154755, 1.000000000000000000),
 ( 1.000000000000000000, 0.7107238315755263214, 1.000000000000000000),
 ( 1.000000000000000000, 0.7110073749539205235, 1.000000000000000000) ) ) 
 REPRESENTATION_ITEM ( '' )  SURFACE ( )  );
#15131 = AXIS2_PLACEMENT_3D ( 'NONE', #249822, #26950, #251083 ) ;
#15133 = CARTESIAN_POINT ( 'NONE',  ( -22.50000000000000000, 64.35023708198002623, -103.1119174609113145 ) ) ;
#15134 = CARTESIAN_POINT ( 'NONE',  ( 19.83283456528360489, 11.75000000001116263, -58.34999999942034776 ) ) ;
#15135 = DIRECTION ( 'NONE',  ( 0.000000000000000000, -1.000000000000000000, 0.000000000000000000 ) ) ;
#15136 = AXIS2_PLACEMENT_3D ( 'NONE', #157292, #119436, #178136 ) ;
#15137 = CARTESIAN_POINT ( 'NONE',  ( 21.14999999999999503, -0.09999999998884338825, -122.3504291924552234 ) ) ;
#15138 = FACE_OUTER_BOUND ( 'NONE', #195856, .T. ) ;
#15139 = ORIENTED_EDGE ( 'NONE', *, *, #184429, .T. ) ;
#15140 = ORIENTED_EDGE ( 'NONE', *, *, #154765, .F. ) ;
#15141 = CARTESIAN_POINT ( 'NONE',  ( 21.04999999999965254, 30.88828517705548649, -252.0799250334554813 ) ) ;
#15142 = VECTOR ( 'NONE', #156678, 1000.000000000000114 ) ;
#15143 = ORIENTED_EDGE ( 'NONE', *, *, #199853, .F. ) ;
#15144 = DIRECTION ( 'NONE',  ( -0.000000000000000000, 1.000000000000000000, -0.000000000000000000 ) ) ;
#15145 = ORIENTED_EDGE ( 'NONE', *, *, #146126, .T. ) ;
#15146 = DIRECTION ( 'NONE',  ( 0.000000000000000000, -1.000000000000000000, 0.000000000000000000 ) ) ;
#15147 =( BOUNDED_CURVE ( )  B_SPLINE_CURVE ( 3, ( #109227, #193927, #174400, #153554 ),
 .UNSPECIFIED., .F., .F. ) 
 B_SPLINE_CURVE_WITH_KNOTS ( ( 4, 4 ),
 ( 3.141592653589793116, 4.712388980384689674 ),
 .UNSPECIFIED. ) 
 CURVE ( )  GEOMETRIC_REPRESENTATION_ITEM ( )  RATIONAL_B_SPLINE_CURVE ( ( 1.000000000000000000, 0.8047378541243649375, 0.8047378541243649375, 1.000000000000000000 ) ) 
 REPRESENTATION_ITEM ( '' )  );
#15148 = EDGE_CURVE ( 'NONE', #44661, #134285, #183833, .T. ) ;
#15149 = DIRECTION ( 'NONE',  ( -0.000000000000000000, -1.000000000000000000, -6.982962677686266711E-15 ) ) ;
#15150 = ORIENTED_EDGE ( 'NONE', *, *, #215445, .T. ) ;
#15151 = CARTESIAN_POINT ( 'NONE',  ( 23.14999999999999503, 17.01923898301590654, -224.3994341343041867 ) ) ;
#15152 = ORIENTED_EDGE ( 'NONE', *, *, #139163, .F. ) ;
#15154 = EDGE_CURVE ( 'NONE', #58451, #50622, #2480, .T. ) ;
#15153 = LINE ( 'NONE', #10011, #29772 ) ;
#15155 = ORIENTED_EDGE ( 'NONE', *, *, #29871, .T. ) ;
#15156 = AXIS2_PLACEMENT_3D ( 'NONE', #60674, #140209, #222302 ) ;
#15157 = DIRECTION ( 'NONE',  ( 1.000000000000000000, 0.000000000000000000, 0.000000000000000000 ) ) ;
#15158 = CIRCLE ( 'NONE', #148444, 1.749999999999998002 ) ;
#15159 = CARTESIAN_POINT ( 'NONE',  ( 23.25000000000000000, -8.596261682231833845, -109.9501275171503210 ) ) ;
#15160 = EDGE_CURVE ( 'NONE', #188542, #128905, #84690, .T. ) ;
#15162 = ADVANCED_FACE ( 'NONE', ( #164285 ), #194056, .T. ) ;
#15161 = CIRCLE ( 'NONE', #40131, 0.09999999999998898659 ) ;
#15163 = CIRCLE ( 'NONE', #160915, 0.1000000000000028644 ) ;
#15164 = ORIENTED_EDGE ( 'NONE', *, *, #183292, .T. ) ;
#15165 = PLANE ( 'NONE',  #223421 ) ;
#15166 = EDGE_LOOP ( 'NONE', ( #157242, #105619, #201458, #169047 ) ) ;
#15169 = ORIENTED_EDGE ( 'NONE', *, *, #129776, .F. ) ;
#15168 = CARTESIAN_POINT ( 'NONE',  ( 23.24999999999999645, 1.115600667400684642E-11, -100.5000000000000426 ) ) ;
#15167 = DIRECTION ( 'NONE',  ( -0.000000000000000000, 0.000000000000000000, -1.000000000000000000 ) ) ;
#15170 = CARTESIAN_POINT ( 'NONE',  ( -21.05000000000000426, -0.09999999998884338825, -27.02293297887525014 ) ) ;
#15171 = VERTEX_POINT ( 'NONE', #65159 ) ;
#15172 = VECTOR ( 'NONE', #94721, 1000.000000000000000 ) ;
#15173 = VERTEX_POINT ( 'NONE', #108154 ) ;
#15175 = ADVANCED_FACE ( 'NONE', ( #50710 ), #248957, .F. ) ;
#15174 = CARTESIAN_POINT ( 'NONE',  ( 18.49999999999998934, 10.25000000001115552, -192.2499999999999716 ) ) ;
#15176 = VERTEX_POINT ( 'NONE', #230677 ) ;
#15177 = ADVANCED_FACE ( 'NONE', ( #168169 ), #33791, .T. ) ;
#15178 = CARTESIAN_POINT ( 'NONE',  ( 18.59999999999999076, 6.982009704867611077, -204.6961521182562649 ) ) ;
#15179 = LINE ( 'NONE', #94692, #34577 ) ;
#15180 = DIRECTION ( 'NONE',  ( 0.000000000000000000, 0.000000000000000000, 1.000000000000000000 ) ) ;
#15181 = PLANE ( 'NONE',  #160171 ) ;
#15182 = EDGE_CURVE ( 'NONE', #218877, #230655, #206510, .T. ) ;
#15183 = AXIS2_PLACEMENT_3D ( 'NONE', #146506, #184358, #29201 ) ;
#15184 = CARTESIAN_POINT ( 'NONE',  ( -21.10320863425827298, 0.02502225123826237740, -60.59972261354081269 ) ) ;
#15185 = AXIS2_PLACEMENT_3D ( 'NONE', #26269, #244007, #206182 ) ;
#15186 = ORIENTED_EDGE ( 'NONE', *, *, #59631, .F. ) ;
#15187 = CARTESIAN_POINT ( 'NONE',  ( 23.24999999999999645, 5.600000000011153389, -45.90526601891310321 ) ) ;
#15188 = DIRECTION ( 'NONE',  ( -1.000000000000000000, -0.000000000000000000, 0.000000000000000000 ) ) ;
#15189 = CARTESIAN_POINT ( 'NONE',  ( 18.69999999999999929, -10.64999999999999325, 31.39999999999999858 ) ) ;
#15190 = EDGE_LOOP ( 'NONE', ( #123367, #42656, #54340, #33180 ) ) ;
#15191 = CARTESIAN_POINT ( 'NONE',  ( 22.00356870143462373, 7.088088014901702927, -199.4562900056679382 ) ) ;
#15192 = ORIENTED_EDGE ( 'NONE', *, *, #64090, .T. ) ;
#15193 = CARTESIAN_POINT ( 'NONE',  ( 20.85000000000000142, 70.22659352830977753, -197.9852579278363578 ) ) ;
#15194 = EDGE_LOOP ( 'NONE', ( #229468, #95873, #98961, #151637 ) ) ;
#15195 = DIRECTION ( 'NONE',  ( 0.000000000000000000, 6.982962677686266711E-15, -1.000000000000000000 ) ) ;
#15196 = CARTESIAN_POINT ( 'NONE',  ( -21.05000000000000071, 76.00000000001244871, -170.0231074845243597 ) ) ;
#15197 = EDGE_CURVE ( 'NONE', #254577, #199182, #69044, .T. ) ;
#15198 = AXIS2_PLACEMENT_3D ( 'NONE', #103703, #47593, #163713 ) ;
#15200 = ORIENTED_EDGE ( 'NONE', *, *, #74145, .F. ) ;
#15199 = FACE_OUTER_BOUND ( 'NONE', #20014, .T. ) ;
#15201 = EDGE_CURVE ( 'NONE', #115244, #225971, #185830, .T. ) ;
#15202 = CARTESIAN_POINT ( 'NONE',  ( -18.69999999999999929, -8.250000000000005329, -15.00000000000000000 ) ) ;
#15203 = ORIENTED_EDGE ( 'NONE', *, *, #30436, .T. ) ;
#15204 = ADVANCED_FACE ( 'NONE', ( #71611 ), #35830, .T. ) ;
#15205 = DIRECTION ( 'NONE',  ( 1.000000000000000000, 0.000000000000000000, 0.000000000000000000 ) ) ;
#15206 = CARTESIAN_POINT ( 'NONE',  ( -16.87401514999241314, 9.950000000011137047, -113.2199820074682179 ) ) ;
#15207 = ORIENTED_EDGE ( 'NONE', *, *, #96816, .T. ) ;
#15208 = CARTESIAN_POINT ( 'NONE',  ( -18.59999999999999787, 77.16270174995010223, -128.4231074845242802 ) ) ;
#15209 = CARTESIAN_POINT ( 'NONE',  ( -20.94560253601877164, 11.75000000001115197, -194.0100835125150240 ) ) ;
#15210 = ORIENTED_EDGE ( 'NONE', *, *, #241183, .F. ) ;
#15211 = CARTESIAN_POINT ( 'NONE',  ( 21.05000000000000071, 5.499999999999998224, -21.09473398108690390 ) ) ;
#15212 = CIRCLE ( 'NONE', #52610, 11.75000000000001066 ) ;
#15213 = AXIS2_PLACEMENT_3D ( 'NONE', #223725, #63366, #202890 ) ;
#15214 = AXIS2_PLACEMENT_3D ( 'NONE', #5796, #161054, #202732 ) ;
#15215 = AXIS2_PLACEMENT_3D ( 'NONE', #37426, #40012, #214754 ) ;
#15216 = EDGE_LOOP ( 'NONE', ( #134559, #82947, #197092, #139887 ) ) ;
#15217 = CARTESIAN_POINT ( 'NONE',  ( 12.60873083341396850, 9.389571634557563939, -118.3176407123691831 ) ) ;
#15218 = CARTESIAN_POINT ( 'NONE',  ( -18.41418431465368855, -9.499999999989071853, -73.60018939122146264 ) ) ;
#15219 = EDGE_CURVE ( 'NONE', #144016, #202492, #144115, .T. ) ;
#15220 = ADVANCED_FACE ( 'NONE', ( #233260 ), #114925, .F. ) ;
#15222 = ORIENTED_EDGE ( 'NONE', *, *, #146087, .F. ) ;
#15221 = FACE_OUTER_BOUND ( 'NONE', #239408, .T. ) ;
#15223 = DIRECTION ( 'NONE',  ( 0.000000000000000000, 6.982962677686266711E-15, -1.000000000000000000 ) ) ;
#15224 = CARTESIAN_POINT ( 'NONE',  ( 6.100000000000060929, 64.35000000001120668, -25.92310748452479174 ) ) ;
#15226 = EDGE_CURVE ( 'NONE', #203555, #250586, #252275, .T. ) ;
#15225 = CARTESIAN_POINT ( 'NONE',  ( 23.14999999999999503, 66.54223038922117439, -213.7542166125332415 ) ) ;
#15227 = AXIS2_PLACEMENT_3D ( 'NONE', #11150, #153261, #16305 ) ;
#15229 = DIRECTION ( 'NONE',  ( 0.000000000000000000, 0.000000000000000000, 1.000000000000000000 ) ) ;
#15228 = CARTESIAN_POINT ( 'NONE',  ( -16.94445028196807002, 63.05630424923659660, -213.0754291771441729 ) ) ;
#15230 = CARTESIAN_POINT ( 'NONE',  ( 18.59999999999998721, 56.14960075277911500, -201.2428044267231257 ) ) ;
#15231 = FACE_OUTER_BOUND ( 'NONE', #120734, .T. ) ;
#15232 = CIRCLE ( 'NONE', #65291, 0.09999999999999939493 ) ;
#15233 = TOROIDAL_SURFACE ( 'NONE', #106791, 11.90000000000000213, 0.1000000000000000056 ) ;
#15234 = CARTESIAN_POINT ( 'NONE',  ( -23.25000000000000000, -4.914013037343267776, -233.1828366659746905 ) ) ;
#15235 = DIRECTION ( 'NONE',  ( 1.000000000000000000, 7.304098846218134667E-16, 5.100424963727256530E-30 ) ) ;
#15236 = ORIENTED_EDGE ( 'NONE', *, *, #30883, .F. ) ;
#15237 = ORIENTED_EDGE ( 'NONE', *, *, #85909, .T. ) ;
#15238 = CYLINDRICAL_SURFACE ( 'NONE', #112498, 0.1000000000000000472 ) ;
#15239 = AXIS2_PLACEMENT_3D ( 'NONE', #153044, #73496, #35660 ) ;
#15241 = ORIENTED_EDGE ( 'NONE', *, *, #244045, .F. ) ;
#15240 = DIRECTION ( 'NONE',  ( -3.440080580676165868E-14, -0.1298341882520124002, -0.9915357197604841577 ) ) ;
#15242 = EDGE_LOOP ( 'NONE', ( #157551, #208439, #99121, #177452 ) ) ;
#15243 = CARTESIAN_POINT ( 'NONE',  ( 21.14999999999999858, 11.75000000001116263, -146.1500000000000341 ) ) ;
#15244 = ORIENTED_EDGE ( 'NONE', *, *, #2245, .F. ) ;
#15245 = CARTESIAN_POINT ( 'NONE',  ( 21.13461538461538680, 43.58999342716159475, -234.8150793036844846 ) ) ;
#15246 = EDGE_CURVE ( 'NONE', #235449, #197047, #209824, .T. ) ;
#15247 = VERTEX_POINT ( 'NONE', #92422 ) ;
#15249 = ADVANCED_FACE ( 'NONE', ( #31227 ), #212401, .T. ) ;
#15248 = CYLINDRICAL_SURFACE ( 'NONE', #161476, 11.74999999999999822 ) ;
#15252 = ORIENTED_EDGE ( 'NONE', *, *, #52736, .F. ) ;
#15251 = ORIENTED_EDGE ( 'NONE', *, *, #227436, .F. ) ;
#15250 = CIRCLE ( 'NONE', #227615, 0.09999999999999939493 ) ;
#15253 = ORIENTED_EDGE ( 'NONE', *, *, #152843, .T. ) ;
#15254 = ORIENTED_EDGE ( 'NONE', *, *, #208907, .F. ) ;
#15255 = VERTEX_POINT ( 'NONE', #14209 ) ;
#15256 = EDGE_CURVE ( 'NONE', #118730, #235869, #139854, .T. ) ;
#15257 = DIRECTION ( 'NONE',  ( -1.000000000000000000, 0.000000000000000000, 0.000000000000000000 ) ) ;
#15258 = FACE_OUTER_BOUND ( 'NONE', #101382, .T. ) ;
#15259 = CARTESIAN_POINT ( 'NONE',  ( -23.15000000000000213, 2.000000000011154189, -147.2246219227621111 ) ) ;
#15262 = ADVANCED_FACE ( 'NONE', ( #131564 ), #91644, .T. ) ;
#15261 = VERTEX_POINT ( 'NONE', #11638 ) ;
#15260 = FACE_OUTER_BOUND ( 'NONE', #88619, .T. ) ;
#15263 = CARTESIAN_POINT ( 'NONE',  ( 20.58091095332318332, 40.65476404443996472, -237.8789846480217705 ) ) ;
#15264 = DIRECTION ( 'NONE',  ( 0.000000000000000000, 0.2211802418851293583, -0.9752329468386697897 ) ) ;
#15266 = ORIENTED_EDGE ( 'NONE', *, *, #47286, .T. ) ;
#15265 = CARTESIAN_POINT ( 'NONE',  ( -21.05000000000000071, 44.06843597547145208, -258.9974126733344519 ) ) ;
#15267 = DIRECTION ( 'NONE',  ( 0.000000000000000000, 0.1350103645451807832, 0.9908441862701610203 ) ) ;
#15268 = ORIENTED_EDGE ( 'NONE', *, *, #71376, .F. ) ;
#15269 = ADVANCED_FACE ( 'NONE', ( #96266 ), #156296, .F. ) ;
#15271 = AXIS2_PLACEMENT_3D ( 'NONE', #99626, #160934, #200051 ) ;
#15270 = FACE_OUTER_BOUND ( 'NONE', #22279, .T. ) ;
#15273 = ORIENTED_EDGE ( 'NONE', *, *, #135923, .F. ) ;
#15272 = CARTESIAN_POINT ( 'NONE',  ( 20.94999999999999929, 5.400000000011154988, -155.0947339810869323 ) ) ;
#15274 = CARTESIAN_POINT ( 'NONE',  ( -21.64999999999999858, 65.95000000001152785, -48.67310748452439384 ) ) ;
#15275 = CARTESIAN_POINT ( 'NONE',  ( -16.85718274719421217, 9.976142314632873820, -113.0633463321825758 ) ) ;
#15276 = CIRCLE ( 'NONE', #44502, 0.2000000000000057288 ) ;
#15277 = EDGE_LOOP ( 'NONE', ( #143142, #47800, #150012 ) ) ;
#15278 = CARTESIAN_POINT ( 'NONE',  ( -21.05000000000000071, -11.48912529307605901, -2.900000000000001688 ) ) ;
#15279 = CARTESIAN_POINT ( 'NONE',  ( -18.59999999999999787, 14.80545736607782814, -235.9842437978701639 ) ) ;
#15280 = AXIS2_PLACEMENT_3D ( 'NONE', #169550, #249060, #196629 ) ;
#15281 = AXIS2_PLACEMENT_3D ( 'NONE', #153177, #132280, #14924 ) ;
#15282 = EDGE_CURVE ( 'NONE', #56738, #164486, #255301, .T. ) ;
#15283 = CARTESIAN_POINT ( 'NONE',  ( -21.05000000000000071, 67.23127455305841238, -235.8551265064783991 ) ) ;
#15284 = LINE ( 'NONE', #111808, #180768 ) ;
#15285 = ADVANCED_FACE ( 'NONE', ( #157590 ), #106516, .F. ) ;
#15286 = ORIENTED_EDGE ( 'NONE', *, *, #146992, .F. ) ;
#15287 = ORIENTED_EDGE ( 'NONE', *, *, #13001, .F. ) ;
#15288 = AXIS2_PLACEMENT_3D ( 'NONE', #243994, #7974, #62801 ) ;
#15289 = DIRECTION ( 'NONE',  ( 1.000000000000000000, 0.000000000000000000, 0.000000000000000000 ) ) ;
#15290 = FACE_OUTER_BOUND ( 'NONE', #81324, .T. ) ;
#15291 = ORIENTED_EDGE ( 'NONE', *, *, #69356, .T. ) ;
#15292 = DIRECTION ( 'NONE',  ( 0.000000000000000000, 0.6728971962617388280, 0.7397360091702248619 ) ) ;
#15293 = EDGE_LOOP ( 'NONE', ( #131620, #175146, #4286, #155005 ) ) ;
#15294 = EDGE_CURVE ( 'NONE', #194512, #109477, #173240, .T. ) ;
#15295 = FACE_OUTER_BOUND ( 'NONE', #73383, .T. ) ;
#15296 = CYLINDRICAL_SURFACE ( 'NONE', #8628, 1.749999999999999778 ) ;
#15297 = ORIENTED_EDGE ( 'NONE', *, *, #18649, .F. ) ;
#15298 = DIRECTION ( 'NONE',  ( 1.000000000000000000, 0.000000000000000000, 0.000000000000000000 ) ) ;
#15299 = ADVANCED_FACE ( 'NONE', ( #37614 ), #136680, .F. ) ;
#15300 = AXIS2_PLACEMENT_3D ( 'NONE', #197183, #175112, #18561 ) ;
#15301 = ORIENTED_EDGE ( 'NONE', *, *, #59030, .T. ) ;
#15302 = ORIENTED_EDGE ( 'NONE', *, *, #147899, .T. ) ;
#15303 = CIRCLE ( 'NONE', #131807, 0.1000000000000026007 ) ;
#15304 = ORIENTED_EDGE ( 'NONE', *, *, #41430, .F. ) ;
#15305 = ADVANCED_FACE ( 'NONE', ( #158851 ), #80535, .T. ) ;
#15307 = CARTESIAN_POINT ( 'NONE',  ( -18.59999999999999787, 11.65000000001115232, -179.6499999999999773 ) ) ;
#15306 = AXIS2_PLACEMENT_3D ( 'NONE', #12400, #250970, #9806 ) ;
#15308 = CARTESIAN_POINT ( 'NONE',  ( 21.05000000000000071, 76.00000000001234923, -165.7231074845243484 ) ) ;
#15309 = FACE_OUTER_BOUND ( 'NONE', #203605, .T. ) ;
#15310 = DIRECTION ( 'NONE',  ( -0.000000000000000000, 0.1350103645451876666, 0.9908441862701600211 ) ) ;
#15311 = CIRCLE ( 'NONE', #190081, 0.09999999999998898659 ) ;
#15312 = CARTESIAN_POINT ( 'NONE',  ( 12.26145404764308999, 66.64858632091066681, -119.5427639169754315 ) ) ;
#15313 = CARTESIAN_POINT ( 'NONE',  ( -18.50000000000000000, 66.75000000001199396, -115.2731074845243597 ) ) ;
#15315 = ORIENTED_EDGE ( 'NONE', *, *, #173741, .T. ) ;
#15314 = DIRECTION ( 'NONE',  ( 0.000000000000000000, 0.000000000000000000, -1.000000000000000000 ) ) ;
#15316 = DIRECTION ( 'NONE',  ( 1.000000000000000000, -0.000000000000000000, 0.000000000000000000 ) ) ;
#15317 = VERTEX_POINT ( 'NONE', #114571 ) ;
#15318 = AXIS2_PLACEMENT_3D ( 'NONE', #239311, #63217, #41133 ) ;
#15319 = DIRECTION ( 'NONE',  ( 0.000000000000000000, -0.8814952561688476074, 0.4721928772777262417 ) ) ;
#15320 = AXIS2_PLACEMENT_3D ( 'NONE', #21366, #138679, #180421 ) ;
#15321 = EDGE_CURVE ( 'NONE', #148927, #157514, #237082, .T. ) ;
#15322 = ORIENTED_EDGE ( 'NONE', *, *, #10738, .T. ) ;
#15323 = ORIENTED_EDGE ( 'NONE', *, *, #99735, .F. ) ;
#15324 = DIRECTION ( 'NONE',  ( 1.000000000000000000, 0.000000000000000000, 0.000000000000000000 ) ) ;
#15325 = CARTESIAN_POINT ( 'NONE',  ( -16.93302609847409457, 9.996682520814371031, -46.08638849536255577 ) ) ;
#15326 = DIRECTION ( 'NONE',  ( 0.000000000000000000, 0.000000000000000000, -1.000000000000000000 ) ) ;
#15327 = DIRECTION ( 'NONE',  ( 1.000000000000000000, 0.000000000000000000, 0.000000000000000000 ) ) ;
#15328 = VECTOR ( 'NONE', #196117, 1000.000000000000000 ) ;
#15329 = LINE ( 'NONE', #190101, #4985 ) ;
#15331 = ORIENTED_EDGE ( 'NONE', *, *, #160148, .F. ) ;
#15330 = TOROIDAL_SURFACE ( 'NONE', #165148, 0.2000000000000000111, 0.1000000000000000056 ) ;
#15332 = ORIENTED_EDGE ( 'NONE', *, *, #135325, .T. ) ;
#15333 = VECTOR ( 'NONE', #176717, 1000.000000000000000 ) ;
#15334 = CARTESIAN_POINT ( 'NONE',  ( 21.14999999999999503, 64.35000000001267040, -203.5231074845244166 ) ) ;
#15336 = ADVANCED_FACE ( 'NONE', ( #60999 ), #164984, .T. ) ;
#15335 = ORIENTED_EDGE ( 'NONE', *, *, #174, .T. ) ;
#15337 = DIRECTION ( 'NONE',  ( 0.000000000000000000, -0.1495327102803689356, -0.9887567792719336168 ) ) ;
#15338 = CARTESIAN_POINT ( 'NONE',  ( 18.54999999999999716, 67.25000000001257661, -190.8731074845244109 ) ) ;
#15339 = ORIENTED_EDGE ( 'NONE', *, *, #180098, .T. ) ;
#15340 = DIRECTION ( 'NONE',  ( -1.000000000000000000, 3.854941057726231589E-15, 0.000000000000000000 ) ) ;
#15341 = CARTESIAN_POINT ( 'NONE',  ( -20.85000000000000142, 11.75000000001115197, -60.21613433702190576 ) ) ;
#15342 = CARTESIAN_POINT ( 'NONE',  ( -21.05000000000000071, 6.093673009692400555, -199.5727803633481301 ) ) ;
#15343 = CARTESIAN_POINT ( 'NONE',  ( 21.09551895715237180, 65.37856267284352896, -157.7859828186254845 ) ) ;
#15344 = EDGE_LOOP ( 'NONE', ( #6058, #33021, #206710, #76244 ) ) ;
#15345 = DIRECTION ( 'NONE',  ( 1.000000000000000000, 0.000000000000000000, 0.000000000000000000 ) ) ;
#15346 = DIRECTION ( 'NONE',  ( 1.000000000000000000, 0.000000000000000000, 0.000000000000000000 ) ) ;
#15347 = AXIS2_PLACEMENT_3D ( 'NONE', #149617, #229132, #170494 ) ;
#15348 = VERTEX_POINT ( 'NONE', #100103 ) ;
#15350 = EDGE_CURVE ( 'NONE', #140891, #62297, #127396, .T. ) ;
#15349 = CARTESIAN_POINT ( 'NONE',  ( 18.49999999999998934, 64.35000000001251408, -178.7731074845244450 ) ) ;
#15351 = ORIENTED_EDGE ( 'NONE', *, *, #35618, .T. ) ;
#15352 = CARTESIAN_POINT ( 'NONE',  ( -18.50000000000000000, 66.75000000001253397, -182.2731074845244166 ) ) ;
#15353 = CARTESIAN_POINT ( 'NONE',  ( -16.94445028196807002, 14.20918193489391790, -219.2878138714100373 ) ) ;
#15354 = DIRECTION ( 'NONE',  ( 0.000000000000000000, 0.000000000000000000, 1.000000000000000000 ) ) ;
#15355 = DIRECTION ( 'NONE',  ( 0.000000000000000000, 0.000000000000000000, -1.000000000000000000 ) ) ;
#15356 = FACE_OUTER_BOUND ( 'NONE', #5740, .T. ) ;
#15357 = DIRECTION ( 'NONE',  ( 1.000000000000000000, 0.000000000000000000, 0.000000000000000000 ) ) ;
#15359 = ORIENTED_EDGE ( 'NONE', *, *, #192842, .T. ) ;
#15358 = AXIS2_PLACEMENT_3D ( 'NONE', #38588, #163676, #244481 ) ;
#15360 = CARTESIAN_POINT ( 'NONE',  ( -20.64999999999999858, 81.91411460262999356, -215.0718681741873013 ) ) ;
#15361 = DIRECTION ( 'NONE',  ( 1.000000000000000000, 0.000000000000000000, 0.000000000000000000 ) ) ;
#15362 = TOROIDAL_SURFACE ( 'NONE', #106906, 0.2000000000000000111, 0.1000000000000000056 ) ;
#15363 = CIRCLE ( 'NONE', #161094, 0.4000000000000114575 ) ;
#15364 = CARTESIAN_POINT ( 'NONE',  ( -20.85000000000000142, 7.070967871809997973, -137.7465642218683399 ) ) ;
#15365 = CARTESIAN_POINT ( 'NONE',  ( -18.50000000000000711, 64.25000000001264766, -196.5083017138704236 ) ) ;
#15366 = EDGE_CURVE ( 'NONE', #103678, #65240, #198305, .T. ) ;
#15367 = LINE ( 'NONE', #253939, #224022 ) ;
#15368 = AXIS2_PLACEMENT_3D ( 'NONE', #69119, #30002, #112098 ) ;
#15369 = ORIENTED_EDGE ( 'NONE', *, *, #21445, .F. ) ;
#15370 = ORIENTED_EDGE ( 'NONE', *, *, #5732, .T. ) ;
#15371 = DIRECTION ( 'NONE',  ( 0.000000000000000000, -6.454785026890489601E-15, 1.000000000000000000 ) ) ;
#15372 = CARTESIAN_POINT ( 'NONE',  ( -21.06025298249096522, 6.342459739380975847, 12.00000000173892722 ) ) ;
#15373 = CARTESIAN_POINT ( 'NONE',  ( 20.94999999999999929, 70.60000000001186038, -90.61784146561124942 ) ) ;
#15374 = DIRECTION ( 'NONE',  ( 1.000000000000000000, -1.772924042024179204E-16, 4.808324575169891715E-17 ) ) ;
#15375 = DIRECTION ( 'NONE',  ( 0.000000000000000000, -0.9446535261619708468, 0.3280696808755038663 ) ) ;
#15376 = ORIENTED_EDGE ( 'NONE', *, *, #199509, .F. ) ;
#15377 = CARTESIAN_POINT ( 'NONE',  ( 20.85000000000000142, 77.83585931145570669, -125.0186683157258045 ) ) ;
#15378 = AXIS2_PLACEMENT_3D ( 'NONE', #56397, #14756, #190831 ) ;
#15379 = DIRECTION ( 'NONE',  ( 0.7070776581708964059, -0.1504792239192832004, 0.6909393522475117955 ) ) ;
#15380 = VECTOR ( 'NONE', #136910, 1000.000000000000000 ) ;
#15381 = ORIENTED_EDGE ( 'NONE', *, *, #139933, .T. ) ;
#15382 = DIRECTION ( 'NONE',  ( 0.000000000000000000, -0.9651348961777157509, 0.2617529984165031243 ) ) ;
#15383 = DIRECTION ( 'NONE',  ( 2.952720810173289112E-16, -1.000000000000000000, 0.000000000000000000 ) ) ;
#15384 = VERTEX_POINT ( 'NONE', #182247 ) ;
#15385 = CARTESIAN_POINT ( 'NONE',  ( 23.24999999999999645, 36.65892442174935439, -249.5511627012433848 ) ) ;
#15386 = B_SPLINE_CURVE_WITH_KNOTS ( 'NONE', 3,
 ( #120616, #223524, #25371, #81430, #43632, #104838, #145275, #161011, #240542, #220962 ),
 .UNSPECIFIED., .F., .F.,
 ( 4, 3, 3, 4 ),
 ( 7.632826238683908479E-06, 4.756916949875625587E-05, 9.484459048150416206E-05, 0.0001435500935099911655 ),
 .UNSPECIFIED. ) ;
#15387 = ORIENTED_EDGE ( 'NONE', *, *, #11231, .T. ) ;
#15388 = CARTESIAN_POINT ( 'NONE',  ( -21.05000000000000071, 76.00000000001126921, -203.5231074845248997 ) ) ;
#15389 = SPHERICAL_SURFACE ( 'NONE', #146355, 0.1000000000000000056 ) ;
#15390 = CARTESIAN_POINT ( 'NONE',  ( -23.15000000000000213, 43.03453229697098692, -233.8197729272505114 ) ) ;
#15391 = CARTESIAN_POINT ( 'NONE',  ( 19.75857864376268935, 11.75000000000000355, -24.85000000000000142 ) ) ;
#15392 = CARTESIAN_POINT ( 'NONE',  ( -20.54999999999999716, 1.115625160336667635E-11, -169.5000000000000284 ) ) ;
#15393 = CARTESIAN_POINT ( 'NONE',  ( 20.27550659511089037, 29.85975963366233898, -235.4540239816438429 ) ) ;
#15394 = DIRECTION ( 'NONE',  ( -1.000000000000000000, -3.265361837132813093E-16, 0.000000000000000000 ) ) ;
#15395 = ADVANCED_FACE ( 'NONE', ( #243487 ), #111445, .T. ) ;
#15396 = DIRECTION ( 'NONE',  ( -1.000000000000000000, 1.836970198721029934E-16, 1.601412966608202925E-30 ) ) ;
#15398 = LINE ( 'NONE', #234415, #58047 ) ;
#15397 = DIRECTION ( 'NONE',  ( 1.000000000000000000, 3.448943450116723568E-16, 6.438528483529607644E-16 ) ) ;
#15399 = CYLINDRICAL_SURFACE ( 'NONE', #233804, 0.09999999999998898659 ) ;
#15400 = DIRECTION ( 'NONE',  ( 4.408576920032446739E-17, 0.1350103645451945777, -0.9908441862701590219 ) ) ;
#15401 = CYLINDRICAL_SURFACE ( 'NONE', #181384, 0.1000000000000024342 ) ;
#15402 = CYLINDRICAL_SURFACE ( 'NONE', #119849, 11.80000000000000426 ) ;
#15403 = AXIS2_PLACEMENT_3D ( 'NONE', #249150, #27556, #48356 ) ;
#15404 = ORIENTED_EDGE ( 'NONE', *, *, #36383, .T. ) ;
#15405 = CIRCLE ( 'NONE', #27889, 2.000000000000001776 ) ;
#15406 = AXIS2_PLACEMENT_3D ( 'NONE', #125475, #139875, #21265 ) ;
#15407 = CIRCLE ( 'NONE', #2901, 0.1000000000000028644 ) ;
#15408 = DIRECTION ( 'NONE',  ( -1.000000000000000000, 0.000000000000000000, 0.000000000000000000 ) ) ;
#15409 = DIRECTION ( 'NONE',  ( -0.000000000000000000, -0.7397360091702755991, -0.6728971962616832059 ) ) ;
#15410 = VERTEX_POINT ( 'NONE', #81815 ) ;
#15411 = FACE_OUTER_BOUND ( 'NONE', #18535, .T. ) ;
#15413 = EDGE_CURVE ( 'NONE', #3257, #118478, #23379, .T. ) ;
#15412 = DIRECTION ( 'NONE',  ( 0.000000000000000000, 0.000000000000000000, 1.000000000000000000 ) ) ;
#15414 = CARTESIAN_POINT ( 'NONE',  ( 20.85000000000000142, 1.115600667400684642E-11, -200.9999999999999432 ) ) ;
#15415 = ORIENTED_EDGE ( 'NONE', *, *, #191678, .F. ) ;
#15416 = EDGE_CURVE ( 'NONE', #15545, #139599, #223242, .T. ) ;
#15417 = DIRECTION ( 'NONE',  ( 0.000000000000000000, 1.000000000000000000, 0.000000000000000000 ) ) ;
#15418 = AXIS2_PLACEMENT_3D ( 'NONE', #94217, #192069, #55073 ) ;
#15419 = ORIENTED_EDGE ( 'NONE', *, *, #248052, .F. ) ;
#15420 = FACE_OUTER_BOUND ( 'NONE', #75635, .T. ) ;
#15421 = CARTESIAN_POINT ( 'NONE',  ( 21.72449340488910252, 60.61704490885460217, -220.9543136786127491 ) ) ;
#15422 = AXIS2_PLACEMENT_3D ( 'NONE', #139072, #38738, #158707 ) ;
#15423 = CIRCLE ( 'NONE', #77931, 0.09999999999999939493 ) ;
#15424 = EDGE_CURVE ( 'NONE', #27358, #233060, #31764, .T. ) ;
#15425 = CIRCLE ( 'NONE', #161350, 0.1000000000000028644 ) ;
#15426 = ORIENTED_EDGE ( 'NONE', *, *, #255409, .T. ) ;
#15427 = CARTESIAN_POINT ( 'NONE',  ( -18.59999999999999787, 0.5663372425336981042, -209.0641885820623997 ) ) ;
#15428 = ORIENTED_EDGE ( 'NONE', *, *, #57389, .T. ) ;
#15429 = EDGE_CURVE ( 'NONE', #237026, #33150, #180962, .T. ) ;
#15430 = DIRECTION ( 'NONE',  ( -1.836970198721029934E-16, -1.000000000000000000, -6.982962677686266711E-15 ) ) ;
#15431 = CARTESIAN_POINT ( 'NONE',  ( -23.15000000000000213, 7.128833340093095217, -233.7327013124392749 ) ) ;
#15432 = DIRECTION ( 'NONE',  ( -1.000000000000000000, 2.775557561562908012E-13, 0.000000000000000000 ) ) ;
#15433 = PLANE ( 'NONE',  #75039 ) ;
#15434 = CARTESIAN_POINT ( 'NONE',  ( 21.05000000000005400, 65.19115966511134275, -30.12310748452479103 ) ) ;
#15435 = CARTESIAN_POINT ( 'NONE',  ( -23.25000000000000000, 4.250000000011156409, -179.6499999999999773 ) ) ;
#15436 = EDGE_CURVE ( 'NONE', #75372, #204523, #223910, .T. ) ;
#15437 = FACE_OUTER_BOUND ( 'NONE', #24588, .T. ) ;
#15438 = CARTESIAN_POINT ( 'NONE',  ( -22.57848426163148758, 64.15977721266104083, -247.1966340115571938 ) ) ;
#15440 = VERTEX_POINT ( 'NONE', #246073 ) ;
#15439 = CARTESIAN_POINT ( 'NONE',  ( 21.13422380239054732, 69.50667348520630640, -103.0231074845243597 ) ) ;
#15441 = ORIENTED_EDGE ( 'NONE', *, *, #71368, .T. ) ;
#15443 = CARTESIAN_POINT ( 'NONE',  ( -20.00857864376270001, 13.53887499352833146, -219.6971619212644669 ) ) ;
#15442 = CARTESIAN_POINT ( 'NONE',  ( -21.05000000000000071, 6.257814610476114758, 0.09779029130879343668 ) ) ;
#15444 = ORIENTED_EDGE ( 'NONE', *, *, #65169, .F. ) ;
#15446 = ORIENTED_EDGE ( 'NONE', *, *, #766, .T. ) ;
#15445 = DIRECTION ( 'NONE',  ( 0.000000000000000000, -6.938893903907270030E-14, 1.000000000000000000 ) ) ;
#15447 = CIRCLE ( 'NONE', #65486, 0.09999999999998898659 ) ;
#15448 = VERTEX_POINT ( 'NONE', #83094 ) ;
#15449 = CARTESIAN_POINT ( 'NONE',  ( -18.59999999999999787, 11.75000000001115197, -155.3500000000000227 ) ) ;
#15450 = CARTESIAN_POINT ( 'NONE',  ( 20.12481660106788084, 9.526343992285099205, -175.7261416690961937 ) ) ;
#15451 = CARTESIAN_POINT ( 'NONE',  ( -23.25000000000000000, 76.00000000001264766, -199.4731074845243484 ) ) ;
#15452 = CARTESIAN_POINT ( 'NONE',  ( -23.25000000000000000, 76.00000000001244871, -170.0231074845243597 ) ) ;
#15453 = DIRECTION ( 'NONE',  ( 0.000000000000000000, -1.000000000000000000, -6.860497997771532351E-15 ) ) ;
#15455 = CARTESIAN_POINT ( 'NONE',  ( -22.59999999999999787, 76.00000000001237765, -170.0231074845243597 ) ) ;
#15454 = CIRCLE ( 'NONE', #40416, 0.1000000000000028644 ) ;
#15456 = CARTESIAN_POINT ( 'NONE',  ( -23.15000000000000213, -6.688413578037177842, -212.5825622730469036 ) ) ;
#15457 = ADVANCED_FACE ( 'NONE', ( #23191 ), #62290, .F. ) ;
#15459 = AXIS2_PLACEMENT_3D ( 'NONE', #250790, #214244, #33083 ) ;
#15458 = FACE_OUTER_BOUND ( 'NONE', #176141, .T. ) ;
#15460 = ORIENTED_EDGE ( 'NONE', *, *, #164799, .F. ) ;
#15461 = ORIENTED_EDGE ( 'NONE', *, *, #228679, .F. ) ;
#15462 = LINE ( 'NONE', #254039, #106439 ) ;
#15463 = CIRCLE ( 'NONE', #123785, 0.09999999999999939493 ) ;
#15464 = VECTOR ( 'NONE', #82545, 1000.000000000000000 ) ;
#15465 = ORIENTED_EDGE ( 'NONE', *, *, #206902, .F. ) ;
#15466 = DIRECTION ( 'NONE',  ( 0.000000000000000000, -7.147358527629766941E-15, 1.000000000000000000 ) ) ;
#15467 = VERTEX_POINT ( 'NONE', #45298 ) ;
#15468 = CARTESIAN_POINT ( 'NONE',  ( 18.41832399655377372, -9.682403266673746955, -40.15684362002786401 ) ) ;
#15469 = PRODUCT_DEFINITION_FORMATION_WITH_SPECIFIED_SOURCE ( 'ANY', '', #14100, .NOT_KNOWN. ) ;
#15470 = EDGE_CURVE ( 'NONE', #197810, #215091, #73623, .T. ) ;
#15471 = VECTOR ( 'NONE', #79661, 1000.000000000000000 ) ;
#15472 = DIRECTION ( 'NONE',  ( 0.000000000000000000, 0.000000000000000000, -1.000000000000000000 ) ) ;
#15473 = CARTESIAN_POINT ( 'NONE',  ( -23.15000000000000213, 76.00000000001243450, -167.9231074845243938 ) ) ;
#15474 = AXIS2_PLACEMENT_3D ( 'NONE', #164131, #65011, #6314 ) ;
#15476 = ORIENTED_EDGE ( 'NONE', *, *, #23308, .T. ) ;
#15475 = CARTESIAN_POINT ( 'NONE',  ( -22.01447462590972748, 7.263800201241075172, -33.40096299994046092 ) ) ;
#15477 = CARTESIAN_POINT ( 'NONE',  ( 21.05000000000000071, 59.16775194334852017, -221.0793150863668473 ) ) ;
#15478 = ORIENTED_EDGE ( 'NONE', *, *, #121372, .T. ) ;
#15480 = ADVANCED_FACE ( 'NONE', ( #220086 ), #145664, .T. ) ;
#15479 = CARTESIAN_POINT ( 'NONE',  ( -18.40904629823844729, -9.499999999988851584, -207.6001895624822566 ) ) ;
#15481 = CARTESIAN_POINT ( 'NONE',  ( -18.47140463609787986, 85.67147468523226905, -29.35034702625017999 ) ) ;
#15482 = DIRECTION ( 'NONE',  ( -1.000000000000000000, -0.000000000000000000, -0.000000000000000000 ) ) ;
#15483 = FACE_OUTER_BOUND ( 'NONE', #1288, .T. ) ;
#15484 = LINE ( 'NONE', #153749, #7378 ) ;
#15485 = EDGE_CURVE ( 'NONE', #12655, #226018, #165174, .T. ) ;
#15486 = ORIENTED_EDGE ( 'NONE', *, *, #117947, .F. ) ;
#15488 = DIRECTION ( 'NONE',  ( 0.000000000000000000, 0.000000000000000000, -1.000000000000000000 ) ) ;
#15487 = CARTESIAN_POINT ( 'NONE',  ( -22.00411653962163072, 7.253442868381378084, -133.9009618942314148 ) ) ;
#15489 = AXIS2_PLACEMENT_3D ( 'NONE', #177360, #193048, #96477 ) ;
#15490 = ORIENTED_EDGE ( 'NONE', *, *, #75291, .T. ) ;
#15493 = ORIENTED_EDGE ( 'NONE', *, *, #68181, .T. ) ;
#15492 = CARTESIAN_POINT ( 'NONE',  ( 20.85000000000000142, 87.65000000001192859, -105.9231074845242091 ) ) ;
#15491 = CARTESIAN_POINT ( 'NONE',  ( -23.15000000000000213, 8.793666940903476004, -220.9353059101866847 ) ) ;
#15494 = EDGE_CURVE ( 'NONE', #163406, #41329, #46558, .T. ) ;
#15495 = FACE_OUTER_BOUND ( 'NONE', #57722, .T. ) ;
#15496 = AXIS2_PLACEMENT_3D ( 'NONE', #78642, #197309, #120395 ) ;
#15497 = CIRCLE ( 'NONE', #69835, 4.049999999999998934 ) ;
#15498 = CARTESIAN_POINT ( 'NONE',  ( -23.39999999999994529, 77.36076146337680370, -43.99645795275012006 ) ) ;
#15499 = ORIENTED_EDGE ( 'NONE', *, *, #19436, .F. ) ;
#15500 = SPHERICAL_SURFACE ( 'NONE', #217921, 0.1000000000000000056 ) ;
#15501 = CIRCLE ( 'NONE', #65353, 0.09999999999999971412 ) ;
#15503 = EDGE_CURVE ( 'NONE', #48651, #181045, #83234, .T. ) ;
#15502 = DIRECTION ( 'NONE',  ( 0.000000000000000000, 0.000000000000000000, -1.000000000000000000 ) ) ;
#15504 = VECTOR ( 'NONE', #147285, 1000.000000000000000 ) ;
#15505 = DIRECTION ( 'NONE',  ( 2.952720810173289112E-16, 1.000000000000000000, -6.088138035986627436E-46 ) ) ;
#15506 = AXIS2_PLACEMENT_3D ( 'NONE', #232409, #70774, #94147 ) ;
#15508 = ORIENTED_EDGE ( 'NONE', *, *, #51111, .T. ) ;
#15507 = CARTESIAN_POINT ( 'NONE',  ( -20.85000000000000142, 1.115600667400684642E-11, -200.9999999999999432 ) ) ;
#15509 = EDGE_CURVE ( 'NONE', #168004, #25144, #140024, .T. ) ;
#15510 = EDGE_CURVE ( 'NONE', #250352, #112246, #231650, .T. ) ;
#15511 = ORIENTED_EDGE ( 'NONE', *, *, #218929, .F. ) ;
#15512 = CARTESIAN_POINT ( 'NONE',  ( -16.91256925476570672, 9.985731158139332209, -113.0323575109947427 ) ) ;
#15513 = CYLINDRICAL_SURFACE ( 'NONE', #157553, 0.09999999999999939493 ) ;
#15514 = CARTESIAN_POINT ( 'NONE',  ( -16.78055652883087134, 44.14664813320825232, -235.2974609155759254 ) ) ;
#15515 = AXIS2_PLACEMENT_3D ( 'NONE', #159270, #194556, #254465 ) ;
#15516 = CARTESIAN_POINT ( 'NONE',  ( -16.86578989773641624, 66.01519019875350125, -157.4877723711466615 ) ) ;
#15517 = ORIENTED_EDGE ( 'NONE', *, *, #125789, .T. ) ;
#15519 = VECTOR ( 'NONE', #128860, 1000.000000000000000 ) ;
#15518 = CARTESIAN_POINT ( 'NONE',  ( 20.94999999999999929, -11.64999999998883595, -97.60000000000005116 ) ) ;
#15520 = EDGE_CURVE ( 'NONE', #229182, #181669, #192508, .T. ) ;
#15521 = SPHERICAL_SURFACE ( 'NONE', #114017, 0.1000000000000000056 ) ;
#15522 = LINE ( 'NONE', #175873, #172620 ) ;
#15523 = ORIENTED_EDGE ( 'NONE', *, *, #203737, .F. ) ;
#15524 = ADVANCED_FACE ( 'NONE', ( #229076 ), #13873, .F. ) ;
#15525 = CARTESIAN_POINT ( 'NONE',  ( 20.96937028524355640, 58.93813165352695904, -225.8439030394954159 ) ) ;
#15526 = EDGE_CURVE ( 'NONE', #235080, #254106, #27668, .T. ) ;
#15527 = CARTESIAN_POINT ( 'NONE',  ( 21.05000000000000071, 11.75000000001116263, -93.48519422934610645 ) ) ;
#15528 = CIRCLE ( 'NONE', #48812, 11.90000000000000213 ) ;
#15529 = ORIENTED_EDGE ( 'NONE', *, *, #69402, .F. ) ;
#15530 = CARTESIAN_POINT ( 'NONE',  ( 20.85000000000000142, 11.65000000001115943, -160.7161343370219129 ) ) ;
#15531 = FACE_OUTER_BOUND ( 'NONE', #248955, .T. ) ;
#15532 = DIRECTION ( 'NONE',  ( 1.000000000000000000, 0.000000000000000000, 0.000000000000000000 ) ) ;
#15533 = VERTEX_POINT ( 'NONE', #152120 ) ;
#15534 = ORIENTED_EDGE ( 'NONE', *, *, #77722, .F. ) ;
#15535 = CIRCLE ( 'NONE', #44739, 0.1000000000000024342 ) ;
#15536 = CARTESIAN_POINT ( 'NONE',  ( -21.05000000000000071, 55.11435547888748232, -226.8560373590520101 ) ) ;
#15537 = EDGE_LOOP ( 'NONE', ( #95086, #155109, #39859, #108724, #101982, #196386, #60827, #78650, #19642, #1982, #35311, #142590 ) ) ;
#15539 = VERTEX_POINT ( 'NONE', #28336 ) ;
#15538 = DIRECTION ( 'NONE',  ( 0.7071067811865475727, 0.6909108974501237954, 0.1504730267678056066 ) ) ;
#15540 = EDGE_CURVE ( 'NONE', #6487, #209133, #150809, .T. ) ;
#15541 = EDGE_CURVE ( 'NONE', #89873, #144828, #106901, .T. ) ;
#15542 = TOROIDAL_SURFACE ( 'NONE', #257073, 0.2000000000000000111, 0.1000000000000000056 ) ;
#15543 = AXIS2_PLACEMENT_3D ( 'NONE', #47552, #51389, #90540 ) ;
#15546 = ORIENTED_EDGE ( 'NONE', *, *, #216461, .F. ) ;
#15545 = VERTEX_POINT ( 'NONE', #52984 ) ;
#15544 = CARTESIAN_POINT ( 'NONE',  ( 21.14999999999999858, 60.91865828504416669, -234.1430899377568267 ) ) ;
#15547 = CIRCLE ( 'NONE', #111202, 0.5000000000000004441 ) ;
#15548 = CIRCLE ( 'NONE', #223796, 0.09999999999999158173 ) ;
#15550 = EDGE_CURVE ( 'NONE', #2377, #256658, #131858, .T. ) ;
#15549 = FACE_OUTER_BOUND ( 'NONE', #231038, .T. ) ;
#15551 = CARTESIAN_POINT ( 'NONE',  ( -16.89155683852503387, 12.54753878115997701, -211.8558912009372932 ) ) ;
#15552 = CARTESIAN_POINT ( 'NONE',  ( 21.05193202509564543, 10.72393601970834354, -112.6725346033258006 ) ) ;
#15553 = CARTESIAN_POINT ( 'NONE',  ( 20.95262331984766391, 65.49584273722271632, -195.9622191549311481 ) ) ;
#15554 = VECTOR ( 'NONE', #30982, 1000.000000000000000 ) ;
#15555 = DIRECTION ( 'NONE',  ( 0.000000000000000000, 7.116814260417668513E-15, -1.000000000000000000 ) ) ;
#15556 = CARTESIAN_POINT ( 'NONE',  ( -22.45437739390952459, 26.02743911632091312, -254.3139371337572072 ) ) ;
#15557 = ORIENTED_EDGE ( 'NONE', *, *, #78794, .F. ) ;
#15558 = ORIENTED_EDGE ( 'NONE', *, *, #207947, .T. ) ;
#15559 = EDGE_LOOP ( 'NONE', ( #162881, #114282, #36473, #36130 ) ) ;
#15560 = DIRECTION ( 'NONE',  ( 1.000000000000000000, 0.000000000000000000, 0.000000000000000000 ) ) ;
#15562 = ORIENTED_EDGE ( 'NONE', *, *, #163064, .T. ) ;
#15561 = DIRECTION ( 'NONE',  ( -0.000000000000000000, -0.000000000000000000, -1.000000000000000000 ) ) ;
#15563 = CARTESIAN_POINT ( 'NONE',  ( 18.59999999999999076, 64.18627039993180006, -224.3513032416919089 ) ) ;
#15564 = ORIENTED_EDGE ( 'NONE', *, *, #21655, .T. ) ;
#15565 = CARTESIAN_POINT ( 'NONE',  ( 21.53699400380799389, 6.787711793200783106, -100.4999999999817106 ) ) ;
#15566 = EDGE_LOOP ( 'NONE', ( #62034, #90173, #240324, #214786 ) ) ;
#15567 = CARTESIAN_POINT ( 'NONE',  ( -20.85000000000000142, -1.164121893230052995, -141.8148480855716684 ) ) ;
#15568 = AXIS2_PLACEMENT_3D ( 'NONE', #98911, #218875, #162788 ) ;
#15569 = VECTOR ( 'NONE', #154916, 1000.000000000000000 ) ;
#15570 = EDGE_CURVE ( 'NONE', #1130, #120155, #132536, .T. ) ;
#15571 = EDGE_LOOP ( 'NONE', ( #181339, #200859, #159091, #36117 ) ) ;
#15572 = DIRECTION ( 'NONE',  ( -1.000000000000000000, 0.000000000000000000, -0.000000000000000000 ) ) ;
#15574 = EDGE_CURVE ( 'NONE', #8977, #27613, #119389, .T. ) ;
#15573 = CYLINDRICAL_SURFACE ( 'NONE', #15368, 0.1000000000000055844 ) ;
#15575 = CIRCLE ( 'NONE', #198701, 11.89999999999999325 ) ;
#15577 = EDGE_LOOP ( 'NONE', ( #206334, #87764, #247105, #116318 ) ) ;
#15576 = ORIENTED_EDGE ( 'NONE', *, *, #50600, .F. ) ;
#15578 = ORIENTED_EDGE ( 'NONE', *, *, #128190, .T. ) ;
#15579 = DIRECTION ( 'NONE',  ( 1.000000000000000000, 0.000000000000000000, 0.000000000000000000 ) ) ;
#15580 = ORIENTED_EDGE ( 'NONE', *, *, #163663, .T. ) ;
#15581 = ORIENTED_EDGE ( 'NONE', *, *, #5501, .F. ) ;
#15582 = CARTESIAN_POINT ( 'NONE',  ( 18.59999999999999432, -1.835859311432484375, -112.0044391687985694 ) ) ;
#15585 = EDGE_CURVE ( 'NONE', #224010, #175406, #86028, .T. ) ;
#15584 = ORIENTED_EDGE ( 'NONE', *, *, #93633, .F. ) ;
#15583 = CARTESIAN_POINT ( 'NONE',  ( 21.05000000000000071, 76.00000000001216449, -140.6231074845243256 ) ) ;
#15586 = DIRECTION ( 'NONE',  ( 0.000000000000000000, 0.8814952561688437216, -0.4721928772777334582 ) ) ;
#15588 = FACE_OUTER_BOUND ( 'NONE', #256301, .T. ) ;
#15587 = DIRECTION ( 'NONE',  ( 0.000000000000000000, 0.8814952561688722543, -0.4721928772776801675 ) ) ;
#15589 = DIRECTION ( 'NONE',  ( 0.000000000000000000, 0.2128009952263604232, -0.9770955615653316162 ) ) ;
#15590 = CARTESIAN_POINT ( 'NONE',  ( 18.41356215285961895, -9.499999999988869348, -74.03206939669966857 ) ) ;
#15591 = CARTESIAN_POINT ( 'NONE',  ( 21.17356465864818560, 30.75698776691031000, -252.0867744921908695 ) ) ;
#15592 = VERTEX_POINT ( 'NONE', #226472 ) ;
#15593 = ADVANCED_FACE ( 'NONE', ( #70016, #30900 ), #127405, .F. ) ;
#15594 = VERTEX_POINT ( 'NONE', #111682 ) ;
#15595 = CARTESIAN_POINT ( 'NONE',  ( 21.05000000000000071, 76.00000000001240608, -174.3231074845243995 ) ) ;
#15596 = DIRECTION ( 'NONE',  ( 0.000000000000000000, -0.3738317757009718689, 0.9274965247785342815 ) ) ;
#15597 = DIRECTION ( 'NONE',  ( 0.000000000000000000, 0.000000000000000000, -1.000000000000000000 ) ) ;
#15598 = EDGE_CURVE ( 'NONE', #116437, #70665, #50399, .T. ) ;
#15599 = ORIENTED_EDGE ( 'NONE', *, *, #227048, .F. ) ;
#15600 = VECTOR ( 'NONE', #8934, 1000.000000000000000 ) ;
#15601 = CIRCLE ( 'NONE', #40554, 0.1999999999999987899 ) ;
#15602 = DIRECTION ( 'NONE',  ( 1.000000000000000000, 0.000000000000000000, 0.000000000000000000 ) ) ;
#15603 = AXIS2_PLACEMENT_3D ( 'NONE', #199889, #121639, #22534 ) ;
#15604 = AXIS2_PLACEMENT_3D ( 'NONE', #187574, #168029, #169311 ) ;
#15605 = EDGE_CURVE ( 'NONE', #243331, #92348, #149555, .T. ) ;
#15606 = CARTESIAN_POINT ( 'NONE',  ( -16.94132844910801339, 51.64367728818032788, -231.8888519332613214 ) ) ;
#15607 = DIRECTION ( 'NONE',  ( -1.000000000000000000, -0.000000000000000000, 0.000000000000000000 ) ) ;
#15609 = EDGE_CURVE ( 'NONE', #238460, #83068, #177691, .T. ) ;
#15608 = EDGE_CURVE ( 'NONE', #85479, #48315, #89539, .T. ) ;
#15610 = EDGE_LOOP ( 'NONE', ( #226684, #234267, #208657, #16189 ) ) ;
#15611 = ORIENTED_EDGE ( 'NONE', *, *, #136692, .T. ) ;
#15612 = DIRECTION ( 'NONE',  ( 0.000000000000000000, -0.9964539953858893018, -0.08413937888704772772 ) ) ;
#15613 = LINE ( 'NONE', #75580, #14988 ) ;
#15614 = ORIENTED_EDGE ( 'NONE', *, *, #6505, .F. ) ;
#15615 = DIRECTION ( 'NONE',  ( 1.000000000000000000, 0.000000000000000000, 0.000000000000000000 ) ) ;
#15616 = VERTEX_POINT ( 'NONE', #230340 ) ;
#15617 = CARTESIAN_POINT ( 'NONE',  ( 18.40916198585730967, -9.499999999988844479, -140.6001896318244349 ) ) ;
#15618 = CARTESIAN_POINT ( 'NONE',  ( -16.77732147262506146, 9.945966932629788815, -154.8364912432759013 ) ) ;
#15620 = FACE_OUTER_BOUND ( 'NONE', #245586, .T. ) ;
#15619 = CYLINDRICAL_SURFACE ( 'NONE', #78202, 0.1000000000000033362 ) ;
#15621 = DIRECTION ( 'NONE',  ( 0.000000000000000000, 0.000000000000000000, -1.000000000000000000 ) ) ;
#15622 = DIRECTION ( 'NONE',  ( 0.000000000000000000, -1.000000000000000000, 0.000000000000000000 ) ) ;
#15623 = AXIS2_PLACEMENT_3D ( 'NONE', #190578, #173616, #11943 ) ;
#15624 = AXIS2_PLACEMENT_3D ( 'NONE', #85899, #42965, #63808 ) ;
#15625 = CARTESIAN_POINT ( 'NONE',  ( -20.85000000000000142, 66.90607807833499976, -235.8243394455619182 ) ) ;
#15626 = EDGE_CURVE ( 'NONE', #126709, #126005, #51679, .T. ) ;
#15627 = EDGE_CURVE ( 'NONE', #254522, #60369, #248379, .T. ) ;
#15629 = ORIENTED_EDGE ( 'NONE', *, *, #102149, .T. ) ;
#15628 = VERTEX_POINT ( 'NONE', #154692 ) ;
#15630 = AXIS2_PLACEMENT_3D ( 'NONE', #72234, #34403, #172657 ) ;
#15631 = ORIENTED_EDGE ( 'NONE', *, *, #176735, .F. ) ;
#15632 = ADVANCED_FACE ( 'NONE', ( #256255 ), #98483, .F. ) ;
#15633 = CYLINDRICAL_SURFACE ( 'NONE', #29487, 2.599999999999998312 ) ;
#15634 = CARTESIAN_POINT ( 'NONE',  ( -20.54999999999999716, 1.999999999999998224, -20.27537807723789953 ) ) ;
#15635 = CARTESIAN_POINT ( 'NONE',  ( -21.05000000000000071, 11.65000000001115232, -33.60000000000000142 ) ) ;
#15636 = CARTESIAN_POINT ( 'NONE',  ( -18.47653818581419927, -9.465280387751805691, -107.6259608161398518 ) ) ;
#15638 = CARTESIAN_POINT ( 'NONE',  ( -12.29659703204452015, 66.64411154550927563, -86.73446458774640178 ) ) ;
#15637 = CARTESIAN_POINT ( 'NONE',  ( -16.83199318825828072, 66.06935387203138532, -182.7955222963152266 ) ) ;
#15639 = ADVANCED_FACE ( 'NONE', ( #16463 ), #231834, .T. ) ;
#15640 = CARTESIAN_POINT ( 'NONE',  ( 20.94999999999999574, 0.000000000000000000, 0.000000000000000000 ) ) ;
#15641 = ORIENTED_EDGE ( 'NONE', *, *, #31968, .F. ) ;
#15642 = CARTESIAN_POINT ( 'NONE',  ( -20.85000000000000142, 7.654382455240002159, -241.6162809886059790 ) ) ;
#15643 = ADVANCED_FACE ( 'NONE', ( #217183 ), #15165, .T. ) ;
#15644 = ORIENTED_EDGE ( 'NONE', *, *, #141080, .F. ) ;
#15645 = ORIENTED_EDGE ( 'NONE', *, *, #183746, .T. ) ;
#15646 = CARTESIAN_POINT ( 'NONE',  ( -21.14999999999999858, 87.75000000001267608, -203.5231074845243029 ) ) ;
#15647 = DIRECTION ( 'NONE',  ( 0.000000000000000000, -1.000000000000000000, 0.000000000000000000 ) ) ;
#15648 = CIRCLE ( 'NONE', #107361, 0.2000000000000000944 ) ;
#15649 = DIRECTION ( 'NONE',  ( 0.000000000000000000, 0.000000000000000000, 1.000000000000000000 ) ) ;
#15650 = DIRECTION ( 'NONE',  ( -1.000000000000000000, 0.000000000000000000, 0.000000000000000000 ) ) ;
#15651 = ORIENTED_EDGE ( 'NONE', *, *, #135513, .F. ) ;
#15652 = ORIENTED_EDGE ( 'NONE', *, *, #222922, .T. ) ;
#15653 = CARTESIAN_POINT ( 'NONE',  ( -21.05000000000000071, 16.44800918141279311, -240.8068063186265135 ) ) ;
#15654 = CARTESIAN_POINT ( 'NONE',  ( -20.85000000000000142, 77.16412189325330928, -128.6082593989527254 ) ) ;
#15655 = EDGE_CURVE ( 'NONE', #15694, #24871, #175536, .T. ) ;
#15656 = DIRECTION ( 'NONE',  ( 1.000000000000000000, -0.000000000000000000, -0.000000000000000000 ) ) ;
#15657 = LINE ( 'NONE', #232121, #27734 ) ;
#15658 = AXIS2_PLACEMENT_3D ( 'NONE', #175721, #235655, #51875 ) ;
#15659 = CARTESIAN_POINT ( 'NONE',  ( -23.25000000000000000, 65.66751761918692409, -130.9282609406112670 ) ) ;
#15660 = DIRECTION ( 'NONE',  ( 0.000000000000000000, 1.000000000000000000, -0.000000000000000000 ) ) ;
#15661 = DIRECTION ( 'NONE',  ( 0.000000000000000000, -0.8660254037844384856, 0.5000000000000003331 ) ) ;
#15663 = CARTESIAN_POINT ( 'NONE',  ( 18.59999999999999432, 77.83585931145546510, -91.51866831572576189 ) ) ;
#15662 = DIRECTION ( 'NONE',  ( 1.000000000000000000, 7.304098846218134667E-16, 5.100424963727256530E-30 ) ) ;
#15664 = DIRECTION ( 'NONE',  ( -1.000000000000000000, -0.000000000000000000, -0.000000000000000000 ) ) ;
#15665 = CIRCLE ( 'NONE', #148912, 12.87499999999999822 ) ;
#15667 = EDGE_CURVE ( 'NONE', #250279, #75355, #227519, .T. ) ;
#15666 = DIRECTION ( 'NONE',  ( 0.000000000000000000, 1.000000000000000000, 0.000000000000000000 ) ) ;
#15668 = CARTESIAN_POINT ( 'NONE',  ( -23.25000000000000000, 64.35000000001245724, -181.7731074845244450 ) ) ;
#15669 = AXIS2_PLACEMENT_3D ( 'NONE', #129632, #30555, #90493 ) ;
#15671 = EDGE_LOOP ( 'NONE', ( #250005, #217592, #97912, #69773 ) ) ;
#15670 = CARTESIAN_POINT ( 'NONE',  ( 19.88284271247461632, 54.46607474075112520, -228.7627709682279260 ) ) ;
#15672 = AXIS2_PLACEMENT_3D ( 'NONE', #222405, #244561, #5935 ) ;
#15673 = AXIS2_PLACEMENT_3D ( 'NONE', #83185, #45377, #166647 ) ;
#15675 = EDGE_CURVE ( 'NONE', #229949, #161543, #6951, .T. ) ;
#15674 = DIRECTION ( 'NONE',  ( 0.000000000000000000, 0.000000000000000000, -1.000000000000000000 ) ) ;
#15676 = AXIS2_PLACEMENT_3D ( 'NONE', #236906, #23028, #42553 ) ;
#15677 = ORIENTED_EDGE ( 'NONE', *, *, #92021, .F. ) ;
#15678 = CARTESIAN_POINT ( 'NONE',  ( 20.85000000000000142, 1.115600667400684642E-11, -141.8000000000000398 ) ) ;
#15679 = VERTEX_POINT ( 'NONE', #59374 ) ;
#15680 = CARTESIAN_POINT ( 'NONE',  ( 21.30000000000002558, 32.96286418198891255, -251.2069521516576174 ) ) ;
#15681 = CARTESIAN_POINT ( 'NONE',  ( 13.12229106158773284, 9.430637101707896264, -85.26826061806100654 ) ) ;
#15682 = DIRECTION ( 'NONE',  ( -1.000000000000000000, 0.000000000000000000, 0.000000000000000000 ) ) ;
#15683 = AXIS2_PLACEMENT_3D ( 'NONE', #102895, #82036, #159069 ) ;
#15684 = DIRECTION ( 'NONE',  ( -1.000000000000000000, -0.000000000000000000, -0.000000000000000000 ) ) ;
#15685 = CIRCLE ( 'NONE', #161417, 12.87499999999999822 ) ;
#15686 = CARTESIAN_POINT ( 'NONE',  ( 23.25000000000000000, 85.60000000001262777, -193.6291383618718385 ) ) ;
#15687 = LINE ( 'NONE', #74385, #119633 ) ;
#15688 = AXIS2_PLACEMENT_3D ( 'NONE', #78392, #220495, #120141 ) ;
#15689 = STYLED_ITEM ( 'NONE', ( #249642 ), #21402 ) ;
#15690 = ORIENTED_EDGE ( 'NONE', *, *, #105097, .T. ) ;
#15691 = DIRECTION ( 'NONE',  ( 1.000000000000000000, 3.265361837132813093E-16, -0.000000000000000000 ) ) ;
#15694 = VERTEX_POINT ( 'NONE', #253746 ) ;
#15693 = DIRECTION ( 'NONE',  ( 0.000000000000000000, 1.000000000000000000, 0.000000000000000000 ) ) ;
#15692 = AXIS2_PLACEMENT_3D ( 'NONE', #212704, #56166, #34095 ) ;
#15695 = DIRECTION ( 'NONE',  ( 1.000000000000000000, 0.000000000000000000, 0.000000000000000000 ) ) ;
#15696 = CARTESIAN_POINT ( 'NONE',  ( 18.59999999999999432, 1.162701749949165642, -75.10000000000003695 ) ) ;
#15697 = TOROIDAL_SURFACE ( 'NONE', #36548, 11.65000000000000036, 0.1000000000000000056 ) ;
#15698 = CARTESIAN_POINT ( 'NONE',  ( -22.48660254037844552, 31.80946045771259634, -238.8484668136873381 ) ) ;
#15699 = ORIENTED_EDGE ( 'NONE', *, *, #98140, .F. ) ;
#15700 = DIRECTION ( 'NONE',  ( 0.000000000000000000, -1.000000000000000000, 0.000000000000000000 ) ) ;
#15701 = SHAPE_DEFINITION_REPRESENTATION ( #186745, #1804 ) ;
#15702 = DIRECTION ( 'NONE',  ( 1.000000000000000000, -5.945622153099073960E-16, 5.981866248895712861E-16 ) ) ;
#15703 = DIRECTION ( 'NONE',  ( 7.304098846218134667E-16, 1.000000000000000000, -0.000000000000000000 ) ) ;
#15704 = VERTEX_POINT ( 'NONE', #76388 ) ;
#15705 = CARTESIAN_POINT ( 'NONE',  ( -23.15000000000000213, 69.09936979046463534, -247.6075824278584605 ) ) ;
#15706 = SPHERICAL_SURFACE ( 'NONE', #138301, 0.1000000000000000056 ) ;
#15707 = TOROIDAL_SURFACE ( 'NONE', #177998, 11.65000000000000036, 0.1000000000000000056 ) ;
#15708 = TOROIDAL_SURFACE ( 'NONE', #153088, 4.099999999999999645, 0.1000000000000000056 ) ;
#15709 = VECTOR ( 'NONE', #179548, 1000.000000000000000 ) ;
#15710 = CARTESIAN_POINT ( 'NONE',  ( -16.77683809663752257, 9.945835743215303282, -121.3360509808958341 ) ) ;
#15711 = EDGE_LOOP ( 'NONE', ( #228419, #12664, #122847, #137825 ) ) ;
#15712 = ORIENTED_EDGE ( 'NONE', *, *, #138285, .T. ) ;
#15713 = LINE ( 'NONE', #109632, #154843 ) ;
#15714 = DIRECTION ( 'NONE',  ( 0.000000000000000000, 1.000000000000000000, 1.224646799147353207E-16 ) ) ;
#15716 = AXIS2_PLACEMENT_3D ( 'NONE', #68861, #4990, #84503 ) ;
#15715 = DIRECTION ( 'NONE',  ( -0.000000000000000000, -0.000000000000000000, 1.000000000000000000 ) ) ;
#15717 = DIRECTION ( 'NONE',  ( 1.000000000000000000, 0.000000000000000000, 0.000000000000000000 ) ) ;
#15718 = EDGE_CURVE ( 'NONE', #78646, #76812, #133805, .T. ) ;
#15719 = CIRCLE ( 'NONE', #248740, 0.1000000000000051958 ) ;
#15721 = CYLINDRICAL_SURFACE ( 'NONE', #24414, 0.09999999999999939493 ) ;
#15720 = CARTESIAN_POINT ( 'NONE',  ( 21.05000000000000071, -1.476250985535760840, -194.6915786084529145 ) ) ;
#15722 = CARTESIAN_POINT ( 'NONE',  ( 18.59999999999999787, -8.150000000000007461, 32.89999999999999858 ) ) ;
#15723 = AXIS2_PLACEMENT_3D ( 'NONE', #188221, #69574, #231221 ) ;
#15724 = LINE ( 'NONE', #196886, #135280 ) ;
#15725 = DIRECTION ( 'NONE',  ( 0.7071067811865494601, -0.2890913453342123240, 0.6453109281988432810 ) ) ;
#15726 = DIRECTION ( 'NONE',  ( 0.000000000000000000, 0.000000000000000000, -1.000000000000000000 ) ) ;
#15727 = ORIENTED_EDGE ( 'NONE', *, *, #84728, .F. ) ;
#15728 = ORIENTED_EDGE ( 'NONE', *, *, #102361, .F. ) ;
#15729 = DIRECTION ( 'NONE',  ( 1.000000000000000000, 3.265361837132813093E-16, -0.000000000000000000 ) ) ;
#15730 = DIRECTION ( 'NONE',  ( -1.000000000000000000, -7.304098846218135653E-16, -4.639676173203994055E-30 ) ) ;
#15732 = CARTESIAN_POINT ( 'NONE',  ( -21.05000000000000071, 87.48912529308749697, -39.12310748452424747 ) ) ;
#15731 = FACE_OUTER_BOUND ( 'NONE', #128574, .T. ) ;
#15733 = CIRCLE ( 'NONE', #32486, 0.09999999999999939493 ) ;
#15734 = LINE ( 'NONE', #73143, #201803 ) ;
#15735 = ADVANCED_FACE ( 'NONE', ( #174277 ), #197629, .F. ) ;
#15736 = CARTESIAN_POINT ( 'NONE',  ( 15.57250062127603485, 12.88570875296796814, -216.1309391439169190 ) ) ;
#15737 = ORIENTED_EDGE ( 'NONE', *, *, #141405, .T. ) ;
#15738 = AXIS2_PLACEMENT_3D ( 'NONE', #59417, #734, #119444 ) ;
#15739 = ORIENTED_EDGE ( 'NONE', *, *, #234141, .T. ) ;
#15740 = ADVANCED_FACE ( 'NONE', ( #18990 ), #111013, .F. ) ;
#15741 = CIRCLE ( 'NONE', #44755, 0.09999999999998898659 ) ;
#15742 = AXIS2_PLACEMENT_3D ( 'NONE', #125632, #47358, #64381 ) ;
#15743 = CARTESIAN_POINT ( 'NONE',  ( -23.25000000000000000, 85.00000000001207923, -126.6291383618717816 ) ) ;
#15744 = VECTOR ( 'NONE', #224850, 1000.000000000000000 ) ;
#15745 = EDGE_LOOP ( 'NONE', ( #61527, #176850, #31869, #11656 ) ) ;
#15746 = DIRECTION ( 'NONE',  ( 2.952720810173289112E-16, -1.000000000000000000, 0.000000000000000000 ) ) ;
#15747 = ADVANCED_FACE ( 'NONE', ( #116824 ), #173433, .T. ) ;
#15748 = VECTOR ( 'NONE', #65913, 1000.000000000000000 ) ;
#15749 = DIRECTION ( 'NONE',  ( 5.603264701231745086E-32, -1.897661533703520636E-16, 1.000000000000000000 ) ) ;
#15750 = FACE_OUTER_BOUND ( 'NONE', #44696, .T. ) ;
#15751 = EDGE_CURVE ( 'NONE', #210814, #256383, #198501, .T. ) ;
#15752 = ADVANCED_FACE ( 'NONE', ( #75157 ), #98491, .T. ) ;
#15753 = VERTEX_POINT ( 'NONE', #55520 ) ;
#15754 = CARTESIAN_POINT ( 'NONE',  ( -23.25000000000000000, 76.00000000001270450, -207.5731074845243427 ) ) ;
#15755 = ADVANCED_FACE ( 'NONE', ( #176812 ), #94678, .F. ) ;
#15756 = LINE ( 'NONE', #254310, #112038 ) ;
#15757 = LINE ( 'NONE', #22163, #224292 ) ;
#15759 = CIRCLE ( 'NONE', #182332, 0.09999999999999939493 ) ;
#15758 = CARTESIAN_POINT ( 'NONE',  ( 21.05000000000000071, 77.16270174995064224, -195.4231074845243370 ) ) ;
#15760 = CARTESIAN_POINT ( 'NONE',  ( 21.40925344232283223, 75.90104981139253937, -143.1816263439147292 ) ) ;
#15761 = FACE_OUTER_BOUND ( 'NONE', #199988, .T. ) ;
#15763 = DIRECTION ( 'NONE',  ( 0.000000000000000000, 0.000000000000000000, 1.000000000000000000 ) ) ;
#15762 = FACE_OUTER_BOUND ( 'NONE', #80776, .T. ) ;
#15764 = EDGE_CURVE ( 'NONE', #171125, #125125, #94260, .T. ) ;
#15765 = LINE ( 'NONE', #31475, #32410 ) ;
#15766 = VERTEX_POINT ( 'NONE', #164930 ) ;
#15767 = CARTESIAN_POINT ( 'NONE',  ( -18.59999999999999787, 74.16465844978787914, -158.4679561919613775 ) ) ;
#15768 = ORIENTED_EDGE ( 'NONE', *, *, #27877, .T. ) ;
#15770 = VERTEX_POINT ( 'NONE', #180649 ) ;
#15769 = CARTESIAN_POINT ( 'NONE',  ( 23.24999999999999645, 7.128833340094563376, -233.7327013124401276 ) ) ;
#15771 = CIRCLE ( 'NONE', #215629, 0.5000000000000004441 ) ;
#15772 = ORIENTED_EDGE ( 'NONE', *, *, #16495, .F. ) ;
#15773 = CARTESIAN_POINT ( 'NONE',  ( -18.59999999999999787, 66.65000000001259650, -191.2731074845244166 ) ) ;
#15774 = EDGE_CURVE ( 'NONE', #8389, #200654, #127584, .T. ) ;
#15775 = CARTESIAN_POINT ( 'NONE',  ( -23.25000000000000000, 1.115600667400684642E-11, -33.50000000000000000 ) ) ;
#15776 = DIRECTION ( 'NONE',  ( 1.000000000000000000, -0.000000000000000000, -0.000000000000000000 ) ) ;
#15777 = DIRECTION ( 'NONE',  ( 1.000000000000000000, 0.000000000000000000, 0.000000000000000000 ) ) ;
#15778 = ORIENTED_EDGE ( 'NONE', *, *, #170152, .F. ) ;
#15779 = EDGE_CURVE ( 'NONE', #152369, #127414, #103647, .T. ) ;
#15780 = DIRECTION ( 'NONE',  ( 1.000000000000000000, 0.000000000000000000, 0.000000000000000000 ) ) ;
#15781 = CARTESIAN_POINT ( 'NONE',  ( 22.59999985501178799, 64.25013020700970401, -203.5887061543243419 ) ) ;
#15782 = ORIENTED_EDGE ( 'NONE', *, *, #102713, .T. ) ;
#15784 = ADVANCED_FACE ( 'NONE', ( #219757 ), #181747, .T. ) ;
#15783 = CARTESIAN_POINT ( 'NONE',  ( 20.94999999999999929, 68.87972903831429505, -99.36354444268502561 ) ) ;
#15785 = CARTESIAN_POINT ( 'NONE',  ( -20.94999999999999929, 1.162701749938009677, -8.000000000000000000 ) ) ;
#15786 = AXIS2_PLACEMENT_3D ( 'NONE', #3472, #67304, #82980 ) ;
#15787 = ORIENTED_EDGE ( 'NONE', *, *, #13671, .T. ) ;
#15789 = ORIENTED_EDGE ( 'NONE', *, *, #172367, .F. ) ;
#15788 = AXIS2_PLACEMENT_3D ( 'NONE', #223456, #46112, #180504 ) ;
#15790 = CARTESIAN_POINT ( 'NONE',  ( -16.92973740335290245, 9.992503814478434165, -188.4060590352027873 ) ) ;
#15791 = AXIS2_PLACEMENT_3D ( 'NONE', #99963, #139085, #179556 ) ;
#15792 = ORIENTED_EDGE ( 'NONE', *, *, #220093, .T. ) ;
#15793 = DIRECTION ( 'NONE',  ( 0.000000000000000000, 0.000000000000000000, -1.000000000000000000 ) ) ;
#15794 = ORIENTED_EDGE ( 'NONE', *, *, #13863, .F. ) ;
#15795 = LINE ( 'NONE', #176142, #151037 ) ;
#15796 = EDGE_CURVE ( 'NONE', #132728, #146076, #102595, .T. ) ;
#15797 = DIRECTION ( 'NONE',  ( 0.000000000000000000, -1.000000000000000000, 0.000000000000000000 ) ) ;
#15798 = LINE ( 'NONE', #253077, #3770 ) ;
#15799 = VECTOR ( 'NONE', #140525, 1000.000000000000000 ) ;
#15801 = VECTOR ( 'NONE', #205231, 1000.000000000000000 ) ;
#15800 = DIRECTION ( 'NONE',  ( 0.000000000000000000, 0.9126074666063771490, 0.4088369013363281623 ) ) ;
#15802 = DIRECTION ( 'NONE',  ( -0.000000000000000000, -0.1298341882519737922, -0.9915357197604890427 ) ) ;
#15803 = FACE_OUTER_BOUND ( 'NONE', #95074, .T. ) ;
#15804 = EDGE_LOOP ( 'NONE', ( #169491, #181668, #123083 ) ) ;
#15806 = DIRECTION ( 'NONE',  ( 0.000000000000000000, 0.9908441862701782288, -0.1350103645450542456 ) ) ;
#15805 = CARTESIAN_POINT ( 'NONE',  ( 21.13461538461538325, 22.93928069810350223, -230.1603595318553630 ) ) ;
#15807 = ORIENTED_EDGE ( 'NONE', *, *, #86463, .F. ) ;
#15810 = EDGE_LOOP ( 'NONE', ( #104953, #173350, #188589, #115058 ) ) ;
#15809 = DIRECTION ( 'NONE',  ( 0.000000000000000000, 0.000000000000000000, -1.000000000000000000 ) ) ;
#15808 = CARTESIAN_POINT ( 'NONE',  ( -20.54999999999999716, 9.690755012883057518, -211.4266134137857023 ) ) ;
#15811 = ADVANCED_FACE ( 'NONE', ( #163654 ), #181933, .T. ) ;
#15812 = VERTEX_POINT ( 'NONE', #124532 ) ;
#15813 = CIRCLE ( 'NONE', #53370, 0.09999999999999939493 ) ;
#15814 = CARTESIAN_POINT ( 'NONE',  ( -22.39999999999999858, 11.65000000001115588, -33.40000000000000568 ) ) ;
#15815 = CARTESIAN_POINT ( 'NONE',  ( 21.05000000000000071, 1.115600667400684642E-11, -100.5000000000000426 ) ) ;
#15816 = CARTESIAN_POINT ( 'NONE',  ( 20.94999999999999929, 7.128833340093095217, -233.7327013124392749 ) ) ;
#15817 = CARTESIAN_POINT ( 'NONE',  ( 21.30000000000002558, 67.23127455305841238, -235.8551265064783991 ) ) ;
#15818 = ORIENTED_EDGE ( 'NONE', *, *, #182618, .F. ) ;
#15820 = VERTEX_POINT ( 'NONE', #121958 ) ;
#15819 = DIRECTION ( 'NONE',  ( 1.000000000000000000, 0.000000000000000000, 0.000000000000000000 ) ) ;
#15821 = EDGE_CURVE ( 'NONE', #108079, #107188, #184482, .T. ) ;
#15824 = FACE_OUTER_BOUND ( 'NONE', #23735, .T. ) ;
#15823 = FACE_OUTER_BOUND ( 'NONE', #250485, .T. ) ;
#15822 = B_SPLINE_CURVE_WITH_KNOTS ( 'NONE', 3,
 ( #26798, #64600, #123311, #122019 ),
 .UNSPECIFIED., .F., .F.,
 ( 4, 4 ),
 ( 0.000000000000000000, 0.0002118541922231923684 ),
 .UNSPECIFIED. ) ;
#15826 = ORIENTED_EDGE ( 'NONE', *, *, #159015, .F. ) ;
#15825 = DIRECTION ( 'NONE',  ( 1.000000000000000000, -0.000000000000000000, -0.000000000000000000 ) ) ;
#15827 = EDGE_CURVE ( 'NONE', #84354, #153027, #102351, .T. ) ;
#15828 = EDGE_CURVE ( 'NONE', #14606, #211829, #144063, .T. ) ;
#15829 = ORIENTED_EDGE ( 'NONE', *, *, #128080, .F. ) ;
#15830 = EDGE_CURVE ( 'NONE', #237460, #100304, #161088, .T. ) ;
#15831 = ADVANCED_FACE ( 'NONE', ( #101049 ), #24158, .F. ) ;
#15832 = AXIS2_PLACEMENT_3D ( 'NONE', #20017, #81228, #177813 ) ;
#15833 = CARTESIAN_POINT ( 'NONE',  ( 20.95462737510932882, 11.92587769522588559, -206.1500708958423047 ) ) ;
#15834 = VERTEX_POINT ( 'NONE', #81506 ) ;
#15835 = DIRECTION ( 'NONE',  ( 1.000000000000000000, 0.000000000000000000, 0.000000000000000000 ) ) ;
#15836 = EDGE_LOOP ( 'NONE', ( #42630, #159585, #174437, #214903 ) ) ;
#15837 = ADVANCED_FACE ( 'NONE', ( #161096 ), #689, .F. ) ;
#15838 = FACE_OUTER_BOUND ( 'NONE', #135539, .T. ) ;
#15839 = AXIS2_PLACEMENT_3D ( 'NONE', #136226, #152004, #33352 ) ;
#15840 = ORIENTED_EDGE ( 'NONE', *, *, #189492, .F. ) ;
#15841 = DIRECTION ( 'NONE',  ( 2.715809747126117987E-16, 1.000000000000000000, 7.604267291953130166E-15 ) ) ;
#15842 = CIRCLE ( 'NONE', #86505, 0.1000000000000028644 ) ;
#15843 = AXIS2_PLACEMENT_3D ( 'NONE', #77458, #18787, #133602 ) ;
#15844 = FACE_OUTER_BOUND ( 'NONE', #172963, .T. ) ;
#15845 = AXIS2_PLACEMENT_3D ( 'NONE', #252407, #54216, #213289 ) ;
#15846 = ADVANCED_FACE ( 'NONE', ( #82780 ), #162382, .T. ) ;
#15847 = VERTEX_POINT ( 'NONE', #4557 ) ;
#15848 = ORIENTED_EDGE ( 'NONE', *, *, #25632, .T. ) ;
#15850 = DIRECTION ( 'NONE',  ( 0.000000000000000000, 0.000000000000000000, -1.000000000000000000 ) ) ;
#15849 = AXIS2_PLACEMENT_3D ( 'NONE', #126860, #205088, #207696 ) ;
#15851 = ORIENTED_EDGE ( 'NONE', *, *, #9379, .T. ) ;
#15852 = VERTEX_POINT ( 'NONE', #205320 ) ;
#15854 = ORIENTED_EDGE ( 'NONE', *, *, #219217, .T. ) ;
#15853 = CARTESIAN_POINT ( 'NONE',  ( 20.85000000000000142, 75.83895117929372987, -170.3072973288845731 ) ) ;
#15855 = EDGE_CURVE ( 'NONE', #222619, #94122, #84056, .T. ) ;
#15856 =( REPRESENTATION_RELATIONSHIP ('NONE','NONE', #36900, #1804 ) REPRESENTATION_RELATIONSHIP_WITH_TRANSFORMATION ( #105433 )SHAPE_REPRESENTATION_RELATIONSHIP( ) );
#15857 = EDGE_CURVE ( 'NONE', #193457, #29920, #232014, .T. ) ;
#15858 = ORIENTED_EDGE ( 'NONE', *, *, #203376, .F. ) ;
#15859 = ORIENTED_EDGE ( 'NONE', *, *, #214614, .F. ) ;
#15862 = ORIENTED_EDGE ( 'NONE', *, *, #229000, .T. ) ;
#15861 = ORIENTED_EDGE ( 'NONE', *, *, #8996, .F. ) ;
#15860 = DIRECTION ( 'NONE',  ( -1.000000000000000000, -0.000000000000000000, 0.000000000000000000 ) ) ;
#15864 = ORIENTED_EDGE ( 'NONE', *, *, #89846, .F. ) ;
#15863 = VECTOR ( 'NONE', #183440, 1000.000000000000114 ) ;
#15865 = TOROIDAL_SURFACE ( 'NONE', #157325, 11.65000000000000036, 0.1000000000000000056 ) ;
#15866 = VECTOR ( 'NONE', #27145, 1000.000000000000000 ) ;
#15867 = DIRECTION ( 'NONE',  ( 0.000000000000000000, 0.2128009952263568427, -0.9770955615653322823 ) ) ;
#15868 = CIRCLE ( 'NONE', #49149, 0.5000000000000004441 ) ;
#15869 = ORIENTED_EDGE ( 'NONE', *, *, #148852, .T. ) ;
#15870 = AXIS2_PLACEMENT_3D ( 'NONE', #98814, #256589, #3595 ) ;
#15871 = DIRECTION ( 'NONE',  ( 1.000000000000000000, 0.000000000000000000, 0.000000000000000000 ) ) ;
#15872 =( BOUNDED_SURFACE ( )  B_SPLINE_SURFACE ( 3, 2, ( 
 ( #123744, #115072, #237590 ),
 ( #19840, #195909, #194637 ),
 ( #203268, #58911, #96754 ),
 ( #15998, #176349, #135891 ) ),
 .UNSPECIFIED., .F., .F., .F. ) 
 B_SPLINE_SURFACE_WITH_KNOTS ( ( 4, 4 ),
 ( 3, 3 ),
 ( 0.000000000000000000, 1.570796326794896558 ),
 ( 0.000000000000000000, 1.000000000000000000 ),
 .UNSPECIFIED. ) 
 GEOMETRIC_REPRESENTATION_ITEM ( )  RATIONAL_B_SPLINE_SURFACE ( (
 ( 1.000000000000000000, 0.7644017236018784134, 1.000000000000000000),
 ( 1.000000000000000000, 0.7651312202474060964, 1.000000000000000000),
 ( 1.000000000000000000, 0.7389971855005991186, 1.000000000000000000),
 ( 1.000000000000000000, 0.7071067811865444641, 1.000000000000000000) ) ) 
 REPRESENTATION_ITEM ( '' )  SURFACE ( )  );
#15874 = ORIENTED_EDGE ( 'NONE', *, *, #175580, .T. ) ;
#15873 = DIRECTION ( 'NONE',  ( 1.000000000000000000, 0.000000000000000000, 0.000000000000000000 ) ) ;
#15875 = PLANE ( 'NONE',  #29933 ) ;
#15876 = ORIENTED_EDGE ( 'NONE', *, *, #222511, .T. ) ;
#15877 = CIRCLE ( 'NONE', #199000, 0.1000000000000009492 ) ;
#15878 = ORIENTED_EDGE ( 'NONE', *, *, #138840, .F. ) ;
#15879 = CARTESIAN_POINT ( 'NONE',  ( 18.39999999999999858, 85.50000000001161027, -62.49103808782458458 ) ) ;
#15881 = EDGE_CURVE ( 'NONE', #184818, #33376, #223591, .T. ) ;
#15880 = CARTESIAN_POINT ( 'NONE',  ( 18.51697539158856998, 18.38637412622488299, -236.9471295141160283 ) ) ;
#15882 = ORIENTED_EDGE ( 'NONE', *, *, #69037, .T. ) ;
#15883 = ORIENTED_EDGE ( 'NONE', *, *, #130796, .T. ) ;
#15884 = LINE ( 'NONE', #249661, #218526 ) ;
#15885 = DIRECTION ( 'NONE',  ( 0.000000000000000000, -1.000000000000000000, 0.000000000000000000 ) ) ;
#15886 = AXIS2_PLACEMENT_3D ( 'NONE', #94771, #92199, #34833 ) ;
#15888 = EDGE_LOOP ( 'NONE', ( #170810, #2283 ) ) ;
#15887 = ORIENTED_EDGE ( 'NONE', *, *, #163950, .T. ) ;
#15889 = ORIENTED_EDGE ( 'NONE', *, *, #195982, .T. ) ;
#15890 = CARTESIAN_POINT ( 'NONE',  ( -40.23850191057533010, 65.25000000001119815, -4.423107484524790856 ) ) ;
#15891 = ORIENTED_EDGE ( 'NONE', *, *, #226891, .F. ) ;
#15892 = EDGE_LOOP ( 'NONE', ( #83183, #205712, #155994, #203197 ) ) ;
#15893 = CARTESIAN_POINT ( 'NONE',  ( 20.95159278453404283, 18.81431913549488399, -229.8868573851966062 ) ) ;
#15894 = EDGE_LOOP ( 'NONE', ( #90887, #23496, #189905, #175031 ) ) ;
#15895 = CARTESIAN_POINT ( 'NONE',  ( -16.93302609847409457, 12.44611011958480518, -211.1708003455683524 ) ) ;
#15896 = DIRECTION ( 'NONE',  ( 0.000000000000000000, -1.000000000000000000, 0.000000000000000000 ) ) ;
#15897 = ORIENTED_EDGE ( 'NONE', *, *, #61535, .F. ) ;
#15898 = CIRCLE ( 'NONE', #257585, 0.09999999999998898659 ) ;
#15899 = EDGE_CURVE ( 'NONE', #86132, #137741, #69523, .T. ) ;
#15900 = AXIS2_PLACEMENT_3D ( 'NONE', #70146, #28464, #8863 ) ;
#15901 = ORIENTED_EDGE ( 'NONE', *, *, #130987, .F. ) ;
#15902 = CARTESIAN_POINT ( 'NONE',  ( 23.15000000000000213, -11.48912529306489994, -97.40000000000004832 ) ) ;
#15903 = EDGE_CURVE ( 'NONE', #126100, #131047, #90333, .T. ) ;
#15904 = ORIENTED_EDGE ( 'NONE', *, *, #8164, .T. ) ;
#15905 = EDGE_CURVE ( 'NONE', #146870, #227485, #91818, .T. ) ;
#15906 = DIRECTION ( 'NONE',  ( 1.000000000000000000, -0.000000000000000000, 0.000000000000000000 ) ) ;
#15907 = ADVANCED_FACE ( 'NONE', ( #167529 ), #71000, .F. ) ;
#15908 = VERTEX_POINT ( 'NONE', #128383 ) ;
#15909 = EDGE_LOOP ( 'NONE', ( #99667, #105679, #224918, #17767 ) ) ;
#15910 = CARTESIAN_POINT ( 'NONE',  ( 23.25000000000000000, 48.79765034352288922, -253.5326144460178170 ) ) ;
#15912 = ORIENTED_EDGE ( 'NONE', *, *, #64587, .F. ) ;
#15911 = FACE_OUTER_BOUND ( 'NONE', #240915, .T. ) ;
#15913 = CARTESIAN_POINT ( 'NONE',  ( 20.94999999999999929, 76.00000000001195133, -103.0231074845243171 ) ) ;
#15914 = DIRECTION ( 'NONE',  ( 0.000000000000000000, 0.000000000000000000, -1.000000000000000000 ) ) ;
#15915 = ORIENTED_EDGE ( 'NONE', *, *, #44975, .T. ) ;
#15916 = AXIS2_PLACEMENT_3D ( 'NONE', #141290, #220818, #60450 ) ;
#15917 = DIRECTION ( 'NONE',  ( -1.000000000000000000, 0.000000000000000000, 0.000000000000000000 ) ) ;
#15918 = CARTESIAN_POINT ( 'NONE',  ( -21.05000000000000071, -11.64999999998884306, -97.60000000000005116 ) ) ;
#15919 = LINE ( 'NONE', #177570, #219483 ) ;
#15920 = DIRECTION ( 'NONE',  ( -1.000000000000000000, -1.836970198721029934E-16, -3.186635328391151676E-31 ) ) ;
#15921 = DIRECTION ( 'NONE',  ( 0.000000000000000000, 1.897661533703519897E-16, -1.000000000000000000 ) ) ;
#15923 = VECTOR ( 'NONE', #149404, 1000.000000000000000 ) ;
#15922 = CARTESIAN_POINT ( 'NONE',  ( -21.05000000000000071, 6.540656951712397138, -33.60000000000000142 ) ) ;
#15924 = CIRCLE ( 'NONE', #69898, 0.09999999999999864553 ) ;
#15925 = FACE_OUTER_BOUND ( 'NONE', #48088, .T. ) ;
#15926 = DIRECTION ( 'NONE',  ( -1.000000000000000000, 1.652117596168391700E-15, 0.000000000000000000 ) ) ;
#15928 = DIRECTION ( 'NONE',  ( 1.000000000000000000, 0.000000000000000000, 0.000000000000000000 ) ) ;
#15927 = AXIS2_PLACEMENT_3D ( 'NONE', #170923, #169633, #249140 ) ;
#15930 = ORIENTED_EDGE ( 'NONE', *, *, #76111, .F. ) ;
#15929 = AXIS2_PLACEMENT_3D ( 'NONE', #147328, #10402, #22589 ) ;
#15931 = ADVANCED_FACE ( 'NONE', ( #29317, #107519, #151817 ), #51366, .F. ) ;
#15932 = EDGE_CURVE ( 'NONE', #125446, #87825, #186217, .T. ) ;
#15934 = VERTEX_POINT ( 'NONE', #28023 ) ;
#15933 = ORIENTED_EDGE ( 'NONE', *, *, #11419, .F. ) ;
#15935 = ORIENTED_EDGE ( 'NONE', *, *, #151014, .T. ) ;
#15936 = CARTESIAN_POINT ( 'NONE',  ( -21.09316766718153247, 0.03926340232583033080, -94.12984668752531547 ) ) ;
#15937 = FACE_OUTER_BOUND ( 'NONE', #120027, .T. ) ;
#15939 = CARTESIAN_POINT ( 'NONE',  ( 20.94999999999999929, 67.23127455305835554, -235.8551265064784559 ) ) ;
#15938 = CARTESIAN_POINT ( 'NONE',  ( 23.04999999999999716, 8.822561741666397950, -12.65000000000000746 ) ) ;
#15940 = VERTEX_POINT ( 'NONE', #90519 ) ;
#15941 = ORIENTED_EDGE ( 'NONE', *, *, #30031, .T. ) ;
#15942 = CIRCLE ( 'NONE', #165775, 0.09999999999999939493 ) ;
#15943 = CARTESIAN_POINT ( 'NONE',  ( -18.39999999999999858, -9.519327731081281385, -174.4729763765593020 ) ) ;
#15944 = EDGE_CURVE ( 'NONE', #184818, #79286, #170120, .T. ) ;
#15945 = CARTESIAN_POINT ( 'NONE',  ( -21.04999999999994387, 83.90000000001120384, -34.86056257560453986 ) ) ;
#15946 = FACE_OUTER_BOUND ( 'NONE', #94023, .T. ) ;
#15947 = EDGE_CURVE ( 'NONE', #29656, #102316, #247023, .T. ) ;
#15948 = CARTESIAN_POINT ( 'NONE',  ( 18.46905048506369340, -9.473744257371235378, -73.67598629225537366 ) ) ;
#15949 = ORIENTED_EDGE ( 'NONE', *, *, #216838, .T. ) ;
#15950 = ORIENTED_EDGE ( 'NONE', *, *, #34747, .F. ) ;
#15951 = VECTOR ( 'NONE', #96532, 1000.000000000000114 ) ;
#15952 = CYLINDRICAL_SURFACE ( 'NONE', #238205, 0.1000000000000001443 ) ;
#15953 = LINE ( 'NONE', #171189, #188650 ) ;
#15954 = ORIENTED_EDGE ( 'NONE', *, *, #95767, .T. ) ;
#15955 = CARTESIAN_POINT ( 'NONE',  ( -20.94999999999999929, 68.87972903831482085, -166.3635444426850825 ) ) ;
#15956 = CARTESIAN_POINT ( 'NONE',  ( 18.41832399655356411, 77.26488349376249687, -241.9697967040461322 ) ) ;
#15957 = CYLINDRICAL_SURFACE ( 'NONE', #156846, 0.09999999999999939493 ) ;
#15958 = EDGE_CURVE ( 'NONE', #140958, #72309, #77859, .T. ) ;
#15959 = CARTESIAN_POINT ( 'NONE',  ( 18.50000000000000000, -9.399999999988843058, -40.79725975966329798 ) ) ;
#15960 = CARTESIAN_POINT ( 'NONE',  ( 18.39999999999999503, 11.75000000001113953, -146.6500000000000341 ) ) ;
#15961 = ORIENTED_EDGE ( 'NONE', *, *, #198290, .T. ) ;
#15962 = FACE_OUTER_BOUND ( 'NONE', #1298, .T. ) ;
#15963 = LINE ( 'NONE', #32973, #126668 ) ;
#15964 = FACE_OUTER_BOUND ( 'NONE', #93420, .T. ) ;
#15966 = CARTESIAN_POINT ( 'NONE',  ( -13.40000000000000213, -8.350000000000004974, 15.00000000000000355 ) ) ;
#15965 = CARTESIAN_POINT ( 'NONE',  ( -20.85000000000000142, 46.46967969402479781, -243.0849751855955674 ) ) ;
#15967 = DIRECTION ( 'NONE',  ( 0.000000000000000000, 0.9126074666063769270, 0.4088369013363280513 ) ) ;
#15969 = ADVANCED_FACE ( 'NONE', ( #187087 ), #111200, .T. ) ;
#15968 = CARTESIAN_POINT ( 'NONE',  ( -20.94999999999999929, 7.070967871809997973, -171.2465642218683115 ) ) ;
#15970 = VECTOR ( 'NONE', #201059, 1000.000000000000000 ) ;
#15971 = AXIS2_PLACEMENT_3D ( 'NONE', #249471, #89092, #248177 ) ;
#15972 = AXIS2_PLACEMENT_3D ( 'NONE', #101103, #181992, #103699 ) ;
#15973 = CARTESIAN_POINT ( 'NONE',  ( -18.59999999999999787, 11.65000000001115232, -200.9999999999999432 ) ) ;
#15974 = CARTESIAN_POINT ( 'NONE',  ( -21.07946286933444924, 69.67096268100443979, -136.5997913277807925 ) ) ;
#15975 = VERTEX_POINT ( 'NONE', #30584 ) ;
#15976 =( BOUNDED_SURFACE ( )  B_SPLINE_SURFACE ( 3, 2, ( 
 ( #241596, #184178, #60379 ),
 ( #64245, #222004, #163354 ),
 ( #43397, #160807, #122944 ),
 ( #103348, #223300, #4252 ) ),
 .UNSPECIFIED., .F., .F., .F. ) 
 B_SPLINE_SURFACE_WITH_KNOTS ( ( 4, 4 ),
 ( 3, 3 ),
 ( 1.219727444046192488E-19, 0.0003124336600439509004 ),
 ( 0.000000000000000000, 1.000000000000000000 ),
 .UNSPECIFIED. ) 
 GEOMETRIC_REPRESENTATION_ITEM ( )  RATIONAL_B_SPLINE_SURFACE ( (
 ( 1.000000000000000000, 0.7071067811865475727, 1.000000000000000000),
 ( 1.000000000000000000, 0.7089187706049692173, 1.000000000000000000),
 ( 1.000000000000000000, 0.7039288185052148261, 1.000000000000000000),
 ( 1.000000000000000000, 0.7040654476016184882, 1.000000000000000000) ) ) 
 REPRESENTATION_ITEM ( '' )  SURFACE ( )  );
#15977 = ORIENTED_EDGE ( 'NONE', *, *, #225619, .T. ) ;
#15978 = PLANE ( 'NONE',  #111246 ) ;
#15979 = ORIENTED_EDGE ( 'NONE', *, *, #116788, .F. ) ;
#15980 = EDGE_CURVE ( 'NONE', #234078, #192351, #48832, .T. ) ;
#15981 = CARTESIAN_POINT ( 'NONE',  ( 18.59999999999999076, 6.982009704867611077, -171.1961521182563217 ) ) ;
#15982 = ORIENTED_EDGE ( 'NONE', *, *, #81253, .T. ) ;
#15983 = EDGE_CURVE ( 'NONE', #255544, #16182, #67116, .T. ) ;
#15984 = TOROIDAL_SURFACE ( 'NONE', #170115, 11.65000000000000036, 0.1000000000000000056 ) ;
#15985 = AXIS2_PLACEMENT_3D ( 'NONE', #31478, #53578, #254320 ) ;
#15986 = DIRECTION ( 'NONE',  ( 0.000000000000000000, 0.000000000000000000, -1.000000000000000000 ) ) ;
#15987 = ORIENTED_EDGE ( 'NONE', *, *, #202958, .F. ) ;
#15988 = CIRCLE ( 'NONE', #20244, 0.9000000000000014655 ) ;
#15989 = CARTESIAN_POINT ( 'NONE',  ( -22.39999999999999858, -0.09999999998884338825, -21.85042919245520210 ) ) ;
#15990 = DIRECTION ( 'NONE',  ( 0.000000000000000000, 0.000000000000000000, 1.000000000000000000 ) ) ;
#15991 = DIRECTION ( 'NONE',  ( 1.000000000000000000, 0.000000000000000000, 0.000000000000000000 ) ) ;
#15993 = ORIENTED_EDGE ( 'NONE', *, *, #164644, .T. ) ;
#15992 = CARTESIAN_POINT ( 'NONE',  ( -16.84981964351505468, 29.99731868204598939, -234.7321595084263492 ) ) ;
#15995 = CARTESIAN_POINT ( 'NONE',  ( 19.97071067695831559, 11.72071067696947644, -192.1762534328032075 ) ) ;
#15994 = CARTESIAN_POINT ( 'NONE',  ( 21.14999999999999858, 6.390846877240202950, -199.6081416912452653 ) ) ;
#15996 = CARTESIAN_POINT ( 'NONE',  ( 18.50000000000000000, -9.499999999988842703, -88.75000000000004263 ) ) ;
#15997 = CARTESIAN_POINT ( 'NONE',  ( -23.15000000000000213, 11.75000000001115552, -59.98519422934606382 ) ) ;
#15998 = CARTESIAN_POINT ( 'NONE',  ( -20.09999999999999787, 5.552655413246002425, 16.61686199900910310 ) ) ;
#15999 = CARTESIAN_POINT ( 'NONE',  ( 23.14999999999999858, 11.65000000001116298, -93.48519422934610645 ) ) ;
#16000 = ORIENTED_EDGE ( 'NONE', *, *, #147961, .T. ) ;
#16001 = LINE ( 'NONE', #255819, #125089 ) ;
#16002 = VERTEX_POINT ( 'NONE', #132230 ) ;
#16003 = CIRCLE ( 'NONE', #103250, 0.09999999999998898659 ) ;
#16004 = CARTESIAN_POINT ( 'NONE',  ( -20.94999999999999929, 76.00000000001244871, -170.0231074845243597 ) ) ;
#16005 = ORIENTED_EDGE ( 'NONE', *, *, #101873, .F. ) ;
#16006 = CIRCLE ( 'NONE', #124310, 0.09999999999999939493 ) ;
#16007 = AXIS2_PLACEMENT_3D ( 'NONE', #53217, #132775, #192738 ) ;
#16008 = CARTESIAN_POINT ( 'NONE',  ( -20.64999999999999858, 47.70572087816298534, -241.8629305864830030 ) ) ;
#16009 = CARTESIAN_POINT ( 'NONE',  ( -16.93301857435212554, 9.976309354735457546, -20.88577557116142813 ) ) ;
#16010 = LINE ( 'NONE', #100614, #203481 ) ;
#16011 = ORIENTED_EDGE ( 'NONE', *, *, #132796, .F. ) ;
#16012 = AXIS2_PLACEMENT_3D ( 'NONE', #55104, #33061, #171291 ) ;
#16013 = ORIENTED_EDGE ( 'NONE', *, *, #105266, .T. ) ;
#16014 = DIRECTION ( 'NONE',  ( 0.000000000000000000, 0.9126074666063660468, 0.4088369013363524762 ) ) ;
#16015 = DIRECTION ( 'NONE',  ( 1.000000000000000000, 0.000000000000000000, 0.000000000000000000 ) ) ;
#16016 = CARTESIAN_POINT ( 'NONE',  ( -16.77431908686106610, 63.08607373851209132, -213.1423865084627209 ) ) ;
#16017 = CARTESIAN_POINT ( 'NONE',  ( -21.05000000000000071, -0.2561057920810652089, -33.46510355832771211 ) ) ;
#16018 = ADVANCED_FACE ( 'NONE', ( #230045 ), #138088, .T. ) ;
#16020 = DIRECTION ( 'NONE',  ( 0.000000000000000000, -0.1350103645451945777, 0.9908441862701590219 ) ) ;
#16019 = FACE_OUTER_BOUND ( 'NONE', #134501, .T. ) ;
#16021 = AXIS2_PLACEMENT_3D ( 'NONE', #145026, #27703, #242851 ) ;
#16023 = SPHERICAL_SURFACE ( 'NONE', #182564, 0.1000000000000000056 ) ;
#16022 = AXIS2_PLACEMENT_3D ( 'NONE', #141028, #81020, #220557 ) ;
#16024 = DIRECTION ( 'NONE',  ( 0.000000000000000000, -1.000000000000000000, -6.982962677686265922E-15 ) ) ;
#16025 = FACE_OUTER_BOUND ( 'NONE', #65533, .T. ) ;
#16026 = AXIS2_PLACEMENT_3D ( 'NONE', #184443, #110046, #25397 ) ;
#16027 = ORIENTED_EDGE ( 'NONE', *, *, #134268, .T. ) ;
#16028 = CARTESIAN_POINT ( 'NONE',  ( -16.87036670365548474, 9.989418819301645769, -20.97956011730205006 ) ) ;
#16030 = ORIENTED_EDGE ( 'NONE', *, *, #51186, .T. ) ;
#16029 = CARTESIAN_POINT ( 'NONE',  ( -21.14999999999999858, 64.25313205997782973, -247.2214437328673853 ) ) ;
#16031 = CARTESIAN_POINT ( 'NONE',  ( 21.05000000000000071, 4.850467289719617270, -12.03426740900167857 ) ) ;
#16032 = CARTESIAN_POINT ( 'NONE',  ( -18.59999999999999787, -1.149570369564537842, -108.3159124845020074 ) ) ;
#16034 = DIRECTION ( 'NONE',  ( -0.000000000000000000, 0.9651348961777157509, -0.2617529984165031243 ) ) ;
#16033 = DIRECTION ( 'NONE',  ( 1.000000000000000000, 0.000000000000000000, 0.000000000000000000 ) ) ;
#16035 = EDGE_CURVE ( 'NONE', #4561, #39320, #19627, .T. ) ;
#16037 = EDGE_LOOP ( 'NONE', ( #86342, #76349, #203770, #158557 ) ) ;
#16036 = DIRECTION ( 'NONE',  ( 0.000000000000000000, -0.8814952561688430555, 0.4721928772777346239 ) ) ;
#16039 = CARTESIAN_POINT ( 'NONE',  ( -23.25000000000000000, 11.75000000001115552, -155.7499999999999716 ) ) ;
#16038 = DIRECTION ( 'NONE',  ( 0.000000000000000000, 0.000000000000000000, 1.000000000000000000 ) ) ;
#16040 = DIRECTION ( 'NONE',  ( -0.7071067811865475727, -0.7071067811865475727, -0.000000000000000000 ) ) ;
#16041 = DIRECTION ( 'NONE',  ( -1.000000000000000000, 0.000000000000000000, 0.000000000000000000 ) ) ;
#16042 = FACE_OUTER_BOUND ( 'NONE', #47930, .T. ) ;
#16043 = CARTESIAN_POINT ( 'NONE',  ( -18.51697539158857353, 10.31565961587945957, -139.5364194119178478 ) ) ;
#16044 = EDGE_LOOP ( 'NONE', ( #112107, #166714, #210141, #176270 ) ) ;
#16045 = CARTESIAN_POINT ( 'NONE',  ( 23.24999999999999645, 7.128833340094563376, -233.7327013124401276 ) ) ;
#16046 = VECTOR ( 'NONE', #139764, 1000.000000000000000 ) ;
#16048 = ADVANCED_FACE ( 'NONE', ( #56514 ), #33170, .F. ) ;
#16047 = ORIENTED_EDGE ( 'NONE', *, *, #151680, .F. ) ;
#16049 = CARTESIAN_POINT ( 'NONE',  ( 23.14999999999999858, 6.650000000011155876, -45.85000000000000142 ) ) ;
#16050 = AXIS2_PLACEMENT_3D ( 'NONE', #62857, #221905, #182838 ) ;
#16051 = ORIENTED_EDGE ( 'NONE', *, *, #208238, .T. ) ;
#16052 = CARTESIAN_POINT ( 'NONE',  ( -20.92356734117541706, 46.42459709376391430, -243.0752906381742662 ) ) ;
#16053 = ORIENTED_EDGE ( 'NONE', *, *, #89303, .T. ) ;
#16054 = VECTOR ( 'NONE', #249393, 1000.000000000000000 ) ;
#16055 = DIRECTION ( 'NONE',  ( 1.000000000000000000, 0.000000000000000000, 0.000000000000000000 ) ) ;
#16057 = CARTESIAN_POINT ( 'NONE',  ( 20.94999999999999929, 71.00000000001230660, -157.6178414656113205 ) ) ;
#16056 =( GEOMETRIC_REPRESENTATION_CONTEXT ( 3 ) GLOBAL_UNCERTAINTY_ASSIGNED_CONTEXT ( ( #80551 ) ) GLOBAL_UNIT_ASSIGNED_CONTEXT ( ( #66681, #142349, #6694 ) ) REPRESENTATION_CONTEXT ( 'NONE', 'WORKASPACE' ) );
#16058 = AXIS2_PLACEMENT_3D ( 'NONE', #250344, #211218, #32623 ) ;
#16059 = CIRCLE ( 'NONE', #182633, 4.050000000000000711 ) ;
#16060 = EDGE_CURVE ( 'NONE', #249334, #173650, #96912, .T. ) ;
#16062 = EDGE_CURVE ( 'NONE', #52763, #203994, #194798, .T. ) ;
#16061 = DIRECTION ( 'NONE',  ( 0.000000000000000000, 0.000000000000000000, -1.000000000000000000 ) ) ;
#16063 = ORIENTED_EDGE ( 'NONE', *, *, #117310, .F. ) ;
#16064 = AXIS2_PLACEMENT_3D ( 'NONE', #132282, #110151, #28082 ) ;
#16065 = CARTESIAN_POINT ( 'NONE',  ( -22.37643362114956602, -1.525963729632202837, -193.5277898285476397 ) ) ;
#16066 = DIRECTION ( 'NONE',  ( -1.000000000000000000, -0.000000000000000000, -0.000000000000000000 ) ) ;
#16067 = FACE_OUTER_BOUND ( 'NONE', #36833, .T. ) ;
#16068 = CARTESIAN_POINT ( 'NONE',  ( -23.25000000000000000, 1.115649040949250830E-11, -63.10000000000000142 ) ) ;
#16069 = EDGE_LOOP ( 'NONE', ( #235286, #125234, #192212, #145513 ) ) ;
#16071 = AXIS2_PLACEMENT_3D ( 'NONE', #76731, #57150, #153769 ) ;
#16070 = DIRECTION ( 'NONE',  ( 0.000000000000000000, 0.5826443254699606999, 0.8127272543711416830 ) ) ;
#16072 = VECTOR ( 'NONE', #254560, 1000.000000000000114 ) ;
#16073 = ORIENTED_EDGE ( 'NONE', *, *, #25509, .F. ) ;
#16075 = VERTEX_POINT ( 'NONE', #134769 ) ;
#16074 = CARTESIAN_POINT ( 'NONE',  ( -18.50000000000000000, 64.25000000001179501, -81.67310748452439384 ) ) ;
#16076 = ORIENTED_EDGE ( 'NONE', *, *, #104411, .F. ) ;
#16077 = CARTESIAN_POINT ( 'NONE',  ( 22.00411653889209873, 0.09903810579706272266, -59.74655713235965493 ) ) ;
#16078 = CLOSED_SHELL ( 'NONE', ( #114748, #235998, #2548, #163033, #16117, #129052, #101375, #101041, #24713, #38558, #109404, #82852, #133080, #224577, #184670, #212507, #167420, #167536, #98380, #84554, #86889, #239566, #158134, #44216, #250729, #135563, #123821, #181916, #11684, #164566, #9826, #252335, #57627, #214030, #170477, #71359, #127141, #113343, #193406, #211503, #168401, #22585, #4419, #184841, #199110, #61050, #90876, #37472, #165377, #75791, #48707, #234951, #77646, #150367, #10779, #127628, #95580, #253796, #27238, #181306, #148597, #93442, #244860, #233250, #94758, #173673, #102306, #65682, #128795, #88767, #31397, #188094, #36521, #233343, #161380, #212716, #224946, #224406, #22824, #2203, #86779, #162433, #171137, #141806, #192281, #83168, #49105, #26121, #72362, #226620, #64778, #4781, #238146, #29951, #133260, #109120, #109649, #81396, #225110, #214704, #153229, #167715, #73443, #164590, #94601, #216156, #61190, #152830, #70300, #218904, #185313, #170999, #68481, #1668, #31645, #197933, #134786, #206350, #46707, #32985, #197564, #115266, #235003, #137212, #223461, #84492, #68412, #220721, #155183, #155254, #133572, #50882, #135093, #16780, #34429, #6310, #134908, #117942, #8443, #148892, #62168, #26534, #62046, #39476, #163069, #130713, #184340, #74687, #16899, #46988, #1485, #145326, #108479, #143812, #114865, #81060, #5322, #126335, #221014, #141412, #92968, #217844, #255160, #192306, #246848, #194113, #53872, #22607, #137393, #140284, #87681, #140139, #28026, #211901, #150602, #61195, #189269, #198027, #175014, #11002, #212630, #40502, #253105, #253351, #9762, #99425, #6657, #26298, #241828, #219, #72067, #65200, #77569, #20185, #170513, #159468, #136476, #181663, #218940, #129177, #114151, #220976, #75003, #255647, #64358, #170613, #217774, #123983, #123299, #126728, #234135, #26542, #217447, #133245, #42168, #33988, #172153, #199469, #225327, #199826, #203284, #126298, #12372, #136185, #151621, #89141, #130262, #223543, #123946, #141541, #144995, #196008, #203691, #222672, #128333, #119580, #93613, #118357, #74494, #72248, #169686, #149729, #72439, #37896, #103420, #142730, #149839, #183868, #16891, #202549, #92541, #148613, #156583, #184665, #37822, #78025, #210336, #60111, #41762, #234833, #51253, #4862, #3997, #223974, #155333, #231097, #41639, #226929, #30051, #166524, #4798, #82182, #39723, #13704, #201126, #236157, #91176, #136472, #159472, #91474, #187211, #92554, #125357, #253147, #59040, #51086, #92935, #197871, #235903, #58563, #59552, #140678, #66635, #199705, #193029, #66215, #125048, #183827, #130115, #177528, #37015, #10847, #64224, #9406, #203989, #28157, #194119, #202941, #233230, #229609, #249309, #181154, #39060, #183228, #123312, #78946, #54931, #50475, #86745, #241600, #26167, #128196, #44119, #7998, #50647, #240987, #222935, #37118, #97388, #192166, #71742, #248282, #99150, #82905, #210176, #150999, #180365, #8465, #208358, #242412, #106672, #105587, #41517, #240749, #137531, #76656, #73150, #16555, #30651, #222290, #127053, #220006, #51415, #14817, #253342, #20739, #204281, #67345, #1407, #149524, #154261, #48897, #214788, #157103, #155432, #67671, #229486, #137211, #108127, #214320, #195181, #235073, #43783, #17694, #17369, #48947, #243945, #241318, #2786, #161899, #108364, #122889, #212297, #88428, #66693, #156186, #98184, #101952, #151522, #209010, #186810, #81337, #229664, #111771, #37879, #198566, #157744, #42649, #105353, #111672, #16970, #149655, #91780, #91009, #128846, #138297, #240926, #9036, #221169, #74949, #189581, #191747, #107061, #150390, #240409, #190197, #213370, #81887, #254412, #42065, #78474, #178621, #112303, #128472, #205684, #237560, #164711, #204954, #107592, #46235, #201476, #106873, #49739, #95415, #162090, #217856, #232589, #141314, #160100, #98281, #19968, #110031, #16810, #198584, #134435, #227134, #254618, #130086, #134695, #68982, #180700, #107903, #203685, #24601, #142043, #138617, #228955, #24836, #102849, #108243, #116162, #209022, #183295, #39040, #117845, #127055, #87095, #20452, #247488, #14065, #85605, #4680, #31164, #174015, #153907, #238113, #228221, #126105 ) ) ;
#16079 = EDGE_CURVE ( 'NONE', #85377, #253683, #214336, .T. ) ;
#16080 = FACE_OUTER_BOUND ( 'NONE', #157821, .T. ) ;
#16081 = DIRECTION ( 'NONE',  ( 0.000000000000000000, 0.000000000000000000, 1.000000000000000000 ) ) ;
#16082 = CARTESIAN_POINT ( 'NONE',  ( 20.94999999999999929, 9.374458193048763377, -220.5475659691911119 ) ) ;
#16083 = ORIENTED_EDGE ( 'NONE', *, *, #71997, .T. ) ;
#16084 = FACE_OUTER_BOUND ( 'NONE', #112155, .T. ) ;
#16085 = CARTESIAN_POINT ( 'NONE',  ( -2.995603634470891112E-16, 6.650000000011155876, -188.6499999999999488 ) ) ;
#16086 = ORIENTED_EDGE ( 'NONE', *, *, #242478, .F. ) ;
#16087 = TOROIDAL_SURFACE ( 'NONE', #207606, 3.899999999999999467, 0.1000000000000000056 ) ;
#16089 = ORIENTED_EDGE ( 'NONE', *, *, #234291, .T. ) ;
#16088 = DIRECTION ( 'NONE',  ( 0.000000000000000000, 1.000000000000000000, 1.734723475976817507E-14 ) ) ;
#16090 = AXIS2_PLACEMENT_3D ( 'NONE', #42227, #241703, #106015 ) ;
#16092 = EDGE_CURVE ( 'NONE', #119534, #3185, #198670, .T. ) ;
#16091 = DIRECTION ( 'NONE',  ( 1.000000000000000000, 0.000000000000000000, 0.000000000000000000 ) ) ;
#16093 = CIRCLE ( 'NONE', #215944, 0.09999999999999939493 ) ;
#16094 = CARTESIAN_POINT ( 'NONE',  ( -16.89935556175729303, 9.950000000011135270, -80.13967636288485608 ) ) ;
#16095 = AXIS2_PLACEMENT_3D ( 'NONE', #69168, #89974, #249083 ) ;
#16096 = CARTESIAN_POINT ( 'NONE',  ( -18.40000000000000213, 64.66825945288634614, -48.67310748452440805 ) ) ;
#16097 = ORIENTED_EDGE ( 'NONE', *, *, #75206, .F. ) ;
#16098 = LINE ( 'NONE', #175194, #88174 ) ;
#16099 = CARTESIAN_POINT ( 'NONE',  ( 20.96428641294449235, 64.25000000001249134, -176.8482143065824062 ) ) ;
#16100 = VECTOR ( 'NONE', #64020, 1000.000000000000000 ) ;
#16101 = CARTESIAN_POINT ( 'NONE',  ( 23.14999999999999503, 11.65000000000000746, 11.75000000000000000 ) ) ;
#16102 = CIRCLE ( 'NONE', #199242, 0.09999999999999939493 ) ;
#16103 = AXIS2_PLACEMENT_3D ( 'NONE', #41962, #105733, #100590 ) ;
#16104 = AXIS2_PLACEMENT_3D ( 'NONE', #184490, #239349, #1999 ) ;
#16105 = VERTEX_POINT ( 'NONE', #177801 ) ;
#16106 = CARTESIAN_POINT ( 'NONE',  ( 21.05000000000000071, 67.07338541492448769, -61.05142446530125966 ) ) ;
#16107 = EDGE_CURVE ( 'NONE', #241382, #137660, #2850, .T. ) ;
#16108 = EDGE_CURVE ( 'NONE', #85480, #152615, #78658, .T. ) ;
#16109 = ORIENTED_EDGE ( 'NONE', *, *, #104843, .T. ) ;
#16110 = DIRECTION ( 'NONE',  ( 0.000000000000000000, -0.8496786552930076786, -0.5273008465188218086 ) ) ;
#16111 = CYLINDRICAL_SURFACE ( 'NONE', #216559, 0.09999999999998898659 ) ;
#16113 = EDGE_LOOP ( 'NONE', ( #98849, #63173, #1952, #28126 ) ) ;
#16112 = CARTESIAN_POINT ( 'NONE',  ( 21.04999999999999716, 10.62872031401550466, -146.1500000000000341 ) ) ;
#16114 = DIRECTION ( 'NONE',  ( 1.000000000000000000, 0.000000000000000000, 0.000000000000000000 ) ) ;
#16115 = FACE_OUTER_BOUND ( 'NONE', #124654, .T. ) ;
#16117 = ADVANCED_FACE ( 'NONE', ( #37009 ), #244453, .T. ) ;
#16116 = CARTESIAN_POINT ( 'NONE',  ( 22.49231231312463208, 64.35001509633467265, -103.0841603721257655 ) ) ;
#16119 = ADVANCED_FACE ( 'NONE', ( #176508 ), #190316, .T. ) ;
#16118 = CARTESIAN_POINT ( 'NONE',  ( -23.25000000000000000, 15.90518444080776028, -219.2841490888777116 ) ) ;
#16120 = LINE ( 'NONE', #175218, #160198 ) ;
#16121 = AXIS2_PLACEMENT_3D ( 'NONE', #140477, #141762, #136627 ) ;
#16122 = DIRECTION ( 'NONE',  ( 0.000000000000000000, 0.000000000000000000, -1.000000000000000000 ) ) ;
#16123 = CARTESIAN_POINT ( 'NONE',  ( 21.11927991906888025, 6.448493118502572230, -66.99091632052613932 ) ) ;
#16125 = EDGE_LOOP ( 'NONE', ( #84967, #46722, #10094, #257880 ) ) ;
#16124 = FACE_OUTER_BOUND ( 'NONE', #256356, .T. ) ;
#16126 = EDGE_CURVE ( 'NONE', #28771, #40138, #28015, .T. ) ;
#16127 = EDGE_CURVE ( 'NONE', #603, #32631, #144491, .T. ) ;
#16129 = EDGE_CURVE ( 'NONE', #55330, #42401, #252160, .T. ) ;
#16128 = ADVANCED_FACE ( 'NONE', ( #93091 ), #165370, .T. ) ;
#16130 = DIRECTION ( 'NONE',  ( -1.000000000000000000, 0.000000000000000000, 0.000000000000000000 ) ) ;
#16131 = CARTESIAN_POINT ( 'NONE',  ( 23.14999999999999858, 5.500000000011153745, -54.59473398108690390 ) ) ;
#16132 = DIRECTION ( 'NONE',  ( -1.000000000000000000, 0.000000000000000000, 0.000000000000000000 ) ) ;
#16133 = EDGE_LOOP ( 'NONE', ( #41152, #86266, #230424, #8093 ) ) ;
#16134 = CARTESIAN_POINT ( 'NONE',  ( -18.39999999999999858, -9.499999999988849808, -107.1001893912220879 ) ) ;
#16135 = EDGE_CURVE ( 'NONE', #186188, #49960, #253447, .T. ) ;
#16136 = DIRECTION ( 'NONE',  ( 0.000000000000000000, -1.077886431674909336E-14, 1.000000000000000000 ) ) ;
#16137 = SURFACE_STYLE_FILL_AREA ( #240303 ) ;
#16138 = AXIS2_PLACEMENT_3D ( 'NONE', #159087, #223718, #237321 ) ;
#16139 = AXIS2_PLACEMENT_3D ( 'NONE', #56560, #236507, #197380 ) ;
#16140 = B_SPLINE_CURVE_WITH_KNOTS ( 'NONE', 3,
 ( #1741, #66872, #44749, #225908, #185537, #81267, #160853, #203807 ),
 .UNSPECIFIED., .F., .F.,
 ( 4, 2, 2, 4 ),
 ( 0.000000000000000000, 0.0001881495939909161091, 0.0002822243909863741637, 0.0003762991879818322182 ),
 .UNSPECIFIED. ) ;
#16141 = ORIENTED_EDGE ( 'NONE', *, *, #128146, .F. ) ;
#16142 = ADVANCED_FACE ( 'NONE', ( #2975 ), #118308, .T. ) ;
#16143 = CIRCLE ( 'NONE', #207669, 12.87499999999999822 ) ;
#16144 = EDGE_CURVE ( 'NONE', #169097, #22978, #43403, .T. ) ;
#16145 = DIRECTION ( 'NONE',  ( 2.952720810173289112E-16, 1.000000000000000000, -6.088138035986627436E-46 ) ) ;
#16146 = LINE ( 'NONE', #254678, #222156 ) ;
#16147 = EDGE_CURVE ( 'NONE', #109794, #170736, #42137, .T. ) ;
#16148 = ORIENTED_EDGE ( 'NONE', *, *, #43437, .F. ) ;
#16149 = CIRCLE ( 'NONE', #195220, 11.65000000000000746 ) ;
#16150 = CARTESIAN_POINT ( 'NONE',  ( -23.15000000000000213, -4.914013037343267776, -233.1828366659746905 ) ) ;
#16151 = ORIENTED_EDGE ( 'NONE', *, *, #248160, .T. ) ;
#16152 = DIRECTION ( 'NONE',  ( 0.000000000000000000, 0.000000000000000000, -1.000000000000000000 ) ) ;
#16154 = EDGE_LOOP ( 'NONE', ( #249134, #251480, #185549, #8413 ) ) ;
#16153 = CARTESIAN_POINT ( 'NONE',  ( 20.94999999999999929, 36.65892442174935439, -249.5511627012433848 ) ) ;
#16155 = ADVANCED_FACE ( 'NONE', ( #179095 ), #121677, .T. ) ;
#16156 = EDGE_LOOP ( 'NONE', ( #222120, #112422, #116970, #83913 ) ) ;
#16157 = FACE_OUTER_BOUND ( 'NONE', #48609, .T. ) ;
#16158 = AXIS2_PLACEMENT_3D ( 'NONE', #214349, #192233, #93106 ) ;
#16159 = AXIS2_PLACEMENT_3D ( 'NONE', #200960, #87421, #104401 ) ;
#16160 = ORIENTED_EDGE ( 'NONE', *, *, #225089, .F. ) ;
#16162 = ORIENTED_EDGE ( 'NONE', *, *, #240335, .F. ) ;
#16161 = ORIENTED_EDGE ( 'NONE', *, *, #88754, .F. ) ;
#16164 = CARTESIAN_POINT ( 'NONE',  ( 18.43473516226069364, 85.49494228277033869, -129.4772088011747257 ) ) ;
#16163 = VECTOR ( 'NONE', #186374, 1000.000000000000000 ) ;
#16165 = ORIENTED_EDGE ( 'NONE', *, *, #185330, .T. ) ;
#16166 = CARTESIAN_POINT ( 'NONE',  ( 20.04999999999999716, 10.51799536955199166, -208.1761252362501864 ) ) ;
#16167 = VERTEX_POINT ( 'NONE', #404 ) ;
#16168 = VECTOR ( 'NONE', #8521, 1000.000000000000227 ) ;
#16169 = ORIENTED_EDGE ( 'NONE', *, *, #56557, .F. ) ;
#16170 = CARTESIAN_POINT ( 'NONE',  ( -23.25000000000000000, 36.65892442174935439, -249.5511627012433848 ) ) ;
#16171 = CARTESIAN_POINT ( 'NONE',  ( 20.85000000000000142, 77.83585931145546510, -91.51866831572576189 ) ) ;
#16172 = LINE ( 'NONE', #137358, #236369 ) ;
#16173 = VERTEX_POINT ( 'NONE', #23869 ) ;
#16174 = DIRECTION ( 'NONE',  ( 1.000000000000000000, 0.000000000000000000, 0.000000000000000000 ) ) ;
#16175 = CARTESIAN_POINT ( 'NONE',  ( -18.49999999999997158, -9.321008403350138138, -74.23593824907793248 ) ) ;
#16176 = CYLINDRICAL_SURFACE ( 'NONE', #6441, 0.09999999999999939493 ) ;
#16177 = VERTEX_POINT ( 'NONE', #143773 ) ;
#16178 = DIRECTION ( 'NONE',  ( 1.000000000000000000, 0.000000000000000000, 0.000000000000000000 ) ) ;
#16179 = CARTESIAN_POINT ( 'NONE',  ( -18.33682934331562109, 38.25511225049375241, -261.1960286750406794 ) ) ;
#16180 = DIRECTION ( 'NONE',  ( 0.000000000000000000, 0.000000000000000000, -1.000000000000000000 ) ) ;
#16181 = CIRCLE ( 'NONE', #161929, 11.90000000000000391 ) ;
#16182 = VERTEX_POINT ( 'NONE', #103354 ) ;
#16183 = CARTESIAN_POINT ( 'NONE',  ( -17.11825945287481687, 14.25671114421267305, -219.2337924566137701 ) ) ;
#16184 = ORIENTED_EDGE ( 'NONE', *, *, #220862, .T. ) ;
#16185 = AXIS2_PLACEMENT_3D ( 'NONE', #29683, #184867, #84439 ) ;
#16186 = ORIENTED_EDGE ( 'NONE', *, *, #229537, .F. ) ;
#16187 = AXIS2_PLACEMENT_3D ( 'NONE', #22474, #101953, #94589 ) ;
#16188 = CYLINDRICAL_SURFACE ( 'NONE', #5475, 0.1000000000000124678 ) ;
#16189 = ORIENTED_EDGE ( 'NONE', *, *, #54521, .F. ) ;
#16190 = ORIENTED_EDGE ( 'NONE', *, *, #131233, .F. ) ;
#16191 = DIRECTION ( 'NONE',  ( 0.000000000000000000, 0.000000000000000000, -1.000000000000000000 ) ) ;
#16192 = CARTESIAN_POINT ( 'NONE',  ( -16.93353400591625757, 10.00461239618409515, -188.4326844702054018 ) ) ;
#16193 = VERTEX_POINT ( 'NONE', #124238 ) ;
#16194 = CIRCLE ( 'NONE', #249234, 0.1000000000000028644 ) ;
#16195 = ORIENTED_EDGE ( 'NONE', *, *, #169356, .F. ) ;
#16196 = CARTESIAN_POINT ( 'NONE',  ( -23.25000000000000000, 4.837354856632041113E-16, -29.60000000000000142 ) ) ;
#16197 = DIRECTION ( 'NONE',  ( 0.000000000000000000, -0.9998779222360104635, -0.01562499999996343723 ) ) ;
#16198 = EDGE_LOOP ( 'NONE', ( #152724, #48434, #228400, #146662 ) ) ;
#16199 = EDGE_CURVE ( 'NONE', #210485, #195345, #111375, .T. ) ;
#16200 = CIRCLE ( 'NONE', #45210, 0.09999999999999485689 ) ;
#16201 = TOROIDAL_SURFACE ( 'NONE', #28699, 3.899999999999999467, 0.1000000000000000056 ) ;
#16202 = EDGE_CURVE ( 'NONE', #41248, #199581, #248760, .T. ) ;
#16204 = ORIENTED_EDGE ( 'NONE', *, *, #115386, .F. ) ;
#16203 = AXIS2_PLACEMENT_3D ( 'NONE', #47705, #145525, #225051 ) ;
#16206 = DIRECTION ( 'NONE',  ( 1.000000000000000000, -7.304098846218134667E-16, -5.100424963727256530E-30 ) ) ;
#16205 = AXIS2_PLACEMENT_3D ( 'NONE', #5073, #101599, #126336 ) ;
#16207 = EDGE_CURVE ( 'NONE', #120003, #97490, #69699, .T. ) ;
#16208 = DIRECTION ( 'NONE',  ( 1.000000000000000000, 2.952720810173289112E-16, -0.000000000000000000 ) ) ;
#16209 = EDGE_CURVE ( 'NONE', #139486, #2368, #36388, .T. ) ;
#16210 = DIRECTION ( 'NONE',  ( -0.000000000000000000, 0.9876197685951276783, 0.1568667991644721316 ) ) ;
#16211 = DIRECTION ( 'NONE',  ( 7.304098846218134667E-16, -1.000000000000000000, 0.000000000000000000 ) ) ;
#16212 = AXIS2_PLACEMENT_3D ( 'NONE', #169919, #211573, #225952 ) ;
#16214 = CIRCLE ( 'NONE', #136991, 0.09999999999999939493 ) ;
#16213 = FACE_OUTER_BOUND ( 'NONE', #45792, .T. ) ;
#16215 = CARTESIAN_POINT ( 'NONE',  ( -20.64999999999999858, 1.115600667400684642E-11, -200.9999999999999432 ) ) ;
#16216 = FACE_OUTER_BOUND ( 'NONE', #141349, .T. ) ;
#16218 = CARTESIAN_POINT ( 'NONE',  ( 20.94999999999999574, 1.750000000011155743, -45.16951155790165018 ) ) ;
#16217 = CARTESIAN_POINT ( 'NONE',  ( -23.25000000000000000, 69.01799029515495931, -32.32695536626808774 ) ) ;
#16219 = DIRECTION ( 'NONE',  ( 0.7071359030028113724, 0.000000000000000000, 0.7070776581708677622 ) ) ;
#16220 = DIRECTION ( 'NONE',  ( -1.000000000000000000, -0.000000000000000000, 1.073024830501117725E-15 ) ) ;
#16221 = CIRCLE ( 'NONE', #224477, 0.09999999999998898659 ) ;
#16222 = FACE_OUTER_BOUND ( 'NONE', #60796, .T. ) ;
#16223 = DIRECTION ( 'NONE',  ( -1.000000000000000000, 0.000000000000000000, -0.000000000000000000 ) ) ;
#16224 = ORIENTED_EDGE ( 'NONE', *, *, #25549, .T. ) ;
#16225 = ADVANCED_FACE ( 'NONE', ( #83766 ), #181642, .F. ) ;
#16226 = AXIS2_PLACEMENT_3D ( 'NONE', #54724, #75603, #170882 ) ;
#16228 = EDGE_CURVE ( 'NONE', #59145, #40125, #223788, .T. ) ;
#16227 = CIRCLE ( 'NONE', #220226, 0.1999999999999981515 ) ;
#16229 = AXIS2_PLACEMENT_3D ( 'NONE', #7575, #165373, #145786 ) ;
#16231 = EDGE_LOOP ( 'NONE', ( #182843, #139904, #65165, #163755 ) ) ;
#16230 = CARTESIAN_POINT ( 'NONE',  ( 18.59999999999999076, 76.00000000001126921, -203.5231074845248997 ) ) ;
#16232 = AXIS2_PLACEMENT_3D ( 'NONE', #23925, #203811, #120463 ) ;
#16233 = CYLINDRICAL_SURFACE ( 'NONE', #135895, 0.09999999999999543976 ) ;
#16234 = FACE_OUTER_BOUND ( 'NONE', #218423, .T. ) ;
#16235 = ORIENTED_EDGE ( 'NONE', *, *, #2737, .T. ) ;
#16236 = SURFACE_STYLE_USAGE ( .BOTH. , #31948 ) ;
#16237 = EDGE_CURVE ( 'NONE', #34543, #56882, #53110, .T. ) ;
#16238 = DIRECTION ( 'NONE',  ( 0.000000000000000000, -0.8700118002898359348, 0.4930308989875165082 ) ) ;
#16239 = PRODUCT_DEFINITION_SHAPE ( 'NONE', 'NONE',  #258138 ) ;
#16240 = EDGE_CURVE ( 'NONE', #156295, #85685, #65520, .T. ) ;
#16241 = CARTESIAN_POINT ( 'NONE',  ( -16.97092634996618443, 10.00088896635888958, -54.36985723370199253 ) ) ;
#16242 = CIRCLE ( 'NONE', #7861, 1.749999999999998002 ) ;
#16243 = AXIS2_PLACEMENT_3D ( 'NONE', #202019, #143315, #44236 ) ;
#16244 = EDGE_LOOP ( 'NONE', ( #61321, #223840 ) ) ;
#16245 = DIRECTION ( 'NONE',  ( 0.000000000000000000, 7.026728003956695223E-15, -1.000000000000000000 ) ) ;
#16247 = CIRCLE ( 'NONE', #249470, 0.1000000000000028644 ) ;
#16246 = CARTESIAN_POINT ( 'NONE',  ( 20.85000000000000142, -11.74999999998883560, -197.9999999999999432 ) ) ;
#16248 = DIRECTION ( 'NONE',  ( 0.000000000000000000, -0.4999999999999543698, -0.8660254037844650199 ) ) ;
#16250 = VERTEX_POINT ( 'NONE', #160811 ) ;
#16249 = DIRECTION ( 'NONE',  ( -0.000000000000000000, -0.1350103645451718737, 0.9908441862701622416 ) ) ;
#16251 = ADVANCED_FACE ( 'NONE', ( #114606 ), #208891, .F. ) ;
#16253 = EDGE_LOOP ( 'NONE', ( #125426, #79208, #58829, #247057 ) ) ;
#16252 = CARTESIAN_POINT ( 'NONE',  ( -18.44204374631839016, 85.49103638961018703, -96.39690621430322892 ) ) ;
#16254 = TOROIDAL_SURFACE ( 'NONE', #162008, 11.65000000000000036, 0.1000000000000000056 ) ;
#16255 = DIRECTION ( 'NONE',  ( -1.000000000000000000, 0.000000000000000000, 0.000000000000000000 ) ) ;
#16256 = FACE_OUTER_BOUND ( 'NONE', #186281, .T. ) ;
#16257 = CARTESIAN_POINT ( 'NONE',  ( -20.85000000000000142, 75.83895117929318985, -103.3072973288845162 ) ) ;
#16258 = ADVANCED_FACE ( 'NONE', ( #194164 ), #248013, .F. ) ;
#16259 = CIRCLE ( 'NONE', #228637, 0.1999999999999996503 ) ;
#16260 = LINE ( 'NONE', #71088, #10907 ) ;
#16262 = DIRECTION ( 'NONE',  ( 0.000000000000000000, -0.2128009952263403282, 0.9770955615653358350 ) ) ;
#16261 = CARTESIAN_POINT ( 'NONE',  ( -16.97683810757273193, 9.950000000011137047, -154.2364232875389121 ) ) ;
#16263 = CARTESIAN_POINT ( 'NONE',  ( 23.14999999999999503, 64.35000000001156195, -57.37310748452439668 ) ) ;
#16264 = AXIS2_PLACEMENT_3D ( 'NONE', #16689, #217414, #136598 ) ;
#16266 = EDGE_CURVE ( 'NONE', #118818, #144465, #119772, .T. ) ;
#16265 = DIRECTION ( 'NONE',  ( 0.000000000000000000, 0.9868171638914216004, -0.1618390714546136255 ) ) ;
#16267 = FACE_OUTER_BOUND ( 'NONE', #242984, .T. ) ;
#16268 = FACE_OUTER_BOUND ( 'NONE', #93488, .T. ) ;
#16270 = VERTEX_POINT ( 'NONE', #108507 ) ;
#16269 = AXIS2_PLACEMENT_3D ( 'NONE', #254789, #132323, #112770 ) ;
#16271 = FACE_OUTER_BOUND ( 'NONE', #82687, .T. ) ;
#16272 = VERTEX_POINT ( 'NONE', #249323 ) ;
#16273 = VERTEX_POINT ( 'NONE', #9400 ) ;
#16274 = DIRECTION ( 'NONE',  ( 1.000000000000000000, -0.000000000000000000, 0.000000000000000000 ) ) ;
#16275 = DIRECTION ( 'NONE',  ( 1.000000000000000000, -2.952720810173289112E-16, -2.061873921506763405E-30 ) ) ;
#16276 = ORIENTED_EDGE ( 'NONE', *, *, #33190, .F. ) ;
#16277 = ADVANCED_FACE ( 'NONE', ( #88929 ), #35112, .F. ) ;
#16278 = CIRCLE ( 'NONE', #20366, 0.2000000000000057288 ) ;
#16279 = ORIENTED_EDGE ( 'NONE', *, *, #47004, .T. ) ;
#16280 = EDGE_CURVE ( 'NONE', #256668, #190582, #10701, .T. ) ;
#16281 = AXIS2_PLACEMENT_3D ( 'NONE', #202487, #122958, #98202 ) ;
#16282 = DIRECTION ( 'NONE',  ( 7.304098846218136639E-16, -0.4721928772777346239, -0.8814952561688430555 ) ) ;
#16283 = VERTEX_POINT ( 'NONE', #228477 ) ;
#16284 = AXIS2_PLACEMENT_3D ( 'NONE', #132962, #33895, #192928 ) ;
#16285 = ORIENTED_EDGE ( 'NONE', *, *, #81549, .T. ) ;
#16286 = CARTESIAN_POINT ( 'NONE',  ( 21.14999999999999858, 76.00000000001195133, -102.9231074845243228 ) ) ;
#16287 = DIRECTION ( 'NONE',  ( 0.000000000000000000, 0.000000000000000000, -1.000000000000000000 ) ) ;
#16288 = DIRECTION ( 'NONE',  ( -1.000000000000000000, -0.000000000000000000, -0.000000000000000000 ) ) ;
#16289 = CYLINDRICAL_SURFACE ( 'NONE', #174158, 0.1000000000000013933 ) ;
#16290 = CYLINDRICAL_SURFACE ( 'NONE', #144168, 0.09999999999999939493 ) ;
#16291 = B_SPLINE_CURVE_WITH_KNOTS ( 'NONE', 3,
 ( #114265, #54278, #133823, #213349, #36028, #178110, #196361, #17710, #176824, #256266, #173002, #234196, #212099, #135091, #19004, #38582 ),
 .UNSPECIFIED., .F., .F.,
 ( 4, 3, 3, 3, 3, 4 ),
 ( 0.000000000000000000, 2.209833635978134735E-05, 5.595056164119275948E-05, 8.979992002655095445E-05, 0.0001236482757198940658, 0.0001574984039362993960 ),
 .UNSPECIFIED. ) ;
#16292 = ADVANCED_FACE ( 'NONE', ( #90206 ), #245472, .T. ) ;
#16294 = DIRECTION ( 'NONE',  ( 0.000000000000000000, -6.982962677686266711E-15, 1.000000000000000000 ) ) ;
#16293 = CARTESIAN_POINT ( 'NONE',  ( 24.30000000000000071, -12.79999999999999716, -347.0000000000001137 ) ) ;
#16295 = CARTESIAN_POINT ( 'NONE',  ( -18.60000000000000142, -8.250000000000005329, 32.89999999999999858 ) ) ;
#16297 = ORIENTED_EDGE ( 'NONE', *, *, #223502, .T. ) ;
#16296 = CARTESIAN_POINT ( 'NONE',  ( 20.85000000000000142, 11.75000000001115907, -194.2161343370218560 ) ) ;
#16299 = FACE_OUTER_BOUND ( 'NONE', #8718, .T. ) ;
#16298 = DIRECTION ( 'NONE',  ( 0.000000000000000000, 0.2617529984165030688, 0.9651348961777158619 ) ) ;
#16300 = ORIENTED_EDGE ( 'NONE', *, *, #134881, .F. ) ;
#16301 = FACE_OUTER_BOUND ( 'NONE', #107670, .T. ) ;
#16302 = CARTESIAN_POINT ( 'NONE',  ( 20.94999999999999929, 6.450000000011156587, -177.5170271704400022 ) ) ;
#16303 = EDGE_LOOP ( 'NONE', ( #5906, #21744, #142772, #173740 ) ) ;
#16304 = DIRECTION ( 'NONE',  ( 0.000000000000000000, 0.4999999999999949485, -0.8660254037844415942 ) ) ;
#16305 = DIRECTION ( 'NONE',  ( 0.000000000000000000, 0.000000000000000000, -1.000000000000000000 ) ) ;
#16306 = CARTESIAN_POINT ( 'NONE',  ( -22.57320508075687115, 64.25000000001269029, -203.5231074845244166 ) ) ;
#16307 = ORIENTED_EDGE ( 'NONE', *, *, #24830, .F. ) ;
#16308 = ORIENTED_EDGE ( 'NONE', *, *, #90460, .T. ) ;
#16309 = CYLINDRICAL_SURFACE ( 'NONE', #203337, 0.5000000000000004441 ) ;
#16310 = DIRECTION ( 'NONE',  ( -1.073024830501117725E-15, 0.000000000000000000, 1.000000000000000000 ) ) ;
#16311 = DIRECTION ( 'NONE',  ( -0.000000000000000000, -6.982962677686266711E-15, 1.000000000000000000 ) ) ;
#16312 = PLANE ( 'NONE',  #72170 ) ;
#16313 = ORIENTED_EDGE ( 'NONE', *, *, #144072, .F. ) ;
#16314 = CARTESIAN_POINT ( 'NONE',  ( 12.60053434924910754, 47.12508421510193557, -234.5737628866445164 ) ) ;
#16315 = DIRECTION ( 'NONE',  ( 1.000000000000000000, 0.000000000000000000, 0.000000000000000000 ) ) ;
#16316 = DIRECTION ( 'NONE',  ( 1.000000000000000000, 0.000000000000000000, -0.000000000000000000 ) ) ;
#16317 = AXIS2_PLACEMENT_3D ( 'NONE', #153679, #76636, #233183 ) ;
#16318 = CARTESIAN_POINT ( 'NONE',  ( 21.14999999999999858, 11.65000000001116298, -45.75000000000000711 ) ) ;
#16319 = AXIS2_PLACEMENT_3D ( 'NONE', #250629, #190703, #194555 ) ;
#16320 = VECTOR ( 'NONE', #253957, 1000.000000000000000 ) ;
#16321 = DIRECTION ( 'NONE',  ( -1.000000000000000000, -0.000000000000000000, -0.000000000000000000 ) ) ;
#16323 = ORIENTED_EDGE ( 'NONE', *, *, #69135, .F. ) ;
#16322 = FACE_OUTER_BOUND ( 'NONE', #141089, .T. ) ;
#16324 = CIRCLE ( 'NONE', #182912, 6.258578643762710669 ) ;
#16325 = CARTESIAN_POINT ( 'NONE',  ( -20.54999999999999716, 29.19585636832770703, -237.3287400596392445 ) ) ;
#16326 = DIRECTION ( 'NONE',  ( -1.000000000000000000, 2.849773892568378313E-16, -7.728835255496647986E-17 ) ) ;
#16327 = CARTESIAN_POINT ( 'NONE',  ( -12.25000000000000178, 66.15000000001204228, -119.7731074845243739 ) ) ;
#16328 = CARTESIAN_POINT ( 'NONE',  ( -22.50485643085239928, -0.07878633906603056680, -122.2502050608276107 ) ) ;
#16329 = EDGE_CURVE ( 'NONE', #71080, #4663, #123864, .T. ) ;
#16330 = DIRECTION ( 'NONE',  ( 0.000000000000000000, 1.000000000000000000, 0.000000000000000000 ) ) ;
#16332 = ORIENTED_EDGE ( 'NONE', *, *, #43215, .F. ) ;
#16331 = CARTESIAN_POINT ( 'NONE',  ( -20.65000000000000568, 18.70606281991846842, -231.7096448200342138 ) ) ;
#16333 = PLANE ( 'NONE',  #83987 ) ;
#16334 = DIRECTION ( 'NONE',  ( 0.000000000000000000, 0.2128009952263605342, -0.9770955615653315052 ) ) ;
#16335 = FACE_OUTER_BOUND ( 'NONE', #19657, .T. ) ;
#16336 = EDGE_LOOP ( 'NONE', ( #102908, #54971, #189783, #108592 ) ) ;
#16337 = LINE ( 'NONE', #253620, #205137 ) ;
#16338 = CARTESIAN_POINT ( 'NONE',  ( -21.64999999999999858, 7.350000000011155166, -112.8500000000000369 ) ) ;
#16340 = EDGE_CURVE ( 'NONE', #135756, #76729, #148938, .T. ) ;
#16339 = DIRECTION ( 'NONE',  ( 3.469446951953635015E-14, -0.000000000000000000, 1.000000000000000000 ) ) ;
#16341 = VECTOR ( 'NONE', #97586, 999.9999999999998863 ) ;
#16343 = ADVANCED_FACE ( 'NONE', ( #27730 ), #186784, .F. ) ;
#16342 = AXIS2_PLACEMENT_3D ( 'NONE', #176020, #93882, #74364 ) ;
#16344 = DIRECTION ( 'NONE',  ( 0.000000000000000000, 0.000000000000000000, -1.000000000000000000 ) ) ;
#16345 = AXIS2_PLACEMENT_3D ( 'NONE', #170391, #172949, #30856 ) ;
#16346 = CARTESIAN_POINT ( 'NONE',  ( -18.45037301276627062, 78.22618665882693278, -231.5710384046198271 ) ) ;
#16347 = CYLINDRICAL_SURFACE ( 'NONE', #204949, 7.900000000000003908 ) ;
#16348 = AXIS2_PLACEMENT_3D ( 'NONE', #56313, #116322, #118893 ) ;
#16349 = ORIENTED_EDGE ( 'NONE', *, *, #155894, .T. ) ;
#16350 = ORIENTED_EDGE ( 'NONE', *, *, #8978, .F. ) ;
#16351 = DIRECTION ( 'NONE',  ( 1.000000000000000000, 0.000000000000000000, 0.000000000000000000 ) ) ;
#16352 = FACE_OUTER_BOUND ( 'NONE', #198885, .T. ) ;
#16353 = ADVANCED_FACE ( 'NONE', ( #95037 ), #15542, .T. ) ;
#16354 = CARTESIAN_POINT ( 'NONE',  ( -21.14999999999999858, 38.04609728753135300, -236.0545303518866547 ) ) ;
#16355 = DIRECTION ( 'NONE',  ( 0.000000000000000000, 0.000000000000000000, -1.000000000000000000 ) ) ;
#16356 = CARTESIAN_POINT ( 'NONE',  ( 21.05000000000000071, 2.859758780633683273, -208.6670499591424459 ) ) ;
#16357 = CARTESIAN_POINT ( 'NONE',  ( 21.14999999999999858, 11.65000000001115943, -79.15000000000004832 ) ) ;
#16359 = CARTESIAN_POINT ( 'NONE',  ( -17.11825945287481332, 14.25671114421267127, -219.2337924566137701 ) ) ;
#16358 = VECTOR ( 'NONE', #34042, 1000.000000000000000 ) ;
#16360 = ORIENTED_EDGE ( 'NONE', *, *, #252200, .F. ) ;
#16361 = DIRECTION ( 'NONE',  ( 0.000000000000000000, 1.000000000000000000, 0.000000000000000000 ) ) ;
#16362 = EDGE_LOOP ( 'NONE', ( #76648, #148320, #66267, #26139 ) ) ;
#16363 = ORIENTED_EDGE ( 'NONE', *, *, #176559, .F. ) ;
#16364 = ADVANCED_FACE ( 'NONE', ( #87646 ), #109780, .T. ) ;
#16365 = CARTESIAN_POINT ( 'NONE',  ( 23.14999999999999503, 64.35000000001197407, -115.1731074845243796 ) ) ;
#16366 = CARTESIAN_POINT ( 'NONE',  ( -17.04761207306819060, 65.97354912661410253, -90.37310748452436826 ) ) ;
#16367 = EDGE_CURVE ( 'NONE', #120605, #116285, #211346, .T. ) ;
#16368 = CARTESIAN_POINT ( 'NONE',  ( -21.05000000000000071, 1.115600667400684642E-11, -100.5000000000000284 ) ) ;
#16369 = VECTOR ( 'NONE', #222084, 1000.000000000000000 ) ;
#16371 = ORIENTED_EDGE ( 'NONE', *, *, #136060, .T. ) ;
#16370 = DIRECTION ( 'NONE',  ( -4.391705002472929091E-16, 1.000000000000000000, 0.000000000000000000 ) ) ;
#16372 = LINE ( 'NONE', #215809, #94830 ) ;
#16373 = DIRECTION ( 'NONE',  ( -1.000000000000000000, 0.000000000000000000, 0.000000000000000000 ) ) ;
#16374 = FACE_BOUND ( 'NONE', #85381, .T. ) ;
#16375 = ORIENTED_EDGE ( 'NONE', *, *, #67315, .F. ) ;
#16376 = CARTESIAN_POINT ( 'NONE',  ( -20.94999999999999929, 7.021664781900089913, -37.33356540189728889 ) ) ;
#16377 = CARTESIAN_POINT ( 'NONE',  ( 21.87500000000000355, 66.25000000001223555, -148.7731074845244450 ) ) ;
#16378 = DIRECTION ( 'NONE',  ( 0.000000000000000000, -1.000000000000000000, -2.081668171172166936E-15 ) ) ;
#16380 = EDGE_CURVE ( 'NONE', #92030, #216037, #198855, .T. ) ;
#16379 = DIRECTION ( 'NONE',  ( 0.000000000000000000, 6.982962677686266711E-15, -1.000000000000000000 ) ) ;
#16381 = AXIS2_PLACEMENT_3D ( 'NONE', #231492, #110235, #189786 ) ;
#16382 = VECTOR ( 'NONE', #115113, 1000.000000000000000 ) ;
#16383 = CIRCLE ( 'NONE', #107945, 12.97499999999998721 ) ;
#16384 = ORIENTED_EDGE ( 'NONE', *, *, #252970, .F. ) ;
#16385 = CYLINDRICAL_SURFACE ( 'NONE', #218507, 0.5000000000000004441 ) ;
#16386 = DIRECTION ( 'NONE',  ( -1.000000000000000000, 0.000000000000000000, 0.000000000000000000 ) ) ;
#16387 = ORIENTED_EDGE ( 'NONE', *, *, #144772, .T. ) ;
#16388 = DIRECTION ( 'NONE',  ( 1.000000000000000000, -0.000000000000000000, -0.000000000000000000 ) ) ;
#16389 = CARTESIAN_POINT ( 'NONE',  ( 13.40000000000005898, 67.65000000001118963, -21.02310748452479316 ) ) ;
#16390 = CIRCLE ( 'NONE', #20489, 11.75000000000000000 ) ;
#16391 = CIRCLE ( 'NONE', #74682, 0.2000000000000057288 ) ;
#16392 = EDGE_CURVE ( 'NONE', #123238, #85747, #244640, .T. ) ;
#16393 = ORIENTED_EDGE ( 'NONE', *, *, #95399, .F. ) ;
#16394 = LINE ( 'NONE', #230274, #183808 ) ;
#16395 = CARTESIAN_POINT ( 'NONE',  ( -20.64999999999999858, 27.91464654983916205, -239.9322955902566719 ) ) ;
#16396 = ORIENTED_EDGE ( 'NONE', *, *, #102032, .F. ) ;
#16397 = AXIS2_PLACEMENT_3D ( 'NONE', #225329, #205784, #187535 ) ;
#16398 = AXIS2_PLACEMENT_3D ( 'NONE', #10804, #128182, #12109 ) ;
#16399 = CIRCLE ( 'NONE', #249627, 1.999999999999997335 ) ;
#16400 = EDGE_CURVE ( 'NONE', #56290, #38211, #6840, .T. ) ;
#16401 = ORIENTED_EDGE ( 'NONE', *, *, #198553, .F. ) ;
#16402 = CARTESIAN_POINT ( 'NONE',  ( -16.86420534634261514, 9.970615445602874161, -87.91833654923743779 ) ) ;
#16403 = VECTOR ( 'NONE', #116291, 1000.000000000000000 ) ;
#16404 = LINE ( 'NONE', #249860, #50320 ) ;
#16406 = ORIENTED_EDGE ( 'NONE', *, *, #114079, .F. ) ;
#16405 = CARTESIAN_POINT ( 'NONE',  ( -20.85000000000000497, 11.75000000001115019, -60.08085275404129533 ) ) ;
#16407 = FACE_OUTER_BOUND ( 'NONE', #108730, .T. ) ;
#16408 = CARTESIAN_POINT ( 'NONE',  ( -23.15000000000000213, 5.950000000011163692, -56.69429769496518645 ) ) ;
#16409 = EDGE_CURVE ( 'NONE', #90507, #19078, #153113, .T. ) ;
#16411 = ADVANCED_FACE ( 'NONE', ( #158893 ), #19820, .F. ) ;
#16410 = DIRECTION ( 'NONE',  ( 0.000000000000000000, 0.1575546449569621699, -0.9875102702516493913 ) ) ;
#16412 = DIRECTION ( 'NONE',  ( 0.000000000000000000, -0.8814952561688444987, 0.4721928772777320149 ) ) ;
#16413 = PLANE ( 'NONE',  #145898 ) ;
#16414 = CARTESIAN_POINT ( 'NONE',  ( 18.59999999999999076, 64.25000000001263345, -195.4231074845244223 ) ) ;
#16415 = CARTESIAN_POINT ( 'NONE',  ( 20.94999999999999929, -9.400000000000002132, -9.893969122652443104 ) ) ;
#16417 = ORIENTED_EDGE ( 'NONE', *, *, #24137, .F. ) ;
#16416 = CARTESIAN_POINT ( 'NONE',  ( -23.15000000000000213, 1.115600667400684642E-11, -54.12500000000000711 ) ) ;
#16419 = ORIENTED_EDGE ( 'NONE', *, *, #200332, .F. ) ;
#16418 = CARTESIAN_POINT ( 'NONE',  ( 21.05000000000000071, 53.86595165227826243, -236.3638196928718855 ) ) ;
#16421 = CARTESIAN_POINT ( 'NONE',  ( 20.85882249326303040, 10.33248238083634796, -72.59484654391314962 ) ) ;
#16420 = DIRECTION ( 'NONE',  ( -1.000000000000000000, 0.000000000000000000, 0.000000000000000000 ) ) ;
#16423 = ORIENTED_EDGE ( 'NONE', *, *, #137323, .T. ) ;
#16422 = DIRECTION ( 'NONE',  ( 0.000000000000000000, 1.000000000000000000, 6.853228547068871147E-15 ) ) ;
#16424 = ORIENTED_EDGE ( 'NONE', *, *, #102616, .T. ) ;
#16425 = CARTESIAN_POINT ( 'NONE',  ( -18.59999999999999787, 10.33248238083634440, -106.0948465439131922 ) ) ;
#16426 = CIRCLE ( 'NONE', #116375, 11.65000000000000036 ) ;
#16427 = DIRECTION ( 'NONE',  ( 0.000000000000000000, 7.026728003956683390E-15, -1.000000000000000000 ) ) ;
#16428 = ADVANCED_FACE ( 'NONE', ( #200557 ), #156334, .T. ) ;
#16429 = EDGE_CURVE ( 'NONE', #156170, #173939, #232211, .T. ) ;
#16430 = DIRECTION ( 'NONE',  ( 1.000000000000000000, 0.000000000000000000, 0.000000000000000000 ) ) ;
#16431 = CARTESIAN_POINT ( 'NONE',  ( 19.96984138294285671, 11.75000000001126921, -58.22457207120090317 ) ) ;
#16432 = CARTESIAN_POINT ( 'NONE',  ( 23.14999999999999858, 69.35000000001259934, -191.1731074845243938 ) ) ;
#16433 = EDGE_CURVE ( 'NONE', #254080, #162811, #20659, .T. ) ;
#16434 = DIRECTION ( 'NONE',  ( 1.000000000000000000, 0.000000000000000000, 0.000000000000000000 ) ) ;
#16435 = AXIS2_PLACEMENT_3D ( 'NONE', #195715, #256888, #178729 ) ;
#16436 = CARTESIAN_POINT ( 'NONE',  ( -16.81744102076748959, 66.05000000001201954, -115.6731074845243796 ) ) ;
#16438 = ORIENTED_EDGE ( 'NONE', *, *, #95705, .T. ) ;
#16437 = EDGE_CURVE ( 'NONE', #75563, #62135, #102986, .T. ) ;
#16439 = VERTEX_POINT ( 'NONE', #160179 ) ;
#16440 = CARTESIAN_POINT ( 'NONE',  ( 21.15000000000000213, 30.68987205111127281, -252.2252246220829193 ) ) ;
#16441 = ORIENTED_EDGE ( 'NONE', *, *, #217433, .F. ) ;
#16442 = EDGE_CURVE ( 'NONE', #56972, #196513, #115898, .T. ) ;
#16443 = ADVANCED_FACE ( 'NONE', ( #155051 ), #186410, .F. ) ;
#16444 = CARTESIAN_POINT ( 'NONE',  ( -20.64999999999999858, -9.499999999988848032, -110.3939691226524786 ) ) ;
#16445 = AXIS2_PLACEMENT_3D ( 'NONE', #6937, #225953, #86443 ) ;
#16446 = DIRECTION ( 'NONE',  ( 1.000000000000000000, 0.000000000000000000, 0.000000000000000000 ) ) ;
#16447 = CARTESIAN_POINT ( 'NONE',  ( -22.47007471830798764, -1.642974910573230973, -193.4561278898739545 ) ) ;
#16448 = EDGE_CURVE ( 'NONE', #150904, #174607, #78042, .T. ) ;
#16449 = ORIENTED_EDGE ( 'NONE', *, *, #91654, .T. ) ;
#16450 = CARTESIAN_POINT ( 'NONE',  ( 21.05000000000000071, 70.15000000001266756, -193.3906102602464330 ) ) ;
#16451 = ORIENTED_EDGE ( 'NONE', *, *, #36735, .T. ) ;
#16452 = DIRECTION ( 'NONE',  ( 1.000000000000000000, -0.000000000000000000, -0.000000000000000000 ) ) ;
#16453 = EDGE_LOOP ( 'NONE', ( #1931, #209899, #186178 ) ) ;
#16454 = EDGE_CURVE ( 'NONE', #87552, #12088, #135438, .T. ) ;
#16455 = CIRCLE ( 'NONE', #58097, 0.1000000000000015737 ) ;
#16456 = DIRECTION ( 'NONE',  ( 1.000000000000000000, 0.000000000000000000, 0.000000000000000000 ) ) ;
#16457 = ADVANCED_FACE ( 'NONE', ( #19360 ), #61035, .F. ) ;
#16458 = DIRECTION ( 'NONE',  ( -0.7071067811865388020, 0.7071067811865561215, 0.000000000000000000 ) ) ;
#16459 = AXIS2_PLACEMENT_3D ( 'NONE', #95377, #113650, #212769 ) ;
#16460 = DIRECTION ( 'NONE',  ( 0.000000000000000000, -0.000000000000000000, 1.000000000000000000 ) ) ;
#16462 = ORIENTED_EDGE ( 'NONE', *, *, #48738, .F. ) ;
#16461 = EDGE_CURVE ( 'NONE', #50256, #172993, #194617, .T. ) ;
#16463 = FACE_OUTER_BOUND ( 'NONE', #53296, .T. ) ;
#16464 = EDGE_LOOP ( 'NONE', ( #23261, #47620, #205130, #248786 ) ) ;
#16465 = CARTESIAN_POINT ( 'NONE',  ( 23.14999999999998437, 78.57160958314655375, -238.9307242378722833 ) ) ;
#16466 = CIRCLE ( 'NONE', #162031, 0.09999999999999939493 ) ;
#16467 = ORIENTED_EDGE ( 'NONE', *, *, #130630, .F. ) ;
#16468 = VERTEX_POINT ( 'NONE', #18064 ) ;
#16469 = DIRECTION ( 'NONE',  ( 0.000000000000000000, 0.000000000000000000, -1.000000000000000000 ) ) ;
#16470 = VERTEX_POINT ( 'NONE', #139276 ) ;
#16471 = ADVANCED_FACE ( 'NONE', ( #58454 ), #57170, .F. ) ;
#16472 = CARTESIAN_POINT ( 'NONE',  ( 20.94999999999999929, 6.650000000011155876, -79.15000000000004832 ) ) ;
#16473 = CYLINDRICAL_SURFACE ( 'NONE', #92803, 0.1000000000000028644 ) ;
#16474 = DIRECTION ( 'NONE',  ( 1.000000000000000000, -0.000000000000000000, -0.000000000000000000 ) ) ;
#16475 = CARTESIAN_POINT ( 'NONE',  ( 21.05000000000005400, 66.15000000001120384, -5.923107484524795296 ) ) ;
#16476 = CARTESIAN_POINT ( 'NONE',  ( -21.07933241753356413, 0.09337959043042065588, -60.67135405162031248 ) ) ;
#16477 = ORIENTED_EDGE ( 'NONE', *, *, #52348, .T. ) ;
#16478 = FACE_OUTER_BOUND ( 'NONE', #41857, .T. ) ;
#16479 = CARTESIAN_POINT ( 'NONE',  ( 21.05000000000000071, 8.876614585098254295, -175.8850804788446567 ) ) ;
#16480 = CARTESIAN_POINT ( 'NONE',  ( -20.85000000106584750, 11.75000000001115197, -160.6555046564734539 ) ) ;
#16481 = EDGE_LOOP ( 'NONE', ( #117317, #241452, #143571, #86998 ) ) ;
#16482 = DIRECTION ( 'NONE',  ( 0.000000000000000000, 1.000000000000000000, 0.000000000000000000 ) ) ;
#16483 = EDGE_LOOP ( 'NONE', ( #223056, #107679, #130941, #176405 ) ) ;
#16484 = DIRECTION ( 'NONE',  ( -1.000000000000000000, 0.000000000000000000, 0.000000000000000000 ) ) ;
#16485 = ORIENTED_EDGE ( 'NONE', *, *, #243562, .F. ) ;
#16486 = CARTESIAN_POINT ( 'NONE',  ( 18.59999999999999076, 65.79142135624930177, -115.2731074845243597 ) ) ;
#16487 = LINE ( 'NONE', #255006, #131221 ) ;
#16489 = ORIENTED_EDGE ( 'NONE', *, *, #152020, .T. ) ;
#16488 = CARTESIAN_POINT ( 'NONE',  ( -18.50000000000000000, 85.40000000001209912, -129.2258477248609552 ) ) ;
#16490 = CARTESIAN_POINT ( 'NONE',  ( -18.47079683080355750, 8.922807857279824617, -245.4386816022545190 ) ) ;
#16491 = ORIENTED_EDGE ( 'NONE', *, *, #251691, .F. ) ;
#16492 = CARTESIAN_POINT ( 'NONE',  ( 23.14999999999999503, 11.65000000001116298, -146.1500000000000341 ) ) ;
#16493 = CARTESIAN_POINT ( 'NONE',  ( -20.64999999999999858, 4.350000000011156054, -146.3500000000000227 ) ) ;
#16494 = VERTEX_POINT ( 'NONE', #175886 ) ;
#16495 = EDGE_CURVE ( 'NONE', #239369, #64016, #144867, .T. ) ;
#16496 = LINE ( 'NONE', #76438, #239223 ) ;
#16497 = CYLINDRICAL_SURFACE ( 'NONE', #98496, 0.1000000000000098310 ) ;
#16498 = VERTEX_POINT ( 'NONE', #40233 ) ;
#16499 = AXIS2_PLACEMENT_3D ( 'NONE', #176713, #77564, #141413 ) ;
#16501 = DIRECTION ( 'NONE',  ( 1.000000000000000000, 0.000000000000000000, 0.000000000000000000 ) ) ;
#16500 = TOROIDAL_SURFACE ( 'NONE', #203916, 0.9750000000000019762, 0.1000000000000000056 ) ;
#16502 = EDGE_CURVE ( 'NONE', #124577, #144086, #51763, .T. ) ;
#16503 = VERTEX_POINT ( 'NONE', #140575 ) ;
#16504 = DIRECTION ( 'NONE',  ( 0.000000000000000000, -0.9908441862701596881, 0.1350103645451904977 ) ) ;
#16505 = CIRCLE ( 'NONE', #253793, 7.900000000000003908 ) ;
#16506 = DIRECTION ( 'NONE',  ( -1.000000000000000000, -0.000000000000000000, -0.000000000000000000 ) ) ;
#16508 = EDGE_LOOP ( 'NONE', ( #246935, #73339, #81065, #98287 ) ) ;
#16507 = CARTESIAN_POINT ( 'NONE',  ( 21.14999999999999858, 6.550000000011156231, -112.8500000000000369 ) ) ;
#16509 = DIRECTION ( 'NONE',  ( 1.000000000000000000, 0.000000000000000000, 0.000000000000000000 ) ) ;
#16510 = CIRCLE ( 'NONE', #245467, 0.1000000000000001305 ) ;
#16511 = DIRECTION ( 'NONE',  ( 0.000000000000000000, -0.9126074666063622720, -0.4088369013363611360 ) ) ;
#16512 = CARTESIAN_POINT ( 'NONE',  ( -16.93826681692523195, 10.01142872028771258, -20.94545846735944039 ) ) ;
#16513 = AXIS2_PLACEMENT_3D ( 'NONE', #6470, #166877, #127721 ) ;
#16514 = CARTESIAN_POINT ( 'NONE',  ( -22.47120815636973745, 75.97109617810856719, -181.6730394732778393 ) ) ;
#16516 = EDGE_CURVE ( 'NONE', #108350, #169542, #161460, .T. ) ;
#16515 = DIRECTION ( 'NONE',  ( -1.000000000000000000, -1.646408749285562691E-14, 1.073024830501117725E-15 ) ) ;
#16517 = SPHERICAL_SURFACE ( 'NONE', #90130, 0.1000000000000000056 ) ;
#16518 = LINE ( 'NONE', #154750, #218259 ) ;
#16519 = DIRECTION ( 'NONE',  ( 0.000000000000000000, 0.000000000000000000, -1.000000000000000000 ) ) ;
#16520 = AXIS2_PLACEMENT_3D ( 'NONE', #246518, #251661, #197774 ) ;
#16521 = VERTEX_POINT ( 'NONE', #223957 ) ;
#16522 = EDGE_LOOP ( 'NONE', ( #223656, #245540, #197763, #150986 ) ) ;
#16523 = CARTESIAN_POINT ( 'NONE',  ( 18.50000000000000355, 85.41920976342157701, -162.7753380217652648 ) ) ;
#16525 = VERTEX_POINT ( 'NONE', #67461 ) ;
#16524 = CARTESIAN_POINT ( 'NONE',  ( -20.85000000000000142, 64.25000000001196554, -109.8647081744214375 ) ) ;
#16526 = ORIENTED_EDGE ( 'NONE', *, *, #48219, .T. ) ;
#16527 = CARTESIAN_POINT ( 'NONE',  ( -18.38817693311004575, 64.51850848411275763, -179.2731074845244450 ) ) ;
#16528 = ORIENTED_EDGE ( 'NONE', *, *, #197824, .F. ) ;
#16529 = CARTESIAN_POINT ( 'NONE',  ( 20.95443524775735256, 8.878554263872812768, -8.533722275600151619 ) ) ;
#16530 = ORIENTED_EDGE ( 'NONE', *, *, #155408, .T. ) ;
#16531 = DIRECTION ( 'NONE',  ( 1.000000000000000000, 0.000000000000000000, 0.000000000000000000 ) ) ;
#16532 = DIRECTION ( 'NONE',  ( 1.000000000000000000, 0.000000000000000000, 0.000000000000000000 ) ) ;
#16533 = AXIS2_PLACEMENT_3D ( 'NONE', #57394, #97791, #136947 ) ;
#16535 = ORIENTED_EDGE ( 'NONE', *, *, #166951, .F. ) ;
#16534 = ORIENTED_EDGE ( 'NONE', *, *, #106157, .F. ) ;
#16536 = VERTEX_POINT ( 'NONE', #102711 ) ;
#16537 = VERTEX_POINT ( 'NONE', #103994 ) ;
#16538 = ORIENTED_EDGE ( 'NONE', *, *, #104654, .T. ) ;
#16539 = DIRECTION ( 'NONE',  ( -1.000000000000000000, 0.000000000000000000, 0.000000000000000000 ) ) ;
#16540 = CARTESIAN_POINT ( 'NONE',  ( -23.15000000000000213, 4.349999999999999645, -12.25000000000000000 ) ) ;
#16542 = ORIENTED_EDGE ( 'NONE', *, *, #77576, .F. ) ;
#16541 = DIRECTION ( 'NONE',  ( 1.000000000000000000, 0.000000000000000000, 0.000000000000000000 ) ) ;
#16543 = AXIS2_PLACEMENT_3D ( 'NONE', #125581, #145129, #160879 ) ;
#16544 = CARTESIAN_POINT ( 'NONE',  ( -18.50000000000000000, 74.83729825007408465, -128.4231074845243086 ) ) ;
#16545 = CARTESIAN_POINT ( 'NONE',  ( 13.76927104934457624, 12.43387192838033251, -213.6554569813165472 ) ) ;
#16547 = ORIENTED_EDGE ( 'NONE', *, *, #185462, .T. ) ;
#16546 = CARTESIAN_POINT ( 'NONE',  ( -21.05000000000000071, -11.64999999998884483, -134.0000000000000000 ) ) ;
#16548 = DIRECTION ( 'NONE',  ( 1.000000000000000000, 0.000000000000000000, 0.000000000000000000 ) ) ;
#16549 = VERTEX_POINT ( 'NONE', #45336 ) ;
#16550 = DIRECTION ( 'NONE',  ( 1.000000000000000000, 0.000000000000000000, 0.000000000000000000 ) ) ;
#16551 = EDGE_CURVE ( 'NONE', #115457, #174034, #186596, .T. ) ;
#16552 = EDGE_LOOP ( 'NONE', ( #20389, #53373, #223723, #69689 ) ) ;
#16553 = DIRECTION ( 'NONE',  ( 0.000000000000000000, 0.8814952561688476074, -0.4721928772777262417 ) ) ;
#16554 = DIRECTION ( 'NONE',  ( 0.000000000000000000, 6.982962677686267499E-15, -1.000000000000000000 ) ) ;
#16555 = ADVANCED_FACE ( 'NONE', ( #201841 ), #2338, .T. ) ;
#16556 = CARTESIAN_POINT ( 'NONE',  ( -20.54999999999999716, 76.00000000001192291, -105.0231074845243029 ) ) ;
#16557 = ORIENTED_EDGE ( 'NONE', *, *, #128949, .T. ) ;
#16559 = DIRECTION ( 'NONE',  ( 0.000000000000000000, 1.000000000000000000, 0.000000000000000000 ) ) ;
#16558 = FACE_OUTER_BOUND ( 'NONE', #41911, .T. ) ;
#16560 = VECTOR ( 'NONE', #235069, 1000.000000000000000 ) ;
#16561 = CARTESIAN_POINT ( 'NONE',  ( 18.39999999999999858, 85.50000000001242029, -163.1009576351939643 ) ) ;
#16562 = DIRECTION ( 'NONE',  ( 0.000000000000000000, 1.000000000000000000, 6.982962677686266711E-15 ) ) ;
#16563 = DIRECTION ( 'NONE',  ( 1.000000000000000000, 0.000000000000000000, 0.000000000000000000 ) ) ;
#16564 = AXIS2_PLACEMENT_3D ( 'NONE', #82394, #43312, #122853 ) ;
#16565 = ORIENTED_EDGE ( 'NONE', *, *, #69648, .T. ) ;
#16566 = ORIENTED_EDGE ( 'NONE', *, *, #139765, .T. ) ;
#16567 = ADVANCED_FACE ( 'NONE', ( #124878 ), #171637, .F. ) ;
#16568 = CARTESIAN_POINT ( 'NONE',  ( 20.95263205890667635, 8.895740107894022586, -8.489508406941629559 ) ) ;
#16569 = CARTESIAN_POINT ( 'NONE',  ( -18.40000000000000213, 62.49259387941005173, -209.4439336506227960 ) ) ;
#16570 = VERTEX_POINT ( 'NONE', #186131 ) ;
#16572 = DIRECTION ( 'NONE',  ( 1.000000000000000000, 0.000000000000000000, 0.000000000000000000 ) ) ;
#16571 = AXIS2_PLACEMENT_3D ( 'NONE', #231489, #32014, #30736 ) ;
#16573 = ORIENTED_EDGE ( 'NONE', *, *, #118486, .T. ) ;
#16574 = DIRECTION ( 'NONE',  ( 0.000000000000000000, -0.7071067811865477948, -0.7071067811865473507 ) ) ;
#16575 = CARTESIAN_POINT ( 'NONE',  ( 20.94999999999999929, 70.60000000001180354, -81.92837350343744163 ) ) ;
#16576 = EDGE_CURVE ( 'NONE', #39159, #100102, #174148, .T. ) ;
#16577 = AXIS2_PLACEMENT_3D ( 'NONE', #229556, #105710, #185286 ) ;
#16578 = EDGE_CURVE ( 'NONE', #171633, #169815, #136479, .T. ) ;
#16579 = CIRCLE ( 'NONE', #187269, 0.09999999999998898659 ) ;
#16580 = ORIENTED_EDGE ( 'NONE', *, *, #146163, .T. ) ;
#16581 = ADVANCED_FACE ( 'NONE', ( #25777 ), #141860, .F. ) ;
#16582 = CARTESIAN_POINT ( 'NONE',  ( -22.94999999999999929, -1.901609089591594692, -11.59510167572422112 ) ) ;
#16583 = FILL_AREA_STYLE ('',( #76524 ) ) ;
#16585 = ORIENTED_EDGE ( 'NONE', *, *, #123296, .T. ) ;
#16584 = VECTOR ( 'NONE', #232761, 999.9999999999998863 ) ;
#16586 = VERTEX_POINT ( 'NONE', #84408 ) ;
#16587 = VECTOR ( 'NONE', #149468, 1000.000000000000000 ) ;
#16588 = VECTOR ( 'NONE', #48631, 1000.000000000000000 ) ;
#16589 = EDGE_LOOP ( 'NONE', ( #73188, #126947, #76049, #228109 ) ) ;
#16590 = CIRCLE ( 'NONE', #45790, 0.1000000000000008799 ) ;
#16591 = VECTOR ( 'NONE', #92388, 1000.000000000000000 ) ;
#16592 = CARTESIAN_POINT ( 'NONE',  ( 21.05000000000000071, 7.872214528623318053, -209.6555322433423783 ) ) ;
#16593 = DIRECTION ( 'NONE',  ( -1.000000000000000000, 0.000000000000000000, -0.000000000000000000 ) ) ;
#16594 = DIRECTION ( 'NONE',  ( 1.476360405086644309E-16, 1.000000000000000000, 0.000000000000000000 ) ) ;
#16595 = CYLINDRICAL_SURFACE ( 'NONE', #28215, 0.09999999999999939493 ) ;
#16596 = CARTESIAN_POINT ( 'NONE',  ( 13.77030915526558630, 66.54399267394271078, -118.0344739903776201 ) ) ;
#16597 = AXIS2_PLACEMENT_3D ( 'NONE', #178212, #80330, #158649 ) ;
#16598 = ADVANCED_FACE ( 'NONE', ( #7488 ), #68045, .T. ) ;
#16600 = CYLINDRICAL_SURFACE ( 'NONE', #244926, 0.1000000000000052097 ) ;
#16599 = CARTESIAN_POINT ( 'NONE',  ( 21.05000000000000071, -0.09999993529482809063, -161.0219217789056643 ) ) ;
#16602 = ORIENTED_EDGE ( 'NONE', *, *, #166306, .T. ) ;
#16601 = CARTESIAN_POINT ( 'NONE',  ( -21.05000000000000071, 1.835341550235567887, -179.0551512925629538 ) ) ;
#16603 = CARTESIAN_POINT ( 'NONE',  ( -16.86337532320262156, 9.979967204235514089, -79.55107553101724704 ) ) ;
#16604 = VERTEX_POINT ( 'NONE', #126139 ) ;
#16605 = CARTESIAN_POINT ( 'NONE',  ( -20.94999999999999929, 43.17747518314619271, -245.0773422074893233 ) ) ;
#16606 = ORIENTED_EDGE ( 'NONE', *, *, #92327, .F. ) ;
#16607 = ORIENTED_EDGE ( 'NONE', *, *, #163865, .F. ) ;
#16608 = DIRECTION ( 'NONE',  ( 2.557131231893037478E-16, 0.8660254037844420383, -0.4999999999999942824 ) ) ;
#16609 = CARTESIAN_POINT ( 'NONE',  ( -21.07954640115340439, 6.329287696035428290, -133.9339922928604381 ) ) ;
#16610 = DIRECTION ( 'NONE',  ( 0.000000000000000000, 0.2617529984165174461, 0.9651348961777118651 ) ) ;
#16611 = CARTESIAN_POINT ( 'NONE',  ( 21.05000000000000071, 82.20113918088273408, -215.0418453737790401 ) ) ;
#16612 = VERTEX_POINT ( 'NONE', #206980 ) ;
#16613 = VERTEX_POINT ( 'NONE', #183571 ) ;
#16614 = CARTESIAN_POINT ( 'NONE',  ( -18.50000000000000000, 13.56015509305096778, -219.7948714774209691 ) ) ;
#16615 = ORIENTED_EDGE ( 'NONE', *, *, #78435, .F. ) ;
#16616 = FACE_OUTER_BOUND ( 'NONE', #31292, .T. ) ;
#16617 = ORIENTED_EDGE ( 'NONE', *, *, #81161, .T. ) ;
#16618 = CARTESIAN_POINT ( 'NONE',  ( 18.59999999999998366, 1.115600667400684642E-11, -167.5000000000000284 ) ) ;
#16619 = DIRECTION ( 'NONE',  ( 0.000000000000000000, -0.8660254037844412611, -0.4999999999999956701 ) ) ;
#16620 = DIRECTION ( 'NONE',  ( 0.000000000000000000, 0.8814952561688438326, -0.4721928772777331806 ) ) ;
#16621 = ORIENTED_EDGE ( 'NONE', *, *, #130522, .F. ) ;
#16622 = AXIS2_PLACEMENT_3D ( 'NONE', #119703, #141804, #25721 ) ;
#16623 = CARTESIAN_POINT ( 'NONE',  ( 18.59999999999999432, 74.73788286442776041, -233.7359682632885267 ) ) ;
#16624 = LINE ( 'NONE', #248814, #253801 ) ;
#16625 = VECTOR ( 'NONE', #3954, 1000.000000000000000 ) ;
#16626 = DIRECTION ( 'NONE',  ( 1.000000000000000000, 0.000000000000000000, 0.000000000000000000 ) ) ;
#16627 = TOROIDAL_SURFACE ( 'NONE', #199967, 0.6000000000000009770, 0.1000000000000000056 ) ;
#16628 = EDGE_CURVE ( 'NONE', #143978, #107290, #229153, .T. ) ;
#16629 = EDGE_LOOP ( 'NONE', ( #27848, #257461, #225904, #257985, #152776, #54003, #243282 ) ) ;
#16630 = CARTESIAN_POINT ( 'NONE',  ( 21.06089410995832623, 10.72529553212358699, -12.20238073104318488 ) ) ;
#16631 = EDGE_LOOP ( 'NONE', ( #167766, #53895, #154128, #3294 ) ) ;
#16632 = CYLINDRICAL_SURFACE ( 'NONE', #39152, 0.1000000000000013933 ) ;
#16633 = EDGE_CURVE ( 'NONE', #1479, #116380, #204196, .T. ) ;
#16634 = DIRECTION ( 'NONE',  ( 1.000000000000000000, 0.000000000000000000, 0.000000000000000000 ) ) ;
#16635 = CARTESIAN_POINT ( 'NONE',  ( -21.55000000000000071, 68.65000000001157332, -57.27310748452437394 ) ) ;
#16636 = CARTESIAN_POINT ( 'NONE',  ( -16.92778301347281911, 10.00094491684643927, -46.07148189203164890 ) ) ;
#16637 = DIRECTION ( 'NONE',  ( 0.000000000000000000, -1.000000000000000000, 0.000000000000000000 ) ) ;
#16638 = CIRCLE ( 'NONE', #54025, 0.09999999999999824307 ) ;
#16639 = ORIENTED_EDGE ( 'NONE', *, *, #87554, .T. ) ;
#16640 = CARTESIAN_POINT ( 'NONE',  ( -16.94062896051973865, 66.00728089491138917, -123.9205909424055676 ) ) ;
#16641 = CARTESIAN_POINT ( 'NONE',  ( 21.07199075132371746, 67.22505500089597774, -124.3095753229114990 ) ) ;
#16642 = ADVANCED_FACE ( 'NONE', ( #70063 ), #128135, .F. ) ;
#16643 = EDGE_CURVE ( 'NONE', #56828, #70573, #24107, .T. ) ;
#16644 = CARTESIAN_POINT ( 'NONE',  ( -18.50000000000000000, 13.98997548377051459, -210.4902890347897255 ) ) ;
#16645 = FACE_OUTER_BOUND ( 'NONE', #105945, .T. ) ;
#16646 = AXIS2_PLACEMENT_3D ( 'NONE', #138683, #14943, #34515 ) ;
#16647 = FACE_OUTER_BOUND ( 'NONE', #38562, .T. ) ;
#16648 = ORIENTED_EDGE ( 'NONE', *, *, #9094, .T. ) ;
#16649 = ORIENTED_EDGE ( 'NONE', *, *, #234861, .T. ) ;
#16650 = FACE_OUTER_BOUND ( 'NONE', #194230, .T. ) ;
#16651 = CARTESIAN_POINT ( 'NONE',  ( 18.39999999999999858, 85.60000000001210196, -129.9229180933022576 ) ) ;
#16652 = CARTESIAN_POINT ( 'NONE',  ( -21.05000000000000071, 69.74218538953657287, -203.6208977758331855 ) ) ;
#16653 = DIRECTION ( 'NONE',  ( 0.000000000000000000, 0.000000000000000000, -1.000000000000000000 ) ) ;
#16654 = EDGE_CURVE ( 'NONE', #164486, #1095, #207440, .T. ) ;
#16655 =( BOUNDED_CURVE ( )  B_SPLINE_CURVE ( 3, ( #170939, #32705, #250412, #112217 ),
 .UNSPECIFIED., .F., .F. ) 
 B_SPLINE_CURVE_WITH_KNOTS ( ( 4, 4 ),
 ( 4.712388980384686121, 5.672655318024754756 ),
 .UNSPECIFIED. ) 
 CURVE ( )  GEOMETRIC_REPRESENTATION_ITEM ( )  RATIONAL_B_SPLINE_CURVE ( ( 1.000000000000000000, 0.9246222802177250788, 0.9246222802177250788, 1.000000000000000000 ) ) 
 REPRESENTATION_ITEM ( '' )  );
#16656 = EDGE_LOOP ( 'NONE', ( #197056, #93286, #230449, #44137 ) ) ;
#16657 = LINE ( 'NONE', #250122, #184741 ) ;
#16658 = EDGE_CURVE ( 'NONE', #60849, #3474, #73920, .T. ) ;
#16659 = CARTESIAN_POINT ( 'NONE',  ( -21.14999999999999858, 76.00000000001203659, -114.6726782920691221 ) ) ;
#16660 = VERTEX_POINT ( 'NONE', #171738 ) ;
#16661 = DIRECTION ( 'NONE',  ( 0.000000000000000000, 6.982962677686266711E-15, -1.000000000000000000 ) ) ;
#16662 = PRODUCT_RELATED_PRODUCT_CATEGORY ( 'part', '', ( #130599 ) ) ;
#16663 = AXIS2_PLACEMENT_3D ( 'NONE', #163919, #6104, #85618 ) ;
#16664 = CIRCLE ( 'NONE', #133178, 0.09999999999999939493 ) ;
#16665 = DIRECTION ( 'NONE',  ( -1.000000000000000000, -2.952720810173289112E-16, 0.000000000000000000 ) ) ;
#16666 = ORIENTED_EDGE ( 'NONE', *, *, #236088, .F. ) ;
#16668 =( BOUNDED_CURVE ( )  B_SPLINE_CURVE ( 3, ( #211098, #74195, #55838, #75468 ),
 .UNSPECIFIED., .F., .F. ) 
 B_SPLINE_CURVE_WITH_KNOTS ( ( 4, 4 ),
 ( 0.000000000000000000, 1.570796326794908992 ),
 .UNSPECIFIED. ) 
 CURVE ( )  GEOMETRIC_REPRESENTATION_ITEM ( )  RATIONAL_B_SPLINE_CURVE ( ( 1.000000000000000000, 0.8047378541243619399, 0.8047378541243619399, 1.000000000000000000 ) ) 
 REPRESENTATION_ITEM ( '' )  );
#16667 = CARTESIAN_POINT ( 'NONE',  ( 21.05000000000000071, 11.16079915604378492, -211.0041093385139561 ) ) ;
#16669 = EDGE_CURVE ( 'NONE', #129072, #97490, #247373, .T. ) ;
#16670 = ORIENTED_EDGE ( 'NONE', *, *, #48135, .F. ) ;
#16671 = ADVANCED_FACE ( 'NONE', ( #251220 ), #13923, .F. ) ;
#16672 = DIRECTION ( 'NONE',  ( -1.000000000000000000, 0.000000000000000000, 0.000000000000000000 ) ) ;
#16673 = EDGE_CURVE ( 'NONE', #16833, #31671, #148290, .T. ) ;
#16674 = CARTESIAN_POINT ( 'NONE',  ( -20.54999999999999716, 74.00000000001223555, -149.3477294072864652 ) ) ;
#16675 = DIRECTION ( 'NONE',  ( 1.073024830501117725E-15, 0.000000000000000000, 1.000000000000000000 ) ) ;
#16676 = DIRECTION ( 'NONE',  ( 0.000000000000000000, 0.000000000000000000, 1.000000000000000000 ) ) ;
#16677 = DIRECTION ( 'NONE',  ( -1.000000000000000000, -0.000000000000000000, -0.000000000000000000 ) ) ;
#16678 = CARTESIAN_POINT ( 'NONE',  ( 20.94999999999999574, 36.65892442174472876, -249.5511627012454596 ) ) ;
#16679 = DIRECTION ( 'NONE',  ( -0.000000000000000000, 6.982962677686266711E-15, -1.000000000000000000 ) ) ;
#16680 = LINE ( 'NONE', #238265, #137182 ) ;
#16681 = CIRCLE ( 'NONE', #108255, 0.1000000000000000472 ) ;
#16682 = CARTESIAN_POINT ( 'NONE',  ( 21.14999999999999858, 64.35000000001267040, -203.4231074845244507 ) ) ;
#16683 = VECTOR ( 'NONE', #142575, 1000.000000000000227 ) ;
#16684 = LINE ( 'NONE', #214861, #202128 ) ;
#16686 = CARTESIAN_POINT ( 'NONE',  ( -17.01473183483380680, 30.11817903451004952, -234.7598257170722889 ) ) ;
#16685 = CIRCLE ( 'NONE', #83278, 0.1000000000000067224 ) ;
#16687 = CIRCLE ( 'NONE', #33458, 12.87499999999999822 ) ;
#16688 = VERTEX_POINT ( 'NONE', #29657 ) ;
#16689 = CARTESIAN_POINT ( 'NONE',  ( 18.59999999999999076, 11.65000000000000391, -24.85000000000000142 ) ) ;
#16690 = CARTESIAN_POINT ( 'NONE',  ( -23.25000000000000000, 1.115600667400684642E-11, -141.9000000000000341 ) ) ;
#16691 =( BOUNDED_CURVE ( )  B_SPLINE_CURVE ( 3, ( #194758, #249581, #214297, #70966 ),
 .UNSPECIFIED., .F., .F. ) 
 B_SPLINE_CURVE_WITH_KNOTS ( ( 4, 4 ),
 ( 3.432212674861196522, 3.693332928900582068 ),
 .UNSPECIFIED. ) 
 CURVE ( )  GEOMETRIC_REPRESENTATION_ITEM ( )  RATIONAL_B_SPLINE_CURVE ( ( 1.000000000000000000, 0.9943260843901261525, 0.9943260843901261525, 1.000000000000000000 ) ) 
 REPRESENTATION_ITEM ( '' )  );
#16692 = AXIS2_PLACEMENT_3D ( 'NONE', #48054, #105423, #70222 ) ;
#16693 = ORIENTED_EDGE ( 'NONE', *, *, #184880, .T. ) ;
#16694 = CARTESIAN_POINT ( 'NONE',  ( -17.22361732159832215, 63.03919232351000090, -211.7895729146322026 ) ) ;
#16695 = CARTESIAN_POINT ( 'NONE',  ( -20.85000000000000142, -1.164121893230052995, -175.4148480855716059 ) ) ;
#16696 = EDGE_LOOP ( 'NONE', ( #93953, #122212, #130847 ) ) ;
#16697 = FACE_OUTER_BOUND ( 'NONE', #69200, .T. ) ;
#16698 = VECTOR ( 'NONE', #239513, 1000.000000000000000 ) ;
#16699 = EDGE_CURVE ( 'NONE', #7066, #257484, #11625, .T. ) ;
#16701 = CIRCLE ( 'NONE', #125032, 0.2000000000000057288 ) ;
#16700 = LINE ( 'NONE', #12855, #76187 ) ;
#16702 = EDGE_LOOP ( 'NONE', ( #106284, #245868, #121127, #6123 ) ) ;
#16703 = CARTESIAN_POINT ( 'NONE',  ( 21.14999999999999858, 43.54959646497384540, -234.7249050332107458 ) ) ;
#16704 = CARTESIAN_POINT ( 'NONE',  ( 21.15000000000005187, 74.94272479589878344, -8.023107484524793165 ) ) ;
#16705 = ORIENTED_EDGE ( 'NONE', *, *, #62797, .T. ) ;
#16706 = DIRECTION ( 'NONE',  ( -0.000000000000000000, -2.891205793294679805E-16, 1.000000000000000000 ) ) ;
#16707 = EDGE_CURVE ( 'NONE', #101212, #219433, #149599, .T. ) ;
#16708 = VERTEX_POINT ( 'NONE', #30943 ) ;
#16709 = DIRECTION ( 'NONE',  ( 0.000000000000000000, 7.109473446599835262E-15, -1.000000000000000000 ) ) ;
#16710 = CARTESIAN_POINT ( 'NONE',  ( -21.05000000000000071, 70.47363787294415260, -228.3418745167492432 ) ) ;
#16712 = CARTESIAN_POINT ( 'NONE',  ( 23.24999999999999645, 4.775700934590584090, -179.3487681040459165 ) ) ;
#16711 = UNCERTAINTY_MEASURE_WITH_UNIT (LENGTH_MEASURE( 1.000000000000000082E-05 ), #218277, 'distance_accuracy_value', 'NONE');
#16713 = EDGE_CURVE ( 'NONE', #20260, #53618, #19997, .T. ) ;
#16714 = DIRECTION ( 'NONE',  ( 1.000000000000000000, 0.000000000000000000, 0.000000000000000000 ) ) ;
#16715 = DIRECTION ( 'NONE',  ( 2.840903330521631775E-16, -0.8700118002898321601, 0.4930308989875230585 ) ) ;
#16716 = CARTESIAN_POINT ( 'NONE',  ( -14.77738660682463312, 46.65242889160100503, -234.7339858363278040 ) ) ;
#16717 = DIRECTION ( 'NONE',  ( 1.000000000000000000, 0.000000000000000000, 0.000000000000000000 ) ) ;
#16718 = DIRECTION ( 'NONE',  ( 0.000000000000000000, -0.9651348961777379554, 0.2617529984164210233 ) ) ;
#16719 = EDGE_CURVE ( 'NONE', #241241, #14564, #230392, .T. ) ;
#16721 = VERTEX_POINT ( 'NONE', #231693 ) ;
#16720 = CARTESIAN_POINT ( 'NONE',  ( 21.05000000000000071, 69.69548367074791884, -103.0020041764652063 ) ) ;
#16722 = ORIENTED_EDGE ( 'NONE', *, *, #128289, .T. ) ;
#16724 = DIRECTION ( 'NONE',  ( 1.000000000000000000, -1.476360405086644309E-16, 0.000000000000000000 ) ) ;
#16723 = FACE_OUTER_BOUND ( 'NONE', #245211, .T. ) ;
#16726 = ORIENTED_EDGE ( 'NONE', *, *, #51374, .F. ) ;
#16725 = LINE ( 'NONE', #50675, #6906 ) ;
#16727 = AXIS2_PLACEMENT_3D ( 'NONE', #206882, #182196, #42669 ) ;
#16728 = EDGE_LOOP ( 'NONE', ( #255760, #202446, #84176, #145665, #190088, #218155 ) ) ;
#16729 = DIRECTION ( 'NONE',  ( 1.000000000000000000, 0.000000000000000000, 0.000000000000000000 ) ) ;
#16730 = CARTESIAN_POINT ( 'NONE',  ( 20.22516295850462598, 9.899364295461838381, -175.4100657120905566 ) ) ;
#16731 = EDGE_CURVE ( 'NONE', #183349, #227433, #240561, .T. ) ;
#16732 = EDGE_CURVE ( 'NONE', #148718, #43391, #77715, .T. ) ;
#16733 = FACE_OUTER_BOUND ( 'NONE', #74538, .T. ) ;
#16734 = CARTESIAN_POINT ( 'NONE',  ( 18.48536876927980543, -9.463527249867304647, -7.048618265082689405 ) ) ;
#16735 = AXIS2_PLACEMENT_3D ( 'NONE', #198099, #254203, #156448 ) ;
#16736 = DIRECTION ( 'NONE',  ( 2.952720810173289112E-16, -1.000000000000000000, 0.000000000000000000 ) ) ;
#16737 = DIRECTION ( 'NONE',  ( 0.000000000000000000, -1.000000000000000000, 0.000000000000000000 ) ) ;
#16738 = CARTESIAN_POINT ( 'NONE',  ( 23.14999999999999503, 69.55000000001260219, -191.1731074845243938 ) ) ;
#16739 = DIRECTION ( 'NONE',  ( 1.000000000000000000, 0.000000000000000000, 0.000000000000000000 ) ) ;
#16740 = ORIENTED_EDGE ( 'NONE', *, *, #248990, .F. ) ;
#16741 = VERTEX_POINT ( 'NONE', #179423 ) ;
#16742 = DIRECTION ( 'NONE',  ( -0.7071067811865475727, 0.7071067811865475727, 4.937700262164531476E-15 ) ) ;
#16743 = CIRCLE ( 'NONE', #224823, 0.9000000000000014655 ) ;
#16744 = EDGE_CURVE ( 'NONE', #44088, #235594, #207260, .T. ) ;
#16745 = ORIENTED_EDGE ( 'NONE', *, *, #215831, .T. ) ;
#16746 = FACE_OUTER_BOUND ( 'NONE', #110335, .T. ) ;
#16749 = EDGE_CURVE ( 'NONE', #123238, #75618, #58149, .T. ) ;
#16748 = ORIENTED_EDGE ( 'NONE', *, *, #226237, .F. ) ;
#16747 = AXIS2_PLACEMENT_3D ( 'NONE', #96521, #216490, #59963 ) ;
#16750 = CARTESIAN_POINT ( 'NONE',  ( -16.86133551771148475, 14.14864742250337137, -219.2075304419909116 ) ) ;
#16751 = VECTOR ( 'NONE', #73410, 1000.000000000000000 ) ;
#16752 = DIRECTION ( 'NONE',  ( -1.000000000000000000, -2.952720810173289112E-16, 0.000000000000000000 ) ) ;
#16753 = DIRECTION ( 'NONE',  ( -1.000000000000000000, -1.836970198721029934E-16, -3.186635328391151676E-31 ) ) ;
#16754 = EDGE_CURVE ( 'NONE', #208088, #31295, #215595, .T. ) ;
#16756 = ORIENTED_EDGE ( 'NONE', *, *, #213121, .T. ) ;
#16755 = DIRECTION ( 'NONE',  ( -0.000000000000000000, 0.8660254037844411501, 0.4999999999999956701 ) ) ;
#16757 = DIRECTION ( 'NONE',  ( -1.000000000000000000, 0.000000000000000000, -0.000000000000000000 ) ) ;
#16758 = ORIENTED_EDGE ( 'NONE', *, *, #80399, .F. ) ;
#16759 = AXIS2_PLACEMENT_3D ( 'NONE', #48021, #46732, #27218 ) ;
#16761 = AXIS2_PLACEMENT_3D ( 'NONE', #192777, #213604, #153704 ) ;
#16760 = PLANE ( 'NONE',  #237657 ) ;
#16762 = CARTESIAN_POINT ( 'NONE',  ( -18.50000000000000000, 7.021664781911246322, -171.3335654018973173 ) ) ;
#16763 = FACE_OUTER_BOUND ( 'NONE', #216797, .T. ) ;
#16764 = EDGE_CURVE ( 'NONE', #112286, #25147, #194788, .T. ) ;
#16765 = DIRECTION ( 'NONE',  ( 1.000000000000000000, 1.394253735153569469E-16, 2.602809386958778209E-16 ) ) ;
#16766 = LINE ( 'NONE', #76705, #28270 ) ;
#16768 = ORIENTED_EDGE ( 'NONE', *, *, #166442, .T. ) ;
#16767 = EDGE_CURVE ( 'NONE', #145044, #176334, #57379, .T. ) ;
#16769 = CARTESIAN_POINT ( 'NONE',  ( -18.39999999999999858, 85.50000000001138289, -29.42291809330222563 ) ) ;
#16770 = ORIENTED_EDGE ( 'NONE', *, *, #72224, .T. ) ;
#16773 = ORIENTED_EDGE ( 'NONE', *, *, #141590, .T. ) ;
#16772 = FACE_OUTER_BOUND ( 'NONE', #178100, .T. ) ;
#16771 = DIRECTION ( 'NONE',  ( 0.000000000000000000, -0.8814952561688476074, 0.4721928772777262417 ) ) ;
#16774 = AXIS2_PLACEMENT_3D ( 'NONE', #196186, #234020, #256090 ) ;
#16775 = CARTESIAN_POINT ( 'NONE',  ( 22.50497660315936699, 76.07871793023755913, -114.7729029894197339 ) ) ;
#16776 = AXIS2_PLACEMENT_3D ( 'NONE', #178690, #116125, #4 ) ;
#16777 = AXIS2_PLACEMENT_3D ( 'NONE', #250391, #90022, #228274 ) ;
#16778 = TOROIDAL_SURFACE ( 'NONE', #29271, 11.65000000000000036, 0.1000000000000000056 ) ;
#16779 = AXIS2_PLACEMENT_3D ( 'NONE', #60182, #177608, #200993 ) ;
#16780 = ADVANCED_FACE ( 'NONE', ( #94723 ), #138956, .T. ) ;
#16781 = DIRECTION ( 'NONE',  ( 0.000000000000000000, -6.982962677686266711E-15, 1.000000000000000000 ) ) ;
#16782 = VERTEX_POINT ( 'NONE', #136389 ) ;
#16783 = DIRECTION ( 'NONE',  ( 0.000000000000000000, -0.1350103645451807555, -0.9908441862701610203 ) ) ;
#16784 = DIRECTION ( 'NONE',  ( 0.000000000000000000, -7.304098846218139203E-15, 1.000000000000000000 ) ) ;
#16785 = CARTESIAN_POINT ( 'NONE',  ( 23.15000000000000213, 85.00000000001188027, -93.12913836187181005 ) ) ;
#16786 = ADVANCED_FACE ( 'NONE', ( #37347 ), #193843, .T. ) ;
#16788 = EDGE_LOOP ( 'NONE', ( #216731, #246363, #145209, #216619 ) ) ;
#16787 = CARTESIAN_POINT ( 'NONE',  ( -20.64999999999999858, 73.50000000001180922, -82.74772940728642823 ) ) ;
#16789 = DIRECTION ( 'NONE',  ( 0.000000000000000000, 0.1335171055202901691, -0.9910465087640861759 ) ) ;
#16790 = VERTEX_POINT ( 'NONE', #15211 ) ;
#16791 = DIRECTION ( 'NONE',  ( -1.000000000000000000, 0.000000000000000000, -0.000000000000000000 ) ) ;
#16792 = CARTESIAN_POINT ( 'NONE',  ( 18.52165635395191501, -9.481150711270952769, -74.02483758286261661 ) ) ;
#16793 = CARTESIAN_POINT ( 'NONE',  ( -16.78569801330233702, 44.14263524120624282, -235.2979910463945714 ) ) ;
#16794 = ORIENTED_EDGE ( 'NONE', *, *, #193020, .T. ) ;
#16795 = CARTESIAN_POINT ( 'NONE',  ( 23.25000000000000000, 11.31726856452598184, -246.8669175193824969 ) ) ;
#16796 = ORIENTED_EDGE ( 'NONE', *, *, #139595, .F. ) ;
#16797 = DIRECTION ( 'NONE',  ( 1.000000000000000000, -0.000000000000000000, -0.000000000000000000 ) ) ;
#16798 = CARTESIAN_POINT ( 'NONE',  ( -21.05000000000000071, -11.48912529306489994, -64.00000000000000000 ) ) ;
#16799 = CARTESIAN_POINT ( 'NONE',  ( -17.11825945287482753, 9.950000000011138823, -46.25000000000000000 ) ) ;
#16800 = VERTEX_POINT ( 'NONE', #95997 ) ;
#16801 = DIRECTION ( 'NONE',  ( 0.000000000000000000, -0.9915357197604982575, 0.1298341882519033486 ) ) ;
#16802 = AXIS2_PLACEMENT_3D ( 'NONE', #139885, #43379, #59047 ) ;
#16803 = DIRECTION ( 'NONE',  ( 1.000000000000000000, 0.000000000000000000, 0.000000000000000000 ) ) ;
#16804 = AXIS2_PLACEMENT_3D ( 'NONE', #13928, #234235, #16504 ) ;
#16805 = VERTEX_POINT ( 'NONE', #174324 ) ;
#16806 = DIRECTION ( 'NONE',  ( -3.035766082959430717E-14, -6.982962677686266711E-15, 1.000000000000000000 ) ) ;
#16807 = PLANE ( 'NONE',  #77483 ) ;
#16808 = CARTESIAN_POINT ( 'NONE',  ( 22.39999999999999503, 11.45959274888149970, -198.4018787499352641 ) ) ;
#16809 = VECTOR ( 'NONE', #65020, 1000.000000000000000 ) ;
#16810 = ADVANCED_FACE ( 'NONE', ( #75194 ), #94685, .T. ) ;
#16811 = ORIENTED_EDGE ( 'NONE', *, *, #68904, .F. ) ;
#16812 = DIRECTION ( 'NONE',  ( 0.000000000000000000, -0.9667078373770112698, -0.2558827019434132821 ) ) ;
#16813 = ORIENTED_EDGE ( 'NONE', *, *, #25728, .F. ) ;
#16815 = ORIENTED_EDGE ( 'NONE', *, *, #30240, .T. ) ;
#16814 = CARTESIAN_POINT ( 'NONE',  ( -21.05000000000000071, -11.48912529307605546, -30.50000000000000000 ) ) ;
#16816 = CONICAL_SURFACE ( 'NONE', #208365, 4.049999999999998046, 0.7853981633974604915 ) ;
#16819 = EDGE_LOOP ( 'NONE', ( #247055, #240239, #145425, #113716 ) ) ;
#16818 = EDGE_LOOP ( 'NONE', ( #214245, #94111, #167259 ) ) ;
#16817 = DIRECTION ( 'NONE',  ( 0.000000000000000000, 0.000000000000000000, -1.000000000000000000 ) ) ;
#16820 = AXIS2_PLACEMENT_3D ( 'NONE', #222050, #123001, #248068 ) ;
#16821 = CARTESIAN_POINT ( 'NONE',  ( 20.94999999999999929, -1.135018845899022466, -74.71697688343232358 ) ) ;
#16822 = CARTESIAN_POINT ( 'NONE',  ( 18.39999999999999503, 70.35000000001207354, -123.8731074845243398 ) ) ;
#16823 = DIRECTION ( 'NONE',  ( 0.000000000000000000, 6.982962677686266711E-15, -1.000000000000000000 ) ) ;
#16825 = EDGE_CURVE ( 'NONE', #248838, #196126, #44931, .T. ) ;
#16824 = FACE_OUTER_BOUND ( 'NONE', #112413, .T. ) ;
#16826 = VECTOR ( 'NONE', #73349, 1000.000000000000000 ) ;
#16827 = CARTESIAN_POINT ( 'NONE',  ( 20.85000000000000142, -1.835859311432481045, -179.0044391687985410 ) ) ;
#16828 = VECTOR ( 'NONE', #220213, 1000.000000000000000 ) ;
#16829 = CARTESIAN_POINT ( 'NONE',  ( 20.94999999999999574, -1.162701749926853712, -75.10000000000003695 ) ) ;
#16830 = DIRECTION ( 'NONE',  ( 0.000000000000000000, 1.000000000000000000, 0.000000000000000000 ) ) ;
#16831 = ORIENTED_EDGE ( 'NONE', *, *, #29896, .F. ) ;
#16832 = ORIENTED_EDGE ( 'NONE', *, *, #134045, .F. ) ;
#16833 = VERTEX_POINT ( 'NONE', #97255 ) ;
#16834 = FACE_OUTER_BOUND ( 'NONE', #48777, .T. ) ;
#16836 = ORIENTED_EDGE ( 'NONE', *, *, #74002, .T. ) ;
#16835 = CARTESIAN_POINT ( 'NONE',  ( -16.93262454970419384, 65.99797953208218360, -182.5960312582870984 ) ) ;
#16837 = DIRECTION ( 'NONE',  ( 1.000000000000000000, 0.000000000000000000, 0.000000000000000000 ) ) ;
#16838 = VERTEX_POINT ( 'NONE', #176859 ) ;
#16839 = CARTESIAN_POINT ( 'NONE',  ( 22.00356870142688948, 7.254242362487860696, -100.5000000000000711 ) ) ;
#16840 = VERTEX_POINT ( 'NONE', #256302 ) ;
#16841 = LINE ( 'NONE', #136755, #108716 ) ;
#16842 = ORIENTED_EDGE ( 'NONE', *, *, #198126, .T. ) ;
#16843 = AXIS2_PLACEMENT_3D ( 'NONE', #145443, #144149, #67203 ) ;
#16844 = VECTOR ( 'NONE', #30224, 1000.000000000000114 ) ;
#16845 = CARTESIAN_POINT ( 'NONE',  ( -21.14999999999999858, 11.65000000000000036, -6.783865662978153743 ) ) ;
#16846 = DIRECTION ( 'NONE',  ( 0.7071067811865708874, -0.3338907855511046296, -0.6233112732207185536 ) ) ;
#16848 = ORIENTED_EDGE ( 'NONE', *, *, #61557, .T. ) ;
#16847 = ORIENTED_EDGE ( 'NONE', *, *, #90244, .T. ) ;
#16849 = ORIENTED_EDGE ( 'NONE', *, *, #238717, .T. ) ;
#16850 = CARTESIAN_POINT ( 'NONE',  ( 20.94999999999999929, 47.95459712139159336, -246.5019368548292675 ) ) ;
#16851 = ORIENTED_EDGE ( 'NONE', *, *, #48242, .T. ) ;
#16852 = ORIENTED_EDGE ( 'NONE', *, *, #213353, .T. ) ;
#16853 = CARTESIAN_POINT ( 'NONE',  ( 21.05000000000000071, 61.88149656937974896, -248.1136133839584090 ) ) ;
#16854 = VERTEX_POINT ( 'NONE', #38618 ) ;
#16855 = CARTESIAN_POINT ( 'NONE',  ( -23.15000000000000213, 7.128833340093095217, -233.7327013124392749 ) ) ;
#16856 = B_SPLINE_CURVE_WITH_KNOTS ( 'NONE', 3,
 ( #247425, #205731, #45381, #145751, #124930, #27141, #203168, #49228 ),
 .UNSPECIFIED., .F., .F.,
 ( 4, 2, 2, 4 ),
 ( 0.000000000000000000, 0.0002181133598169129764, 0.0003271700397253546246, 0.0004362267196337962999 ),
 .UNSPECIFIED. ) ;
#16858 = DIRECTION ( 'NONE',  ( 0.000000000000000000, -1.000000000000000000, -0.000000000000000000 ) ) ;
#16857 = DIRECTION ( 'NONE',  ( 0.000000000000000000, 6.982962677686267499E-15, -1.000000000000000000 ) ) ;
#16859 = CARTESIAN_POINT ( 'NONE',  ( 21.05000000000000071, -0.09999999998884338825, -155.8504291924551808 ) ) ;
#16860 = DIRECTION ( 'NONE',  ( -1.000000000000000000, -0.000000000000000000, -0.000000000000000000 ) ) ;
#16861 = VERTEX_POINT ( 'NONE', #118149 ) ;
#16862 = ORIENTED_EDGE ( 'NONE', *, *, #70304, .F. ) ;
#16863 = CARTESIAN_POINT ( 'NONE',  ( 18.46932045258648358, 85.67068520027757472, -96.34924711152753218 ) ) ;
#16865 = AXIS2_PLACEMENT_3D ( 'NONE', #18308, #97812, #255582 ) ;
#16864 = CARTESIAN_POINT ( 'NONE',  ( 21.97500000000000497, 9.750000000011153745, -79.25000000000004263 ) ) ;
#16866 = LINE ( 'NONE', #79370, #224661 ) ;
#16867 = VECTOR ( 'NONE', #108313, 1000.000000000000000 ) ;
#16868 = ADVANCED_FACE ( 'NONE', ( #21626 ), #125838, .T. ) ;
#16869 = AXIS2_PLACEMENT_3D ( 'NONE', #52814, #256095, #97042 ) ;
#16870 = ORIENTED_EDGE ( 'NONE', *, *, #91639, .T. ) ;
#16871 = DIRECTION ( 'NONE',  ( 0.000000000000000000, -1.000000000000000000, -5.551115123125768187E-14 ) ) ;
#16872 = CARTESIAN_POINT ( 'NONE',  ( 23.50000000000005684, 77.16254490893143725, -44.02310748452479316 ) ) ;
#16873 = AXIS2_PLACEMENT_3D ( 'NONE', #123439, #81698, #80414 ) ;
#16874 = CARTESIAN_POINT ( 'NONE',  ( -21.44999999999999929, 65.77012247227901298, -213.5448142138000378 ) ) ;
#16875 = ORIENTED_EDGE ( 'NONE', *, *, #196405, .T. ) ;
#16876 = ORIENTED_EDGE ( 'NONE', *, *, #167200, .F. ) ;
#16877 = EDGE_CURVE ( 'NONE', #112680, #53080, #236450, .T. ) ;
#16878 = FACE_OUTER_BOUND ( 'NONE', #257581, .T. ) ;
#16879 = CARTESIAN_POINT ( 'NONE',  ( -16.80438519320023616, 66.05022090354371755, -123.8723692036030997 ) ) ;
#16880 = VERTEX_POINT ( 'NONE', #64581 ) ;
#16881 = DIRECTION ( 'NONE',  ( 0.000000000000000000, -0.7071067811865472397, -0.7071067811865479058 ) ) ;
#16882 = VERTEX_POINT ( 'NONE', #162430 ) ;
#16883 = CARTESIAN_POINT ( 'NONE',  ( -23.25000000000000000, 77.16412189325258453, -28.10825939895270764 ) ) ;
#16884 = LINE ( 'NONE', #70463, #257848 ) ;
#16886 = DIRECTION ( 'NONE',  ( 1.000000000000000000, -7.049440681616512959E-16, 1.911869773728117674E-16 ) ) ;
#16885 = CARTESIAN_POINT ( 'NONE',  ( -20.64999999999999858, -8.999999999988844479, -124.1060308773475924 ) ) ;
#16887 = EDGE_CURVE ( 'NONE', #29497, #84837, #244702, .T. ) ;
#16888 = AXIS2_PLACEMENT_3D ( 'NONE', #245303, #227009, #91369 ) ;
#16889 = DIRECTION ( 'NONE',  ( 2.952720810173288619E-16, -1.000000000000000000, 0.000000000000000000 ) ) ;
#16890 = CARTESIAN_POINT ( 'NONE',  ( 21.11701782572533048, 65.27839088400440914, -90.77807005501317406 ) ) ;
#16891 = ADVANCED_FACE ( 'NONE', ( #106263 ), #183265, .T. ) ;
#16892 = CARTESIAN_POINT ( 'NONE',  ( -18.59999999999999787, 85.48068669529064323, -62.58199231576639932 ) ) ;
#16894 = EDGE_LOOP ( 'NONE', ( #14878, #131398, #60078, #189232 ) ) ;
#16893 = ORIENTED_EDGE ( 'NONE', *, *, #212430, .F. ) ;
#16895 = VERTEX_POINT ( 'NONE', #241936 ) ;
#16896 = CARTESIAN_POINT ( 'NONE',  ( 22.47809213839789066, 0.03753706762852151990, 11.64997333478780206 ) ) ;
#16897 = CARTESIAN_POINT ( 'NONE',  ( -23.25000000000000000, 10.33248238083634440, -139.5948465439131780 ) ) ;
#16898 = CARTESIAN_POINT ( 'NONE',  ( -33.72168855820452649, 52.34166666667924517, -186.7731074845245303 ) ) ;
#16899 = ADVANCED_FACE ( 'NONE', ( #184529 ), #86694, .F. ) ;
#16901 = CARTESIAN_POINT ( 'NONE',  ( 21.14999999999999858, 6.650000000011155876, -179.6499999999999773 ) ) ;
#16900 = CARTESIAN_POINT ( 'NONE',  ( 20.97107704358301916, 8.875478152021283762, -8.558973229389252424 ) ) ;
#16902 = DIRECTION ( 'NONE',  ( 0.000000000000000000, 2.891205793294679805E-16, -1.000000000000000000 ) ) ;
#16903 = VERTEX_POINT ( 'NONE', #166300 ) ;
#16904 = FACE_OUTER_BOUND ( 'NONE', #226858, .T. ) ;
#16905 = VERTEX_POINT ( 'NONE', #240660 ) ;
#16906 = VERTEX_POINT ( 'NONE', #145403 ) ;
#16907 = PLANE ( 'NONE',  #232 ) ;
#16908 = FACE_OUTER_BOUND ( 'NONE', #36751, .T. ) ;
#16909 = LINE ( 'NONE', #1160, #116888 ) ;
#16910 = DIRECTION ( 'NONE',  ( 0.000000000000000000, 0.9770955615653548199, 0.2128009952262535920 ) ) ;
#16911 = AXIS2_PLACEMENT_3D ( 'NONE', #98149, #76054, #14832 ) ;
#16912 = CARTESIAN_POINT ( 'NONE',  ( -20.00857864376270001, 9.350000000011156942, -188.6499999999999488 ) ) ;
#16913 = CARTESIAN_POINT ( 'NONE',  ( 20.02499999999999858, 51.97441255244040548, -232.0063394385699667 ) ) ;
#16914 = ORIENTED_EDGE ( 'NONE', *, *, #147422, .F. ) ;
#16915 = ORIENTED_EDGE ( 'NONE', *, *, #129763, .T. ) ;
#16916 = LINE ( 'NONE', #96417, #254908 ) ;
#16917 = VECTOR ( 'NONE', #3087, 1000.000000000000000 ) ;
#16918 = CARTESIAN_POINT ( 'NONE',  ( -21.05000000000000071, 74.16465844978765176, -124.9679561919613207 ) ) ;
#16919 = FACE_OUTER_BOUND ( 'NONE', #162451, .T. ) ;
#16920 = DIRECTION ( 'NONE',  ( 0.000000000000000000, 0.000000000000000000, -1.000000000000000000 ) ) ;
#16921 = CARTESIAN_POINT ( 'NONE',  ( -23.25000000000000000, 87.48912529308749697, -39.12310748452424747 ) ) ;
#16922 = PLANE ( 'NONE',  #213235 ) ;
#16924 = EDGE_CURVE ( 'NONE', #198003, #231948, #111565, .T. ) ;
#16923 = FACE_OUTER_BOUND ( 'NONE', #55468, .T. ) ;
#16925 = B_SPLINE_CURVE_WITH_KNOTS ( 'NONE', 3,
 ( #57188, #79322, #158909, #238418, #40248, #213716, #194180, #27106, #121074, #144422, #62356, #182315, #204411, #3649, #41527, #161472, #46612, #102727, #240994 ),
 .UNSPECIFIED., .F., .F.,
 ( 4, 3, 3, 3, 3, 3, 4 ),
 ( 1.387778780781445521E-17, 2.646747978908964204E-05, 5.271166642128792909E-05, 9.008788829885240981E-05, 0.0001426648776561058600, 0.0001897378458659877839, 0.0001917382627806327297 ),
 .UNSPECIFIED. ) ;
#16927 = CARTESIAN_POINT ( 'NONE',  ( -14.00000000000000178, 66.15000000001185754, -86.27310748452437394 ) ) ;
#16926 = CARTESIAN_POINT ( 'NONE',  ( -22.50000000000000000, 0.09263750060947925635, 11.64969720704075051 ) ) ;
#16928 = DIRECTION ( 'NONE',  ( -7.304098846218134667E-16, -1.000000000000000000, 0.000000000000000000 ) ) ;
#16929 = DIRECTION ( 'NONE',  ( 0.000000000000000000, -6.982962677686266711E-15, 1.000000000000000000 ) ) ;
#16930 = DIRECTION ( 'NONE',  ( -1.000000000000000000, 0.000000000000000000, 0.000000000000000000 ) ) ;
#16931 = CARTESIAN_POINT ( 'NONE',  ( 23.50000000000005684, 79.78873604695631627, -7.297728304630792806 ) ) ;
#16932 = AXIS2_PLACEMENT_3D ( 'NONE', #256502, #213584, #75399 ) ;
#16934 = ORIENTED_EDGE ( 'NONE', *, *, #180729, .T. ) ;
#16933 = FACE_OUTER_BOUND ( 'NONE', #126493, .T. ) ;
#16935 = AXIS2_PLACEMENT_3D ( 'NONE', #201747, #220035, #3541 ) ;
#16936 = EDGE_CURVE ( 'NONE', #71912, #176927, #257248, .T. ) ;
#16937 = AXIS2_PLACEMENT_3D ( 'NONE', #184020, #142322, #22409 ) ;
#16938 = DIRECTION ( 'NONE',  ( 1.000000000000000000, 0.000000000000000000, 0.000000000000000000 ) ) ;
#16939 = VERTEX_POINT ( 'NONE', #7167 ) ;
#16941 = ADVANCED_FACE ( 'NONE', ( #62039 ), #245804, .T. ) ;
#16940 = VECTOR ( 'NONE', #33426, 1000.000000000000000 ) ;
#16942 = LINE ( 'NONE', #1192, #182692 ) ;
#16943 = CARTESIAN_POINT ( 'NONE',  ( -18.59999999999999787, 64.35000000001208775, -129.5083017138703667 ) ) ;
#16944 = ORIENTED_EDGE ( 'NONE', *, *, #250398, .F. ) ;
#16945 = DIRECTION ( 'NONE',  ( 0.000000000000000000, 0.000000000000000000, -1.000000000000000000 ) ) ;
#16946 = EDGE_CURVE ( 'NONE', #242236, #16800, #129375, .T. ) ;
#16947 = FACE_OUTER_BOUND ( 'NONE', #55042, .T. ) ;
#16948 = CARTESIAN_POINT ( 'NONE',  ( 18.59999999999999076, 69.35000000001254250, -182.1731074845243938 ) ) ;
#16949 = AXIS2_PLACEMENT_3D ( 'NONE', #41342, #235651, #139090 ) ;
#16950 = DIRECTION ( 'NONE',  ( 1.000000000000000000, 0.000000000000000000, 0.000000000000000000 ) ) ;
#16951 = AXIS2_PLACEMENT_3D ( 'NONE', #40468, #118700, #199522 ) ;
#16952 = AXIS2_PLACEMENT_3D ( 'NONE', #11488, #230533, #7626 ) ;
#16954 = CARTESIAN_POINT ( 'NONE',  ( 18.52928932188133970, 10.27928932188134503, -24.65000000000000213 ) ) ;
#16953 = B_SPLINE_CURVE_WITH_KNOTS ( 'NONE', 3,
 ( #227050, #246612, #127965, #88805, #247900, #69285 ),
 .UNSPECIFIED., .F., .F.,
 ( 4, 2, 4 ),
 ( 0.000000000000000000, 0.0002113392456165985155, 0.0004226784912331970311 ),
 .UNSPECIFIED. ) ;
#16955 = CARTESIAN_POINT ( 'NONE',  ( 18.49999999999999289, 65.75000000001253397, -182.1731074845244223 ) ) ;
#16956 = VECTOR ( 'NONE', #56963, 1000.000000000000000 ) ;
#16957 = CIRCLE ( 'NONE', #8564, 0.1000000000000028644 ) ;
#16958 = EDGE_LOOP ( 'NONE', ( #120618, #150177, #53891, #35754 ) ) ;
#16959 = DIRECTION ( 'NONE',  ( 1.000000000000000000, 0.000000000000000000, 0.000000000000000000 ) ) ;
#16961 = EDGE_LOOP ( 'NONE', ( #37168, #228849, #123456, #66845 ) ) ;
#16960 = DIRECTION ( 'NONE',  ( 0.000000000000000000, 6.982962677686266711E-15, -1.000000000000000000 ) ) ;
#16962 = FACE_OUTER_BOUND ( 'NONE', #66118, .T. ) ;
#16963 = EDGE_CURVE ( 'NONE', #252190, #157610, #211521, .T. ) ;
#16964 = CARTESIAN_POINT ( 'NONE',  ( -21.59780538579341069, 69.15290947006911892, -170.1220861541223996 ) ) ;
#16965 = DIRECTION ( 'NONE',  ( 0.000000000000000000, 0.000000000000000000, -1.000000000000000000 ) ) ;
#16966 = ORIENTED_EDGE ( 'NONE', *, *, #109434, .T. ) ;
#16967 = CARTESIAN_POINT ( 'NONE',  ( -16.77180007708461673, 66.05000000001261640, -190.8874933655695827 ) ) ;
#16968 = ADVANCED_FACE ( 'NONE', ( #103690 ), #4599, .F. ) ;
#16969 = APPLICATION_PROTOCOL_DEFINITION ( 'draft international standard', 'automotive_design', 1998, #39080 ) ;
#16970 = ADVANCED_FACE ( 'NONE', ( #84097 ), #53304, .F. ) ;
#16971 = AXIS2_PLACEMENT_3D ( 'NONE', #125223, #243870, #185191 ) ;
#16972 = DIRECTION ( 'NONE',  ( -1.000000000000000000, -0.000000000000000000, -0.000000000000000000 ) ) ;
#16973 = CARTESIAN_POINT ( 'NONE',  ( -27.30103769104855971, 12.19999999999999574, -347.0000000000001137 ) ) ;
#16974 = EDGE_LOOP ( 'NONE', ( #6360, #99811, #232006 ) ) ;
#16975 = FACE_OUTER_BOUND ( 'NONE', #208904, .T. ) ;
#16976 = DIRECTION ( 'NONE',  ( 0.000000000000000000, 0.9651348961777156399, -0.2617529984165037349 ) ) ;
#16977 = B_SPLINE_CURVE_WITH_KNOTS ( 'NONE', 3,
 ( #120058, #253101, #178758, #176172, #77038, #237410, #177466, #219109, #233568, #114892, #135723, #254373, #75775, #57465, #215275, #40532, #37945, #39233, #58737, #174923, #155336, #35393 ),
 .UNSPECIFIED., .F., .F.,
 ( 4, 3, 3, 3, 3, 3, 3, 4 ),
 ( 0.000000000000000000, 7.307836821079277406E-06, 4.161455748548289888E-05, 7.576591810647585821E-05, 0.0001098090429817541203, 0.0001438003617351132435, 0.0001777914035423700445, 0.0002117966137403027368 ),
 .UNSPECIFIED. ) ;
#16978 = ADVANCED_FACE ( 'NONE', ( #45029 ), #61865, .F. ) ;
#16979 = SURFACE_SIDE_STYLE ('',( #177354 ) ) ;
#16980 = ORIENTED_EDGE ( 'NONE', *, *, #68251, .F. ) ;
#16981 = ORIENTED_EDGE ( 'NONE', *, *, #9228, .T. ) ;
#16982 = EDGE_CURVE ( 'NONE', #194417, #51689, #107640, .T. ) ;
#16983 = EDGE_CURVE ( 'NONE', #20386, #83522, #228817, .T. ) ;
#16984 = CYLINDRICAL_SURFACE ( 'NONE', #167496, 0.1000000000000054040 ) ;
#16985 = DIRECTION ( 'NONE',  ( 0.000000000000000000, 0.000000000000000000, 1.000000000000000000 ) ) ;
#16986 = CARTESIAN_POINT ( 'NONE',  ( -21.65000000000000213, 42.13647595316535188, -239.1530172309881834 ) ) ;
#16987 = PLANE ( 'NONE',  #153421 ) ;
#16989 = CARTESIAN_POINT ( 'NONE',  ( -18.59999999999999787, 72.06821323333463170, -225.0920403225231610 ) ) ;
#16988 = CARTESIAN_POINT ( 'NONE',  ( 21.05000000000000071, -1.387796589506715250, -194.7104960456530023 ) ) ;
#16990 = DIRECTION ( 'NONE',  ( 0.000000000000000000, 0.000000000000000000, -1.000000000000000000 ) ) ;
#16991 = DIRECTION ( 'NONE',  ( 0.000000000000000000, 0.000000000000000000, 1.000000000000000000 ) ) ;
#16992 = CARTESIAN_POINT ( 'NONE',  ( 18.50000972452444969, 65.70673848566912056, -30.56382523348295166 ) ) ;
#16993 = LINE ( 'NONE', #256809, #82188 ) ;
#16994 = EDGE_LOOP ( 'NONE', ( #96701, #187121, #212255, #29009 ) ) ;
#16995 = AXIS2_PLACEMENT_3D ( 'NONE', #112690, #172710, #190964 ) ;
#16996 = ORIENTED_EDGE ( 'NONE', *, *, #206602, .F. ) ;
#16997 = CARTESIAN_POINT ( 'NONE',  ( -23.25000000000000000, -11.74999999998884448, -67.00000000000004263 ) ) ;
#16998 = CARTESIAN_POINT ( 'NONE',  ( 20.94999999999999574, 2.953700692300310848, -208.6327728934509764 ) ) ;
#17000 = CARTESIAN_POINT ( 'NONE',  ( 22.60000000000000142, 67.23127455305841238, -235.8551265064783991 ) ) ;
#16999 = CARTESIAN_POINT ( 'NONE',  ( 23.25000000000000000, 87.75000000001247713, -173.1231074845242688 ) ) ;
#17001 = AXIS2_PLACEMENT_3D ( 'NONE', #130087, #28476, #225322 ) ;
#17002 = ADVANCED_FACE ( 'NONE', ( #168876 ), #248369, .T. ) ;
#17003 = CYLINDRICAL_SURFACE ( 'NONE', #106109, 0.1000000000000028644 ) ;
#17005 = ADVANCED_FACE ( 'NONE', ( #149291 ), #47578, .F. ) ;
#17004 = DIRECTION ( 'NONE',  ( 1.000000000000000000, 0.000000000000000000, 0.000000000000000000 ) ) ;
#17006 = DIRECTION ( 'NONE',  ( 0.000000000000000000, -0.3042567129659849434, -0.9525900758537926283 ) ) ;
#17007 = EDGE_LOOP ( 'NONE', ( #225484, #253190, #257005, #11909, #49282 ) ) ;
#17008 = ORIENTED_EDGE ( 'NONE', *, *, #96738, .T. ) ;
#17009 = CIRCLE ( 'NONE', #212640, 0.09999999999999867328 ) ;
#17010 = EDGE_CURVE ( 'NONE', #3674, #205356, #87978, .T. ) ;
#17011 = CARTESIAN_POINT ( 'NONE',  ( -20.64999999999999858, 68.28002175382172823, -222.4371999040225774 ) ) ;
#17012 = ORIENTED_EDGE ( 'NONE', *, *, #173561, .T. ) ;
#17013 = CARTESIAN_POINT ( 'NONE',  ( -18.50000000000000000, 74.36282728704192380, -158.4409541190523498 ) ) ;
#17014 = AXIS2_PLACEMENT_3D ( 'NONE', #224376, #24925, #139691 ) ;
#17015 = CIRCLE ( 'NONE', #141881, 11.75000000000000533 ) ;
#17016 = DIRECTION ( 'NONE',  ( 0.000000000000000000, 0.8700118002898393765, -0.4930308989875104575 ) ) ;
#17017 = CARTESIAN_POINT ( 'NONE',  ( -23.15000000000000213, 87.75000000001246292, -181.7731074845242745 ) ) ;
#17018 = AXIS2_PLACEMENT_3D ( 'NONE', #182977, #37372, #256329 ) ;
#17019 = VERTEX_POINT ( 'NONE', #147986 ) ;
#17020 = DIRECTION ( 'NONE',  ( -1.000000000000000000, -6.834672213024256725E-16, 4.941700349840508052E-16 ) ) ;
#17021 = ORIENTED_EDGE ( 'NONE', *, *, #115871, .F. ) ;
#17022 = CARTESIAN_POINT ( 'NONE',  ( -18.46902351632713035, 85.50947011869320136, -163.0366535502669763 ) ) ;
#17023 = DIRECTION ( 'NONE',  ( -0.000000000000000000, 0.2617529984165031243, 0.9651348961777157509 ) ) ;
#17024 = DIRECTION ( 'NONE',  ( -5.603264701231743991E-32, -7.172728831056617961E-15, 1.000000000000000000 ) ) ;
#17025 = EDGE_CURVE ( 'NONE', #143756, #165658, #253090, .T. ) ;
#17026 = LINE ( 'NONE', #211369, #41520 ) ;
#17027 = CARTESIAN_POINT ( 'NONE',  ( 21.05000000000000071, -4.161311414658873886, -226.0656773515597706 ) ) ;
#17029 = LINE ( 'NONE', #96522, #233441 ) ;
#17028 = CARTESIAN_POINT ( 'NONE',  ( -18.59999999999999787, 9.350000000011156942, -188.7499999999999716 ) ) ;
#17030 = AXIS2_PLACEMENT_3D ( 'NONE', #83102, #44018, #242211 ) ;
#17031 = CARTESIAN_POINT ( 'NONE',  ( 17.23472005113827166, 65.69211804551146372, -147.9765306244557621 ) ) ;
#17032 = EDGE_CURVE ( 'NONE', #28751, #68121, #53489, .T. ) ;
#17033 = ORIENTED_EDGE ( 'NONE', *, *, #148849, .F. ) ;
#17035 = CARTESIAN_POINT ( 'NONE',  ( 23.15000000000000213, 85.50000000001179501, -79.41707660717668205 ) ) ;
#17034 = DIRECTION ( 'NONE',  ( 0.000000000000000000, 0.000000000000000000, -1.000000000000000000 ) ) ;
#17036 = ORIENTED_EDGE ( 'NONE', *, *, #78120, .F. ) ;
#17038 = VERTEX_POINT ( 'NONE', #26322 ) ;
#17037 = DIRECTION ( 'NONE',  ( 1.000000000000000000, -0.000000000000000000, 0.000000000000000000 ) ) ;
#17039 = EDGE_LOOP ( 'NONE', ( #153258, #127188, #2782, #232813 ) ) ;
#17040 = CARTESIAN_POINT ( 'NONE',  ( 23.24999999999999645, 1.115600667400684642E-11, -134.0000000000000000 ) ) ;
#17041 = FACE_OUTER_BOUND ( 'NONE', #138564, .T. ) ;
#17042 = CARTESIAN_POINT ( 'NONE',  ( 18.49999999999999289, 65.50857864377445594, -78.17310748452437963 ) ) ;
#17043 = CARTESIAN_POINT ( 'NONE',  ( -23.25000000000000355, 5.650000000011139001, -79.65000000000004832 ) ) ;
#17044 = ORIENTED_EDGE ( 'NONE', *, *, #37175, .T. ) ;
#17045 = EDGE_CURVE ( 'NONE', #82597, #62401, #22484, .T. ) ;
#17046 = LINE ( 'NONE', #39186, #33899 ) ;
#17047 = CARTESIAN_POINT ( 'NONE',  ( 22.50000000000000000, 7.790779598373383408, 0.09999999999999939493 ) ) ;
#17048 = ADVANCED_FACE ( 'NONE', ( #144955 ), #27633, .T. ) ;
#17049 = ORIENTED_EDGE ( 'NONE', *, *, #27153, .F. ) ;
#17050 = CARTESIAN_POINT ( 'NONE',  ( 21.05000000000000071, 87.29603075034744109, -139.5710066441881452 ) ) ;
#17051 = AXIS2_PLACEMENT_3D ( 'NONE', #228733, #192174, #13525 ) ;
#17052 = CIRCLE ( 'NONE', #221019, 4.149999999999987033 ) ;
#17054 = EDGE_CURVE ( 'NONE', #72480, #10263, #25056, .T. ) ;
#17053 = CIRCLE ( 'NONE', #83624, 11.65000000000000213 ) ;
#17056 = AXIS2_PLACEMENT_3D ( 'NONE', #107041, #92296, #86179 ) ;
#17055 = CARTESIAN_POINT ( 'NONE',  ( 21.07928932188134397, 6.328516656393303741, 0.09889514565439641580 ) ) ;
#17057 = VERTEX_POINT ( 'NONE', #44599 ) ;
#17058 = ORIENTED_EDGE ( 'NONE', *, *, #91718, .F. ) ;
#17059 = CARTESIAN_POINT ( 'NONE',  ( 23.25000000000000000, 87.75000000001156764, -57.37310748452424036 ) ) ;
#17060 = EDGE_CURVE ( 'NONE', #164329, #58209, #111738, .T. ) ;
#17061 = ORIENTED_EDGE ( 'NONE', *, *, #111400, .T. ) ;
#17062 = CIRCLE ( 'NONE', #4545, 0.09999999999999326095 ) ;
#17063 = DIRECTION ( 'NONE',  ( -1.000000000000000000, -3.265361837132813093E-16, 0.000000000000000000 ) ) ;
#17066 = EDGE_CURVE ( 'NONE', #70073, #14366, #188491, .T. ) ;
#17065 = ADVANCED_FACE ( 'NONE', ( #8044 ), #185383, .F. ) ;
#17064 = VERTEX_POINT ( 'NONE', #142400 ) ;
#17067 = DIRECTION ( 'NONE',  ( 0.000000000000000000, -0.4721928772777342354, -0.8814952561688431665 ) ) ;
#17068 = DIRECTION ( 'NONE',  ( -7.304098846217948299E-16, -1.000000000000000000, 0.000000000000000000 ) ) ;
#17069 = CARTESIAN_POINT ( 'NONE',  ( 21.05000000000000071, 60.85896401437204872, -225.4389122456526025 ) ) ;
#17070 = EDGE_CURVE ( 'NONE', #160725, #64945, #95179, .T. ) ;
#17071 = CARTESIAN_POINT ( 'NONE',  ( -16.86420534634261870, 63.08372296379771882, -213.0562714438781313 ) ) ;
#17072 = CARTESIAN_POINT ( 'NONE',  ( -22.50000000000000000, 0.1000000000111554016, -122.3504291924552234 ) ) ;
#17073 = CARTESIAN_POINT ( 'NONE',  ( 18.46163235739470920, -9.480150806907120753, -73.65761053987772300 ) ) ;
#17074 = FACE_OUTER_BOUND ( 'NONE', #125058, .T. ) ;
#17076 = ORIENTED_EDGE ( 'NONE', *, *, #34634, .F. ) ;
#17075 = EDGE_CURVE ( 'NONE', #43683, #22150, #82399, .T. ) ;
#17079 = ADVANCED_FACE ( 'NONE', ( #125422 ), #153483, .F. ) ;
#17078 = CARTESIAN_POINT ( 'NONE',  ( 18.49999999999996803, 68.92903212821327941, -132.7765432626560766 ) ) ;
#17077 = CARTESIAN_POINT ( 'NONE',  ( -22.39999999999999858, 0.1000000000111554016, -126.2092204016266379 ) ) ;
#17080 = EDGE_LOOP ( 'NONE', ( #86014, #212746, #249986, #79210 ) ) ;
#17083 = ORIENTED_EDGE ( 'NONE', *, *, #61616, .F. ) ;
#17082 = DIRECTION ( 'NONE',  ( 0.000000000000000000, -0.8103668758649498205, 0.5859227990963324917 ) ) ;
#17081 = DIRECTION ( 'NONE',  ( 4.408576920032446123E-17, -0.9371753822965315228, 0.3488585713686134238 ) ) ;
#17084 = ORIENTED_EDGE ( 'NONE', *, *, #248568, .F. ) ;
#17085 = FACE_OUTER_BOUND ( 'NONE', #68079, .T. ) ;
#17086 = CARTESIAN_POINT ( 'NONE',  ( -23.25000000000000000, 64.35000000001173248, -81.27310748452440237 ) ) ;
#17087 = CARTESIAN_POINT ( 'NONE',  ( 23.24999999999999289, 11.65000000001116298, -100.5000000000000284 ) ) ;
#17088 = EDGE_CURVE ( 'NONE', #24027, #210045, #245019, .T. ) ;
#17089 = CARTESIAN_POINT ( 'NONE',  ( -18.40000000000000213, 64.66825945288681510, -115.6731074845243796 ) ) ;
#17090 = ORIENTED_EDGE ( 'NONE', *, *, #144136, .F. ) ;
#17092 = VERTEX_POINT ( 'NONE', #241509 ) ;
#17091 = CARTESIAN_POINT ( 'NONE',  ( -23.15000000000000213, 64.25000000001229239, -157.7731074845244450 ) ) ;
#17093 = AXIS2_PLACEMENT_3D ( 'NONE', #54150, #35905, #132423 ) ;
#17094 = DIRECTION ( 'NONE',  ( 0.000000000000000000, 1.000000000000000000, 0.000000000000000000 ) ) ;
#17095 = ADVANCED_FACE ( 'NONE', ( #244063 ), #66729, .F. ) ;
#17097 = DIRECTION ( 'NONE',  ( 1.000000000000000000, 0.000000000000000000, 0.000000000000000000 ) ) ;
#17096 = CARTESIAN_POINT ( 'NONE',  ( 20.90000000000000213, 6.644425182197214674, 9.641788261573355001 ) ) ;
#17098 = ADVANCED_FACE ( 'NONE', ( #163428 ), #104685, .T. ) ;
#17100 = ORIENTED_EDGE ( 'NONE', *, *, #95246, .F. ) ;
#17099 = LINE ( 'NONE', #78316, #114160 ) ;
#17101 = AXIS2_PLACEMENT_3D ( 'NONE', #99965, #140394, #43881 ) ;
#17102 = ORIENTED_EDGE ( 'NONE', *, *, #15197, .T. ) ;
#17103 = VECTOR ( 'NONE', #27685, 1000.000000000000000 ) ;
#17104 = LINE ( 'NONE', #215280, #180989 ) ;
#17105 = DIRECTION ( 'NONE',  ( 0.000000000000000000, 0.000000000000000000, -1.000000000000000000 ) ) ;
#17106 = EDGE_LOOP ( 'NONE', ( #121464, #123948, #247329, #171010 ) ) ;
#17107 = FACE_OUTER_BOUND ( 'NONE', #48559, .T. ) ;
#17108 = ORIENTED_EDGE ( 'NONE', *, *, #244393, .F. ) ;
#17109 = DIRECTION ( 'NONE',  ( 1.000000000000000000, 0.000000000000000000, 0.000000000000000000 ) ) ;
#17110 = AXIS2_PLACEMENT_3D ( 'NONE', #98023, #55051, #135875 ) ;
#17112 = EDGE_CURVE ( 'NONE', #97495, #241107, #128496, .T. ) ;
#17111 = CARTESIAN_POINT ( 'NONE',  ( -18.39418127959864790, 11.48390560170929220, -158.2500000000000284 ) ) ;
#17113 = CARTESIAN_POINT ( 'NONE',  ( -23.25000000000000000, 11.65000000001115588, -188.7499999999999716 ) ) ;
#17114 = ORIENTED_EDGE ( 'NONE', *, *, #247190, .T. ) ;
#17115 = DIRECTION ( 'NONE',  ( 0.000000000000000000, 0.9126074666063768159, 0.4088369013363282178 ) ) ;
#17116 = ADVANCED_FACE ( 'NONE', ( #202543 ), #119163, .F. ) ;
#17117 = VECTOR ( 'NONE', #115455, 1000.000000000000114 ) ;
#17118 = DIRECTION ( 'NONE',  ( 0.000000000000000000, 0.5000000000000078826, 0.8660254037844340447 ) ) ;
#17119 = AXIS2_PLACEMENT_3D ( 'NONE', #54875, #191871, #106179 ) ;
#17121 = ORIENTED_EDGE ( 'NONE', *, *, #126748, .F. ) ;
#17120 = CIRCLE ( 'NONE', #125253, 0.1000000000000054040 ) ;
#17122 = ORIENTED_EDGE ( 'NONE', *, *, #137893, .T. ) ;
#17123 = CARTESIAN_POINT ( 'NONE',  ( -18.40904629823847216, -9.499999999988851584, -73.60018956248165978 ) ) ;
#17124 = CIRCLE ( 'NONE', #254396, 11.70000000000000284 ) ;
#17125 = ORIENTED_EDGE ( 'NONE', *, *, #145596, .T. ) ;
#17126 = EDGE_CURVE ( 'NONE', #163726, #110634, #74372, .T. ) ;
#17127 = EDGE_LOOP ( 'NONE', ( #141531, #25257, #194479, #156056 ) ) ;
#17129 = ORIENTED_EDGE ( 'NONE', *, *, #54259, .T. ) ;
#17128 = FACE_OUTER_BOUND ( 'NONE', #113414, .T. ) ;
#17130 = AXIS2_PLACEMENT_3D ( 'NONE', #241450, #204862, #223144 ) ;
#17131 = AXIS2_PLACEMENT_3D ( 'NONE', #61943, #120651, #257503 ) ;
#17132 = ORIENTED_EDGE ( 'NONE', *, *, #69419, .T. ) ;
#17133 = DIRECTION ( 'NONE',  ( -1.073024830501117725E-15, 0.000000000000000000, 1.000000000000000000 ) ) ;
#17136 = ORIENTED_EDGE ( 'NONE', *, *, #29106, .F. ) ;
#17135 = VERTEX_POINT ( 'NONE', #21364 ) ;
#17134 = CYLINDRICAL_SURFACE ( 'NONE', #14608, 0.1000000000000028644 ) ;
#17137 = ORIENTED_EDGE ( 'NONE', *, *, #222637, .T. ) ;
#17138 = LINE ( 'NONE', #217855, #52112 ) ;
#17139 = EDGE_CURVE ( 'NONE', #156062, #141640, #165934, .T. ) ;
#17140 = CIRCLE ( 'NONE', #83709, 0.09999999999999939493 ) ;
#17141 = VECTOR ( 'NONE', #133161, 1000.000000000000000 ) ;
#17142 = AXIS2_PLACEMENT_3D ( 'NONE', #35876, #191104, #17557 ) ;
#17143 = DIRECTION ( 'NONE',  ( 0.000000000000000000, 6.982962677686266711E-15, -1.000000000000000000 ) ) ;
#17144 = CIRCLE ( 'NONE', #95645, 0.1000000000000028644 ) ;
#17145 = AXIS2_PLACEMENT_3D ( 'NONE', #25451, #8452, #87949 ) ;
#17146 = LINE ( 'NONE', #96621, #142505 ) ;
#17147 = VERTEX_POINT ( 'NONE', #182998 ) ;
#17148 = CARTESIAN_POINT ( 'NONE',  ( 20.94999999999999574, 67.23127455305841238, -235.8551265064783991 ) ) ;
#17150 = ORIENTED_EDGE ( 'NONE', *, *, #237480, .T. ) ;
#17149 = CARTESIAN_POINT ( 'NONE',  ( -21.05000000000000071, 18.14639373905162145, -237.6648341169113792 ) ) ;
#17151 = DIRECTION ( 'NONE',  ( 0.000000000000000000, 6.982962677686266711E-15, -1.000000000000000000 ) ) ;
#17153 = ORIENTED_EDGE ( 'NONE', *, *, #184238, .F. ) ;
#17152 = DIRECTION ( 'NONE',  ( -3.440080580676165868E-14, -0.1298341882520124002, -0.9915357197604841577 ) ) ;
#17154 = VERTEX_POINT ( 'NONE', #219524 ) ;
#17155 = LINE ( 'NONE', #216609, #27653 ) ;
#17156 = AXIS2_PLACEMENT_3D ( 'NONE', #123632, #3666, #144440 ) ;
#17157 = ORIENTED_EDGE ( 'NONE', *, *, #185900, .F. ) ;
#17158 = ORIENTED_EDGE ( 'NONE', *, *, #181541, .T. ) ;
#17159 = CARTESIAN_POINT ( 'NONE',  ( -16.94037747912386038, 10.01353938249748410, -180.0511309579754595 ) ) ;
#17160 = CARTESIAN_POINT ( 'NONE',  ( 23.14999999999999858, 76.00000000001142553, -36.02310748452432421 ) ) ;
#17162 = ORIENTED_EDGE ( 'NONE', *, *, #138471, .T. ) ;
#17161 = VERTEX_POINT ( 'NONE', #4327 ) ;
#17163 = ORIENTED_EDGE ( 'NONE', *, *, #156789, .T. ) ;
#17164 = LINE ( 'NONE', #15890, #244964 ) ;
#17165 = VERTEX_POINT ( 'NONE', #42197 ) ;
#17166 = ORIENTED_EDGE ( 'NONE', *, *, #81735, .F. ) ;
#17167 = DIRECTION ( 'NONE',  ( 0.000000000000000000, -1.000000000000000000, 0.000000000000000000 ) ) ;
#17168 = ORIENTED_EDGE ( 'NONE', *, *, #136809, .F. ) ;
#17169 = CARTESIAN_POINT ( 'NONE',  ( -16.94180778212363236, 12.44575456678690806, -211.1890899969216946 ) ) ;
#17171 = CARTESIAN_POINT ( 'NONE',  ( -22.49231231312463208, 64.35001509633539740, -203.5841603721258082 ) ) ;
#17170 = DIRECTION ( 'NONE',  ( -1.000000000000000000, 0.000000000000000000, 0.000000000000000000 ) ) ;
#17172 = ORIENTED_EDGE ( 'NONE', *, *, #250428, .T. ) ;
#17173 = EDGE_CURVE ( 'NONE', #146335, #165316, #82484, .T. ) ;
#17174 = EDGE_LOOP ( 'NONE', ( #78536, #233287, #38461, #47343 ) ) ;
#17175 = FACE_OUTER_BOUND ( 'NONE', #219417, .T. ) ;
#17176 = ORIENTED_EDGE ( 'NONE', *, *, #242687, .T. ) ;
#17177 = TOROIDAL_SURFACE ( 'NONE', #179498, 2.100000000000002309, 0.1000000000000000056 ) ;
#17178 = DIRECTION ( 'NONE',  ( -0.000000000000000000, -0.000000000000000000, -1.000000000000000000 ) ) ;
#17179 = ORIENTED_EDGE ( 'NONE', *, *, #45405, .F. ) ;
#17180 = ORIENTED_EDGE ( 'NONE', *, *, #102635, .T. ) ;
#17181 = EDGE_CURVE ( 'NONE', #50256, #237441, #182503, .T. ) ;
#17182 = DIRECTION ( 'NONE',  ( 0.000000000000000000, 6.982962677686266711E-15, -1.000000000000000000 ) ) ;
#17184 = ORIENTED_EDGE ( 'NONE', *, *, #5513, .F. ) ;
#17183 = CARTESIAN_POINT ( 'NONE',  ( 18.48536876927988715, 85.46352724987978888, -162.9744892194416934 ) ) ;
#17185 = CARTESIAN_POINT ( 'NONE',  ( 23.14999999999999858, 0.000000000000000000, 0.000000000000000000 ) ) ;
#17186 = FACE_OUTER_BOUND ( 'NONE', #80253, .T. ) ;
#17187 = ORIENTED_EDGE ( 'NONE', *, *, #53915, .T. ) ;
#17188 = CARTESIAN_POINT ( 'NONE',  ( -23.15000000000000213, -9.599999999988847676, -143.8939691226524644 ) ) ;
#17189 = DIRECTION ( 'NONE',  ( 0.000000000000000000, 0.2617529984165152257, 0.9651348961777124202 ) ) ;
#17190 = LINE ( 'NONE', #193249, #144448 ) ;
#17191 = ADVANCED_FACE ( 'NONE', ( #181705 ), #160869, .F. ) ;
#17192 = CARTESIAN_POINT ( 'NONE',  ( 18.59999999999999432, -1.736257131586239844, -179.0686523290174819 ) ) ;
#17193 = DIRECTION ( 'NONE',  ( -0.000000000000000000, -0.000000000000000000, 1.000000000000000000 ) ) ;
#17194 = FACE_OUTER_BOUND ( 'NONE', #179496, .T. ) ;
#17195 = DIRECTION ( 'NONE',  ( -7.304098846218134667E-16, -1.000000000000000000, 0.000000000000000000 ) ) ;
#17196 = DIRECTION ( 'NONE',  ( 0.000000000000000000, 0.000000000000000000, -1.000000000000000000 ) ) ;
#17197 = DIRECTION ( 'NONE',  ( -3.265361837132812600E-16, 0.9770955615653313941, 0.2128009952263603677 ) ) ;
#17198 = AXIS2_PLACEMENT_3D ( 'NONE', #165398, #250063, #186246 ) ;
#17199 = ADVANCED_FACE ( 'NONE', ( #64321 ), #115841, .F. ) ;
#17200 = ORIENTED_EDGE ( 'NONE', *, *, #168825, .F. ) ;
#17201 = AXIS2_PLACEMENT_3D ( 'NONE', #151902, #174051, #16245 ) ;
#17202 = AXIS2_PLACEMENT_3D ( 'NONE', #156318, #255324, #139256 ) ;
#17203 = EDGE_CURVE ( 'NONE', #149928, #220244, #143839, .T. ) ;
#17205 = EDGE_LOOP ( 'NONE', ( #51320, #169501, #101134 ) ) ;
#17204 = ORIENTED_EDGE ( 'NONE', *, *, #113665, .T. ) ;
#17206 = ORIENTED_EDGE ( 'NONE', *, *, #130251, .T. ) ;
#17207 = EDGE_CURVE ( 'NONE', #241870, #12552, #100828, .T. ) ;
#17208 = CARTESIAN_POINT ( 'NONE',  ( -18.79999999999999716, 3.461118860469513336, 28.84309995045515507 ) ) ;
#17209 = DIRECTION ( 'NONE',  ( 0.000000000000000000, 6.982962677686266711E-15, -1.000000000000000000 ) ) ;
#17210 = EDGE_CURVE ( 'NONE', #33088, #183270, #145121, .T. ) ;
#17212 = DIRECTION ( 'NONE',  ( -0.7071067811865474617, -0.7071067811865474617, -0.000000000000000000 ) ) ;
#17211 = CARTESIAN_POINT ( 'NONE',  ( -18.59999999999999787, 45.93315328338058379, -256.6017782078560003 ) ) ;
#17213 = ORIENTED_EDGE ( 'NONE', *, *, #188524, .T. ) ;
#17214 = DIRECTION ( 'NONE',  ( 1.000000000000000000, -0.000000000000000000, 0.000000000000000000 ) ) ;
#17215 = CARTESIAN_POINT ( 'NONE',  ( -23.24999999999999645, 85.60000000001166143, -62.82291809330219223 ) ) ;
#17216 = EDGE_CURVE ( 'NONE', #68656, #125839, #164709, .T. ) ;
#17218 = AXIS2_PLACEMENT_3D ( 'NONE', #196053, #216878, #99481 ) ;
#17217 = DIRECTION ( 'NONE',  ( 1.000000000000000000, -0.000000000000000000, 0.000000000000000000 ) ) ;
#17219 = DIRECTION ( 'NONE',  ( 0.000000000000000000, -0.8660254037844384856, 0.5000000000000002220 ) ) ;
#17220 = EDGE_LOOP ( 'NONE', ( #109483, #29980, #159103, #144460 ) ) ;
#17221 = ORIENTED_EDGE ( 'NONE', *, *, #85558, .T. ) ;
#17222 = FACE_OUTER_BOUND ( 'NONE', #14723, .T. ) ;
#17223 = B_SPLINE_CURVE_WITH_KNOTS ( 'NONE', 3,
 ( #105559, #146000, #229407, #209840, #225513, #208572, #89872, #169469 ),
 .UNSPECIFIED., .F., .F.,
 ( 4, 2, 2, 4 ),
 ( 0.000000000000000000, 0.0001049670497870137855, 0.0002099340995740275710, 0.0004198681991480551420 ),
 .UNSPECIFIED. ) ;
#17224 = EDGE_LOOP ( 'NONE', ( #188080, #172234, #120444, #128689 ) ) ;
#17225 = CARTESIAN_POINT ( 'NONE',  ( 18.60000000000000142, -7.631834139420945462, -210.1304494778855769 ) ) ;
#17226 = CARTESIAN_POINT ( 'NONE',  ( 21.05000000000000071, 85.00000000001251976, -179.9170766071767389 ) ) ;
#17227 = DIRECTION ( 'NONE',  ( -0.000000000000000000, -0.000000000000000000, 1.000000000000000000 ) ) ;
#17228 = LINE ( 'NONE', #231458, #68608 ) ;
#17229 = DIRECTION ( 'NONE',  ( 0.000000000000000000, 0.000000000000000000, 1.000000000000000000 ) ) ;
#17230 = CARTESIAN_POINT ( 'NONE',  ( -23.15000000000000213, 19.28991295610541812, -237.9781866380819793 ) ) ;
#17231 = ORIENTED_EDGE ( 'NONE', *, *, #234512, .T. ) ;
#17232 = DIRECTION ( 'NONE',  ( 0.000000000000000000, -0.4088369013363281068, 0.9126074666063770380 ) ) ;
#17233 = CARTESIAN_POINT ( 'NONE',  ( 20.94999999999999929, 81.86853375790846599, -214.9828603846715964 ) ) ;
#17235 = EDGE_CURVE ( 'NONE', #23645, #221894, #142556, .T. ) ;
#17234 = CARTESIAN_POINT ( 'NONE',  ( -20.15000000000000568, 66.70857864377474300, -124.1731074845243654 ) ) ;
#17238 = CARTESIAN_POINT ( 'NONE',  ( 20.94999999999999574, 77.16270174995034381, -161.9231074845243370 ) ) ;
#17237 = CIRCLE ( 'NONE', #46421, 0.09999999999999761857 ) ;
#17236 = DIRECTION ( 'NONE',  ( 0.000000000000000000, 1.000000000000000000, -6.938893903907270030E-14 ) ) ;
#17240 = DIRECTION ( 'NONE',  ( 1.000000000000000000, 1.836970198721029934E-16, 0.000000000000000000 ) ) ;
#17239 = AXIS2_PLACEMENT_3D ( 'NONE', #115784, #171950, #239589 ) ;
#17241 = VECTOR ( 'NONE', #140400, 1000.000000000000000 ) ;
#17242 = CARTESIAN_POINT ( 'NONE',  ( -23.25000000000000000, 85.60000000001231513, -160.1291383618718385 ) ) ;
#17243 = CARTESIAN_POINT ( 'NONE',  ( -20.94999999999999929, 16.44800918141279666, -240.8068063186265135 ) ) ;
#17244 = DIRECTION ( 'NONE',  ( 0.7071067811865463515, 0.7071067811865487940, 7.587431340288849180E-16 ) ) ;
#17245 = VERTEX_POINT ( 'NONE', #224666 ) ;
#17246 = ORIENTED_EDGE ( 'NONE', *, *, #20975, .T. ) ;
#17247 = EDGE_CURVE ( 'NONE', #46680, #144467, #90884, .T. ) ;
#17248 = CARTESIAN_POINT ( 'NONE',  ( -18.59999999999999787, 43.08613539620618837, -254.3146655184800409 ) ) ;
#17249 = EDGE_LOOP ( 'NONE', ( #223439, #248896, #88222, #251591 ) ) ;
#17250 = CARTESIAN_POINT ( 'NONE',  ( -23.25000000000000000, -7.274670914976377745, -212.7102428701827250 ) ) ;
#17251 = AXIS2_PLACEMENT_3D ( 'NONE', #196557, #62196, #158752 ) ;
#17252 = CARTESIAN_POINT ( 'NONE',  ( -23.25000000000000000, 56.02567683926420727, -227.9999002286038774 ) ) ;
#17253 = ORIENTED_EDGE ( 'NONE', *, *, #252209, .T. ) ;
#17254 = EDGE_CURVE ( 'NONE', #38617, #201868, #149187, .T. ) ;
#17255 = CARTESIAN_POINT ( 'NONE',  ( 21.09610168723072832, 0.03358950690265592037, -161.1210442847751665 ) ) ;
#17256 = CARTESIAN_POINT ( 'NONE',  ( 21.05000000000000071, 11.65000000001116298, -93.48519422934610645 ) ) ;
#17257 = DIRECTION ( 'NONE',  ( 0.000000000000000000, 0.000000000000000000, -1.000000000000000000 ) ) ;
#17258 = CARTESIAN_POINT ( 'NONE',  ( 18.49999999999999289, 10.49142135624846439, -192.3499999999999659 ) ) ;
#17260 = ORIENTED_EDGE ( 'NONE', *, *, #138465, .F. ) ;
#17259 = CARTESIAN_POINT ( 'NONE',  ( -16.87683809663752399, 9.850000000011139178, -187.5976359818036485 ) ) ;
#17262 = DIRECTION ( 'NONE',  ( 0.000000000000000000, 6.982962677686266711E-15, -1.000000000000000000 ) ) ;
#17261 = DIRECTION ( 'NONE',  ( -0.000000000000000000, -0.000000000000000000, 1.000000000000000000 ) ) ;
#17264 = CARTESIAN_POINT ( 'NONE',  ( 19.88284271247461987, 64.30857864377418309, -44.77310748452440237 ) ) ;
#17263 = AXIS2_PLACEMENT_3D ( 'NONE', #87196, #23425, #83331 ) ;
#17265 = ADVANCED_FACE ( 'NONE', ( #46031 ), #39882, .T. ) ;
#17266 = CARTESIAN_POINT ( 'NONE',  ( -18.59999999999999787, 77.85102823015347440, -191.8691942151018566 ) ) ;
#17267 = CARTESIAN_POINT ( 'NONE',  ( 18.52351027002949380, 87.06367156776640570, -199.5660463946405514 ) ) ;
#17268 = EDGE_LOOP ( 'NONE', ( #2749, #239736, #115345, #218782, #225574, #246458, #234271, #215721, #146737, #132893 ) ) ;
#17269 = AXIS2_PLACEMENT_3D ( 'NONE', #117967, #59228, #236618 ) ;
#17270 = EDGE_CURVE ( 'NONE', #173345, #168528, #70070, .T. ) ;
#17271 = CARTESIAN_POINT ( 'NONE',  ( -23.25000000000000000, 67.23127455305835554, -235.8551265064784559 ) ) ;
#17272 = EDGE_CURVE ( 'NONE', #256678, #204385, #229806, .T. ) ;
#17273 = VERTEX_POINT ( 'NONE', #168609 ) ;
#17274 = AXIS2_PLACEMENT_3D ( 'NONE', #209488, #154685, #12604 ) ;
#17275 = CARTESIAN_POINT ( 'NONE',  ( 23.24999999999999645, 45.89348038176515843, -239.2231437130149061 ) ) ;
#17276 = ORIENTED_EDGE ( 'NONE', *, *, #28442, .T. ) ;
#17277 = CARTESIAN_POINT ( 'NONE',  ( 23.24999999999999289, 66.54223038922117439, -213.7542166125332415 ) ) ;
#17278 = AXIS2_PLACEMENT_3D ( 'NONE', #181476, #41968, #39411 ) ;
#17279 = EDGE_CURVE ( 'NONE', #119976, #71875, #57558, .T. ) ;
#17281 = DIRECTION ( 'NONE',  ( -1.000000000000000000, -0.000000000000000000, 0.000000000000000000 ) ) ;
#17280 = CIRCLE ( 'NONE', #21381, 7.720710678118662074 ) ;
#17282 = PLANE ( 'NONE',  #78572 ) ;
#17283 = EDGE_LOOP ( 'NONE', ( #74086, #36358, #11967, #24862 ) ) ;
#17284 = ORIENTED_EDGE ( 'NONE', *, *, #90939, .F. ) ;
#17285 = CIRCLE ( 'NONE', #154669, 0.09999999999999939493 ) ;
#17286 = DIRECTION ( 'NONE',  ( 1.000000000000000000, 0.000000000000000000, -0.000000000000000000 ) ) ;
#17287 = DIRECTION ( 'NONE',  ( 0.000000000000000000, -0.1350103645451974088, 0.9908441862701587999 ) ) ;
#17288 = CARTESIAN_POINT ( 'NONE',  ( -16.87683809663752399, 62.98531230502843670, -213.8799296553602005 ) ) ;
#17289 = DIRECTION ( 'NONE',  ( -3.265361837132813093E-16, -0.4088369013363053472, 0.9126074666063872520 ) ) ;
#17291 = CARTESIAN_POINT ( 'NONE',  ( 20.04142135623730070, 64.25000000001250555, -178.8731074845244393 ) ) ;
#17290 = CYLINDRICAL_SURFACE ( 'NONE', #149113, 0.1000000000000024342 ) ;
#17292 = CIRCLE ( 'NONE', #29796, 0.1000000000000028644 ) ;
#17293 = LINE ( 'NONE', #241467, #60853 ) ;
#17294 = CARTESIAN_POINT ( 'NONE',  ( 13.12229106158772751, 9.430637101707892711, -51.76826061806093549 ) ) ;
#17296 = DIRECTION ( 'NONE',  ( -1.000000000000000000, -1.836970198721029934E-16, 0.000000000000000000 ) ) ;
#17295 = CIRCLE ( 'NONE', #42231, 0.09999999999999938105 ) ;
#17297 = ORIENTED_EDGE ( 'NONE', *, *, #239817, .F. ) ;
#17298 = LINE ( 'NONE', #152982, #73068 ) ;
#17300 = EDGE_LOOP ( 'NONE', ( #59593, #211163, #127519, #111959 ) ) ;
#17299 = FACE_OUTER_BOUND ( 'NONE', #84154, .T. ) ;
#17301 = LINE ( 'NONE', #138486, #126885 ) ;
#17302 = CARTESIAN_POINT ( 'NONE',  ( -18.59999999999999787, 1.250000000011155299, -108.5000000000000426 ) ) ;
#17304 = FACE_OUTER_BOUND ( 'NONE', #194484, .T. ) ;
#17303 = DIRECTION ( 'NONE',  ( 1.000000000000000000, 0.000000000000000000, 0.000000000000000000 ) ) ;
#17305 = CIRCLE ( 'NONE', #175522, 0.4000000000000045186 ) ;
#17306 = ADVANCED_FACE ( 'NONE', ( #30345, #105986 ), #186852, .T. ) ;
#17307 = EDGE_LOOP ( 'NONE', ( #109049, #160124, #146554, #241321, #188780, #181521, #137982, #122356, #169313, #97415, #125828, #203504, #148462, #217882, #31061, #129330, #143807, #22161, #55229, #237576, #49712, #143657, #110303, #180685, #227848 ) ) ;
#17309 = DIRECTION ( 'NONE',  ( -2.557131231893037478E-16, -0.8660254037844420383, 0.4999999999999941713 ) ) ;
#17308 = CARTESIAN_POINT ( 'NONE',  ( -20.94999999999999929, 68.92903212821283887, -65.77654326265606244 ) ) ;
#17311 = ADVANCED_FACE ( 'NONE', ( #130704 ), #108583, .T. ) ;
#17310 = CARTESIAN_POINT ( 'NONE',  ( -23.15000000000000213, 1.115600667400684642E-11, -134.0000000000000284 ) ) ;
#17312 = LINE ( 'NONE', #118977, #126142 ) ;
#17313 = DIRECTION ( 'NONE',  ( 0.000000000000000000, 6.467318590049456648E-15, -1.000000000000000000 ) ) ;
#17315 = LINE ( 'NONE', #197212, #178360 ) ;
#17314 = CIRCLE ( 'NONE', #104734, 12.77500000000000568 ) ;
#17316 = VERTEX_POINT ( 'NONE', #210266 ) ;
#17317 = DIRECTION ( 'NONE',  ( -1.000000000000000000, 0.000000000000000000, 0.000000000000000000 ) ) ;
#17318 = ORIENTED_EDGE ( 'NONE', *, *, #163785, .T. ) ;
#17319 = EDGE_CURVE ( 'NONE', #216189, #31617, #12076, .T. ) ;
#17320 = EDGE_LOOP ( 'NONE', ( #221282, #67946, #155969, #165082, #180171, #192692 ) ) ;
#17322 = CARTESIAN_POINT ( 'NONE',  ( -20.94999999999999929, 46.32970330538243786, -243.0551226933711746 ) ) ;
#17321 = AXIS2_PLACEMENT_3D ( 'NONE', #176102, #118686, #80798 ) ;
#17323 = AXIS2_PLACEMENT_3D ( 'NONE', #176056, #117341, #196860 ) ;
#17324 = VERTEX_POINT ( 'NONE', #68172 ) ;
#17325 = CIRCLE ( 'NONE', #179819, 6.258578643762722216 ) ;
#17326 = DIRECTION ( 'NONE',  ( 1.000000000000000000, -0.000000000000000000, -0.000000000000000000 ) ) ;
#17327 = CYLINDRICAL_SURFACE ( 'NONE', #230335, 0.09999999999999939493 ) ;
#17328 = EDGE_LOOP ( 'NONE', ( #78792, #83146, #212480, #141607 ) ) ;
#17329 = DIRECTION ( 'NONE',  ( 0.000000000000000000, 0.000000000000000000, 1.000000000000000000 ) ) ;
#17330 = DIRECTION ( 'NONE',  ( -1.000000000000000000, 0.000000000000000000, 0.000000000000000000 ) ) ;
#17331 = DIRECTION ( 'NONE',  ( 0.000000000000000000, 4.336808689942494997E-15, -1.000000000000000000 ) ) ;
#17332 = DIRECTION ( 'NONE',  ( 1.000000000000000000, 0.000000000000000000, 0.000000000000000000 ) ) ;
#17333 = DIRECTION ( 'NONE',  ( 0.000000000000000000, 0.000000000000000000, 1.000000000000000000 ) ) ;
#17334 = ADVANCED_FACE ( 'NONE', ( #249391 ), #205091, .F. ) ;
#17335 = VERTEX_POINT ( 'NONE', #185551 ) ;
#17336 = CARTESIAN_POINT ( 'NONE',  ( 20.95000000000005613, 67.82483145523551116, -25.59432346794077162 ) ) ;
#17337 = ORIENTED_EDGE ( 'NONE', *, *, #54937, .F. ) ;
#17339 = VERTEX_POINT ( 'NONE', #225923 ) ;
#17338 = CARTESIAN_POINT ( 'NONE',  ( 21.05000000000000071, 11.27293161222461748, -225.9964495734431864 ) ) ;
#17340 = VERTEX_POINT ( 'NONE', #245537 ) ;
#17341 = DIRECTION ( 'NONE',  ( -0.000000000000000000, 0.9910827722268049644, 0.1332476588733589318 ) ) ;
#17342 = DIRECTION ( 'NONE',  ( 0.000000000000000000, 1.000000000000000000, 6.853228547068871147E-15 ) ) ;
#17343 = DIRECTION ( 'NONE',  ( -2.840903330521631775E-16, 0.8700118002898321601, -0.4930308989875230030 ) ) ;
#17344 = DIRECTION ( 'NONE',  ( 0.000000000000000000, 1.000000000000000000, 0.000000000000000000 ) ) ;
#17345 = ORIENTED_EDGE ( 'NONE', *, *, #139454, .F. ) ;
#17346 = EDGE_CURVE ( 'NONE', #167339, #26064, #145051, .T. ) ;
#17347 = CARTESIAN_POINT ( 'NONE',  ( -16.84421487269769102, 9.950000000011135270, -146.6695021224449533 ) ) ;
#17348 = DIRECTION ( 'NONE',  ( 0.000000000000000000, 1.000000000000000000, -6.308085367188393199E-16 ) ) ;
#17350 = ORIENTED_EDGE ( 'NONE', *, *, #253780, .F. ) ;
#17349 = AXIS2_PLACEMENT_3D ( 'NONE', #228809, #192255, #50144 ) ;
#17351 = EDGE_CURVE ( 'NONE', #216955, #19089, #194599, .T. ) ;
#17353 = EDGE_LOOP ( 'NONE', ( #86560, #58983, #96955, #119435 ) ) ;
#17352 = DIRECTION ( 'NONE',  ( 0.000000000000000000, 6.938893903907222067E-15, -1.000000000000000000 ) ) ;
#17354 = CARTESIAN_POINT ( 'NONE',  ( -16.77683809663752257, 9.945835743204147761, -20.83605098089580210 ) ) ;
#17355 = EDGE_CURVE ( 'NONE', #103163, #211446, #27797, .T. ) ;
#17356 = CARTESIAN_POINT ( 'NONE',  ( 18.79999999999999716, 11.75000000000000000, -7.800000000000000711 ) ) ;
#17357 = EDGE_CURVE ( 'NONE', #182190, #41483, #202937, .T. ) ;
#17358 = VECTOR ( 'NONE', #256084, 1000.000000000000000 ) ;
#17359 = CARTESIAN_POINT ( 'NONE',  ( 22.50000000000000000, 1.115600667400684642E-11, -100.5000000000000284 ) ) ;
#17361 = EDGE_CURVE ( 'NONE', #133367, #160229, #227884, .T. ) ;
#17360 = EDGE_LOOP ( 'NONE', ( #243242, #146343, #104824 ) ) ;
#17362 = CYLINDRICAL_SURFACE ( 'NONE', #208655, 0.8750000000000007772 ) ;
#17363 = DIRECTION ( 'NONE',  ( -1.000000000000000000, -0.000000000000000000, 0.000000000000000000 ) ) ;
#17364 = CARTESIAN_POINT ( 'NONE',  ( 12.93279065517212345, 66.58230930894843880, -51.38150678775981106 ) ) ;
#17365 = CARTESIAN_POINT ( 'NONE',  ( -21.65000000000000213, 9.950000000011140600, -87.75000000000005684 ) ) ;
#17366 = CIRCLE ( 'NONE', #200516, 0.1000000000000028644 ) ;
#17367 = AXIS2_PLACEMENT_3D ( 'NONE', #60460, #160882, #196138 ) ;
#17368 = EDGE_CURVE ( 'NONE', #179805, #116279, #148787, .T. ) ;
#17369 = ADVANCED_FACE ( 'NONE', ( #193266 ), #14644, .F. ) ;
#17371 = ORIENTED_EDGE ( 'NONE', *, *, #203827, .F. ) ;
#17370 = AXIS2_PLACEMENT_3D ( 'NONE', #161654, #24717, #6398 ) ;
#17372 = CARTESIAN_POINT ( 'NONE',  ( -18.59999999999999787, 74.83909925395606422, -233.7225145625711491 ) ) ;
#17373 = ORIENTED_EDGE ( 'NONE', *, *, #205926, .F. ) ;
#17374 = SPHERICAL_SURFACE ( 'NONE', #72859, 0.1000000000000000056 ) ;
#17375 = ADVANCED_FACE ( 'NONE', ( #134544 ), #177587, .T. ) ;
#17376 = DIRECTION ( 'NONE',  ( 0.000000000000000000, 0.4999999999999348299, -0.8660254037844762331 ) ) ;
#17378 = ORIENTED_EDGE ( 'NONE', *, *, #69726, .T. ) ;
#17377 =( BOUNDED_CURVE ( )  B_SPLINE_CURVE ( 3, ( #125808, #12318, #171408, #247033 ),
 .UNSPECIFIED., .F., .F. ) 
 B_SPLINE_CURVE_WITH_KNOTS ( ( 4, 4 ),
 ( 4.712388980384689674, 6.231880751915386263 ),
 .UNSPECIFIED. ) 
 CURVE ( )  GEOMETRIC_REPRESENTATION_ITEM ( )  RATIONAL_B_SPLINE_CURVE ( ( 1.000000000000000000, 0.8166740347213228279, 0.8166740347213228279, 1.000000000000000000 ) ) 
 REPRESENTATION_ITEM ( '' )  );
#17379 = CARTESIAN_POINT ( 'NONE',  ( -23.25000000000000000, 1.115626384983466906E-11, -165.4000000000000341 ) ) ;
#17380 = DIRECTION ( 'NONE',  ( 1.000000000000000000, -0.000000000000000000, -0.000000000000000000 ) ) ;
#17381 = DIRECTION ( 'NONE',  ( 0.000000000000000000, -7.086529944415894657E-15, 1.000000000000000000 ) ) ;
#17382 = FACE_OUTER_BOUND ( 'NONE', #92491, .T. ) ;
#17383 = FACE_OUTER_BOUND ( 'NONE', #92708, .T. ) ;
#17385 = EDGE_CURVE ( 'NONE', #77226, #118476, #56296, .T. ) ;
#17384 = CARTESIAN_POINT ( 'NONE',  ( -18.47079683080343315, 85.47166410525701963, -129.4142469435320209 ) ) ;
#17387 = ORIENTED_EDGE ( 'NONE', *, *, #37533, .F. ) ;
#17386 = DIRECTION ( 'NONE',  ( 1.073024830501117725E-15, 0.000000000000000000, 1.000000000000000000 ) ) ;
#17388 = CIRCLE ( 'NONE', #21493, 0.1000000000000028644 ) ;
#17389 = EDGE_CURVE ( 'NONE', #15908, #137320, #95437, .T. ) ;
#17390 = CARTESIAN_POINT ( 'NONE',  ( -23.25000000000000000, 1.115600667400684642E-11, -138.0500000000000114 ) ) ;
#17392 = EDGE_CURVE ( 'NONE', #55645, #208604, #241152, .T. ) ;
#17391 = CARTESIAN_POINT ( 'NONE',  ( 20.94999999999999574, -1.162701749926853712, -41.60000000000000142 ) ) ;
#17393 = LINE ( 'NONE', #257230, #230458 ) ;
#17394 = ORIENTED_EDGE ( 'NONE', *, *, #28833, .T. ) ;
#17395 = DIRECTION ( 'NONE',  ( 0.000000000000000000, 0.000000000000000000, -1.000000000000000000 ) ) ;
#17396 = AXIS2_PLACEMENT_3D ( 'NONE', #94308, #130872, #248261 ) ;
#17397 = CARTESIAN_POINT ( 'NONE',  ( -18.60000000000000142, 85.32100840337290037, -62.28716923544637751 ) ) ;
#17398 = VECTOR ( 'NONE', #134940, 1000.000000000000000 ) ;
#17399 = EDGE_CURVE ( 'NONE', #195135, #51112, #36791, .T. ) ;
#17400 = EDGE_LOOP ( 'NONE', ( #104660, #73171, #232660, #208778 ) ) ;
#17401 = CARTESIAN_POINT ( 'NONE',  ( 18.59999999999999432, 1.162701749949165642, -142.0000000000000284 ) ) ;
#17402 = CARTESIAN_POINT ( 'NONE',  ( 23.14999999999999503, 11.65000000001116298, -112.7500000000000284 ) ) ;
#17403 = ORIENTED_EDGE ( 'NONE', *, *, #240845, .F. ) ;
#17404 = DIRECTION ( 'NONE',  ( -0.7071067811865475727, 0.7071067811865475727, 4.937700262164531476E-15 ) ) ;
#17405 = ORIENTED_EDGE ( 'NONE', *, *, #132700, .F. ) ;
#17407 = EDGE_CURVE ( 'NONE', #120569, #207660, #257032, .T. ) ;
#17406 = FACE_OUTER_BOUND ( 'NONE', #214394, .T. ) ;
#17408 = ORIENTED_EDGE ( 'NONE', *, *, #151110, .F. ) ;
#17409 = CIRCLE ( 'NONE', #250630, 0.1999999999999866329 ) ;
#17410 = DIRECTION ( 'NONE',  ( 0.000000000000000000, 1.000000000000000000, -0.000000000000000000 ) ) ;
#17411 = EDGE_LOOP ( 'NONE', ( #172090, #174480, #101206 ) ) ;
#17412 = FACE_OUTER_BOUND ( 'NONE', #209980, .T. ) ;
#17413 = ORIENTED_EDGE ( 'NONE', *, *, #127127, .T. ) ;
#17415 = VERTEX_POINT ( 'NONE', #231123 ) ;
#17414 = ORIENTED_EDGE ( 'NONE', *, *, #170281, .T. ) ;
#17416 = DIRECTION ( 'NONE',  ( 0.000000000000000000, 0.8814952561688442767, -0.4721928772777324035 ) ) ;
#17417 = ORIENTED_EDGE ( 'NONE', *, *, #65045, .F. ) ;
#17418 = DIRECTION ( 'NONE',  ( 1.000000000000000000, 0.000000000000000000, -0.000000000000000000 ) ) ;
#17419 = ORIENTED_EDGE ( 'NONE', *, *, #19029, .T. ) ;
#17420 = VERTEX_POINT ( 'NONE', #35504 ) ;
#17421 = CARTESIAN_POINT ( 'NONE',  ( -20.54999999999999716, 76.00000000001190870, -103.0231074845243029 ) ) ;
#17423 = CARTESIAN_POINT ( 'NONE',  ( 21.14999999999998082, 41.46275801244657799, -260.2743004338703940 ) ) ;
#17422 = TOROIDAL_SURFACE ( 'NONE', #88128, 0.6000000000000017542, 0.1000000000000000056 ) ;
#17424 = CARTESIAN_POINT ( 'NONE',  ( 18.39999999999999147, 67.17743825834548943, -93.77310748452437394 ) ) ;
#17425 = CARTESIAN_POINT ( 'NONE',  ( -20.94999999999999929, -1.835341550213255957, -145.6551512925629766 ) ) ;
#17426 = ORIENTED_EDGE ( 'NONE', *, *, #226224, .F. ) ;
#17427 = CARTESIAN_POINT ( 'NONE',  ( 21.07928932188134397, 1.115600667400684642E-11, -100.5000000000000284 ) ) ;
#17428 = CARTESIAN_POINT ( 'NONE',  ( 21.05000000000000071, 30.73075574124490217, -252.3164853687435709 ) ) ;
#17429 = CARTESIAN_POINT ( 'NONE',  ( -20.65000000000000568, 5.650000000011139001, -180.1499999999999773 ) ) ;
#17430 = VECTOR ( 'NONE', #136849, 1000.000000000000000 ) ;
#17431 = ORIENTED_EDGE ( 'NONE', *, *, #239855, .F. ) ;
#17432 = DIRECTION ( 'NONE',  ( 0.000000000000000000, 0.2617529984165152257, 0.9651348961777124202 ) ) ;
#17433 = CARTESIAN_POINT ( 'NONE',  ( -18.43634282235085564, 37.95953089239920075, -261.2289615770415594 ) ) ;
#17434 = CARTESIAN_POINT ( 'NONE',  ( 20.94999999999999929, -1.135018845899022466, -141.7169768834323520 ) ) ;
#17435 = VECTOR ( 'NONE', #68397, 1000.000000000000000 ) ;
#17436 = VERTEX_POINT ( 'NONE', #52441 ) ;
#17437 = CARTESIAN_POINT ( 'NONE',  ( -16.91247567987038636, 66.04091731634262885, -90.39438302598703956 ) ) ;
#17438 = VERTEX_POINT ( 'NONE', #34213 ) ;
#17439 = ORIENTED_EDGE ( 'NONE', *, *, #117959, .T. ) ;
#17440 = CIRCLE ( 'NONE', #204687, 0.1000000000000028644 ) ;
#17441 = DIRECTION ( 'NONE',  ( 0.000000000000000000, 0.4088369013363281068, -0.9126074666063770380 ) ) ;
#17442 = ORIENTED_EDGE ( 'NONE', *, *, #29178, .F. ) ;
#17443 = AXIS2_PLACEMENT_3D ( 'NONE', #205842, #227976, #27243 ) ;
#17444 = ORIENTED_EDGE ( 'NONE', *, *, #29263, .F. ) ;
#17445 = CARTESIAN_POINT ( 'NONE',  ( -16.87036670365548474, 10.08494996326643189, -121.4500000000000313 ) ) ;
#17446 = CARTESIAN_POINT ( 'NONE',  ( -16.93860193097148326, 9.993107767340401182, -188.4001383673068233 ) ) ;
#17447 = ORIENTED_EDGE ( 'NONE', *, *, #84055, .F. ) ;
#17448 = ORIENTED_EDGE ( 'NONE', *, *, #158154, .F. ) ;
#17449 = CARTESIAN_POINT ( 'NONE',  ( -23.25000000000000000, 85.00000000001253397, -179.3170766071767446 ) ) ;
#17450 = VECTOR ( 'NONE', #105361, 1000.000000000000000 ) ;
#17451 = DIRECTION ( 'NONE',  ( 0.000000000000000000, 0.000000000000000000, 1.000000000000000000 ) ) ;
#17453 = ORIENTED_EDGE ( 'NONE', *, *, #250870, .F. ) ;
#17452 = CIRCLE ( 'NONE', #163213, 11.79999999999999716 ) ;
#17454 = EDGE_CURVE ( 'NONE', #221551, #206051, #190497, .T. ) ;
#17455 = ORIENTED_EDGE ( 'NONE', *, *, #90033, .F. ) ;
#17456 = CIRCLE ( 'NONE', #133982, 12.87499999999999822 ) ;
#17457 = ORIENTED_EDGE ( 'NONE', *, *, #150697, .T. ) ;
#17458 = CARTESIAN_POINT ( 'NONE',  ( 20.94999999999999929, -9.499999999988848032, -110.3939691226524786 ) ) ;
#17460 =( BOUNDED_CURVE ( )  B_SPLINE_CURVE ( 3, ( #10606, #90112, #169715, #191834 ),
 .UNSPECIFIED., .F., .F. ) 
 B_SPLINE_CURVE_WITH_KNOTS ( ( 4, 4 ),
 ( 4.712388980384689674, 5.672655318024675708 ),
 .UNSPECIFIED. ) 
 CURVE ( )  GEOMETRIC_REPRESENTATION_ITEM ( )  RATIONAL_B_SPLINE_CURVE ( ( 1.000000000000000000, 0.9246222802177378464, 0.9246222802177378464, 1.000000000000000000 ) ) 
 REPRESENTATION_ITEM ( '' )  );
#17459 = AXIS2_PLACEMENT_3D ( 'NONE', #55700, #79139, #157452 ) ;
#17461 = DIRECTION ( 'NONE',  ( -0.8660254037843277963, 0.000000000000000000, -0.5000000000001921796 ) ) ;
#17462 = CIRCLE ( 'NONE', #163239, 0.09999999999999543976 ) ;
#17463 = DIRECTION ( 'NONE',  ( -0.000000000000000000, 1.000000000000000000, -0.000000000000000000 ) ) ;
#17464 = CARTESIAN_POINT ( 'NONE',  ( 20.85000000000000142, 76.00000000001213607, -136.5231074845243313 ) ) ;
#17465 = CARTESIAN_POINT ( 'NONE',  ( -15.55912972643741199, 67.50912972644930221, -90.37310748452436826 ) ) ;
#17466 = EDGE_CURVE ( 'NONE', #243985, #248236, #228468, .T. ) ;
#17467 = CARTESIAN_POINT ( 'NONE',  ( -22.49231231312463208, 11.64998490368843953, -66.93894711239866524 ) ) ;
#17468 = CARTESIAN_POINT ( 'NONE',  ( -21.65000000000000213, 68.25000000001158185, -57.17310748452437963 ) ) ;
#17470 = CARTESIAN_POINT ( 'NONE',  ( -23.39999999999994529, 83.80000000001119531, -34.86056257560453986 ) ) ;
#17469 = CARTESIAN_POINT ( 'NONE',  ( 23.14999999999999858, 1.115649653272650466E-11, -163.5000000000000284 ) ) ;
#17471 = CARTESIAN_POINT ( 'NONE',  ( 21.13736287352038445, 67.95335762362780940, -82.17310748452437963 ) ) ;
#17472 = CARTESIAN_POINT ( 'NONE',  ( -23.25000000000000355, 70.35000000001255671, -182.6731074845243938 ) ) ;
#17473 = DIRECTION ( 'NONE',  ( 0.000000000000000000, 0.9126074666063772600, 0.4088369013363274962 ) ) ;
#17474 = AXIS2_PLACEMENT_3D ( 'NONE', #171346, #194733, #193441 ) ;
#17475 = CARTESIAN_POINT ( 'NONE',  ( 21.05543885634738643, 44.19062562409153117, -236.5609025269668848 ) ) ;
#17477 = ORIENTED_EDGE ( 'NONE', *, *, #209843, .F. ) ;
#17476 = CIRCLE ( 'NONE', #138269, 0.1000000000000028644 ) ;
#17478 = AXIS2_PLACEMENT_3D ( 'NONE', #131396, #212243, #252620 ) ;
#17479 = EDGE_CURVE ( 'NONE', #183861, #165380, #244356, .T. ) ;
#17481 = ORIENTED_EDGE ( 'NONE', *, *, #93584, .T. ) ;
#17480 = CARTESIAN_POINT ( 'NONE',  ( -21.14999999999999858, -3.275978944802464099, -228.2735455795363748 ) ) ;
#17482 = ADVANCED_FACE ( 'NONE', ( #232408 ), #113717, .F. ) ;
#17483 = FACE_OUTER_BOUND ( 'NONE', #76390, .T. ) ;
#17484 = EDGE_CURVE ( 'NONE', #77128, #125903, #119851, .T. ) ;
#17485 = DIRECTION ( 'NONE',  ( 1.000000000000000000, 1.875376730785737719E-16, 0.000000000000000000 ) ) ;
#17486 = ORIENTED_EDGE ( 'NONE', *, *, #116193, .T. ) ;
#17487 = DIRECTION ( 'NONE',  ( -1.000000000000000000, 0.000000000000000000, -0.000000000000000000 ) ) ;
#17488 = EDGE_CURVE ( 'NONE', #56714, #129778, #19775, .T. ) ;
#17489 = CARTESIAN_POINT ( 'NONE',  ( -16.89797118371616591, 66.02361927736852465, -157.4604008520840921 ) ) ;
#17490 = VECTOR ( 'NONE', #170886, 1000.000000000000000 ) ;
#17491 = ORIENTED_EDGE ( 'NONE', *, *, #130543, .F. ) ;
#17492 = FACE_OUTER_BOUND ( 'NONE', #201872, .T. ) ;
#17493 = DIRECTION ( 'NONE',  ( -1.000000000000000000, 0.000000000000000000, 0.000000000000000000 ) ) ;
#17494 = EDGE_CURVE ( 'NONE', #1482, #105325, #115446, .T. ) ;
#17495 = DIRECTION ( 'NONE',  ( 0.000000000000000000, -0.9126074666063545004, -0.4088369013363783999 ) ) ;
#17497 = EDGE_LOOP ( 'NONE', ( #170548, #233066, #176917 ) ) ;
#17496 = CARTESIAN_POINT ( 'NONE',  ( 18.49999999999999289, 64.35000000001177511, -78.17310748452437963 ) ) ;
#17499 = VERTEX_POINT ( 'NONE', #122732 ) ;
#17498 = CARTESIAN_POINT ( 'NONE',  ( -18.46154800491001424, 85.48020627425391638, -96.36565664614275306 ) ) ;
#17500 = CYLINDRICAL_SURFACE ( 'NONE', #224841, 0.09999999999999939493 ) ;
#17501 = DIRECTION ( 'NONE',  ( 2.952720810173288619E-16, -1.000000000000000000, 0.000000000000000000 ) ) ;
#17502 = CARTESIAN_POINT ( 'NONE',  ( 18.54999999999999716, 67.25000000001222134, -149.1731074845244223 ) ) ;
#17504 = EDGE_CURVE ( 'NONE', #12856, #81812, #221775, .T. ) ;
#17503 = CARTESIAN_POINT ( 'NONE',  ( -14.23072895065542731, 9.455987233623897481, -182.5115311668977824 ) ) ;
#17506 = DIRECTION ( 'NONE',  ( 0.000000000000000000, 0.000000000000000000, -1.000000000000000000 ) ) ;
#17505 = CARTESIAN_POINT ( 'NONE',  ( -20.94999999999999929, 76.00000000001244871, -170.0231074845243597 ) ) ;
#17507 = CARTESIAN_POINT ( 'NONE',  ( -23.15000000000000213, 64.25000000001146816, -42.86470817442146597 ) ) ;
#17508 = DIRECTION ( 'NONE',  ( 0.000000000000000000, -1.000000000000000000, 0.000000000000000000 ) ) ;
#17509 = CARTESIAN_POINT ( 'NONE',  ( -21.04999999999994387, 76.00000000001119815, -36.02310748452479316 ) ) ;
#17510 = CARTESIAN_POINT ( 'NONE',  ( 21.07933241753356768, 10.03486121375300222, -228.1099367534912687 ) ) ;
#17511 = EDGE_LOOP ( 'NONE', ( #247274, #69847, #59187 ) ) ;
#17512 = CARTESIAN_POINT ( 'NONE',  ( 21.09107601085557349, 0.03930716472865622424, -94.13612202464047130 ) ) ;
#17513 = VERTEX_POINT ( 'NONE', #178871 ) ;
#17514 = ORIENTED_EDGE ( 'NONE', *, *, #123126, .T. ) ;
#17515 = CARTESIAN_POINT ( 'NONE',  ( 18.59999999999999076, 67.74990736105834799, -227.9721689390126755 ) ) ;
#17516 = DIRECTION ( 'NONE',  ( 0.000000000000000000, -0.2128009952263501814, 0.9770955615653337256 ) ) ;
#17517 = ORIENTED_EDGE ( 'NONE', *, *, #187026, .F. ) ;
#17518 = ORIENTED_EDGE ( 'NONE', *, *, #7199, .T. ) ;
#17519 = FACE_OUTER_BOUND ( 'NONE', #71324, .T. ) ;
#17520 = VERTEX_POINT ( 'NONE', #101829 ) ;
#17521 = ORIENTED_EDGE ( 'NONE', *, *, #159230, .F. ) ;
#17522 = CIRCLE ( 'NONE', #250583, 0.9750000000000036415 ) ;
#17523 = EDGE_CURVE ( 'NONE', #164185, #149408, #223772, .T. ) ;
#17524 = DIRECTION ( 'NONE',  ( 1.000000000000000000, -3.265361837132813093E-16, -2.280189983783949500E-30 ) ) ;
#17525 = CARTESIAN_POINT ( 'NONE',  ( -22.10000000000000142, -11.65000000000000036, 12.09999999999999609 ) ) ;
#17526 = FACE_OUTER_BOUND ( 'NONE', #66391, .T. ) ;
#17527 = EDGE_CURVE ( 'NONE', #188417, #169022, #23646, .T. ) ;
#17528 = DIRECTION ( 'NONE',  ( 0.000000000000000000, -0.8814952561688476074, 0.4721928772777262417 ) ) ;
#17529 = CARTESIAN_POINT ( 'NONE',  ( 14.56326696814971555, 9.446648990628860432, -15.08916329592317851 ) ) ;
#17530 = DIRECTION ( 'NONE',  ( -7.304098846218134667E-16, -1.000000000000000000, 0.000000000000000000 ) ) ;
#17531 = FACE_OUTER_BOUND ( 'NONE', #185700, .T. ) ;
#17533 = EDGE_LOOP ( 'NONE', ( #165661, #142729, #212435, #102755 ) ) ;
#17532 = CARTESIAN_POINT ( 'NONE',  ( 21.00000000000000000, 66.25000000001253397, -182.3731074845244393 ) ) ;
#17535 = CYLINDRICAL_SURFACE ( 'NONE', #150149, 0.1000000000000124678 ) ;
#17534 = FACE_OUTER_BOUND ( 'NONE', #60167, .T. ) ;
#17536 = EDGE_CURVE ( 'NONE', #76942, #170174, #104400, .T. ) ;
#17537 = DIRECTION ( 'NONE',  ( -0.000000000000000000, 6.982962677686266711E-15, -1.000000000000000000 ) ) ;
#17538 = EDGE_CURVE ( 'NONE', #27504, #4255, #102969, .T. ) ;
#17539 = VERTEX_POINT ( 'NONE', #44471 ) ;
#17540 = CARTESIAN_POINT ( 'NONE',  ( -21.05000000000000071, 1.750000000011155743, -145.6695115579016715 ) ) ;
#17541 = DIRECTION ( 'NONE',  ( 1.000000000000000000, 2.885090398161910739E-16, 6.283419270304611573E-17 ) ) ;
#17542 = ORIENTED_EDGE ( 'NONE', *, *, #57355, .F. ) ;
#17543 = AXIS2_PLACEMENT_3D ( 'NONE', #4914, #84432, #127463 ) ;
#17544 = EDGE_CURVE ( 'NONE', #29887, #138550, #99271, .T. ) ;
#17545 = LINE ( 'NONE', #198756, #203794 ) ;
#17546 = ADVANCED_FACE ( 'NONE', ( #183964 ), #200958, .T. ) ;
#17547 = CARTESIAN_POINT ( 'NONE',  ( 20.94999999999999929, 1.115600667400684642E-11, -180.3749999999999716 ) ) ;
#17548 = ADVANCED_FACE ( 'NONE', ( #61452 ), #5292, .T. ) ;
#17549 = ORIENTED_EDGE ( 'NONE', *, *, #97517, .T. ) ;
#17550 = ORIENTED_EDGE ( 'NONE', *, *, #225634, .T. ) ;
#17551 = CARTESIAN_POINT ( 'NONE',  ( 22.59999999999999432, 64.05844819680035584, -247.1686437718134357 ) ) ;
#17552 = ADVANCED_FACE ( 'NONE', ( #39347 ), #4038, .F. ) ;
#17553 = CARTESIAN_POINT ( 'NONE',  ( -18.49999999999999645, -0.6245386572416675719, -242.4051462500093237 ) ) ;
#17554 = DIRECTION ( 'NONE',  ( 0.000000000000000000, -0.9229812358756199764, 0.3848449534832346086 ) ) ;
#17555 = CARTESIAN_POINT ( 'NONE',  ( 18.59999999999999076, 65.79142135624880439, -48.17310748452439384 ) ) ;
#17556 = VERTEX_POINT ( 'NONE', #118874 ) ;
#17557 = DIRECTION ( 'NONE',  ( -1.000000000000000000, 0.000000000000000000, 0.000000000000000000 ) ) ;
#17558 = EDGE_CURVE ( 'NONE', #53814, #25213, #40649, .T. ) ;
#17559 = AXIS2_PLACEMENT_3D ( 'NONE', #200819, #203388, #2599 ) ;
#17560 = CIRCLE ( 'NONE', #30089, 0.1000000000000028644 ) ;
#17561 = AXIS2_PLACEMENT_3D ( 'NONE', #66991, #206503, #109964 ) ;
#17562 = CARTESIAN_POINT ( 'NONE',  ( 20.04999999999999716, 8.750000000011173285, -79.65000000000004832 ) ) ;
#17563 = LINE ( 'NONE', #180512, #132649 ) ;
#17564 = EDGE_CURVE ( 'NONE', #51770, #25295, #144666, .T. ) ;
#17565 = ADVANCED_FACE ( 'NONE', ( #41915 ), #82260, .T. ) ;
#17566 = PLANE ( 'NONE',  #88464 ) ;
#17567 = EDGE_CURVE ( 'NONE', #4296, #64828, #182681, .T. ) ;
#17569 = ORIENTED_EDGE ( 'NONE', *, *, #4588, .T. ) ;
#17568 = CARTESIAN_POINT ( 'NONE',  ( 18.49999999999999289, 11.65000000001115588, -67.00000000000000000 ) ) ;
#17570 = CARTESIAN_POINT ( 'NONE',  ( -21.05000000000000071, 61.06755371101182561, -205.0964418925513826 ) ) ;
#17571 = CARTESIAN_POINT ( 'NONE',  ( -16.85722902420156188, 66.05000000001189164, -90.25756001075384916 ) ) ;
#17572 = CARTESIAN_POINT ( 'NONE',  ( -23.15000000000000213, 4.150000000011156764, -21.75000000000000355 ) ) ;
#17573 = DIRECTION ( 'NONE',  ( -1.000000000000000000, -0.000000000000000000, -0.000000000000000000 ) ) ;
#17574 = CARTESIAN_POINT ( 'NONE',  ( 21.05000000000251958, 10.50253167713809965, -175.0588298170762869 ) ) ;
#17575 = EDGE_CURVE ( 'NONE', #166644, #152244, #46996, .T. ) ;
#17577 = EDGE_LOOP ( 'NONE', ( #63159, #50175, #253092, #255822, #198391 ) ) ;
#17576 = CARTESIAN_POINT ( 'NONE',  ( -18.40000000000000213, 11.47316190337364183, -91.17405393319209850 ) ) ;
#17578 = CARTESIAN_POINT ( 'NONE',  ( -18.59999999999999787, 68.97833521811203639, -132.6895420826271277 ) ) ;
#17579 = ADVANCED_FACE ( 'NONE', ( #208688 ), #189105, .T. ) ;
#17580 = DIRECTION ( 'NONE',  ( 1.000000000000000000, 0.000000000000000000, -0.000000000000000000 ) ) ;
#17581 = DIRECTION ( 'NONE',  ( 1.000000000000000000, 0.000000000000000000, 0.000000000000000000 ) ) ;
#17582 = ORIENTED_EDGE ( 'NONE', *, *, #9386, .F. ) ;
#17583 = CARTESIAN_POINT ( 'NONE',  ( 18.39999999999999503, 64.25000000001207923, -123.8731074845243683 ) ) ;
#17584 = FACE_OUTER_BOUND ( 'NONE', #170238, .T. ) ;
#17585 = CARTESIAN_POINT ( 'NONE',  ( 20.94999999999999929, 5.000000000011153745, -45.90526601891310321 ) ) ;
#17586 = CARTESIAN_POINT ( 'NONE',  ( -27.30103769104855971, 12.19999999999999574, 33.00000000000000000 ) ) ;
#17587 = CARTESIAN_POINT ( 'NONE',  ( -18.49719636458532790, 78.19930753737976659, -231.5026796452758617 ) ) ;
#17588 = AXIS2_PLACEMENT_3D ( 'NONE', #163112, #122703, #137111 ) ;
#17589 = DIRECTION ( 'NONE',  ( 1.000000000000000000, 0.000000000000000000, 0.000000000000000000 ) ) ;
#17590 = ORIENTED_EDGE ( 'NONE', *, *, #137929, .T. ) ;
#17591 = VERTEX_POINT ( 'NONE', #27507 ) ;
#17592 = FACE_OUTER_BOUND ( 'NONE', #59569, .T. ) ;
#17593 = CYLINDRICAL_SURFACE ( 'NONE', #229010, 0.9000000000000014655 ) ;
#17594 = AXIS2_PLACEMENT_3D ( 'NONE', #122665, #164352, #48239 ) ;
#17595 = DIRECTION ( 'NONE',  ( -0.000000000000000000, 0.000000000000000000, -1.000000000000000000 ) ) ;
#17596 = CARTESIAN_POINT ( 'NONE',  ( -23.25000000000000000, -11.64999999998884483, -33.50000000000000000 ) ) ;
#17597 = EDGE_LOOP ( 'NONE', ( #192319, #216289, #115148 ) ) ;
#17598 = LINE ( 'NONE', #153317, #155260 ) ;
#17599 = VECTOR ( 'NONE', #181137, 1000.000000000000000 ) ;
#17600 = CIRCLE ( 'NONE', #159116, 0.1999999999999987899 ) ;
#17601 = CARTESIAN_POINT ( 'NONE',  ( -21.05000000000000071, 74.16465844978819177, -191.9679561919613775 ) ) ;
#17602 = AXIS2_PLACEMENT_3D ( 'NONE', #36716, #35436, #15867 ) ;
#17603 = CIRCLE ( 'NONE', #163381, 0.09999999999998898659 ) ;
#17604 = FACE_OUTER_BOUND ( 'NONE', #230299, .T. ) ;
#17605 = CIRCLE ( 'NONE', #13358, 0.09999999999999939493 ) ;
#17606 = ORIENTED_EDGE ( 'NONE', *, *, #132398, .F. ) ;
#17607 = DIRECTION ( 'NONE',  ( 0.000000000000000000, -1.000000000000000000, -6.982962677686266711E-15 ) ) ;
#17608 = ORIENTED_EDGE ( 'NONE', *, *, #91212, .T. ) ;
#17609 = ORIENTED_EDGE ( 'NONE', *, *, #125109, .F. ) ;
#17610 = CARTESIAN_POINT ( 'NONE',  ( -21.05000000000000071, 0.09779029131994597390, -27.24218538952387902 ) ) ;
#17611 = DIRECTION ( 'NONE',  ( -0.000000000000000000, -6.982962677686266711E-15, 1.000000000000000000 ) ) ;
#17612 = DIRECTION ( 'NONE',  ( 0.000000000000000000, 0.000000000000000000, 1.000000000000000000 ) ) ;
#17613 = ORIENTED_EDGE ( 'NONE', *, *, #69120, .F. ) ;
#17614 = CARTESIAN_POINT ( 'NONE',  ( -23.49999999999994316, 87.60324567546805952, -34.17184040628037422 ) ) ;
#17615 = DIRECTION ( 'NONE',  ( 0.000000000000000000, -0.9126074666063765939, -0.4088369013363289950 ) ) ;
#17617 = CARTESIAN_POINT ( 'NONE',  ( -16.79363873026997922, 30.20239522323781856, -234.8062423651074653 ) ) ;
#17616 = TOROIDAL_SURFACE ( 'NONE', #163394, 0.2000000000000000111, 0.1000000000000000056 ) ;
#17618 = ORIENTED_EDGE ( 'NONE', *, *, #245437, .F. ) ;
#17619 = CYLINDRICAL_SURFACE ( 'NONE', #33361, 0.09999999999999939493 ) ;
#17620 = AXIS2_PLACEMENT_3D ( 'NONE', #50901, #130465, #91357 ) ;
#17621 = ADVANCED_FACE ( 'NONE', ( #165711 ), #211322, .T. ) ;
#17623 = VERTEX_POINT ( 'NONE', #129132 ) ;
#17622 = CARTESIAN_POINT ( 'NONE',  ( 18.52928932188133970, 65.72071067813085676, -145.3731074845244109 ) ) ;
#17624 = CARTESIAN_POINT ( 'NONE',  ( -20.94999999999999929, -1.835341550213255957, -112.0551512925630249 ) ) ;
#17625 = CARTESIAN_POINT ( 'NONE',  ( -18.40000000000000213, 85.51932773110476660, -163.0501311079649724 ) ) ;
#17626 = AXIS2_PLACEMENT_3D ( 'NONE', #121934, #3239, #144038 ) ;
#17627 = CIRCLE ( 'NONE', #146800, 0.09999999999998898659 ) ;
#17628 = ADVANCED_FACE ( 'NONE', ( #108290 ), #185251, .T. ) ;
#17629 = AXIS2_PLACEMENT_3D ( 'NONE', #71131, #251004, #86799 ) ;
#17630 = AXIS2_PLACEMENT_3D ( 'NONE', #103343, #122939, #219440 ) ;
#17631 = ORIENTED_EDGE ( 'NONE', *, *, #136694, .F. ) ;
#17632 = AXIS2_PLACEMENT_3D ( 'NONE', #144244, #244641, #145540 ) ;
#17633 = DIRECTION ( 'NONE',  ( 0.000000000000000000, 0.000000000000000000, -1.000000000000000000 ) ) ;
#17635 = EDGE_CURVE ( 'NONE', #65906, #119824, #10471, .T. ) ;
#17634 = DIRECTION ( 'NONE',  ( 1.000000000000000000, 0.000000000000000000, 0.000000000000000000 ) ) ;
#17636 = CARTESIAN_POINT ( 'NONE',  ( 20.94999999999999929, 1.115600667400684642E-11, -202.8999999999999773 ) ) ;
#17638 = ADVANCED_FACE ( 'NONE', ( #6605 ), #65299, .T. ) ;
#17637 = ORIENTED_EDGE ( 'NONE', *, *, #33114, .F. ) ;
#17639 = DIRECTION ( 'NONE',  ( 0.000000000000000000, -0.6728971962616697722, 0.7397360091702875895 ) ) ;
#17640 = CIRCLE ( 'NONE', #96736, 0.09999999999998898659 ) ;
#17641 = CARTESIAN_POINT ( 'NONE',  ( 22.49533356619868130, 55.97040697584030511, -232.8685561480749300 ) ) ;
#17642 = DIRECTION ( 'NONE',  ( 1.000000000000000000, 0.000000000000000000, 0.000000000000000000 ) ) ;
#17643 = VERTEX_POINT ( 'NONE', #87419 ) ;
#17644 = EDGE_LOOP ( 'NONE', ( #66734, #183287, #222633, #77003 ) ) ;
#17645 = AXIS2_PLACEMENT_3D ( 'NONE', #223811, #182143, #45185 ) ;
#17646 = AXIS2_PLACEMENT_3D ( 'NONE', #11588, #92378, #51955 ) ;
#17647 = VECTOR ( 'NONE', #199081, 1000.000000000000000 ) ;
#17648 = EDGE_CURVE ( 'NONE', #143516, #9216, #48304, .T. ) ;
#17649 = ORIENTED_EDGE ( 'NONE', *, *, #84753, .F. ) ;
#17650 = CARTESIAN_POINT ( 'NONE',  ( 18.59999999999999432, -1.162701749926855266, -142.1000000000000227 ) ) ;
#17651 = CARTESIAN_POINT ( 'NONE',  ( 21.05000000000000071, 8.776282889879928106, -45.67621514106831171 ) ) ;
#17653 = EDGE_LOOP ( 'NONE', ( #123656, #232742, #195357 ) ) ;
#17652 = DIRECTION ( 'NONE',  ( 0.000000000000000000, 0.000000000000000000, -1.000000000000000000 ) ) ;
#17654 = DIRECTION ( 'NONE',  ( -1.000000000000000000, 0.000000000000000000, 0.000000000000000000 ) ) ;
#17655 = CARTESIAN_POINT ( 'NONE',  ( -20.64999999999999858, 4.349999999999999645, -21.15000000000000213 ) ) ;
#17656 = DIRECTION ( 'NONE',  ( 1.000000000000000000, 0.000000000000000000, 0.000000000000000000 ) ) ;
#17657 = DIRECTION ( 'NONE',  ( -1.646408749285562691E-14, 1.000000000000000000, 0.000000000000000000 ) ) ;
#17658 = DIRECTION ( 'NONE',  ( -0.000000000000000000, -0.000000000000000000, -1.000000000000000000 ) ) ;
#17659 = CYLINDRICAL_SURFACE ( 'NONE', #155626, 0.09999999999999939493 ) ;
#17662 = ORIENTED_EDGE ( 'NONE', *, *, #196481, .F. ) ;
#17661 = EDGE_CURVE ( 'NONE', #148690, #175914, #123847, .T. ) ;
#17660 = CARTESIAN_POINT ( 'NONE',  ( -20.94999999999999929, 87.29603075034691528, -66.47520832486038955 ) ) ;
#17664 = VERTEX_POINT ( 'NONE', #49593 ) ;
#17663 = DIRECTION ( 'NONE',  ( 0.000000000000000000, 0.000000000000000000, -1.000000000000000000 ) ) ;
#17666 = CARTESIAN_POINT ( 'NONE',  ( -16.93710578446435022, 51.37355040952256502, -232.0563660034529221 ) ) ;
#17665 = DIRECTION ( 'NONE',  ( 1.000000000000000000, -1.145314911736513911E-16, 3.106193895438251633E-17 ) ) ;
#17668 = ORIENTED_EDGE ( 'NONE', *, *, #249108, .T. ) ;
#17667 = CARTESIAN_POINT ( 'NONE',  ( 20.95429402530545815, 8.876194151113343977, -75.52308669793789875 ) ) ;
#17669 = ORIENTED_EDGE ( 'NONE', *, *, #219163, .T. ) ;
#17670 = ADVANCED_FACE ( 'NONE', ( #225627 ), #109545, .T. ) ;
#17671 = FACE_OUTER_BOUND ( 'NONE', #246048, .T. ) ;
#17672 = AXIS2_PLACEMENT_3D ( 'NONE', #217629, #42875, #220242 ) ;
#17673 = CARTESIAN_POINT ( 'NONE',  ( -23.25000000000000000, 1.115600667400684642E-11, -104.5500000000000256 ) ) ;
#17674 = LINE ( 'NONE', #37273, #200812 ) ;
#17675 = VECTOR ( 'NONE', #253322, 1000.000000000000000 ) ;
#17676 = LINE ( 'NONE', #241867, #156793 ) ;
#17677 = DIRECTION ( 'NONE',  ( 1.000000000000000000, 0.000000000000000000, 0.000000000000000000 ) ) ;
#17679 = EDGE_CURVE ( 'NONE', #104851, #164361, #13891, .T. ) ;
#17678 = LINE ( 'NONE', #38546, #57108 ) ;
#17680 = ADVANCED_FACE ( 'NONE', ( #206099 ), #125283, .F. ) ;
#17681 = DIRECTION ( 'NONE',  ( 0.000000000000000000, 0.000000000000000000, 1.000000000000000000 ) ) ;
#17682 = VERTEX_POINT ( 'NONE', #110842 ) ;
#17683 = ORIENTED_EDGE ( 'NONE', *, *, #36955, .F. ) ;
#17684 = SPHERICAL_SURFACE ( 'NONE', #185761, 0.1000000000000000056 ) ;
#17685 = EDGE_CURVE ( 'NONE', #25818, #30259, #248736, .T. ) ;
#17686 = ORIENTED_EDGE ( 'NONE', *, *, #198802, .F. ) ;
#17687 = CARTESIAN_POINT ( 'NONE',  ( 18.57399277249656322, 68.10911674539558192, -224.1414149070238864 ) ) ;
#17688 = CARTESIAN_POINT ( 'NONE',  ( -15.70407651835961005, 66.64419340838139760, -53.23200495297821533 ) ) ;
#17689 = VECTOR ( 'NONE', #136236, 1000.000000000000000 ) ;
#17690 = CARTESIAN_POINT ( 'NONE',  ( -22.50000000000000000, 67.20509925321675837, -235.9516399960961337 ) ) ;
#17691 = ORIENTED_EDGE ( 'NONE', *, *, #2737, .F. ) ;
#17692 = CARTESIAN_POINT ( 'NONE',  ( 18.59999999999999076, 74.16465844978819177, -191.8679561919614116 ) ) ;
#17693 = ORIENTED_EDGE ( 'NONE', *, *, #225619, .F. ) ;
#17694 = ADVANCED_FACE ( 'NONE', ( #67862 ), #88686, .F. ) ;
#17695 = CARTESIAN_POINT ( 'NONE',  ( -22.39999999999999858, 76.00000000001246292, -181.6726782920691505 ) ) ;
#17696 = ORIENTED_EDGE ( 'NONE', *, *, #65637, .T. ) ;
#17697 = DIRECTION ( 'NONE',  ( 0.000000000000000000, -0.9770955615653315052, -0.2128009952263603954 ) ) ;
#17698 = EDGE_CURVE ( 'NONE', #117566, #174236, #190408, .T. ) ;
#17699 = CARTESIAN_POINT ( 'NONE',  ( 23.25000000000000000, 85.60000000001278408, -215.2731074845243029 ) ) ;
#17700 = VERTEX_POINT ( 'NONE', #234645 ) ;
#17702 = DIRECTION ( 'NONE',  ( 1.000000000000000000, 0.000000000000000000, 0.000000000000000000 ) ) ;
#17701 = CIRCLE ( 'NONE', #163469, 0.09999999999999990841 ) ;
#17704 = ORIENTED_EDGE ( 'NONE', *, *, #95180, .F. ) ;
#17703 = FACE_OUTER_BOUND ( 'NONE', #198077, .T. ) ;
#17705 = DIRECTION ( 'NONE',  ( 0.000000000000000000, 0.9654421110809058293, 0.2606175937108693996 ) ) ;
#17706 = ORIENTED_EDGE ( 'NONE', *, *, #108607, .T. ) ;
#17707 = DIRECTION ( 'NONE',  ( 1.000000000000000000, 0.000000000000000000, 0.000000000000000000 ) ) ;
#17708 = VERTEX_POINT ( 'NONE', #76846 ) ;
#17709 = DIRECTION ( 'NONE',  ( 0.000000000000000000, 1.000000000000000000, 0.000000000000000000 ) ) ;
#17710 = CARTESIAN_POINT ( 'NONE',  ( 22.46250603428203618, 64.16148097394537331, -247.0932813659109115 ) ) ;
#17711 = DIRECTION ( 'NONE',  ( -1.000000000000000000, 0.000000000000000000, 0.000000000000000000 ) ) ;
#17712 = LINE ( 'NONE', #102365, #60358 ) ;
#17713 = CARTESIAN_POINT ( 'NONE',  ( -21.08884785362073089, 0.04978309507788075683, -60.64280663257443393 ) ) ;
#17714 = AXIS2_PLACEMENT_3D ( 'NONE', #253510, #189700, #132287 ) ;
#17715 = EDGE_LOOP ( 'NONE', ( #16165, #120385 ) ) ;
#17716 = AXIS2_PLACEMENT_3D ( 'NONE', #38917, #95019, #118457 ) ;
#17717 = DIRECTION ( 'NONE',  ( 0.000000000000000000, 0.2128009952263605065, -0.9770955615653315052 ) ) ;
#17718 = CARTESIAN_POINT ( 'NONE',  ( -20.99551997958453953, 64.25000000001158185, -109.8714483468347538 ) ) ;
#17719 = CARTESIAN_POINT ( 'NONE',  ( -21.05000000000000071, 11.75000000001115197, -160.4851942293460638 ) ) ;
#17720 = VERTEX_POINT ( 'NONE', #112156 ) ;
#17721 = CARTESIAN_POINT ( 'NONE',  ( -20.07928932188135107, 66.77928932189357170, -148.7731074845244166 ) ) ;
#17722 = VERTEX_POINT ( 'NONE', #191705 ) ;
#17723 = DIRECTION ( 'NONE',  ( -1.186688945009010077E-16, 1.000000000000000000, 0.000000000000000000 ) ) ;
#17724 = VERTEX_POINT ( 'NONE', #13060 ) ;
#17725 = CARTESIAN_POINT ( 'NONE',  ( 21.05000000000000071, -3.685352791942196227, -226.3713951780953550 ) ) ;
#17726 = DIRECTION ( 'NONE',  ( 1.000000000000000000, 0.000000000000000000, 0.000000000000000000 ) ) ;
#17727 = AXIS2_PLACEMENT_3D ( 'NONE', #126406, #242503, #66442 ) ;
#17729 = EDGE_LOOP ( 'NONE', ( #60761, #191038, #130573, #103437 ) ) ;
#17728 = DIRECTION ( 'NONE',  ( 1.000000000000000000, 0.000000000000000000, 0.000000000000000000 ) ) ;
#17730 = DIRECTION ( 'NONE',  ( -1.000000000000000000, 0.000000000000000000, 0.000000000000000000 ) ) ;
#17731 = VERTEX_POINT ( 'NONE', #113418 ) ;
#17732 = FACE_OUTER_BOUND ( 'NONE', #21279, .T. ) ;
#17733 = CIRCLE ( 'NONE', #221741, 0.09999999999998898659 ) ;
#17734 = AXIS2_PLACEMENT_3D ( 'NONE', #165823, #163246, #64136 ) ;
#17735 = CARTESIAN_POINT ( 'NONE',  ( 18.39999999999999503, 43.39957528361355799, -233.6562381667159798 ) ) ;
#17736 = ORIENTED_EDGE ( 'NONE', *, *, #122388, .T. ) ;
#17737 = CIRCLE ( 'NONE', #88656, 0.1000000000000028644 ) ;
#17738 = VERTEX_POINT ( 'NONE', #252917 ) ;
#17739 = DIRECTION ( 'NONE',  ( -1.000000000000000000, -0.000000000000000000, -0.000000000000000000 ) ) ;
#17740 = CARTESIAN_POINT ( 'NONE',  ( -21.04386569057742307, 11.75000000001181277, -194.1428373517780130 ) ) ;
#17741 = VERTEX_POINT ( 'NONE', #14345 ) ;
#17742 = CARTESIAN_POINT ( 'NONE',  ( 21.05000000000000071, 10.21728496540352893, -227.9671432372869049 ) ) ;
#17743 = EDGE_LOOP ( 'NONE', ( #240706, #218308, #245701, #221088 ) ) ;
#17744 = VERTEX_POINT ( 'NONE', #153881 ) ;
#17745 = CARTESIAN_POINT ( 'NONE',  ( 22.59999999999999076, 25.91621630664725728, -254.3113660372828804 ) ) ;
#17746 = DIRECTION ( 'NONE',  ( -1.000000000000000000, 0.000000000000000000, 0.000000000000000000 ) ) ;
#17747 = EDGE_CURVE ( 'NONE', #255303, #191355, #237887, .T. ) ;
#17749 = ORIENTED_EDGE ( 'NONE', *, *, #117481, .F. ) ;
#17748 = CARTESIAN_POINT ( 'NONE',  ( 21.05000000000000071, 67.17357026049440094, -61.10905277158068571 ) ) ;
#17750 = EDGE_CURVE ( 'NONE', #5080, #122251, #213798, .T. ) ;
#17751 = DIRECTION ( 'NONE',  ( 0.000000000000000000, -2.168404344970946706E-14, -1.000000000000000000 ) ) ;
#17752 = EDGE_CURVE ( 'NONE', #3898, #26858, #186392, .T. ) ;
#17753 = LINE ( 'NONE', #118162, #127554 ) ;
#17754 = FACE_OUTER_BOUND ( 'NONE', #119532, .T. ) ;
#17756 = CARTESIAN_POINT ( 'NONE',  ( -22.44366136229477249, 75.99065843052638058, -181.6728260419982632 ) ) ;
#17755 = CARTESIAN_POINT ( 'NONE',  ( 20.12500000000000000, 59.94448977088796937, -225.4740812377367263 ) ) ;
#17757 = CARTESIAN_POINT ( 'NONE',  ( -21.05000000000000071, 76.08579911628621062, -142.9370863660131761 ) ) ;
#17758 = FACE_OUTER_BOUND ( 'NONE', #67536, .T. ) ;
#17759 = AXIS2_PLACEMENT_3D ( 'NONE', #120350, #21243, #218103 ) ;
#17760 = CARTESIAN_POINT ( 'NONE',  ( -20.85000000000000142, 43.27008861172207332, -245.2265230569236110 ) ) ;
#17761 = AXIS2_PLACEMENT_3D ( 'NONE', #23303, #61111, #20727 ) ;
#17762 = CARTESIAN_POINT ( 'NONE',  ( -21.05000000000000071, 77.16270174995034381, -161.9231074845243370 ) ) ;
#17763 = VERTEX_POINT ( 'NONE', #251643 ) ;
#17764 = EDGE_LOOP ( 'NONE', ( #182018, #167033, #82234, #6838 ) ) ;
#17765 = DIRECTION ( 'NONE',  ( -1.000000000000000000, -0.000000000000000000, -0.000000000000000000 ) ) ;
#17767 = ORIENTED_EDGE ( 'NONE', *, *, #241977, .T. ) ;
#17766 = CARTESIAN_POINT ( 'NONE',  ( -23.15000000000000213, 56.46250644710310951, -240.6794019422471251 ) ) ;
#17768 = ORIENTED_EDGE ( 'NONE', *, *, #112644, .F. ) ;
#17769 = EDGE_CURVE ( 'NONE', #11722, #83610, #236433, .T. ) ;
#17771 = CARTESIAN_POINT ( 'NONE',  ( 21.05000000000000071, -6.488386256076840830, -212.2361678873109554 ) ) ;
#17770 = CIRCLE ( 'NONE', #80108, 2.000000000000002665 ) ;
#17772 = ORIENTED_EDGE ( 'NONE', *, *, #64320, .T. ) ;
#17773 = DIRECTION ( 'NONE',  ( -1.000000000000000000, -0.000000000000000000, -0.000000000000000000 ) ) ;
#17774 = ORIENTED_EDGE ( 'NONE', *, *, #224895, .T. ) ;
#17775 = CIRCLE ( 'NONE', #46821, 11.89999999999999325 ) ;
#17777 = CIRCLE ( 'NONE', #1218, 11.80000000000000959 ) ;
#17776 = SURFACE_STYLE_USAGE ( .BOTH. , #136431 ) ;
#17778 = CARTESIAN_POINT ( 'NONE',  ( -13.40000000000000213, -12.25000000000000178, 15.00000000000000355 ) ) ;
#17779 = VECTOR ( 'NONE', #250311, 1000.000000000000000 ) ;
#17781 = ORIENTED_EDGE ( 'NONE', *, *, #62343, .T. ) ;
#17780 = ORIENTED_EDGE ( 'NONE', *, *, #185928, .F. ) ;
#17782 = ORIENTED_EDGE ( 'NONE', *, *, #235572, .F. ) ;
#17783 = AXIS2_PLACEMENT_3D ( 'NONE', #238241, #40082, #175736 ) ;
#17784 = ORIENTED_EDGE ( 'NONE', *, *, #168950, .T. ) ;
#17786 = VERTEX_POINT ( 'NONE', #54720 ) ;
#17785 = VECTOR ( 'NONE', #234489, 1000.000000000000000 ) ;
#17787 = DIRECTION ( 'NONE',  ( 0.000000000000000000, 0.000000000000000000, -1.000000000000000000 ) ) ;
#17788 = CARTESIAN_POINT ( 'NONE',  ( 18.69999999999999929, 1.350000000000000089, 22.10000000000000142 ) ) ;
#17790 = EDGE_LOOP ( 'NONE', ( #165832, #248407, #230577, #193376 ) ) ;
#17789 = DIRECTION ( 'NONE',  ( 0.000000000000000000, -0.2128009952263403282, 0.9770955615653358350 ) ) ;
#17791 = EDGE_CURVE ( 'NONE', #133225, #230526, #157088, .T. ) ;
#17792 = ADVANCED_FACE ( 'NONE', ( #232099 ), #114698, .T. ) ;
#17793 = CARTESIAN_POINT ( 'NONE',  ( -21.93340585971078838, 33.66454284798572161, -242.8670914416577773 ) ) ;
#17794 = CARTESIAN_POINT ( 'NONE',  ( 15.52844286134407881, 12.53760658702568165, -214.5091953838863219 ) ) ;
#17796 = ORIENTED_EDGE ( 'NONE', *, *, #30452, .T. ) ;
#17795 = CARTESIAN_POINT ( 'NONE',  ( -21.04999999999994387, 67.75000000001118394, -51.02310748452479316 ) ) ;
#17797 = DIRECTION ( 'NONE',  ( 0.000000000000000000, 0.000000000000000000, 1.000000000000000000 ) ) ;
#17798 = ORIENTED_EDGE ( 'NONE', *, *, #137459, .T. ) ;
#17799 = FACE_OUTER_BOUND ( 'NONE', #68499, .T. ) ;
#17800 = CIRCLE ( 'NONE', #109387, 0.09999999999999939493 ) ;
#17802 = ORIENTED_EDGE ( 'NONE', *, *, #192481, .T. ) ;
#17801 = DIRECTION ( 'NONE',  ( 0.000000000000000000, 0.2617529984165033463, 0.9651348961777157509 ) ) ;
#17803 = DIRECTION ( 'NONE',  ( 0.000000000000000000, 0.9126074666063660468, 0.4088369013363524762 ) ) ;
#17804 = DIRECTION ( 'NONE',  ( 0.000000000000000000, 0.1350103645451876666, -0.9908441862701600211 ) ) ;
#17806 = EDGE_CURVE ( 'NONE', #1674, #172993, #165738, .T. ) ;
#17805 = CARTESIAN_POINT ( 'NONE',  ( -17.05016517656156694, 9.950000000013657697, -87.82730200399912235 ) ) ;
#17807 = VERTEX_POINT ( 'NONE', #174726 ) ;
#17808 = VECTOR ( 'NONE', #128399, 1000.000000000000000 ) ;
#17810 = DIRECTION ( 'NONE',  ( -0.000000000000000000, 0.9525900758537790836, -0.3042567129660269099 ) ) ;
#17809 = CARTESIAN_POINT ( 'NONE',  ( -16.89935556175677789, 9.950000000011137047, -46.63967636288582241 ) ) ;
#17811 = CARTESIAN_POINT ( 'NONE',  ( 22.42357213249528769, 7.672932386371071445, -133.9009130359984567 ) ) ;
#17812 = DIRECTION ( 'NONE',  ( 0.000000000000000000, 1.000000000000000000, 0.000000000000000000 ) ) ;
#17813 = CARTESIAN_POINT ( 'NONE',  ( -21.05000000000000071, 77.16270174994961906, -61.42310748452431568 ) ) ;
#17815 = VERTEX_POINT ( 'NONE', #254188 ) ;
#17814 = VECTOR ( 'NONE', #214028, 1000.000000000000000 ) ;
#17816 = VERTEX_POINT ( 'NONE', #155147 ) ;
#17817 = AXIS2_PLACEMENT_3D ( 'NONE', #223485, #44869, #184362 ) ;
#17818 = CIRCLE ( 'NONE', #146987, 0.09999999999999939493 ) ;
#17819 = CARTESIAN_POINT ( 'NONE',  ( 21.05000000000000071, 6.277629359189123903, -229.8243190661787878 ) ) ;
#17820 = CIRCLE ( 'NONE', #230812, 1.500000000000001332 ) ;
#17821 = DIRECTION ( 'NONE',  ( 0.000000000000000000, 0.000000000000000000, 1.000000000000000000 ) ) ;
#17822 = ORIENTED_EDGE ( 'NONE', *, *, #149436, .F. ) ;
#17823 = CARTESIAN_POINT ( 'NONE',  ( -20.54999999999999716, 7.150000000011155876, -188.6499999999999488 ) ) ;
#17824 = ORIENTED_EDGE ( 'NONE', *, *, #39306, .T. ) ;
#17825 = LINE ( 'NONE', #98616, #52413 ) ;
#17826 = CARTESIAN_POINT ( 'NONE',  ( -21.65000000000000213, 68.75000000001159606, -56.87310748452436826 ) ) ;
#17827 = EDGE_LOOP ( 'NONE', ( #138959, #243093, #90552, #143264 ) ) ;
#17828 = FACE_OUTER_BOUND ( 'NONE', #86726, .T. ) ;
#17829 = VECTOR ( 'NONE', #245104, 1000.000000000000000 ) ;
#17830 = CIRCLE ( 'NONE', #84431, 0.09999999999999939493 ) ;
#17831 = ORIENTED_EDGE ( 'NONE', *, *, #103926, .F. ) ;
#17833 = VERTEX_POINT ( 'NONE', #135525 ) ;
#17832 = CIRCLE ( 'NONE', #142903, 0.9000000000000014655 ) ;
#17834 = ORIENTED_EDGE ( 'NONE', *, *, #140015, .F. ) ;
#17835 = ADVANCED_FACE ( 'NONE', ( #215079 ), #255438, .T. ) ;
#17836 = FACE_OUTER_BOUND ( 'NONE', #250083, .T. ) ;
#17837 = CARTESIAN_POINT ( 'NONE',  ( 22.44352723754029810, 75.99072290496948767, -215.1728288298730831 ) ) ;
#17838 = DIRECTION ( 'NONE',  ( 1.000000000000000000, 0.000000000000000000, 0.000000000000000000 ) ) ;
#17839 = EDGE_CURVE ( 'NONE', #64432, #169963, #28191, .T. ) ;
#17840 = DIRECTION ( 'NONE',  ( -0.000000000000000000, 6.982962677686266711E-15, -1.000000000000000000 ) ) ;
#17841 = DIRECTION ( 'NONE',  ( -0.000000000000000000, 0.000000000000000000, 1.000000000000000000 ) ) ;
#17843 = DIRECTION ( 'NONE',  ( 1.000000000000000000, 0.000000000000000000, 0.000000000000000000 ) ) ;
#17842 = CARTESIAN_POINT ( 'NONE',  ( -18.59999999999999787, 0.000000000000000000, 0.000000000000000000 ) ) ;
#17844 = LINE ( 'NONE', #56951, #187392 ) ;
#17846 = VERTEX_POINT ( 'NONE', #157726 ) ;
#17845 = CARTESIAN_POINT ( 'NONE',  ( 21.30000000000002558, 76.00000000001197975, -107.0731074845243143 ) ) ;
#17847 = CARTESIAN_POINT ( 'NONE',  ( -23.25000000000000000, 51.38014393322265505, -230.1906178717505611 ) ) ;
#17848 = ORIENTED_EDGE ( 'NONE', *, *, #5235, .F. ) ;
#17849 = EDGE_CURVE ( 'NONE', #36016, #168134, #217619, .T. ) ;
#17850 = FACE_OUTER_BOUND ( 'NONE', #63500, .T. ) ;
#17851 = EDGE_CURVE ( 'NONE', #79888, #186782, #119753, .T. ) ;
#17852 = ORIENTED_EDGE ( 'NONE', *, *, #27927, .T. ) ;
#17853 = VERTEX_POINT ( 'NONE', #143232 ) ;
#17854 = CARTESIAN_POINT ( 'NONE',  ( -16.93234230245721861, 66.00189262946443591, -48.60541720285813483 ) ) ;
#17855 = DIRECTION ( 'NONE',  ( 0.000000000000000000, -1.000000000000000000, -6.352154140967427193E-15 ) ) ;
#17856 = DIRECTION ( 'NONE',  ( 2.840903330521633255E-16, 0.8700118002898357128, -0.4930308989875171188 ) ) ;
#17857 = VERTEX_POINT ( 'NONE', #119859 ) ;
#17858 = ADVANCED_FACE ( 'NONE', ( #59830 ), #90683, .T. ) ;
#17859 = CARTESIAN_POINT ( 'NONE',  ( -23.49999999999994316, 74.94272479589878344, -8.023107484524793165 ) ) ;
#17861 = EDGE_CURVE ( 'NONE', #19219, #78948, #86381, .T. ) ;
#17860 = ADVANCED_FACE ( 'NONE', ( #22032 ), #196789, .F. ) ;
#17862 = ORIENTED_EDGE ( 'NONE', *, *, #64704, .F. ) ;
#17863 = ORIENTED_EDGE ( 'NONE', *, *, #245728, .F. ) ;
#17864 = AXIS2_PLACEMENT_3D ( 'NONE', #158460, #235388, #196265 ) ;
#17865 = CARTESIAN_POINT ( 'NONE',  ( -18.39999999999999858, 85.50000000001138289, -29.42291809330221497 ) ) ;
#17866 = VERTEX_POINT ( 'NONE', #42865 ) ;
#17867 = LINE ( 'NONE', #157431, #23859 ) ;
#17868 = DIRECTION ( 'NONE',  ( 0.000000000000000000, 0.000000000000000000, 1.000000000000000000 ) ) ;
#17869 = ORIENTED_EDGE ( 'NONE', *, *, #36400, .F. ) ;
#17870 = DIRECTION ( 'NONE',  ( -1.000000000000000000, -1.394253735153569469E-16, -2.602809386958778209E-16 ) ) ;
#17871 = EDGE_CURVE ( 'NONE', #221278, #135540, #122405, .T. ) ;
#17872 = FACE_OUTER_BOUND ( 'NONE', #111409, .T. ) ;
#17873 = CARTESIAN_POINT ( 'NONE',  ( 22.59999999999999432, 11.74956712350054566, -133.8991416309013118 ) ) ;
#17874 = ORIENTED_EDGE ( 'NONE', *, *, #17635, .T. ) ;
#17875 = CARTESIAN_POINT ( 'NONE',  ( -21.00000000000000000, 7.800000000000000711, 0.000000000000000000 ) ) ;
#17876 = EDGE_CURVE ( 'NONE', #90831, #164109, #48996, .T. ) ;
#17877 = DIRECTION ( 'NONE',  ( 0.000000000000000000, -0.9274965247785504907, -0.3738317757009320674 ) ) ;
#17878 = CARTESIAN_POINT ( 'NONE',  ( -22.47120815636973390, 26.01529255436784993, -254.2877069526234948 ) ) ;
#17879 = EDGE_CURVE ( 'NONE', #16805, #48144, #44916, .T. ) ;
#17880 = EDGE_CURVE ( 'NONE', #248008, #206865, #225401, .T. ) ;
#17881 = EDGE_LOOP ( 'NONE', ( #3967, #182900, #93581, #62279 ) ) ;
#17882 = ADVANCED_FACE ( 'NONE', ( #83240 ), #257233, .F. ) ;
#17883 = CARTESIAN_POINT ( 'NONE',  ( 20.97468175916167965, 10.62526516437102231, -12.25476143541283314 ) ) ;
#17884 = VERTEX_POINT ( 'NONE', #138095 ) ;
#17885 = DIRECTION ( 'NONE',  ( 1.000000000000000000, 0.000000000000000000, 0.000000000000000000 ) ) ;
#17886 = DIRECTION ( 'NONE',  ( 0.000000000000000000, 0.000000000000000000, -1.000000000000000000 ) ) ;
#17887 = CARTESIAN_POINT ( 'NONE',  ( 18.59999999999999432, 74.83729825007462466, -195.4231074845243654 ) ) ;
#17888 = EDGE_CURVE ( 'NONE', #171894, #244003, #169597, .T. ) ;
#17889 = CARTESIAN_POINT ( 'NONE',  ( -24.30000000000000071, 3.175288713399619045, 33.00000000000000000 ) ) ;
#17890 = DIRECTION ( 'NONE',  ( 0.000000000000000000, -6.982962677686266711E-15, 1.000000000000000000 ) ) ;
#17891 = CARTESIAN_POINT ( 'NONE',  ( -23.25000000000000000, 4.350000000011156054, -146.3500000000000227 ) ) ;
#17892 = VERTEX_POINT ( 'NONE', #79401 ) ;
#17893 = CARTESIAN_POINT ( 'NONE',  ( -17.11825945287481687, 66.05000000001224691, -149.2731074845244450 ) ) ;
#17894 = CARTESIAN_POINT ( 'NONE',  ( 21.05095171578076574, 67.22382012124101891, -124.3572342078864779 ) ) ;
#17896 = EDGE_CURVE ( 'NONE', #119060, #201799, #139370, .T. ) ;
#17895 = CARTESIAN_POINT ( 'NONE',  ( -22.50000000000088463, 0.04536165658774753140, 11.65050883420956573 ) ) ;
#17897 = CARTESIAN_POINT ( 'NONE',  ( 16.87683809663749557, 66.05000000001203375, -115.6731074845243654 ) ) ;
#17898 = CIRCLE ( 'NONE', #76156, 0.1000000000000028644 ) ;
#17900 = FACE_OUTER_BOUND ( 'NONE', #39410, .T. ) ;
#17899 = VECTOR ( 'NONE', #107798, 1000.000000000000000 ) ;
#17901 = ORIENTED_EDGE ( 'NONE', *, *, #90739, .T. ) ;
#17902 = ORIENTED_EDGE ( 'NONE', *, *, #99216, .T. ) ;
#17903 = LINE ( 'NONE', #33682, #20796 ) ;
#17905 = DIRECTION ( 'NONE',  ( 1.000000000000000000, 0.000000000000000000, 0.000000000000000000 ) ) ;
#17904 = AXIS2_PLACEMENT_3D ( 'NONE', #42544, #202907, #23022 ) ;
#17906 = FACE_OUTER_BOUND ( 'NONE', #86457, .T. ) ;
#17907 = CARTESIAN_POINT ( 'NONE',  ( -20.54999999999999716, -8.999999999988846255, -176.8939691226524076 ) ) ;
#17908 = CARTESIAN_POINT ( 'NONE',  ( 21.14999999999999503, 11.75000000001115552, -134.0000000000000284 ) ) ;
#17909 = EDGE_CURVE ( 'NONE', #253099, #60368, #107258, .T. ) ;
#17910 = ORIENTED_EDGE ( 'NONE', *, *, #239462, .T. ) ;
#17911 = CARTESIAN_POINT ( 'NONE',  ( -22.39999999999999858, 64.35000000001195986, -103.0231074845244024 ) ) ;
#17912 = CARTESIAN_POINT ( 'NONE',  ( -19.99999999999999645, 4.513204987021263825, 22.00000000000000355 ) ) ;
#17913 = AXIS2_PLACEMENT_3D ( 'NONE', #59802, #242311, #121124 ) ;
#17914 = EDGE_LOOP ( 'NONE', ( #170686, #185163, #99423, #224636 ) ) ;
#17915 = AXIS2_PLACEMENT_3D ( 'NONE', #226494, #88264, #49163 ) ;
#17916 = CYLINDRICAL_SURFACE ( 'NONE', #146382, 2.000000000000001776 ) ;
#17917 = AXIS2_PLACEMENT_3D ( 'NONE', #161004, #163570, #61899 ) ;
#17918 = FACE_OUTER_BOUND ( 'NONE', #213726, .T. ) ;
#17919 = EDGE_LOOP ( 'NONE', ( #151768, #99821, #143837, #92593 ) ) ;
#17920 = DIRECTION ( 'NONE',  ( 0.000000000000000000, -6.982962677686266711E-15, 1.000000000000000000 ) ) ;
#17921 = B_SPLINE_CURVE_WITH_KNOTS ( 'NONE', 3,
 ( #208500, #225447, #3859, #148510, #65109, #104221, #46811, #5101, #67676, #203346, #106795, #222892, #88496, #44281, #185055, #123812, #144637, #6416, #224176 ),
 .UNSPECIFIED., .F., .F.,
 ( 4, 3, 3, 3, 3, 3, 4 ),
 ( 0.000000000000000000, 2.646747978908523070E-05, 5.271166642128864737E-05, 9.008788829882664645E-05, 0.0001426648776560804626, 0.0001897378458659709517, 0.0001917382627806279321 ),
 .UNSPECIFIED. ) ;
#17922 = CIRCLE ( 'NONE', #213749, 11.74999999999999289 ) ;
#17923 = ORIENTED_EDGE ( 'NONE', *, *, #227971, .T. ) ;
#17924 = DIRECTION ( 'NONE',  ( 0.000000000000000000, 0.000000000000000000, -1.000000000000000000 ) ) ;
#17925 = CARTESIAN_POINT ( 'NONE',  ( 21.13422380239035192, 69.50667348520698852, -170.0231074845243882 ) ) ;
#17926 = LINE ( 'NONE', #158761, #232483 ) ;
#17927 = LINE ( 'NONE', #33703, #257199 ) ;
#17929 = AXIS2_PLACEMENT_3D ( 'NONE', #188215, #248192, #65690 ) ;
#17928 = LINE ( 'NONE', #55745, #211176 ) ;
#17930 = CARTESIAN_POINT ( 'NONE',  ( 18.39999999999999858, -9.499999999988842703, -140.6001893912220737 ) ) ;
#17932 = DIRECTION ( 'NONE',  ( -1.186688945009010077E-16, 1.000000000000000000, 0.000000000000000000 ) ) ;
#17931 = CIRCLE ( 'NONE', #34717, 4.150000000000001243 ) ;
#17933 = AXIS2_PLACEMENT_3D ( 'NONE', #195347, #252707, #134049 ) ;
#17934 = DIRECTION ( 'NONE',  ( 1.000000000000000000, 0.000000000000000000, 0.000000000000000000 ) ) ;
#17936 = DIRECTION ( 'NONE',  ( 0.000000000000000000, 1.000000000000000000, 0.000000000000000000 ) ) ;
#17935 = AXIS2_PLACEMENT_3D ( 'NONE', #253613, #17573, #193666 ) ;
#17937 = EDGE_CURVE ( 'NONE', #206030, #185310, #136456, .T. ) ;
#17938 = DIRECTION ( 'NONE',  ( 0.000000000000000000, 0.000000000000000000, -1.000000000000000000 ) ) ;
#17939 = DIRECTION ( 'NONE',  ( 0.000000000000000000, -0.8814952561688449428, 0.4721928772777310157 ) ) ;
#17940 = CARTESIAN_POINT ( 'NONE',  ( 18.56579813702274961, 10.33025634372637924, -206.5870929282638429 ) ) ;
#17941 = EDGE_CURVE ( 'NONE', #192518, #120023, #144508, .T. ) ;
#17942 = DIRECTION ( 'NONE',  ( 0.000000000000000000, 0.000000000000000000, -1.000000000000000000 ) ) ;
#17943 = CARTESIAN_POINT ( 'NONE',  ( 20.96428641293985962, 56.19879751615954433, -227.9223442982753625 ) ) ;
#17944 = ORIENTED_EDGE ( 'NONE', *, *, #102054, .F. ) ;
#17945 = CARTESIAN_POINT ( 'NONE',  ( 21.07928932188134397, 6.328516656393312623, 0.09889514565439468108 ) ) ;
#17947 = EDGE_CURVE ( 'NONE', #98230, #108404, #69871, .T. ) ;
#17946 = DIRECTION ( 'NONE',  ( 1.000000000000000000, 2.952720810173289112E-16, -0.000000000000000000 ) ) ;
#17948 = CARTESIAN_POINT ( 'NONE',  ( 20.96937028524355640, 10.62446937163783289, -40.99142610116961549 ) ) ;
#17949 = ADVANCED_FACE ( 'NONE', ( #145798 ), #45429, .F. ) ;
#17950 = ORIENTED_EDGE ( 'NONE', *, *, #222939, .T. ) ;
#17951 = CARTESIAN_POINT ( 'NONE',  ( -20.64999999999999858, 1.999999999999998224, -20.27537807723789953 ) ) ;
#17952 = CARTESIAN_POINT ( 'NONE',  ( -22.39999999999999858, 7.790779598384560245, -33.39999999999999858 ) ) ;
#17953 = CIRCLE ( 'NONE', #163714, 0.09999999999998898659 ) ;
#17954 = VERTEX_POINT ( 'NONE', #46697 ) ;
#17955 = CYLINDRICAL_SURFACE ( 'NONE', #25600, 4.000000000000000000 ) ;
#17956 = DIRECTION ( 'NONE',  ( 0.000000000000000000, 0.2128009952263601456, -0.9770955615653316162 ) ) ;
#17957 = TOROIDAL_SURFACE ( 'NONE', #92983, 4.149999999999999467, 0.1000000000000000056 ) ;
#17958 = ORIENTED_EDGE ( 'NONE', *, *, #73826, .T. ) ;
#17959 = ORIENTED_EDGE ( 'NONE', *, *, #59048, .T. ) ;
#17961 = CARTESIAN_POINT ( 'NONE',  ( 23.14999999999999147, 76.00000000001267608, -203.5231074845243597 ) ) ;
#17960 = CIRCLE ( 'NONE', #43108, 7.900000000000007461 ) ;
#17962 = CIRCLE ( 'NONE', #221955, 0.1999999999999996503 ) ;
#17963 = ORIENTED_EDGE ( 'NONE', *, *, #253019, .F. ) ;
#17964 = CARTESIAN_POINT ( 'NONE',  ( -21.55000000000000426, 29.52010233258345906, -236.9352117192826199 ) ) ;
#17965 = DIRECTION ( 'NONE',  ( 0.000000000000000000, 1.000000000000000000, 1.387778780781444413E-14 ) ) ;
#17967 = CIRCLE ( 'NONE', #9601, 0.1000000000000028644 ) ;
#17966 = DIRECTION ( 'NONE',  ( 0.8049926720990051576, 0.5932847527679298016, -0.000000000000000000 ) ) ;
#17968 = CARTESIAN_POINT ( 'NONE',  ( -20.65000000000000568, 7.249999999999983125, -9.250000000000001776 ) ) ;
#17969 = LINE ( 'NONE', #192778, #201482 ) ;
#17970 = CARTESIAN_POINT ( 'NONE',  ( -12.25000000000000178, 48.12247445990688988, -234.1702647910923361 ) ) ;
#17971 = AXIS2_PLACEMENT_3D ( 'NONE', #21598, #101061, #68416 ) ;
#17972 = CYLINDRICAL_SURFACE ( 'NONE', #101184, 0.8750000000000007772 ) ;
#17974 = DIRECTION ( 'NONE',  ( 0.000000000000000000, 0.8814952561688437216, -0.4721928772777334582 ) ) ;
#17973 = VECTOR ( 'NONE', #77416, 1000.000000000000227 ) ;
#17975 = AXIS2_PLACEMENT_3D ( 'NONE', #179777, #98904, #143184 ) ;
#17977 = ORIENTED_EDGE ( 'NONE', *, *, #200364, .F. ) ;
#17976 = DIRECTION ( 'NONE',  ( 1.000000000000000000, -0.000000000000000000, -0.000000000000000000 ) ) ;
#17978 = ORIENTED_EDGE ( 'NONE', *, *, #122954, .T. ) ;
#17980 = CARTESIAN_POINT ( 'NONE',  ( -21.03571358705830718, 64.25000000001162448, -62.69800066246598647 ) ) ;
#17979 = CARTESIAN_POINT ( 'NONE',  ( -20.64999999999999858, 71.65000000001180069, -81.77310748452433131 ) ) ;
#17981 = ORIENTED_EDGE ( 'NONE', *, *, #14984, .T. ) ;
#17982 = EDGE_LOOP ( 'NONE', ( #112617, #195850, #181578, #80466, #119256, #245111, #90958 ) ) ;
#17983 = EDGE_CURVE ( 'NONE', #185172, #111286, #65755, .T. ) ;
#17984 = DIRECTION ( 'NONE',  ( 2.952720810173289112E-16, 1.000000000000000000, 6.982962677686266711E-15 ) ) ;
#17985 = CARTESIAN_POINT ( 'NONE',  ( 20.75572585718237661, 8.882316728409755058, -175.9972583987020016 ) ) ;
#17986 = TOROIDAL_SURFACE ( 'NONE', #113666, 0.4000000000000003553, 0.1000000000000000056 ) ;
#17987 = CYLINDRICAL_SURFACE ( 'NONE', #133979, 4.000000000000006217 ) ;
#17988 = CARTESIAN_POINT ( 'NONE',  ( -18.50000000000000000, 71.93512633425886804, -225.1442869522136334 ) ) ;
#17989 = CARTESIAN_POINT ( 'NONE',  ( -21.65000000000000213, 12.43531352672262180, -211.3405985074572300 ) ) ;
#17990 = FACE_OUTER_BOUND ( 'NONE', #225529, .T. ) ;
#17991 = AXIS2_PLACEMENT_3D ( 'NONE', #43228, #65346, #122781 ) ;
#17993 = ADVANCED_FACE ( 'NONE', ( #8872 ), #53089, .T. ) ;
#17992 = DIRECTION ( 'NONE',  ( 1.000000000000000000, 0.000000000000000000, 0.000000000000000000 ) ) ;
#17994 = AXIS2_PLACEMENT_3D ( 'NONE', #193765, #235439, #15135 ) ;
#17995 = EDGE_CURVE ( 'NONE', #227995, #19574, #199026, .T. ) ;
#17996 = DIRECTION ( 'NONE',  ( -1.000000000000000000, 0.000000000000000000, 0.000000000000000000 ) ) ;
#17997 = AXIS2_PLACEMENT_3D ( 'NONE', #6531, #245156, #27428 ) ;
#17998 = EDGE_LOOP ( 'NONE', ( #175306, #196932, #154323, #46991, #83207, #96275, #218169, #53147, #74169, #144698, #228350, #176031, #206038, #167880, #237174, #93757, #104266, #23591 ) ) ;
#17999 = ORIENTED_EDGE ( 'NONE', *, *, #151713, .T. ) ;
#18000 = DIRECTION ( 'NONE',  ( 1.000000000000000000, 0.000000000000000000, 0.000000000000000000 ) ) ;
#18001 = ORIENTED_EDGE ( 'NONE', *, *, #226944, .T. ) ;
#18002 = LINE ( 'NONE', #256567, #42699 ) ;
#18003 = ORIENTED_EDGE ( 'NONE', *, *, #113526, .T. ) ;
#18005 = AXIS2_PLACEMENT_3D ( 'NONE', #56857, #53037, #33529 ) ;
#18004 = CARTESIAN_POINT ( 'NONE',  ( -22.49436431346200038, 64.35004905235869899, -136.5900110142466417 ) ) ;
#18006 = AXIS2_PLACEMENT_3D ( 'NONE', #214221, #237635, #18586 ) ;
#18007 = AXIS2_PLACEMENT_3D ( 'NONE', #185776, #1986, #201475 ) ;
#18008 = EDGE_CURVE ( 'NONE', #109246, #49859, #203115, .T. ) ;
#18009 = VECTOR ( 'NONE', #92936, 1000.000000000000000 ) ;
#18010 = FACE_OUTER_BOUND ( 'NONE', #47671, .T. ) ;
#18011 = CARTESIAN_POINT ( 'NONE',  ( -23.25000000000000000, 8.555687629545136730, -220.7824469969188783 ) ) ;
#18013 = ORIENTED_EDGE ( 'NONE', *, *, #6288, .F. ) ;
#18012 = CARTESIAN_POINT ( 'NONE',  ( -21.07928932188134041, 6.328516656404449492, -33.40110485434561127 ) ) ;
#18014 = ADVANCED_FACE ( 'NONE', ( #25882 ), #186231, .F. ) ;
#18015 = LINE ( 'NONE', #97520, #183199 ) ;
#18016 = ORIENTED_EDGE ( 'NONE', *, *, #46548, .T. ) ;
#18017 = EDGE_CURVE ( 'NONE', #202146, #197574, #187531, .T. ) ;
#18018 = CARTESIAN_POINT ( 'NONE',  ( -22.50000000000000000, 1.115600667400684642E-11, -60.75000000000004974 ) ) ;
#18019 = CARTESIAN_POINT ( 'NONE',  ( -20.94999999999999929, 7.128833340094563376, -233.7327013124401276 ) ) ;
#18020 = DIRECTION ( 'NONE',  ( 0.000000000000000000, 0.9126074666063772600, 0.4088369013363274962 ) ) ;
#18021 = CARTESIAN_POINT ( 'NONE',  ( -23.15000000000000213, 71.65000000001253966, -182.2731074845243882 ) ) ;
#18022 = EDGE_CURVE ( 'NONE', #251754, #59275, #208376, .T. ) ;
#18023 = CARTESIAN_POINT ( 'NONE',  ( 18.59999999999999787, -1.263275465206102233, -108.4018646667464481 ) ) ;
#18024 = EDGE_LOOP ( 'NONE', ( #104683, #130053, #92776, #246641 ) ) ;
#18025 = DIRECTION ( 'NONE',  ( 0.000000000000000000, 0.000000000000000000, -1.000000000000000000 ) ) ;
#18026 = AXIS2_PLACEMENT_3D ( 'NONE', #34438, #56506, #193490 ) ;
#18027 = ORIENTED_EDGE ( 'NONE', *, *, #8179, .F. ) ;
#18030 = VERTEX_POINT ( 'NONE', #147078 ) ;
#18029 = CARTESIAN_POINT ( 'NONE',  ( -22.50000000000000000, 76.00000000001165290, -69.52310748452431710 ) ) ;
#18028 = CARTESIAN_POINT ( 'NONE',  ( -22.50014994444006078, 64.25028026812042015, -203.6061876412429683 ) ) ;
#18031 = AXIS2_PLACEMENT_3D ( 'NONE', #236705, #135029, #196302 ) ;
#18032 = TOROIDAL_SURFACE ( 'NONE', #234509, 0.2000000000000000111, 0.1000000000000000056 ) ;
#18033 = DIRECTION ( 'NONE',  ( -0.000000000000000000, 1.000000000000000000, 6.982962677686266711E-15 ) ) ;
#18034 = CIRCLE ( 'NONE', #172213, 2.599999999999998312 ) ;
#18035 = CARTESIAN_POINT ( 'NONE',  ( -22.57320508075686405, 64.25000000001163869, -69.52310748452435973 ) ) ;
#18036 = EDGE_LOOP ( 'NONE', ( #71969, #246943, #126998, #181418 ) ) ;
#18037 = CARTESIAN_POINT ( 'NONE',  ( 18.40916198585728480, 85.50000000001209344, -129.9229178527008912 ) ) ;
#18038 = EDGE_CURVE ( 'NONE', #108161, #135650, #140566, .T. ) ;
#18039 = DIRECTION ( 'NONE',  ( 0.000000000000000000, 1.000000000000000000, 0.000000000000000000 ) ) ;
#18041 = DIRECTION ( 'NONE',  ( 0.000000000000000000, 0.8814952561688436106, -0.4721928772777334027 ) ) ;
#18040 = B_SPLINE_CURVE_WITH_KNOTS ( 'NONE', 3,
 ( #123895, #67759, #26079, #105565, #127745, #63911, #187730, #27392, #147294, #143441 ),
 .UNSPECIFIED., .F., .F.,
 ( 4, 3, 3, 4 ),
 ( 1.957469226477651626E-15, 8.145022132839031210E-06, 1.905645951092787237E-05, 2.061107371226127689E-05 ),
 .UNSPECIFIED. ) ;
#18043 = EDGE_LOOP ( 'NONE', ( #67699, #16852, #252501, #122915, #215323, #130953, #47247 ) ) ;
#18042 = DIRECTION ( 'NONE',  ( 0.000000000000000000, 1.000000000000000000, 0.000000000000000000 ) ) ;
#18044 = CARTESIAN_POINT ( 'NONE',  ( -21.65000000000000213, 28.93140779147704933, -237.1870821964559184 ) ) ;
#18045 = VERTEX_POINT ( 'NONE', #24613 ) ;
#18046 = CARTESIAN_POINT ( 'NONE',  ( -20.64999999999999858, 1.115600667400684642E-11, -134.0000000000000284 ) ) ;
#18047 = DIRECTION ( 'NONE',  ( 1.000000000000000000, 0.000000000000000000, 0.000000000000000000 ) ) ;
#18048 = CARTESIAN_POINT ( 'NONE',  ( -16.79184697841823493, 44.13976825150989214, -235.2983682103465526 ) ) ;
#18049 = ORIENTED_EDGE ( 'NONE', *, *, #142107, .T. ) ;
#18050 = DIRECTION ( 'NONE',  ( -1.000000000000000000, -1.836970198721029934E-16, 0.000000000000000000 ) ) ;
#18051 = ORIENTED_EDGE ( 'NONE', *, *, #43120, .F. ) ;
#18052 = CYLINDRICAL_SURFACE ( 'NONE', #123069, 0.1000000000000002554 ) ;
#18053 = AXIS2_PLACEMENT_3D ( 'NONE', #147873, #30500, #48749 ) ;
#18054 = CARTESIAN_POINT ( 'NONE',  ( 18.59999999999999787, 77.83585931145570669, -125.0186683157258329 ) ) ;
#18055 = CARTESIAN_POINT ( 'NONE',  ( 22.59080734064467322, 11.47432927991815887, -198.4695429027906926 ) ) ;
#18056 = EDGE_LOOP ( 'NONE', ( #141498, #146830, #40717, #137068, #129026 ) ) ;
#18057 = DIRECTION ( 'NONE',  ( 0.000000000000000000, 0.000000000000000000, -1.000000000000000000 ) ) ;
#18058 = CARTESIAN_POINT ( 'NONE',  ( -22.50000000000000000, 11.75000000001115552, -33.50000000000000000 ) ) ;
#18059 = DIRECTION ( 'NONE',  ( 8.673617379884087537E-15, -0.000000000000000000, 1.000000000000000000 ) ) ;
#18060 = ORIENTED_EDGE ( 'NONE', *, *, #178854, .T. ) ;
#18061 = CARTESIAN_POINT ( 'NONE',  ( -21.64999999999999858, 65.95000000001260787, -190.7731074845244166 ) ) ;
#18062 = DIRECTION ( 'NONE',  ( 0.000000000000000000, 0.2128009952263590909, -0.9770955615653318382 ) ) ;
#18064 = CARTESIAN_POINT ( 'NONE',  ( 22.88900146558018989, 67.29609520889870566, -48.67310748452439384 ) ) ;
#18063 = AXIS2_PLACEMENT_3D ( 'NONE', #160120, #158838, #146603 ) ;
#18065 = EDGE_CURVE ( 'NONE', #237888, #156851, #207077, .T. ) ;
#18066 = VECTOR ( 'NONE', #54822, 1000.000000000000114 ) ;
#18067 = EDGE_LOOP ( 'NONE', ( #183759, #152798, #62884, #11421, #235777, #81441, #227077, #31086, #125338, #97668, #126497, #58550, #105387, #49134, #164218, #246183 ) ) ;
#18068 = CIRCLE ( 'NONE', #76898, 0.1000000000000052097 ) ;
#18069 = CARTESIAN_POINT ( 'NONE',  ( 23.14999999999999858, 76.00000000001244871, -170.0231074845243597 ) ) ;
#18070 = ORIENTED_EDGE ( 'NONE', *, *, #80659, .F. ) ;
#18071 = ORIENTED_EDGE ( 'NONE', *, *, #81387, .F. ) ;
#18072 = ADVANCED_FACE ( 'NONE', ( #127535 ), #94783, .T. ) ;
#18075 = EDGE_LOOP ( 'NONE', ( #40777, #81483, #99974, #63599 ) ) ;
#18074 = VERTEX_POINT ( 'NONE', #28477 ) ;
#18073 = CARTESIAN_POINT ( 'NONE',  ( -18.50000000000000000, 66.75000000001185185, -90.67310748452436542 ) ) ;
#18076 = EDGE_CURVE ( 'NONE', #177623, #116279, #107974, .T. ) ;
#18077 = CARTESIAN_POINT ( 'NONE',  ( 20.94999999999999929, 1.115600667400684642E-11, -100.5000000000000426 ) ) ;
#18078 = ADVANCED_FACE ( 'NONE', ( #167979 ), #247476, .F. ) ;
#18079 = CARTESIAN_POINT ( 'NONE',  ( -21.12757541349819590, 0.005161215820883788274, -161.0266194287484041 ) ) ;
#18080 = FACE_OUTER_BOUND ( 'NONE', #117527, .T. ) ;
#18081 = DIRECTION ( 'NONE',  ( -0.000000000000000000, 0.9876197685951279004, -0.1568667991644694115 ) ) ;
#18082 = DIRECTION ( 'NONE',  ( 0.000000000000000000, 0.000000000000000000, 1.000000000000000000 ) ) ;
#18083 = DIRECTION ( 'NONE',  ( 0.000000000000000000, 0.000000000000000000, 1.000000000000000000 ) ) ;
#18084 = CIRCLE ( 'NONE', #172268, 0.1000000000000000472 ) ;
#18085 = CARTESIAN_POINT ( 'NONE',  ( -18.50000000000000000, 18.34711819382569686, -236.8747682978092541 ) ) ;
#18087 = CARTESIAN_POINT ( 'NONE',  ( 18.59999999999999787, 1.851028230152016674, -45.15391326942249606 ) ) ;
#18086 = DIRECTION ( 'NONE',  ( 0.000000000000000000, 0.001293682058376932620, 0.9999991631930158498 ) ) ;
#18088 = ORIENTED_EDGE ( 'NONE', *, *, #221686, .T. ) ;
#18089 = AXIS2_PLACEMENT_3D ( 'NONE', #144861, #164450, #108322 ) ;
#18090 = VERTEX_POINT ( 'NONE', #164100 ) ;
#18091 = ORIENTED_EDGE ( 'NONE', *, *, #74992, .F. ) ;
#18092 = AXIS2_PLACEMENT_3D ( 'NONE', #158078, #116348, #195888 ) ;
#18093 = DIRECTION ( 'NONE',  ( 0.000000000000000000, 0.000000000000000000, 1.000000000000000000 ) ) ;
#18095 = ORIENTED_EDGE ( 'NONE', *, *, #77801, .T. ) ;
#18094 = CYLINDRICAL_SURFACE ( 'NONE', #187059, 0.1000000000000000056 ) ;
#18096 = DIRECTION ( 'NONE',  ( 0.7071359030028288029, 0.000000000000000000, -0.7070776581708504427 ) ) ;
#18097 = VERTEX_POINT ( 'NONE', #93533 ) ;
#18098 = EDGE_CURVE ( 'NONE', #191031, #143511, #82294, .T. ) ;
#18099 = DIRECTION ( 'NONE',  ( 1.000000000000000000, 0.000000000000000000, 0.000000000000000000 ) ) ;
#18100 = VERTEX_POINT ( 'NONE', #36151 ) ;
#18101 = SPHERICAL_SURFACE ( 'NONE', #37827, 0.1000000000000000056 ) ;
#18102 = ADVANCED_FACE ( 'NONE', ( #213480 ), #34884, .F. ) ;
#18103 = AXIS2_PLACEMENT_3D ( 'NONE', #22003, #101476, #181083 ) ;
#18104 = AXIS2_PLACEMENT_3D ( 'NONE', #165968, #125530, #206361 ) ;
#18105 = ORIENTED_EDGE ( 'NONE', *, *, #204836, .T. ) ;
#18106 = VECTOR ( 'NONE', #108428, 1000.000000000000000 ) ;
#18107 = DIRECTION ( 'NONE',  ( -1.000000000000000000, -2.885090398161910739E-16, -6.283419270304611573E-17 ) ) ;
#18108 = LINE ( 'NONE', #140615, #248768 ) ;
#18110 = ORIENTED_EDGE ( 'NONE', *, *, #168509, .F. ) ;
#18109 = EDGE_LOOP ( 'NONE', ( #83442, #141340, #74889 ) ) ;
#18111 = ORIENTED_EDGE ( 'NONE', *, *, #186388, .T. ) ;
#18112 = CARTESIAN_POINT ( 'NONE',  ( 20.94999999999999574, 74.16465844978745281, -91.46795619196133487 ) ) ;
#18113 = VERTEX_POINT ( 'NONE', #15308 ) ;
#18114 = EDGE_LOOP ( 'NONE', ( #211316, #58507, #160223, #247767 ) ) ;
#18115 = EDGE_CURVE ( 'NONE', #182718, #81112, #174414, .T. ) ;
#18117 = DIRECTION ( 'NONE',  ( 0.5735764363510460484, -0.8191520442889919096, 0.000000000000000000 ) ) ;
#18116 = CIRCLE ( 'NONE', #68191, 0.09999999999998898659 ) ;
#18119 = ORIENTED_EDGE ( 'NONE', *, *, #181748, .F. ) ;
#18118 = CARTESIAN_POINT ( 'NONE',  ( 18.49999999999999289, 10.20857864376269575, -24.65000000000000213 ) ) ;
#18120 = EDGE_CURVE ( 'NONE', #10689, #133593, #53474, .T. ) ;
#18121 = EDGE_CURVE ( 'NONE', #77834, #18296, #203312, .T. ) ;
#18123 = CARTESIAN_POINT ( 'NONE',  ( 20.94999999999999574, 65.52661458509942349, -162.4444530202758870 ) ) ;
#18122 = FACE_OUTER_BOUND ( 'NONE', #11666, .T. ) ;
#18124 = CARTESIAN_POINT ( 'NONE',  ( -23.25000000000000000, 11.65000000001115588, -55.25000000000004974 ) ) ;
#18125 = CARTESIAN_POINT ( 'NONE',  ( -21.05000000000000071, 67.23127455305835554, -235.8551265064784559 ) ) ;
#18126 = DIRECTION ( 'NONE',  ( 0.000000000000000000, 0.000000000000000000, -1.000000000000000000 ) ) ;
#18127 = ORIENTED_EDGE ( 'NONE', *, *, #173328, .T. ) ;
#18128 = AXIS2_PLACEMENT_3D ( 'NONE', #57365, #99052, #236016 ) ;
#18129 = AXIS2_PLACEMENT_3D ( 'NONE', #58747, #60047, #79600 ) ;
#18130 = CIRCLE ( 'NONE', #43083, 0.09999999999999939493 ) ;
#18131 = ORIENTED_EDGE ( 'NONE', *, *, #73558, .T. ) ;
#18133 = AXIS2_PLACEMENT_3D ( 'NONE', #20840, #216438, #239875 ) ;
#18132 = CARTESIAN_POINT ( 'NONE',  ( 18.37172112093835352, 85.57096165225564732, -96.20637303104089710 ) ) ;
#18134 = DIRECTION ( 'NONE',  ( 0.000000000000000000, 0.2617529984165034573, 0.9651348961777156399 ) ) ;
#18135 = EDGE_CURVE ( 'NONE', #231343, #112163, #257408, .T. ) ;
#18136 = VERTEX_POINT ( 'NONE', #153566 ) ;
#18137 = CARTESIAN_POINT ( 'NONE',  ( -21.64999999999999858, 9.350000000011133849, -188.3499999999999659 ) ) ;
#18138 = DIRECTION ( 'NONE',  ( 0.000000000000000000, 0.000000000000000000, -1.000000000000000000 ) ) ;
#18139 = CARTESIAN_POINT ( 'NONE',  ( 20.85000000000000142, 7.120270961697594103, -37.15956304183931991 ) ) ;
#18140 = ORIENTED_EDGE ( 'NONE', *, *, #179806, .T. ) ;
#18141 = ORIENTED_EDGE ( 'NONE', *, *, #18501, .F. ) ;
#18142 = LINE ( 'NONE', #254170, #185671 ) ;
#18143 = EDGE_LOOP ( 'NONE', ( #167267, #140934, #34819, #250659 ) ) ;
#18144 = CARTESIAN_POINT ( 'NONE',  ( -21.05000000000000071, -11.48912529306489994, -131.1000000000000227 ) ) ;
#18145 = ORIENTED_EDGE ( 'NONE', *, *, #90844, .T. ) ;
#18146 = CYLINDRICAL_SURFACE ( 'NONE', #73134, 0.09999999999998898659 ) ;
#18147 = DIRECTION ( 'NONE',  ( 0.000000000000000000, 1.897661533703519897E-16, -1.000000000000000000 ) ) ;
#18149 = CARTESIAN_POINT ( 'NONE',  ( -22.48660254037843842, 55.97436536266720708, -232.8539608197349651 ) ) ;
#18148 = DIRECTION ( 'NONE',  ( -1.000000000000000000, 0.000000000000000000, 0.000000000000000000 ) ) ;
#18150 = CYLINDRICAL_SURFACE ( 'NONE', #90685, 0.1000000000000028644 ) ;
#18151 = EDGE_CURVE ( 'NONE', #193539, #22349, #145030, .T. ) ;
#18152 = CARTESIAN_POINT ( 'NONE',  ( -23.25000000000000000, 51.28888318656201761, -230.2315015618842153 ) ) ;
#18153 = AXIS2_PLACEMENT_3D ( 'NONE', #84286, #79199, #120944 ) ;
#18154 = AXIS2_PLACEMENT_3D ( 'NONE', #158049, #79718, #180144 ) ;
#18155 = DIRECTION ( 'NONE',  ( 0.7071067811865462405, -0.3338907855510739875, -0.6233112732207629625 ) ) ;
#18156 = AXIS2_PLACEMENT_3D ( 'NONE', #6738, #142394, #160717 ) ;
#18158 = VERTEX_POINT ( 'NONE', #90967 ) ;
#18157 = ORIENTED_EDGE ( 'NONE', *, *, #15779, .F. ) ;
#18159 = ORIENTED_EDGE ( 'NONE', *, *, #234208, .T. ) ;
#18160 = CIRCLE ( 'NONE', #197226, 0.1000000000000013933 ) ;
#18161 = EDGE_CURVE ( 'NONE', #54460, #30238, #210921, .T. ) ;
#18162 = DIRECTION ( 'NONE',  ( 0.000000000000000000, 0.000000000000000000, 1.000000000000000000 ) ) ;
#18163 = DIRECTION ( 'NONE',  ( -1.000000000000000000, -3.265361837132813093E-16, 0.000000000000000000 ) ) ;
#18164 = VECTOR ( 'NONE', #149982, 1000.000000000000000 ) ;
#18165 = CARTESIAN_POINT ( 'NONE',  ( -18.50000000000000000, 68.22930980752001062, -227.7331931781284879 ) ) ;
#18166 = CARTESIAN_POINT ( 'NONE',  ( 23.15000000000000213, 87.39257802171813694, -173.0970570643562212 ) ) ;
#18167 =( BOUNDED_SURFACE ( )  B_SPLINE_SURFACE ( 3, 2, ( 
 ( #185028, #205869, #42958 ),
 ( #83327, #2524, #239880 ),
 ( #65078, #143327, #125068 ),
 ( #3824, #144600, #121250 ) ),
 .UNSPECIFIED., .F., .F., .F. ) 
 B_SPLINE_SURFACE_WITH_KNOTS ( ( 4, 4 ),
 ( 3, 3 ),
 ( 0.04058434257139475337, 0.04256401539001600925 ),
 ( 0.000000000000000000, 1.000000000000000000 ),
 .UNSPECIFIED. ) 
 GEOMETRIC_REPRESENTATION_ITEM ( )  RATIONAL_B_SPLINE_SURFACE ( (
 ( 1.000000000000000000, 0.7103081912008133436, 1.000000000000000000),
 ( 1.000000000000000000, 0.7104998333555530010, 1.000000000000000000),
 ( 1.000000000000000000, 0.7107238315755207703, 1.000000000000000000),
 ( 1.000000000000000000, 0.7110073749539380650, 1.000000000000000000) ) ) 
 REPRESENTATION_ITEM ( '' )  SURFACE ( )  );
#18169 = DIRECTION ( 'NONE',  ( 1.000000000000000000, 0.000000000000000000, 0.000000000000000000 ) ) ;
#18168 = DIRECTION ( 'NONE',  ( 1.070816960479510500E-16, -1.000000000000000000, 0.000000000000000000 ) ) ;
#18170 = DIRECTION ( 'NONE',  ( 0.000000000000000000, -0.7071067811865477948, 0.7071067811865473507 ) ) ;
#18171 = ORIENTED_EDGE ( 'NONE', *, *, #255441, .F. ) ;
#18172 = ADVANCED_FACE ( 'NONE', ( #14018 ), #65933, .T. ) ;
#18173 = CARTESIAN_POINT ( 'NONE',  ( 22.47007471830797343, 68.27928934808518591, -69.52310748452437394 ) ) ;
#18174 = ORIENTED_EDGE ( 'NONE', *, *, #251561, .T. ) ;
#18175 = ORIENTED_EDGE ( 'NONE', *, *, #200424, .T. ) ;
#18176 = LINE ( 'NONE', #135541, #112676 ) ;
#18177 = VECTOR ( 'NONE', #2984, 1000.000000000000227 ) ;
#18178 = CARTESIAN_POINT ( 'NONE',  ( 21.87500000000000355, 9.750000000011153745, -88.15000000000004832 ) ) ;
#18179 = DIRECTION ( 'NONE',  ( 0.000000000000000000, 0.000000000000000000, 1.000000000000000000 ) ) ;
#18180 = CARTESIAN_POINT ( 'NONE',  ( 18.60000000000000142, 78.12133356376091342, -231.3112718935514636 ) ) ;
#18181 = VECTOR ( 'NONE', #35494, 1000.000000000000000 ) ;
#18182 = TOROIDAL_SURFACE ( 'NONE', #163932, 12.97499999999999609, 0.1000000000000000056 ) ;
#18183 = EDGE_CURVE ( 'NONE', #240042, #129336, #228269, .T. ) ;
#18184 = DIRECTION ( 'NONE',  ( -0.000000000000000000, -0.000000000000000000, -1.000000000000000000 ) ) ;
#18185 = EDGE_CURVE ( 'NONE', #2351, #91508, #166146, .T. ) ;
#18186 = ORIENTED_EDGE ( 'NONE', *, *, #203589, .F. ) ;
#18187 = ORIENTED_EDGE ( 'NONE', *, *, #104362, .F. ) ;
#18188 =( BOUNDED_SURFACE ( )  B_SPLINE_SURFACE ( 3, 2, ( 
 ( #59865, #162871, #164142 ),
 ( #102842, #122443, #1184 ),
 ( #5025, #201978, #63743 ),
 ( #19495, #143274, #119897 ),
 ( #98983, #62470, #42905 ),
 ( #80718, #84542, #161585 ) ),
 .UNSPECIFIED., .F., .F., .F. ) 
 B_SPLINE_SURFACE_WITH_KNOTS ( ( 4, 2, 4 ),
 ( 3, 3 ),
 ( 0.0001300404313046668353, 0.0003183318589266786276, 0.0005066232865486904741 ),
 ( 0.000000000000000000, 1.000000000000000000 ),
 .UNSPECIFIED. ) 
 GEOMETRIC_REPRESENTATION_ITEM ( )  RATIONAL_B_SPLINE_SURFACE ( (
 ( 1.000000000000000000, 0.7071067811865475727, 1.000000000000000000),
 ( 1.000000000000000000, 0.7625113560559803050, 1.000000000000000000),
 ( 1.000000000000000000, 0.8126073484662428292, 1.000000000000000000),
 ( 1.000000000000000000, 0.8923049332758562491, 1.000000000000000000),
 ( 1.000000000000000000, 0.9231914937750119732, 1.000000000000000000),
 ( 1.000000000000000000, 0.9238795325112866275, 1.000000000000000000) ) ) 
 REPRESENTATION_ITEM ( '' )  SURFACE ( )  );
#18189 = CARTESIAN_POINT ( 'NONE',  ( 18.39999999999999858, 85.60000000001137721, -29.32291809330221355 ) ) ;
#18190 = DIRECTION ( 'NONE',  ( 0.000000000000000000, -1.000000000000000000, 0.000000000000000000 ) ) ;
#18191 = VERTEX_POINT ( 'NONE', #120837 ) ;
#18192 = CARTESIAN_POINT ( 'NONE',  ( 21.14999999999999503, 76.00000000001213607, -136.5231074845242745 ) ) ;
#18193 = CARTESIAN_POINT ( 'NONE',  ( 20.73486653747088582, 18.70606281991848974, -231.7096448200341854 ) ) ;
#18194 = DIRECTION ( 'NONE',  ( 0.000000000000000000, 0.000000000000000000, -1.000000000000000000 ) ) ;
#18195 = DIRECTION ( 'NONE',  ( -0.000000000000000000, 1.000000000000000000, 2.891205793294679805E-16 ) ) ;
#18196 = CARTESIAN_POINT ( 'NONE',  ( -21.05000000000000071, 0.09779029130879170195, 6.257814610476114758 ) ) ;
#18198 = DIRECTION ( 'NONE',  ( -0.000000000000000000, 0.1350103645451945777, -0.9908441862701590219 ) ) ;
#18197 = DIRECTION ( 'NONE',  ( 1.000000000000000000, 0.000000000000000000, 0.000000000000000000 ) ) ;
#18199 = CYLINDRICAL_SURFACE ( 'NONE', #220624, 0.09999999999999939493 ) ;
#18200 = CARTESIAN_POINT ( 'NONE',  ( -18.50000000000000000, 1.866714910057309273, -11.75267524628200633 ) ) ;
#18201 = CIRCLE ( 'NONE', #9994, 11.64999999999999325 ) ;
#18202 = ADVANCED_FACE ( 'NONE', ( #81636 ), #97351, .T. ) ;
#18203 = CYLINDRICAL_SURFACE ( 'NONE', #128939, 0.09999999999998898659 ) ;
#18204 = CARTESIAN_POINT ( 'NONE',  ( 21.08198257630413508, 69.66340326599762989, -203.5957508083089920 ) ) ;
#18206 = ORIENTED_EDGE ( 'NONE', *, *, #106835, .T. ) ;
#18205 = CARTESIAN_POINT ( 'NONE',  ( -17.27223548802641062, 10.34539739141212955, -55.63360617919391160 ) ) ;
#18207 = EDGE_CURVE ( 'NONE', #74110, #190072, #194950, .T. ) ;
#18208 = TOROIDAL_SURFACE ( 'NONE', #255480, 0.2000000000000000111, 0.1000000000000000056 ) ;
#18209 =( BOUNDED_CURVE ( )  B_SPLINE_CURVE ( 3, ( #71295, #188645, #145659, #208233 ),
 .UNSPECIFIED., .F., .T. ) 
 B_SPLINE_CURVE_WITH_KNOTS ( ( 4, 4 ),
 ( 3.192897208853993085, 4.712388980384689674 ),
 .UNSPECIFIED. ) 
 CURVE ( )  GEOMETRIC_REPRESENTATION_ITEM ( )  RATIONAL_B_SPLINE_CURVE ( ( 1.000000000000000000, 0.8166740347213228279, 0.8166740347213228279, 1.000000000000000000 ) ) 
 REPRESENTATION_ITEM ( '' )  );
#18210 = AXIS2_PLACEMENT_3D ( 'NONE', #44694, #244148, #21297 ) ;
#18211 = AXIS2_PLACEMENT_3D ( 'NONE', #101252, #180853, #140420 ) ;
#18212 = EDGE_CURVE ( 'NONE', #203961, #213320, #243683, .T. ) ;
#18213 = DIRECTION ( 'NONE',  ( 1.000000000000000000, 0.000000000000000000, 0.000000000000000000 ) ) ;
#18214 = ORIENTED_EDGE ( 'NONE', *, *, #174641, .F. ) ;
#18215 = DIRECTION ( 'NONE',  ( 1.000000000000000000, 0.000000000000000000, 0.000000000000000000 ) ) ;
#18216 = CARTESIAN_POINT ( 'NONE',  ( 22.57856590037848932, 64.15964591429192865, -247.1965985637075391 ) ) ;
#18217 = ADVANCED_FACE ( 'NONE', ( #176959 ), #149169, .F. ) ;
#18218 = ORIENTED_EDGE ( 'NONE', *, *, #179507, .T. ) ;
#18219 = CARTESIAN_POINT ( 'NONE',  ( -18.59999999999999787, 70.65875701002006792, -79.32975769101238939 ) ) ;
#18221 = EDGE_CURVE ( 'NONE', #102756, #155438, #111724, .T. ) ;
#18220 = CARTESIAN_POINT ( 'NONE',  ( 20.85000000000000142, -1.164121893230052995, -175.4148480855716059 ) ) ;
#18222 = CARTESIAN_POINT ( 'NONE',  ( 22.43288208788031568, 0.004899854896538678728, -21.85034815628092630 ) ) ;
#18223 = VECTOR ( 'NONE', #52357, 999.9999999999998863 ) ;
#18224 = VECTOR ( 'NONE', #25109, 1000.000000000000000 ) ;
#18225 = CIRCLE ( 'NONE', #43172, 0.1999999999999987899 ) ;
#18227 = CARTESIAN_POINT ( 'NONE',  ( 18.59999999999999432, 1.728086936805619311, -87.38443500516778784 ) ) ;
#18226 = VECTOR ( 'NONE', #78702, 1000.000000000000000 ) ;
#18228 = CARTESIAN_POINT ( 'NONE',  ( 18.49999999999999289, 10.24999999999999822, -24.64999999999999503 ) ) ;
#18229 = DIRECTION ( 'NONE',  ( -1.000000000000000000, 2.952720810173289112E-16, 2.061873921506763405E-30 ) ) ;
#18230 = ORIENTED_EDGE ( 'NONE', *, *, #129959, .T. ) ;
#18231 = DIRECTION ( 'NONE',  ( -1.000000000000000000, -0.000000000000000000, -0.000000000000000000 ) ) ;
#18233 = VERTEX_POINT ( 'NONE', #3404 ) ;
#18232 = CARTESIAN_POINT ( 'NONE',  ( 18.79999999999999716, 1.149999999999999911, 21.90000000000000213 ) ) ;
#18234 = PLANE ( 'NONE',  #242477 ) ;
#18235 = CARTESIAN_POINT ( 'NONE',  ( -23.15000000000000213, 76.00000000001215028, -138.5231074845243313 ) ) ;
#18236 = EDGE_CURVE ( 'NONE', #3343, #170827, #37437, .T. ) ;
#18237 = CARTESIAN_POINT ( 'NONE',  ( 20.95512820512820440, 65.37615131629998189, -90.87310748452438247 ) ) ;
#18238 = VERTEX_POINT ( 'NONE', #116956 ) ;
#18239 = DIRECTION ( 'NONE',  ( 1.000000000000000000, -0.000000000000000000, -0.000000000000000000 ) ) ;
#18240 = EDGE_CURVE ( 'NONE', #131589, #23059, #57542, .T. ) ;
#18241 = PRODUCT_CONTEXT ( 'NONE', #208885, 'mechanical' ) ;
#18242 = CARTESIAN_POINT ( 'NONE',  ( -18.49999999999997158, 85.32100840337318459, -95.78716923544637041 ) ) ;
#18243 = ORIENTED_EDGE ( 'NONE', *, *, #174401, .T. ) ;
#18244 = CARTESIAN_POINT ( 'NONE',  ( 20.27550659511088682, 9.216043722520002035, -143.2500000000000284 ) ) ;
#18245 = CYLINDRICAL_SURFACE ( 'NONE', #5029, 0.1000000000000106498 ) ;
#18246 = AXIS2_PLACEMENT_3D ( 'NONE', #65442, #180269, #142412 ) ;
#18247 = CARTESIAN_POINT ( 'NONE',  ( 18.59999999999999787, 85.40000000001185754, -96.14106563635155567 ) ) ;
#18248 = ORIENTED_EDGE ( 'NONE', *, *, #140649, .F. ) ;
#18249 = EDGE_LOOP ( 'NONE', ( #135789, #16745, #59741, #12576 ) ) ;
#18250 = CARTESIAN_POINT ( 'NONE',  ( -23.25000000000000000, -4.756823075239758225, -233.1486023682345490 ) ) ;
#18251 = CARTESIAN_POINT ( 'NONE',  ( -23.25000000000000000, 1.115600667400684642E-11, -100.5000000000000284 ) ) ;
#18252 = DIRECTION ( 'NONE',  ( 7.304098846218134667E-16, -1.000000000000000000, 0.000000000000000000 ) ) ;
#18253 = FACE_OUTER_BOUND ( 'NONE', #3860, .T. ) ;
#18254 = CARTESIAN_POINT ( 'NONE',  ( 18.49999999999999289, 10.41716543472752932, -125.3499999994178182 ) ) ;
#18256 = CYLINDRICAL_SURFACE ( 'NONE', #132920, 0.09999999999999939493 ) ;
#18255 = CARTESIAN_POINT ( 'NONE',  ( -23.15000000000000213, 36.65892442174472876, -249.5511627012454596 ) ) ;
#18257 = CARTESIAN_POINT ( 'NONE',  ( 23.14999999999999503, 11.65000000000000746, -21.35000000000000142 ) ) ;
#18258 = LINE ( 'NONE', #53532, #235243 ) ;
#18259 = CARTESIAN_POINT ( 'NONE',  ( 18.55121869061587958, 65.67252876774480796, -30.44570419949946327 ) ) ;
#18261 = CARTESIAN_POINT ( 'NONE',  ( -16.87845715379269507, 9.957858113908169884, -146.6238006510589287 ) ) ;
#18260 = VECTOR ( 'NONE', #83739, 999.9999999999998863 ) ;
#18262 = ORIENTED_EDGE ( 'NONE', *, *, #168992, .F. ) ;
#18263 = ADVANCED_FACE ( 'NONE', ( #21712 ), #236896, .T. ) ;
#18264 = CIRCLE ( 'NONE', #234742, 0.1999999999999987899 ) ;
#18265 = VERTEX_POINT ( 'NONE', #118238 ) ;
#18266 = CARTESIAN_POINT ( 'NONE',  ( -23.15000000000000213, 11.65000000000000036, 0.000000000000000000 ) ) ;
#18269 = CARTESIAN_POINT ( 'NONE',  ( -21.93642651522410247, 7.327166239325803687, -1.462266042833962457E-16 ) ) ;
#18268 = CARTESIAN_POINT ( 'NONE',  ( -18.50000000000000000, 66.65000000001157332, -57.17310748452438673 ) ) ;
#18267 = CIRCLE ( 'NONE', #159734, 0.1000000000000124678 ) ;
#18270 = LINE ( 'NONE', #183766, #72846 ) ;
#18271 = LINE ( 'NONE', #155250, #174817 ) ;
#18272 = CARTESIAN_POINT ( 'NONE',  ( 13.22461703343585171, 13.11968191886198554, -216.8952266020228592 ) ) ;
#18273 = ORIENTED_EDGE ( 'NONE', *, *, #72639, .F. ) ;
#18274 = ORIENTED_EDGE ( 'NONE', *, *, #203063, .F. ) ;
#18275 = CYLINDRICAL_SURFACE ( 'NONE', #51044, 4.049999999999987388 ) ;
#18276 = ORIENTED_EDGE ( 'NONE', *, *, #1607, .T. ) ;
#18277 = EDGE_CURVE ( 'NONE', #188810, #212797, #82925, .T. ) ;
#18278 = AXIS2_PLACEMENT_3D ( 'NONE', #15352, #75339, #32366 ) ;
#18280 = CARTESIAN_POINT ( 'NONE',  ( 18.31572054635712732, 85.54847543579028013, -29.17253731977572428 ) ) ;
#18279 = CIRCLE ( 'NONE', #14216, 0.09999999999999939493 ) ;
#18281 = AXIS2_PLACEMENT_3D ( 'NONE', #112052, #48204, #211137 ) ;
#18282 = ORIENTED_EDGE ( 'NONE', *, *, #11888, .T. ) ;
#18283 = LINE ( 'NONE', #199512, #239235 ) ;
#18284 = ORIENTED_EDGE ( 'NONE', *, *, #164388, .F. ) ;
#18285 = CARTESIAN_POINT ( 'NONE',  ( -18.39999999999999858, 85.51932773110476660, -163.0501311079649440 ) ) ;
#18286 = LINE ( 'NONE', #116120, #36908 ) ;
#18287 = LINE ( 'NONE', #40464, #170080 ) ;
#18288 = AXIS2_PLACEMENT_3D ( 'NONE', #172790, #213148, #76196 ) ;
#18290 = DIRECTION ( 'NONE',  ( -1.073024830501117725E-15, -0.000000000000000000, -1.000000000000000000 ) ) ;
#18289 = AXIS2_PLACEMENT_3D ( 'NONE', #237146, #117199, #158914 ) ;
#18291 = CARTESIAN_POINT ( 'NONE',  ( 21.05000000000022453, 65.56236711878459289, -242.0759453707015609 ) ) ;
#18294 = DIRECTION ( 'NONE',  ( 0.000000000000000000, 0.000000000000000000, -1.000000000000000000 ) ) ;
#18293 = AXIS2_PLACEMENT_3D ( 'NONE', #94622, #253692, #148185 ) ;
#18292 = CARTESIAN_POINT ( 'NONE',  ( -22.10000000000000142, -11.65000000000000036, 32.89999999999999858 ) ) ;
#18295 = DIRECTION ( 'NONE',  ( -1.000000000000000000, -3.469446951953635015E-14, -2.422701857770461054E-28 ) ) ;
#18296 = VERTEX_POINT ( 'NONE', #256393 ) ;
#18298 = CARTESIAN_POINT ( 'NONE',  ( -16.78493211734303614, 66.05416425680782311, -115.6870565036283978 ) ) ;
#18297 = CARTESIAN_POINT ( 'NONE',  ( -20.85000000000000142, 14.76289716703255728, -235.7888246855571026 ) ) ;
#18299 = AXIS2_PLACEMENT_3D ( 'NONE', #52645, #111354, #167499 ) ;
#18300 = ORIENTED_EDGE ( 'NONE', *, *, #92092, .F. ) ;
#18302 = ORIENTED_EDGE ( 'NONE', *, *, #100533, .F. ) ;
#18301 = DIRECTION ( 'NONE',  ( 0.000000000000000000, 0.000000000000000000, -1.000000000000000000 ) ) ;
#18303 = ORIENTED_EDGE ( 'NONE', *, *, #137818, .F. ) ;
#18304 = LINE ( 'NONE', #241222, #253231 ) ;
#18305 = CARTESIAN_POINT ( 'NONE',  ( -21.53752568622133268, 0.09897446127756706624, -26.71319212545143174 ) ) ;
#18306 = DIRECTION ( 'NONE',  ( -1.000000000000000000, -0.000000000000000000, -0.000000000000000000 ) ) ;
#18307 = AXIS2_PLACEMENT_3D ( 'NONE', #159193, #40545, #241289 ) ;
#18308 = CARTESIAN_POINT ( 'NONE',  ( -20.64999999999999858, 1.115623935689868526E-11, -165.6000000000000227 ) ) ;
#18309 = VERTEX_POINT ( 'NONE', #77808 ) ;
#18310 = CARTESIAN_POINT ( 'NONE',  ( -23.25000000000000355, 5.649999999999983480, -9.250000000000001776 ) ) ;
#18311 = DIRECTION ( 'NONE',  ( -0.7071067811865487940, -0.7071067811865463515, -4.216150419019404490E-15 ) ) ;
#18312 = CIRCLE ( 'NONE', #72488, 0.09999999999998898659 ) ;
#18313 = ORIENTED_EDGE ( 'NONE', *, *, #244569, .F. ) ;
#18314 = TOROIDAL_SURFACE ( 'NONE', #176551, 4.099999999999999645, 0.1000000000000000056 ) ;
#18315 = FACE_OUTER_BOUND ( 'NONE', #4788, .T. ) ;
#18316 = AXIS2_PLACEMENT_3D ( 'NONE', #234403, #901, #197847 ) ;
#18317 = ADVANCED_FACE ( 'NONE', ( #180787 ), #86753, .F. ) ;
#18318 = LINE ( 'NONE', #156584, #89030 ) ;
#18319 = VERTEX_POINT ( 'NONE', #79085 ) ;
#18320 = EDGE_LOOP ( 'NONE', ( #109054, #117596, #136868, #162762 ) ) ;
#18321 = CARTESIAN_POINT ( 'NONE',  ( -20.94999999999999929, 87.39257802171711376, -39.09705706435617856 ) ) ;
#18322 = ORIENTED_EDGE ( 'NONE', *, *, #127089, .T. ) ;
#18323 = FACE_OUTER_BOUND ( 'NONE', #43596, .T. ) ;
#18324 = ORIENTED_EDGE ( 'NONE', *, *, #245581, .T. ) ;
#18325 = DIRECTION ( 'NONE',  ( -3.265361837132813093E-16, -0.9651348961777157509, 0.2617529984165031243 ) ) ;
#18326 = EDGE_CURVE ( 'NONE', #223354, #69705, #232371, .T. ) ;
#18327 = DIRECTION ( 'NONE',  ( 1.836970198721029934E-16, 1.000000000000000000, 6.982962677686266711E-15 ) ) ;
#18328 = CARTESIAN_POINT ( 'NONE',  ( 21.05000000000000071, 61.00122447389661318, -225.2976766370351527 ) ) ;
#18329 = EDGE_CURVE ( 'NONE', #210147, #6205, #199061, .T. ) ;
#18330 = CARTESIAN_POINT ( 'NONE',  ( 20.95289811251229750, 60.87354190138334076, -225.3219200926538690 ) ) ;
#18331 = AXIS2_PLACEMENT_3D ( 'NONE', #232873, #55455, #15095 ) ;
#18333 = B_SPLINE_CURVE_WITH_KNOTS ( 'NONE', 3,
 ( #238143, #139011, #218572, #199034, #20410, #99892, #179488, #242002, #64647, #180757 ),
 .UNSPECIFIED., .F., .F.,
 ( 4, 3, 3, 4 ),
 ( 1.953076773942978418E-15, 8.145022132834464008E-06, 1.905645951092501956E-05, 2.061107371225841053E-05 ),
 .UNSPECIFIED. ) ;
#18332 = AXIS2_PLACEMENT_3D ( 'NONE', #22851, #183194, #123208 ) ;
#18334 = DIRECTION ( 'NONE',  ( 0.000000000000000000, 0.000000000000000000, 1.000000000000000000 ) ) ;
#18335 = ADVANCED_FACE ( 'NONE', ( #206759 ), #232563, .T. ) ;
#18336 = CARTESIAN_POINT ( 'NONE',  ( 23.14999999999999858, 76.00000000001145395, -40.02310748452431710 ) ) ;
#18337 = CARTESIAN_POINT ( 'NONE',  ( 23.25000000000000000, 75.49601185175264106, -250.2710592679604531 ) ) ;
#18338 = CIRCLE ( 'NONE', #64139, 0.09999999999999939493 ) ;
#18339 = EDGE_LOOP ( 'NONE', ( #142797, #191647, #23697, #37940 ) ) ;
#18341 = CARTESIAN_POINT ( 'NONE',  ( -21.05000000000000071, 74.73821383144687047, -94.93660852097883662 ) ) ;
#18340 = CARTESIAN_POINT ( 'NONE',  ( 21.14999999999999503, 31.85509083104287598, -238.8280249686205536 ) ) ;
#18342 = ORIENTED_EDGE ( 'NONE', *, *, #211172, .F. ) ;
#18345 = VERTEX_POINT ( 'NONE', #127224 ) ;
#18344 = DIRECTION ( 'NONE',  ( 0.000000000000000000, 0.9999631594459058581, 0.008583690987093516023 ) ) ;
#18343 = CARTESIAN_POINT ( 'NONE',  ( 23.14999999999999858, 74.00000000001190870, -103.0231074845243171 ) ) ;
#18346 = EDGE_LOOP ( 'NONE', ( #218892, #76411, #209500, #160825 ) ) ;
#18347 = CARTESIAN_POINT ( 'NONE',  ( 22.39999999999999858, 1.115600667400684642E-11, -134.0000000000000000 ) ) ;
#18348 = CARTESIAN_POINT ( 'NONE',  ( 23.15000000000000213, 84.16003609933891028, -218.3250942044780345 ) ) ;
#18349 = AXIS2_PLACEMENT_3D ( 'NONE', #26056, #143417, #160447 ) ;
#18350 = DIRECTION ( 'NONE',  ( 0.000000000000000000, 0.8814952561688429444, -0.4721928772777349015 ) ) ;
#18351 = DIRECTION ( 'NONE',  ( -1.000000000000000000, 0.000000000000000000, 0.000000000000000000 ) ) ;
#18352 = AXIS2_PLACEMENT_3D ( 'NONE', #18144, #37738, #160255 ) ;
#18353 = ORIENTED_EDGE ( 'NONE', *, *, #142074, .T. ) ;
#18354 = DIRECTION ( 'NONE',  ( 0.1538461538461520228, -0.9536447854760599085, 0.2586367802170949082 ) ) ;
#18355 = EDGE_CURVE ( 'NONE', #131461, #51901, #4684, .T. ) ;
#18356 = CARTESIAN_POINT ( 'NONE',  ( -22.39999999999999858, 11.65000000001115588, -66.90000000000004832 ) ) ;
#18357 = AXIS2_PLACEMENT_3D ( 'NONE', #132432, #13765, #16355 ) ;
#18359 = CARTESIAN_POINT ( 'NONE',  ( 18.59999999999999076, 30.76917518201224055, -234.8152055956155380 ) ) ;
#18358 = CARTESIAN_POINT ( 'NONE',  ( 23.50000000000005684, 76.00000000001119815, -36.02310748452479316 ) ) ;
#18361 = VERTEX_POINT ( 'NONE', #28150 ) ;
#18360 = DIRECTION ( 'NONE',  ( -0.000000000000000000, 0.2617529984165031243, 0.9651348961777157509 ) ) ;
#18362 = CONICAL_SURFACE ( 'NONE', #168242, 4.000000000000000000, 0.7853981633974489451 ) ;
#18363 = AXIS2_PLACEMENT_3D ( 'NONE', #41905, #221767, #171806 ) ;
#18364 = EDGE_LOOP ( 'NONE', ( #183795, #244428, #228169, #251987 ) ) ;
#18365 = AXIS2_PLACEMENT_3D ( 'NONE', #113308, #57159, #74224 ) ;
#18366 = DIRECTION ( 'NONE',  ( -1.000000000000000000, -8.673617379884087537E-15, 0.000000000000000000 ) ) ;
#18367 = ORIENTED_EDGE ( 'NONE', *, *, #185402, .F. ) ;
#18368 = CARTESIAN_POINT ( 'NONE',  ( -18.59999999999999787, 76.00000000001165290, -69.52310748452431710 ) ) ;
#18369 = ORIENTED_EDGE ( 'NONE', *, *, #84584, .T. ) ;
#18370 = PLANE ( 'NONE',  #105758 ) ;
#18371 = CARTESIAN_POINT ( 'NONE',  ( 23.25000000000000000, 28.37802281961254991, -258.4449340416662722 ) ) ;
#18372 = CYLINDRICAL_SURFACE ( 'NONE', #105716, 0.09999999999999939493 ) ;
#18373 = AXIS2_PLACEMENT_3D ( 'NONE', #244327, #22749, #63116 ) ;
#18374 = VERTEX_POINT ( 'NONE', #202903 ) ;
#18375 = AXIS2_PLACEMENT_3D ( 'NONE', #71057, #166322, #29382 ) ;
#18376 = MANIFOLD_SOLID_BREP ( 'Stock-MAS-200-1', #140954 ) ;
#18377 = CARTESIAN_POINT ( 'NONE',  ( -20.94999999999999929, 11.60000000001115161, -73.92820323027559937 ) ) ;
#18378 = TOROIDAL_SURFACE ( 'NONE', #122450, 11.70000000000000107, 0.1000000000000000056 ) ;
#18379 = EDGE_CURVE ( 'NONE', #221298, #239536, #5969, .T. ) ;
#18380 = VERTEX_POINT ( 'NONE', #204176 ) ;
#18381 = AXIS2_PLACEMENT_3D ( 'NONE', #166151, #181823, #146525 ) ;
#18382 = ORIENTED_EDGE ( 'NONE', *, *, #90651, .T. ) ;
#18383 = PLANE ( 'NONE',  #19577 ) ;
#18384 = ORIENTED_EDGE ( 'NONE', *, *, #8252, .T. ) ;
#18385 = EDGE_LOOP ( 'NONE', ( #44764, #106456, #205013, #37117 ) ) ;
#18387 = ORIENTED_EDGE ( 'NONE', *, *, #225931, .T. ) ;
#18386 = DIRECTION ( 'NONE',  ( 0.000000000000000000, -1.000000000000000000, -2.891205793294679805E-16 ) ) ;
#18388 = EDGE_CURVE ( 'NONE', #252739, #79944, #63379, .T. ) ;
#18389 = ORIENTED_EDGE ( 'NONE', *, *, #43134, .F. ) ;
#18392 = ORIENTED_EDGE ( 'NONE', *, *, #26052, .T. ) ;
#18391 = VERTEX_POINT ( 'NONE', #184623 ) ;
#18390 = DIRECTION ( 'NONE',  ( 1.000000000000000000, 0.000000000000000000, 0.000000000000000000 ) ) ;
#18393 = ADVANCED_FACE ( 'NONE', ( #103777 ), #132576, .F. ) ;
#18394 = EDGE_CURVE ( 'NONE', #80403, #53303, #85484, .T. ) ;
#18395 = VERTEX_POINT ( 'NONE', #146750 ) ;
#18396 = CIRCLE ( 'NONE', #172004, 0.09999999999999939493 ) ;
#18397 = DIRECTION ( 'NONE',  ( -1.000000000000000000, 0.000000000000000000, 0.000000000000000000 ) ) ;
#18398 = AXIS2_PLACEMENT_3D ( 'NONE', #69978, #184757, #109069 ) ;
#18399 = CARTESIAN_POINT ( 'NONE',  ( 21.05000000000000071, 64.40000000001175806, -76.45131071479988805 ) ) ;
#18400 = CARTESIAN_POINT ( 'NONE',  ( -16.85722902420155123, 14.13441297064198743, -219.1421716323650344 ) ) ;
#18401 = VERTEX_POINT ( 'NONE', #205461 ) ;
#18402 = DIRECTION ( 'NONE',  ( 1.000000000000000000, 0.000000000000000000, 0.000000000000000000 ) ) ;
#18403 = EDGE_CURVE ( 'NONE', #219200, #164553, #219861, .T. ) ;
#18405 = ORIENTED_EDGE ( 'NONE', *, *, #40577, .F. ) ;
#18404 = CARTESIAN_POINT ( 'NONE',  ( 22.32929514600007792, 7.578647565387638174, -167.4009243218860661 ) ) ;
#18406 = CARTESIAN_POINT ( 'NONE',  ( -20.64999999999999858, 7.150000000011155876, -121.7500000000000426 ) ) ;
#18408 = ORIENTED_EDGE ( 'NONE', *, *, #207622, .F. ) ;
#18407 = CARTESIAN_POINT ( 'NONE',  ( -20.64999999999999858, -8.730841121484170131, -90.90192528101572123 ) ) ;
#18409 = ADVANCED_FACE ( 'NONE', ( #185907 ), #163794, .F. ) ;
#18410 = ORIENTED_EDGE ( 'NONE', *, *, #237291, .F. ) ;
#18411 = EDGE_CURVE ( 'NONE', #218484, #176547, #253184, .T. ) ;
#18412 = DIRECTION ( 'NONE',  ( -0.000000000000000000, -0.7397890806274223241, -0.6728388485993012091 ) ) ;
#18413 = FACE_OUTER_BOUND ( 'NONE', #210123, .T. ) ;
#18414 = VERTEX_POINT ( 'NONE', #88061 ) ;
#18415 = ORIENTED_EDGE ( 'NONE', *, *, #60317, .T. ) ;
#18416 = LINE ( 'NONE', #38012, #231055 ) ;
#18417 = DIRECTION ( 'NONE',  ( 0.000000000000000000, 1.000000000000000000, 6.938893903907222067E-15 ) ) ;
#18418 = EDGE_CURVE ( 'NONE', #98837, #9423, #103329, .T. ) ;
#18420 = VERTEX_POINT ( 'NONE', #73695 ) ;
#18419 = ORIENTED_EDGE ( 'NONE', *, *, #35282, .T. ) ;
#18421 = CIRCLE ( 'NONE', #14176, 0.3999999999999975797 ) ;
#18422 = ORIENTED_EDGE ( 'NONE', *, *, #236081, .T. ) ;
#18423 = CARTESIAN_POINT ( 'NONE',  ( 21.05995757104869881, 61.95389314678300963, -221.7884135696254475 ) ) ;
#18424 = ORIENTED_EDGE ( 'NONE', *, *, #197196, .F. ) ;
#18425 = VERTEX_POINT ( 'NONE', #111512 ) ;
#18426 = EDGE_CURVE ( 'NONE', #162457, #26532, #140766, .T. ) ;
#18427 = PLANE ( 'NONE',  #213241 ) ;
#18428 = ORIENTED_EDGE ( 'NONE', *, *, #93496, .F. ) ;
#18429 = EDGE_CURVE ( 'NONE', #89005, #25173, #170044, .T. ) ;
#18430 = CARTESIAN_POINT ( 'NONE',  ( -16.93772744219065984, 12.44552478725261757, -211.1828749433600478 ) ) ;
#18431 = EDGE_CURVE ( 'NONE', #213938, #150130, #207428, .T. ) ;
#18433 = CARTESIAN_POINT ( 'NONE',  ( 21.98333005346336932, 76.00000000001170974, -76.89718281358098295 ) ) ;
#18432 = CARTESIAN_POINT ( 'NONE',  ( -20.65000000000000568, 17.95055421627409231, -233.1200372299043693 ) ) ;
#18434 = VERTEX_POINT ( 'NONE', #74978 ) ;
#18436 = VERTEX_POINT ( 'NONE', #89359 ) ;
#18435 = ORIENTED_EDGE ( 'NONE', *, *, #157878, .F. ) ;
#18437 = PLANE ( 'NONE',  #224302 ) ;
#18438 = CIRCLE ( 'NONE', #118213, 0.09999999999999939493 ) ;
#18439 = ORIENTED_EDGE ( 'NONE', *, *, #20638, .T. ) ;
#18440 = CIRCLE ( 'NONE', #164205, 0.09999999999999895084 ) ;
#18441 = AXIS2_PLACEMENT_3D ( 'NONE', #143560, #82273, #240108 ) ;
#18442 = VECTOR ( 'NONE', #79056, 1000.000000000000000 ) ;
#18443 = CARTESIAN_POINT ( 'NONE',  ( -18.50000000000000711, 85.41920341803854910, -95.77532167409560770 ) ) ;
#18444 = ORIENTED_EDGE ( 'NONE', *, *, #148203, .F. ) ;
#18445 = EDGE_CURVE ( 'NONE', #224075, #94099, #15898, .T. ) ;
#18446 = ORIENTED_EDGE ( 'NONE', *, *, #211998, .T. ) ;
#18447 = ADVANCED_FACE ( 'NONE', ( #154526 ), #211911, .T. ) ;
#18448 = DIRECTION ( 'NONE',  ( 0.000000000000000000, 0.000000000000000000, 1.000000000000000000 ) ) ;
#18449 = ORIENTED_EDGE ( 'NONE', *, *, #188615, .T. ) ;
#18450 = DIRECTION ( 'NONE',  ( -1.000000000000000000, 0.000000000000000000, 0.000000000000000000 ) ) ;
#18451 = CARTESIAN_POINT ( 'NONE',  ( -18.44085059012131822, 33.93338217529301204, -235.0292534346912703 ) ) ;
#18452 = ORIENTED_EDGE ( 'NONE', *, *, #113758, .F. ) ;
#18453 = FACE_OUTER_BOUND ( 'NONE', #223939, .T. ) ;
#18454 = FACE_OUTER_BOUND ( 'NONE', #226452, .T. ) ;
#18456 = FACE_OUTER_BOUND ( 'NONE', #93697, .T. ) ;
#18455 = FACE_OUTER_BOUND ( 'NONE', #237125, .T. ) ;
#18457 = CARTESIAN_POINT ( 'NONE',  ( -20.54999999999999716, 7.128833340094563376, -233.7327013124401276 ) ) ;
#18458 = DIRECTION ( 'NONE',  ( -0.000000000000000000, 0.2128009952263603677, -0.9770955615653313941 ) ) ;
#18459 = DIRECTION ( 'NONE',  ( 0.000000000000000000, 1.429471705525953388E-14, -1.000000000000000000 ) ) ;
#18460 = DIRECTION ( 'NONE',  ( 0.000000000000000000, 1.000000000000000000, 0.000000000000000000 ) ) ;
#18461 = EDGE_CURVE ( 'NONE', #236918, #101582, #94500, .T. ) ;
#18462 = AXIS2_PLACEMENT_3D ( 'NONE', #238662, #196954, #75749 ) ;
#18463 = CARTESIAN_POINT ( 'NONE',  ( 22.43288208788031568, 75.99510014512684108, -148.1727593282433872 ) ) ;
#18464 = DIRECTION ( 'NONE',  ( -1.000000000000000000, 0.000000000000000000, 0.000000000000000000 ) ) ;
#18465 = VECTOR ( 'NONE', #148120, 1000.000000000000000 ) ;
#18466 = VERTEX_POINT ( 'NONE', #112799 ) ;
#18467 = AXIS2_PLACEMENT_3D ( 'NONE', #138892, #21569, #218449 ) ;
#18468 = CIRCLE ( 'NONE', #14401, 4.041421356237306917 ) ;
#18470 = VERTEX_POINT ( 'NONE', #214446 ) ;
#18469 = VERTEX_POINT ( 'NONE', #170253 ) ;
#18471 = ORIENTED_EDGE ( 'NONE', *, *, #138136, .T. ) ;
#18473 = ORIENTED_EDGE ( 'NONE', *, *, #20834, .F. ) ;
#18472 = VECTOR ( 'NONE', #204899, 1000.000000000000114 ) ;
#18474 = CARTESIAN_POINT ( 'NONE',  ( -21.08884785362073089, 0.04978309507788075683, -94.14280663257441972 ) ) ;
#18475 = FACE_OUTER_BOUND ( 'NONE', #7659, .T. ) ;
#18477 = DIRECTION ( 'NONE',  ( 0.000000000000000000, 0.000000000000000000, -1.000000000000000000 ) ) ;
#18476 = DIRECTION ( 'NONE',  ( 0.000000000000000000, 7.056502275159890043E-15, -1.000000000000000000 ) ) ;
#18478 = ORIENTED_EDGE ( 'NONE', *, *, #187578, .F. ) ;
#18479 = CIRCLE ( 'NONE', #164234, 0.09999999999999939493 ) ;
#18480 = EDGE_CURVE ( 'NONE', #252532, #220385, #30720, .T. ) ;
#18481 = FACE_BOUND ( 'NONE', #110793, .T. ) ;
#18483 = CIRCLE ( 'NONE', #201637, 0.09999999999999609201 ) ;
#18482 = SHAPE_REPRESENTATION_RELATIONSHIP ( 'NONE' , 'NONE' ,  #171686, #179045 ) ;
#18485 = AXIS2_PLACEMENT_3D ( 'NONE', #155917, #59319, #235412 ) ;
#18484 = PLANE ( 'NONE',  #166688 ) ;
#18486 = DIRECTION ( 'NONE',  ( 0.000000000000000000, -2.602085213965497408E-13, 1.000000000000000000 ) ) ;
#18487 = EDGE_CURVE ( 'NONE', #102676, #227500, #11130, .T. ) ;
#18488 = CARTESIAN_POINT ( 'NONE',  ( -21.00857864376268935, 57.84918772656043018, -226.1321410194968280 ) ) ;
#18490 = EDGE_LOOP ( 'NONE', ( #35116, #167739, #162359, #148289 ) ) ;
#18489 = AXIS2_PLACEMENT_3D ( 'NONE', #48057, #70225, #250116 ) ;
#18491 = FACE_OUTER_BOUND ( 'NONE', #39288, .T. ) ;
#18492 = EDGE_CURVE ( 'NONE', #197047, #99410, #13680, .T. ) ;
#18493 = VECTOR ( 'NONE', #20634, 1000.000000000000000 ) ;
#18494 = ADVANCED_FACE ( 'NONE', ( #168962 ), #146453, .F. ) ;
#18495 = ORIENTED_EDGE ( 'NONE', *, *, #112962, .F. ) ;
#18496 = DIRECTION ( 'NONE',  ( -1.000000000000000000, -0.000000000000000000, -0.000000000000000000 ) ) ;
#18497 = LINE ( 'NONE', #197115, #194620 ) ;
#18498 = CARTESIAN_POINT ( 'NONE',  ( -18.59999999999999787, 11.75000000001115197, -21.75000000000000355 ) ) ;
#18499 = CARTESIAN_POINT ( 'NONE',  ( -20.54999999999999716, 74.05981308412370367, -56.69398827347101388 ) ) ;
#18500 = CIRCLE ( 'NONE', #205931, 0.1000000000000124678 ) ;
#18501 = EDGE_CURVE ( 'NONE', #158940, #29061, #7687, .T. ) ;
#18502 = DIRECTION ( 'NONE',  ( -1.000000000000000000, 0.000000000000000000, 0.000000000000000000 ) ) ;
#18504 = ORIENTED_EDGE ( 'NONE', *, *, #121536, .T. ) ;
#18503 = AXIS2_PLACEMENT_3D ( 'NONE', #130240, #131533, #11609 ) ;
#18505 = CARTESIAN_POINT ( 'NONE',  ( 22.39999999999999503, 65.20268881533050376, -243.3349219518556765 ) ) ;
#18506 = DIRECTION ( 'NONE',  ( -1.000000000000000000, 7.136802563874199107E-16, 1.554319503706931963E-16 ) ) ;
#18507 = CYLINDRICAL_SURFACE ( 'NONE', #245893, 0.09999999999998898659 ) ;
#18508 = VECTOR ( 'NONE', #214536, 1000.000000000000114 ) ;
#18510 = CARTESIAN_POINT ( 'NONE',  ( 20.94999999999999929, 71.18691588786246882, -114.9646252410481537 ) ) ;
#18509 = CARTESIAN_POINT ( 'NONE',  ( -20.54999999999999716, 27.91464654983916205, -239.9322955902566719 ) ) ;
#18511 = CARTESIAN_POINT ( 'NONE',  ( 20.73486653747088582, 65.69159657275403674, -213.8343546826533554 ) ) ;
#18512 = CARTESIAN_POINT ( 'NONE',  ( 20.94999999999999929, 76.00000000001170974, -69.52310748452431710 ) ) ;
#18513 = ORIENTED_EDGE ( 'NONE', *, *, #105712, .F. ) ;
#18514 = EDGE_CURVE ( 'NONE', #137205, #171663, #532, .T. ) ;
#18515 = EDGE_CURVE ( 'NONE', #141210, #27482, #81330, .T. ) ;
#18516 = ORIENTED_EDGE ( 'NONE', *, *, #133655, .F. ) ;
#18517 = CARTESIAN_POINT ( 'NONE',  ( 23.24999999999999289, 59.16775194334852017, -221.0793150863668473 ) ) ;
#18518 = ORIENTED_EDGE ( 'NONE', *, *, #203059, .F. ) ;
#18519 = ADVANCED_FACE ( 'NONE', ( #98319 ), #136851, .F. ) ;
#18520 = CARTESIAN_POINT ( 'NONE',  ( 23.25000000000000000, -4.756823075239758225, -233.1486023682345490 ) ) ;
#18521 = CIRCLE ( 'NONE', #151814, 0.1000000000000028644 ) ;
#18522 = FACE_OUTER_BOUND ( 'NONE', #155759, .T. ) ;
#18523 = CIRCLE ( 'NONE', #235009, 4.049999999999999822 ) ;
#18524 = EDGE_CURVE ( 'NONE', #24271, #85212, #218284, .T. ) ;
#18525 = DIRECTION ( 'NONE',  ( 0.000000000000000000, -1.000000000000000000, -6.982962677686266711E-15 ) ) ;
#18526 = EDGE_LOOP ( 'NONE', ( #317, #193214, #126025 ) ) ;
#18527 = DIRECTION ( 'NONE',  ( -3.469446951953604722E-14, -0.9999176327611370985, -0.01283462868040260302 ) ) ;
#18528 = CARTESIAN_POINT ( 'NONE',  ( -14.11361717019515538, 9.457426452500055092, -52.00004186840004650 ) ) ;
#18529 = CARTESIAN_POINT ( 'NONE',  ( -18.50016250449483479, 65.70233904877011355, -97.54874109119680270 ) ) ;
#18530 = CIRCLE ( 'NONE', #222694, 0.1000000000000028644 ) ;
#18531 = EDGE_CURVE ( 'NONE', #197537, #41243, #45267, .T. ) ;
#18532 = AXIS2_PLACEMENT_3D ( 'NONE', #214749, #16572, #21698 ) ;
#18533 = DIRECTION ( 'NONE',  ( -0.000000000000000000, 1.000000000000000000, 0.000000000000000000 ) ) ;
#18535 = EDGE_LOOP ( 'NONE', ( #1421, #12074, #22889, #237767 ) ) ;
#18534 = DIRECTION ( 'NONE',  ( 0.000000000000000000, -1.000000000000000000, 0.000000000000000000 ) ) ;
#18537 = CARTESIAN_POINT ( 'NONE',  ( 23.14999999999999858, 7.128833340094563376, -233.7327013124401276 ) ) ;
#18536 = LINE ( 'NONE', #139740, #163035 ) ;
#18538 = DIRECTION ( 'NONE',  ( 1.000000000000000000, 1.875376730785737719E-16, 0.000000000000000000 ) ) ;
#18539 = ADVANCED_FACE ( 'NONE', ( #95774 ), #57933, .T. ) ;
#18540 = CARTESIAN_POINT ( 'NONE',  ( -21.14999999999999858, 11.75000000001115552, -40.28386566297815108 ) ) ;
#18541 = VECTOR ( 'NONE', #46161, 1000.000000000000000 ) ;
#18542 = CARTESIAN_POINT ( 'NONE',  ( 18.59999999999999076, 64.25000000001207923, -128.4231074845243654 ) ) ;
#18543 = CARTESIAN_POINT ( 'NONE',  ( 18.59999999999999076, 62.46832465249013921, -225.2232495205141731 ) ) ;
#18544 = EDGE_LOOP ( 'NONE', ( #229751, #65742, #190842, #17083 ) ) ;
#18545 = ADVANCED_FACE ( 'NONE', ( #59191 ), #237874, .T. ) ;
#18546 = CIRCLE ( 'NONE', #189236, 0.09999999999998898659 ) ;
#18547 = DIRECTION ( 'NONE',  ( 1.000000000000000000, 0.000000000000000000, 0.000000000000000000 ) ) ;
#18548 = DIRECTION ( 'NONE',  ( 1.000000000000000000, 0.000000000000000000, 0.000000000000000000 ) ) ;
#18549 = AXIS2_PLACEMENT_3D ( 'NONE', #51589, #231557, #230254 ) ;
#18550 = AXIS2_PLACEMENT_3D ( 'NONE', #105017, #185878, #42516 ) ;
#18551 = ORIENTED_EDGE ( 'NONE', *, *, #180633, .T. ) ;
#18552 = LINE ( 'NONE', #238881, #102860 ) ;
#18553 = VERTEX_POINT ( 'NONE', #78776 ) ;
#18554 = CARTESIAN_POINT ( 'NONE',  ( 20.94999999999999574, 44.43513953521873106, -247.3415577889845736 ) ) ;
#18555 = CARTESIAN_POINT ( 'NONE',  ( -23.25000000000000000, 76.00000000001213607, -136.5231074845242745 ) ) ;
#18556 = DIRECTION ( 'NONE',  ( 1.000000000000000000, 0.000000000000000000, 0.000000000000000000 ) ) ;
#18557 = ADVANCED_FACE ( 'NONE', ( #220867 ), #173191, .F. ) ;
#18558 = EDGE_LOOP ( 'NONE', ( #173327, #149018, #65673, #2573 ) ) ;
#18559 = AXIS2_PLACEMENT_3D ( 'NONE', #211651, #128254, #48697 ) ;
#18560 = ORIENTED_EDGE ( 'NONE', *, *, #118066, .F. ) ;
#18561 = DIRECTION ( 'NONE',  ( 0.000000000000000000, 1.000000000000000000, 6.608470384673536824E-15 ) ) ;
#18563 = TOROIDAL_SURFACE ( 'NONE', #93003, 11.89999999999999858, 0.1000000000000000056 ) ;
#18562 = DIRECTION ( 'NONE',  ( 1.000000000000000000, 0.000000000000000000, 0.000000000000000000 ) ) ;
#18564 = FACE_OUTER_BOUND ( 'NONE', #95049, .T. ) ;
#18565 = DIRECTION ( 'NONE',  ( 1.000000000000000000, 0.000000000000000000, 0.000000000000000000 ) ) ;
#18567 = DIRECTION ( 'NONE',  ( -0.000000000000000000, -6.982962677686266711E-15, 1.000000000000000000 ) ) ;
#18566 = CARTESIAN_POINT ( 'NONE',  ( -20.85000000000000142, 1.115600667400684642E-11, -67.00000000000000000 ) ) ;
#18568 = CARTESIAN_POINT ( 'NONE',  ( -18.43707690579160641, -9.682403433476396870, -40.15684337741278398 ) ) ;
#18569 = CARTESIAN_POINT ( 'NONE',  ( 21.12400247839515899, 65.27851195598147171, -90.77310748452438816 ) ) ;
#18570 = CARTESIAN_POINT ( 'NONE',  ( 20.94999999999999929, 45.06922343725926083, -238.6062154437373124 ) ) ;
#18571 = AXIS2_PLACEMENT_3D ( 'NONE', #98905, #123650, #239743 ) ;
#18572 = ORIENTED_EDGE ( 'NONE', *, *, #145528, .T. ) ;
#18573 = DIRECTION ( 'NONE',  ( 1.000000000000000000, 0.000000000000000000, 0.000000000000000000 ) ) ;
#18574 = AXIS2_PLACEMENT_3D ( 'NONE', #167917, #248707, #47920 ) ;
#18576 = ORIENTED_EDGE ( 'NONE', *, *, #56872, .T. ) ;
#18575 = CYLINDRICAL_SURFACE ( 'NONE', #128105, 0.09999999999999939493 ) ;
#18577 = AXIS2_PLACEMENT_3D ( 'NONE', #221898, #100660, #219351 ) ;
#18578 = DIRECTION ( 'NONE',  ( 1.661467591126378393E-14, -0.9910827722268042983, -0.1332476588733650935 ) ) ;
#18579 = CARTESIAN_POINT ( 'NONE',  ( 15.48841904831874849, 67.43841904833084300, -123.8731074845243683 ) ) ;
#18580 = CARTESIAN_POINT ( 'NONE',  ( 20.85000000000000142, 1.115600667400684642E-11, -100.5000000000000426 ) ) ;
#18581 = EDGE_CURVE ( 'NONE', #184441, #61365, #253377, .T. ) ;
#18582 = VERTEX_POINT ( 'NONE', #60499 ) ;
#18584 = FACE_OUTER_BOUND ( 'NONE', #51933, .T. ) ;
#18583 = CARTESIAN_POINT ( 'NONE',  ( 18.59999999999999076, 1.115600667400684642E-11, -200.9999999999999432 ) ) ;
#18585 = LINE ( 'NONE', #176392, #245324 ) ;
#18586 = DIRECTION ( 'NONE',  ( -1.000000000000000000, 0.000000000000000000, 0.000000000000000000 ) ) ;
#18587 = DIRECTION ( 'NONE',  ( 0.000000000000000000, 6.982962677686266711E-15, -1.000000000000000000 ) ) ;
#18589 = CARTESIAN_POINT ( 'NONE',  ( -18.58222699835055280, 10.33200063080771969, -139.5931674956643462 ) ) ;
#18588 = SHAPE_REPRESENTATION ( 'Snap Open Cable Crossbars 3', ( #2425 ), #27429 ) ;
#18590 = ORIENTED_EDGE ( 'NONE', *, *, #235884, .T. ) ;
#18591 = CARTESIAN_POINT ( 'NONE',  ( -22.50000000000000000, 31.80488924422933295, -238.9605610896540213 ) ) ;
#18592 = ORIENTED_EDGE ( 'NONE', *, *, #133197, .F. ) ;
#18593 = CARTESIAN_POINT ( 'NONE',  ( 20.94999999999999929, 70.10000000001251408, -180.2422072491807796 ) ) ;
#18594 = ORIENTED_EDGE ( 'NONE', *, *, #36566, .F. ) ;
#18595 = EDGE_CURVE ( 'NONE', #200730, #147041, #219579, .T. ) ;
#18596 = DIRECTION ( 'NONE',  ( 0.000000000000000000, 1.000000000000000000, 0.000000000000000000 ) ) ;
#18597 = AXIS2_PLACEMENT_3D ( 'NONE', #52424, #109832, #151574 ) ;
#18598 = VERTEX_POINT ( 'NONE', #200040 ) ;
#18599 = FACE_OUTER_BOUND ( 'NONE', #234478, .T. ) ;
#18600 = VECTOR ( 'NONE', #234737, 1000.000000000000114 ) ;
#18601 = CARTESIAN_POINT ( 'NONE',  ( -21.05000000000000071, 61.95000000001191154, -97.50941241376341395 ) ) ;
#18602 = ORIENTED_EDGE ( 'NONE', *, *, #186278, .T. ) ;
#18603 = DIRECTION ( 'NONE',  ( 0.000000000000000000, 0.000000000000000000, 1.000000000000000000 ) ) ;
#18604 = CARTESIAN_POINT ( 'NONE',  ( 23.04999999999999716, 67.17743825834537574, -78.77310748452437394 ) ) ;
#18605 = DIRECTION ( 'NONE',  ( 0.000000000000000000, 0.9126074666063660468, 0.4088369013363524762 ) ) ;
#18606 = DIRECTION ( 'NONE',  ( 1.000000000000000000, 0.000000000000000000, 0.000000000000000000 ) ) ;
#18607 = DIRECTION ( 'NONE',  ( -1.000000000000000000, -0.000000000000000000, -0.000000000000000000 ) ) ;
#18608 = CARTESIAN_POINT ( 'NONE',  ( 20.00000000000000355, 62.34315093393704643, -208.9889535843037436 ) ) ;
#18609 = ORIENTED_EDGE ( 'NONE', *, *, #49124, .T. ) ;
#18610 = CARTESIAN_POINT ( 'NONE',  ( 18.49999999999999289, 69.15387683765929694, -99.28538121767448388 ) ) ;
#18611 = VERTEX_POINT ( 'NONE', #21424 ) ;
#18613 = EDGE_LOOP ( 'NONE', ( #181104, #208922, #113591, #240406 ) ) ;
#18612 = DIRECTION ( 'NONE',  ( 0.000000000000000000, 0.000000000000000000, -1.000000000000000000 ) ) ;
#18614 = CIRCLE ( 'NONE', #89890, 0.09999999999999939493 ) ;
#18615 = VERTEX_POINT ( 'NONE', #56630 ) ;
#18616 = AXIS2_PLACEMENT_3D ( 'NONE', #152408, #173279, #214912 ) ;
#18617 = CARTESIAN_POINT ( 'NONE',  ( -18.79999999999999716, 1.885425182446137438, -11.49641995933507843 ) ) ;
#18618 = CARTESIAN_POINT ( 'NONE',  ( 23.14999999999999858, 1.115600667400684642E-11, -167.5000000000000284 ) ) ;
#18619 = LINE ( 'NONE', #153033, #184692 ) ;
#18620 = FACE_OUTER_BOUND ( 'NONE', #50980, .T. ) ;
#18621 = VERTEX_POINT ( 'NONE', #100882 ) ;
#18622 = DIRECTION ( 'NONE',  ( -1.000000000000000000, 0.000000000000000000, 0.000000000000000000 ) ) ;
#18623 = ORIENTED_EDGE ( 'NONE', *, *, #240316, .F. ) ;
#18625 = EDGE_LOOP ( 'NONE', ( #169334, #164077, #142258, #253728 ) ) ;
#18624 = LINE ( 'NONE', #138541, #150946 ) ;
#18626 = EDGE_CURVE ( 'NONE', #193318, #188520, #82645, .T. ) ;
#18627 = SPHERICAL_SURFACE ( 'NONE', #6644, 0.1000000000000000056 ) ;
#18629 = AXIS2_PLACEMENT_3D ( 'NONE', #86013, #243831, #191601 ) ;
#18628 = CARTESIAN_POINT ( 'NONE',  ( -16.92280123533722858, 9.950000000011137047, -79.85063231408514639 ) ) ;
#18630 = ORIENTED_EDGE ( 'NONE', *, *, #67050, .T. ) ;
#18631 = AXIS2_PLACEMENT_3D ( 'NONE', #189267, #249243, #187983 ) ;
#18632 = AXIS2_PLACEMENT_3D ( 'NONE', #110544, #53142, #36167 ) ;
#18633 = AXIS2_PLACEMENT_3D ( 'NONE', #179316, #77592, #39813 ) ;
#18634 = CARTESIAN_POINT ( 'NONE',  ( 20.85000000106584750, 64.25000000001195133, -109.8676028280505790 ) ) ;
#18635 = ORIENTED_EDGE ( 'NONE', *, *, #117869, .F. ) ;
#18636 = PRESENTATION_LAYER_ASSIGNMENT (  '', '', ( #47647 ) ) ;
#18637 = ADVANCED_FACE ( 'NONE', ( #116642 ), #196181, .T. ) ;
#18638 = DIRECTION ( 'NONE',  ( 1.000000000000000000, 0.000000000000000000, 0.000000000000000000 ) ) ;
#18639 = CARTESIAN_POINT ( 'NONE',  ( 15.39170923737819763, 66.61047060254480812, -51.70599957163072702 ) ) ;
#18640 = B_SPLINE_CURVE_WITH_KNOTS ( 'NONE', 3,
 ( #149627, #257619, #38645, #154762, #16527, #119473, #234259 ),
 .UNSPECIFIED., .F., .F.,
 ( 4, 3, 4 ),
 ( 3.469446951953614189E-18, 3.882884552234413736E-05, 5.798605692158458936E-05 ),
 .UNSPECIFIED. ) ;
#18641 = EDGE_CURVE ( 'NONE', #206043, #140485, #132778, .T. ) ;
#18642 = CYLINDRICAL_SURFACE ( 'NONE', #101110, 0.09999999999999216460 ) ;
#18643 = EDGE_CURVE ( 'NONE', #171376, #110731, #61844, .T. ) ;
#18644 = CIRCLE ( 'NONE', #60323, 0.1000000000000028644 ) ;
#18645 = CIRCLE ( 'NONE', #68719, 11.80000000000000426 ) ;
#18646 = EDGE_LOOP ( 'NONE', ( #214146, #127453, #180429, #134608 ) ) ;
#18647 = FACE_BOUND ( 'NONE', #201737, .T. ) ;
#18648 = TOROIDAL_SURFACE ( 'NONE', #197694, 11.65000000000000036, 0.1000000000000000056 ) ;
#18649 = EDGE_CURVE ( 'NONE', #85681, #169497, #44813, .T. ) ;
#18650 = AXIS2_PLACEMENT_3D ( 'NONE', #11562, #114495, #32426 ) ;
#18651 = ORIENTED_EDGE ( 'NONE', *, *, #103497, .F. ) ;
#18652 = FACE_OUTER_BOUND ( 'NONE', #54582, .T. ) ;
#18653 = LINE ( 'NONE', #138561, #49958 ) ;
#18655 = ORIENTED_EDGE ( 'NONE', *, *, #253164, .F. ) ;
#18654 = CARTESIAN_POINT ( 'NONE',  ( 21.08804281139612868, 10.62183430185230826, -146.3499999673788636 ) ) ;
#18656 = DIRECTION ( 'NONE',  ( 0.000000000000000000, 0.9126074666063660468, 0.4088369013363524762 ) ) ;
#18657 = ADVANCED_FACE ( 'NONE', ( #201312 ), #244280, .F. ) ;
#18658 = DIRECTION ( 'NONE',  ( 0.000000000000000000, 0.000000000000000000, 1.000000000000000000 ) ) ;
#18659 = DIRECTION ( 'NONE',  ( -1.000000000000000000, 0.000000000000000000, 0.000000000000000000 ) ) ;
#18660 = CARTESIAN_POINT ( 'NONE',  ( -18.59999999999999787, 77.25000000001239187, -162.2226267301092548 ) ) ;
#18661 = CIRCLE ( 'NONE', #14588, 0.09999999999999939493 ) ;
#18662 = CARTESIAN_POINT ( 'NONE',  ( -23.15000000000000213, 31.85509083104287598, -238.8280249686205536 ) ) ;
#18663 = VECTOR ( 'NONE', #55776, 1000.000000000000000 ) ;
#18664 = CARTESIAN_POINT ( 'NONE',  ( -18.60000000000000142, 85.32100840337339775, -129.2871692354463562 ) ) ;
#18666 = VERTEX_POINT ( 'NONE', #163476 ) ;
#18665 = CARTESIAN_POINT ( 'NONE',  ( -21.14999999999999858, 0.000000000000000000, 0.000000000000000000 ) ) ;
#18667 = AXIS2_PLACEMENT_3D ( 'NONE', #249573, #128340, #69655 ) ;
#18668 = EDGE_CURVE ( 'NONE', #123667, #62433, #182663, .T. ) ;
#18669 = CARTESIAN_POINT ( 'NONE',  ( -23.15000000000000213, -4.914013037343267776, -233.1828366659746905 ) ) ;
#18670 = AXIS2_PLACEMENT_3D ( 'NONE', #256272, #99804, #138923 ) ;
#18671 = VERTEX_POINT ( 'NONE', #225976 ) ;
#18672 = VECTOR ( 'NONE', #67333, 1000.000000000000000 ) ;
#18673 = DIRECTION ( 'NONE',  ( -0.000000000000000000, -0.1298341882520022694, -0.9915357197604853789 ) ) ;
#18674 = CARTESIAN_POINT ( 'NONE',  ( -18.51991288638512856, 85.39243678968547613, -196.3798410805651145 ) ) ;
#18675 = AXIS2_PLACEMENT_3D ( 'NONE', #95367, #237443, #133211 ) ;
#18677 = EDGE_LOOP ( 'NONE', ( #178131, #233185, #2657, #145285 ) ) ;
#18676 = AXIS2_PLACEMENT_3D ( 'NONE', #209476, #206911, #28309 ) ;
#18678 = DIRECTION ( 'NONE',  ( 0.000000000000000000, 0.000000000000000000, -1.000000000000000000 ) ) ;
#18679 = ADVANCED_FACE ( 'NONE', ( #103475 ), #106039, .T. ) ;
#18680 = CARTESIAN_POINT ( 'NONE',  ( -18.46946985241262240, 85.50931722872306295, -62.53644491902446134 ) ) ;
#18681 = ORIENTED_EDGE ( 'NONE', *, *, #102099, .F. ) ;
#18682 = DIRECTION ( 'NONE',  ( 1.000000000000000000, 0.000000000000000000, 0.000000000000000000 ) ) ;
#18683 = DIRECTION ( 'NONE',  ( 1.000000000000000000, 7.136802563874199107E-16, 1.554319503706925307E-16 ) ) ;
#18684 = ADVANCED_FACE ( 'NONE', ( #143901 ), #66937, .F. ) ;
#18685 = ORIENTED_EDGE ( 'NONE', *, *, #252515, .T. ) ;
#18686 = FACE_OUTER_BOUND ( 'NONE', #94763, .T. ) ;
#18687 = ORIENTED_EDGE ( 'NONE', *, *, #13334, .T. ) ;
#18688 = CARTESIAN_POINT ( 'NONE',  ( 5.899999999999997691, -11.25000000000000000, 13.90000000000000213 ) ) ;
#18690 = EDGE_LOOP ( 'NONE', ( #210591, #80799, #13796, #153418 ) ) ;
#18689 = DIRECTION ( 'NONE',  ( 0.000000000000000000, 0.000000000000000000, -1.000000000000000000 ) ) ;
#18691 = FACE_OUTER_BOUND ( 'NONE', #249107, .T. ) ;
#18692 = ORIENTED_EDGE ( 'NONE', *, *, #182802, .F. ) ;
#18693 = AXIS2_PLACEMENT_3D ( 'NONE', #75429, #16724, #96232 ) ;
#18694 = DIRECTION ( 'NONE',  ( 0.000000000000000000, -0.9908441862701600211, -0.1350103645451876666 ) ) ;
#18695 = ORIENTED_EDGE ( 'NONE', *, *, #143026, .T. ) ;
#18696 = CIRCLE ( 'NONE', #131126, 0.1999999999999987899 ) ;
#18698 = VERTEX_POINT ( 'NONE', #181758 ) ;
#18697 = ORIENTED_EDGE ( 'NONE', *, *, #151879, .F. ) ;
#18699 = DIRECTION ( 'NONE',  ( 0.000000000000000000, 1.000000000000000000, 6.982962677686266711E-15 ) ) ;
#18700 = EDGE_LOOP ( 'NONE', ( #145452, #203947, #131846, #245793 ) ) ;
#18701 = ADVANCED_FACE ( 'NONE', ( #91339 ), #249297, .T. ) ;
#18702 = CIRCLE ( 'NONE', #143600, 0.09999999999999939493 ) ;
#18703 = ORIENTED_EDGE ( 'NONE', *, *, #169765, .T. ) ;
#18704 = ADVANCED_FACE ( 'NONE', ( #50888 ), #16087, .T. ) ;
#18705 = AXIS2_PLACEMENT_3D ( 'NONE', #79615, #97880, #216577 ) ;
#18706 = VECTOR ( 'NONE', #78452, 1000.000000000000000 ) ;
#18707 = ORIENTED_EDGE ( 'NONE', *, *, #174259, .T. ) ;
#18708 = LINE ( 'NONE', #151827, #232750 ) ;
#18709 = CARTESIAN_POINT ( 'NONE',  ( -23.15000000000000213, 2.000000000011154189, -120.7753780772379315 ) ) ;
#18710 = EDGE_CURVE ( 'NONE', #140937, #58899, #186757, .T. ) ;
#18712 = ORIENTED_EDGE ( 'NONE', *, *, #37330, .T. ) ;
#18711 = CARTESIAN_POINT ( 'NONE',  ( 23.24999999999999645, 2.100000000000002309, -33.50000000000000000 ) ) ;
#18713 = CARTESIAN_POINT ( 'NONE',  ( 20.27550659511089037, 66.78395627750320784, -123.8731074845243683 ) ) ;
#18714 = ORIENTED_EDGE ( 'NONE', *, *, #168436, .T. ) ;
#18715 = CARTESIAN_POINT ( 'NONE',  ( -23.15000000000000213, 54.31427625645084589, -236.9847968147713857 ) ) ;
#18716 = CARTESIAN_POINT ( 'NONE',  ( -20.64999999999999858, 63.56320957583155717, -222.0641766000055668 ) ) ;
#18718 = ORIENTED_EDGE ( 'NONE', *, *, #191749, .T. ) ;
#18717 = ADVANCED_FACE ( 'NONE', ( #184309 ), #3091, .T. ) ;
#18720 = EDGE_CURVE ( 'NONE', #35026, #130077, #157760, .T. ) ;
#18719 = DIRECTION ( 'NONE',  ( -1.000000000000000000, -0.000000000000000000, -0.000000000000000000 ) ) ;
#18721 = CARTESIAN_POINT ( 'NONE',  ( -21.05000000000000071, 74.75000000001189449, -95.02310748452431710 ) ) ;
#18722 = FACE_OUTER_BOUND ( 'NONE', #35097, .T. ) ;
#18723 = VECTOR ( 'NONE', #221678, 1000.000000000000114 ) ;
#18724 = VERTEX_POINT ( 'NONE', #11821 ) ;
#18725 = DIRECTION ( 'NONE',  ( 0.000000000000000000, -0.9651348961777157509, 0.2617529984165031243 ) ) ;
#18726 = ORIENTED_EDGE ( 'NONE', *, *, #245976, .F. ) ;
#18727 = ORIENTED_EDGE ( 'NONE', *, *, #99089, .T. ) ;
#18728 = DIRECTION ( 'NONE',  ( -1.000000000000000000, -0.000000000000000000, -0.000000000000000000 ) ) ;
#18729 = ADVANCED_FACE ( 'NONE', ( #85179 ), #63079, .F. ) ;
#18730 = EDGE_LOOP ( 'NONE', ( #29690, #166679, #113832, #180043, #132593 ) ) ;
#18731 = ORIENTED_EDGE ( 'NONE', *, *, #217651, .T. ) ;
#18732 = DIRECTION ( 'NONE',  ( 1.186688945009009831E-16, 1.000000000000000000, 6.982962677686266711E-15 ) ) ;
#18733 = CARTESIAN_POINT ( 'NONE',  ( -21.05000000000000071, 76.00000000001267608, -203.5231074845243597 ) ) ;
#18734 = ORIENTED_EDGE ( 'NONE', *, *, #139777, .T. ) ;
#18735 = CIRCLE ( 'NONE', #152032, 0.1999999999999987899 ) ;
#18736 = ORIENTED_EDGE ( 'NONE', *, *, #123635, .F. ) ;
#18737 = CARTESIAN_POINT ( 'NONE',  ( -20.54999999999999716, 7.250000000011155521, -155.2500000000000284 ) ) ;
#18738 = CARTESIAN_POINT ( 'NONE',  ( 22.57856590037849287, 76.00412833007710844, -215.2731659471998000 ) ) ;
#18739 = ORIENTED_EDGE ( 'NONE', *, *, #237753, .F. ) ;
#18740 = ORIENTED_EDGE ( 'NONE', *, *, #39306, .F. ) ;
#18741 = ORIENTED_EDGE ( 'NONE', *, *, #102791, .T. ) ;
#18742 = CIRCLE ( 'NONE', #143640, 0.09999999999999939493 ) ;
#18743 = TOROIDAL_SURFACE ( 'NONE', #139346, 11.89999999999999858, 0.1000000000000000056 ) ;
#18744 = CARTESIAN_POINT ( 'NONE',  ( -20.94999999999999929, 76.00000000001263345, -195.6231074845243540 ) ) ;
#18745 = EDGE_CURVE ( 'NONE', #253449, #185405, #20347, .T. ) ;
#18746 = EDGE_CURVE ( 'NONE', #50997, #164020, #43538, .T. ) ;
#18747 = DIRECTION ( 'NONE',  ( 1.000000000000000000, -2.952720810173289112E-16, -2.061873921506763405E-30 ) ) ;
#18748 = DIRECTION ( 'NONE',  ( 0.000000000000000000, -0.000000000000000000, 1.000000000000000000 ) ) ;
#18749 = DIRECTION ( 'NONE',  ( 6.484947573744954877E-15, 0.9274965247785529332, -0.3738317757009255171 ) ) ;
#18750 = DIRECTION ( 'NONE',  ( 0.000000000000000000, 2.664535259100376486E-15, -1.000000000000000000 ) ) ;
#18751 = DIRECTION ( 'NONE',  ( -1.000000000000000000, 0.000000000000000000, 0.000000000000000000 ) ) ;
#18753 = DIRECTION ( 'NONE',  ( 0.000000000000000000, -0.000000000000000000, 1.000000000000000000 ) ) ;
#18752 = CYLINDRICAL_SURFACE ( 'NONE', #181863, 11.80000000000000426 ) ;
#18754 = DIRECTION ( 'NONE',  ( 0.000000000000000000, -0.2617529984164856383, -0.9651348961777204138 ) ) ;
#18755 = CARTESIAN_POINT ( 'NONE',  ( -21.44999999999999929, 7.250000000011155521, -121.7500000000000426 ) ) ;
#18756 = ADVANCED_FACE ( 'NONE', ( #97712 ), #234692, .T. ) ;
#18757 = CARTESIAN_POINT ( 'NONE',  ( 21.14999999999999503, 4.184122562697137226, -245.3714803909117279 ) ) ;
#18758 = LINE ( 'NONE', #120468, #105170 ) ;
#18759 = AXIS2_PLACEMENT_3D ( 'NONE', #196444, #197733, #257641 ) ;
#18760 = ORIENTED_EDGE ( 'NONE', *, *, #173721, .F. ) ;
#18761 = AXIS2_PLACEMENT_3D ( 'NONE', #106765, #127632, #186328 ) ;
#18763 = ORIENTED_EDGE ( 'NONE', *, *, #218098, .F. ) ;
#18762 = FACE_OUTER_BOUND ( 'NONE', #200068, .T. ) ;
#18764 = FACE_OUTER_BOUND ( 'NONE', #133946, .T. ) ;
#18765 = SPHERICAL_SURFACE ( 'NONE', #198758, 0.1000000000000000056 ) ;
#18766 = VERTEX_POINT ( 'NONE', #216402 ) ;
#18767 = LINE ( 'NONE', #216958, #78950 ) ;
#18768 = EDGE_CURVE ( 'NONE', #207133, #256678, #211878, .T. ) ;
#18769 = CARTESIAN_POINT ( 'NONE',  ( -17.11825945287481687, 10.05000000001113847, -54.35000000000000853 ) ) ;
#18770 = ORIENTED_EDGE ( 'NONE', *, *, #213862, .F. ) ;
#18772 = CARTESIAN_POINT ( 'NONE',  ( -23.25000000000000000, 1.115600667400684642E-11, -200.9999999999999432 ) ) ;
#18771 = AXIS2_PLACEMENT_3D ( 'NONE', #127435, #4889, #85697 ) ;
#18773 = VECTOR ( 'NONE', #2930, 1000.000000000000000 ) ;
#18774 = DIRECTION ( 'NONE',  ( 0.5000000000001141309, -6.047423072554455661E-15, 0.8660254037843729824 ) ) ;
#18775 = CARTESIAN_POINT ( 'NONE',  ( 18.54999999999999716, 67.25000000001251976, -182.6731074845244223 ) ) ;
#18776 = EDGE_CURVE ( 'NONE', #144062, #183616, #166111, .T. ) ;
#18777 = CARTESIAN_POINT ( 'NONE',  ( -21.14999999999999858, 10.21728496540352182, -227.9671432372868765 ) ) ;
#18779 = ORIENTED_EDGE ( 'NONE', *, *, #225541, .T. ) ;
#18778 = CARTESIAN_POINT ( 'NONE',  ( -21.05000000000000071, 64.40000000001195701, -109.9513107147998880 ) ) ;
#18781 = ORIENTED_EDGE ( 'NONE', *, *, #45954, .F. ) ;
#18780 = CARTESIAN_POINT ( 'NONE',  ( -18.50000000000000000, 85.48068669529084218, -96.08199231576638510 ) ) ;
#18783 = ADVANCED_FACE ( 'NONE', ( #96437 ), #120337, .T. ) ;
#18782 = DIRECTION ( 'NONE',  ( -1.000000000000000000, 0.000000000000000000, 0.000000000000000000 ) ) ;
#18784 = CARTESIAN_POINT ( 'NONE',  ( 21.14261333020286671, 10.71569264925490650, -12.25000000000021316 ) ) ;
#18785 = DIRECTION ( 'NONE',  ( -0.000000000000000000, 0.2128009952263597848, -0.9770955615653316162 ) ) ;
#18786 = FACE_OUTER_BOUND ( 'NONE', #179225, .T. ) ;
#18788 = FACE_OUTER_BOUND ( 'NONE', #231203, .T. ) ;
#18787 = DIRECTION ( 'NONE',  ( 0.000000000000000000, -1.000000000000000000, 0.000000000000000000 ) ) ;
#18790 = EDGE_CURVE ( 'NONE', #255597, #95948, #120144, .T. ) ;
#18789 = CARTESIAN_POINT ( 'NONE',  ( -20.85000000000000142, 43.26562470876307742, -245.1245614952171081 ) ) ;
#18791 = CARTESIAN_POINT ( 'NONE',  ( 20.99999999999999645, 9.750000000011137757, -176.7499999999999716 ) ) ;
#18792 = VECTOR ( 'NONE', #141538, 1000.000000000000000 ) ;
#18793 = CARTESIAN_POINT ( 'NONE',  ( 23.24999999999999645, 5.000000000011153745, -121.5947339810869465 ) ) ;
#18794 = CARTESIAN_POINT ( 'NONE',  ( -18.41809261886924887, 85.68240331476904714, -163.3662639344331922 ) ) ;
#18795 = VECTOR ( 'NONE', #195704, 1000.000000000000000 ) ;
#18796 = CARTESIAN_POINT ( 'NONE',  ( 20.94999999999999929, 74.16465844978819177, -191.9679561919613775 ) ) ;
#18797 = AXIS2_PLACEMENT_3D ( 'NONE', #251010, #72420, #254825 ) ;
#18798 = EDGE_LOOP ( 'NONE', ( #131641, #211155, #99168 ) ) ;
#18799 = AXIS2_PLACEMENT_3D ( 'NONE', #254413, #140922, #75810 ) ;
#18800 = ADVANCED_FACE ( 'NONE', ( #211280 ), #93889, .T. ) ;
#18801 = CYLINDRICAL_SURFACE ( 'NONE', #134618, 0.1000000000000028644 ) ;
#18803 = EDGE_CURVE ( 'NONE', #108455, #201436, #216129, .T. ) ;
#18802 = EDGE_CURVE ( 'NONE', #64202, #192209, #140966, .T. ) ;
#18804 = ORIENTED_EDGE ( 'NONE', *, *, #88965, .T. ) ;
#18805 = ORIENTED_EDGE ( 'NONE', *, *, #101475, .T. ) ;
#18806 = DIRECTION ( 'NONE',  ( 1.000000000000000000, 0.000000000000000000, 0.000000000000000000 ) ) ;
#18807 = DIRECTION ( 'NONE',  ( 0.000000000000000000, -0.1350103645451807555, -0.9908441862701610203 ) ) ;
#18808 = ORIENTED_EDGE ( 'NONE', *, *, #35537, .T. ) ;
#18809 = VERTEX_POINT ( 'NONE', #235961 ) ;
#18810 = PRESENTATION_STYLE_ASSIGNMENT (( #117906 ) ) ;
#18811 = ORIENTED_EDGE ( 'NONE', *, *, #109709, .F. ) ;
#18813 = EDGE_CURVE ( 'NONE', #57380, #174151, #57311, .T. ) ;
#18812 = B_SPLINE_CURVE_WITH_KNOTS ( 'NONE', 3,
 ( #238959, #198531, #60296, #21216, #98114, #235104, #19916, #78579, #137268, #194713, #79844, #158174, #138531, #39501, #255888, #1608, #135974, #156875, #141141, #40781, #119013, #236375, #159426, #100682, #199844, #220672 ),
 .UNSPECIFIED., .F., .F.,
 ( 4, 2, 2, 2, 2, 2, 2, 2, 2, 2, 2, 2, 4 ),
 ( 0.005476422646581303143, 0.006160811967703551384, 0.006845201288825798758, 0.007187395949386892954, 0.007529590609947988886, 0.007871785270509083082, 0.008213979931070177279, 0.008556174591631273210, 0.008898369252192367407, 0.009240563912753461603, 0.009582758573314555800, 0.01026714789443679970, 0.01095153721555904534 ),
 .UNSPECIFIED. ) ;
#18814 = EDGE_CURVE ( 'NONE', #22873, #7608, #149527, .T. ) ;
#18815 = CIRCLE ( 'NONE', #56412, 11.65000000000000746 ) ;
#18816 = ORIENTED_EDGE ( 'NONE', *, *, #87612, .T. ) ;
#18817 = VECTOR ( 'NONE', #256664, 1000.000000000000114 ) ;
#18818 = FACE_OUTER_BOUND ( 'NONE', #199780, .T. ) ;
#18819 = DIRECTION ( 'NONE',  ( -0.000000000000000000, -0.000000000000000000, -1.000000000000000000 ) ) ;
#18820 = CARTESIAN_POINT ( 'NONE',  ( -18.59999999999999787, 13.53887499352833146, -219.6971619212644669 ) ) ;
#18821 = AXIS2_PLACEMENT_3D ( 'NONE', #154933, #14136, #93646 ) ;
#18822 = DIRECTION ( 'NONE',  ( 0.000000000000000000, -0.9525900758537790836, 0.3042567129660269099 ) ) ;
#18823 = CARTESIAN_POINT ( 'NONE',  ( 15.74999999999999645, 9.349999999999983658, -16.75000000000000000 ) ) ;
#18824 = EDGE_CURVE ( 'NONE', #129423, #136769, #132959, .T. ) ;
#18825 = CARTESIAN_POINT ( 'NONE',  ( 21.13614978966382196, 65.53011441033059725, -242.1276392481308619 ) ) ;
#18826 = CARTESIAN_POINT ( 'NONE',  ( -23.15000000000000213, 23.34004772283015328, -229.2004250369967338 ) ) ;
#18828 = EDGE_LOOP ( 'NONE', ( #206792, #162092, #39824, #21012 ) ) ;
#18827 = CARTESIAN_POINT ( 'NONE',  ( -22.37643362114956957, 75.90091862633033770, -77.14889747848272350 ) ) ;
#18830 = SPHERICAL_SURFACE ( 'NONE', #62651, 0.1000000000000000056 ) ;
#18829 = DIRECTION ( 'NONE',  ( 1.000000000000000000, 0.000000000000000000, 0.000000000000000000 ) ) ;
#18831 = FACE_OUTER_BOUND ( 'NONE', #67298, .T. ) ;
#18832 = ORIENTED_EDGE ( 'NONE', *, *, #163849, .T. ) ;
#18833 = AXIS2_PLACEMENT_3D ( 'NONE', #233825, #17348, #218083 ) ;
#18834 = CARTESIAN_POINT ( 'NONE',  ( 20.94999999999999929, 65.69992488703364586, -222.9708107233114163 ) ) ;
#18835 = DIRECTION ( 'NONE',  ( 0.000000000000000000, 0.000000000000000000, -1.000000000000000000 ) ) ;
#18836 = AXIS2_PLACEMENT_3D ( 'NONE', #25087, #4196, #198551 ) ;
#18837 = ORIENTED_EDGE ( 'NONE', *, *, #146318, .T. ) ;
#18838 = ADVANCED_FACE ( 'NONE', ( #157773 ), #237265, .T. ) ;
#18840 = CARTESIAN_POINT ( 'NONE',  ( 22.45305468355010703, 76.10085836911147794, -81.27267460801404297 ) ) ;
#18839 = DIRECTION ( 'NONE',  ( 1.224646799147353207E-16, -0.9651348961777157509, 0.2617529984165031243 ) ) ;
#18841 = EDGE_CURVE ( 'NONE', #201875, #49319, #141148, .T. ) ;
#18842 = DIRECTION ( 'NONE',  ( -1.000000000000000000, 0.000000000000000000, -0.000000000000000000 ) ) ;
#18843 = CARTESIAN_POINT ( 'NONE',  ( 19.92426406871192412, 16.76897757977919667, -222.7804130109902871 ) ) ;
#18844 = EDGE_LOOP ( 'NONE', ( #60694, #136667, #223098, #9010 ) ) ;
#18845 = DIRECTION ( 'NONE',  ( 0.000000000000000000, -0.000000000000000000, 1.000000000000000000 ) ) ;
#18846 = VECTOR ( 'NONE', #184193, 1000.000000000000114 ) ;
#18847 = DIRECTION ( 'NONE',  ( -0.000000000000000000, 1.000000000000000000, 6.982962677686266711E-15 ) ) ;
#18848 = DIRECTION ( 'NONE',  ( 0.000000000000000000, 0.9126074666063660468, 0.4088369013363524762 ) ) ;
#18850 = ADVANCED_FACE ( 'NONE', ( #252957 ), #153663, .T. ) ;
#18849 = CARTESIAN_POINT ( 'NONE',  ( 33.30000000000001137, 3.332938107839120701, 33.00000000000000000 ) ) ;
#18851 = ORIENTED_EDGE ( 'NONE', *, *, #146752, .F. ) ;
#18852 = CIRCLE ( 'NONE', #10676, 0.09999999999999939493 ) ;
#18853 = VECTOR ( 'NONE', #149222, 1000.000000000000000 ) ;
#18854 = LINE ( 'NONE', #176669, #13055 ) ;
#18856 = EDGE_CURVE ( 'NONE', #207360, #229115, #174511, .T. ) ;
#18855 = DIRECTION ( 'NONE',  ( 0.000000000000000000, -7.026728003956695223E-15, 1.000000000000000000 ) ) ;
#18857 = SPHERICAL_SURFACE ( 'NONE', #111804, 0.1000000000000000056 ) ;
#18858 = DIRECTION ( 'NONE',  ( -0.8660254037844653530, 0.000000000000000000, 0.4999999999999539257 ) ) ;
#18859 = DIRECTION ( 'NONE',  ( 1.000000000000000000, 0.000000000000000000, 0.000000000000000000 ) ) ;
#18861 = ORIENTED_EDGE ( 'NONE', *, *, #78798, .F. ) ;
#18860 = DIRECTION ( 'NONE',  ( 1.000000000000000000, 0.000000000000000000, 0.000000000000000000 ) ) ;
#18862 = LINE ( 'NONE', #257417, #168459 ) ;
#18863 = CARTESIAN_POINT ( 'NONE',  ( -16.96982749440708815, 66.05000000001187743, -89.89832907571251042 ) ) ;
#18864 = LINE ( 'NONE', #21463, #79560 ) ;
#18865 = CARTESIAN_POINT ( 'NONE',  ( -20.94999999999999929, 1.148907358139439339E-11, -201.0000000000015064 ) ) ;
#18866 = EDGE_CURVE ( 'NONE', #3656, #131987, #150785, .T. ) ;
#18867 = CARTESIAN_POINT ( 'NONE',  ( 20.94999999999999929, 2.739812813550879245, -213.5801053551551547 ) ) ;
#18869 = ORIENTED_EDGE ( 'NONE', *, *, #11708, .T. ) ;
#18868 = FACE_OUTER_BOUND ( 'NONE', #133814, .T. ) ;
#18870 = CARTESIAN_POINT ( 'NONE',  ( 22.49231231312462853, 64.35001509633508476, -170.0841603721258082 ) ) ;
#18871 = DIRECTION ( 'NONE',  ( 1.000000000000000000, 0.000000000000000000, 0.000000000000000000 ) ) ;
#18872 = DIRECTION ( 'NONE',  ( 1.000000000000000000, 0.000000000000000000, -0.000000000000000000 ) ) ;
#18873 = ORIENTED_EDGE ( 'NONE', *, *, #166916, .T. ) ;
#18874 = CARTESIAN_POINT ( 'NONE',  ( -18.59999999999999787, 66.65000000001150227, -48.17310748452438673 ) ) ;
#18875 = AXIS2_PLACEMENT_3D ( 'NONE', #23150, #126057, #2256 ) ;
#18876 = CARTESIAN_POINT ( 'NONE',  ( 21.13435531349836438, 76.00000000001242029, -176.5168285481167914 ) ) ;
#18877 = CARTESIAN_POINT ( 'NONE',  ( 18.49999999999999289, 64.35000000001173248, -81.27310748452440237 ) ) ;
#18879 = VECTOR ( 'NONE', #104918, 1000.000000000000000 ) ;
#18878 = DIRECTION ( 'NONE',  ( 0.000000000000000000, -0.9651348961777157509, 0.2617529984165031243 ) ) ;
#18880 = CIRCLE ( 'NONE', #243744, 11.80000000000000426 ) ;
#18881 = DIRECTION ( 'NONE',  ( 0.000000000000000000, 0.9999631594459053030, 0.008583690987162899758 ) ) ;
#18882 = CARTESIAN_POINT ( 'NONE',  ( 23.14999999999999858, 45.51971589178210564, -240.3486087337583399 ) ) ;
#18883 = ORIENTED_EDGE ( 'NONE', *, *, #178395, .T. ) ;
#18884 = ORIENTED_EDGE ( 'NONE', *, *, #223352, .F. ) ;
#18885 = VECTOR ( 'NONE', #116506, 1000.000000000000000 ) ;
#18886 = CARTESIAN_POINT ( 'NONE',  ( 22.39999999999999503, -1.657885652111590336, -193.3876638332971538 ) ) ;
#18887 = AXIS2_PLACEMENT_3D ( 'NONE', #79426, #23357, #20779 ) ;
#18888 = CARTESIAN_POINT ( 'NONE',  ( -22.39999999999999858, 0.1000000000111554016, -134.0000000000000000 ) ) ;
#18889 =( BOUNDED_SURFACE ( )  B_SPLINE_SURFACE ( 3, 2, ( 
 ( #247768, #224349, #108270 ),
 ( #243906, #6583, #208664 ),
 ( #9162, #65277, #165692 ),
 ( #86092, #164390, #104378 ),
 ( #206081, #223061, #123986 ),
 ( #126543, #168282, #45715 ) ),
 .UNSPECIFIED., .F., .F., .F. ) 
 B_SPLINE_SURFACE_WITH_KNOTS ( ( 4, 2, 4 ),
 ( 3, 3 ),
 ( 1.570796326794895448, 2.356194490192343505, 3.141592653589791784 ),
 ( 0.000000000000000000, 1.000000000000000000 ),
 .UNSPECIFIED. ) 
 GEOMETRIC_REPRESENTATION_ITEM ( )  RATIONAL_B_SPLINE_SURFACE ( (
 ( 1.000000000000000000, 0.7071067811865597852, 1.000000000000000000),
 ( 1.000000000000000000, 0.6611148371788475586, 1.000000000000000000),
 ( 1.000000000000000000, 0.6092287576683730332, 1.000000000000000000),
 ( 1.000000000000000000, 0.5278258667070037102, 1.000000000000000000),
 ( 1.000000000000000000, 0.4993418825324473231, 1.000000000000000000),
 ( 1.000000000000000000, 0.4999999999999960587, 1.000000000000000000) ) ) 
 REPRESENTATION_ITEM ( '' )  SURFACE ( )  );
#18890 = DIRECTION ( 'NONE',  ( 0.000000000000000000, 0.9856811345164832039, 0.1686199900910280158 ) ) ;
#18891 = DIRECTION ( 'NONE',  ( 0.000000000000000000, 0.3042567129660006531, 0.9525900758537875213 ) ) ;
#18892 = ORIENTED_EDGE ( 'NONE', *, *, #190249, .F. ) ;
#18893 = TOROIDAL_SURFACE ( 'NONE', #239664, 0.2000000000000000111, 0.1000000000000000056 ) ;
#18895 = AXIS2_PLACEMENT_3D ( 'NONE', #90973, #110535, #47992 ) ;
#18894 = DIRECTION ( 'NONE',  ( 0.000000000000000000, 1.000000000000000000, 0.000000000000000000 ) ) ;
#18896 = CARTESIAN_POINT ( 'NONE',  ( 20.12481660106788084, 11.05867956686307352, -207.0105110312538272 ) ) ;
#18897 = AXIS2_PLACEMENT_3D ( 'NONE', #52027, #127583, #105411 ) ;
#18898 = CYLINDRICAL_SURFACE ( 'NONE', #28998, 0.09999999999998898659 ) ;
#18899 = DIRECTION ( 'NONE',  ( 1.000000000000000000, 0.000000000000000000, 0.000000000000000000 ) ) ;
#18900 = VERTEX_POINT ( 'NONE', #139416 ) ;
#18901 = DIRECTION ( 'NONE',  ( 0.000000000000000000, -0.9126074666063660468, -0.4088369013363524762 ) ) ;
#18902 = ORIENTED_EDGE ( 'NONE', *, *, #59822, .T. ) ;
#18903 = DIRECTION ( 'NONE',  ( -4.336808689941752679E-15, -0.8103668758649498205, 0.5859227990963324917 ) ) ;
#18904 = VERTEX_POINT ( 'NONE', #181151 ) ;
#18905 = CARTESIAN_POINT ( 'NONE',  ( -17.01764560440359730, 9.950000000011138823, -154.7500000007889298 ) ) ;
#18906 = LINE ( 'NONE', #218376, #18508 ) ;
#18907 = DIRECTION ( 'NONE',  ( -0.000000000000000000, -0.1298341882519737922, -0.9915357197604890427 ) ) ;
#18909 = EDGE_LOOP ( 'NONE', ( #206407, #165913, #107249, #170297 ) ) ;
#18908 = TOROIDAL_SURFACE ( 'NONE', #123162, 0.6000000000000004219, 0.1000000000000000056 ) ;
#18910 = CARTESIAN_POINT ( 'NONE',  ( 20.89999999999999858, -11.65000000000000036, 11.89999999999999680 ) ) ;
#18911 = DIRECTION ( 'NONE',  ( 0.000000000000000000, 0.9651348961777157509, -0.2617529984165031243 ) ) ;
#18912 = DIRECTION ( 'NONE',  ( -1.000000000000000000, -0.000000000000000000, -0.000000000000000000 ) ) ;
#18913 = ORIENTED_EDGE ( 'NONE', *, *, #114941, .T. ) ;
#18914 = DIRECTION ( 'NONE',  ( -1.476360405086644309E-16, 1.000000000000000000, -0.000000000000000000 ) ) ;
#18916 = ORIENTED_EDGE ( 'NONE', *, *, #107374, .T. ) ;
#18915 = CARTESIAN_POINT ( 'NONE',  ( -21.00000000000000000, 0.000000000000000000, 0.000000000000000000 ) ) ;
#18917 = EDGE_CURVE ( 'NONE', #142612, #250542, #70442, .T. ) ;
#18918 = DIRECTION ( 'NONE',  ( 0.000000000000000000, 0.9955484899852913294, -0.09425075112701486457 ) ) ;
#18919 = CARTESIAN_POINT ( 'NONE',  ( -18.54159361262948735, 85.46313213550538990, -162.9739852682313597 ) ) ;
#18920 = AXIS2_PLACEMENT_3D ( 'NONE', #42348, #22810, #102276 ) ;
#18921 = EDGE_LOOP ( 'NONE', ( #212775, #154333, #199069, #61402 ) ) ;
#18922 = CARTESIAN_POINT ( 'NONE',  ( 20.97224591636398472, 65.37484658384894942, -191.2731815798608466 ) ) ;
#18923 = DIRECTION ( 'NONE',  ( 0.000000000000000000, 0.000000000000000000, -1.000000000000000000 ) ) ;
#18924 = DIRECTION ( 'NONE',  ( 0.000000000000000000, -0.8814952561688430555, 0.4721928772777346239 ) ) ;
#18925 = VERTEX_POINT ( 'NONE', #122456 ) ;
#18926 = CARTESIAN_POINT ( 'NONE',  ( 21.14999999999999858, 6.540656951712400691, -134.0000000000000000 ) ) ;
#18927 = EDGE_CURVE ( 'NONE', #114500, #142483, #62031, .T. ) ;
#18928 = DIRECTION ( 'NONE',  ( 0.000000000000000000, 0.000000000000000000, -1.000000000000000000 ) ) ;
#18929 = CARTESIAN_POINT ( 'NONE',  ( -23.25000000000000000, 87.65000000001246860, -173.1231074845242688 ) ) ;
#18930 = EDGE_CURVE ( 'NONE', #89024, #120435, #220265, .T. ) ;
#18931 = ORIENTED_EDGE ( 'NONE', *, *, #73852, .F. ) ;
#18932 = VERTEX_POINT ( 'NONE', #218964 ) ;
#18933 = AXIS2_PLACEMENT_3D ( 'NONE', #4648, #142867, #26832 ) ;
#18934 = ADVANCED_FACE ( 'NONE', ( #242377 ), #203680, .T. ) ;
#18935 = VECTOR ( 'NONE', #98725, 1000.000000000000000 ) ;
#18936 = ORIENTED_EDGE ( 'NONE', *, *, #232710, .T. ) ;
#18937 = EDGE_CURVE ( 'NONE', #112246, #233645, #112118, .T. ) ;
#18938 = DIRECTION ( 'NONE',  ( 0.000000000000000000, 0.9651348961777157509, -0.2617529984165031243 ) ) ;
#18940 = EDGE_LOOP ( 'NONE', ( #84965, #239730, #165000, #251265 ) ) ;
#18939 = FACE_OUTER_BOUND ( 'NONE', #59178, .T. ) ;
#18941 = DIRECTION ( 'NONE',  ( 0.000000000000000000, 0.008583690987127625890, 0.9999631594459055250 ) ) ;
#18942 = LINE ( 'NONE', #239292, #190526 ) ;
#18943 = EDGE_CURVE ( 'NONE', #36331, #108582, #5031, .T. ) ;
#18944 = DIRECTION ( 'NONE',  ( -1.652117596168391700E-15, 1.000000000000000000, 6.982962677686266711E-15 ) ) ;
#18945 = DIRECTION ( 'NONE',  ( -1.000000000000000000, 0.000000000000000000, 0.000000000000000000 ) ) ;
#18946 = DIRECTION ( 'NONE',  ( 0.000000000000000000, -0.9651348961777161950, 0.2617529984165014589 ) ) ;
#18947 = CARTESIAN_POINT ( 'NONE',  ( -16.94107738177414291, 14.24304960796391306, -219.3391119284832484 ) ) ;
#18949 = EDGE_LOOP ( 'NONE', ( #100185, #247221, #47829, #251205 ) ) ;
#18948 = CARTESIAN_POINT ( 'NONE',  ( -16.87036670365548474, 66.01058118071088643, -182.5435473672224020 ) ) ;
#18951 = ORIENTED_EDGE ( 'NONE', *, *, #44673, .F. ) ;
#18950 = DIRECTION ( 'NONE',  ( 1.000000000000000000, 0.000000000000000000, 0.000000000000000000 ) ) ;
#18953 = CARTESIAN_POINT ( 'NONE',  ( 20.87600722750343252, 10.33112638556969465, -72.59012289269746532 ) ) ;
#18952 = FACE_OUTER_BOUND ( 'NONE', #224335, .T. ) ;
#18954 = EDGE_CURVE ( 'NONE', #26637, #113, #1751, .T. ) ;
#18955 = ORIENTED_EDGE ( 'NONE', *, *, #32733, .F. ) ;
#18956 = ORIENTED_EDGE ( 'NONE', *, *, #230496, .T. ) ;
#18957 = CARTESIAN_POINT ( 'NONE',  ( -20.54999999999999716, 2.400000000011155432, -180.7246219227620543 ) ) ;
#18958 = CARTESIAN_POINT ( 'NONE',  ( -20.85000000000000142, 76.00000000001142553, -36.02310748452432421 ) ) ;
#18959 = AXIS2_PLACEMENT_3D ( 'NONE', #11039, #72314, #153158 ) ;
#18960 = EDGE_CURVE ( 'NONE', #244396, #109775, #216385, .T. ) ;
#18961 = CYLINDRICAL_SURFACE ( 'NONE', #121716, 0.09999999999999939493 ) ;
#18962 = DIRECTION ( 'NONE',  ( 0.000000000000000000, 0.2128009952263485993, -0.9770955615653341697 ) ) ;
#18963 = DIRECTION ( 'NONE',  ( 0.000000000000000000, 0.1298341882519953583, 0.9915357197604861561 ) ) ;
#18964 = DIRECTION ( 'NONE',  ( 0.000000000000000000, 0.000000000000000000, 1.000000000000000000 ) ) ;
#18965 = EDGE_CURVE ( 'NONE', #30421, #81280, #140717, .T. ) ;
#18966 = CARTESIAN_POINT ( 'NONE',  ( 21.14999999999999858, 69.35000000001259934, -191.3731074845244109 ) ) ;
#18967 = ORIENTED_EDGE ( 'NONE', *, *, #105931, .T. ) ;
#18968 = EDGE_LOOP ( 'NONE', ( #46890, #65261, #70565, #102436 ) ) ;
#18969 = DIRECTION ( 'NONE',  ( 1.000000000000000000, 0.000000000000000000, -0.000000000000000000 ) ) ;
#18970 = AXIS2_PLACEMENT_3D ( 'NONE', #101760, #243867, #62681 ) ;
#18971 = AXIS2_PLACEMENT_3D ( 'NONE', #74171, #33772, #97508 ) ;
#18972 = ORIENTED_EDGE ( 'NONE', *, *, #257998, .F. ) ;
#18973 = DIRECTION ( 'NONE',  ( 0.000000000000000000, -7.086529944415894657E-15, 1.000000000000000000 ) ) ;
#18974 = CARTESIAN_POINT ( 'NONE',  ( -18.40000000000000213, 5.649999999999983480, -12.65000000000000213 ) ) ;
#18975 = AXIS2_PLACEMENT_3D ( 'NONE', #75948, #77213, #3792 ) ;
#18976 = AXIS2_PLACEMENT_3D ( 'NONE', #209885, #211157, #71664 ) ;
#18977 = DIRECTION ( 'NONE',  ( 0.000000000000000000, -1.000000000000000000, -1.445602896647339410E-16 ) ) ;
#18978 =( BOUNDED_SURFACE ( )  B_SPLINE_SURFACE ( 3, 2, ( 
 ( #12930, #233259, #11637 ),
 ( #36332, #155002, #234501 ),
 ( #31226, #170746, #211102 ),
 ( #32506, #112017, #191565 ) ),
 .UNSPECIFIED., .F., .F., .T. ) 
 B_SPLINE_SURFACE_WITH_KNOTS ( ( 4, 4 ),
 ( 3, 3 ),
 ( 4.712388980384689674, 5.765869716888553320 ),
 ( 0.000000000000000000, 1.000000000000000000 ),
 .UNSPECIFIED. ) 
 GEOMETRIC_REPRESENTATION_ITEM ( )  RATIONAL_B_SPLINE_SURFACE ( (
 ( 1.000000000000000000, 0.7071067811865366926, 1.000000000000000000),
 ( 1.000000000000000000, 0.7953136715914939092, 1.000000000000000000),
 ( 1.000000000000000000, 0.8646876308614021012, 1.000000000000000000),
 ( 1.000000000000000000, 0.8984936768950643193, 1.000000000000000000) ) ) 
 REPRESENTATION_ITEM ( '' )  SURFACE ( )  );
#18979 = LINE ( 'NONE', #17690, #122042 ) ;
#18980 = MECHANICAL_DESIGN_GEOMETRIC_PRESENTATION_REPRESENTATION (  '', ( #185591 ), #93821 ) ;
#18981 = ORIENTED_EDGE ( 'NONE', *, *, #211864, .F. ) ;
#18982 = CARTESIAN_POINT ( 'NONE',  ( -12.30589683808040391, 66.64325398293378555, -119.3197477631602084 ) ) ;
#18983 = EDGE_LOOP ( 'NONE', ( #71893, #80288, #157638, #182612 ) ) ;
#18984 = DIRECTION ( 'NONE',  ( 0.000000000000000000, 0.000000000000000000, -1.000000000000000000 ) ) ;
#18985 = ORIENTED_EDGE ( 'NONE', *, *, #251384, .T. ) ;
#18986 = CARTESIAN_POINT ( 'NONE',  ( -16.89081410710458542, 9.951318529858268036, -87.85440591983640957 ) ) ;
#18987 = LINE ( 'NONE', #98486, #63233 ) ;
#18988 = CARTESIAN_POINT ( 'NONE',  ( -21.05000000000000071, 1.115600667400684642E-11, -100.5000000000000284 ) ) ;
#18989 = VERTEX_POINT ( 'NONE', #159031 ) ;
#18990 = FACE_OUTER_BOUND ( 'NONE', #107341, .T. ) ;
#18992 = ORIENTED_EDGE ( 'NONE', *, *, #208866, .F. ) ;
#18991 = CARTESIAN_POINT ( 'NONE',  ( -20.64999999999999858, 76.00000000001195133, -103.0231074845243171 ) ) ;
#18993 = CARTESIAN_POINT ( 'NONE',  ( -18.59999999999999787, 76.00000000001190870, -103.0231074845243029 ) ) ;
#18995 = VERTEX_POINT ( 'NONE', #40382 ) ;
#18994 = TOROIDAL_SURFACE ( 'NONE', #27427, 7.791421356237335338, 0.1000000000000000056 ) ;
#18996 = AXIS2_PLACEMENT_3D ( 'NONE', #126179, #8820, #10100 ) ;
#18997 = ADVANCED_FACE ( 'NONE', ( #119907 ), #224892, .F. ) ;
#18998 = CIRCLE ( 'NONE', #60682, 0.09999999999999967248 ) ;
#18999 = DIRECTION ( 'NONE',  ( 0.000000000000000000, 0.8814952561688429444, -0.4721928772777345684 ) ) ;
#19000 = VERTEX_POINT ( 'NONE', #70201 ) ;
#19001 = AXIS2_PLACEMENT_3D ( 'NONE', #177717, #44601, #61590 ) ;
#19002 = CARTESIAN_POINT ( 'NONE',  ( -23.25000000000000000, 24.26958830762006869, -252.6664436919618879 ) ) ;
#19003 = ADVANCED_FACE ( 'NONE', ( #25922 ), #165435, .T. ) ;
#19004 = CARTESIAN_POINT ( 'NONE',  ( 22.49999999999999645, 64.09620057108240587, -247.0754729532595206 ) ) ;
#19005 = ADVANCED_FACE ( 'NONE', ( #227964 ), #101990, .T. ) ;
#19006 = DIRECTION ( 'NONE',  ( 0.000000000000000000, -0.1071148137998806232, -0.9942466578594150173 ) ) ;
#19007 = CARTESIAN_POINT ( 'NONE',  ( 18.49999999999999645, 7.128833340094563376, -233.7327013124401276 ) ) ;
#19008 = AXIS2_PLACEMENT_3D ( 'NONE', #76998, #193111, #93985 ) ;
#19009 = TOROIDAL_SURFACE ( 'NONE', #118996, 11.65000000000000036, 0.1000000000000000056 ) ;
#19010 = VECTOR ( 'NONE', #126521, 999.9999999999998863 ) ;
#19011 = CARTESIAN_POINT ( 'NONE',  ( -20.85000000000000142, 87.75000000001246292, -170.0231074845242745 ) ) ;
#19013 = ORIENTED_EDGE ( 'NONE', *, *, #197365, .F. ) ;
#19012 = EDGE_CURVE ( 'NONE', #202965, #57945, #24649, .T. ) ;
#19014 = EDGE_CURVE ( 'NONE', #158859, #124985, #168031, .T. ) ;
#19015 = CARTESIAN_POINT ( 'NONE',  ( 23.15000000000000213, 84.59626168225457832, -60.07297996737398194 ) ) ;
#19016 = CARTESIAN_POINT ( 'NONE',  ( 21.05000000000000071, 6.304516329275134723, -100.5211033080587413 ) ) ;
#19017 = CARTESIAN_POINT ( 'NONE',  ( -21.05000000000000071, 11.75000000001115197, -160.6583993101029364 ) ) ;
#19018 = EDGE_CURVE ( 'NONE', #91747, #257602, #232918, .T. ) ;
#19019 = VERTEX_POINT ( 'NONE', #147131 ) ;
#19020 = DIRECTION ( 'NONE',  ( -1.000000000000000000, 2.849773892568378313E-16, -7.728835255496647986E-17 ) ) ;
#19022 = EDGE_CURVE ( 'NONE', #182384, #10704, #224098, .T. ) ;
#19021 = ORIENTED_EDGE ( 'NONE', *, *, #170538, .T. ) ;
#19023 = CARTESIAN_POINT ( 'NONE',  ( -20.94999999999999929, 77.16412189325360771, -162.1082593989527254 ) ) ;
#19024 = VERTEX_POINT ( 'NONE', #45471 ) ;
#19025 = CIRCLE ( 'NONE', #6553, 0.5000000000000004441 ) ;
#19026 = AXIS2_PLACEMENT_3D ( 'NONE', #130804, #36886, #53844 ) ;
#19027 = CARTESIAN_POINT ( 'NONE',  ( -21.14999999999999858, 6.257814610487270279, -33.40220970869120265 ) ) ;
#19028 = CARTESIAN_POINT ( 'NONE',  ( -21.05000000000000071, 76.00000000001213607, -136.5231074845242745 ) ) ;
#19029 = EDGE_CURVE ( 'NONE', #213934, #86243, #224519, .T. ) ;
#19031 = VERTEX_POINT ( 'NONE', #125023 ) ;
#19030 = CARTESIAN_POINT ( 'NONE',  ( -20.64999999999999858, 68.75000000001230660, -157.7731074845244166 ) ) ;
#19032 = CARTESIAN_POINT ( 'NONE',  ( -18.51555513499602412, 9.055083425720873436, -245.3745321141128670 ) ) ;
#19033 = VERTEX_POINT ( 'NONE', #108023 ) ;
#19034 = CIRCLE ( 'NONE', #119018, 0.09999999999999939493 ) ;
#19035 = TOROIDAL_SURFACE ( 'NONE', #160736, 0.4000000000000015210, 0.1000000000000000056 ) ;
#19036 = CARTESIAN_POINT ( 'NONE',  ( 18.49999999999998934, 69.45000000001260787, -193.5060803140843859 ) ) ;
#19037 = DIRECTION ( 'NONE',  ( 1.000000000000000000, -0.000000000000000000, -0.000000000000000000 ) ) ;
#19038 = VERTEX_POINT ( 'NONE', #204538 ) ;
#19039 = ORIENTED_EDGE ( 'NONE', *, *, #212330, .F. ) ;
#19040 = CARTESIAN_POINT ( 'NONE',  ( 23.14999999999999503, 11.75000000001116263, -155.3500000000000227 ) ) ;
#19041 = CARTESIAN_POINT ( 'NONE',  ( 20.95443524775735256, 67.12144573613906573, -94.48938520892421877 ) ) ;
#19042 = VERTEX_POINT ( 'NONE', #105407 ) ;
#19043 = CARTESIAN_POINT ( 'NONE',  ( 21.04999999999999716, 10.01651311888475249, -228.1334776613284987 ) ) ;
#19044 = ORIENTED_EDGE ( 'NONE', *, *, #224253, .F. ) ;
#19045 = ORIENTED_EDGE ( 'NONE', *, *, #78182, .F. ) ;
#19046 = EDGE_CURVE ( 'NONE', #26389, #92187, #207127, .T. ) ;
#19047 = DIRECTION ( 'NONE',  ( 1.000000000000000000, 0.000000000000000000, 0.000000000000000000 ) ) ;
#19048 = ADVANCED_FACE ( 'NONE', ( #8918 ), #235279, .F. ) ;
#19049 = EDGE_CURVE ( 'NONE', #117472, #119183, #228636, .T. ) ;
#19051 = ORIENTED_EDGE ( 'NONE', *, *, #119051, .T. ) ;
#19050 = DIRECTION ( 'NONE',  ( 0.000000000000000000, 0.000000000000000000, 1.000000000000000000 ) ) ;
#19052 = B_SPLINE_CURVE_WITH_KNOTS ( 'NONE', 3,
 ( #134403, #71905, #112316, #35373, #152747, #194430, #232272, #114867, #174899, #185745 ),
 .UNSPECIFIED., .F., .F.,
 ( 4, 3, 3, 4 ),
 ( 4.906538933386797396E-18, 0.0002000000000002859679, 0.001000000000045107602, 0.001967863649472130407 ),
 .UNSPECIFIED. ) ;
#19053 = AXIS2_PLACEMENT_3D ( 'NONE', #122596, #203406, #6471 ) ;
#19054 = CARTESIAN_POINT ( 'NONE',  ( -22.57320508075687115, 11.75000000001115552, -100.5000000000000284 ) ) ;
#19055 = CARTESIAN_POINT ( 'NONE',  ( 21.15000000000005187, 74.16448838626247664, -47.52760213295649550 ) ) ;
#19056 = TOROIDAL_SURFACE ( 'NONE', #60734, 0.2000000000000000111, 0.1000000000000000056 ) ;
#19057 = DIRECTION ( 'NONE',  ( 0.000000000000000000, 0.000000000000000000, 1.000000000000000000 ) ) ;
#19059 = DIRECTION ( 'NONE',  ( 1.000000000000000000, -7.304098846218134667E-16, -5.100424963727255829E-30 ) ) ;
#19058 = CARTESIAN_POINT ( 'NONE',  ( 20.95443524775735256, 8.878554263883968289, -42.03372227560014807 ) ) ;
#19060 = CYLINDRICAL_SURFACE ( 'NONE', #111366, 0.1000000000000028644 ) ;
#19061 = VECTOR ( 'NONE', #47831, 1000.000000000000000 ) ;
#19062 = DIRECTION ( 'NONE',  ( 0.000000000000000000, 0.9979305700607959961, 0.06430067914209769420 ) ) ;
#19063 = CARTESIAN_POINT ( 'NONE',  ( 18.50000000000000000, -9.399999999988843058, -40.79725975966329798 ) ) ;
#19064 = DIRECTION ( 'NONE',  ( 0.000000000000000000, -7.429790795770644761E-15, 1.000000000000000000 ) ) ;
#19066 = EDGE_LOOP ( 'NONE', ( #158436, #99733, #129575, #39325 ) ) ;
#19065 = TOROIDAL_SURFACE ( 'NONE', #164835, 0.2000000000000000111, 0.1000000000000000056 ) ;
#19068 = ORIENTED_EDGE ( 'NONE', *, *, #243088, .T. ) ;
#19067 = DIRECTION ( 'NONE',  ( -1.000000000000000000, -0.000000000000000000, -0.000000000000000000 ) ) ;
#19069 = ORIENTED_EDGE ( 'NONE', *, *, #157422, .F. ) ;
#19070 = DIRECTION ( 'NONE',  ( 0.000000000000000000, 0.8659859643398412077, -0.5000683049008356473 ) ) ;
#19071 = VERTEX_POINT ( 'NONE', #96130 ) ;
#19072 = CARTESIAN_POINT ( 'NONE',  ( 20.04142135623730070, 64.25000000001222134, -148.6731074845244507 ) ) ;
#19073 = AXIS2_PLACEMENT_3D ( 'NONE', #219213, #237515, #97962 ) ;
#19074 = AXIS2_PLACEMENT_3D ( 'NONE', #51509, #230175, #74986 ) ;
#19075 = ORIENTED_EDGE ( 'NONE', *, *, #234321, .F. ) ;
#19076 = CIRCLE ( 'NONE', #177350, 0.2000000000000003997 ) ;
#19077 = CYLINDRICAL_SURFACE ( 'NONE', #61509, 0.09999999999999939493 ) ;
#19079 = EDGE_LOOP ( 'NONE', ( #157306, #32382, #196079, #34169 ) ) ;
#19078 = VERTEX_POINT ( 'NONE', #56988 ) ;
#19080 = ORIENTED_EDGE ( 'NONE', *, *, #80881, .F. ) ;
#19081 = ORIENTED_EDGE ( 'NONE', *, *, #91399, .F. ) ;
#19082 = CYLINDRICAL_SURFACE ( 'NONE', #233673, 0.09999999999999939493 ) ;
#19083 = DIRECTION ( 'NONE',  ( 1.000000000000000000, 0.000000000000000000, 0.000000000000000000 ) ) ;
#19085 = EDGE_LOOP ( 'NONE', ( #249951, #100389, #1733, #256198 ) ) ;
#19084 = DIRECTION ( 'NONE',  ( 0.000000000000000000, 0.7106264324241517993, -0.7035695228903270371 ) ) ;
#19086 = AXIS2_PLACEMENT_3D ( 'NONE', #197995, #217548, #158907 ) ;
#19087 = CARTESIAN_POINT ( 'NONE',  ( -21.53752568617673191, 33.79390208800049322, -243.3979355726113738 ) ) ;
#19088 = DIRECTION ( 'NONE',  ( -0.000000000000000000, -0.2617529984165031243, -0.9651348961777157509 ) ) ;
#19089 = VERTEX_POINT ( 'NONE', #33664 ) ;
#19090 = LINE ( 'NONE', #152225, #179210 ) ;
#19091 = VERTEX_POINT ( 'NONE', #250096 ) ;
#19092 = CARTESIAN_POINT ( 'NONE',  ( -23.15000000000000213, 1.115600667400684642E-11, -167.5000000000000284 ) ) ;
#19094 = ORIENTED_EDGE ( 'NONE', *, *, #126746, .F. ) ;
#19093 = CARTESIAN_POINT ( 'NONE',  ( -21.13614978966382196, 6.499104701844943044, -167.5000000000000000 ) ) ;
#19095 = CARTESIAN_POINT ( 'NONE',  ( 21.05000000000000071, 11.46684968301824625, -245.9610388612851750 ) ) ;
#19097 = ADVANCED_FACE ( 'NONE', ( #192693 ), #152305, .F. ) ;
#19096 = CARTESIAN_POINT ( 'NONE',  ( -20.94999999999999929, 76.00000000001234923, -167.1231074845243825 ) ) ;
#19098 = CARTESIAN_POINT ( 'NONE',  ( 20.87155475150661132, 11.75000000001115907, -60.09558652915745114 ) ) ;
#19099 = ORIENTED_EDGE ( 'NONE', *, *, #96921, .F. ) ;
#19101 = CARTESIAN_POINT ( 'NONE',  ( -12.25000000000000178, 62.10905854918435409, -217.1108499610990918 ) ) ;
#19100 = CARTESIAN_POINT ( 'NONE',  ( -16.97683809663752186, 9.950000000011137047, -46.90236401819648648 ) ) ;
#19103 = EDGE_CURVE ( 'NONE', #102134, #217631, #145397, .T. ) ;
#19102 = CARTESIAN_POINT ( 'NONE',  ( -12.25000000000000000, 66.65000000001184333, -86.15736431725046884 ) ) ;
#19104 = CARTESIAN_POINT ( 'NONE',  ( -21.05000000000000071, 1.115600667400684642E-11, -130.0000000000000284 ) ) ;
#19105 = AXIS2_PLACEMENT_3D ( 'NONE', #128512, #106352, #65968 ) ;
#19106 = AXIS2_PLACEMENT_3D ( 'NONE', #132661, #167960, #248758 ) ;
#19107 = LINE ( 'NONE', #81612, #1526 ) ;
#19108 = TOROIDAL_SURFACE ( 'NONE', #64891, 0.6000000000000013101, 0.1000000000000000056 ) ;
#19110 = CARTESIAN_POINT ( 'NONE',  ( 23.14999999999999858, 4.000000000011155521, -134.0000000000000284 ) ) ;
#19109 = AXIS2_PLACEMENT_3D ( 'NONE', #59823, #79396, #117264 ) ;
#19111 = ORIENTED_EDGE ( 'NONE', *, *, #104104, .F. ) ;
#19112 = VERTEX_POINT ( 'NONE', #153610 ) ;
#19113 = ORIENTED_EDGE ( 'NONE', *, *, #149217, .F. ) ;
#19114 = B_SPLINE_CURVE_WITH_KNOTS ( 'NONE', 3,
 ( #103937, #183505, #25714, #105201 ),
 .UNSPECIFIED., .F., .F.,
 ( 4, 4 ),
 ( 3.469446951953614189E-18, 0.0001058379652594852396 ),
 .UNSPECIFIED. ) ;
#19115 = EDGE_CURVE ( 'NONE', #170560, #56802, #82825, .T. ) ;
#19116 = CARTESIAN_POINT ( 'NONE',  ( -17.04761207306821191, 10.02645087340893326, -180.1499999999999488 ) ) ;
#19117 = EDGE_CURVE ( 'NONE', #121991, #68040, #87140, .T. ) ;
#19118 = ORIENTED_EDGE ( 'NONE', *, *, #176937, .F. ) ;
#19119 = LINE ( 'NONE', #55640, #93534 ) ;
#19120 = VERTEX_POINT ( 'NONE', #233124 ) ;
#19121 = DIRECTION ( 'NONE',  ( 0.000000000000000000, 0.000000000000000000, -1.000000000000000000 ) ) ;
#19122 = B_SPLINE_CURVE_WITH_KNOTS ( 'NONE', 3,
 ( #57406, #59969, #1284, #136956, #159123, #37887, #61279, #202079 ),
 .UNSPECIFIED., .F., .F.,
 ( 4, 2, 2, 4 ),
 ( 0.000000000000000000, 0.0001094981963948526792, 0.0002189963927897053584, 0.0004379927855794107168 ),
 .UNSPECIFIED. ) ;
#19123 = EDGE_LOOP ( 'NONE', ( #56240, #244718, #204206, #231578, #231698 ) ) ;
#19124 = AXIS2_PLACEMENT_3D ( 'NONE', #28832, #181452, #82300 ) ;
#19125 = DIRECTION ( 'NONE',  ( 1.000000000000000000, 0.000000000000000000, -0.000000000000000000 ) ) ;
#19126 = AXIS2_PLACEMENT_3D ( 'NONE', #87735, #150313, #27818 ) ;
#19127 = ORIENTED_EDGE ( 'NONE', *, *, #235833, .F. ) ;
#19128 = EDGE_CURVE ( 'NONE', #57537, #250431, #107804, .T. ) ;
#19129 = ORIENTED_EDGE ( 'NONE', *, *, #7509, .T. ) ;
#19130 = ADVANCED_FACE ( 'NONE', ( #54450 ), #120493, .T. ) ;
#19131 = ORIENTED_EDGE ( 'NONE', *, *, #5630, .F. ) ;
#19132 = DIRECTION ( 'NONE',  ( 0.000000000000000000, -7.056502275159890043E-15, 1.000000000000000000 ) ) ;
#19133 = CARTESIAN_POINT ( 'NONE',  ( 22.49066049874202022, 75.94365674848053516, -215.1731197220414913 ) ) ;
#19134 = AXIS2_PLACEMENT_3D ( 'NONE', #86575, #145278, #187016 ) ;
#19135 = CARTESIAN_POINT ( 'NONE',  ( 22.19999999999999929, -11.75000000000000000, -15.00000000000000000 ) ) ;
#19136 = FACE_OUTER_BOUND ( 'NONE', #83859, .T. ) ;
#19137 = CARTESIAN_POINT ( 'NONE',  ( 18.59999999999999787, 77.83534155023700407, -191.9679561919613491 ) ) ;
#19139 = CARTESIAN_POINT ( 'NONE',  ( 20.94999999999999929, 70.60134440767089359, -223.4290147181903023 ) ) ;
#19138 = CARTESIAN_POINT ( 'NONE',  ( 15.48841904831874849, 67.43841904833107037, -157.3731074845244393 ) ) ;
#19140 = DIRECTION ( 'NONE',  ( 0.000000000000000000, 0.2617529984165152257, 0.9651348961777124202 ) ) ;
#19142 = ORIENTED_EDGE ( 'NONE', *, *, #47631, .T. ) ;
#19141 = CARTESIAN_POINT ( 'NONE',  ( -20.94999999999999929, 1.261786168576181755, -75.08649896354552311 ) ) ;
#19143 = FACE_OUTER_BOUND ( 'NONE', #189079, .T. ) ;
#19144 = ORIENTED_EDGE ( 'NONE', *, *, #36135, .T. ) ;
#19145 = CARTESIAN_POINT ( 'NONE',  ( -18.45037301276647312, -9.490200447530892092, -141.0126741364146312 ) ) ;
#19146 = ORIENTED_EDGE ( 'NONE', *, *, #152458, .T. ) ;
#19147 = EDGE_LOOP ( 'NONE', ( #211263, #129109, #247784, #165265, #221423 ) ) ;
#19148 = CYLINDRICAL_SURFACE ( 'NONE', #189509, 0.09999999999998898659 ) ;
#19149 = DIRECTION ( 'NONE',  ( 0.000000000000000000, 0.000000000000000000, 1.000000000000000000 ) ) ;
#19150 = VERTEX_POINT ( 'NONE', #136540 ) ;
#19151 = EDGE_CURVE ( 'NONE', #206067, #239754, #128669, .T. ) ;
#19152 = EDGE_CURVE ( 'NONE', #203324, #167384, #28761, .T. ) ;
#19153 = CIRCLE ( 'NONE', #152461, 0.2000000000000118627 ) ;
#19154 = DIRECTION ( 'NONE',  ( 1.000000000000000000, 0.000000000000000000, 0.000000000000000000 ) ) ;
#19155 = VERTEX_POINT ( 'NONE', #196525 ) ;
#19156 = ORIENTED_EDGE ( 'NONE', *, *, #82656, .F. ) ;
#19157 = DIRECTION ( 'NONE',  ( 3.469446951953635015E-14, 6.982962677686266711E-15, -1.000000000000000000 ) ) ;
#19158 = VERTEX_POINT ( 'NONE', #55694 ) ;
#19159 = DIRECTION ( 'NONE',  ( 1.000000000000000000, 0.000000000000000000, 0.000000000000000000 ) ) ;
#19160 = DIRECTION ( 'NONE',  ( 0.000000000000000000, 0.000000000000000000, 1.000000000000000000 ) ) ;
#19161 = ORIENTED_EDGE ( 'NONE', *, *, #215541, .T. ) ;
#19162 = DIRECTION ( 'NONE',  ( 0.000000000000000000, 1.000000000000000000, 0.000000000000000000 ) ) ;
#19163 = DIRECTION ( 'NONE',  ( 0.7071359030027593029, 0.7070776581709197206, 0.000000000000000000 ) ) ;
#19165 = EDGE_CURVE ( 'NONE', #133, #86132, #144775, .T. ) ;
#19164 = CARTESIAN_POINT ( 'NONE',  ( 22.49544290803751423, 11.74987023786900942, -133.9346880407421452 ) ) ;
#19166 = VERTEX_POINT ( 'NONE', #191438 ) ;
#19167 = B_SPLINE_CURVE_WITH_KNOTS ( 'NONE', 3,
 ( #30738, #90667, #33316, #52821, #206781, #148094, #171536, #168982, #129803, #151967, #209336, #227614, #188495, #153259 ),
 .UNSPECIFIED., .F., .F.,
 ( 4, 2, 2, 2, 2, 2, 4 ),
 ( 0.000000000000000000, 2.389617747645413252E-05, 4.779235495290826504E-05, 9.558470990574708694E-05, 0.0001911694198114958273, 0.0003823388396229836857, 0.0007646776792460279783 ),
 .UNSPECIFIED. ) ;
#19168 = EDGE_CURVE ( 'NONE', #38969, #80372, #53171, .T. ) ;
#19169 = DIRECTION ( 'NONE',  ( 0.000000000000000000, 0.9126074666063769270, 0.4088369013363280513 ) ) ;
#19170 = CARTESIAN_POINT ( 'NONE',  ( -18.50000000000000000, 11.65000000001115232, -141.0148057706540214 ) ) ;
#19171 = B_SPLINE_CURVE_WITH_KNOTS ( 'NONE', 3,
 ( #257435, #158431, #93938, #226038, #244342, #86532, #65715, #246912 ),
 .UNSPECIFIED., .F., .F.,
 ( 4, 2, 2, 4 ),
 ( 0.000000000000000000, 0.0001094981963948357250, 0.0002189963927896714500, 0.0004379927855794142947 ),
 .UNSPECIFIED. ) ;
#19172 = AXIS2_PLACEMENT_3D ( 'NONE', #11703, #108223, #91233 ) ;
#19173 = EDGE_CURVE ( 'NONE', #164389, #79953, #95346, .T. ) ;
#19174 = DIRECTION ( 'NONE',  ( 0.000000000000000000, 0.9126074666063769270, 0.4088369013363280513 ) ) ;
#19175 = VECTOR ( 'NONE', #150497, 1000.000000000000000 ) ;
#19176 = AXIS2_PLACEMENT_3D ( 'NONE', #28538, #244959, #188841 ) ;
#19177 = VECTOR ( 'NONE', #170491, 1000.000000000000000 ) ;
#19178 = ORIENTED_EDGE ( 'NONE', *, *, #184566, .F. ) ;
#19180 = ORIENTED_EDGE ( 'NONE', *, *, #137926, .T. ) ;
#19179 = DIRECTION ( 'NONE',  ( 1.000000000000000000, 0.000000000000000000, 0.000000000000000000 ) ) ;
#19181 = ORIENTED_EDGE ( 'NONE', *, *, #198190, .F. ) ;
#19182 = DIRECTION ( 'NONE',  ( 0.000000000000000000, -0.9394191166662618775, -0.3427706569150580362 ) ) ;
#19183 = ADVANCED_FACE ( 'NONE', ( #119584 ), #16254, .T. ) ;
#19184 = CARTESIAN_POINT ( 'NONE',  ( -22.48660254037843487, 12.58580559757028183, -223.4396719342083770 ) ) ;
#19185 = CARTESIAN_POINT ( 'NONE',  ( 20.94999999999999929, 67.22371710471909978, -57.37310748452438247 ) ) ;
#19186 = CARTESIAN_POINT ( 'NONE',  ( -23.25000000000000000, 5.354661166737471056, -213.3684367965233832 ) ) ;
#19187 = PLANE ( 'NONE',  #675 ) ;
#19188 = CARTESIAN_POINT ( 'NONE',  ( 20.85000000000000142, 76.30149234032609229, -203.6488173052385946 ) ) ;
#19189 = ORIENTED_EDGE ( 'NONE', *, *, #108037, .F. ) ;
#19190 = DIRECTION ( 'NONE',  ( -1.000000000000000000, 0.000000000000000000, 0.000000000000000000 ) ) ;
#19191 = EDGE_CURVE ( 'NONE', #138432, #231688, #212060, .T. ) ;
#19192 = CARTESIAN_POINT ( 'NONE',  ( -16.80438519320023616, 9.949779096479501206, -146.6507382809213027 ) ) ;
#19193 = CARTESIAN_POINT ( 'NONE',  ( -18.39999999999999858, 77.26488334054519669, -241.9697969554615611 ) ) ;
#19194 = CARTESIAN_POINT ( 'NONE',  ( 21.97500000000000497, 9.750000000011153745, -179.7499999999999716 ) ) ;
#19195 = VECTOR ( 'NONE', #168858, 999.9999999999998863 ) ;
#19196 = DIRECTION ( 'NONE',  ( -0.000000000000000000, 6.982962677686266711E-15, -1.000000000000000000 ) ) ;
#19197 = TOROIDAL_SURFACE ( 'NONE', #227467, 0.4000000000000012990, 0.1000000000000000056 ) ;
#19198 = ORIENTED_EDGE ( 'NONE', *, *, #104441, .F. ) ;
#19199 = ORIENTED_EDGE ( 'NONE', *, *, #74493, .T. ) ;
#19200 = CARTESIAN_POINT ( 'NONE',  ( -20.85000000000000142, 64.25000000001196554, -109.8069731475024895 ) ) ;
#19201 = LINE ( 'NONE', #158743, #209340 ) ;
#19202 = CARTESIAN_POINT ( 'NONE',  ( -17.01473183483381391, 66.05000000001261640, -190.7731074845244166 ) ) ;
#19203 = CARTESIAN_POINT ( 'NONE',  ( -21.05000000000000071, 69.45934304831143891, -203.4231074845244223 ) ) ;
#19204 = DIRECTION ( 'NONE',  ( -0.000000000000000000, -0.000000000000000000, -1.000000000000000000 ) ) ;
#19205 = AXIS2_PLACEMENT_3D ( 'NONE', #237356, #216498, #139520 ) ;
#19206 = ORIENTED_EDGE ( 'NONE', *, *, #166921, .T. ) ;
#19207 = CARTESIAN_POINT ( 'NONE',  ( -20.64999999999999858, -8.730841121484171907, -43.09807471898432851 ) ) ;
#19208 = CIRCLE ( 'NONE', #10841, 0.09999999999998898659 ) ;
#19209 = AXIS2_PLACEMENT_3D ( 'NONE', #41240, #761, #182010 ) ;
#19210 = FACE_OUTER_BOUND ( 'NONE', #31289, .T. ) ;
#19211 = EDGE_LOOP ( 'NONE', ( #96614, #53670, #254626, #165549 ) ) ;
#19212 = DIRECTION ( 'NONE',  ( -1.000000000000000000, 0.000000000000000000, 0.000000000000000000 ) ) ;
#19213 = SPHERICAL_SURFACE ( 'NONE', #199670, 0.1000000000000000056 ) ;
#19214 = VECTOR ( 'NONE', #181993, 1000.000000000000114 ) ;
#19215 = AXIS2_PLACEMENT_3D ( 'NONE', #2108, #81625, #118227 ) ;
#19216 = ORIENTED_EDGE ( 'NONE', *, *, #49673, .T. ) ;
#19218 = DIRECTION ( 'NONE',  ( 0.000000000000000000, -0.4088369013362687654, 0.9126074666064034613 ) ) ;
#19217 = VECTOR ( 'NONE', #69922, 1000.000000000000114 ) ;
#19219 = VERTEX_POINT ( 'NONE', #102526 ) ;
#19220 = CARTESIAN_POINT ( 'NONE',  ( -21.05000000000000071, 75.94867256767035713, -75.82329082079064619 ) ) ;
#19221 = DIRECTION ( 'NONE',  ( -0.000000000000000000, -1.000000000000000000, -6.982962677686266711E-15 ) ) ;
#19222 = LINE ( 'NONE', #195322, #253293 ) ;
#19223 = AXIS2_PLACEMENT_3D ( 'NONE', #180690, #99822, #176851 ) ;
#19224 = CARTESIAN_POINT ( 'NONE',  ( 21.05000000000000071, 70.50000000001180922, -81.92837350343744163 ) ) ;
#19225 = DIRECTION ( 'NONE',  ( 0.000000000000000000, 0.2128009952263603677, -0.9770955615653313941 ) ) ;
#19226 = DIRECTION ( 'NONE',  ( 1.000000000000000000, 1.186688945009010077E-16, 0.000000000000000000 ) ) ;
#19227 = FACE_OUTER_BOUND ( 'NONE', #101525, .T. ) ;
#19228 = DIRECTION ( 'NONE',  ( 1.000000000000000000, 0.000000000000000000, 0.000000000000000000 ) ) ;
#19229 = DIRECTION ( 'NONE',  ( -0.000000000000000000, -0.2128009952263603677, 0.9770955615653313941 ) ) ;
#19230 = EDGE_CURVE ( 'NONE', #202644, #217587, #116214, .T. ) ;
#19231 = CARTESIAN_POINT ( 'NONE',  ( -20.94999999999999929, 87.41227409416161720, -100.0231074845242318 ) ) ;
#19232 = TOROIDAL_SURFACE ( 'NONE', #86398, 12.97499999999999609, 0.1000000000000000056 ) ;
#19233 = DIRECTION ( 'NONE',  ( -0.000000000000000000, 0.000000000000000000, 1.000000000000000000 ) ) ;
#19234 = CARTESIAN_POINT ( 'NONE',  ( -14.00000000000000178, 9.850000000011133849, -117.2500000000000284 ) ) ;
#19235 = DIRECTION ( 'NONE',  ( -1.000000000000000000, 0.000000000000000000, 0.000000000000000000 ) ) ;
#19236 = ORIENTED_EDGE ( 'NONE', *, *, #150576, .T. ) ;
#19237 = LINE ( 'NONE', #180889, #148011 ) ;
#19238 = DIRECTION ( 'NONE',  ( 0.000000000000000000, 1.000000000000000000, 0.000000000000000000 ) ) ;
#19240 = EDGE_CURVE ( 'NONE', #91227, #125758, #83487, .T. ) ;
#19239 = CARTESIAN_POINT ( 'NONE',  ( 20.51284917709620359, 10.31088662285602275, -41.17247318559201830 ) ) ;
#19241 =( REPRESENTATION_RELATIONSHIP ('NONE','NONE', #36900, #61981 ) REPRESENTATION_RELATIONSHIP_WITH_TRANSFORMATION ( #214834 )SHAPE_REPRESENTATION_RELATIONSHIP( ) );
#19242 = VERTEX_POINT ( 'NONE', #60862 ) ;
#19243 = DIRECTION ( 'NONE',  ( 0.000000000000000000, 0.8660254037844378194, 0.5000000000000016653 ) ) ;
#19244 = EDGE_CURVE ( 'NONE', #39283, #104351, #242066, .T. ) ;
#19245 = EDGE_CURVE ( 'NONE', #62135, #138031, #63428, .T. ) ;
#19246 = VECTOR ( 'NONE', #30920, 1000.000000000000000 ) ;
#19247 = DIRECTION ( 'NONE',  ( 0.000000000000000000, -0.2044060691543873876, 0.9788861828082220384 ) ) ;
#19248 = ORIENTED_EDGE ( 'NONE', *, *, #3112, .F. ) ;
#19250 = AXIS2_PLACEMENT_3D ( 'NONE', #154810, #212204, #210902 ) ;
#19249 = CARTESIAN_POINT ( 'NONE',  ( 20.94999999999999929, 46.32970330538243786, -243.0551226933711746 ) ) ;
#19251 = CARTESIAN_POINT ( 'NONE',  ( 22.49999999999999645, 31.76322370622490965, -238.8696546380523955 ) ) ;
#19252 = VECTOR ( 'NONE', #53962, 1000.000000000000000 ) ;
#19253 = ORIENTED_EDGE ( 'NONE', *, *, #183217, .T. ) ;
#19254 = VECTOR ( 'NONE', #106567, 1000.000000000000000 ) ;
#19255 = ORIENTED_EDGE ( 'NONE', *, *, #134150, .T. ) ;
#19256 = EDGE_CURVE ( 'NONE', #210177, #144164, #42592, .T. ) ;
#19257 = ORIENTED_EDGE ( 'NONE', *, *, #61404, .F. ) ;
#19259 = CIRCLE ( 'NONE', #40140, 11.69999999999998863 ) ;
#19258 = CARTESIAN_POINT ( 'NONE',  ( 18.49999999999999645, 5.950000000011100632, -110.8057023050348988 ) ) ;
#19260 = CYLINDRICAL_SURFACE ( 'NONE', #91214, 7.900000000000003908 ) ;
#19262 = DIRECTION ( 'NONE',  ( 0.000000000000000000, -7.086529944415894657E-15, 1.000000000000000000 ) ) ;
#19261 = UNCERTAINTY_MEASURE_WITH_UNIT (LENGTH_MEASURE( 1.000000000000000082E-05 ), #43242, 'distance_accuracy_value', 'NONE');
#19263 = CARTESIAN_POINT ( 'NONE',  ( 18.39999999999998082, 64.52683809664961245, -127.2731074845243882 ) ) ;
#19264 = CIRCLE ( 'NONE', #115136, 0.09999999999999971412 ) ;
#19265 = DIRECTION ( 'NONE',  ( 0.000000000000000000, -1.000000000000000000, 0.000000000000000000 ) ) ;
#19266 = DIRECTION ( 'NONE',  ( 0.000000000000000000, -6.982962677686266711E-15, 1.000000000000000000 ) ) ;
#19267 = AXIS2_PLACEMENT_3D ( 'NONE', #237610, #202324, #121541 ) ;
#19268 = CARTESIAN_POINT ( 'NONE',  ( -18.50000000000000000, 77.16270174995034381, -161.9231074845243370 ) ) ;
#19269 = CARTESIAN_POINT ( 'NONE',  ( 22.00356870068858228, 0.7342531111018623102, -230.3072997391775800 ) ) ;
#19271 = ORIENTED_EDGE ( 'NONE', *, *, #11962, .T. ) ;
#19270 = CARTESIAN_POINT ( 'NONE',  ( 18.31325810956447953, 87.00173612015743174, -199.3903144367706943 ) ) ;
#19272 = ORIENTED_EDGE ( 'NONE', *, *, #12914, .F. ) ;
#19274 = CARTESIAN_POINT ( 'NONE',  ( -20.94999999999999929, 64.25000000001161027, -62.68150679462727481 ) ) ;
#19273 = CARTESIAN_POINT ( 'NONE',  ( 22.50000000000000000, 0.1008583690987118059, 11.74956712348939369 ) ) ;
#19277 = ORIENTED_EDGE ( 'NONE', *, *, #208760, .T. ) ;
#19276 = CARTESIAN_POINT ( 'NONE',  ( -16.93710578446436443, 61.00971801480476842, -220.7822956305894877 ) ) ;
#19275 = CARTESIAN_POINT ( 'NONE',  ( -20.94999999999999929, -11.64999999998884483, -36.50000000000000711 ) ) ;
#19278 = ORIENTED_EDGE ( 'NONE', *, *, #101176, .T. ) ;
#19279 = CARTESIAN_POINT ( 'NONE',  ( -21.05000000000000071, 18.92285928089247804, -233.3572654221044900 ) ) ;
#19280 = CARTESIAN_POINT ( 'NONE',  ( -21.05000000000000071, 87.39257802171731271, -66.44915790469229933 ) ) ;
#19281 = EDGE_CURVE ( 'NONE', #22150, #111790, #77854, .T. ) ;
#19282 = CARTESIAN_POINT ( 'NONE',  ( -18.59999999999999787, 9.350000000000001421, -21.15000000000000213 ) ) ;
#19283 = CARTESIAN_POINT ( 'NONE',  ( 23.14999999999999503, 62.92003201576280702, -207.2439188921395612 ) ) ;
#19285 = DIRECTION ( 'NONE',  ( -1.000000000000000000, 0.000000000000000000, 0.000000000000000000 ) ) ;
#19284 = CIRCLE ( 'NONE', #131897, 0.09999999999998898659 ) ;
#19286 = DIRECTION ( 'NONE',  ( -0.000000000000000000, 0.000000000000000000, 1.000000000000000000 ) ) ;
#19287 = DIRECTION ( 'NONE',  ( 0.000000000000000000, -7.026728003956683390E-15, 1.000000000000000000 ) ) ;
#19288 = ADVANCED_FACE ( 'NONE', ( #200387 ), #241906, .F. ) ;
#19289 = CARTESIAN_POINT ( 'NONE',  ( 18.59999999999999432, 70.47363787294415260, -228.3418745167492432 ) ) ;
#19290 = EDGE_LOOP ( 'NONE', ( #156411, #38523, #109732, #129186 ) ) ;
#19291 = ORIENTED_EDGE ( 'NONE', *, *, #169031, .F. ) ;
#19292 = CARTESIAN_POINT ( 'NONE',  ( -20.94999999999999929, -11.64999999998884306, -137.1000000000000227 ) ) ;
#19293 = CIRCLE ( 'NONE', #6819, 0.09999999999999939493 ) ;
#19294 = AXIS2_PLACEMENT_3D ( 'NONE', #94801, #239461, #99908 ) ;
#19295 = VERTEX_POINT ( 'NONE', #157445 ) ;
#19296 = AXIS2_PLACEMENT_3D ( 'NONE', #152728, #75735, #117421 ) ;
#19298 = DIRECTION ( 'NONE',  ( 2.879366945564059217E-14, 0.9875055080513762684, -0.1575844902526679081 ) ) ;
#19297 = AXIS2_PLACEMENT_3D ( 'NONE', #93526, #33610, #251309 ) ;
#19299 = ORIENTED_EDGE ( 'NONE', *, *, #227965, .T. ) ;
#19300 = DIRECTION ( 'NONE',  ( -1.000000000000000000, 1.836970198721029934E-16, 1.282749433769087757E-30 ) ) ;
#19301 = CARTESIAN_POINT ( 'NONE',  ( 23.14999999999998437, 87.75000000001267608, -203.5231074845243029 ) ) ;
#19302 = CYLINDRICAL_SURFACE ( 'NONE', #222617, 0.1000000000000013933 ) ;
#19303 = DIRECTION ( 'NONE',  ( 1.000000000000000000, 0.000000000000000000, 0.000000000000000000 ) ) ;
#19304 = CARTESIAN_POINT ( 'NONE',  ( -11.60000000000000320, -11.65000000000000036, 17.60000000000000497 ) ) ;
#19305 = ORIENTED_EDGE ( 'NONE', *, *, #835, .T. ) ;
#19306 = CARTESIAN_POINT ( 'NONE',  ( -21.05000000000000071, 11.64999999999999680, -6.783865662978152855 ) ) ;
#19307 = ADVANCED_FACE ( 'NONE', ( #236943 ), #58284, .T. ) ;
#19308 = CARTESIAN_POINT ( 'NONE',  ( 20.94999999999999574, 1.162701749949165642, -142.0000000000000284 ) ) ;
#19309 = CARTESIAN_POINT ( 'NONE',  ( -21.05000000000000071, 72.05339752741123505, -225.0867394276846483 ) ) ;
#19310 = CARTESIAN_POINT ( 'NONE',  ( -22.57320508075687115, 11.48087284840413425, -198.4995883060917663 ) ) ;
#19311 = CIRCLE ( 'NONE', #239905, 0.6000000000000064171 ) ;
#19312 = CARTESIAN_POINT ( 'NONE',  ( -21.05000000000000071, 11.64999999999999680, -6.783865662978151967 ) ) ;
#19313 = EDGE_LOOP ( 'NONE', ( #129385, #25235, #108090, #237630 ) ) ;
#19314 = VECTOR ( 'NONE', #211259, 1000.000000000000000 ) ;
#19315 = CARTESIAN_POINT ( 'NONE',  ( -18.41809261886929860, 85.68240331476805238, -29.36626393443318861 ) ) ;
#19316 = EDGE_LOOP ( 'NONE', ( #51722, #39906, #82491, #87754, #243208 ) ) ;
#19319 = VERTEX_POINT ( 'NONE', #867 ) ;
#19318 = DIRECTION ( 'NONE',  ( 0.000000000000000000, 0.000000000000000000, 1.000000000000000000 ) ) ;
#19317 = LINE ( 'NONE', #257874, #94928 ) ;
#19320 = DIRECTION ( 'NONE',  ( 1.000000000000000000, -0.000000000000000000, 0.000000000000000000 ) ) ;
#19321 = ADVANCED_FACE ( 'NONE', ( #159999 ), #75364, .T. ) ;
#19322 = DIRECTION ( 'NONE',  ( -1.000000000000000000, 0.000000000000000000, 0.000000000000000000 ) ) ;
#19323 = AXIS2_PLACEMENT_3D ( 'NONE', #231277, #51300, #72198 ) ;
#19324 = ORIENTED_EDGE ( 'NONE', *, *, #132832, .T. ) ;
#19326 = ADVANCED_FACE ( 'NONE', ( #137824 ), #191895, .F. ) ;
#19325 = DIRECTION ( 'NONE',  ( 0.000000000000000000, 0.000000000000000000, -1.000000000000000000 ) ) ;
#19327 = DIRECTION ( 'NONE',  ( -1.000000000000000000, 0.000000000000000000, 0.000000000000000000 ) ) ;
#19328 = EDGE_CURVE ( 'NONE', #63115, #100189, #62164, .T. ) ;
#19329 = CARTESIAN_POINT ( 'NONE',  ( -23.25000000000000000, -9.000000000000001776, -23.60603087734756045 ) ) ;
#19330 = EDGE_CURVE ( 'NONE', #185124, #61748, #178283, .T. ) ;
#19332 = ORIENTED_EDGE ( 'NONE', *, *, #139135, .T. ) ;
#19331 = LINE ( 'NONE', #20632, #193475 ) ;
#19333 = CARTESIAN_POINT ( 'NONE',  ( 20.94999999999999574, 77.34908441863964867, -195.5366085209788594 ) ) ;
#19335 = ORIENTED_EDGE ( 'NONE', *, *, #70913, .F. ) ;
#19334 = EDGE_CURVE ( 'NONE', #235551, #156427, #196133, .T. ) ;
#19336 = CYLINDRICAL_SURFACE ( 'NONE', #103511, 0.09999999999999939493 ) ;
#19337 = CARTESIAN_POINT ( 'NONE',  ( -16.94445028196807002, 9.992063609708893068, -188.3926698215815350 ) ) ;
#19338 = DIRECTION ( 'NONE',  ( 0.000000000000000000, 0.000000000000000000, -1.000000000000000000 ) ) ;
#19339 = EDGE_CURVE ( 'NONE', #74995, #226175, #150184, .T. ) ;
#19340 = CIRCLE ( 'NONE', #115017, 0.09999999999998898659 ) ;
#19341 = EDGE_LOOP ( 'NONE', ( #142626, #43780, #208666, #82593 ) ) ;
#19342 = CARTESIAN_POINT ( 'NONE',  ( -23.15000000000000213, 74.00000000001151079, -49.24772940728643533 ) ) ;
#19345 = ADVANCED_FACE ( 'NONE', ( #49006 ), #89410, .T. ) ;
#19344 = EDGE_CURVE ( 'NONE', #157687, #215487, #133582, .T. ) ;
#19343 = ORIENTED_EDGE ( 'NONE', *, *, #168005, .T. ) ;
#19346 = DIRECTION ( 'NONE',  ( 0.000000000000000000, 1.000000000000000000, -6.938893903907240999E-14 ) ) ;
#19347 = DIRECTION ( 'NONE',  ( 1.000000000000000000, 0.000000000000000000, 0.000000000000000000 ) ) ;
#19348 = CARTESIAN_POINT ( 'NONE',  ( -21.65000000000000213, 44.13548170601895038, -235.2989316066074821 ) ) ;
#19349 = EDGE_LOOP ( 'NONE', ( #121429, #178057, #1138, #127045, #137642, #198313, #69430, #29722, #257127, #164834, #1088, #122217, #57490, #131488, #73272, #201159 ) ) ;
#19350 = DIRECTION ( 'NONE',  ( 0.000000000000000000, -0.9126074666063660468, -0.4088369013363524762 ) ) ;
#19351 = AXIS2_PLACEMENT_3D ( 'NONE', #256096, #77497, #120536 ) ;
#19352 = FACE_OUTER_BOUND ( 'NONE', #118220, .T. ) ;
#19353 = EDGE_CURVE ( 'NONE', #161516, #233936, #107695, .T. ) ;
#19354 = CARTESIAN_POINT ( 'NONE',  ( -20.94999999999999929, 64.36312671090843196, -176.8448666978491701 ) ) ;
#19355 = ORIENTED_EDGE ( 'NONE', *, *, #236335, .F. ) ;
#19356 = CIRCLE ( 'NONE', #252379, 12.87500000000000000 ) ;
#19357 = CARTESIAN_POINT ( 'NONE',  ( 22.39999999999999503, -0.09999999998884338825, -122.3504291924552234 ) ) ;
#19358 = CARTESIAN_POINT ( 'NONE',  ( 20.94999999999999929, 86.45856254523212669, -209.4679346046102921 ) ) ;
#19359 = EDGE_CURVE ( 'NONE', #178493, #101170, #175316, .T. ) ;
#19361 = EDGE_CURVE ( 'NONE', #243903, #241027, #9879, .T. ) ;
#19360 = FACE_OUTER_BOUND ( 'NONE', #32273, .T. ) ;
#19362 = VECTOR ( 'NONE', #78832, 1000.000000000000000 ) ;
#19363 = AXIS2_PLACEMENT_3D ( 'NONE', #11055, #47594, #48890 ) ;
#19364 = ORIENTED_EDGE ( 'NONE', *, *, #223145, .T. ) ;
#19365 = COLOUR_RGB ( '', 0.72549020, 0.75294118, 0.79215686) ;
#19366 = EDGE_CURVE ( 'NONE', #41279, #91128, #69881, .T. ) ;
#19367 = CARTESIAN_POINT ( 'NONE',  ( -5.999999999999938716, 64.65000000001120384, -26.02310748452479316 ) ) ;
#19368 = ORIENTED_EDGE ( 'NONE', *, *, #256839, .F. ) ;
#19370 = EDGE_LOOP ( 'NONE', ( #60146, #118366, #121942, #85736 ) ) ;
#19369 = FACE_OUTER_BOUND ( 'NONE', #30442, .T. ) ;
#19371 = ADVANCED_FACE ( 'NONE', ( #24336, #245938, #88102 ), #183397, .F. ) ;
#19374 = VERTEX_POINT ( 'NONE', #205506 ) ;
#19373 = ORIENTED_EDGE ( 'NONE', *, *, #152507, .T. ) ;
#19372 = CARTESIAN_POINT ( 'NONE',  ( -21.08198257630413508, 0.07264332378459012474, 6.336596734015067511 ) ) ;
#19375 = DIRECTION ( 'NONE',  ( 1.000000000000000000, -0.000000000000000000, -0.000000000000000000 ) ) ;
#19376 = LINE ( 'NONE', #21948, #56587 ) ;
#19377 = FACE_OUTER_BOUND ( 'NONE', #52825, .T. ) ;
#19378 = DIRECTION ( 'NONE',  ( 0.000000000000000000, -6.853228547068871147E-15, 1.000000000000000000 ) ) ;
#19379 = FACE_BOUND ( 'NONE', #196060, .T. ) ;
#19380 = VECTOR ( 'NONE', #184041, 1000.000000000000000 ) ;
#19381 = DIRECTION ( 'NONE',  ( -1.000000000000000000, 0.000000000000000000, 0.000000000000000000 ) ) ;
#19382 = CARTESIAN_POINT ( 'NONE',  ( -21.05000000000000071, 76.00000000001142553, -36.02310748452432421 ) ) ;
#19384 = LINE ( 'NONE', #200580, #168188 ) ;
#19383 = CARTESIAN_POINT ( 'NONE',  ( -20.00857864376270001, 9.350000000011156942, -54.65000000000000568 ) ) ;
#19385 = AXIS2_PLACEMENT_3D ( 'NONE', #133499, #155665, #77359 ) ;
#19386 = EDGE_LOOP ( 'NONE', ( #42840, #176497, #154445, #23566 ) ) ;
#19387 = ORIENTED_EDGE ( 'NONE', *, *, #237473, .T. ) ;
#19389 = LINE ( 'NONE', #98883, #199814 ) ;
#19388 = AXIS2_PLACEMENT_3D ( 'NONE', #71087, #129755, #29413 ) ;
#19391 = ORIENTED_EDGE ( 'NONE', *, *, #78794, .T. ) ;
#19390 = DIRECTION ( 'NONE',  ( 0.000000000000000000, 1.000000000000000000, 0.000000000000000000 ) ) ;
#19393 = CARTESIAN_POINT ( 'NONE',  ( -21.44999999999999929, 68.75000000001185185, -90.67310748452436542 ) ) ;
#19392 = VECTOR ( 'NONE', #46830, 1000.000000000000000 ) ;
#19394 = ORIENTED_EDGE ( 'NONE', *, *, #185638, .T. ) ;
#19395 = DIRECTION ( 'NONE',  ( 1.000000000000000000, 0.000000000000000000, 0.000000000000000000 ) ) ;
#19396 = ORIENTED_EDGE ( 'NONE', *, *, #223282, .F. ) ;
#19397 = DIRECTION ( 'NONE',  ( 1.000000000000000000, 0.000000000000000000, 0.000000000000000000 ) ) ;
#19398 = TOROIDAL_SURFACE ( 'NONE', #227666, 0.2000000000000000111, 0.1000000000000000056 ) ;
#19399 = CIRCLE ( 'NONE', #185982, 0.1000000000000013933 ) ;
#19400 = EDGE_LOOP ( 'NONE', ( #143498, #183961, #162501, #61480 ) ) ;
#19401 = CARTESIAN_POINT ( 'NONE',  ( -23.15000000000000213, -11.64999999998884483, -197.8999999999999773 ) ) ;
#19402 = CARTESIAN_POINT ( 'NONE',  ( -16.94107738177414291, 30.32481141862675145, -234.7976376674202186 ) ) ;
#19405 = ORIENTED_EDGE ( 'NONE', *, *, #195711, .T. ) ;
#19404 = VERTEX_POINT ( 'NONE', #124705 ) ;
#19403 = VECTOR ( 'NONE', #112434, 1000.000000000000000 ) ;
#19406 = ORIENTED_EDGE ( 'NONE', *, *, #137839, .T. ) ;
#19407 = LINE ( 'NONE', #181060, #236200 ) ;
#19408 = VECTOR ( 'NONE', #223418, 1000.000000000000000 ) ;
#19409 = ORIENTED_EDGE ( 'NONE', *, *, #229048, .F. ) ;
#19410 = VECTOR ( 'NONE', #20522, 1000.000000000000000 ) ;
#19411 = ORIENTED_EDGE ( 'NONE', *, *, #161900, .T. ) ;
#19412 = DIRECTION ( 'NONE',  ( 1.000000000000000000, -0.000000000000000000, -0.000000000000000000 ) ) ;
#19414 = ORIENTED_EDGE ( 'NONE', *, *, #146782, .F. ) ;
#19413 = DIRECTION ( 'NONE',  ( 0.000000000000000000, -0.000000000000000000, 1.000000000000000000 ) ) ;
#19416 = DIRECTION ( 'NONE',  ( 0.000000000000000000, 0.8814952561688437216, -0.4721928772777334582 ) ) ;
#19415 = PLANE ( 'NONE',  #207393 ) ;
#19417 = CARTESIAN_POINT ( 'NONE',  ( 23.15000000000000213, 84.66355140188063899, -45.54720860259157433 ) ) ;
#19418 = FACE_OUTER_BOUND ( 'NONE', #48718, .T. ) ;
#19419 = DIRECTION ( 'NONE',  ( 0.000000000000000000, -0.01562499999996343723, -0.9998779222360104635 ) ) ;
#19420 = ORIENTED_EDGE ( 'NONE', *, *, #45505, .T. ) ;
#19421 = ORIENTED_EDGE ( 'NONE', *, *, #22886, .T. ) ;
#19422 = FACE_OUTER_BOUND ( 'NONE', #101648, .T. ) ;
#19423 = DIRECTION ( 'NONE',  ( -1.000000000000000000, 0.000000000000000000, 0.000000000000000000 ) ) ;
#19425 = EDGE_CURVE ( 'NONE', #193155, #61614, #29570, .T. ) ;
#19424 = CARTESIAN_POINT ( 'NONE',  ( 21.05000000000005400, 67.75000000001118394, -51.02310748452479316 ) ) ;
#19426 = CIRCLE ( 'NONE', #140190, 0.09999999999999907574 ) ;
#19427 = EDGE_LOOP ( 'NONE', ( #256072, #100960, #66818, #233692 ) ) ;
#19428 = FACE_OUTER_BOUND ( 'NONE', #229626, .T. ) ;
#19429 = EDGE_CURVE ( 'NONE', #195237, #234608, #71067, .T. ) ;
#19430 = DIRECTION ( 'NONE',  ( 0.000000000000000000, 0.8700118002898393765, -0.4930308989875104575 ) ) ;
#19431 = CARTESIAN_POINT ( 'NONE',  ( -15.39946565075090845, 12.51008756600233873, -214.3176843001242560 ) ) ;
#19432 = ORIENTED_EDGE ( 'NONE', *, *, #180719, .F. ) ;
#19433 = ORIENTED_EDGE ( 'NONE', *, *, #28620, .F. ) ;
#19434 = EDGE_CURVE ( 'NONE', #119565, #103333, #187776, .T. ) ;
#19435 = DIRECTION ( 'NONE',  ( 0.000000000000000000, -4.336808689942494997E-15, -1.000000000000000000 ) ) ;
#19436 = EDGE_CURVE ( 'NONE', #227579, #170828, #46100, .T. ) ;
#19437 = ORIENTED_EDGE ( 'NONE', *, *, #50449, .T. ) ;
#19438 = DIRECTION ( 'NONE',  ( 0.000000000000000000, -0.7071067811865479058, 0.7071067811865472397 ) ) ;
#19439 = EDGE_LOOP ( 'NONE', ( #156077, #253588, #94106, #203531, #6667, #245333, #98860, #16013, #17419, #153224, #61679, #76511, #30616, #114956 ) ) ;
#19440 = DIRECTION ( 'NONE',  ( 1.073024830501117528E-15, 0.8814952561688430555, -0.4721928772777346239 ) ) ;
#19441 = LINE ( 'NONE', #156416, #70676 ) ;
#19443 = CARTESIAN_POINT ( 'NONE',  ( -20.93975676684922504, 68.05374558910872906, -224.1882283518532120 ) ) ;
#19442 = LINE ( 'NONE', #2416, #7284 ) ;
#19444 = VECTOR ( 'NONE', #10018, 1000.000000000000000 ) ;
#19445 = DIRECTION ( 'NONE',  ( 1.000000000000000000, 3.265361837132813093E-16, -0.000000000000000000 ) ) ;
#19446 = CIRCLE ( 'NONE', #194428, 0.1000000000000033362 ) ;
#19447 = CARTESIAN_POINT ( 'NONE',  ( -20.64999999999999858, 68.75000000001185185, -90.67310748452436542 ) ) ;
#19448 = CIRCLE ( 'NONE', #56807, 0.5000000000000004441 ) ;
#19449 = CIRCLE ( 'NONE', #219344, 0.1999999999999987899 ) ;
#19450 = DIRECTION ( 'NONE',  ( 0.000000000000000000, 0.9126074666063132002, 0.4088369013364708815 ) ) ;
#19451 = EDGE_CURVE ( 'NONE', #97347, #184180, #208625, .T. ) ;
#19453 = VERTEX_POINT ( 'NONE', #146809 ) ;
#19452 = ORIENTED_EDGE ( 'NONE', *, *, #247386, .T. ) ;
#19454 = VERTEX_POINT ( 'NONE', #85529 ) ;
#19455 = EDGE_CURVE ( 'NONE', #133216, #134711, #54478, .T. ) ;
#19456 = LINE ( 'NONE', #22031, #213164 ) ;
#19457 = CARTESIAN_POINT ( 'NONE',  ( 18.59999999999999787, -1.835341550213255957, -45.05515129256298223 ) ) ;
#19458 = CARTESIAN_POINT ( 'NONE',  ( -21.05000000000000071, 87.48912529308769592, -66.62310748452424036 ) ) ;
#19459 = LINE ( 'NONE', #36477, #174404 ) ;
#19460 = AXIS2_PLACEMENT_3D ( 'NONE', #53771, #52466, #91615 ) ;
#19462 = CYLINDRICAL_SURFACE ( 'NONE', #148898, 0.1000000000000055844 ) ;
#19461 = FACE_OUTER_BOUND ( 'NONE', #45408, .T. ) ;
#19463 = ORIENTED_EDGE ( 'NONE', *, *, #67790, .F. ) ;
#19464 = CARTESIAN_POINT ( 'NONE',  ( -16.80100914604134843, 66.05685090590795028, -48.70606335723675073 ) ) ;
#19465 = ORIENTED_EDGE ( 'NONE', *, *, #153417, .F. ) ;
#19466 = CYLINDRICAL_SURFACE ( 'NONE', #121755, 0.5000000000000004441 ) ;
#19467 = CIRCLE ( 'NONE', #15378, 0.1000000000000028644 ) ;
#19468 = ORIENTED_EDGE ( 'NONE', *, *, #240402, .F. ) ;
#19469 = ORIENTED_EDGE ( 'NONE', *, *, #157483, .F. ) ;
#19470 = CARTESIAN_POINT ( 'NONE',  ( -21.14999999999994174, 64.25000000001119815, -30.12310748452479103 ) ) ;
#19471 = VECTOR ( 'NONE', #65075, 1000.000000000000000 ) ;
#19472 = LINE ( 'NONE', #141968, #64420 ) ;
#19473 = LINE ( 'NONE', #178569, #195847 ) ;
#19474 = EDGE_CURVE ( 'NONE', #202146, #107897, #87783, .T. ) ;
#19475 = CARTESIAN_POINT ( 'NONE',  ( 19.58285714285715073, 10.38499851036257837, -175.1296846673899097 ) ) ;
#19476 = B_SPLINE_CURVE_WITH_KNOTS ( 'NONE', 3,
 ( #197186, #53835, #133379, #113804, #193362, #142346, #81079, #180215 ),
 .UNSPECIFIED., .F., .F.,
 ( 4, 2, 2, 4 ),
 ( 0.000000000000000000, 0.0001049670497869906649, 0.0002099340995739813298, 0.0004198681991480182249 ),
 .UNSPECIFIED. ) ;
#19477 = EDGE_CURVE ( 'NONE', #28426, #129778, #112744, .T. ) ;
#19478 = DIRECTION ( 'NONE',  ( 0.000000000000000000, 0.000000000000000000, -1.000000000000000000 ) ) ;
#19479 = ORIENTED_EDGE ( 'NONE', *, *, #230864, .T. ) ;
#19480 = ORIENTED_EDGE ( 'NONE', *, *, #214676, .T. ) ;
#19481 = DIRECTION ( 'NONE',  ( 0.000000000000000000, 0.000000000000000000, -1.000000000000000000 ) ) ;
#19482 = CIRCLE ( 'NONE', #214705, 12.87499999999999822 ) ;
#19483 = CARTESIAN_POINT ( 'NONE',  ( 19.88284271247462343, 62.42586252704481353, -208.9077732303340440 ) ) ;
#19484 = EDGE_LOOP ( 'NONE', ( #22136, #23310, #84002, #185400 ) ) ;
#19485 = CARTESIAN_POINT ( 'NONE',  ( -16.95709691156270793, 22.98693315318278252, -230.9398125205108840 ) ) ;
#19486 = CARTESIAN_POINT ( 'NONE',  ( -18.59999999999999787, 1.091828907200461884, -220.1187534104809913 ) ) ;
#19487 = DIRECTION ( 'NONE',  ( 0.000000000000000000, 1.000000000000000000, 0.000000000000000000 ) ) ;
#19488 = DIRECTION ( 'NONE',  ( -1.000000000000000000, -0.000000000000000000, -0.000000000000000000 ) ) ;
#19490 = ADVANCED_FACE ( 'NONE', ( #86830 ), #67288, .T. ) ;
#19489 = DIRECTION ( 'NONE',  ( -1.000000000000000000, 0.000000000000000000, -0.000000000000000000 ) ) ;
#19491 = CARTESIAN_POINT ( 'NONE',  ( -21.05000000000000426, -0.02103547654011232379, 6.304455821947658301 ) ) ;
#19492 = CARTESIAN_POINT ( 'NONE',  ( -16.93935632781549572, 30.25768881656566123, -234.7951577570964901 ) ) ;
#19493 = CARTESIAN_POINT ( 'NONE',  ( 20.95512820512820440, 8.876151316299271343, -42.05862899514094977 ) ) ;
#19494 = EDGE_CURVE ( 'NONE', #125207, #70458, #128550, .T. ) ;
#19495 = CARTESIAN_POINT ( 'NONE',  ( -21.09107601085580086, 6.209752320307551976, -199.6073535771626553 ) ) ;
#19496 = CARTESIAN_POINT ( 'NONE',  ( 20.94999999999999929, 5.400000000011154988, -179.9052660189130677 ) ) ;
#19497 = AXIS2_PLACEMENT_3D ( 'NONE', #236284, #194629, #15990 ) ;
#19500 = ORIENTED_EDGE ( 'NONE', *, *, #22389, .T. ) ;
#19499 = AXIS2_PLACEMENT_3D ( 'NONE', #162204, #102166, #159616 ) ;
#19498 = CARTESIAN_POINT ( 'NONE',  ( 18.59999999999999076, 6.450000000011156587, -54.75000000000000000 ) ) ;
#19501 = CIRCLE ( 'NONE', #194306, 0.1000000000000028644 ) ;
#19502 = CIRCLE ( 'NONE', #73677, 0.09999999999999363565 ) ;
#19503 = EDGE_CURVE ( 'NONE', #148396, #245147, #104344, .T. ) ;
#19504 = EDGE_LOOP ( 'NONE', ( #5356, #154089, #3817, #31451 ) ) ;
#19505 = DIRECTION ( 'NONE',  ( -1.000000000000000000, 0.000000000000000000, 0.000000000000000000 ) ) ;
#19506 = EDGE_LOOP ( 'NONE', ( #180394, #112059, #250658, #207530 ) ) ;
#19507 = EDGE_CURVE ( 'NONE', #96104, #20283, #146053, .T. ) ;
#19508 = CYLINDRICAL_SURFACE ( 'NONE', #8557, 0.09999999999998898659 ) ;
#19509 = CARTESIAN_POINT ( 'NONE',  ( -18.38639463286148867, 11.48019957384713230, -109.7500000000000426 ) ) ;
#19510 = DIRECTION ( 'NONE',  ( -1.000000000000000000, -0.000000000000000000, -0.000000000000000000 ) ) ;
#19511 = EDGE_LOOP ( 'NONE', ( #79472, #45987, #132900, #20620 ) ) ;
#19512 = CARTESIAN_POINT ( 'NONE',  ( 18.57071067811864040, 10.17928932189250091, -155.3500000000000227 ) ) ;
#19513 = EDGE_CURVE ( 'NONE', #12745, #96642, #83665, .T. ) ;
#19514 = AXIS2_PLACEMENT_3D ( 'NONE', #67265, #7285, #248478 ) ;
#19515 = CARTESIAN_POINT ( 'NONE',  ( 18.49999999999996803, 7.070967871809997973, -137.7465642218683399 ) ) ;
#19516 = CARTESIAN_POINT ( 'NONE',  ( 23.24999999999999645, 1.115600667400684642E-11, -100.5000000000000284 ) ) ;
#19517 = CIRCLE ( 'NONE', #115180, 0.09999999999998898659 ) ;
#19518 = AXIS2_PLACEMENT_3D ( 'NONE', #62620, #3925, #70350 ) ;
#19519 = CARTESIAN_POINT ( 'NONE',  ( 23.14999999999999503, 64.35000000001258513, -191.3731074845244393 ) ) ;
#19520 = CARTESIAN_POINT ( 'NONE',  ( 18.52351027002948314, 85.64216290470682225, -62.80806053401445865 ) ) ;
#19521 = FACE_OUTER_BOUND ( 'NONE', #6472, .T. ) ;
#19522 = CIRCLE ( 'NONE', #161159, 0.09999999999999949207 ) ;
#19523 = ORIENTED_EDGE ( 'NONE', *, *, #57886, .T. ) ;
#19524 = CARTESIAN_POINT ( 'NONE',  ( -23.15000000000000213, 76.00000000001142553, -36.02310748452432421 ) ) ;
#19526 = VERTEX_POINT ( 'NONE', #73732 ) ;
#19525 = LINE ( 'NONE', #176043, #30310 ) ;
#19528 = B_SPLINE_CURVE_WITH_KNOTS ( 'NONE', 3,
 ( #51604, #32105, #111622, #191179, #92048, #251106, #171628, #181505, #218020, #60243 ),
 .UNSPECIFIED., .F., .F.,
 ( 4, 2, 2, 2, 4 ),
 ( 0.000000000000000000, 0.0001660831991682680617, 0.0002491247987524029600, 0.0002906455985444370157, 0.0003321663983364710171 ),
 .UNSPECIFIED. ) ;
#19527 = DIRECTION ( 'NONE',  ( 0.000000000000000000, -0.5000000000000016653, 0.8660254037844377084 ) ) ;
#19529 = ADVANCED_FACE ( 'NONE', ( #171557 ), #137659, .T. ) ;
#19530 = DIRECTION ( 'NONE',  ( 0.000000000000000000, 0.9999176327611370985, -0.01283462868041289687 ) ) ;
#19531 = DIRECTION ( 'NONE',  ( 1.000000000000000000, 0.000000000000000000, -0.000000000000000000 ) ) ;
#19532 = EDGE_LOOP ( 'NONE', ( #33983, #125396, #11979, #55453 ) ) ;
#19533 = CARTESIAN_POINT ( 'NONE',  ( 23.24999999999999289, 64.35000000001222986, -148.6731074845244507 ) ) ;
#19534 = PRODUCT_CONTEXT ( 'NONE', #20799, 'mechanical' ) ;
#19535 = CARTESIAN_POINT ( 'NONE',  ( -18.51991288638525646, 85.39243678968526297, -95.87984108056610921 ) ) ;
#19536 = ORIENTED_EDGE ( 'NONE', *, *, #209469, .F. ) ;
#19537 = DIRECTION ( 'NONE',  ( 1.000000000000000000, 0.000000000000000000, 0.000000000000000000 ) ) ;
#19538 = CARTESIAN_POINT ( 'NONE',  ( -21.65000000000000213, 18.70606281991846842, -231.7096448200342138 ) ) ;
#19539 = CIRCLE ( 'NONE', #256791, 0.09999999999999609201 ) ;
#19540 = CARTESIAN_POINT ( 'NONE',  ( -21.05000000000000071, 5.900000000011102586, -77.21909976465646253 ) ) ;
#19541 = VERTEX_POINT ( 'NONE', #150683 ) ;
#19542 = VERTEX_POINT ( 'NONE', #254848 ) ;
#19543 = PLANE ( 'NONE',  #68204 ) ;
#19544 = TOROIDAL_SURFACE ( 'NONE', #194527, 12.97499999999999609, 0.1000000000000000056 ) ;
#19545 = CARTESIAN_POINT ( 'NONE',  ( -19.89999999999999858, 1.250000000000000000, 22.00000000000000355 ) ) ;
#19546 = CARTESIAN_POINT ( 'NONE',  ( -23.15000000000000213, 76.00000000001170974, -69.52310748452431710 ) ) ;
#19547 = CARTESIAN_POINT ( 'NONE',  ( 23.15000000000000213, -9.599999999988845900, -43.39396912265245021 ) ) ;
#19548 = DIRECTION ( 'NONE',  ( -1.836970198721029934E-16, 1.000000000000000000, 0.000000000000000000 ) ) ;
#19549 = CARTESIAN_POINT ( 'NONE',  ( 22.57856590037849287, -3.230736822513305295, -228.1880465021345685 ) ) ;
#19551 = DIRECTION ( 'NONE',  ( 1.000000000000000000, 0.000000000000000000, 0.000000000000000000 ) ) ;
#19550 = AXIS2_PLACEMENT_3D ( 'NONE', #50308, #143329, #65081 ) ;
#19552 = CARTESIAN_POINT ( 'NONE',  ( 20.94403535211772294, 65.69367753730607262, -30.51892380663481674 ) ) ;
#19553 = DIRECTION ( 'NONE',  ( 0.000000000000000000, 0.2128009952263590909, -0.9770955615653318382 ) ) ;
#19554 = DIRECTION ( 'NONE',  ( -2.602085213965226419E-14, 6.982962677686266711E-15, -1.000000000000000000 ) ) ;
#19555 = LINE ( 'NONE', #219015, #142994 ) ;
#19556 = CIRCLE ( 'NONE', #240134, 12.87500000000000178 ) ;
#19557 = ORIENTED_EDGE ( 'NONE', *, *, #149206, .T. ) ;
#19558 = CIRCLE ( 'NONE', #36311, 0.1000000000000124678 ) ;
#19559 = ORIENTED_EDGE ( 'NONE', *, *, #113844, .T. ) ;
#19560 = LINE ( 'NONE', #219022, #124397 ) ;
#19561 = CARTESIAN_POINT ( 'NONE',  ( 23.24999999999999645, 67.23127455305835554, -235.8551265064784559 ) ) ;
#19562 = AXIS2_PLACEMENT_3D ( 'NONE', #27568, #107049, #164481 ) ;
#19563 = CIRCLE ( 'NONE', #178352, 0.5000000000000004441 ) ;
#19564 = DIRECTION ( 'NONE',  ( 0.000000000000000000, 0.000000000000000000, -1.000000000000000000 ) ) ;
#19565 = DIRECTION ( 'NONE',  ( -0.000000000000000000, -6.982962677686266711E-15, 1.000000000000000000 ) ) ;
#19566 = AXIS2_PLACEMENT_3D ( 'NONE', #154850, #233104, #55679 ) ;
#19567 = ADVANCED_FACE ( 'NONE', ( #95812 ), #211950, .F. ) ;
#19568 = VERTEX_POINT ( 'NONE', #133678 ) ;
#19569 = CARTESIAN_POINT ( 'NONE',  ( -23.25000000000000000, -8.999999999988844479, -157.6060308773475924 ) ) ;
#19570 = VERTEX_POINT ( 'NONE', #153284 ) ;
#19571 = ADVANCED_FACE ( 'NONE', ( #30759 ), #155363, .T. ) ;
#19572 = EDGE_CURVE ( 'NONE', #64408, #148732, #91668, .T. ) ;
#19573 = DIRECTION ( 'NONE',  ( 1.000000000000000000, 0.000000000000000000, 0.000000000000000000 ) ) ;
#19574 = VERTEX_POINT ( 'NONE', #213200 ) ;
#19575 = DIRECTION ( 'NONE',  ( 0.000000000000000000, -1.000000000000000000, 0.000000000000000000 ) ) ;
#19576 = VECTOR ( 'NONE', #155229, 1000.000000000000000 ) ;
#19577 = AXIS2_PLACEMENT_3D ( 'NONE', #6185, #81842, #236147 ) ;
#19578 = CARTESIAN_POINT ( 'NONE',  ( 18.39999999999999858, 85.50000000001136868, -29.42291809330220786 ) ) ;
#19579 = VECTOR ( 'NONE', #194596, 1000.000000000000000 ) ;
#19580 = ORIENTED_EDGE ( 'NONE', *, *, #231334, .T. ) ;
#19581 = CARTESIAN_POINT ( 'NONE',  ( 20.94999999999999929, 76.00000000001190870, -103.0231074845243029 ) ) ;
#19582 = EDGE_CURVE ( 'NONE', #246816, #247434, #93262, .T. ) ;
#19583 = ORIENTED_EDGE ( 'NONE', *, *, #49360, .F. ) ;
#19584 = AXIS2_PLACEMENT_3D ( 'NONE', #2627, #204676, #1337 ) ;
#19585 = DIRECTION ( 'NONE',  ( -0.7071067811865463515, 0.7071067811865487940, -0.000000000000000000 ) ) ;
#19586 = CIRCLE ( 'NONE', #198632, 0.5000000000000004441 ) ;
#19587 = CARTESIAN_POINT ( 'NONE',  ( -20.94999999999999929, -1.164121893241208960, -41.21484808557161017 ) ) ;
#19588 = DIRECTION ( 'NONE',  ( 0.000000000000000000, 0.8814952561688430555, -0.4721928772777346239 ) ) ;
#19589 = LINE ( 'NONE', #42999, #249967 ) ;
#19590 = CARTESIAN_POINT ( 'NONE',  ( 21.05000000000000426, 65.51923798433686841, -242.1677427744925808 ) ) ;
#19592 = CARTESIAN_POINT ( 'NONE',  ( 18.50000324121758055, 65.70692517833235513, -131.0644653378304554 ) ) ;
#19591 = DIRECTION ( 'NONE',  ( -0.000000000000000000, 0.4721928772777347905, 0.8814952561688430555 ) ) ;
#19593 = DIRECTION ( 'NONE',  ( 0.000000000000000000, 0.8660254037844424824, 0.4999999999999934497 ) ) ;
#19594 = VERTEX_POINT ( 'NONE', #94540 ) ;
#19596 = CARTESIAN_POINT ( 'NONE',  ( -16.80100914604134132, 66.05685090590840503, -115.7060633572367010 ) ) ;
#19595 = FACE_OUTER_BOUND ( 'NONE', #231651, .T. ) ;
#19597 = ORIENTED_EDGE ( 'NONE', *, *, #48994, .T. ) ;
#19599 = ORIENTED_EDGE ( 'NONE', *, *, #57404, .T. ) ;
#19598 = CARTESIAN_POINT ( 'NONE',  ( -22.39999999999999858, 64.35000000001268461, -203.6231074845244393 ) ) ;
#19600 = AXIS2_PLACEMENT_3D ( 'NONE', #211217, #190392, #127840 ) ;
#19601 = ORIENTED_EDGE ( 'NONE', *, *, #221247, .T. ) ;
#19602 = CARTESIAN_POINT ( 'NONE',  ( 20.94999999999999929, 62.04503132991427350, -248.4786563706009588 ) ) ;
#19603 = AXIS2_PLACEMENT_3D ( 'NONE', #138718, #16275, #179204 ) ;
#19604 = DIRECTION ( 'NONE',  ( -1.000000000000000000, -0.000000000000000000, 0.000000000000000000 ) ) ;
#19605 = DIRECTION ( 'NONE',  ( -0.000000000000000000, 6.982962677686266711E-15, -1.000000000000000000 ) ) ;
#19606 = ORIENTED_EDGE ( 'NONE', *, *, #40637, .F. ) ;
#19607 = ADVANCED_FACE ( 'NONE', ( #16322 ), #237653, .F. ) ;
#19609 = ADVANCED_FACE ( 'NONE', ( #76261 ), #78816, .T. ) ;
#19608 = DIRECTION ( 'NONE',  ( 1.000000000000000000, -0.000000000000000000, 0.000000000000000000 ) ) ;
#19610 = CARTESIAN_POINT ( 'NONE',  ( 21.09787244211732471, 8.775370707348422172, -112.7392533843174789 ) ) ;
#19611 = CARTESIAN_POINT ( 'NONE',  ( 20.04142135623730070, 34.35873842494069663, -235.1028360029684166 ) ) ;
#19612 = ORIENTED_EDGE ( 'NONE', *, *, #138131, .T. ) ;
#19613 = FACE_OUTER_BOUND ( 'NONE', #178671, .T. ) ;
#19614 = CIRCLE ( 'NONE', #7109, 0.09999999999999971412 ) ;
#19615 = EDGE_CURVE ( 'NONE', #212825, #77135, #66956, .T. ) ;
#19616 = CARTESIAN_POINT ( 'NONE',  ( 21.05000000000000071, 1.115600667400684642E-11, -167.4999999999999716 ) ) ;
#19617 = ORIENTED_EDGE ( 'NONE', *, *, #24666, .T. ) ;
#19618 = ORIENTED_EDGE ( 'NONE', *, *, #127837, .F. ) ;
#19619 = DIRECTION ( 'NONE',  ( 1.000000000000000000, 0.000000000000000000, 0.000000000000000000 ) ) ;
#19620 = ORIENTED_EDGE ( 'NONE', *, *, #232126, .F. ) ;
#19621 = CARTESIAN_POINT ( 'NONE',  ( -17.22767730082987825, 10.34924421246758719, -11.35757130942880977 ) ) ;
#19622 = ORIENTED_EDGE ( 'NONE', *, *, #207522, .T. ) ;
#19623 = CYLINDRICAL_SURFACE ( 'NONE', #71936, 0.09999999999999939493 ) ;
#19624 = DIRECTION ( 'NONE',  ( 0.000000000000000000, 0.000000000000000000, -1.000000000000000000 ) ) ;
#19625 = LINE ( 'NONE', #159155, #93448 ) ;
#19626 = DIRECTION ( 'NONE',  ( 1.000000000000000000, 0.000000000000000000, 0.000000000000000000 ) ) ;
#19627 = CIRCLE ( 'NONE', #206868, 0.1000000000000075273 ) ;
#19628 = CIRCLE ( 'NONE', #144493, 0.1000000000000002554 ) ;
#19629 = EDGE_CURVE ( 'NONE', #251476, #79207, #87950, .T. ) ;
#19630 = VECTOR ( 'NONE', #141021, 1000.000000000000000 ) ;
#19631 = PLANE ( 'NONE',  #250327 ) ;
#19632 = DIRECTION ( 'NONE',  ( 0.000000000000000000, 6.982962677686266711E-15, -1.000000000000000000 ) ) ;
#19633 = CARTESIAN_POINT ( 'NONE',  ( 20.94999999999999574, 67.07338541492480033, -94.55142446530125255 ) ) ;
#19634 = ORIENTED_EDGE ( 'NONE', *, *, #154555, .F. ) ;
#19636 = CARTESIAN_POINT ( 'NONE',  ( -21.14999999999999858, 6.540656951712397138, -33.50000000000000000 ) ) ;
#19635 = CYLINDRICAL_SURFACE ( 'NONE', #95608, 0.1999999999999987899 ) ;
#19637 = ORIENTED_EDGE ( 'NONE', *, *, #182180, .T. ) ;
#19640 = VERTEX_POINT ( 'NONE', #198779 ) ;
#19639 = CARTESIAN_POINT ( 'NONE',  ( -18.50000000000000000, 85.40000000001160174, -62.22584772486096938 ) ) ;
#19638 = DIRECTION ( 'NONE',  ( 0.000000000000000000, 0.000000000000000000, 1.000000000000000000 ) ) ;
#19641 = VECTOR ( 'NONE', #241333, 1000.000000000000000 ) ;
#19642 = ORIENTED_EDGE ( 'NONE', *, *, #151180, .F. ) ;
#19643 = CARTESIAN_POINT ( 'NONE',  ( 21.05000000000000071, 5.900000000011162093, -123.7809002353436654 ) ) ;
#19644 = FACE_OUTER_BOUND ( 'NONE', #165559, .T. ) ;
#19645 = EDGE_CURVE ( 'NONE', #152549, #100865, #176679, .T. ) ;
#19646 = DIRECTION ( 'NONE',  ( 0.000000000000000000, 0.000000000000000000, -1.000000000000000000 ) ) ;
#19648 = ORIENTED_EDGE ( 'NONE', *, *, #23580, .F. ) ;
#19647 =( BOUNDED_CURVE ( )  B_SPLINE_CURVE ( 3, ( #170511, #70101, #27131, #51767 ),
 .UNSPECIFIED., .F., .F. ) 
 B_SPLINE_CURVE_WITH_KNOTS ( ( 4, 4 ),
 ( 3.141592653589793116, 4.712388980384689674 ),
 .UNSPECIFIED. ) 
 CURVE ( )  GEOMETRIC_REPRESENTATION_ITEM ( )  RATIONAL_B_SPLINE_CURVE ( ( 1.000000000000000000, 0.8047378541243649375, 0.8047378541243649375, 1.000000000000000000 ) ) 
 REPRESENTATION_ITEM ( '' )  );
#19649 = DIRECTION ( 'NONE',  ( -0.9880948137434723000, -0.1484822917196432779, 0.04026969206407596952 ) ) ;
#19650 = CARTESIAN_POINT ( 'NONE',  ( 20.94999999999999929, 70.60000000001151932, -48.42837350343745584 ) ) ;
#19651 = EDGE_CURVE ( 'NONE', #37631, #244528, #13000, .T. ) ;
#19653 = CARTESIAN_POINT ( 'NONE',  ( -22.50000000000000000, 64.25000000001269029, -203.5231074845244166 ) ) ;
#19652 = CARTESIAN_POINT ( 'NONE',  ( -21.51976009735018991, 6.910458441670358276, -167.4999999999999716 ) ) ;
#19654 = ADVANCED_FACE ( 'NONE', ( #157116 ), #138772, .T. ) ;
#19655 = AXIS2_PLACEMENT_3D ( 'NONE', #206078, #11752, #131671 ) ;
#19657 = EDGE_LOOP ( 'NONE', ( #105640, #9416, #4500, #203347 ) ) ;
#19656 = CARTESIAN_POINT ( 'NONE',  ( -18.59999999999999787, 22.34215363070824623, -231.2750834139128528 ) ) ;
#19658 = TOROIDAL_SURFACE ( 'NONE', #28040, 0.4000000000000012990, 0.1000000000000000056 ) ;
#19659 = EDGE_LOOP ( 'NONE', ( #155323, #54902, #200500, #42750 ) ) ;
#19660 = VECTOR ( 'NONE', #187002, 1000.000000000000000 ) ;
#19661 = ADVANCED_FACE ( 'NONE', ( #196214 ), #116677, .T. ) ;
#19662 = CARTESIAN_POINT ( 'NONE',  ( -16.94878442675511820, 44.08354183875889731, -235.2764748885172708 ) ) ;
#19664 = EDGE_CURVE ( 'NONE', #70270, #6867, #97076, .T. ) ;
#19663 = VERTEX_POINT ( 'NONE', #17568 ) ;
#19665 = DIRECTION ( 'NONE',  ( 0.000000000000000000, 0.000000000000000000, -1.000000000000000000 ) ) ;
#19666 = ORIENTED_EDGE ( 'NONE', *, *, #181840, .T. ) ;
#19667 = CARTESIAN_POINT ( 'NONE',  ( -23.15000000000000213, 85.50000000001207923, -126.6291383618717816 ) ) ;
#19668 = CARTESIAN_POINT ( 'NONE',  ( 21.14999999999999503, 11.65000000001116298, -100.6000000000000369 ) ) ;
#19669 = DIRECTION ( 'NONE',  ( 0.000000000000000000, 0.9126074666063545004, 0.4088369013363783999 ) ) ;
#19670 = EDGE_CURVE ( 'NONE', #71510, #29887, #21370, .T. ) ;
#19671 = ORIENTED_EDGE ( 'NONE', *, *, #160936, .F. ) ;
#19672 = CARTESIAN_POINT ( 'NONE',  ( -20.94999999999999929, 1.115600667400684642E-11, -200.9999999999999432 ) ) ;
#19673 = ADVANCED_FACE ( 'NONE', ( #42290 ), #192065, .F. ) ;
#19674 = AXIS2_PLACEMENT_3D ( 'NONE', #37812, #18229, #258069 ) ;
#19675 = AXIS2_PLACEMENT_3D ( 'NONE', #203245, #145825, #63731 ) ;
#19676 = DIRECTION ( 'NONE',  ( 0.000000000000000000, -1.000000000000000000, 0.000000000000000000 ) ) ;
#19678 = EDGE_CURVE ( 'NONE', #62589, #135784, #50548, .T. ) ;
#19677 = CIRCLE ( 'NONE', #15406, 0.09999999999999939493 ) ;
#19679 = AXIS2_PLACEMENT_3D ( 'NONE', #35236, #76881, #13090 ) ;
#19680 = EDGE_CURVE ( 'NONE', #203793, #188954, #99657, .T. ) ;
#19681 = ORIENTED_EDGE ( 'NONE', *, *, #245943, .T. ) ;
#19682 = ORIENTED_EDGE ( 'NONE', *, *, #255911, .T. ) ;
#19683 = ORIENTED_EDGE ( 'NONE', *, *, #182989, .T. ) ;
#19684 = EDGE_CURVE ( 'NONE', #103509, #100947, #60548, .T. ) ;
#19685 = LINE ( 'NONE', #103037, #16625 ) ;
#19686 = EDGE_LOOP ( 'NONE', ( #91709, #195489, #141138, #129426, #131841 ) ) ;
#19688 = VERTEX_POINT ( 'NONE', #80082 ) ;
#19687 = CARTESIAN_POINT ( 'NONE',  ( -18.59999999999999787, 9.150000000011157653, -112.8500000000000369 ) ) ;
#19690 = EDGE_CURVE ( 'NONE', #231547, #90736, #66743, .T. ) ;
#19689 = ORIENTED_EDGE ( 'NONE', *, *, #18841, .F. ) ;
#19691 = EDGE_CURVE ( 'NONE', #227674, #228133, #92068, .T. ) ;
#19694 = ORIENTED_EDGE ( 'NONE', *, *, #70088, .T. ) ;
#19693 = ORIENTED_EDGE ( 'NONE', *, *, #104664, .F. ) ;
#19692 = CARTESIAN_POINT ( 'NONE',  ( -16.77683809663752257, 66.05416425680785153, -115.6870565036285683 ) ) ;
#19695 = CIRCLE ( 'NONE', #165443, 0.09999999999999695244 ) ;
#19696 = ADVANCED_FACE ( 'NONE', ( #164807 ), #185651, .F. ) ;
#19697 = TOROIDAL_SURFACE ( 'NONE', #102865, 4.099999999999999645, 0.1000000000000000056 ) ;
#19698 = EDGE_LOOP ( 'NONE', ( #60673, #37912, #194931, #109236, #253158 ) ) ;
#19699 = DIRECTION ( 'NONE',  ( -0.000000000000000000, -0.000000000000000000, -1.000000000000000000 ) ) ;
#19700 = DIRECTION ( 'NONE',  ( 2.879366945564059217E-14, 0.9875055080513762684, -0.1575844902526679081 ) ) ;
#19701 = CIRCLE ( 'NONE', #52803, 0.1000000000000055844 ) ;
#19702 = PLANE ( 'NONE',  #213240 ) ;
#19703 = EDGE_LOOP ( 'NONE', ( #199129, #86771, #217954, #94055, #211050 ) ) ;
#19704 = CARTESIAN_POINT ( 'NONE',  ( -21.05000000000000071, 77.83534155023646406, -124.9679561919612922 ) ) ;
#19706 = ORIENTED_EDGE ( 'NONE', *, *, #241626, .T. ) ;
#19705 = CARTESIAN_POINT ( 'NONE',  ( 20.94999999999999574, 14.81796439977981272, -236.5325475414793743 ) ) ;
#19707 = FACE_OUTER_BOUND ( 'NONE', #30932, .T. ) ;
#19709 = VERTEX_POINT ( 'NONE', #83924 ) ;
#19708 = DIRECTION ( 'NONE',  ( -1.000000000000000000, 0.000000000000000000, -0.000000000000000000 ) ) ;
#19710 = ADVANCED_FACE ( 'NONE', ( #167397 ), #143941, .T. ) ;
#19711 =( BOUNDED_SURFACE ( )  B_SPLINE_SURFACE ( 3, 2, ( 
 ( #237684, #175191, #176447 ),
 ( #139847, #60315, #38214 ),
 ( #215542, #156893, #138549 ),
 ( #42069, #199861, #21233 ),
 ( #57744, #197269, #18634 ),
 ( #19936, #76036, #141158 ) ),
 .UNSPECIFIED., .F., .F., .F. ) 
 B_SPLINE_SURFACE_WITH_KNOTS ( ( 4, 2, 4 ),
 ( 3, 3 ),
 ( -1.776356839400250465E-15, 0.7853981633974468357, 1.570796326794895448 ),
 ( 0.000000000000000000, 1.000000000000000000 ),
 .UNSPECIFIED. ) 
 GEOMETRIC_REPRESENTATION_ITEM ( )  RATIONAL_B_SPLINE_SURFACE ( (
 ( 1.000000000000000000, 0.5000000000000154321, 1.000000000000000000),
 ( 1.000000000000000000, 0.4993418825323190369, 1.000000000000000000),
 ( 1.000000000000000000, 0.5278258667072365240, 1.000000000000000000),
 ( 1.000000000000000000, 0.6092287576681939543, 1.000000000000000000),
 ( 1.000000000000000000, 0.6611148371789450362, 1.000000000000000000),
 ( 1.000000000000000000, 0.7071067811865597852, 1.000000000000000000) ) ) 
 REPRESENTATION_ITEM ( '' )  SURFACE ( )  );
#19712 = EDGE_LOOP ( 'NONE', ( #205396, #58710, #31284, #89260 ) ) ;
#19713 = EDGE_CURVE ( 'NONE', #90604, #15766, #86513, .T. ) ;
#19714 = CARTESIAN_POINT ( 'NONE',  ( 21.05000000000000071, 1.115600667400684642E-11, -100.5000000000000284 ) ) ;
#19715 = CARTESIAN_POINT ( 'NONE',  ( -21.64999999999999858, 10.05000000001113847, -121.3500000000000369 ) ) ;
#19716 = EDGE_LOOP ( 'NONE', ( #126538, #153068, #256599, #61537, #148896 ) ) ;
#19717 = ORIENTED_EDGE ( 'NONE', *, *, #218107, .F. ) ;
#19718 = DIRECTION ( 'NONE',  ( -1.000000000000000000, -0.000000000000000000, 0.000000000000000000 ) ) ;
#19719 = CARTESIAN_POINT ( 'NONE',  ( 21.05000000000000071, 64.25000000001249134, -177.0379132551784096 ) ) ;
#19720 = TOROIDAL_SURFACE ( 'NONE', #240293, 4.099999999999999645, 0.1000000000000000056 ) ;
#19722 = VERTEX_POINT ( 'NONE', #205192 ) ;
#19721 = ORIENTED_EDGE ( 'NONE', *, *, #72032, .F. ) ;
#19723 = VERTEX_POINT ( 'NONE', #206495 ) ;
#19724 = CARTESIAN_POINT ( 'NONE',  ( 21.07199075132372101, 61.95919758692989632, -221.7705522472584221 ) ) ;
#19725 = VERTEX_POINT ( 'NONE', #26595 ) ;
#19726 = ORIENTED_EDGE ( 'NONE', *, *, #229683, .F. ) ;
#19727 = DIRECTION ( 'NONE',  ( 0.000000000000000000, 0.000000000000000000, -1.000000000000000000 ) ) ;
#19728 = ORIENTED_EDGE ( 'NONE', *, *, #137818, .T. ) ;
#19729 = SPHERICAL_SURFACE ( 'NONE', #56424, 0.1000000000000000056 ) ;
#19730 = AXIS2_PLACEMENT_3D ( 'NONE', #158731, #199108, #240809 ) ;
#19732 = CARTESIAN_POINT ( 'NONE',  ( 21.05000000000000071, 11.60000000001116227, -127.0717967697245143 ) ) ;
#19731 = FACE_OUTER_BOUND ( 'NONE', #174934, .T. ) ;
#19733 = VERTEX_POINT ( 'NONE', #8315 ) ;
#19735 = ORIENTED_EDGE ( 'NONE', *, *, #211857, .F. ) ;
#19734 = EDGE_LOOP ( 'NONE', ( #159888, #42005, #149791, #254449 ) ) ;
#19736 = VECTOR ( 'NONE', #211691, 1000.000000000000000 ) ;
#19737 = DIRECTION ( 'NONE',  ( 0.000000000000000000, -0.2128009952263578697, 0.9770955615653320603 ) ) ;
#19739 = ADVANCED_FACE ( 'NONE', ( #65695 ), #9571, .T. ) ;
#19738 = DIRECTION ( 'NONE',  ( 0.000000000000000000, 0.9126074666063660468, 0.4088369013363524762 ) ) ;
#19740 = ORIENTED_EDGE ( 'NONE', *, *, #217306, .F. ) ;
#19741 = AXIS2_PLACEMENT_3D ( 'NONE', #37586, #175813, #58380 ) ;
#19742 = CIRCLE ( 'NONE', #203055, 0.5000000000000004441 ) ;
#19743 = EDGE_CURVE ( 'NONE', #96608, #152513, #71253, .T. ) ;
#19744 =( BOUNDED_CURVE ( )  B_SPLINE_CURVE ( 3, ( #116095, #131791, #11875, #34021 ),
 .UNSPECIFIED., .F., .F. ) 
 B_SPLINE_CURVE_WITH_KNOTS ( ( 4, 4 ),
 ( 1.570796326794916320, 3.141592653589837969 ),
 .UNSPECIFIED. ) 
 CURVE ( )  GEOMETRIC_REPRESENTATION_ITEM ( )  RATIONAL_B_SPLINE_CURVE ( ( 1.000000000000000000, 0.8047378541243590533, 0.8047378541243590533, 1.000000000000000000 ) ) 
 REPRESENTATION_ITEM ( '' )  );
#19745 = ORIENTED_EDGE ( 'NONE', *, *, #23579, .F. ) ;
#19746 = DIRECTION ( 'NONE',  ( -0.000000000000000000, 6.982962677686266711E-15, -1.000000000000000000 ) ) ;
#19747 = CIRCLE ( 'NONE', #202885, 14.30833333333333535 ) ;
#19748 = VERTEX_POINT ( 'NONE', #124401 ) ;
#19749 = ORIENTED_EDGE ( 'NONE', *, *, #73936, .F. ) ;
#19750 = CARTESIAN_POINT ( 'NONE',  ( 23.15000000000000213, -3.363022478626109368, -226.2703567425896267 ) ) ;
#19751 = VECTOR ( 'NONE', #162532, 1000.000000000000000 ) ;
#19752 = ORIENTED_EDGE ( 'NONE', *, *, #131149, .F. ) ;
#19753 = DIRECTION ( 'NONE',  ( 0.000000000000000000, 0.000000000000000000, -1.000000000000000000 ) ) ;
#19754 = CYLINDRICAL_SURFACE ( 'NONE', #172752, 0.1000000000000075273 ) ;
#19755 = ORIENTED_EDGE ( 'NONE', *, *, #7851, .T. ) ;
#19756 = DIRECTION ( 'NONE',  ( -0.000000000000000000, 0.4791956752371485107, 0.8777080977375185666 ) ) ;
#19757 = DIRECTION ( 'NONE',  ( 1.000000000000000000, 0.000000000000000000, 0.000000000000000000 ) ) ;
#19759 = DIRECTION ( 'NONE',  ( -0.000000000000000000, 1.000000000000000000, 6.982962677686266711E-15 ) ) ;
#19758 = DIRECTION ( 'NONE',  ( -1.000000000000000000, 0.000000000000000000, 0.000000000000000000 ) ) ;
#19760 = DIRECTION ( 'NONE',  ( 1.000000000000000000, 0.000000000000000000, 0.000000000000000000 ) ) ;
#19761 = CARTESIAN_POINT ( 'NONE',  ( 23.14999999999999858, 4.000000000011155521, -67.00000000000000000 ) ) ;
#19762 = CARTESIAN_POINT ( 'NONE',  ( -13.40000000000000213, -11.65000000000000036, 12.40000000000000391 ) ) ;
#19763 = CARTESIAN_POINT ( 'NONE',  ( -16.78493211734303614, 66.05416425680807890, -149.1870565036285257 ) ) ;
#19764 = CARTESIAN_POINT ( 'NONE',  ( -20.94999999999999929, 7.128833340094563376, -233.7327013124401276 ) ) ;
#19765 = DIRECTION ( 'NONE',  ( -1.000000000000000000, 0.000000000000000000, 0.000000000000000000 ) ) ;
#19766 = ADVANCED_FACE ( 'NONE', ( #107385 ), #67131, .T. ) ;
#19767 = EDGE_LOOP ( 'NONE', ( #159755, #149827, #238151, #42704 ) ) ;
#19768 = CIRCLE ( 'NONE', #123808, 7.791421356237338003 ) ;
#19771 = VERTEX_POINT ( 'NONE', #106081 ) ;
#19770 = VERTEX_POINT ( 'NONE', #186962 ) ;
#19769 = CIRCLE ( 'NONE', #28148, 0.5000000000000004441 ) ;
#19772 = ORIENTED_EDGE ( 'NONE', *, *, #233839, .T. ) ;
#19773 = VERTEX_POINT ( 'NONE', #203921 ) ;
#19774 = AXIS2_PLACEMENT_3D ( 'NONE', #135705, #255617, #173622 ) ;
#19775 = LINE ( 'NONE', #80992, #36957 ) ;
#19776 = DIRECTION ( 'NONE',  ( 1.000000000000000000, -0.000000000000000000, -0.000000000000000000 ) ) ;
#19777 = AXIS2_PLACEMENT_3D ( 'NONE', #93730, #155017, #33804 ) ;
#19779 = CARTESIAN_POINT ( 'NONE',  ( 18.59999999999998366, 76.00000000001190870, -103.0231074845243029 ) ) ;
#19778 = CARTESIAN_POINT ( 'NONE',  ( 22.60000000000000142, 11.74956712350054744, -167.3991416309012550 ) ) ;
#19780 = DIRECTION ( 'NONE',  ( 1.000000000000000000, 0.000000000000000000, 0.000000000000000000 ) ) ;
#19781 = EDGE_LOOP ( 'NONE', ( #242329, #171297, #115439, #157132, #166602 ) ) ;
#19782 = CARTESIAN_POINT ( 'NONE',  ( -20.86777300164945004, 10.33200063080771969, -106.0931674956643320 ) ) ;
#19783 = PLANE ( 'NONE',  #91642 ) ;
#19784 = CARTESIAN_POINT ( 'NONE',  ( -17.01825945287482966, 10.05000000001113847, -113.1500000000000341 ) ) ;
#19785 = CARTESIAN_POINT ( 'NONE',  ( -23.25000000000000000, 5.950000000011167245, -56.69429769496518645 ) ) ;
#19786 = EDGE_LOOP ( 'NONE', ( #89582, #249358, #173286, #204235 ) ) ;
#19787 = VECTOR ( 'NONE', #93831, 1000.000000000000000 ) ;
#19788 = AXIS2_PLACEMENT_3D ( 'NONE', #236329, #137228, #60250 ) ;
#19789 = CIRCLE ( 'NONE', #69675, 0.1000000000000028644 ) ;
#19790 = LINE ( 'NONE', #141017, #109715 ) ;
#19791 = FACE_OUTER_BOUND ( 'NONE', #66512, .T. ) ;
#19792 = ORIENTED_EDGE ( 'NONE', *, *, #35804, .T. ) ;
#19793 = DIRECTION ( 'NONE',  ( 0.000000000000000000, 0.000000000000000000, -1.000000000000000000 ) ) ;
#19794 = FACE_OUTER_BOUND ( 'NONE', #70630, .T. ) ;
#19795 = CARTESIAN_POINT ( 'NONE',  ( 20.04142135623730070, 11.65000000001115943, -121.8500000000000369 ) ) ;
#19796 = CARTESIAN_POINT ( 'NONE',  ( -18.40000000000000213, 11.75000000001113953, -188.3499999999999659 ) ) ;
#19797 = FACE_OUTER_BOUND ( 'NONE', #164616, .T. ) ;
#19798 = ORIENTED_EDGE ( 'NONE', *, *, #13784, .F. ) ;
#19799 = DIRECTION ( 'NONE',  ( -1.000000000000000000, 0.000000000000000000, 0.000000000000000000 ) ) ;
#19801 = ADVANCED_FACE ( 'NONE', ( #46128 ), #183092, .F. ) ;
#19800 = DIRECTION ( 'NONE',  ( 0.000000000000000000, 0.000000000000000000, -1.000000000000000000 ) ) ;
#19802 = CARTESIAN_POINT ( 'NONE',  ( -23.15000000000000213, 26.18196512540240661, -241.1028522842020152 ) ) ;
#19803 = AXIS2_PLACEMENT_3D ( 'NONE', #69477, #228543, #49888 ) ;
#19805 = CARTESIAN_POINT ( 'NONE',  ( -20.54999999999999716, 87.75000000001151079, -48.37310748452424036 ) ) ;
#19804 = DIRECTION ( 'NONE',  ( 1.000000000000000000, 0.000000000000000000, -0.000000000000000000 ) ) ;
#19806 = LINE ( 'NONE', #240129, #212263 ) ;
#19807 = EDGE_CURVE ( 'NONE', #210872, #220110, #96337, .T. ) ;
#19808 = AXIS2_PLACEMENT_3D ( 'NONE', #5283, #65288, #204783 ) ;
#19809 = CARTESIAN_POINT ( 'NONE',  ( -16.94165728009537375, 9.987869755934930538, -121.3910550085102358 ) ) ;
#19810 = CARTESIAN_POINT ( 'NONE',  ( -14.00000000000000178, 9.850000000011133849, -150.7500000000000284 ) ) ;
#19812 = DIRECTION ( 'NONE',  ( 0.000000000000000000, 2.891205793294679805E-16, -1.000000000000000000 ) ) ;
#19811 = VECTOR ( 'NONE', #252968, 1000.000000000000000 ) ;
#19813 = ORIENTED_EDGE ( 'NONE', *, *, #15774, .F. ) ;
#19814 = CIRCLE ( 'NONE', #86388, 0.5000000000000004441 ) ;
#19815 = ORIENTED_EDGE ( 'NONE', *, *, #127575, .F. ) ;
#19816 = ADVANCED_FACE ( 'NONE', ( #89112 ), #146235, .F. ) ;
#19817 = ORIENTED_EDGE ( 'NONE', *, *, #6203, .F. ) ;
#19818 = ADVANCED_FACE ( 'NONE', ( #43574 ), #200415, .T. ) ;
#19819 = DIRECTION ( 'NONE',  ( -4.336808689942053235E-15, 0.8103668758649498205, -0.5859227990963324917 ) ) ;
#19820 = TOROIDAL_SURFACE ( 'NONE', #40691, 0.4000000000000005773, 0.1000000000000000056 ) ;
#19821 = AXIS2_PLACEMENT_3D ( 'NONE', #6215, #22284, #127460 ) ;
#19822 = AXIS2_PLACEMENT_3D ( 'NONE', #3757, #183691, #84527 ) ;
#19823 = CIRCLE ( 'NONE', #53116, 11.64999999999999325 ) ;
#19824 = CARTESIAN_POINT ( 'NONE',  ( -18.40000000000000213, -9.499999999988851584, -174.5320693966996259 ) ) ;
#19825 = EDGE_CURVE ( 'NONE', #186900, #60596, #4427, .T. ) ;
#19826 = AXIS2_PLACEMENT_3D ( 'NONE', #180602, #98441, #175482 ) ;
#19827 = PLANE ( 'NONE',  #4590 ) ;
#19828 = ORIENTED_EDGE ( 'NONE', *, *, #162361, .F. ) ;
#19829 = VECTOR ( 'NONE', #223999, 1000.000000000000000 ) ;
#19830 = LINE ( 'NONE', #220581, #151305 ) ;
#19831 = CARTESIAN_POINT ( 'NONE',  ( -15.51798037960204901, 9.376659938544690931, -51.12819254821731363 ) ) ;
#19832 = DIRECTION ( 'NONE',  ( -7.304098846218134667E-16, 1.000000000000000000, -0.000000000000000000 ) ) ;
#19834 = EDGE_LOOP ( 'NONE', ( #33258, #140547, #41856, #46276 ) ) ;
#19833 = CARTESIAN_POINT ( 'NONE',  ( -16.85697194749122829, 9.908543714134735225, -188.0649957323861656 ) ) ;
#19836 = CARTESIAN_POINT ( 'NONE',  ( -23.25000000000000000, 76.00000000001190870, -103.0231074845243029 ) ) ;
#19835 = DIRECTION ( 'NONE',  ( 1.000000000000000000, 0.000000000000000000, -0.000000000000000000 ) ) ;
#19837 = EDGE_CURVE ( 'NONE', #196423, #26265, #233750, .T. ) ;
#19838 = CARTESIAN_POINT ( 'NONE',  ( 20.09999999999999787, 22.88362888408688178, -231.1113624623563965 ) ) ;
#19839 = DIRECTION ( 'NONE',  ( 0.000000000000000000, 0.000000000000000000, 1.000000000000000000 ) ) ;
#19840 = CARTESIAN_POINT ( 'NONE',  ( -20.00894256274684579, 5.586869314946281584, 16.41686200241345261 ) ) ;
#19841 = DIRECTION ( 'NONE',  ( -0.7071067811865127117, -0.7071067811865821007, 0.000000000000000000 ) ) ;
#19842 = VERTEX_POINT ( 'NONE', #172561 ) ;
#19843 = AXIS2_PLACEMENT_3D ( 'NONE', #234102, #195009, #134986 ) ;
#19844 = CARTESIAN_POINT ( 'NONE',  ( 0.000000000000000000, 0.000000000000000000, 0.000000000000000000 ) ) ;
#19845 = DIRECTION ( 'NONE',  ( 0.000000000000000000, 0.000000000000000000, -1.000000000000000000 ) ) ;
#19846 = EDGE_LOOP ( 'NONE', ( #124840, #182489, #109143, #1685, #72668 ) ) ;
#19847 = DIRECTION ( 'NONE',  ( 0.000000000000000000, -0.9992764785629962843, -0.03803313543132441632 ) ) ;
#19848 = ORIENTED_EDGE ( 'NONE', *, *, #207468, .T. ) ;
#19849 = AXIS2_PLACEMENT_3D ( 'NONE', #125427, #69310, #129273 ) ;
#19850 = CARTESIAN_POINT ( 'NONE',  ( 20.94999999999999929, 87.29603075034795268, -200.4752083248604038 ) ) ;
#19851 = CARTESIAN_POINT ( 'NONE',  ( 23.14999999999999858, 5.500000000011153745, -45.90526601891310321 ) ) ;
#19852 = DIRECTION ( 'NONE',  ( 0.000000000000000000, 0.000000000000000000, -1.000000000000000000 ) ) ;
#19853 = ORIENTED_EDGE ( 'NONE', *, *, #108175, .T. ) ;
#19854 = ORIENTED_EDGE ( 'NONE', *, *, #226448, .T. ) ;
#19855 = LINE ( 'NONE', #57659, #81875 ) ;
#19856 = CARTESIAN_POINT ( 'NONE',  ( -23.25000000000000000, 63.67210543329348837, -237.4495904216901181 ) ) ;
#19857 = CARTESIAN_POINT ( 'NONE',  ( -16.84981964351515416, 63.05979328488731284, -213.3481213180943712 ) ) ;
#19858 = CARTESIAN_POINT ( 'NONE',  ( 21.05000000000000071, 5.850000000011156942, -190.8675027757220448 ) ) ;
#19860 = SPHERICAL_SURFACE ( 'NONE', #11775, 0.1000000000000000056 ) ;
#19859 = CARTESIAN_POINT ( 'NONE',  ( 21.05000000000000071, 70.15000000001235492, -159.8906102602464330 ) ) ;
#19861 = CIRCLE ( 'NONE', #86447, 0.1000000000000028644 ) ;
#19862 = CIRCLE ( 'NONE', #157442, 0.09999999999998898659 ) ;
#19863 = CARTESIAN_POINT ( 'NONE',  ( 18.49999999999998934, 69.55000000001187743, -93.00608031408432907 ) ) ;
#19864 = CARTESIAN_POINT ( 'NONE',  ( -21.05000000000000071, -11.75000000000000000, -30.39999999999999503 ) ) ;
#19865 = CIRCLE ( 'NONE', #49059, 4.000000000000006217 ) ;
#19866 = DIRECTION ( 'NONE',  ( -1.000000000000000000, -5.945622153099073960E-16, 5.981866248895712861E-16 ) ) ;
#19867 = ORIENTED_EDGE ( 'NONE', *, *, #44203, .T. ) ;
#19868 = CARTESIAN_POINT ( 'NONE',  ( 23.14999999999999858, 72.00000000001141132, -36.02310748452435263 ) ) ;
#19869 = ADVANCED_FACE ( 'NONE', ( #94244 ), #242097, .T. ) ;
#19871 = VERTEX_POINT ( 'NONE', #13443 ) ;
#19870 = DIRECTION ( 'NONE',  ( 0.000000000000000000, 0.000000000000000000, 1.000000000000000000 ) ) ;
#19872 = CARTESIAN_POINT ( 'NONE',  ( 23.14999999999999503, 64.35000000001254250, -182.1731074845244507 ) ) ;
#19873 = DIRECTION ( 'NONE',  ( 0.000000000000000000, -0.000000000000000000, 1.000000000000000000 ) ) ;
#19875 = CARTESIAN_POINT ( 'NONE',  ( -20.94999999999999929, 61.95000000001162022, -64.00941241376342816 ) ) ;
#19874 = CYLINDRICAL_SURFACE ( 'NONE', #75335, 0.1000000000000054040 ) ;
#19876 = ORIENTED_EDGE ( 'NONE', *, *, #30355, .T. ) ;
#19878 = DIRECTION ( 'NONE',  ( 1.000000000000000000, 0.000000000000000000, 0.000000000000000000 ) ) ;
#19877 = CARTESIAN_POINT ( 'NONE',  ( -16.85722902420149083, 66.05000000001159322, -56.75756001075396995 ) ) ;
#19879 = LINE ( 'NONE', #42013, #162310 ) ;
#19880 = DIRECTION ( 'NONE',  ( 0.000000000000000000, -8.267618268485201230E-15, 1.000000000000000000 ) ) ;
#19881 = FACE_OUTER_BOUND ( 'NONE', #226182, .T. ) ;
#19883 = EDGE_CURVE ( 'NONE', #52520, #121571, #109955, .T. ) ;
#19882 = CARTESIAN_POINT ( 'NONE',  ( -15.74999999999999645, 66.65000000001256808, -186.6588398769082460 ) ) ;
#19884 = ORIENTED_EDGE ( 'NONE', *, *, #223004, .T. ) ;
#19885 = DIRECTION ( 'NONE',  ( 0.000000000000000000, -6.938893903907222067E-15, 1.000000000000000000 ) ) ;
#19886 = VERTEX_POINT ( 'NONE', #252039 ) ;
#19887 = EDGE_CURVE ( 'NONE', #103723, #42401, #232505, .T. ) ;
#19888 = VECTOR ( 'NONE', #92419, 1000.000000000000000 ) ;
#19889 = EDGE_CURVE ( 'NONE', #62655, #182152, #121354, .T. ) ;
#19890 = CARTESIAN_POINT ( 'NONE',  ( -22.59999999999999787, 67.23127455305841238, -235.8551265064783991 ) ) ;
#19891 = ORIENTED_EDGE ( 'NONE', *, *, #214755, .T. ) ;
#19892 = CARTESIAN_POINT ( 'NONE',  ( -20.87600722750343252, 46.46487552657982434, -243.0839400145317200 ) ) ;
#19893 = ORIENTED_EDGE ( 'NONE', *, *, #39652, .F. ) ;
#19895 = CARTESIAN_POINT ( 'NONE',  ( 20.94999999999999574, 46.53760404070597900, -243.0973507280067167 ) ) ;
#19894 = AXIS2_PLACEMENT_3D ( 'NONE', #153084, #51333, #252128 ) ;
#19896 = CARTESIAN_POINT ( 'NONE',  ( -21.55000000000000426, 52.90028168070691095, -233.8284721206281915 ) ) ;
#19897 = ORIENTED_EDGE ( 'NONE', *, *, #36092, .T. ) ;
#19898 = EDGE_CURVE ( 'NONE', #83686, #141820, #183682, .T. ) ;
#19899 = EDGE_CURVE ( 'NONE', #114396, #176555, #117212, .T. ) ;
#19900 = CARTESIAN_POINT ( 'NONE',  ( 21.05000000000000071, 17.83900070254454562, -239.4698447713637677 ) ) ;
#19901 = DIRECTION ( 'NONE',  ( 0.000000000000000000, 6.577889128801576950E-15, -1.000000000000000000 ) ) ;
#19902 = CARTESIAN_POINT ( 'NONE',  ( 23.14999999999999858, 1.115600667400684642E-11, -134.0000000000000000 ) ) ;
#19903 = DIRECTION ( 'NONE',  ( 0.000000000000000000, -0.9770955615653316162, -0.2128009952263604232 ) ) ;
#19904 = CARTESIAN_POINT ( 'NONE',  ( 20.94999999999999929, 16.44800918141279666, -240.8068063186265135 ) ) ;
#19905 = CARTESIAN_POINT ( 'NONE',  ( 19.87657994471983258, 62.37345882273933739, -208.8772024246652848 ) ) ;
#19906 = AXIS2_PLACEMENT_3D ( 'NONE', #178875, #197101, #156737 ) ;
#19907 = EDGE_LOOP ( 'NONE', ( #177883, #232608, #248019, #151934 ) ) ;
#19908 = LINE ( 'NONE', #79837, #224042 ) ;
#19910 = ORIENTED_EDGE ( 'NONE', *, *, #6305, .T. ) ;
#19909 = AXIS2_PLACEMENT_3D ( 'NONE', #209200, #228787, #68418 ) ;
#19912 = ORIENTED_EDGE ( 'NONE', *, *, #235281, .F. ) ;
#19911 = CARTESIAN_POINT ( 'NONE',  ( -16.86422026484316916, 66.02955263915120554, -90.44089425885137246 ) ) ;
#19913 = ORIENTED_EDGE ( 'NONE', *, *, #249561, .T. ) ;
#19914 = CARTESIAN_POINT ( 'NONE',  ( 18.60000000000000142, -9.321008403361283001, -7.235938249077890738 ) ) ;
#19915 = LINE ( 'NONE', #158173, #20722 ) ;
#19916 = CARTESIAN_POINT ( 'NONE',  ( 12.93225390519043394, 66.58234804117158490, -188.1643200920839547 ) ) ;
#19917 = DIRECTION ( 'NONE',  ( 1.000000000000000000, 0.000000000000000000, 0.000000000000000000 ) ) ;
#19918 = EDGE_CURVE ( 'NONE', #126571, #936, #216994, .T. ) ;
#19919 = CARTESIAN_POINT ( 'NONE',  ( -18.59999999999999787, -1.249999999988843369, -141.8004807544151333 ) ) ;
#19920 = ORIENTED_EDGE ( 'NONE', *, *, #38761, .F. ) ;
#19921 = EDGE_CURVE ( 'NONE', #195613, #207366, #42202, .T. ) ;
#19922 = EDGE_CURVE ( 'NONE', #209479, #226219, #221240, .T. ) ;
#19923 = FACE_OUTER_BOUND ( 'NONE', #58175, .T. ) ;
#19924 = AXIS2_PLACEMENT_3D ( 'NONE', #87817, #108695, #7018 ) ;
#19925 = DIRECTION ( 'NONE',  ( 0.000000000000000000, 0.8814952561688476074, -0.4721928772777262417 ) ) ;
#19926 = ORIENTED_EDGE ( 'NONE', *, *, #203042, .F. ) ;
#19928 = ORIENTED_EDGE ( 'NONE', *, *, #147508, .T. ) ;
#19927 = DIRECTION ( 'NONE',  ( 1.000000000000000000, 0.000000000000000000, 0.000000000000000000 ) ) ;
#19929 = DIRECTION ( 'NONE',  ( 0.000000000000000000, -1.224646799142015331E-16, 1.000000000000000000 ) ) ;
#19930 = CIRCLE ( 'NONE', #165675, 0.09999999999999939493 ) ;
#19931 = DIRECTION ( 'NONE',  ( -3.469446951953635015E-14, 1.000000000000000000, 0.000000000000000000 ) ) ;
#19932 = AXIS2_PLACEMENT_3D ( 'NONE', #24134, #241869, #81480 ) ;
#19933 = VERTEX_POINT ( 'NONE', #16029 ) ;
#19934 = TOROIDAL_SURFACE ( 'NONE', #82420, 0.2000000000000000111, 0.1000000000000000056 ) ;
#19935 = VECTOR ( 'NONE', #249863, 1000.000000000000000 ) ;
#19936 = CARTESIAN_POINT ( 'NONE',  ( 20.94999999999999929, 64.35000000001195986, -109.8069731475024753 ) ) ;
#19938 = ORIENTED_EDGE ( 'NONE', *, *, #100397, .T. ) ;
#19937 = VECTOR ( 'NONE', #186848, 1000.000000000000000 ) ;
#19939 = DIRECTION ( 'NONE',  ( 1.000000000000000000, 0.000000000000000000, 0.000000000000000000 ) ) ;
#19940 = VECTOR ( 'NONE', #222142, 1000.000000000000000 ) ;
#19941 = DIRECTION ( 'NONE',  ( 0.000000000000000000, -1.000000000000000000, -6.982962677686266711E-15 ) ) ;
#19942 = CARTESIAN_POINT ( 'NONE',  ( -20.54999999999999716, 47.70572087816298534, -241.8629305864830030 ) ) ;
#19943 = LINE ( 'NONE', #99437, #59433 ) ;
#19944 = EDGE_CURVE ( 'NONE', #180003, #51281, #108817, .T. ) ;
#19945 = AXIS2_PLACEMENT_3D ( 'NONE', #135964, #158158, #215510 ) ;
#19946 = AXIS2_PLACEMENT_3D ( 'NONE', #95689, #175278, #254728 ) ;
#19947 = VERTEX_POINT ( 'NONE', #55092 ) ;
#19948 = CARTESIAN_POINT ( 'NONE',  ( -18.59999999999999787, -1.835859311432481045, -78.50443916879852679 ) ) ;
#19949 = CIRCLE ( 'NONE', #182448, 0.09999999999998898659 ) ;
#19950 = ORIENTED_EDGE ( 'NONE', *, *, #224634, .T. ) ;
#19951 = AXIS2_PLACEMENT_3D ( 'NONE', #192834, #71613, #136683 ) ;
#19952 = CARTESIAN_POINT ( 'NONE',  ( -16.91256925476571027, 12.42391174447540081, -211.1203373714319014 ) ) ;
#19953 = EDGE_CURVE ( 'NONE', #65618, #113714, #90391, .T. ) ;
#19954 = CARTESIAN_POINT ( 'NONE',  ( -16.92973740335372668, 9.992503814478325808, -79.59394096479805114 ) ) ;
#19956 = VERTEX_POINT ( 'NONE', #95532 ) ;
#19955 = LINE ( 'NONE', #116476, #204122 ) ;
#19957 = DIRECTION ( 'NONE',  ( 1.000000000000000000, 0.000000000000000000, 0.000000000000000000 ) ) ;
#19959 = CIRCLE ( 'NONE', #140744, 0.6000000000000033085 ) ;
#19958 = CARTESIAN_POINT ( 'NONE',  ( 5.900000000000059863, 64.75000000001119815, -26.02310748452479316 ) ) ;
#19960 = DIRECTION ( 'NONE',  ( 1.000000000000000000, 0.000000000000000000, 0.000000000000000000 ) ) ;
#19961 = DIRECTION ( 'NONE',  ( 1.000000000000000000, 0.000000000000000000, 0.000000000000000000 ) ) ;
#19962 = CARTESIAN_POINT ( 'NONE',  ( -16.80468759584937999, 9.942153675145297242, -79.69001886620168307 ) ) ;
#19963 = EDGE_CURVE ( 'NONE', #10689, #92883, #29768, .T. ) ;
#19964 = CARTESIAN_POINT ( 'NONE',  ( -22.94999999999999929, -11.75000000000000178, 0.000000000000000000 ) ) ;
#19965 = CARTESIAN_POINT ( 'NONE',  ( -18.59999999999999787, 1.835341550235567887, -179.0551512925629538 ) ) ;
#19967 = ORIENTED_EDGE ( 'NONE', *, *, #85312, .F. ) ;
#19966 = DIRECTION ( 'NONE',  ( 0.000000000000000000, -7.147358527629762208E-15, 1.000000000000000000 ) ) ;
#19968 = ADVANCED_FACE ( 'NONE', ( #193375 ), #63026, .T. ) ;
#19969 = AXIS2_PLACEMENT_3D ( 'NONE', #153206, #232727, #133600 ) ;
#19970 = AXIS2_PLACEMENT_3D ( 'NONE', #244857, #226566, #46645 ) ;
#19971 = AXIS2_PLACEMENT_3D ( 'NONE', #11156, #73720, #110246 ) ;
#19973 = EDGE_CURVE ( 'NONE', #237270, #195703, #72140, .T. ) ;
#19972 = CARTESIAN_POINT ( 'NONE',  ( -21.14999999999999858, 0.000000000000000000, 0.000000000000000000 ) ) ;
#19975 = EDGE_CURVE ( 'NONE', #210448, #139103, #12174, .T. ) ;
#19974 = ORIENTED_EDGE ( 'NONE', *, *, #73750, .T. ) ;
#19976 = ORIENTED_EDGE ( 'NONE', *, *, #217389, .F. ) ;
#19977 = CARTESIAN_POINT ( 'NONE',  ( -18.31572283045156269, 85.54843783089712872, -62.67248183346567458 ) ) ;
#19978 = CARTESIAN_POINT ( 'NONE',  ( 22.00411653962182612, 68.74655713164194992, -103.1221455903250188 ) ) ;
#19979 = ORIENTED_EDGE ( 'NONE', *, *, #103594, .T. ) ;
#19980 = VECTOR ( 'NONE', #96398, 1000.000000000000000 ) ;
#19981 = AXIS2_PLACEMENT_3D ( 'NONE', #10145, #225312, #230476 ) ;
#19982 = CARTESIAN_POINT ( 'NONE',  ( -18.58693740092132884, 85.40643215026457824, -62.39829102802289640 ) ) ;
#19984 = EDGE_LOOP ( 'NONE', ( #133292, #201580, #7841, #122249 ) ) ;
#19983 = AXIS2_PLACEMENT_3D ( 'NONE', #126963, #206498, #82661 ) ;
#19986 = EDGE_CURVE ( 'NONE', #41654, #72182, #216956, .T. ) ;
#19985 = FACE_OUTER_BOUND ( 'NONE', #153828, .T. ) ;
#19987 = EDGE_CURVE ( 'NONE', #192209, #119332, #136255, .T. ) ;
#19989 = LINE ( 'NONE', #215587, #105442 ) ;
#19988 = VECTOR ( 'NONE', #176276, 1000.000000000000000 ) ;
#19990 = VERTEX_POINT ( 'NONE', #58943 ) ;
#19991 = CARTESIAN_POINT ( 'NONE',  ( 18.59999999999999787, 0.6656436123793491033, -212.6810495496487476 ) ) ;
#19992 = ORIENTED_EDGE ( 'NONE', *, *, #6717, .F. ) ;
#19993 = ADVANCED_FACE ( 'NONE', ( #78528 ), #118966, .T. ) ;
#19994 = CYLINDRICAL_SURFACE ( 'NONE', #17218, 0.09999999999999939493 ) ;
#19996 = ORIENTED_EDGE ( 'NONE', *, *, #220432, .F. ) ;
#19995 = DIRECTION ( 'NONE',  ( 1.000000000000000000, 0.000000000000000000, 0.000000000000000000 ) ) ;
#19997 = CIRCLE ( 'NONE', #107465, 0.2000000000000057288 ) ;
#19998 = DIRECTION ( 'NONE',  ( 0.000000000000000000, -1.000000000000000000, -8.717686153663073805E-15 ) ) ;
#19999 = ORIENTED_EDGE ( 'NONE', *, *, #99913, .T. ) ;
#20000 = DIRECTION ( 'NONE',  ( -2.952720810173289112E-16, -0.4088369013363281068, 0.9126074666063770380 ) ) ;
#20001 = AXIS2_PLACEMENT_3D ( 'NONE', #80381, #19157, #82946 ) ;
#20003 = ORIENTED_EDGE ( 'NONE', *, *, #96953, .T. ) ;
#20002 = ADVANCED_FACE ( 'NONE', ( #56391 ), #79797, .T. ) ;
#20005 = ORIENTED_EDGE ( 'NONE', *, *, #176783, .F. ) ;
#20004 = ORIENTED_EDGE ( 'NONE', *, *, #164578, .F. ) ;
#20006 = CARTESIAN_POINT ( 'NONE',  ( 21.14999999999999858, 69.45934304831089889, -136.5231074845243313 ) ) ;
#20007 = VECTOR ( 'NONE', #151775, 1000.000000000000000 ) ;
#20008 = ORIENTED_EDGE ( 'NONE', *, *, #7633, .F. ) ;
#20009 = ADVANCED_FACE ( 'NONE', ( #220626 ), #15708, .F. ) ;
#20010 = DIRECTION ( 'NONE',  ( 0.000000000000000000, 0.000000000000000000, -1.000000000000000000 ) ) ;
#20011 = ORIENTED_EDGE ( 'NONE', *, *, #180829, .F. ) ;
#20012 = AXIS2_PLACEMENT_3D ( 'NONE', #140289, #22963, #144140 ) ;
#20013 = EDGE_CURVE ( 'NONE', #182615, #235424, #144658, .T. ) ;
#20014 = EDGE_LOOP ( 'NONE', ( #197304, #193207, #199949, #249919, #30284, #198304 ) ) ;
#20015 = CARTESIAN_POINT ( 'NONE',  ( -22.39999999999999858, 0.09770955616802273758, -200.9787199004788931 ) ) ;
#20016 = CARTESIAN_POINT ( 'NONE',  ( 23.15000000000000213, -7.274670914976375080, -212.7102428701827250 ) ) ;
#20018 = ORIENTED_EDGE ( 'NONE', *, *, #70319, .F. ) ;
#20017 = CARTESIAN_POINT ( 'NONE',  ( 21.05000000000000071, 67.23127455305841238, -235.8551265064783991 ) ) ;
#20019 = CARTESIAN_POINT ( 'NONE',  ( -20.94999999999999929, 5.850000000011108092, -144.1324972242779836 ) ) ;
#20020 = ORIENTED_EDGE ( 'NONE', *, *, #248326, .F. ) ;
#20021 = CARTESIAN_POINT ( 'NONE',  ( -21.55000000000000426, 68.25000000001179501, -81.77310748452435973 ) ) ;
#20022 = DIRECTION ( 'NONE',  ( -0.000000000000000000, -1.000000000000000000, 0.000000000000000000 ) ) ;
#20023 = EDGE_CURVE ( 'NONE', #168244, #103469, #175126, .T. ) ;
#20024 = CARTESIAN_POINT ( 'NONE',  ( -23.15000000000000213, 84.59626168225477727, -78.97323500167452437 ) ) ;
#20025 = CIRCLE ( 'NONE', #194994, 0.09999999999998898659 ) ;
#20026 = VERTEX_POINT ( 'NONE', #255844 ) ;
#20027 = DIRECTION ( 'NONE',  ( 0.000000000000000000, 0.2128009952263601456, -0.9770955615653316162 ) ) ;
#20028 = DIRECTION ( 'NONE',  ( 1.000000000000000000, 7.492892343619937423E-30, -1.073024830501117725E-15 ) ) ;
#20029 = DIRECTION ( 'NONE',  ( 0.000000000000000000, -1.000000000000000000, 0.000000000000000000 ) ) ;
#20030 = VERTEX_POINT ( 'NONE', #99362 ) ;
#20031 = DIRECTION ( 'NONE',  ( 0.000000000000000000, 6.982962677686266711E-15, -1.000000000000000000 ) ) ;
#20032 = ORIENTED_EDGE ( 'NONE', *, *, #56060, .T. ) ;
#20034 = ORIENTED_EDGE ( 'NONE', *, *, #167574, .F. ) ;
#20033 = AXIS2_PLACEMENT_3D ( 'NONE', #85948, #66422, #187673 ) ;
#20035 = CARTESIAN_POINT ( 'NONE',  ( 23.14999999999999858, 76.00000000001170974, -69.52310748452431710 ) ) ;
#20036 = ORIENTED_EDGE ( 'NONE', *, *, #97676, .F. ) ;
#20037 = ORIENTED_EDGE ( 'NONE', *, *, #110135, .F. ) ;
#20038 = DIRECTION ( 'NONE',  ( 0.000000000000000000, -6.938893903907222067E-15, 1.000000000000000000 ) ) ;
#20039 = CARTESIAN_POINT ( 'NONE',  ( 21.05000000000000071, 87.48912529308779540, -72.62310748452422615 ) ) ;
#20040 = ORIENTED_EDGE ( 'NONE', *, *, #79671, .F. ) ;
#20041 = ORIENTED_EDGE ( 'NONE', *, *, #149771, .F. ) ;
#20042 = DIRECTION ( 'NONE',  ( 0.000000000000000000, 0.000000000000000000, -1.000000000000000000 ) ) ;
#20043 = DIRECTION ( 'NONE',  ( 0.000000000000000000, -0.7397360091702802620, 0.6728971962616779878 ) ) ;
#20044 = EDGE_LOOP ( 'NONE', ( #171747, #128100 ) ) ;
#20045 = EDGE_LOOP ( 'NONE', ( #19343, #100321, #206300, #212968 ) ) ;
#20046 = AXIS2_PLACEMENT_3D ( 'NONE', #33537, #113026, #54319 ) ;
#20047 = TOROIDAL_SURFACE ( 'NONE', #36639, 12.97499999999999787, 0.1000000000000000056 ) ;
#20048 = VERTEX_POINT ( 'NONE', #201055 ) ;
#20049 = ADVANCED_FACE ( 'NONE', ( #178967 ), #257045, .T. ) ;
#20050 = DIRECTION ( 'NONE',  ( -1.000000000000000000, -0.000000000000000000, -0.000000000000000000 ) ) ;
#20051 = DIRECTION ( 'NONE',  ( -1.000000000000000000, -0.000000000000000000, -0.000000000000000000 ) ) ;
#20052 = DIRECTION ( 'NONE',  ( 0.000000000000000000, -0.1350103645451876944, -0.9908441862701601321 ) ) ;
#20053 = DIRECTION ( 'NONE',  ( 0.000000000000000000, 1.000000000000000000, 0.000000000000000000 ) ) ;
#20054 = CARTESIAN_POINT ( 'NONE',  ( 21.05000000000000071, 65.27628318601605883, -162.4287082486403051 ) ) ;
#20055 = FACE_OUTER_BOUND ( 'NONE', #157628, .T. ) ;
#20056 = DIRECTION ( 'NONE',  ( 0.000000000000000000, 0.000000000000000000, 1.000000000000000000 ) ) ;
#20059 = CARTESIAN_POINT ( 'NONE',  ( 21.13498764882293557, 6.495618143485025975, -100.4983436052687011 ) ) ;
#20058 = TOROIDAL_SURFACE ( 'NONE', #49264, 4.149999999999999467, 0.1000000000000000056 ) ;
#20057 = DIRECTION ( 'NONE',  ( -1.000000000000000000, -0.000000000000000000, -0.000000000000000000 ) ) ;
#20060 = DIRECTION ( 'NONE',  ( 0.000000000000000000, 0.000000000000000000, -1.000000000000000000 ) ) ;
#20061 = CARTESIAN_POINT ( 'NONE',  ( -16.87333278164172867, 23.37215640887969670, -231.2226159629232711 ) ) ;
#20062 = AXIS2_PLACEMENT_3D ( 'NONE', #121595, #163269, #177715 ) ;
#20063 = CARTESIAN_POINT ( 'NONE',  ( -40.23850191057533010, 66.15000000001120384, -5.923107484524795296 ) ) ;
#20064 = EDGE_CURVE ( 'NONE', #38206, #99016, #173943, .T. ) ;
#20065 = CARTESIAN_POINT ( 'NONE',  ( 20.94999999999999929, 5.900000000011162093, -56.78090023534362984 ) ) ;
#20066 =( BOUNDED_SURFACE ( )  B_SPLINE_SURFACE ( 3, 2, ( 
 ( #76078, #100737, #21278 ),
 ( #196041, #176487, #160788 ),
 ( #61657, #159486, #18680 ),
 ( #156931, #38252, #237727 ),
 ( #198590, #136027, #199901 ),
 ( #59051, #220730, #19982 ),
 ( #99468, #116501, #42115 ),
 ( #155658, #56495, #17397 ) ),
 .UNSPECIFIED., .F., .F., .T. ) 
 B_SPLINE_SURFACE_WITH_KNOTS ( ( 4, 2, 2, 4 ),
 ( 3, 3 ),
 ( 0.0001723339234021441008, 0.0002782939632049910138, 0.0003842540030078378998, 0.0005961740826135316718 ),
 ( 0.000000000000000000, 1.000000000000000000 ),
 .UNSPECIFIED. ) 
 GEOMETRIC_REPRESENTATION_ITEM ( )  RATIONAL_B_SPLINE_SURFACE ( (
 ( 1.000000000000000000, 0.9504532311154639812, 1.000000000000000000),
 ( 1.000000000000000000, 0.9506023220709097776, 1.000000000000000000),
 ( 1.000000000000000000, 0.9395774818182517363, 1.000000000000000000),
 ( 1.000000000000000000, 0.9079328464645827212, 1.000000000000000000),
 ( 1.000000000000000000, 0.8875702416206650014, 1.000000000000000000),
 ( 1.000000000000000000, 0.8205919608037296475, 1.000000000000000000),
 ( 1.000000000000000000, 0.7666842783600821276, 1.000000000000000000),
 ( 1.000000000000000000, 0.7071067811864313324, 1.000000000000000000) ) ) 
 REPRESENTATION_ITEM ( '' )  SURFACE ( )  );
#20067 = ORIENTED_EDGE ( 'NONE', *, *, #40806, .F. ) ;
#20068 = AXIS2_PLACEMENT_3D ( 'NONE', #100196, #196753, #156388 ) ;
#20070 = ORIENTED_EDGE ( 'NONE', *, *, #84983, .T. ) ;
#20069 = LINE ( 'NONE', #123016, #32425 ) ;
#20071 = DIRECTION ( 'NONE',  ( -0.000000000000000000, 0.01283462868039629209, -0.9999176327611372095 ) ) ;
#20072 = CARTESIAN_POINT ( 'NONE',  ( -23.25000000000000355, 11.74999999999998224, -12.65000000000000213 ) ) ;
#20073 = SURFACE_STYLE_FILL_AREA ( #120478 ) ;
#20074 = VERTEX_POINT ( 'NONE', #40737 ) ;
#20075 = CARTESIAN_POINT ( 'NONE',  ( 20.94999027547553894, 10.29326151435327219, -206.4592822510414578 ) ) ;
#20076 = AXIS2_PLACEMENT_3D ( 'NONE', #167985, #229218, #191397 ) ;
#20077 = DIRECTION ( 'NONE',  ( 1.000000000000000000, 0.000000000000000000, 0.000000000000000000 ) ) ;
#20078 = ORIENTED_EDGE ( 'NONE', *, *, #57496, .F. ) ;
#20079 = AXIS2_PLACEMENT_3D ( 'NONE', #415, #79927, #121687 ) ;
#20080 = CIRCLE ( 'NONE', #28500, 0.1000000000000043493 ) ;
#20081 = PLANE ( 'NONE',  #212990 ) ;
#20082 = CARTESIAN_POINT ( 'NONE',  ( -18.50000000000000000, 64.35000000001276987, -215.2731074845244450 ) ) ;
#20083 = DIRECTION ( 'NONE',  ( 0.000000000000000000, 0.4088369013363280513, -0.9126074666063769270 ) ) ;
#20084 = CARTESIAN_POINT ( 'NONE',  ( 20.95000000000005258, 65.25000000001119815, -3.123107484524795474 ) ) ;
#20085 = ORIENTED_EDGE ( 'NONE', *, *, #174729, .T. ) ;
#20086 = AXIS2_PLACEMENT_3D ( 'NONE', #79810, #197211, #141103 ) ;
#20088 = ORIENTED_EDGE ( 'NONE', *, *, #97769, .F. ) ;
#20087 = DIRECTION ( 'NONE',  ( 0.000000000000000000, 0.000000000000000000, 1.000000000000000000 ) ) ;
#20089 = CARTESIAN_POINT ( 'NONE',  ( -21.14999999999999858, 76.00000000001165290, -69.52310748452431710 ) ) ;
#20090 = CARTESIAN_POINT ( 'NONE',  ( -21.64999999999999858, 68.75000000001254818, -182.3731074845244109 ) ) ;
#20091 = ADVANCED_FACE ( 'NONE', ( #238906 ), #254580, .T. ) ;
#20092 = DIRECTION ( 'NONE',  ( 0.000000000000000000, -1.000000000000000000, 6.308085367188393199E-16 ) ) ;
#20093 = CARTESIAN_POINT ( 'NONE',  ( -21.14999999999999858, 0.000000000000000000, 6.540656951701240729 ) ) ;
#20095 = DIRECTION ( 'NONE',  ( 0.000000000000000000, 6.982962677686266711E-15, -1.000000000000000000 ) ) ;
#20094 = LINE ( 'NONE', #244250, #65688 ) ;
#20096 = CARTESIAN_POINT ( 'NONE',  ( -16.91247567987038281, 66.04091731634333939, -190.8943830259870822 ) ) ;
#20098 = ADVANCED_FACE ( 'NONE', ( #17299 ), #211311, .T. ) ;
#20097 = LINE ( 'NONE', #502, #69874 ) ;
#20099 = DIRECTION ( 'NONE',  ( -0.000000000000000000, -0.000000000000000000, -1.000000000000000000 ) ) ;
#20100 = CARTESIAN_POINT ( 'NONE',  ( 22.47071067811865319, 0.09909245471376171288, -159.7799252555019223 ) ) ;
#20101 = CIRCLE ( 'NONE', #157500, 0.1000000000000124678 ) ;
#20102 = CIRCLE ( 'NONE', #78519, 0.09999999999999939493 ) ;
#20103 = LINE ( 'NONE', #99594, #135156 ) ;
#20104 = TOROIDAL_SURFACE ( 'NONE', #49318, 0.2000000000000000111, 0.1000000000000000056 ) ;
#20105 = ORIENTED_EDGE ( 'NONE', *, *, #62846, .T. ) ;
#20106 = CARTESIAN_POINT ( 'NONE',  ( 21.07928932188134397, 0.09889514566578934407, -94.17148334360132367 ) ) ;
#20107 = VECTOR ( 'NONE', #210053, 1000.000000000000000 ) ;
#20108 = ORIENTED_EDGE ( 'NONE', *, *, #226570, .T. ) ;
#20109 = VERTEX_POINT ( 'NONE', #117665 ) ;
#20110 = ADVANCED_FACE ( 'NONE', ( #120276 ), #18575, .T. ) ;
#20111 = DIRECTION ( 'NONE',  ( 1.000000000000000000, 0.000000000000000000, 0.000000000000000000 ) ) ;
#20112 = DIRECTION ( 'NONE',  ( 0.000000000000000000, -6.467318590049456648E-15, 1.000000000000000000 ) ) ;
#20113 = EDGE_LOOP ( 'NONE', ( #122982, #193652, #175135, #60700 ) ) ;
#20114 = EDGE_CURVE ( 'NONE', #111529, #143593, #48985, .T. ) ;
#20115 = EDGE_LOOP ( 'NONE', ( #170389, #106133, #80148, #8979 ) ) ;
#20117 = ADVANCED_FACE ( 'NONE', ( #21168 ), #119742, .F. ) ;
#20116 = CIRCLE ( 'NONE', #11942, 0.09999999999999939493 ) ;
#20118 = ORIENTED_EDGE ( 'NONE', *, *, #118057, .F. ) ;
#20119 = VECTOR ( 'NONE', #163092, 1000.000000000000000 ) ;
#20120 = ORIENTED_EDGE ( 'NONE', *, *, #92904, .F. ) ;
#20122 = DIRECTION ( 'NONE',  ( 1.000000000000000000, 0.000000000000000000, 0.000000000000000000 ) ) ;
#20121 = AXIS2_PLACEMENT_3D ( 'NONE', #29095, #168612, #239434 ) ;
#20123 = CARTESIAN_POINT ( 'NONE',  ( -22.47007471830798409, 1.829591166069288732E-15, 7.720710651926479429 ) ) ;
#20124 = DIRECTION ( 'NONE',  ( -1.000000000000000000, 1.772924042024179204E-16, -4.808324575169892332E-17 ) ) ;
#20125 = PRESENTATION_LAYER_ASSIGNMENT (  '', '', ( #190849 ) ) ;
#20126 = AXIS2_PLACEMENT_3D ( 'NONE', #96675, #35493, #17196 ) ;
#20127 = CARTESIAN_POINT ( 'NONE',  ( -23.25000000000000000, 64.35000000001254250, -182.2731074845244450 ) ) ;
#20128 = DIRECTION ( 'NONE',  ( 1.000000000000000000, 0.000000000000000000, 0.000000000000000000 ) ) ;
#20129 = CIRCLE ( 'NONE', #249267, 11.74999999999999645 ) ;
#20130 = CARTESIAN_POINT ( 'NONE',  ( -18.54270223418606633, 77.31779168390137613, -241.8822140496988595 ) ) ;
#20131 = DIRECTION ( 'NONE',  ( 0.000000000000000000, 0.1350103645451876666, 0.9908441862701600211 ) ) ;
#20133 = ORIENTED_EDGE ( 'NONE', *, *, #241622, .T. ) ;
#20132 = CARTESIAN_POINT ( 'NONE',  ( -22.47071067811865319, 75.90090754530910999, -77.24318222902238062 ) ) ;
#20135 = LINE ( 'NONE', #63088, #137625 ) ;
#20134 = CARTESIAN_POINT ( 'NONE',  ( -16.81744102076748959, 66.05000000001224691, -149.1731074845244223 ) ) ;
#20136 = ADVANCED_FACE ( 'NONE', ( #237623 ), #160679, .T. ) ;
#20137 = CARTESIAN_POINT ( 'NONE',  ( -21.05000000000000071, 76.10000000001174669, -81.17310748452432279 ) ) ;
#20138 = ORIENTED_EDGE ( 'NONE', *, *, #70099, .F. ) ;
#20139 = PLANE ( 'NONE',  #139584 ) ;
#20140 = CARTESIAN_POINT ( 'NONE',  ( 23.14999999999999503, 6.450000000011156587, -79.35000000000005116 ) ) ;
#20141 = VERTEX_POINT ( 'NONE', #45831 ) ;
#20143 = CARTESIAN_POINT ( 'NONE',  ( -16.93294127766158752, 65.99671989705713315, -115.5932002186951451 ) ) ;
#20142 = CARTESIAN_POINT ( 'NONE',  ( 20.04142135623730070, 11.65000000001115943, -21.75000000000000355 ) ) ;
#20144 = DIRECTION ( 'NONE',  ( -1.000000000000000000, -0.000000000000000000, -0.000000000000000000 ) ) ;
#20145 = CARTESIAN_POINT ( 'NONE',  ( 23.14999999999999858, 78.02678328198446422, -204.0727887811995629 ) ) ;
#20146 = AXIS2_PLACEMENT_3D ( 'NONE', #246096, #88261, #28358 ) ;
#20148 = ORIENTED_EDGE ( 'NONE', *, *, #151761, .F. ) ;
#20147 = TOROIDAL_SURFACE ( 'NONE', #232550, 0.4000000000000003553, 0.1000000000000000056 ) ;
#20149 = CIRCLE ( 'NONE', #165909, 0.1000000000000028644 ) ;
#20150 = DIRECTION ( 'NONE',  ( -1.000000000000000000, -1.186688945009010077E-16, -0.000000000000000000 ) ) ;
#20151 = CARTESIAN_POINT ( 'NONE',  ( -18.46919391072059824, -0.9001965033011636308, -242.3115848965057353 ) ) ;
#20152 = DIRECTION ( 'NONE',  ( -1.073024830501117725E-15, 0.000000000000000000, 1.000000000000000000 ) ) ;
#20153 = CARTESIAN_POINT ( 'NONE',  ( -18.50000000000000000, 9.350000000011156942, -79.35000000000005116 ) ) ;
#20154 = EDGE_LOOP ( 'NONE', ( #198621, #116720, #205322, #235928 ) ) ;
#20155 = ADVANCED_FACE ( 'NONE', ( #147502 ), #167102, .F. ) ;
#20156 = CARTESIAN_POINT ( 'NONE',  ( 20.85000000000000142, 77.83585931145570669, -125.0186683157258329 ) ) ;
#20157 = AXIS2_PLACEMENT_3D ( 'NONE', #60811, #200345, #42540 ) ;
#20158 = CARTESIAN_POINT ( 'NONE',  ( -17.80356949362895236, 10.87673139700259028, -123.7130730242463557 ) ) ;
#20159 = DIRECTION ( 'NONE',  ( -1.000000000000000000, 0.000000000000000000, 0.000000000000000000 ) ) ;
#20160 = DIRECTION ( 'NONE',  ( 0.000000000000000000, 0.000000000000000000, -1.000000000000000000 ) ) ;
#20161 = AXIS2_PLACEMENT_3D ( 'NONE', #49687, #249186, #247886 ) ;
#20162 = LINE ( 'NONE', #1843, #55145 ) ;
#20163 = VECTOR ( 'NONE', #225616, 1000.000000000000000 ) ;
#20164 = EDGE_CURVE ( 'NONE', #48436, #41846, #53072, .T. ) ;
#20166 = ORIENTED_EDGE ( 'NONE', *, *, #4389, .F. ) ;
#20165 = DIRECTION ( 'NONE',  ( -1.000000000000000000, -0.000000000000000000, -0.000000000000000000 ) ) ;
#20167 = DIRECTION ( 'NONE',  ( -1.073024830501117725E-15, -0.000000000000000000, -1.000000000000000000 ) ) ;
#20168 = CARTESIAN_POINT ( 'NONE',  ( -16.83558968593870020, 66.05000000001187743, -90.36080229690789167 ) ) ;
#20169 = CARTESIAN_POINT ( 'NONE',  ( 18.59999999999999432, 1.162701749949165642, -108.6000000000000227 ) ) ;
#20170 = CARTESIAN_POINT ( 'NONE',  ( 21.05000000000000071, 10.72371710471868056, -175.1649135690875880 ) ) ;
#20172 = ORIENTED_EDGE ( 'NONE', *, *, #246019, .F. ) ;
#20171 = CARTESIAN_POINT ( 'NONE',  ( 21.05000000000000071, 67.22371710471909978, -57.37310748452438247 ) ) ;
#20173 = DIRECTION ( 'NONE',  ( 0.000000000000000000, 0.9856811345164829818, 0.1686199900910294314 ) ) ;
#20174 = AXIS2_PLACEMENT_3D ( 'NONE', #9750, #29365, #89280 ) ;
#20175 = DIRECTION ( 'NONE',  ( -1.000000000000000000, 0.000000000000000000, 0.000000000000000000 ) ) ;
#20176 = CYLINDRICAL_SURFACE ( 'NONE', #44841, 14.30833333333333890 ) ;
#20177 = EDGE_CURVE ( 'NONE', #76904, #31642, #198823, .T. ) ;
#20178 = VERTEX_POINT ( 'NONE', #27595 ) ;
#20179 = DIRECTION ( 'NONE',  ( 0.000000000000000000, 1.000000000000000000, 6.982962677686266711E-15 ) ) ;
#20180 = DIRECTION ( 'NONE',  ( 1.000000000000000000, -0.000000000000000000, 0.000000000000000000 ) ) ;
#20181 = CIRCLE ( 'NONE', #53491, 0.09999999999999939493 ) ;
#20182 = AXIS2_PLACEMENT_3D ( 'NONE', #128209, #91646, #12135 ) ;
#20183 = DIRECTION ( 'NONE',  ( 0.000000000000000000, -6.982962677686266711E-15, 1.000000000000000000 ) ) ;
#20184 = AXIS2_PLACEMENT_3D ( 'NONE', #230054, #31881, #166261 ) ;
#20185 = ADVANCED_FACE ( 'NONE', ( #202339 ), #163226, .T. ) ;
#20186 = CARTESIAN_POINT ( 'NONE',  ( -22.45305610364634674, -0.1008583690875579225, -88.75043287651064361 ) ) ;
#20187 = CIRCLE ( 'NONE', #15929, 6.329289321881370611 ) ;
#20188 = CARTESIAN_POINT ( 'NONE',  ( 21.14999999999999858, 64.35000000001204512, -124.3731074845243825 ) ) ;
#20189 = ORIENTED_EDGE ( 'NONE', *, *, #253155, .T. ) ;
#20190 = ORIENTED_EDGE ( 'NONE', *, *, #132845, .T. ) ;
#20191 = DIRECTION ( 'NONE',  ( 1.000000000000000000, 3.448943450116723568E-16, 6.438528483529607644E-16 ) ) ;
#20192 = DIRECTION ( 'NONE',  ( -1.000000000000000000, 2.952720810173289112E-16, 2.061873921506763405E-30 ) ) ;
#20193 = ADVANCED_FACE ( 'NONE', ( #244022 ), #157159, .T. ) ;
#20194 = DIRECTION ( 'NONE',  ( -1.000000000000000000, -0.000000000000000000, -0.000000000000000000 ) ) ;
#20195 = LINE ( 'NONE', #184382, #64323 ) ;
#20196 = ORIENTED_EDGE ( 'NONE', *, *, #36727, .T. ) ;
#20197 = FACE_OUTER_BOUND ( 'NONE', #49165, .T. ) ;
#20198 = ADVANCED_FACE ( 'NONE', ( #43272 ), #181513, .F. ) ;
#20200 = ADVANCED_FACE ( 'NONE', ( #127944 ), #94766, .F. ) ;
#20199 = DIRECTION ( 'NONE',  ( 0.000000000000000000, -0.9999631594459057471, 0.008583690987121077309 ) ) ;
#20201 = DIRECTION ( 'NONE',  ( 1.000000000000000000, 0.000000000000000000, 0.000000000000000000 ) ) ;
#20202 = CARTESIAN_POINT ( 'NONE',  ( 20.95512820512820440, 10.62384868372303615, -108.1649135690876449 ) ) ;
#20203 = FACE_OUTER_BOUND ( 'NONE', #121989, .T. ) ;
#20204 = ORIENTED_EDGE ( 'NONE', *, *, #133147, .F. ) ;
#20205 = CARTESIAN_POINT ( 'NONE',  ( -16.87036670365549895, 66.01058118071095748, -191.0026676018264880 ) ) ;
#20206 = EDGE_CURVE ( 'NONE', #123531, #219752, #66687, .T. ) ;
#20207 = ORIENTED_EDGE ( 'NONE', *, *, #244651, .F. ) ;
#20208 = CARTESIAN_POINT ( 'NONE',  ( -16.87683809663752044, 9.864913447280185821, -20.22428155130396021 ) ) ;
#20209 = ORIENTED_EDGE ( 'NONE', *, *, #137688, .F. ) ;
#20210 = CARTESIAN_POINT ( 'NONE',  ( -17.11825945287481687, 10.05000000001113847, -154.8500000000000227 ) ) ;
#20211 = DIRECTION ( 'NONE',  ( 0.000000000000000000, 6.982962677686266711E-15, -1.000000000000000000 ) ) ;
#20212 = PLANE ( 'NONE',  #141368 ) ;
#20213 = ORIENTED_EDGE ( 'NONE', *, *, #32150, .T. ) ;
#20214 = EDGE_CURVE ( 'NONE', #162766, #56965, #86212, .T. ) ;
#20215 = ADVANCED_FACE ( 'NONE', ( #241473 ), #26280, .F. ) ;
#20216 = DIRECTION ( 'NONE',  ( 0.000000000000000000, 0.000000000000000000, 1.000000000000000000 ) ) ;
#20217 = LINE ( 'NONE', #75072, #34646 ) ;
#20218 = ORIENTED_EDGE ( 'NONE', *, *, #32920, .T. ) ;
#20219 = CARTESIAN_POINT ( 'NONE',  ( -15.06720934482786056, 9.417690691074257714, -152.1416006967646695 ) ) ;
#20221 = ORIENTED_EDGE ( 'NONE', *, *, #93068, .F. ) ;
#20220 = CARTESIAN_POINT ( 'NONE',  ( -18.59999999999999787, 76.00000000001185185, -95.12310748452429721 ) ) ;
#20222 = CARTESIAN_POINT ( 'NONE',  ( 21.05000000000000071, 87.29603075034721371, -106.0710066441880883 ) ) ;
#20223 = CARTESIAN_POINT ( 'NONE',  ( -18.49999999999999289, 85.32100840337362513, -162.7871692354464699 ) ) ;
#20224 = VECTOR ( 'NONE', #14129, 1000.000000000000000 ) ;
#20225 = TOROIDAL_SURFACE ( 'NONE', #11864, 0.2000000000000000111, 0.1000000000000000056 ) ;
#20226 = VECTOR ( 'NONE', #239192, 1000.000000000000000 ) ;
#20227 = VERTEX_POINT ( 'NONE', #104491 ) ;
#20228 = CARTESIAN_POINT ( 'NONE',  ( -20.54999999999999716, 7.250000000011155521, -112.7500000000000284 ) ) ;
#20229 = DIRECTION ( 'NONE',  ( -0.000000000000000000, 0.6132151058540549204, -0.7899159663865520375 ) ) ;
#20230 = AXIS2_PLACEMENT_3D ( 'NONE', #108640, #13406, #190782 ) ;
#20231 = CARTESIAN_POINT ( 'NONE',  ( -23.25000000000000000, 85.60000000001251408, -179.9170766071767389 ) ) ;
#20232 = ORIENTED_EDGE ( 'NONE', *, *, #13793, .F. ) ;
#20233 = CARTESIAN_POINT ( 'NONE',  ( 23.15000000000000213, -11.74999999998883737, -121.8500000000000369 ) ) ;
#20234 = EDGE_CURVE ( 'NONE', #24894, #87486, #253300, .T. ) ;
#20235 = EDGE_CURVE ( 'NONE', #70460, #49525, #169661, .T. ) ;
#20236 = CARTESIAN_POINT ( 'NONE',  ( 14.45963434102923806, 49.63592998410994284, -233.3809899335355453 ) ) ;
#20237 = SPHERICAL_SURFACE ( 'NONE', #205696, 0.1000000000000000056 ) ;
#20238 = VERTEX_POINT ( 'NONE', #190507 ) ;
#20239 = AXIS2_PLACEMENT_3D ( 'NONE', #203773, #9413, #225869 ) ;
#20240 = CIRCLE ( 'NONE', #249379, 0.1000000000000000472 ) ;
#20241 = EDGE_CURVE ( 'NONE', #217929, #97383, #88785, .T. ) ;
#20242 = AXIS2_PLACEMENT_3D ( 'NONE', #5432, #245369, #206233 ) ;
#20243 = ORIENTED_EDGE ( 'NONE', *, *, #171564, .T. ) ;
#20244 = AXIS2_PLACEMENT_3D ( 'NONE', #182348, #186190, #241036 ) ;
#20245 = VERTEX_POINT ( 'NONE', #187923 ) ;
#20246 = EDGE_LOOP ( 'NONE', ( #253256, #150628, #104101, #106708 ) ) ;
#20247 = CARTESIAN_POINT ( 'NONE',  ( -16.89268316805465986, 9.951721813253337601, -87.85575247854558256 ) ) ;
#20248 = CARTESIAN_POINT ( 'NONE',  ( -18.50000000000000000, 1.637172712981535883, -145.5821533654720383 ) ) ;
#20250 = EDGE_LOOP ( 'NONE', ( #177095, #83444, #220090, #105906 ) ) ;
#20249 = DIRECTION ( 'NONE',  ( 1.000000000000000000, 0.000000000000000000, 0.000000000000000000 ) ) ;
#20251 = DIRECTION ( 'NONE',  ( 0.000000000000000000, -7.429790795770647916E-15, 1.000000000000000000 ) ) ;
#20252 = CARTESIAN_POINT ( 'NONE',  ( -16.89268316805466341, 9.951721813253341153, -79.64424752145448849 ) ) ;
#20253 = DIRECTION ( 'NONE',  ( 1.000000000000000000, 0.000000000000000000, -0.000000000000000000 ) ) ;
#20254 = CARTESIAN_POINT ( 'NONE',  ( -16.87036670365549895, 10.08494996326643189, -79.55000000000005400 ) ) ;
#20255 = ADVANCED_FACE ( 'NONE', ( #32734 ), #28890, .F. ) ;
#20256 = CARTESIAN_POINT ( 'NONE',  ( 23.14999999999999858, 1.115600667400684642E-11, -136.0000000000000284 ) ) ;
#20258 = ORIENTED_EDGE ( 'NONE', *, *, #228080, .F. ) ;
#20257 = CARTESIAN_POINT ( 'NONE',  ( -23.15000000000000213, 64.35000000001176090, -76.53791325517833855 ) ) ;
#20260 = VERTEX_POINT ( 'NONE', #49683 ) ;
#20259 = CARTESIAN_POINT ( 'NONE',  ( -20.54999999999999716, 4.250000000011156409, -146.3500000000000227 ) ) ;
#20261 = DIRECTION ( 'NONE',  ( 2.557131231893037478E-16, 0.8660254037844420383, -0.4999999999999943379 ) ) ;
#20262 = ORIENTED_EDGE ( 'NONE', *, *, #16237, .T. ) ;
#20263 = EDGE_CURVE ( 'NONE', #17682, #221833, #240526, .T. ) ;
#20264 = AXIS2_PLACEMENT_3D ( 'NONE', #93225, #211916, #232762 ) ;
#20265 = ORIENTED_EDGE ( 'NONE', *, *, #108019, .F. ) ;
#20266 = CARTESIAN_POINT ( 'NONE',  ( -21.05000000000000071, 6.270085863700304962, -167.4651319969869121 ) ) ;
#20268 = CARTESIAN_POINT ( 'NONE',  ( -16.94445028196808778, 9.992063609708889516, -46.10733017841845793 ) ) ;
#20267 = CIRCLE ( 'NONE', #49293, 4.000000000000010658 ) ;
#20269 = CIRCLE ( 'NONE', #136763, 0.2000000000000057288 ) ;
#20270 = DIRECTION ( 'NONE',  ( 1.000000000000000000, 0.000000000000000000, 0.000000000000000000 ) ) ;
#20271 = FACE_OUTER_BOUND ( 'NONE', #142795, .T. ) ;
#20272 = EDGE_CURVE ( 'NONE', #134853, #77934, #78020, .T. ) ;
#20274 = LINE ( 'NONE', #257523, #163756 ) ;
#20273 = AXIS2_PLACEMENT_3D ( 'NONE', #127500, #204452, #46656 ) ;
#20275 = CARTESIAN_POINT ( 'NONE',  ( -18.50000000000000000, 7.633102355717365839, -241.5185714324494484 ) ) ;
#20276 = EDGE_CURVE ( 'NONE', #146298, #34114, #147556, .T. ) ;
#20277 = CARTESIAN_POINT ( 'NONE',  ( 21.05000000000000071, 4.850467289730772791, -146.0342674090016999 ) ) ;
#20278 = EDGE_LOOP ( 'NONE', ( #43849, #118825, #247847, #43837 ) ) ;
#20279 = EDGE_LOOP ( 'NONE', ( #139391, #76055, #1369 ) ) ;
#20280 = EDGE_CURVE ( 'NONE', #219487, #31299, #148967, .T. ) ;
#20281 = CARTESIAN_POINT ( 'NONE',  ( 20.94999999999999929, 70.37092869010230345, -198.1237041667535550 ) ) ;
#20282 = AXIS2_PLACEMENT_3D ( 'NONE', #219121, #40546, #199603 ) ;
#20283 = VERTEX_POINT ( 'NONE', #250448 ) ;
#20284 = CARTESIAN_POINT ( 'NONE',  ( 18.59999999999999787, 36.65892442174472876, -249.5511627012454596 ) ) ;
#20286 = CARTESIAN_POINT ( 'NONE',  ( -17.04295772865519965, 51.58824128325588987, -231.8781152409123933 ) ) ;
#20285 = AXIS2_PLACEMENT_3D ( 'NONE', #106386, #103817, #221209 ) ;
#20288 = EDGE_CURVE ( 'NONE', #141132, #223911, #61467, .T. ) ;
#20287 = CARTESIAN_POINT ( 'NONE',  ( -23.25000000000000000, 70.60814576644823148, -215.7631455941064189 ) ) ;
#20291 = ADVANCED_FACE ( 'NONE', ( #144458 ), #177999, .F. ) ;
#20290 = ADVANCED_FACE ( 'NONE', ( #71836 ), #92655, .F. ) ;
#20289 = CIRCLE ( 'NONE', #149476, 0.09999999999999910349 ) ;
#20292 = DIRECTION ( 'NONE',  ( 0.000000000000000000, 2.168404344971003346E-15, 1.000000000000000000 ) ) ;
#20293 = ORIENTED_EDGE ( 'NONE', *, *, #225350, .F. ) ;
#20294 = CARTESIAN_POINT ( 'NONE',  ( -18.59999999999999787, 77.16270174995064224, -195.4231074845243370 ) ) ;
#20295 = VERTEX_POINT ( 'NONE', #224008 ) ;
#20296 = CARTESIAN_POINT ( 'NONE',  ( -23.15000000000000213, 87.48912529308822172, -139.6231074845242688 ) ) ;
#20297 = ORIENTED_EDGE ( 'NONE', *, *, #153269, .F. ) ;
#20298 = AXIS2_PLACEMENT_3D ( 'NONE', #241701, #223403, #203850 ) ;
#20299 = VECTOR ( 'NONE', #267, 1000.000000000000000 ) ;
#20300 = LINE ( 'NONE', #219753, #148240 ) ;
#20301 = CARTESIAN_POINT ( 'NONE',  ( -16.87845715379269507, 9.957858113908168107, -113.1238006510589287 ) ) ;
#20302 = ORIENTED_EDGE ( 'NONE', *, *, #197449, .T. ) ;
#20303 = AXIS2_PLACEMENT_3D ( 'NONE', #67682, #207214, #191517 ) ;
#20305 = ORIENTED_EDGE ( 'NONE', *, *, #138840, .T. ) ;
#20304 = DIRECTION ( 'NONE',  ( 0.000000000000000000, 0.9126074666063660468, 0.4088369013363524762 ) ) ;
#20306 = EDGE_CURVE ( 'NONE', #125125, #28235, #16856, .T. ) ;
#20307 = DIRECTION ( 'NONE',  ( 0.000000000000000000, -0.8496786552930076786, -0.5273008465188218086 ) ) ;
#20308 = EDGE_CURVE ( 'NONE', #146049, #82068, #182275, .T. ) ;
#20309 = ORIENTED_EDGE ( 'NONE', *, *, #249303, .T. ) ;
#20310 = AXIS2_PLACEMENT_3D ( 'NONE', #77156, #184, #156736 ) ;
#20311 = CIRCLE ( 'NONE', #174478, 0.09999999999999939493 ) ;
#20312 = AXIS2_PLACEMENT_3D ( 'NONE', #61417, #194533, #123974 ) ;
#20313 = EDGE_CURVE ( 'NONE', #164805, #114552, #215574, .T. ) ;
#20314 = DIRECTION ( 'NONE',  ( 1.000000000000000000, 0.000000000000000000, 0.000000000000000000 ) ) ;
#20315 = ORIENTED_EDGE ( 'NONE', *, *, #110811, .T. ) ;
#20317 = CIRCLE ( 'NONE', #41174, 0.09999999999999939493 ) ;
#20316 = DIRECTION ( 'NONE',  ( 0.000000000000000000, 0.2617529984164915779, 0.9651348961777189706 ) ) ;
#20318 = CARTESIAN_POINT ( 'NONE',  ( 20.94999999999999574, 77.16270174994990327, -94.92310748452430857 ) ) ;
#20320 = ADVANCED_FACE ( 'NONE', ( #225277 ), #123649, .F. ) ;
#20319 = DIRECTION ( 'NONE',  ( 0.000000000000000000, -0.000000000000000000, -1.000000000000000000 ) ) ;
#20321 = DIRECTION ( 'NONE',  ( 0.000000000000000000, 0.1455152366551500653, 0.9893560106964507384 ) ) ;
#20322 = CARTESIAN_POINT ( 'NONE',  ( -18.59999999999999787, 76.00000000001195133, -103.0231074845243171 ) ) ;
#20323 = EDGE_CURVE ( 'NONE', #168899, #4548, #99030, .T. ) ;
#20324 = EDGE_LOOP ( 'NONE', ( #200368, #157836, #236761, #201796 ) ) ;
#20325 = CARTESIAN_POINT ( 'NONE',  ( -23.15000000000000213, 11.65000000001115588, -155.3500000000000227 ) ) ;
#20326 = CARTESIAN_POINT ( 'NONE',  ( 21.11833042828144258, 6.445644693866450226, -100.4928994909406015 ) ) ;
#20327 = CYLINDRICAL_SURFACE ( 'NONE', #51113, 0.09999999999999939493 ) ;
#20329 = VERTEX_POINT ( 'NONE', #127489 ) ;
#20328 = B_SPLINE_CURVE_WITH_KNOTS ( 'NONE', 3,
 ( #215463, #95520, #235045, #176372, #132085, #56377, #171264, #195929, #112529, #254566 ),
 .UNSPECIFIED., .F., .F.,
 ( 4, 3, 3, 4 ),
 ( 0.000000000000000000, 3.394313611811828588E-05, 6.779740500700482298E-05, 0.0001049857339142853951 ),
 .UNSPECIFIED. ) ;
#20330 = CARTESIAN_POINT ( 'NONE',  ( -23.15000000000000213, 0.000000000000000000, -31.50000000000000000 ) ) ;
#20332 = ORIENTED_EDGE ( 'NONE', *, *, #163347, .F. ) ;
#20331 = CIRCLE ( 'NONE', #228623, 4.049999999999998046 ) ;
#20334 = CIRCLE ( 'NONE', #253363, 0.09999999999999942268 ) ;
#20333 = DIRECTION ( 'NONE',  ( 3.265361837132813093E-16, -1.000000000000000000, -0.000000000000000000 ) ) ;
#20335 = ORIENTED_EDGE ( 'NONE', *, *, #66408, .F. ) ;
#20336 = VECTOR ( 'NONE', #148539, 1000.000000000000000 ) ;
#20337 = DIRECTION ( 'NONE',  ( 0.000000000000000000, 0.9998779222360102414, 0.01562499999996356907 ) ) ;
#20338 = CARTESIAN_POINT ( 'NONE',  ( -18.37013991200266361, 64.50025238380054304, -179.2300844740073273 ) ) ;
#20339 = ORIENTED_EDGE ( 'NONE', *, *, #52655, .F. ) ;
#20341 = ORIENTED_EDGE ( 'NONE', *, *, #30230, .F. ) ;
#20340 = FACE_OUTER_BOUND ( 'NONE', #192444, .T. ) ;
#20342 = EDGE_CURVE ( 'NONE', #91403, #256883, #136436, .T. ) ;
#20343 = DIRECTION ( 'NONE',  ( 0.000000000000000000, -0.8777080977375715243, 0.4791956752370512551 ) ) ;
#20344 = ORIENTED_EDGE ( 'NONE', *, *, #171742, .T. ) ;
#20345 = EDGE_CURVE ( 'NONE', #15058, #33224, #78203, .T. ) ;
#20346 = CARTESIAN_POINT ( 'NONE',  ( -21.04999999999994387, 67.75000000001118394, -43.82310748452479743 ) ) ;
#20347 = CIRCLE ( 'NONE', #128473, 7.791421356237313134 ) ;
#20348 = DIRECTION ( 'NONE',  ( 0.000000000000000000, 0.8103668758649577031, -0.5859227990963212784 ) ) ;
#20349 = AXIS2_PLACEMENT_3D ( 'NONE', #18046, #61016, #57149 ) ;
#20350 = ORIENTED_EDGE ( 'NONE', *, *, #170187, .T. ) ;
#20352 = ORIENTED_EDGE ( 'NONE', *, *, #131304, .T. ) ;
#20351 = EDGE_CURVE ( 'NONE', #55246, #254433, #190668, .T. ) ;
#20353 = CARTESIAN_POINT ( 'NONE',  ( 13.40000000000005898, 64.25000000001119815, -23.72310748452479601 ) ) ;
#20354 = CARTESIAN_POINT ( 'NONE',  ( 21.04999999999999716, 76.01681986839841443, -209.8305327040897055 ) ) ;
#20355 = VECTOR ( 'NONE', #29848, 1000.000000000000000 ) ;
#20356 = VERTEX_POINT ( 'NONE', #85753 ) ;
#20357 = DIRECTION ( 'NONE',  ( 0.000000000000000000, 0.8814952561688438326, -0.4721928772777330696 ) ) ;
#20358 = ORIENTED_EDGE ( 'NONE', *, *, #60303, .T. ) ;
#20359 = ORIENTED_EDGE ( 'NONE', *, *, #47897, .F. ) ;
#20360 = AXIS2_PLACEMENT_3D ( 'NONE', #100855, #121776, #180450 ) ;
#20361 = CARTESIAN_POINT ( 'NONE',  ( 20.94999999999999929, 87.48912529308822172, -139.4231074845242802 ) ) ;
#20362 = EDGE_CURVE ( 'NONE', #104038, #58341, #219846, .T. ) ;
#20364 = ORIENTED_EDGE ( 'NONE', *, *, #164826, .F. ) ;
#20363 = CARTESIAN_POINT ( 'NONE',  ( 20.94999999999999574, -11.48912529306490349, -137.0000000000000000 ) ) ;
#20365 = FACE_BOUND ( 'NONE', #134320, .T. ) ;
#20366 = AXIS2_PLACEMENT_3D ( 'NONE', #82017, #161620, #202006 ) ;
#20367 = LINE ( 'NONE', #21637, #244067 ) ;
#20368 = CIRCLE ( 'NONE', #32481, 11.70000000000000284 ) ;
#20369 = CARTESIAN_POINT ( 'NONE',  ( -16.87372397896795562, 63.02202630553817642, -213.6276555644750204 ) ) ;
#20370 = CIRCLE ( 'NONE', #83033, 0.09999999999998898659 ) ;
#20372 = CARTESIAN_POINT ( 'NONE',  ( -16.94445028196807002, 9.992063609708893068, -121.3926698215815918 ) ) ;
#20371 = CARTESIAN_POINT ( 'NONE',  ( -17.27223548802834685, 65.65460260866079523, -125.1567136637387421 ) ) ;
#20373 = DIRECTION ( 'NONE',  ( 0.000000000000000000, -1.000000000000000000, 0.000000000000000000 ) ) ;
#20374 = LINE ( 'NONE', #77732, #127758 ) ;
#20375 = CARTESIAN_POINT ( 'NONE',  ( 18.49505832270840600, -9.438028062771733673, -40.69847317489385574 ) ) ;
#20376 = EDGE_CURVE ( 'NONE', #189870, #121616, #165337, .T. ) ;
#20377 = DIRECTION ( 'NONE',  ( 1.000000000000000000, 0.000000000000000000, 0.000000000000000000 ) ) ;
#20378 = ORIENTED_EDGE ( 'NONE', *, *, #188646, .T. ) ;
#20380 = EDGE_LOOP ( 'NONE', ( #102293, #154345, #103467, #185918 ) ) ;
#20379 = LINE ( 'NONE', #223356, #125165 ) ;
#20381 = ORIENTED_EDGE ( 'NONE', *, *, #229317, .F. ) ;
#20382 = CARTESIAN_POINT ( 'NONE',  ( 21.87500000000000355, 63.35728523183471594, -212.8904317177587870 ) ) ;
#20383 = ORIENTED_EDGE ( 'NONE', *, *, #13159, .F. ) ;
#20384 = CARTESIAN_POINT ( 'NONE',  ( 20.95512820512820440, 8.876151316288115822, -8.558628995140949769 ) ) ;
#20385 = VECTOR ( 'NONE', #37255, 1000.000000000000114 ) ;
#20386 = VERTEX_POINT ( 'NONE', #84458 ) ;
#20387 = CARTESIAN_POINT ( 'NONE',  ( 21.14999999999999503, -11.64999999998883595, -136.9000000000000341 ) ) ;
#20389 = ORIENTED_EDGE ( 'NONE', *, *, #145031, .F. ) ;
#20388 = VERTEX_POINT ( 'NONE', #207030 ) ;
#20390 = ORIENTED_EDGE ( 'NONE', *, *, #75114, .F. ) ;
#20391 = VERTEX_POINT ( 'NONE', #222720 ) ;
#20392 = DIRECTION ( 'NONE',  ( -1.000000000000000000, 0.000000000000000000, 0.000000000000000000 ) ) ;
#20393 = FACE_OUTER_BOUND ( 'NONE', #209526, .T. ) ;
#20395 = ORIENTED_EDGE ( 'NONE', *, *, #94412, .T. ) ;
#20394 = CARTESIAN_POINT ( 'NONE',  ( 18.39999999999999858, -0.8467571797981052750, -242.2246066262668194 ) ) ;
#20396 = CARTESIAN_POINT ( 'NONE',  ( -21.14999999999999858, 78.57160958314655375, -238.9307242378722833 ) ) ;
#20398 = ORIENTED_EDGE ( 'NONE', *, *, #228667, .T. ) ;
#20397 = LINE ( 'NONE', #22977, #51836 ) ;
#20399 = CARTESIAN_POINT ( 'NONE',  ( -21.53551880898957904, 0.09896973458281840830, -60.21520223858371423 ) ) ;
#20400 = VERTEX_POINT ( 'NONE', #87051 ) ;
#20401 = CARTESIAN_POINT ( 'NONE',  ( 21.00000000000000000, 1.885425182446133885, -11.49641995933507843 ) ) ;
#20403 = ORIENTED_EDGE ( 'NONE', *, *, #140, .F. ) ;
#20402 = DIRECTION ( 'NONE',  ( -1.073024830501117528E-15, -0.8814952561688430555, 0.4721928772777346239 ) ) ;
#20404 = DIRECTION ( 'NONE',  ( 1.000000000000000000, -0.000000000000000000, -0.000000000000000000 ) ) ;
#20405 = CARTESIAN_POINT ( 'NONE',  ( -20.85000000000000142, -1.835859311432479268, -78.50443916879852679 ) ) ;
#20406 = EDGE_CURVE ( 'NONE', #108582, #247506, #166651, .T. ) ;
#20407 = VERTEX_POINT ( 'NONE', #246155 ) ;
#20410 = CARTESIAN_POINT ( 'NONE',  ( -16.88219499860498019, 44.13476732972441852, -235.2990254453784189 ) ) ;
#20409 = CIRCLE ( 'NONE', #203913, 0.09999999999999939493 ) ;
#20408 = CARTESIAN_POINT ( 'NONE',  ( 18.59999999999999787, -1.835341550213255957, -145.5551512925629822 ) ) ;
#20411 = CARTESIAN_POINT ( 'NONE',  ( -15.75000000000000711, 66.65000000001182912, -86.15883987690827439 ) ) ;
#20412 = AXIS2_PLACEMENT_3D ( 'NONE', #95521, #265, #158115 ) ;
#20413 = AXIS2_PLACEMENT_3D ( 'NONE', #45740, #104404, #26194 ) ;
#20414 = CARTESIAN_POINT ( 'NONE',  ( 18.44206774312973707, 85.49102735755248261, -163.3968799798263092 ) ) ;
#20415 = FACE_OUTER_BOUND ( 'NONE', #5411, .T. ) ;
#20416 = CARTESIAN_POINT ( 'NONE',  ( 20.09999999999999787, 66.25000000001264766, -194.2731074845244166 ) ) ;
#20417 = ORIENTED_EDGE ( 'NONE', *, *, #72059, .F. ) ;
#20418 = EDGE_LOOP ( 'NONE', ( #226591, #22217, #144584, #204682, #109154, #121090 ) ) ;
#20419 = VERTEX_POINT ( 'NONE', #67508 ) ;
#20420 = DIRECTION ( 'NONE',  ( -1.000000000000000000, -0.000000000000000000, -0.000000000000000000 ) ) ;
#20421 = ORIENTED_EDGE ( 'NONE', *, *, #151334, .F. ) ;
#20422 = CARTESIAN_POINT ( 'NONE',  ( -22.39999999999999858, 0.000000000000000000, 0.000000000000000000 ) ) ;
#20423 = ORIENTED_EDGE ( 'NONE', *, *, #157087, .T. ) ;
#20424 = ADVANCED_FACE ( 'NONE', ( #4938 ), #167930, .F. ) ;
#20425 = PLANE ( 'NONE',  #160792 ) ;
#20426 = CARTESIAN_POINT ( 'NONE',  ( 19.99999999999998934, 11.75000000001115907, -158.8500000000000227 ) ) ;
#20427 = EDGE_CURVE ( 'NONE', #172315, #206383, #144837, .T. ) ;
#20428 = AXIS2_PLACEMENT_3D ( 'NONE', #51737, #171748, #208290 ) ;
#20429 = AXIS2_PLACEMENT_3D ( 'NONE', #211271, #16930, #172193 ) ;
#20430 = ORIENTED_EDGE ( 'NONE', *, *, #162699, .T. ) ;
#20431 = TOROIDAL_SURFACE ( 'NONE', #228534, 0.2000000000000000111, 0.1000000000000000056 ) ;
#20432 = DIRECTION ( 'NONE',  ( 1.000000000000000000, 0.000000000000000000, 0.000000000000000000 ) ) ;
#20433 = ADVANCED_FACE ( 'NONE', ( #44103 ), #132627, .F. ) ;
#20434 = ORIENTED_EDGE ( 'NONE', *, *, #229921, .T. ) ;
#20435 = CIRCLE ( 'NONE', #174410, 7.800000000000001599 ) ;
#20436 = ORIENTED_EDGE ( 'NONE', *, *, #205266, .F. ) ;
#20437 = VERTEX_POINT ( 'NONE', #188737 ) ;
#20438 = EDGE_CURVE ( 'NONE', #5729, #83103, #212675, .T. ) ;
#20439 = LINE ( 'NONE', #201618, #254453 ) ;
#20440 = CARTESIAN_POINT ( 'NONE',  ( -21.05000000000000071, 87.39257802171833589, -200.4491579046923277 ) ) ;
#20441 = CARTESIAN_POINT ( 'NONE',  ( 13.99999999999999822, 9.850000000011137402, -50.24999999999999289 ) ) ;
#20443 = ADVANCED_FACE ( 'NONE', ( #15258 ), #233028, .T. ) ;
#20442 = DIRECTION ( 'NONE',  ( 1.000000000000000000, -0.000000000000000000, -0.000000000000000000 ) ) ;
#20444 = DIRECTION ( 'NONE',  ( -0.8660254037843878594, 0.000000000000000000, -0.5000000000000880407 ) ) ;
#20445 =( BOUNDED_CURVE ( )  B_SPLINE_CURVE ( 3, ( #191354, #72689, #152227, #193903 ),
 .UNSPECIFIED., .F., .F. ) 
 B_SPLINE_CURVE_WITH_KNOTS ( ( 4, 4 ),
 ( 4.712388980384689674, 6.283185307179586232 ),
 .UNSPECIFIED. ) 
 CURVE ( )  GEOMETRIC_REPRESENTATION_ITEM ( )  RATIONAL_B_SPLINE_CURVE ( ( 1.000000000000000000, 0.8047378541243649375, 0.8047378541243649375, 1.000000000000000000 ) ) 
 REPRESENTATION_ITEM ( '' )  );
#20446 = CARTESIAN_POINT ( 'NONE',  ( -18.59999999999999787, -11.65000000000000036, 29.89999999999999858 ) ) ;
#20447 = FACE_OUTER_BOUND ( 'NONE', #160786, .T. ) ;
#20449 = ORIENTED_EDGE ( 'NONE', *, *, #240835, .F. ) ;
#20448 = CARTESIAN_POINT ( 'NONE',  ( 22.47071067811865319, 68.27992525551390202, -103.1221999392269737 ) ) ;
#20450 = CARTESIAN_POINT ( 'NONE',  ( -16.94389599338512298, 12.44527457180727836, -211.1927369019190621 ) ) ;
#20451 = ORIENTED_EDGE ( 'NONE', *, *, #144833, .F. ) ;
#20452 = ADVANCED_FACE ( 'NONE', ( #190031 ), #191343, .T. ) ;
#20453 = CARTESIAN_POINT ( 'NONE',  ( -21.14999999999999858, 6.540656951712397138, -167.5999999999999659 ) ) ;
#20454 = ORIENTED_EDGE ( 'NONE', *, *, #45954, .T. ) ;
#20455 = ORIENTED_EDGE ( 'NONE', *, *, #84131, .F. ) ;
#20456 = DIRECTION ( 'NONE',  ( 1.000000000000000000, -0.000000000000000000, 0.000000000000000000 ) ) ;
#20457 = PLANE ( 'NONE',  #176863 ) ;
#20458 = CARTESIAN_POINT ( 'NONE',  ( -0.8999999999999991340, -9.650000000000003908, 23.40000000000000213 ) ) ;
#20459 = ORIENTED_EDGE ( 'NONE', *, *, #39512, .T. ) ;
#20460 = ADVANCED_FACE ( 'NONE', ( #158318 ), #193890, .F. ) ;
#20461 = AXIS2_PLACEMENT_3D ( 'NONE', #233322, #62370, #239722 ) ;
#20462 = AXIS2_PLACEMENT_3D ( 'NONE', #131813, #110973, #230945 ) ;
#20463 = FACE_OUTER_BOUND ( 'NONE', #189315, .T. ) ;
#20464 = VERTEX_POINT ( 'NONE', #229165 ) ;
#20465 = ORIENTED_EDGE ( 'NONE', *, *, #114546, .F. ) ;
#20466 = DIRECTION ( 'NONE',  ( 4.408576920032446739E-17, 0.3896596508880098009, 0.9209589331071360574 ) ) ;
#20467 = VERTEX_POINT ( 'NONE', #59143 ) ;
#20468 = DIRECTION ( 'NONE',  ( 1.000000000000000000, 0.000000000000000000, 0.000000000000000000 ) ) ;
#20469 = ORIENTED_EDGE ( 'NONE', *, *, #189107, .T. ) ;
#20471 = DIRECTION ( 'NONE',  ( 0.000000000000000000, 0.1335171055202867274, -0.9910465087640866200 ) ) ;
#20470 = CIRCLE ( 'NONE', #157871, 11.65000000000000036 ) ;
#20472 = CARTESIAN_POINT ( 'NONE',  ( -23.15000000000000213, 71.65000000001187175, -90.67310748452433700 ) ) ;
#20473 = PLANE ( 'NONE',  #92618 ) ;
#20474 = ORIENTED_EDGE ( 'NONE', *, *, #71904, .T. ) ;
#20475 = ADVANCED_FACE ( 'NONE', ( #114345 ), #72676, .T. ) ;
#20476 = FACE_OUTER_BOUND ( 'NONE', #184758, .T. ) ;
#20477 = SPHERICAL_SURFACE ( 'NONE', #33287, 0.1000000000000000056 ) ;
#20478 = CARTESIAN_POINT ( 'NONE',  ( -22.45372860728439690, 26.02113247230217752, -254.3004129941882638 ) ) ;
#20479 = VECTOR ( 'NONE', #177934, 1000.000000000000114 ) ;
#20480 = AXIS2_PLACEMENT_3D ( 'NONE', #215490, #218035, #158138 ) ;
#20481 = ORIENTED_EDGE ( 'NONE', *, *, #245197, .T. ) ;
#20482 = ADVANCED_FACE ( 'NONE', ( #54360 ), #203106, .F. ) ;
#20484 = ORIENTED_EDGE ( 'NONE', *, *, #74976, .T. ) ;
#20483 = DIRECTION ( 'NONE',  ( -1.000000000000000000, -7.304098846218134667E-16, 0.000000000000000000 ) ) ;
#20485 = ORIENTED_EDGE ( 'NONE', *, *, #15958, .F. ) ;
#20486 = FACE_OUTER_BOUND ( 'NONE', #188413, .T. ) ;
#20487 = LINE ( 'NONE', #175716, #250170 ) ;
#20488 = CARTESIAN_POINT ( 'NONE',  ( -21.05000000000000071, 16.44800918141279311, -240.8068063186265135 ) ) ;
#20489 = AXIS2_PLACEMENT_3D ( 'NONE', #172493, #73371, #233712 ) ;
#20490 = DIRECTION ( 'NONE',  ( -0.000000000000000000, -0.1350103645451945777, 0.9908441862701590219 ) ) ;
#20491 = FACE_OUTER_BOUND ( 'NONE', #166229, .T. ) ;
#20492 = VECTOR ( 'NONE', #131473, 1000.000000000000000 ) ;
#20493 = VERTEX_POINT ( 'NONE', #251268 ) ;
#20494 = CARTESIAN_POINT ( 'NONE',  ( -18.59999999999999787, 76.00000000001170974, -69.52310748452431710 ) ) ;
#20495 = FACE_OUTER_BOUND ( 'NONE', #60586, .T. ) ;
#20496 = CARTESIAN_POINT ( 'NONE',  ( -18.39999999999999858, 77.43243075322048696, -241.6948671442531520 ) ) ;
#20497 = DIRECTION ( 'NONE',  ( -1.000000000000000000, 1.836970198721029934E-16, 1.282749433769087757E-30 ) ) ;
#20498 = CARTESIAN_POINT ( 'NONE',  ( -22.39999999999999858, 76.00000000001199396, -109.2731074845243171 ) ) ;
#20499 = EDGE_CURVE ( 'NONE', #227362, #117472, #50488, .T. ) ;
#20500 = AXIS2_PLACEMENT_3D ( 'NONE', #162836, #4994, #63705 ) ;
#20501 = AXIS2_PLACEMENT_3D ( 'NONE', #145890, #121251, #105455 ) ;
#20503 = VERTEX_POINT ( 'NONE', #174365 ) ;
#20502 = VECTOR ( 'NONE', #20099, 1000.000000000000000 ) ;
#20504 = ORIENTED_EDGE ( 'NONE', *, *, #223855, .T. ) ;
#20505 = CARTESIAN_POINT ( 'NONE',  ( -21.05000000000000071, 74.73821383144729680, -161.9366085209788935 ) ) ;
#20506 = AXIS2_PLACEMENT_3D ( 'NONE', #4952, #81915, #64949 ) ;
#20507 = DIRECTION ( 'NONE',  ( 0.000000000000000000, -1.000000000000000000, -6.982962677686265922E-15 ) ) ;
#20508 = FACE_OUTER_BOUND ( 'NONE', #104315, .T. ) ;
#20509 = DIRECTION ( 'NONE',  ( 0.000000000000000000, 0.000000000000000000, -1.000000000000000000 ) ) ;
#20510 = VECTOR ( 'NONE', #28449, 1000.000000000000000 ) ;
#20511 = EDGE_CURVE ( 'NONE', #216880, #138911, #218228, .T. ) ;
#20512 = ORIENTED_EDGE ( 'NONE', *, *, #65515, .T. ) ;
#20513 = DIRECTION ( 'NONE',  ( -0.000000000000000000, -0.8660254037844411501, -0.4999999999999956701 ) ) ;
#20514 = DIRECTION ( 'NONE',  ( 0.000000000000000000, 0.9126074666063770380, 0.4088369013363281068 ) ) ;
#20515 = ADVANCED_FACE ( 'NONE', ( #152216 ), #170522, .T. ) ;
#20517 = EDGE_CURVE ( 'NONE', #154671, #175678, #161630, .T. ) ;
#20516 = DIRECTION ( 'NONE',  ( -1.000000000000000000, 0.000000000000000000, -0.000000000000000000 ) ) ;
#20518 = PRODUCT_DEFINITION_SHAPE ( 'NONE', 'NONE',  #258130 ) ;
#20519 = CARTESIAN_POINT ( 'NONE',  ( -20.54999999999999716, 7.250000000011155521, -88.15000000000004832 ) ) ;
#20520 = EDGE_CURVE ( 'NONE', #182465, #172315, #103139, .T. ) ;
#20521 = ORIENTED_EDGE ( 'NONE', *, *, #17399, .F. ) ;
#20522 = DIRECTION ( 'NONE',  ( 1.000000000000000000, -0.000000000000000000, -0.000000000000000000 ) ) ;
#20523 = EDGE_CURVE ( 'NONE', #61601, #241398, #107431, .T. ) ;
#20524 = ORIENTED_EDGE ( 'NONE', *, *, #203450, .T. ) ;
#20525 = CARTESIAN_POINT ( 'NONE',  ( -23.15000000000000213, 64.35000000001222986, -148.6731074845244507 ) ) ;
#20526 = DIRECTION ( 'NONE',  ( 1.713247197920696616E-14, -0.9876197685951263461, 0.1568667991644794590 ) ) ;
#20527 = CYLINDRICAL_SURFACE ( 'NONE', #7606, 0.1000000000000124678 ) ;
#20528 = DIRECTION ( 'NONE',  ( -1.000000000000000000, 0.000000000000000000, 0.000000000000000000 ) ) ;
#20530 = AXIS2_PLACEMENT_3D ( 'NONE', #49321, #166742, #67598 ) ;
#20529 = LINE ( 'NONE', #179602, #177870 ) ;
#20531 = DIRECTION ( 'NONE',  ( -1.000000000000000000, 0.000000000000000000, 0.000000000000000000 ) ) ;
#20532 = CARTESIAN_POINT ( 'NONE',  ( 18.59999999999997655, 36.65892442174935439, -249.5511627012433848 ) ) ;
#20533 = FACE_OUTER_BOUND ( 'NONE', #169753, .T. ) ;
#20534 = AXIS2_PLACEMENT_3D ( 'NONE', #117440, #136989, #215250 ) ;
#20535 = CARTESIAN_POINT ( 'NONE',  ( -23.15000000000000213, 2.000000000011154189, -120.7753780772379315 ) ) ;
#20536 = DIRECTION ( 'NONE',  ( 0.000000000000000000, -1.000000000000000000, -0.000000000000000000 ) ) ;
#20537 = AXIS2_PLACEMENT_3D ( 'NONE', #135315, #178337, #234422 ) ;
#20538 = CARTESIAN_POINT ( 'NONE',  ( 18.59999999999999076, 11.65000000001115943, -122.2500000000000284 ) ) ;
#20539 = CARTESIAN_POINT ( 'NONE',  ( 20.85000000000000142, 1.115600667400684642E-11, -67.00000000000000000 ) ) ;
#20540 = MANIFOLD_SOLID_BREP ( 'Stock-MAS-200-1', #94959 ) ;
#20541 = DIRECTION ( 'NONE',  ( 0.000000000000000000, 0.8068669527897506244, 0.5907332058516622242 ) ) ;
#20542 = AXIS2_PLACEMENT_3D ( 'NONE', #94473, #171492, #93194 ) ;
#20543 = EDGE_CURVE ( 'NONE', #104459, #169470, #124018, .T. ) ;
#20544 = VERTEX_POINT ( 'NONE', #141197 ) ;
#20545 =( BOUNDED_SURFACE ( )  B_SPLINE_SURFACE ( 3, 2, ( 
 ( #47732, #46451, #145557 ),
 ( #106413, #206826, #184683 ),
 ( #242089, #161301, #103850 ),
 ( #66028, #166453, #28225 ) ),
 .UNSPECIFIED., .F., .F., .T. ) 
 B_SPLINE_SURFACE_WITH_KNOTS ( ( 4, 4 ),
 ( 3, 3 ),
 ( -3.469446951953614189E-18, 0.001979672783031543714 ),
 ( 0.000000000000000000, 1.000000000000000000 ),
 .UNSPECIFIED. ) 
 GEOMETRIC_REPRESENTATION_ITEM ( )  RATIONAL_B_SPLINE_SURFACE ( (
 ( 1.000000000000000000, 0.7103081912008198939, 1.000000000000000000),
 ( 1.000000000000000000, 0.7104998333558710799, 1.000000000000000000),
 ( 1.000000000000000000, 0.7107238315755350921, 1.000000000000000000),
 ( 1.000000000000000000, 0.7110073749539379540, 1.000000000000000000) ) ) 
 REPRESENTATION_ITEM ( '' )  SURFACE ( )  );
#20546 = DIRECTION ( 'NONE',  ( 0.000000000000000000, 0.000000000000000000, -1.000000000000000000 ) ) ;
#20547 = DIRECTION ( 'NONE',  ( -0.000000000000000000, -0.4721928772777343464, -0.8814952561688431665 ) ) ;
#20548 = CARTESIAN_POINT ( 'NONE',  ( 20.54374330479337374, 10.50501031423420351, -41.22568363488881715 ) ) ;
#20549 = EDGE_CURVE ( 'NONE', #2421, #30032, #140755, .T. ) ;
#20550 = ADVANCED_FACE ( 'NONE', ( #175233 ), #20066, .T. ) ;
#20551 = ORIENTED_EDGE ( 'NONE', *, *, #58726, .F. ) ;
#20552 = CYLINDRICAL_SURFACE ( 'NONE', #84744, 0.1000000000000028644 ) ;
#20553 = CIRCLE ( 'NONE', #228828, 0.09999999999999277522 ) ;
#20554 = DIRECTION ( 'NONE',  ( -0.000000000000000000, -6.982962677686266711E-15, 1.000000000000000000 ) ) ;
#20555 = AXIS2_PLACEMENT_3D ( 'NONE', #17148, #15871, #131933 ) ;
#20556 = ORIENTED_EDGE ( 'NONE', *, *, #188861, .F. ) ;
#20557 = CARTESIAN_POINT ( 'NONE',  ( 20.94999999999999929, 77.16412189325305349, -95.10825939895268277 ) ) ;
#20558 = DIRECTION ( 'NONE',  ( 1.000000000000000000, -0.000000000000000000, -0.000000000000000000 ) ) ;
#20559 = EDGE_CURVE ( 'NONE', #35027, #227982, #186562, .T. ) ;
#20560 = B_SPLINE_CURVE_WITH_KNOTS ( 'NONE', 3,
 ( #202376, #4163, #244056, #245364, #164545, #101956, #66722, #84957, #125416, #141129 ),
 .UNSPECIFIED., .F., .F.,
 ( 4, 2, 2, 2, 4 ),
 ( 0.000000000000000000, 0.0003916577441626381485, 0.0005874866162439739466, 0.0006854010522846671347, 0.0007833154883253604312 ),
 .UNSPECIFIED. ) ;
#20561 = VERTEX_POINT ( 'NONE', #96889 ) ;
#20562 = TOROIDAL_SURFACE ( 'NONE', #149562, 0.2000000000000000111, 0.1000000000000000056 ) ;
#20563 = ORIENTED_EDGE ( 'NONE', *, *, #234296, .T. ) ;
#20564 = DIRECTION ( 'NONE',  ( 0.000000000000000000, 0.8814952561688428334, -0.4721928772777350125 ) ) ;
#20565 = VERTEX_POINT ( 'NONE', #257235 ) ;
#20566 = DIRECTION ( 'NONE',  ( 0.000000000000000000, 1.000000000000000000, 0.000000000000000000 ) ) ;
#20567 = DIRECTION ( 'NONE',  ( -1.000000000000000000, 0.000000000000000000, 0.000000000000000000 ) ) ;
#20568 = CARTESIAN_POINT ( 'NONE',  ( 21.11927991906888025, 34.01425264317992969, -243.6699334763191871 ) ) ;
#20569 = DIRECTION ( 'NONE',  ( -1.000000000000000000, 0.000000000000000000, 0.000000000000000000 ) ) ;
#20570 = PLANE ( 'NONE',  #5837 ) ;
#20571 = EDGE_CURVE ( 'NONE', #104346, #67428, #74155, .T. ) ;
#20572 = CARTESIAN_POINT ( 'NONE',  ( -20.64999999999999858, -8.999999999988844479, -191.6060308773475356 ) ) ;
#20573 = CYLINDRICAL_SURFACE ( 'NONE', #251066, 0.09999999999999939493 ) ;
#20574 = CARTESIAN_POINT ( 'NONE',  ( 21.07016717457008426, 1.556953976783223004, -230.7479980709940435 ) ) ;
#20576 = ORIENTED_EDGE ( 'NONE', *, *, #25672, .T. ) ;
#20575 = CARTESIAN_POINT ( 'NONE',  ( 18.39999999999999858, 87.08727414655709254, -199.6327537731849873 ) ) ;
#20577 = EDGE_LOOP ( 'NONE', ( #245375, #24396 ) ) ;
#20579 = CARTESIAN_POINT ( 'NONE',  ( -22.39999999999999858, 76.00000000001276135, -215.1726782920691505 ) ) ;
#20578 = VECTOR ( 'NONE', #31177, 1000.000000000000000 ) ;
#20581 = ORIENTED_EDGE ( 'NONE', *, *, #125864, .F. ) ;
#20580 = CARTESIAN_POINT ( 'NONE',  ( -16.87998658237717819, 60.99527856349479293, -220.8355367335571771 ) ) ;
#20582 = ORIENTED_EDGE ( 'NONE', *, *, #66136, .F. ) ;
#20583 = CARTESIAN_POINT ( 'NONE',  ( -20.54999999999999716, 4.250000000011156409, -112.7500000000000284 ) ) ;
#20584 = CYLINDRICAL_SURFACE ( 'NONE', #209434, 0.09999999999998898659 ) ;
#20585 = DIRECTION ( 'NONE',  ( 1.000000000000000000, 0.000000000000000000, 0.000000000000000000 ) ) ;
#20586 = FACE_OUTER_BOUND ( 'NONE', #33348, .T. ) ;
#20587 = FACE_OUTER_BOUND ( 'NONE', #150803, .T. ) ;
#20588 = B_SPLINE_CURVE_WITH_KNOTS ( 'NONE', 3,
 ( #188350, #5835, #227462, #164932, #249619, #65827, #28024, #170121, #224887, #107521, #150519, #205321, #207936, #187088, #8437, #87937, #9703, #26732, #106218, #185780, #7130, #86648, #173979, #113941, #31873, #33171 ),
 .UNSPECIFIED., .F., .F.,
 ( 4, 2, 2, 2, 2, 2, 2, 2, 2, 2, 2, 2, 4 ),
 ( 0.005476422646581341307, 0.006160811967703542710, 0.006845201288825743247, 0.007187395949386851321, 0.007529590609947959395, 0.007871785270509067470, 0.008213979931070175544, 0.008556174591631281884, 0.008898369252192389958, 0.009240563912753498033, 0.009582758573314606107, 0.01026714789443682226, 0.01095153721555903667 ),
 .UNSPECIFIED. ) ;
#20589 = EDGE_CURVE ( 'NONE', #158228, #192257, #44669, .T. ) ;
#20590 = CYLINDRICAL_SURFACE ( 'NONE', #181195, 0.1000000000000124678 ) ;
#20591 = VECTOR ( 'NONE', #22799, 1000.000000000000000 ) ;
#20592 = ORIENTED_EDGE ( 'NONE', *, *, #249436, .T. ) ;
#20593 = ORIENTED_EDGE ( 'NONE', *, *, #172732, .T. ) ;
#20594 = AXIS2_PLACEMENT_3D ( 'NONE', #41591, #97659, #160258 ) ;
#20595 = EDGE_CURVE ( 'NONE', #35963, #143544, #181618, .T. ) ;
#20596 = CARTESIAN_POINT ( 'NONE',  ( 23.15000000000000213, -9.599999999999999645, -23.60603087734755690 ) ) ;
#20597 = CIRCLE ( 'NONE', #157999, 0.4000000000000114575 ) ;
#20598 = VECTOR ( 'NONE', #32322, 1000.000000000000000 ) ;
#20599 = EDGE_LOOP ( 'NONE', ( #193845, #18145, #137465 ) ) ;
#20600 = CARTESIAN_POINT ( 'NONE',  ( -22.39999999999999858, 68.20922040163854660, -103.1231074845243540 ) ) ;
#20601 = ORIENTED_EDGE ( 'NONE', *, *, #155138, .T. ) ;
#20602 = CARTESIAN_POINT ( 'NONE',  ( -16.84419801905645997, 14.15485412938328302, -219.2360291138972741 ) ) ;
#20603 = EDGE_CURVE ( 'NONE', #194521, #252230, #240702, .T. ) ;
#20604 = CIRCLE ( 'NONE', #87206, 0.09999999999999939493 ) ;
#20605 = EDGE_CURVE ( 'NONE', #128403, #32139, #82457, .T. ) ;
#20606 = CARTESIAN_POINT ( 'NONE',  ( -14.45422546970484667, 49.62720671425053354, -233.3859273903071312 ) ) ;
#20607 = FACE_OUTER_BOUND ( 'NONE', #146843, .T. ) ;
#20608 = CARTESIAN_POINT ( 'NONE',  ( 23.15000000000000213, 69.16514130714681130, -247.7543978865853660 ) ) ;
#20609 = CARTESIAN_POINT ( 'NONE',  ( -20.94999999999999929, 68.97833521811203639, -132.6895420826271277 ) ) ;
#20610 = ORIENTED_EDGE ( 'NONE', *, *, #209931, .F. ) ;
#20611 = LINE ( 'NONE', #156287, #8701 ) ;
#20613 = CARTESIAN_POINT ( 'NONE',  ( 18.49999999999999289, 43.18640298906419162, -245.2812653309023574 ) ) ;
#20612 = CIRCLE ( 'NONE', #53347, 7.720710678118680725 ) ;
#20614 = CARTESIAN_POINT ( 'NONE',  ( 21.05000000000000071, 77.16270174995064224, -195.6231074845243540 ) ) ;
#20616 = AXIS2_PLACEMENT_3D ( 'NONE', #95917, #157223, #257512 ) ;
#20615 = CARTESIAN_POINT ( 'NONE',  ( 20.94999999999999929, 8.776282895303632259, -179.6499999999999773 ) ) ;
#20617 = CARTESIAN_POINT ( 'NONE',  ( 18.59999999999999076, 69.01799029515542827, -99.32695536626805222 ) ) ;
#20618 = VERTEX_POINT ( 'NONE', #68077 ) ;
#20619 = CARTESIAN_POINT ( 'NONE',  ( -20.85000000000000142, 79.19526988099229925, -196.1889237952725296 ) ) ;
#20620 = ORIENTED_EDGE ( 'NONE', *, *, #63866, .T. ) ;
#20622 = ORIENTED_EDGE ( 'NONE', *, *, #94417, .F. ) ;
#20621 = DIRECTION ( 'NONE',  ( 0.000000000000000000, 0.4930308989874718772, 0.8700118002898612479 ) ) ;
#20624 = ADVANCED_FACE ( 'NONE', ( #221982 ), #115816, .T. ) ;
#20623 = AXIS2_PLACEMENT_3D ( 'NONE', #65314, #41931, #238826 ) ;
#20625 = DIRECTION ( 'NONE',  ( 1.000000000000000000, 0.000000000000000000, 0.000000000000000000 ) ) ;
#20626 = ADVANCED_FACE ( 'NONE', ( #83744 ), #103331, .F. ) ;
#20627 = DIRECTION ( 'NONE',  ( 1.000000000000000000, -0.000000000000000000, -0.000000000000000000 ) ) ;
#20628 = ORIENTED_EDGE ( 'NONE', *, *, #251635, .T. ) ;
#20629 = CARTESIAN_POINT ( 'NONE',  ( 18.48197441911518624, 85.51795479471604722, -129.6328958423155768 ) ) ;
#20630 = CYLINDRICAL_SURFACE ( 'NONE', #78006, 0.09999999999999939493 ) ;
#20631 = LINE ( 'NONE', #243503, #55185 ) ;
#20633 = ORIENTED_EDGE ( 'NONE', *, *, #186865, .F. ) ;
#20632 = CARTESIAN_POINT ( 'NONE',  ( 21.04999999999998650, 6.650000000011155876, -146.2500000000000284 ) ) ;
#20634 = DIRECTION ( 'NONE',  ( 1.000000000000000000, -0.000000000000000000, -0.000000000000000000 ) ) ;
#20635 = EDGE_CURVE ( 'NONE', #255163, #235252, #36736, .T. ) ;
#20636 = ORIENTED_EDGE ( 'NONE', *, *, #186307, .F. ) ;
#20638 = EDGE_CURVE ( 'NONE', #121226, #28056, #165920, .T. ) ;
#20637 = FACE_OUTER_BOUND ( 'NONE', #114303, .T. ) ;
#20639 = CARTESIAN_POINT ( 'NONE',  ( 22.00356870141986576, 60.22995210369071373, -233.9563068168734787 ) ) ;
#20640 = DIRECTION ( 'NONE',  ( 1.000000000000000000, -0.000000000000000000, -0.000000000000000000 ) ) ;
#20641 = TOROIDAL_SURFACE ( 'NONE', #220545, 0.4000000000000015210, 0.1000000000000000056 ) ;
#20642 = ORIENTED_EDGE ( 'NONE', *, *, #76503, .F. ) ;
#20643 = CARTESIAN_POINT ( 'NONE',  ( -16.86379686415369861, 66.02478224075913715, -157.4564973736146953 ) ) ;
#20644 = ORIENTED_EDGE ( 'NONE', *, *, #24521, .F. ) ;
#20645 = CARTESIAN_POINT ( 'NONE',  ( 21.98333005346336577, 65.30108822512866595, -242.9721039335941555 ) ) ;
#20646 = CARTESIAN_POINT ( 'NONE',  ( -20.94999999999999929, 11.75000000001115552, -40.51480577065400013 ) ) ;
#20647 = CYLINDRICAL_SURFACE ( 'NONE', #126766, 12.87499999999999822 ) ;
#20648 = CIRCLE ( 'NONE', #257899, 0.1999999999999881317 ) ;
#20649 = VERTEX_POINT ( 'NONE', #142466 ) ;
#20650 = EDGE_CURVE ( 'NONE', #14587, #211151, #203736, .T. ) ;
#20651 = CARTESIAN_POINT ( 'NONE',  ( 21.05933563467872460, 22.94152016742551226, -230.0368372691647778 ) ) ;
#20652 = DIRECTION ( 'NONE',  ( 0.000000000000000000, -6.308085367188393199E-16, -1.000000000000000000 ) ) ;
#20653 = CARTESIAN_POINT ( 'NONE',  ( -20.85000000106584750, 64.25000000001250555, -176.8676028280509911 ) ) ;
#20654 = ORIENTED_EDGE ( 'NONE', *, *, #148612, .F. ) ;
#20655 = EDGE_CURVE ( 'NONE', #158566, #5080, #136642, .T. ) ;
#20656 = DIRECTION ( 'NONE',  ( -1.000000000000000000, 3.265361837132813093E-16, 2.280189983783949500E-30 ) ) ;
#20657 = CARTESIAN_POINT ( 'NONE',  ( -18.59999999999999787, 77.16412189325330928, -128.7082593989527197 ) ) ;
#20658 = ORIENTED_EDGE ( 'NONE', *, *, #184123, .F. ) ;
#20659 = LINE ( 'NONE', #157627, #61313 ) ;
#20660 = AXIS2_PLACEMENT_3D ( 'NONE', #14449, #10580, #93949 ) ;
#20661 = VERTEX_POINT ( 'NONE', #122928 ) ;
#20662 = VECTOR ( 'NONE', #67998, 1000.000000000000000 ) ;
#20663 = FACE_OUTER_BOUND ( 'NONE', #183629, .T. ) ;
#20664 = ORIENTED_EDGE ( 'NONE', *, *, #160129, .F. ) ;
#20666 = ORIENTED_EDGE ( 'NONE', *, *, #212530, .F. ) ;
#20665 = FACE_OUTER_BOUND ( 'NONE', #39601, .T. ) ;
#20667 = ADVANCED_FACE ( 'NONE', ( #6817 ), #163336, .F. ) ;
#20668 = AXIS2_PLACEMENT_3D ( 'NONE', #40370, #198116, #1180 ) ;
#20669 = AXIS2_PLACEMENT_3D ( 'NONE', #101273, #180876, #182160 ) ;
#20672 = ORIENTED_EDGE ( 'NONE', *, *, #52577, .F. ) ;
#20671 = ORIENTED_EDGE ( 'NONE', *, *, #250125, .T. ) ;
#20670 = CARTESIAN_POINT ( 'NONE',  ( -23.25000000000000000, 77.14957036958755054, -95.20719500002232394 ) ) ;
#20673 = CARTESIAN_POINT ( 'NONE',  ( -23.25000000000000000, 1.115600667400684642E-11, -134.0000000000000000 ) ) ;
#20674 = CARTESIAN_POINT ( 'NONE',  ( -21.14250536705909411, 1.115652671863510454E-11, -160.9818278231192039 ) ) ;
#20675 = DIRECTION ( 'NONE',  ( 0.000000000000000000, -0.9915357197604792727, 0.1298341882520475943 ) ) ;
#20676 = CARTESIAN_POINT ( 'NONE',  ( -16.80621392010911208, 12.41483980993488245, -211.2832333842498826 ) ) ;
#20677 = CARTESIAN_POINT ( 'NONE',  ( -18.59999999999999787, -1.162701749938009677, -8.099999999999999645 ) ) ;
#20678 = DIRECTION ( 'NONE',  ( -0.000000000000000000, 1.000000000000000000, -0.000000000000000000 ) ) ;
#20679 = CIRCLE ( 'NONE', #49878, 11.80000000000000782 ) ;
#20680 = DIRECTION ( 'NONE',  ( 1.000000000000000000, 1.394253735153569469E-16, 2.602809386958778209E-16 ) ) ;
#20682 = CARTESIAN_POINT ( 'NONE',  ( 20.73486653747088582, 7.250000000011182166, -76.25000000000004263 ) ) ;
#20681 = DIRECTION ( 'NONE',  ( 0.000000000000000000, -0.9126074666063622720, -0.4088369013363611360 ) ) ;
#20683 = VECTOR ( 'NONE', #79181, 1000.000000000000000 ) ;
#20684 = AXIS2_PLACEMENT_3D ( 'NONE', #257062, #176319, #198423 ) ;
#20685 = ORIENTED_EDGE ( 'NONE', *, *, #92253, .T. ) ;
#20686 = AXIS2_PLACEMENT_3D ( 'NONE', #99888, #101152, #165032 ) ;
#20688 = ORIENTED_EDGE ( 'NONE', *, *, #222485, .F. ) ;
#20687 = AXIS2_PLACEMENT_3D ( 'NONE', #160096, #239618, #240900 ) ;
#20689 = CARTESIAN_POINT ( 'NONE',  ( 18.59999999999999076, 65.50857864377445594, -78.27310748452438816 ) ) ;
#20691 = ORIENTED_EDGE ( 'NONE', *, *, #153245, .F. ) ;
#20690 = CARTESIAN_POINT ( 'NONE',  ( -18.59999999999999787, 6.846123162363745074, -204.7377262668498190 ) ) ;
#20692 = CARTESIAN_POINT ( 'NONE',  ( 21.05000000000000071, 64.25000000001175238, -76.53791325517833855 ) ) ;
#20693 = VERTEX_POINT ( 'NONE', #145033 ) ;
#20694 = AXIS2_PLACEMENT_3D ( 'NONE', #256368, #77778, #157372 ) ;
#20695 = CARTESIAN_POINT ( 'NONE',  ( 22.47007471830798053, 7.720710651937614522, -100.5000000000000426 ) ) ;
#20696 = ORIENTED_EDGE ( 'NONE', *, *, #151468, .T. ) ;
#20697 = CARTESIAN_POINT ( 'NONE',  ( 21.14999999999999858, 67.21339244341248786, -191.2731074845244166 ) ) ;
#20698 = ORIENTED_EDGE ( 'NONE', *, *, #220569, .T. ) ;
#20699 = CARTESIAN_POINT ( 'NONE',  ( -16.93935632781549572, 66.01526950028672047, -82.13344673581407562 ) ) ;
#20700 =( GEOMETRIC_REPRESENTATION_CONTEXT ( 3 ) GLOBAL_UNCERTAINTY_ASSIGNED_CONTEXT ( ( #200530 ) ) GLOBAL_UNIT_ASSIGNED_CONTEXT ( ( #205219, #47431, #106112 ) ) REPRESENTATION_CONTEXT ( 'NONE', 'WORKASPACE' ) );
#20702 = ORIENTED_EDGE ( 'NONE', *, *, #212262, .T. ) ;
#20701 = EDGE_LOOP ( 'NONE', ( #100535, #184863, #15323, #202214 ) ) ;
#20703 = ORIENTED_EDGE ( 'NONE', *, *, #131224, .T. ) ;
#20704 = CARTESIAN_POINT ( 'NONE',  ( -23.25000000000000000, 4.350000000011156054, -79.25000000000004263 ) ) ;
#20705 = ORIENTED_EDGE ( 'NONE', *, *, #73646, .T. ) ;
#20706 = ORIENTED_EDGE ( 'NONE', *, *, #127167, .T. ) ;
#20707 = CARTESIAN_POINT ( 'NONE',  ( 18.59999999999999432, 2.838478681111047841, -208.5693404029859437 ) ) ;
#20709 = ORIENTED_EDGE ( 'NONE', *, *, #227856, .F. ) ;
#20708 = DIRECTION ( 'NONE',  ( -0.000000000000000000, -0.1335171055202864221, -0.9910465087640866200 ) ) ;
#20711 = CARTESIAN_POINT ( 'NONE',  ( 23.14999999999999858, 68.82573846827003194, -239.4142956262433302 ) ) ;
#20710 = CARTESIAN_POINT ( 'NONE',  ( -23.15000000000000213, 76.00000000001170974, -69.52310748452431710 ) ) ;
#20712 = CARTESIAN_POINT ( 'NONE',  ( -20.54999999999999716, 4.350000000011156054, -79.35000000000005116 ) ) ;
#20713 = FACE_OUTER_BOUND ( 'NONE', #80382, .T. ) ;
#20714 = LINE ( 'NONE', #160235, #209289 ) ;
#20715 = VERTEX_POINT ( 'NONE', #202454 ) ;
#20716 = TOROIDAL_SURFACE ( 'NONE', #208154, 0.2000000000000000111, 0.1000000000000000056 ) ;
#20717 = ORIENTED_EDGE ( 'NONE', *, *, #94085, .T. ) ;
#20718 = DIRECTION ( 'NONE',  ( 0.000000000000000000, 0.000000000000000000, -1.000000000000000000 ) ) ;
#20719 = CARTESIAN_POINT ( 'NONE',  ( 21.14999999999999858, 1.115600667400684642E-11, -134.1000000000000227 ) ) ;
#20720 = FACE_OUTER_BOUND ( 'NONE', #190278, .T. ) ;
#20721 = EDGE_CURVE ( 'NONE', #100115, #192577, #69499, .T. ) ;
#20722 = VECTOR ( 'NONE', #251097, 1000.000000000000000 ) ;
#20723 = ORIENTED_EDGE ( 'NONE', *, *, #256177, .T. ) ;
#20724 = DIRECTION ( 'NONE',  ( 1.186688945009010077E-16, -1.000000000000000000, -0.000000000000000000 ) ) ;
#20725 = VECTOR ( 'NONE', #120211, 1000.000000000000000 ) ;
#20726 = DIRECTION ( 'NONE',  ( 0.000000000000000000, 0.8814952561688437216, -0.4721928772777334582 ) ) ;
#20727 = DIRECTION ( 'NONE',  ( 0.000000000000000000, -0.05616704890742720696, 0.9984213852963240710 ) ) ;
#20728 = EDGE_LOOP ( 'NONE', ( #146061, #119987, #108509, #216571 ) ) ;
#20729 = VERTEX_POINT ( 'NONE', #185461 ) ;
#20730 = CARTESIAN_POINT ( 'NONE',  ( -16.97683809663752186, 66.15000000001188596, -89.62074346632789457 ) ) ;
#20731 = CARTESIAN_POINT ( 'NONE',  ( -21.14999999999994174, 77.36076146337680370, -43.99645795275012006 ) ) ;
#20732 = EDGE_LOOP ( 'NONE', ( #78906, #26119, #97741, #47134 ) ) ;
#20733 = LINE ( 'NONE', #100219, #239106 ) ;
#20734 = EDGE_LOOP ( 'NONE', ( #131252, #4945, #154119, #219070 ) ) ;
#20735 = LINE ( 'NONE', #140655, #156335 ) ;
#20736 = CARTESIAN_POINT ( 'NONE',  ( -20.54999999999999716, 2.000000000011154189, -80.22462192276213955 ) ) ;
#20738 = CARTESIAN_POINT ( 'NONE',  ( -20.94999999999999929, 68.00417547777207972, -224.2303273613012777 ) ) ;
#20737 = CARTESIAN_POINT ( 'NONE',  ( -18.59999999999999787, 31.44980407958351165, -233.5445995079518866 ) ) ;
#20739 = ADVANCED_FACE ( 'NONE', ( #86319 ), #184161, .T. ) ;
#20740 = CARTESIAN_POINT ( 'NONE',  ( 18.59999999999997655, -1.164121893241208960, -41.41484808557160591 ) ) ;
#20741 = CARTESIAN_POINT ( 'NONE',  ( 20.94999999999999929, 87.65000000001190017, -103.0231074845242318 ) ) ;
#20742 = CIRCLE ( 'NONE', #216529, 0.09999999999999939493 ) ;
#20743 = EDGE_LOOP ( 'NONE', ( #65157, #109101, #81618, #202039, #77739 ) ) ;
#20744 = DIRECTION ( 'NONE',  ( 1.000000000000000000, 0.000000000000000000, 0.000000000000000000 ) ) ;
#20745 = TOROIDAL_SURFACE ( 'NONE', #220812, 0.4000000000000010214, 0.1000000000000000056 ) ;
#20747 = ORIENTED_EDGE ( 'NONE', *, *, #29972, .T. ) ;
#20746 = ORIENTED_EDGE ( 'NONE', *, *, #126822, .T. ) ;
#20748 = ORIENTED_EDGE ( 'NONE', *, *, #170138, .T. ) ;
#20749 = EDGE_CURVE ( 'NONE', #3592, #189995, #111710, .T. ) ;
#20750 = CARTESIAN_POINT ( 'NONE',  ( -23.15000000000000213, 11.75000000001115552, -134.0000000000000000 ) ) ;
#20751 = CARTESIAN_POINT ( 'NONE',  ( -18.39999999999999858, -7.785976468740645196, -209.8926132507865816 ) ) ;
#20752 = DIRECTION ( 'NONE',  ( -1.000000000000000000, 0.000000000000000000, 0.000000000000000000 ) ) ;
#20754 = ADVANCED_FACE ( 'NONE', ( #206311 ), #192854, .F. ) ;
#20753 = CARTESIAN_POINT ( 'NONE',  ( -21.05000000000000071, -11.39257802169451139, -164.4260504201680817 ) ) ;
#20755 = CARTESIAN_POINT ( 'NONE',  ( -21.05000000000000071, 70.15000000001235492, -159.8906102602464330 ) ) ;
#20757 = CARTESIAN_POINT ( 'NONE',  ( -15.52965525596987995, 66.62446189796385454, -87.15323160353352705 ) ) ;
#20756 = CARTESIAN_POINT ( 'NONE',  ( 20.84451136049667852, 10.62014191480694159, -7.493924559529303586 ) ) ;
#20758 = VERTEX_POINT ( 'NONE', #194148 ) ;
#20760 = CARTESIAN_POINT ( 'NONE',  ( -21.05000000000000071, 87.48912529308817909, -133.4231074845242233 ) ) ;
#20759 = B_SPLINE_CURVE_WITH_KNOTS ( 'NONE', 3,
 ( #178638, #196876, #255518, #177359, #13278, #70705, #211470, #193206, #14578, #94075, #92789, #32875, #233613, #253151, #212766, #34154 ),
 .UNSPECIFIED., .F., .F.,
 ( 4, 3, 3, 3, 3, 4 ),
 ( 0.000000000000000000, 2.372700795693551704E-05, 5.739057815866934116E-05, 9.073899019179910389E-05, 0.0001243544287365693814, 0.0001585386695601165850 ),
 .UNSPECIFIED. ) ;
#20761 = ORIENTED_EDGE ( 'NONE', *, *, #186557, .T. ) ;
#20762 = EDGE_CURVE ( 'NONE', #73682, #121226, #95016, .T. ) ;
#20763 = CARTESIAN_POINT ( 'NONE',  ( -18.59999999999999787, 64.25000000001199396, -115.1731074845243796 ) ) ;
#20764 = ORIENTED_EDGE ( 'NONE', *, *, #52047, .F. ) ;
#20765 = EDGE_LOOP ( 'NONE', ( #98316, #231911, #253830 ) ) ;
#20766 = DIRECTION ( 'NONE',  ( 0.000000000000000000, 0.000000000000000000, -1.000000000000000000 ) ) ;
#20767 = FACE_OUTER_BOUND ( 'NONE', #4378, .T. ) ;
#20768 = FACE_OUTER_BOUND ( 'NONE', #201104, .T. ) ;
#20769 = CARTESIAN_POINT ( 'NONE',  ( 14.77516762759922031, 9.436674251854004325, -82.17686193099926584 ) ) ;
#20770 = AXIS2_PLACEMENT_3D ( 'NONE', #88194, #51632, #32132 ) ;
#20771 = EDGE_CURVE ( 'NONE', #61614, #193155, #153455, .T. ) ;
#20772 = CIRCLE ( 'NONE', #154072, 3.899999999999987477 ) ;
#20773 = CARTESIAN_POINT ( 'NONE',  ( 20.94999999999999929, 43.12265650693429819, -239.4782534460092052 ) ) ;
#20774 = VERTEX_POINT ( 'NONE', #191592 ) ;
#20776 = ORIENTED_EDGE ( 'NONE', *, *, #112561, .T. ) ;
#20775 = EDGE_CURVE ( 'NONE', #161116, #137320, #195125, .T. ) ;
#20777 = CARTESIAN_POINT ( 'NONE',  ( 18.59999999999999787, 5.899999999999947065, -10.21909976465641456 ) ) ;
#20778 = VERTEX_POINT ( 'NONE', #134136 ) ;
#20779 = DIRECTION ( 'NONE',  ( 0.000000000000000000, -0.9126074666063773710, -0.4088369013363274962 ) ) ;
#20780 = CARTESIAN_POINT ( 'NONE',  ( -20.64999999999999858, 4.349999999999999645, -21.15000000000000213 ) ) ;
#20781 = DIRECTION ( 'NONE',  ( 1.000000000000000000, 3.265361837132813093E-16, -0.000000000000000000 ) ) ;
#20782 = CARTESIAN_POINT ( 'NONE',  ( -17.01825945287482966, 65.95000000001188312, -90.37310748452438247 ) ) ;
#20784 = CARTESIAN_POINT ( 'NONE',  ( -20.94999999999999929, 87.65000000001143121, -36.02310748452423894 ) ) ;
#20783 = DIRECTION ( 'NONE',  ( 0.000000000000000000, -0.9446535261619708468, 0.3280696808755038663 ) ) ;
#20785 = DIRECTION ( 'NONE',  ( 0.000000000000000000, 0.8814952561688430555, -0.4721928772777346239 ) ) ;
#20786 = ADVANCED_FACE ( 'NONE', ( #235807 ), #224131, .T. ) ;
#20787 = DIRECTION ( 'NONE',  ( 0.000000000000000000, 0.000000000000000000, -1.000000000000000000 ) ) ;
#20788 = VECTOR ( 'NONE', #5746, 1000.000000000000000 ) ;
#20789 = B_SPLINE_CURVE_WITH_KNOTS ( 'NONE', 3,
 ( #59898, #119936, #199457, #258075, #97732, #254251, #74392, #198145, #195610, #117333 ),
 .UNSPECIFIED., .F., .F.,
 ( 4, 3, 3, 4 ),
 ( -2.000561356219677529E-06, 0.000000000000000000, 1.787822682429502760E-05, 4.206475347090109142E-05 ),
 .UNSPECIFIED. ) ;
#20790 = CIRCLE ( 'NONE', #124817, 0.1999999999999996503 ) ;
#20791 = CARTESIAN_POINT ( 'NONE',  ( -18.69999999999999929, 6.841561409100513025, 9.675512259591560138 ) ) ;
#20792 = CIRCLE ( 'NONE', #128922, 2.099999999999995204 ) ;
#20793 = AXIS2_PLACEMENT_3D ( 'NONE', #128837, #71440, #187540 ) ;
#20794 = DIRECTION ( 'NONE',  ( 1.000000000000000000, 0.000000000000000000, 0.000000000000000000 ) ) ;
#20795 = EDGE_LOOP ( 'NONE', ( #52094, #134652, #183435, #229665 ) ) ;
#20796 = VECTOR ( 'NONE', #97416, 1000.000000000000000 ) ;
#20797 = CARTESIAN_POINT ( 'NONE',  ( 20.95265033839679347, 10.51225083247831371, -41.06576375602996620 ) ) ;
#20798 = VERTEX_POINT ( 'NONE', #93739 ) ;
#20799 = APPLICATION_CONTEXT ( 'automotive_design' ) ;
#20800 = CARTESIAN_POINT ( 'NONE',  ( 21.05000000000000071, 11.60000000001116227, -93.57179676972454274 ) ) ;
#20801 = CARTESIAN_POINT ( 'NONE',  ( -21.30740335185486245, 0.09893452578700702438, -93.94334207797203362 ) ) ;
#20802 = CARTESIAN_POINT ( 'NONE',  ( 21.05000000000000071, 71.00000000001199396, -115.4283735034374274 ) ) ;
#20803 = AXIS2_PLACEMENT_3D ( 'NONE', #4720, #144230, #226328 ) ;
#20804 = ORIENTED_EDGE ( 'NONE', *, *, #205044, .F. ) ;
#20806 = CIRCLE ( 'NONE', #245645, 0.2000000000000057288 ) ;
#20805 = CARTESIAN_POINT ( 'NONE',  ( 18.59999999999999076, 6.550000000011156231, -121.7500000000000426 ) ) ;
#20807 = LINE ( 'NONE', #79454, #198024 ) ;
#20808 = DIRECTION ( 'NONE',  ( 0.000000000000000000, -0.9876197685951263461, 0.1568667991644794590 ) ) ;
#20809 = VECTOR ( 'NONE', #218604, 1000.000000000000000 ) ;
#20810 = DIRECTION ( 'NONE',  ( -1.000000000000000000, 0.000000000000000000, 0.000000000000000000 ) ) ;
#20811 = CARTESIAN_POINT ( 'NONE',  ( -16.93826681692523550, 10.01142872029886810, -121.4454584673594724 ) ) ;
#20812 = LINE ( 'NONE', #256775, #219556 ) ;
#20813 = EDGE_CURVE ( 'NONE', #204139, #173018, #203298, .T. ) ;
#20814 = EDGE_CURVE ( 'NONE', #57307, #172354, #212422, .T. ) ;
#20815 = EDGE_LOOP ( 'NONE', ( #234589, #87668, #63025, #43144 ) ) ;
#20816 = CARTESIAN_POINT ( 'NONE',  ( 21.14999999999999858, 69.45934304831089889, -136.5231074845243313 ) ) ;
#20818 = ORIENTED_EDGE ( 'NONE', *, *, #75800, .F. ) ;
#20817 = DIRECTION ( 'NONE',  ( -1.000000000000000000, 7.304098846218134667E-16, 4.217023435051625732E-16 ) ) ;
#20819 = FACE_OUTER_BOUND ( 'NONE', #222852, .T. ) ;
#20820 = CARTESIAN_POINT ( 'NONE',  ( -21.07928932188134041, 69.67148334361908724, -170.1220026301787982 ) ) ;
#20822 = EDGE_CURVE ( 'NONE', #73853, #216955, #249283, .T. ) ;
#20821 = DIRECTION ( 'NONE',  ( 1.000000000000000000, 0.000000000000000000, 0.000000000000000000 ) ) ;
#20823 = ADVANCED_FACE ( 'NONE', ( #37638 ), #15513, .T. ) ;
#20824 = ORIENTED_EDGE ( 'NONE', *, *, #249384, .T. ) ;
#20825 = DIRECTION ( 'NONE',  ( 0.000000000000000000, -0.9908441862701605762, 0.1350103645451835310 ) ) ;
#20826 = SHAPE_DEFINITION_REPRESENTATION ( #193165, #133560 ) ;
#20827 = DIRECTION ( 'NONE',  ( 0.000000000000000000, 0.9126074666063545004, 0.4088369013363783999 ) ) ;
#20828 = ADVANCED_FACE ( 'NONE', ( #74218 ), #57054, .T. ) ;
#20829 = ORIENTED_EDGE ( 'NONE', *, *, #125804, .T. ) ;
#20830 = CARTESIAN_POINT ( 'NONE',  ( 23.14999999999999503, 59.16775194334852017, -221.0793150863668473 ) ) ;
#20831 = DIRECTION ( 'NONE',  ( 0.000000000000000000, 0.000000000000000000, -1.000000000000000000 ) ) ;
#20832 = CONICAL_SURFACE ( 'NONE', #166577, 4.000000000000000000, 0.7853981633974489451 ) ;
#20833 = ADVANCED_FACE ( 'NONE', ( #214965 ), #178441, .T. ) ;
#20835 = EDGE_CURVE ( 'NONE', #5474, #198025, #103975, .T. ) ;
#20834 = EDGE_CURVE ( 'NONE', #177357, #210178, #116016, .T. ) ;
#20836 = VERTEX_POINT ( 'NONE', #38914 ) ;
#20837 = EDGE_CURVE ( 'NONE', #232467, #258086, #45066, .T. ) ;
#20838 = AXIS2_PLACEMENT_3D ( 'NONE', #247801, #229535, #48314 ) ;
#20839 = VERTEX_POINT ( 'NONE', #100125 ) ;
#20840 = CARTESIAN_POINT ( 'NONE',  ( 22.39999999999999503, 64.25000000001215028, -136.6231074845243825 ) ) ;
#20841 = VECTOR ( 'NONE', #178387, 1000.000000000000000 ) ;
#20842 = CARTESIAN_POINT ( 'NONE',  ( 23.25000000000000000, 87.65000000001144542, -39.12310748452424747 ) ) ;
#20843 = DIRECTION ( 'NONE',  ( -0.000000000000000000, 0.000000000000000000, -1.000000000000000000 ) ) ;
#20844 = FACE_OUTER_BOUND ( 'NONE', #169277, .T. ) ;
#20845 = ADVANCED_FACE ( 'NONE', ( #140551 ), #139254, .T. ) ;
#20846 = DIRECTION ( 'NONE',  ( -1.000000000000000000, -1.836970198721029934E-16, 0.000000000000000000 ) ) ;
#20847 = FACE_OUTER_BOUND ( 'NONE', #56797, .T. ) ;
#20849 = FACE_OUTER_BOUND ( 'NONE', #123880, .T. ) ;
#20848 = CARTESIAN_POINT ( 'NONE',  ( 18.59999999999999076, 65.50857864377445594, -78.27310748452438816 ) ) ;
#20850 = DIRECTION ( 'NONE',  ( 1.000000000000000000, 0.000000000000000000, 0.000000000000000000 ) ) ;
#20852 = EDGE_CURVE ( 'NONE', #104663, #115992, #28564, .T. ) ;
#20851 = DIRECTION ( 'NONE',  ( -1.000000000000000000, -0.000000000000000000, -0.000000000000000000 ) ) ;
#20853 = CARTESIAN_POINT ( 'NONE',  ( -22.39999999999999858, 0.1000000000111554016, -67.00000000000004263 ) ) ;
#20855 = EDGE_CURVE ( 'NONE', #139316, #232566, #79288, .T. ) ;
#20854 = CYLINDRICAL_SURFACE ( 'NONE', #38993, 0.09999999999998898659 ) ;
#20856 = CIRCLE ( 'NONE', #141619, 0.2000000000000057288 ) ;
#20857 = ORIENTED_EDGE ( 'NONE', *, *, #193902, .T. ) ;
#20858 = EDGE_LOOP ( 'NONE', ( #102424, #24838, #211377, #184603 ) ) ;
#20859 = VECTOR ( 'NONE', #119664, 1000.000000000000114 ) ;
#20860 = DIRECTION ( 'NONE',  ( 0.000000000000000000, 0.2617529984164856383, 0.9651348961777204138 ) ) ;
#20862 = CARTESIAN_POINT ( 'NONE',  ( 21.11747605621531321, 67.22129199451970294, -191.2785443147346598 ) ) ;
#20861 = CARTESIAN_POINT ( 'NONE',  ( -21.05000000000000071, 69.74218538953583391, -103.1208977758331571 ) ) ;
#20863 = EDGE_CURVE ( 'NONE', #48905, #236070, #3554, .T. ) ;
#20864 = AXIS2_PLACEMENT_3D ( 'NONE', #245601, #166094, #9541 ) ;
#20865 = CARTESIAN_POINT ( 'NONE',  ( 22.39999999999999858, 68.20922040163900135, -170.1231074845244109 ) ) ;
#20866 = CARTESIAN_POINT ( 'NONE',  ( -20.94999999999999929, 76.00000000001190870, -103.0231074845243029 ) ) ;
#20867 = DIRECTION ( 'NONE',  ( 0.000000000000000000, 8.881784197001252323E-16, -1.000000000000000000 ) ) ;
#20868 = ADVANCED_FACE ( 'NONE', ( #238376 ), #83699, .F. ) ;
#20869 = ORIENTED_EDGE ( 'NONE', *, *, #128913, .T. ) ;
#20870 = ADVANCED_FACE ( 'NONE', ( #203101 ), #23214, .F. ) ;
#20871 = AXIS2_PLACEMENT_3D ( 'NONE', #188822, #209675, #205817 ) ;
#20872 = DIRECTION ( 'NONE',  ( 0.000000000000000000, -7.026728003956695223E-15, 1.000000000000000000 ) ) ;
#20873 = AXIS2_PLACEMENT_3D ( 'NONE', #108413, #67996, #246623 ) ;
#20874 = ORIENTED_EDGE ( 'NONE', *, *, #134045, .T. ) ;
#20875 = FACE_OUTER_BOUND ( 'NONE', #34750, .T. ) ;
#20876 = ORIENTED_EDGE ( 'NONE', *, *, #249074, .F. ) ;
#20877 = CARTESIAN_POINT ( 'NONE',  ( -18.40000000000000213, 14.17280543801757986, -210.8598471598932349 ) ) ;
#20878 = CIRCLE ( 'NONE', #95833, 0.09999999999999939493 ) ;
#20879 = CIRCLE ( 'NONE', #170753, 0.1000000000000028644 ) ;
#20881 = AXIS2_PLACEMENT_3D ( 'NONE', #9212, #167041, #88725 ) ;
#20880 = CARTESIAN_POINT ( 'NONE',  ( -20.94999999999999929, -1.360870587192041681, -8.072997927090961312 ) ) ;
#20882 = CIRCLE ( 'NONE', #120833, 0.1000000000000052097 ) ;
#20883 = VECTOR ( 'NONE', #73841, 1000.000000000000000 ) ;
#20884 = ORIENTED_EDGE ( 'NONE', *, *, #253906, .T. ) ;
#20885 = FACE_OUTER_BOUND ( 'NONE', #64900, .T. ) ;
#20886 = CIRCLE ( 'NONE', #74681, 0.2000000000000048683 ) ;
#20887 = VERTEX_POINT ( 'NONE', #217516 ) ;
#20888 = CARTESIAN_POINT ( 'NONE',  ( 20.94999999999999929, 1.115600667400684642E-11, -200.9999999999999432 ) ) ;
#20889 = CARTESIAN_POINT ( 'NONE',  ( 18.79999999999999005, 1.212568896937007645, -8.000000000000000000 ) ) ;
#20890 = CARTESIAN_POINT ( 'NONE',  ( 20.94999999999999929, -11.29603075032412995, -36.54789915966387071 ) ) ;
#20891 = CARTESIAN_POINT ( 'NONE',  ( -23.25000000000000000, 11.65000000001115588, -21.75000000000000355 ) ) ;
#20892 = DIRECTION ( 'NONE',  ( -1.073024830501117725E-15, -6.982962677686266711E-15, 1.000000000000000000 ) ) ;
#20894 = DIRECTION ( 'NONE',  ( 0.000000000000000000, -0.8700118002898322711, 0.4930308989875231140 ) ) ;
#20893 = DIRECTION ( 'NONE',  ( 0.000000000000000000, 0.000000000000000000, 1.000000000000000000 ) ) ;
#20895 = FACE_OUTER_BOUND ( 'NONE', #244866, .T. ) ;
#20897 = ORIENTED_EDGE ( 'NONE', *, *, #188315, .F. ) ;
#20896 = CARTESIAN_POINT ( 'NONE',  ( 20.13684514580103624, 66.50414460725946242, -128.3800757988350938 ) ) ;
#20899 = CARTESIAN_POINT ( 'NONE',  ( 21.05000000000000071, 10.72371710470752149, -12.15000000000000036 ) ) ;
#20898 = CARTESIAN_POINT ( 'NONE',  ( -16.88005004766534967, 9.950100503332199864, -188.3503361119487352 ) ) ;
#20900 = ORIENTED_EDGE ( 'NONE', *, *, #32023, .F. ) ;
#20901 = VERTEX_POINT ( 'NONE', #160159 ) ;
#20902 = ORIENTED_EDGE ( 'NONE', *, *, #167567, .T. ) ;
#20903 = CARTESIAN_POINT ( 'NONE',  ( -23.15000000000000213, 11.75000000001115552, -67.00000000000004263 ) ) ;
#20904 = FACE_OUTER_BOUND ( 'NONE', #183304, .T. ) ;
#20905 = DIRECTION ( 'NONE',  ( -1.000000000000000000, 3.265361837132813093E-16, 2.280189983783949500E-30 ) ) ;
#20906 = ORIENTED_EDGE ( 'NONE', *, *, #255019, .T. ) ;
#20907 = DIRECTION ( 'NONE',  ( 0.000000000000000000, 0.000000000000000000, 1.000000000000000000 ) ) ;
#20908 = PLANE ( 'NONE',  #201567 ) ;
#20909 = PLANE ( 'NONE',  #6546 ) ;
#20910 = CARTESIAN_POINT ( 'NONE',  ( -16.94878442675512886, 9.991729103002160883, -154.8882195756378906 ) ) ;
#20911 = CIRCLE ( 'NONE', #141674, 0.1000000000000054040 ) ;
#20912 = CARTESIAN_POINT ( 'NONE',  ( -23.15000000000000213, 76.00000000001244871, -170.0231074845243597 ) ) ;
#20913 = EDGE_CURVE ( 'NONE', #210178, #204053, #61835, .T. ) ;
#20914 = AXIS2_PLACEMENT_3D ( 'NONE', #139591, #161774, #240010 ) ;
#20915 = CARTESIAN_POINT ( 'NONE',  ( 21.13498764882293557, 69.50438185653827361, -136.5247638792556586 ) ) ;
#20916 = ORIENTED_EDGE ( 'NONE', *, *, #41763, .T. ) ;
#20917 = ORIENTED_EDGE ( 'NONE', *, *, #152364, .T. ) ;
#20918 = EDGE_CURVE ( 'NONE', #5568, #691, #161809, .T. ) ;
#20919 = CARTESIAN_POINT ( 'NONE',  ( 20.94999999999999574, 6.550000000011159784, -76.84382208968318650 ) ) ;
#20920 = CIRCLE ( 'NONE', #174885, 0.1000000000000017958 ) ;
#20921 = ORIENTED_EDGE ( 'NONE', *, *, #9159, .F. ) ;
#20922 = CARTESIAN_POINT ( 'NONE',  ( 18.59999999999999076, 1.835341550235567887, -78.55515129256302487 ) ) ;
#20923 = EDGE_LOOP ( 'NONE', ( #176936, #14481, #21869, #236083 ) ) ;
#20924 = FACE_OUTER_BOUND ( 'NONE', #6926, .T. ) ;
#20925 = EDGE_CURVE ( 'NONE', #243110, #1714, #137809, .T. ) ;
#20926 = EDGE_CURVE ( 'NONE', #233793, #55301, #147037, .T. ) ;
#20927 = DIRECTION ( 'NONE',  ( -1.000000000000000000, 0.000000000000000000, 0.000000000000000000 ) ) ;
#20928 = DIRECTION ( 'NONE',  ( -1.000000000000000000, 0.000000000000000000, 0.000000000000000000 ) ) ;
#20929 = DIRECTION ( 'NONE',  ( 1.000000000000000000, 0.000000000000000000, 0.000000000000000000 ) ) ;
#20930 = TOROIDAL_SURFACE ( 'NONE', #154225, 0.2000000000000000111, 0.1000000000000000056 ) ;
#20931 = VECTOR ( 'NONE', #169193, 1000.000000000000114 ) ;
#20932 = DIRECTION ( 'NONE',  ( -1.000000000000000000, -0.000000000000000000, -0.000000000000000000 ) ) ;
#20933 = B_SPLINE_CURVE_WITH_KNOTS ( 'NONE', 3,
 ( #68033, #151442, #69332, #87577, #131856, #48462, #111012, #167172 ),
 .UNSPECIFIED., .F., .F.,
 ( 4, 2, 2, 4 ),
 ( 0.000000000000000000, 0.0001881495939909109049, 0.0002822243909863736758, 0.0003762991879818364466 ),
 .UNSPECIFIED. ) ;
#20934 = DIRECTION ( 'NONE',  ( -0.7071067811865475727, -0.7071067811865475727, 0.000000000000000000 ) ) ;
#20935 = DIRECTION ( 'NONE',  ( -1.000000000000000000, 0.000000000000000000, 0.000000000000000000 ) ) ;
#20936 = VERTEX_POINT ( 'NONE', #243510 ) ;
#20939 = CARTESIAN_POINT ( 'NONE',  ( 21.05000000000000071, 64.40000000001194280, -109.9513107147998880 ) ) ;
#20938 = PLANE ( 'NONE',  #228886 ) ;
#20937 = VECTOR ( 'NONE', #176294, 1000.000000000000000 ) ;
#20940 = VERTEX_POINT ( 'NONE', #29636 ) ;
#20943 = ORIENTED_EDGE ( 'NONE', *, *, #7982, .T. ) ;
#20942 = DIRECTION ( 'NONE',  ( -1.000000000000000000, 0.000000000000000000, 0.000000000000000000 ) ) ;
#20941 = CARTESIAN_POINT ( 'NONE',  ( 21.05000000000000071, 1.115600667400684642E-11, -100.6000000000000227 ) ) ;
#20944 = EDGE_CURVE ( 'NONE', #118817, #26573, #99217, .T. ) ;
#20945 = VECTOR ( 'NONE', #184005, 1000.000000000000000 ) ;
#20946 = VERTEX_POINT ( 'NONE', #8760 ) ;
#20947 = CARTESIAN_POINT ( 'NONE',  ( -18.59999999999999787, 1.162701749949165642, -108.6000000000000227 ) ) ;
#20948 = EDGE_CURVE ( 'NONE', #171479, #108576, #149329, .T. ) ;
#20949 = DIRECTION ( 'NONE',  ( 0.000000000000000000, 0.000000000000000000, -1.000000000000000000 ) ) ;
#20950 = DIRECTION ( 'NONE',  ( 0.000000000000000000, 0.000000000000000000, 1.000000000000000000 ) ) ;
#20951 = CARTESIAN_POINT ( 'NONE',  ( 23.40000000000005187, 76.00000000001119815, -40.17310748452479174 ) ) ;
#20952 = ORIENTED_EDGE ( 'NONE', *, *, #173549, .F. ) ;
#20953 = CARTESIAN_POINT ( 'NONE',  ( -18.60000000000000142, -8.250000000000005329, 33.00000000000000000 ) ) ;
#20954 = DIRECTION ( 'NONE',  ( -2.602085213965226419E-14, -0.2128009952263604232, 0.9770955615653316162 ) ) ;
#20956 = DIRECTION ( 'NONE',  ( -1.000000000000000000, -0.000000000000000000, -0.000000000000000000 ) ) ;
#20955 = FACE_OUTER_BOUND ( 'NONE', #234031, .T. ) ;
#20958 = ORIENTED_EDGE ( 'NONE', *, *, #187590, .F. ) ;
#20957 = DIRECTION ( 'NONE',  ( 1.000000000000000000, 0.000000000000000000, 0.000000000000000000 ) ) ;
#20959 = EDGE_CURVE ( 'NONE', #154671, #256377, #211694, .T. ) ;
#20960 = TOROIDAL_SURFACE ( 'NONE', #233333, 0.2000000000000000111, 0.1000000000000000056 ) ;
#20961 = VECTOR ( 'NONE', #112025, 1000.000000000000000 ) ;
#20962 = ORIENTED_EDGE ( 'NONE', *, *, #126176, .T. ) ;
#20963 = EDGE_CURVE ( 'NONE', #208880, #247553, #165905, .T. ) ;
#20964 = CARTESIAN_POINT ( 'NONE',  ( -22.47071067811865319, 0.09909245471376171288, -59.27992525550198621 ) ) ;
#20965 = VERTEX_POINT ( 'NONE', #70037 ) ;
#20966 = DIRECTION ( 'NONE',  ( -0.000000000000000000, 1.000000000000000000, 6.982962677686266711E-15 ) ) ;
#20967 = ORIENTED_EDGE ( 'NONE', *, *, #62578, .F. ) ;
#20968 = DIRECTION ( 'NONE',  ( -1.652117596168391700E-15, 1.000000000000000000, 6.982962677686266711E-15 ) ) ;
#20969 = B_SPLINE_CURVE_WITH_KNOTS ( 'NONE', 3,
 ( #221624, #39193, #122569, #63861, #160427, #202094, #179971, #1299, #143395, #239943, #2589, #61295, #140834, #121307, #58700, #200809, #44310, #157876, #22187 ),
 .UNSPECIFIED., .F., .F.,
 ( 4, 3, 3, 3, 3, 3, 4 ),
 ( 0.000000000000000000, 2.646747978908389238E-05, 5.271166642128361261E-05, 9.008788829883987372E-05, 0.0001426648776560936627, 0.0001897378458659669401, 0.0001917382627806129159 ),
 .UNSPECIFIED. ) ;
#20970 = DIRECTION ( 'NONE',  ( 1.000000000000000000, -0.000000000000000000, -0.000000000000000000 ) ) ;
#20971 = PLANE ( 'NONE',  #14189 ) ;
#20972 = ORIENTED_EDGE ( 'NONE', *, *, #162558, .F. ) ;
#20973 = EDGE_CURVE ( 'NONE', #183601, #61130, #105242, .T. ) ;
#20974 = CARTESIAN_POINT ( 'NONE',  ( 20.94999999999999929, -8.663551401858002876, -76.52410111806734960 ) ) ;
#20975 = EDGE_CURVE ( 'NONE', #231838, #113005, #127422, .T. ) ;
#20976 = AXIS2_PLACEMENT_3D ( 'NONE', #165850, #184103, #82409 ) ;
#20977 = AXIS2_PLACEMENT_3D ( 'NONE', #124028, #121480, #163157 ) ;
#20978 = AXIS2_PLACEMENT_3D ( 'NONE', #39979, #236855, #180749 ) ;
#20979 = AXIS2_PLACEMENT_3D ( 'NONE', #36159, #214772, #115683 ) ;
#20980 = EDGE_CURVE ( 'NONE', #231838, #55547, #107603, .T. ) ;
#20981 = MANIFOLD_SOLID_BREP ( 'Stock-MAS-200-1', #32659 ) ;
#20982 = DIRECTION ( 'NONE',  ( 0.000000000000000000, -6.982962677686266711E-15, 1.000000000000000000 ) ) ;
#20983 = ORIENTED_EDGE ( 'NONE', *, *, #218872, .T. ) ;
#20984 = AXIS2_PLACEMENT_3D ( 'NONE', #142969, #238240, #41360 ) ;
#20985 = ORIENTED_EDGE ( 'NONE', *, *, #239331, .F. ) ;
#20986 = ORIENTED_EDGE ( 'NONE', *, *, #201182, .F. ) ;
#20987 = DIRECTION ( 'NONE',  ( -0.000000000000000000, -0.8660254037844468122, -0.4999999999999860112 ) ) ;
#20988 = ORIENTED_EDGE ( 'NONE', *, *, #112739, .T. ) ;
#20990 = VERTEX_POINT ( 'NONE', #209522 ) ;
#20989 = CARTESIAN_POINT ( 'NONE',  ( 15.57250062127603663, 66.62931007840995790, -185.9966423578633794 ) ) ;
#20991 = ADVANCED_FACE ( 'NONE', ( #90847 ), #53004, .F. ) ;
#20992 = EDGE_LOOP ( 'NONE', ( #48696, #111032, #238591, #101560 ) ) ;
#20993 = AXIS2_PLACEMENT_3D ( 'NONE', #249772, #151985, #112828 ) ;
#20996 = ORIENTED_EDGE ( 'NONE', *, *, #109447, .T. ) ;
#20995 = VERTEX_POINT ( 'NONE', #154713 ) ;
#20994 = DIRECTION ( 'NONE',  ( 0.000000000000000000, 0.000000000000000000, 1.000000000000000000 ) ) ;
#20997 = EDGE_CURVE ( 'NONE', #168, #96108, #28152, .T. ) ;
#20998 = ORIENTED_EDGE ( 'NONE', *, *, #146992, .T. ) ;
#20999 = FACE_OUTER_BOUND ( 'NONE', #125011, .T. ) ;
#21000 = DIRECTION ( 'NONE',  ( -1.000000000000000000, 0.000000000000000000, 0.000000000000000000 ) ) ;
#21001 = CARTESIAN_POINT ( 'NONE',  ( -16.97683810757273193, 14.02843185299666118, -218.6555494737106642 ) ) ;
#21002 = ORIENTED_EDGE ( 'NONE', *, *, #162874, .T. ) ;
#21003 = CARTESIAN_POINT ( 'NONE',  ( -20.85000000000000142, 18.51199663233067483, -231.2535697180530292 ) ) ;
#21005 = ORIENTED_EDGE ( 'NONE', *, *, #27338, .F. ) ;
#21004 = DIRECTION ( 'NONE',  ( 0.000000000000000000, -0.2617529984165152257, -0.9651348961777124202 ) ) ;
#21006 = DIRECTION ( 'NONE',  ( 1.000000000000000000, 0.000000000000000000, 0.000000000000000000 ) ) ;
#21008 = ORIENTED_EDGE ( 'NONE', *, *, #220248, .T. ) ;
#21007 = CARTESIAN_POINT ( 'NONE',  ( -20.64999999999999858, 85.50000000001197975, -112.9170766071766820 ) ) ;
#21009 = ORIENTED_EDGE ( 'NONE', *, *, #168424, .F. ) ;
#21010 = DIRECTION ( 'NONE',  ( 0.000000000000000000, 0.000000000000000000, 1.000000000000000000 ) ) ;
#21011 = CARTESIAN_POINT ( 'NONE',  ( 21.05000000000000071, 1.115600667400684642E-11, -100.5000000000000426 ) ) ;
#21012 = ORIENTED_EDGE ( 'NONE', *, *, #89721, .F. ) ;
#21013 = ORIENTED_EDGE ( 'NONE', *, *, #31993, .F. ) ;
#21015 = CIRCLE ( 'NONE', #179401, 0.09999999999999939493 ) ;
#21014 = LINE ( 'NONE', #164359, #168731 ) ;
#21016 = CARTESIAN_POINT ( 'NONE',  ( 22.39999999999999503, 0.1000000000111554016, -60.75000000000004974 ) ) ;
#21018 = VERTEX_POINT ( 'NONE', #33497 ) ;
#21017 = ORIENTED_EDGE ( 'NONE', *, *, #65889, .T. ) ;
#21019 = ORIENTED_EDGE ( 'NONE', *, *, #132080, .F. ) ;
#21020 = CARTESIAN_POINT ( 'NONE',  ( 21.06600267594171783, 61.95655793666846023, -221.7794405828697393 ) ) ;
#21021 = ORIENTED_EDGE ( 'NONE', *, *, #159730, .T. ) ;
#21022 = ORIENTED_EDGE ( 'NONE', *, *, #119507, .F. ) ;
#21023 = CARTESIAN_POINT ( 'NONE',  ( 18.39999999999999858, 85.50000000001240608, -163.4229180933022576 ) ) ;
#21024 = CIRCLE ( 'NONE', #137674, 0.5000000000000051070 ) ;
#21025 = EDGE_LOOP ( 'NONE', ( #205902, #209442, #88330, #29246 ) ) ;
#21026 = CARTESIAN_POINT ( 'NONE',  ( -20.94999999999999929, 76.00000000001190870, -103.0231074845243029 ) ) ;
#21028 = CARTESIAN_POINT ( 'NONE',  ( 23.14999999999999858, 1.115600667400684642E-11, -167.5000000000000284 ) ) ;
#21027 = LINE ( 'NONE', #100500, #32242 ) ;
#21029 = ORIENTED_EDGE ( 'NONE', *, *, #201611, .F. ) ;
#21031 = ORIENTED_EDGE ( 'NONE', *, *, #25208, .T. ) ;
#21030 = VERTEX_POINT ( 'NONE', #12629 ) ;
#21032 = CARTESIAN_POINT ( 'NONE',  ( 20.94999999999999929, 1.115600667400684642E-11, -167.5000000000000284 ) ) ;
#21033 = CARTESIAN_POINT ( 'NONE',  ( -16.97683809663752186, 9.949999999999983302, -13.40236401819648648 ) ) ;
#21035 = ORIENTED_EDGE ( 'NONE', *, *, #202847, .T. ) ;
#21034 = VECTOR ( 'NONE', #191175, 1000.000000000000114 ) ;
#21036 = AXIS2_PLACEMENT_3D ( 'NONE', #945, #162639, #80481 ) ;
#21037 = DIRECTION ( 'NONE',  ( 2.952720810173289112E-16, 1.000000000000000000, 6.938893903907229955E-15 ) ) ;
#21038 = ORIENTED_EDGE ( 'NONE', *, *, #173636, .T. ) ;
#21039 = EDGE_LOOP ( 'NONE', ( #71163, #45714, #213503, #239641 ) ) ;
#21040 = CIRCLE ( 'NONE', #120998, 0.5000000000000004441 ) ;
#21041 = SPHERICAL_SURFACE ( 'NONE', #175248, 0.1000000000000000056 ) ;
#21042 = ADVANCED_FACE ( 'NONE', ( #196368 ), #243671, .T. ) ;
#21043 = ORIENTED_EDGE ( 'NONE', *, *, #46488, .F. ) ;
#21044 = CARTESIAN_POINT ( 'NONE',  ( -23.25000000000000000, 1.999999999999998224, -20.27537807723789953 ) ) ;
#21045 = CARTESIAN_POINT ( 'NONE',  ( 21.04999999999999716, 76.03753606329763670, -109.3553797584599749 ) ) ;
#21046 = ORIENTED_EDGE ( 'NONE', *, *, #252511, .T. ) ;
#21047 = AXIS2_PLACEMENT_3D ( 'NONE', #115076, #236299, #58916 ) ;
#21048 = DIRECTION ( 'NONE',  ( 1.000000000000000000, 0.000000000000000000, 0.000000000000000000 ) ) ;
#21050 = CIRCLE ( 'NONE', #212577, 0.1000000000000052097 ) ;
#21049 = CARTESIAN_POINT ( 'NONE',  ( -18.37013991200266005, 11.49974761622312691, -42.70697698948288945 ) ) ;
#21052 = CARTESIAN_POINT ( 'NONE',  ( -21.55000000000000426, 68.25000000001179501, -81.87310748452436826 ) ) ;
#21051 = CARTESIAN_POINT ( 'NONE',  ( -21.64999999999999858, 9.349999999999978328, -20.85000000000000142 ) ) ;
#21053 = DIRECTION ( 'NONE',  ( 0.000000000000000000, 0.6728388485993012091, -0.7397890806274222131 ) ) ;
#21054 = EDGE_CURVE ( 'NONE', #109083, #37631, #41185, .T. ) ;
#21055 = CARTESIAN_POINT ( 'NONE',  ( -20.94999999999999929, 43.08613539620618837, -254.3146655184800409 ) ) ;
#21057 = EDGE_CURVE ( 'NONE', #65120, #59781, #153071, .T. ) ;
#21056 = CARTESIAN_POINT ( 'NONE',  ( -16.81744102076748959, 63.08573235307424198, -213.1276215869287967 ) ) ;
#21058 = PLANE ( 'NONE',  #178021 ) ;
#21059 = DIRECTION ( 'NONE',  ( 0.000000000000000000, 0.000000000000000000, 1.000000000000000000 ) ) ;
#21060 = DIRECTION ( 'NONE',  ( -0.000000000000000000, -6.982962677686266711E-15, 1.000000000000000000 ) ) ;
#21061 = ORIENTED_EDGE ( 'NONE', *, *, #224087, .T. ) ;
#21062 = B_SPLINE_CURVE_WITH_KNOTS ( 'NONE', 3,
 ( #109862, #47311, #87727, #26505, #30360, #29105, #168626, #146411, #49898, #27810, #69490, #90297, #169906, #250660 ),
 .UNSPECIFIED., .F., .F.,
 ( 4, 2, 2, 2, 2, 2, 4 ),
 ( 0.000000000000000000, 2.389617747639151307E-05, 4.779235495278302614E-05, 9.558470990564444010E-05, 0.0001911694198113644762, 0.0003823388396228028950, 0.0007646776792455974416 ),
 .UNSPECIFIED. ) ;
#21063 = AXIS2_PLACEMENT_3D ( 'NONE', #161279, #115720, #158727 ) ;
#21064 = TOROIDAL_SURFACE ( 'NONE', #54329, 0.2000000000000000111, 0.1000000000000000056 ) ;
#21065 = AXIS2_PLACEMENT_3D ( 'NONE', #59543, #82954, #257721 ) ;
#21066 = AXIS2_PLACEMENT_3D ( 'NONE', #70792, #206419, #189436 ) ;
#21067 = CIRCLE ( 'NONE', #166816, 0.09999999999999939493 ) ;
#21069 = ORIENTED_EDGE ( 'NONE', *, *, #54203, .T. ) ;
#21068 = VERTEX_POINT ( 'NONE', #16479 ) ;
#21070 = EDGE_LOOP ( 'NONE', ( #163947, #254500, #30415, #236531 ) ) ;
#21071 = EDGE_LOOP ( 'NONE', ( #165927, #192719, #58350, #117630 ) ) ;
#21072 = EDGE_CURVE ( 'NONE', #101793, #176003, #162784, .T. ) ;
#21073 = CARTESIAN_POINT ( 'NONE',  ( -16.94445028196808778, 9.992063609708889516, -79.60733017841850767 ) ) ;
#21074 = CARTESIAN_POINT ( 'NONE',  ( 20.94999999999999574, 87.48912529308798014, -99.92310748452423752 ) ) ;
#21076 = DIRECTION ( 'NONE',  ( 1.000000000000000000, -3.265361837132813093E-16, -2.280189983783949500E-30 ) ) ;
#21075 = DIRECTION ( 'NONE',  ( 0.000000000000000000, 0.9177795674685970129, 0.3970902486049678326 ) ) ;
#21077 = CARTESIAN_POINT ( 'NONE',  ( 23.14999999999999503, 64.35000000001249987, -177.0379132551783812 ) ) ;
#21078 = ORIENTED_EDGE ( 'NONE', *, *, #99950, .F. ) ;
#21079 = DIRECTION ( 'NONE',  ( 0.000000000000000000, 0.2617529984165024026, 0.9651348961777158619 ) ) ;
#21080 = AXIS2_PLACEMENT_3D ( 'NONE', #132260, #211812, #14904 ) ;
#21081 = CARTESIAN_POINT ( 'NONE',  ( 20.05000000000002913, 7.250000000011171508, -46.15000000000000568 ) ) ;
#21082 = DIRECTION ( 'NONE',  ( 0.000000000000000000, 0.000000000000000000, -1.000000000000000000 ) ) ;
#21083 = FACE_OUTER_BOUND ( 'NONE', #182762, .T. ) ;
#21084 = ORIENTED_EDGE ( 'NONE', *, *, #134877, .F. ) ;
#21085 = CARTESIAN_POINT ( 'NONE',  ( -23.25000000000000000, 47.40541193113006813, -242.6436572752161283 ) ) ;
#21086 = CARTESIAN_POINT ( 'NONE',  ( -21.14999999999999858, 1.115526128501326264E-11, -93.95934304829879125 ) ) ;
#21087 = ORIENTED_EDGE ( 'NONE', *, *, #15796, .F. ) ;
#21088 = EDGE_CURVE ( 'NONE', #230047, #18995, #20331, .T. ) ;
#21089 = CARTESIAN_POINT ( 'NONE',  ( 20.94999999999999929, 1.115600667400684642E-11, -200.9999999999999432 ) ) ;
#21090 = EDGE_CURVE ( 'NONE', #33168, #100804, #152144, .T. ) ;
#21091 = PLANE ( 'NONE',  #36393 ) ;
#21092 = DIRECTION ( 'NONE',  ( 0.000000000000000000, 1.000000000000000000, 0.000000000000000000 ) ) ;
#21093 = CARTESIAN_POINT ( 'NONE',  ( 21.14999999999999858, 1.115600667400684642E-11, -67.00000000000004263 ) ) ;
#21094 = LINE ( 'NONE', #83569, #250090 ) ;
#21095 = ORIENTED_EDGE ( 'NONE', *, *, #156645, .F. ) ;
#21096 = DIRECTION ( 'NONE',  ( 0.000000000000000000, -1.000000000000000000, -6.860497997771531562E-15 ) ) ;
#21097 = DIRECTION ( 'NONE',  ( 0.000000000000000000, 6.853228547068871147E-15, -1.000000000000000000 ) ) ;
#21098 = CARTESIAN_POINT ( 'NONE',  ( 20.94999999999999929, 71.00000000001260503, -191.1178414656112921 ) ) ;
#21100 = DIRECTION ( 'NONE',  ( -1.000000000000000000, 0.000000000000000000, 0.000000000000000000 ) ) ;
#21099 = CARTESIAN_POINT ( 'NONE',  ( 18.57071067811864040, 65.82071067813065213, -115.1731074845243796 ) ) ;
#21101 = DIRECTION ( 'NONE',  ( 1.000000000000000000, 3.265361837132813093E-16, -0.000000000000000000 ) ) ;
#21102 = TOROIDAL_SURFACE ( 'NONE', #41943, 1.900000000000002576, 0.1000000000000000056 ) ;
#21103 = EDGE_CURVE ( 'NONE', #44233, #6026, #234206, .T. ) ;
#21104 = DIRECTION ( 'NONE',  ( -0.000000000000000000, -0.9126074666063769270, -0.4088369013363283844 ) ) ;
#21105 = DIRECTION ( 'NONE',  ( 6.938893903907223644E-15, 0.9651348961777157509, -0.2617529984165028467 ) ) ;
#21106 = CARTESIAN_POINT ( 'NONE',  ( 22.49066049874202022, 75.94365674847981040, -114.6731197220414202 ) ) ;
#21107 = VERTEX_POINT ( 'NONE', #214646 ) ;
#21108 = ORIENTED_EDGE ( 'NONE', *, *, #67783, .T. ) ;
#21109 = AXIS2_PLACEMENT_3D ( 'NONE', #221473, #224050, #182386 ) ;
#21110 = ORIENTED_EDGE ( 'NONE', *, *, #47339, .F. ) ;
#21111 = DIRECTION ( 'NONE',  ( 0.000000000000000000, -0.2128009952263604232, 0.9770955615653316162 ) ) ;
#21112 = DIRECTION ( 'NONE',  ( -0.000000000000000000, 0.8814952561688430555, -0.4721928772777346239 ) ) ;
#21113 = EDGE_CURVE ( 'NONE', #250431, #65749, #193819, .T. ) ;
#21114 = AXIS2_PLACEMENT_3D ( 'NONE', #65274, #186520, #183942 ) ;
#21115 = CARTESIAN_POINT ( 'NONE',  ( -18.55807992284872299, 65.67101464000451472, -30.44043916224794799 ) ) ;
#21116 = CARTESIAN_POINT ( 'NONE',  ( 22.00411653889229058, 65.23707900164814077, -242.8297538143178258 ) ) ;
#21117 = AXIS2_PLACEMENT_3D ( 'NONE', #122420, #161562, #61154 ) ;
#21118 = ORIENTED_EDGE ( 'NONE', *, *, #175402, .F. ) ;
#21119 = TOROIDAL_SURFACE ( 'NONE', #250231, 6.258578643762700899, 0.1000000000000000056 ) ;
#21120 = DIRECTION ( 'NONE',  ( 0.000000000000000000, 0.000000000000000000, -1.000000000000000000 ) ) ;
#21121 = LINE ( 'NONE', #26245, #124234 ) ;
#21123 = DIRECTION ( 'NONE',  ( -1.000000000000000000, -0.000000000000000000, 0.000000000000000000 ) ) ;
#21122 = AXIS2_PLACEMENT_3D ( 'NONE', #225903, #190697, #109829 ) ;
#21124 = EDGE_CURVE ( 'NONE', #71259, #120435, #140539, .T. ) ;
#21125 = ADVANCED_FACE ( 'NONE', ( #36036 ), #179399, .F. ) ;
#21126 = CARTESIAN_POINT ( 'NONE',  ( -18.59999999999999787, 1.115600667400684642E-11, -134.0000000000000284 ) ) ;
#21128 = ORIENTED_EDGE ( 'NONE', *, *, #23, .T. ) ;
#21127 = FACE_OUTER_BOUND ( 'NONE', #74818, .T. ) ;
#21130 = CARTESIAN_POINT ( 'NONE',  ( -21.59142135623730852, 68.15000000001199965, -115.3731074845243540 ) ) ;
#21129 = CYLINDRICAL_SURFACE ( 'NONE', #125584, 0.5000000000000008882 ) ;
#21131 = CARTESIAN_POINT ( 'NONE',  ( 21.05000000000000071, -11.48912529307605901, -3.100000000000000533 ) ) ;
#21132 = EDGE_CURVE ( 'NONE', #221268, #231632, #78571, .T. ) ;
#21133 = EDGE_CURVE ( 'NONE', #166990, #221113, #107226, .T. ) ;
#21134 = ORIENTED_EDGE ( 'NONE', *, *, #234211, .T. ) ;
#21135 = CARTESIAN_POINT ( 'NONE',  ( 0.000000000000000000, 0.000000000000000000, 0.000000000000000000 ) ) ;
#21136 = CARTESIAN_POINT ( 'NONE',  ( 21.05000000000000071, 6.257814610487280937, -100.4022097086912311 ) ) ;
#21137 = DIRECTION ( 'NONE',  ( 0.000000000000000000, 0.000000000000000000, 1.000000000000000000 ) ) ;
#21138 = VECTOR ( 'NONE', #16781, 1000.000000000000000 ) ;
#21139 = ORIENTED_EDGE ( 'NONE', *, *, #19014, .F. ) ;
#21140 = LINE ( 'NONE', #44538, #237641 ) ;
#21141 = DIRECTION ( 'NONE',  ( -1.000000000000000000, 1.836970198721029934E-16, 1.601412966608202925E-30 ) ) ;
#21142 = ORIENTED_EDGE ( 'NONE', *, *, #200167, .T. ) ;
#21143 = EDGE_CURVE ( 'NONE', #203019, #242139, #120320, .T. ) ;
#21144 = DIRECTION ( 'NONE',  ( 0.000000000000000000, 0.000000000000000000, 1.000000000000000000 ) ) ;
#21145 = EDGE_CURVE ( 'NONE', #21183, #211804, #162402, .T. ) ;
#21146 = CYLINDRICAL_SURFACE ( 'NONE', #195017, 0.09999999999999507894 ) ;
#21147 = CARTESIAN_POINT ( 'NONE',  ( -33.72168855820452649, 11.47316190336247033, -9.249999999999998224 ) ) ;
#21148 = VERTEX_POINT ( 'NONE', #256275 ) ;
#21149 = ADVANCED_FACE ( 'NONE', ( #137662 ), #101070, .T. ) ;
#21150 = ORIENTED_EDGE ( 'NONE', *, *, #69149, .T. ) ;
#21151 = DIRECTION ( 'NONE',  ( 1.000000000000000000, -0.000000000000000000, -0.000000000000000000 ) ) ;
#21152 = PLANE ( 'NONE',  #90172 ) ;
#21153 = VECTOR ( 'NONE', #244706, 1000.000000000000000 ) ;
#21154 = EDGE_CURVE ( 'NONE', #7969, #237173, #245177, .T. ) ;
#21155 = CARTESIAN_POINT ( 'NONE',  ( -23.15000000000000213, 2.500000000011154633, -154.2753780772379173 ) ) ;
#21157 = CARTESIAN_POINT ( 'NONE',  ( -11.60000000000000320, -8.250000000000007105, 17.60000000000000497 ) ) ;
#21156 = AXIS2_PLACEMENT_3D ( 'NONE', #93873, #173477, #75624 ) ;
#21160 = CARTESIAN_POINT ( 'NONE',  ( 21.08489834409762054, 10.62232389473552097, -12.35000000000000320 ) ) ;
#21159 = AXIS2_PLACEMENT_3D ( 'NONE', #146468, #8275, #145189 ) ;
#21158 = DIRECTION ( 'NONE',  ( 1.000000000000000000, -3.469446951953718318E-14, 2.003086131649645455E-14 ) ) ;
#21161 = CARTESIAN_POINT ( 'NONE',  ( 20.94999999999999574, -11.64999999998883595, -70.10000000000005116 ) ) ;
#21163 = EDGE_CURVE ( 'NONE', #27371, #239767, #58121, .T. ) ;
#21162 = CARTESIAN_POINT ( 'NONE',  ( 21.05000000000000071, 70.15000000001192859, -92.89061026024637613 ) ) ;
#21165 = EDGE_CURVE ( 'NONE', #217509, #137157, #219650, .T. ) ;
#21164 = CARTESIAN_POINT ( 'NONE',  ( 22.59999999999999432, 75.89914163091350474, -148.2726746080136877 ) ) ;
#21166 = ORIENTED_EDGE ( 'NONE', *, *, #205775, .F. ) ;
#21167 = DIRECTION ( 'NONE',  ( 1.000000000000000000, 0.000000000000000000, 0.000000000000000000 ) ) ;
#21169 = ORIENTED_EDGE ( 'NONE', *, *, #60614, .T. ) ;
#21168 = FACE_OUTER_BOUND ( 'NONE', #78656, .T. ) ;
#21170 = TOROIDAL_SURFACE ( 'NONE', #41825, 0.2000000000000000111, 0.1000000000000000056 ) ;
#21171 = CARTESIAN_POINT ( 'NONE',  ( -21.00219873199083054, 64.39461131213550971, -129.6104600562298401 ) ) ;
#21172 = DIRECTION ( 'NONE',  ( 1.000000000000000000, 0.000000000000000000, 0.000000000000000000 ) ) ;
#21174 = DIRECTION ( 'NONE',  ( 1.000000000000000000, 0.000000000000000000, -0.000000000000000000 ) ) ;
#21173 = CARTESIAN_POINT ( 'NONE',  ( -23.25000000000000000, 12.67709964810647882, -223.3751320524553705 ) ) ;
#21175 = EDGE_CURVE ( 'NONE', #159477, #144497, #172127, .T. ) ;
#21176 = ORIENTED_EDGE ( 'NONE', *, *, #43733, .F. ) ;
#21178 = LINE ( 'NONE', #160690, #969 ) ;
#21177 = FACE_OUTER_BOUND ( 'NONE', #11994, .T. ) ;
#21179 = DIRECTION ( 'NONE',  ( -1.000000000000000000, 0.000000000000000000, 0.000000000000000000 ) ) ;
#21180 = DIRECTION ( 'NONE',  ( -0.000000000000000000, 7.172728831056617961E-15, -1.000000000000000000 ) ) ;
#21181 = FACE_OUTER_BOUND ( 'NONE', #64637, .T. ) ;
#21182 = CARTESIAN_POINT ( 'NONE',  ( -15.31895204843004699, 66.60346600605865319, -185.6171677053510791 ) ) ;
#21183 = VERTEX_POINT ( 'NONE', #80239 ) ;
#21184 = CARTESIAN_POINT ( 'NONE',  ( 21.05000000000000071, 1.360870587203197646, -142.0729979270909951 ) ) ;
#21185 = EDGE_CURVE ( 'NONE', #30609, #134482, #219776, .T. ) ;
#21187 = VERTEX_POINT ( 'NONE', #38590 ) ;
#21186 = AXIS2_PLACEMENT_3D ( 'NONE', #165782, #148778, #127924 ) ;
#21188 = ADVANCED_FACE ( 'NONE', ( #63275 ), #46689, .T. ) ;
#21189 = ADVANCED_FACE ( 'NONE', ( #238059 ), #140229, .T. ) ;
#21190 = CARTESIAN_POINT ( 'NONE',  ( -16.77732147262506146, 9.945966932629787038, -54.33649124327587998 ) ) ;
#21191 = ORIENTED_EDGE ( 'NONE', *, *, #243459, .F. ) ;
#21192 = CARTESIAN_POINT ( 'NONE',  ( -21.05000000000000071, 1.115600667400684642E-11, -33.50000000000000000 ) ) ;
#21193 = EDGE_LOOP ( 'NONE', ( #142905, #255327, #156686, #117802 ) ) ;
#21194 = DIRECTION ( 'NONE',  ( 0.000000000000000000, 6.982962677686266711E-15, -1.000000000000000000 ) ) ;
#21195 =( BOUNDED_SURFACE ( )  B_SPLINE_SURFACE ( 3, 2, ( 
 ( #178214, #16561, #199037 ),
 ( #238145, #257655, #158651 ),
 ( #218574, #96063, #99895 ),
 ( #39992, #119509, #175636 ),
 ( #20414, #179490, #796 ),
 ( #80332, #26842, #146729 ),
 ( #180760, #2096, #47633 ),
 ( #202874, #86761, #240734 ),
 ( #221146, #81609, #166360 ),
 ( #244564, #144167, #165037 ) ),
 .UNSPECIFIED., .F., .F., .F. ) 
 B_SPLINE_SURFACE_WITH_KNOTS ( ( 4, 2, 2, 2, 4 ),
 ( 3, 3 ),
 ( 0.0001701955120502350236, 0.0002247052511886079022, 0.0002792149903269808080, 0.0003882344686037266196, 0.0006062734251572181885 ),
 ( 0.000000000000000000, 1.000000000000000000 ),
 .UNSPECIFIED. ) 
 GEOMETRIC_REPRESENTATION_ITEM ( )  RATIONAL_B_SPLINE_SURFACE ( (
 ( 1.000000000000000000, 0.2966190024561151661, 1.000000000000000000),
 ( 1.000000000000000000, 0.2964522492711512691, 1.000000000000000000),
 ( 1.000000000000000000, 0.3059923531882601799, 1.000000000000000000),
 ( 1.000000000000000000, 0.3355751146946392427, 1.000000000000000000),
 ( 1.000000000000000000, 0.3550672384960338879, 1.000000000000000000),
 ( 1.000000000000000000, 0.4157034672187559510, 1.000000000000000000),
 ( 1.000000000000000000, 0.4588031877649293433, 1.000000000000000000),
 ( 1.000000000000000000, 0.5771441759671969152, 1.000000000000000000),
 ( 1.000000000000000000, 0.6469377121765136351, 1.000000000000000000),
 ( 1.000000000000000000, 0.7071067811865475727, 1.000000000000000000) ) ) 
 REPRESENTATION_ITEM ( '' )  SURFACE ( )  );
#21196 = LINE ( 'NONE', #1583, #9763 ) ;
#21197 = VERTEX_POINT ( 'NONE', #248344 ) ;
#21198 = EDGE_CURVE ( 'NONE', #208145, #229099, #244483, .T. ) ;
#21199 = VECTOR ( 'NONE', #124420, 1000.000000000000000 ) ;
#21200 = CARTESIAN_POINT ( 'NONE',  ( -20.94999999999999929, -11.64999999998884483, -36.39999999999999858 ) ) ;
#21201 = CARTESIAN_POINT ( 'NONE',  ( -22.59999999999999787, 75.89914163091332000, -114.7726746080137019 ) ) ;
#21202 = CARTESIAN_POINT ( 'NONE',  ( -21.05000000000000071, 1.115600667400684642E-11, -167.4999999999999716 ) ) ;
#21203 = AXIS2_PLACEMENT_3D ( 'NONE', #145532, #206806, #25607 ) ;
#21204 = CARTESIAN_POINT ( 'NONE',  ( 16.87683809663749557, 30.20632856012693068, -234.8070450048000737 ) ) ;
#21205 = DIRECTION ( 'NONE',  ( 1.000000000000000000, 0.000000000000000000, 0.000000000000000000 ) ) ;
#21207 = CARTESIAN_POINT ( 'NONE',  ( -20.64999999999999858, 29.19585636832770703, -237.3287400596392445 ) ) ;
#21206 = AXIS2_PLACEMENT_3D ( 'NONE', #68051, #86300, #254054 ) ;
#21208 = ORIENTED_EDGE ( 'NONE', *, *, #126993, .T. ) ;
#21209 = DIRECTION ( 'NONE',  ( -1.000000000000000000, 0.000000000000000000, 0.000000000000000000 ) ) ;
#21210 = ORIENTED_EDGE ( 'NONE', *, *, #23504, .F. ) ;
#21212 = VERTEX_POINT ( 'NONE', #107537 ) ;
#21211 = DIRECTION ( 'NONE',  ( -0.000000000000000000, -0.000000000000000000, 1.000000000000000000 ) ) ;
#21213 = ORIENTED_EDGE ( 'NONE', *, *, #228397, .F. ) ;
#21214 = CARTESIAN_POINT ( 'NONE',  ( 18.60000000000000853, -9.364236010366765228, -7.180254400724614072 ) ) ;
#21215 = DIRECTION ( 'NONE',  ( 1.000000000000000000, 0.000000000000000000, 0.000000000000000000 ) ) ;
#21216 = CARTESIAN_POINT ( 'NONE',  ( 12.47034474403011473, 66.62446189796457929, -187.6532316035335839 ) ) ;
#21217 = DIRECTION ( 'NONE',  ( 1.000000000000000000, 0.000000000000000000, 0.000000000000000000 ) ) ;
#21218 = CARTESIAN_POINT ( 'NONE',  ( 18.49999999999998934, 55.05538098155519577, -230.0782228604559805 ) ) ;
#21219 = AXIS2_PLACEMENT_3D ( 'NONE', #148755, #14395, #32696 ) ;
#21220 = ORIENTED_EDGE ( 'NONE', *, *, #98216, .F. ) ;
#21221 = CARTESIAN_POINT ( 'NONE',  ( -18.50000000000000000, 5.950000000011100632, -43.80570230503486329 ) ) ;
#21222 = DIRECTION ( 'NONE',  ( 0.000000000000000000, 0.000000000000000000, -1.000000000000000000 ) ) ;
#21223 = VERTEX_POINT ( 'NONE', #50131 ) ;
#21224 = CARTESIAN_POINT ( 'NONE',  ( 18.59999994388910238, -9.363566187059905843, -174.6811172368009863 ) ) ;
#21225 = ADVANCED_FACE ( 'NONE', ( #245779 ), #45006, .T. ) ;
#21226 = CARTESIAN_POINT ( 'NONE',  ( -23.25000000000000355, 11.75000000001113953, -143.2500000000000284 ) ) ;
#21227 = AXIS2_PLACEMENT_3D ( 'NONE', #41092, #25379, #203985 ) ;
#21228 = EDGE_LOOP ( 'NONE', ( #112489, #127366, #73414, #154019, #85088, #212505 ) ) ;
#21229 = ADVANCED_FACE ( 'NONE', ( #128398 ), #8456, .T. ) ;
#21230 = CYLINDRICAL_SURFACE ( 'NONE', #1842, 0.09999999999999939493 ) ;
#21231 = CIRCLE ( 'NONE', #83692, 0.09999999999999939493 ) ;
#21232 = AXIS2_PLACEMENT_3D ( 'NONE', #44626, #87575, #147570 ) ;
#21233 = CARTESIAN_POINT ( 'NONE',  ( 20.87155475150661132, 64.25000000001195133, -109.9275209553671147 ) ) ;
#21234 = VERTEX_POINT ( 'NONE', #149266 ) ;
#21235 = FACE_OUTER_BOUND ( 'NONE', #71693, .T. ) ;
#21236 = VECTOR ( 'NONE', #59899, 1000.000000000000114 ) ;
#21237 = EDGE_CURVE ( 'NONE', #135639, #117247, #25456, .T. ) ;
#21238 = EDGE_CURVE ( 'NONE', #47244, #252649, #69724, .T. ) ;
#21239 = DIRECTION ( 'NONE',  ( 1.186688945009010077E-16, -1.000000000000000000, -0.000000000000000000 ) ) ;
#21240 = DIRECTION ( 'NONE',  ( 0.000000000000000000, -1.000000000000000000, 0.000000000000000000 ) ) ;
#21241 = AXIS2_PLACEMENT_3D ( 'NONE', #30959, #206998, #107889 ) ;
#21242 = AXIS2_PLACEMENT_3D ( 'NONE', #163914, #29567, #109058 ) ;
#21243 = DIRECTION ( 'NONE',  ( -0.000000000000000000, 1.000000000000000000, -0.000000000000000000 ) ) ;
#21244 = DIRECTION ( 'NONE',  ( -0.000000000000000000, 0.000000000000000000, 1.000000000000000000 ) ) ;
#21245 = VECTOR ( 'NONE', #148123, 1000.000000000000000 ) ;
#21246 = CIRCLE ( 'NONE', #67004, 0.09999999999999939493 ) ;
#21247 = AXIS2_PLACEMENT_3D ( 'NONE', #53163, #201656, #98662 ) ;
#21248 = EDGE_LOOP ( 'NONE', ( #172753, #148188 ) ) ;
#21250 = CARTESIAN_POINT ( 'NONE',  ( 20.73486653747088937, 7.750000000011182166, -76.25000000000004263 ) ) ;
#21249 = AXIS2_PLACEMENT_3D ( 'NONE', #66299, #42881, #102826 ) ;
#21251 = AXIS2_PLACEMENT_3D ( 'NONE', #65841, #146644, #102369 ) ;
#21252 = ORIENTED_EDGE ( 'NONE', *, *, #67679, .F. ) ;
#21253 = CARTESIAN_POINT ( 'NONE',  ( 20.94999999999999574, 1.851028230152016674, -179.1539132694224463 ) ) ;
#21254 = CARTESIAN_POINT ( 'NONE',  ( -16.86445178670638967, 9.962211629127175172, -79.60922256188266033 ) ) ;
#21256 = ORIENTED_EDGE ( 'NONE', *, *, #82133, .F. ) ;
#21255 = CARTESIAN_POINT ( 'NONE',  ( -23.15000000000000213, 6.855069093508305400, -220.2576993407411692 ) ) ;
#21257 = CARTESIAN_POINT ( 'NONE',  ( -16.77683809663752257, 26.68086916408615750, -212.3318337774905160 ) ) ;
#21258 = LINE ( 'NONE', #176471, #68684 ) ;
#21260 = DIRECTION ( 'NONE',  ( -0.000000000000000000, 1.000000000000000000, 6.982962677686266711E-15 ) ) ;
#21259 =( BOUNDED_CURVE ( )  B_SPLINE_CURVE ( 3, ( #172275, #13162, #155265, #14464 ),
 .UNSPECIFIED., .F., .F. ) 
 B_SPLINE_CURVE_WITH_KNOTS ( ( 4, 4 ),
 ( 4.712388980384689674, 6.283185307179586232 ),
 .UNSPECIFIED. ) 
 CURVE ( )  GEOMETRIC_REPRESENTATION_ITEM ( )  RATIONAL_B_SPLINE_CURVE ( ( 1.000000000000000000, 0.8047378541243649375, 0.8047378541243649375, 1.000000000000000000 ) ) 
 REPRESENTATION_ITEM ( '' )  );
#21261 = LINE ( 'NONE', #98156, #255974 ) ;
#21262 = CARTESIAN_POINT ( 'NONE',  ( -20.94999999999999929, 1.835341550235569663, -145.5551512925629822 ) ) ;
#21263 = CARTESIAN_POINT ( 'NONE',  ( 21.07928932188134397, 6.328516656404459262, -66.90110485434564680 ) ) ;
#21264 = CIRCLE ( 'NONE', #233624, 12.87499999999998934 ) ;
#21266 = EDGE_LOOP ( 'NONE', ( #175609, #50782, #102086, #71222, #47235 ) ) ;
#21265 = DIRECTION ( 'NONE',  ( 1.000000000000000000, 0.000000000000000000, 0.000000000000000000 ) ) ;
#21267 = EDGE_CURVE ( 'NONE', #137060, #231838, #224907, .T. ) ;
#21268 = DIRECTION ( 'NONE',  ( 1.000000000000000000, -0.000000000000000000, -0.000000000000000000 ) ) ;
#21269 = ORIENTED_EDGE ( 'NONE', *, *, #22955, .F. ) ;
#21270 = ORIENTED_EDGE ( 'NONE', *, *, #116453, .T. ) ;
#21271 = CARTESIAN_POINT ( 'NONE',  ( -18.41809261886927374, 85.68240331476842186, -62.86626393443329874 ) ) ;
#21272 = CARTESIAN_POINT ( 'NONE',  ( -18.43599941264928077, 85.51932742860661563, -196.5501306950018829 ) ) ;
#21273 = ORIENTED_EDGE ( 'NONE', *, *, #201565, .F. ) ;
#21274 = EDGE_CURVE ( 'NONE', #175518, #16470, #178571, .T. ) ;
#21275 = CARTESIAN_POINT ( 'NONE',  ( 23.14999999999999503, 11.04098673250373785, -220.4458636211660689 ) ) ;
#21276 = AXIS2_PLACEMENT_3D ( 'NONE', #209536, #93425, #128723 ) ;
#21277 = EDGE_CURVE ( 'NONE', #221570, #159137, #128113, .T. ) ;
#21278 = CARTESIAN_POINT ( 'NONE',  ( -18.40000000000000213, 85.51932773110404185, -62.55013110796492271 ) ) ;
#21279 = EDGE_LOOP ( 'NONE', ( #26445, #172432, #186818, #180456, #1718, #16424, #194262, #125003, #27443, #142415, #91954, #229673, #202806, #25059, #21385, #140502, #182400, #197961 ) ) ;
#21280 = CIRCLE ( 'NONE', #233649, 0.1000000000000124678 ) ;
#21281 = CARTESIAN_POINT ( 'NONE',  ( -23.15000000000000213, 87.65000000001276703, -215.2731074845242745 ) ) ;
#21282 =( BOUNDED_SURFACE ( )  B_SPLINE_SURFACE ( 3, 2, ( 
 ( #45284, #6139, #21876 ),
 ( #242191, #23178, #66128 ),
 ( #46546, #180951, #201780 ),
 ( #126084, #106512, #186082 ) ),
 .UNSPECIFIED., .F., .F., .F. ) 
 B_SPLINE_SURFACE_WITH_KNOTS ( ( 4, 4 ),
 ( 3, 3 ),
 ( 0.0008258556059633677133, 0.0009616864997632747171 ),
 ( 0.000000000000000000, 1.000000000000000000 ),
 .UNSPECIFIED. ) 
 GEOMETRIC_REPRESENTATION_ITEM ( )  RATIONAL_B_SPLINE_SURFACE ( (
 ( 1.000000000000000000, 0.9152888060719329699, 1.000000000000000000),
 ( 1.000000000000000000, 0.9327727094137943098, 1.000000000000000000),
 ( 1.000000000000000000, 0.9369023509258086468, 1.000000000000000000),
 ( 1.000000000000000000, 0.9246339933864506921, 1.000000000000000000) ) ) 
 REPRESENTATION_ITEM ( '' )  SURFACE ( )  );
#21283 = DIRECTION ( 'NONE',  ( -1.000000000000000000, 0.000000000000000000, 0.000000000000000000 ) ) ;
#21284 = EDGE_CURVE ( 'NONE', #13808, #121455, #167550, .T. ) ;
#21286 = ORIENTED_EDGE ( 'NONE', *, *, #159207, .F. ) ;
#21285 = CIRCLE ( 'NONE', #162937, 0.1000000000000028644 ) ;
#21287 = ORIENTED_EDGE ( 'NONE', *, *, #124774, .T. ) ;
#21288 = ORIENTED_EDGE ( 'NONE', *, *, #250244, .F. ) ;
#21289 = CARTESIAN_POINT ( 'NONE',  ( -23.15000000000000213, 47.45383559552795560, -242.5236527704543334 ) ) ;
#21290 = ORIENTED_EDGE ( 'NONE', *, *, #193182, .T. ) ;
#21292 = ORIENTED_EDGE ( 'NONE', *, *, #223882, .T. ) ;
#21291 = CARTESIAN_POINT ( 'NONE',  ( -14.00000000000000178, 26.54497872210690090, -232.9592037335782209 ) ) ;
#21293 = EDGE_CURVE ( 'NONE', #175396, #63066, #85375, .T. ) ;
#21294 = EDGE_CURVE ( 'NONE', #253128, #45881, #128662, .T. ) ;
#21295 = CARTESIAN_POINT ( 'NONE',  ( 21.05000000000000071, 76.00000000001165290, -69.52310748452431710 ) ) ;
#21296 = ORIENTED_EDGE ( 'NONE', *, *, #56498, .F. ) ;
#21297 = DIRECTION ( 'NONE',  ( 0.000000000000000000, 0.000000000000000000, -1.000000000000000000 ) ) ;
#21298 = ORIENTED_EDGE ( 'NONE', *, *, #188316, .T. ) ;
#21300 = EDGE_LOOP ( 'NONE', ( #188833, #147205, #49727, #110491 ) ) ;
#21299 = ORIENTED_EDGE ( 'NONE', *, *, #89789, .F. ) ;
#21301 = DIRECTION ( 'NONE',  ( 0.000000000000000000, -8.673617379883787770E-15, 1.000000000000000000 ) ) ;
#21302 = EDGE_CURVE ( 'NONE', #90545, #245055, #4576, .T. ) ;
#21303 = CARTESIAN_POINT ( 'NONE',  ( -20.54999999999999716, 76.00000000001227818, -157.0481074845243938 ) ) ;
#21304 = AXIS2_PLACEMENT_3D ( 'NONE', #244922, #204502, #188798 ) ;
#21305 = EDGE_LOOP ( 'NONE', ( #221693, #97604, #248495, #83671 ) ) ;
#21306 = CIRCLE ( 'NONE', #225443, 11.90000000000000391 ) ;
#21307 = CIRCLE ( 'NONE', #167059, 0.09999999999999917288 ) ;
#21308 = ORIENTED_EDGE ( 'NONE', *, *, #103234, .F. ) ;
#21309 = DIRECTION ( 'NONE',  ( 0.000000000000000000, 0.9770955615653316162, 0.2128009952263597848 ) ) ;
#21310 = ADVANCED_FACE ( 'NONE', ( #68429 ), #144084, .T. ) ;
#21311 = DIRECTION ( 'NONE',  ( 0.000000000000000000, 0.1350103645451835865, 0.9908441862701605762 ) ) ;
#21313 = ORIENTED_EDGE ( 'NONE', *, *, #5534, .T. ) ;
#21312 = CYLINDRICAL_SURFACE ( 'NONE', #182406, 0.5000000000000004441 ) ;
#21314 = DIRECTION ( 'NONE',  ( -1.000000000000000000, 0.000000000000000000, 0.000000000000000000 ) ) ;
#21315 = ORIENTED_EDGE ( 'NONE', *, *, #65380, .F. ) ;
#21316 = CARTESIAN_POINT ( 'NONE',  ( -22.59999999999999787, 0.1000000000111554016, -122.3504291924552234 ) ) ;
#21317 = CARTESIAN_POINT ( 'NONE',  ( -15.55912972643740488, 8.490870273573721150, -121.3500000000000369 ) ) ;
#21318 = ORIENTED_EDGE ( 'NONE', *, *, #11560, .T. ) ;
#21319 = PLANE ( 'NONE',  #241824 ) ;
#21320 = LINE ( 'NONE', #202496, #94611 ) ;
#21321 = LINE ( 'NONE', #47250, #115600 ) ;
#21322 = AXIS2_PLACEMENT_3D ( 'NONE', #1678, #179082, #60372 ) ;
#21323 = VERTEX_POINT ( 'NONE', #124555 ) ;
#21324 = DIRECTION ( 'NONE',  ( 1.000000000000000000, -0.000000000000000000, -0.000000000000000000 ) ) ;
#21325 = ORIENTED_EDGE ( 'NONE', *, *, #125578, .T. ) ;
#21326 = ORIENTED_EDGE ( 'NONE', *, *, #237406, .T. ) ;
#21327 = CARTESIAN_POINT ( 'NONE',  ( -20.94999999999999929, -11.48912529307605546, -30.39999999999999503 ) ) ;
#21328 = ORIENTED_EDGE ( 'NONE', *, *, #113538, .F. ) ;
#21329 = ORIENTED_EDGE ( 'NONE', *, *, #256621, .T. ) ;
#21330 = CARTESIAN_POINT ( 'NONE',  ( -18.35235881385853318, 11.47341900772405054, -42.75000000000000000 ) ) ;
#21331 = DIRECTION ( 'NONE',  ( 1.000000000000000000, 0.000000000000000000, 0.000000000000000000 ) ) ;
#21332 = ORIENTED_EDGE ( 'NONE', *, *, #197969, .F. ) ;
#21333 = ORIENTED_EDGE ( 'NONE', *, *, #147446, .T. ) ;
#21334 = DIRECTION ( 'NONE',  ( 0.000000000000000000, 0.000000000000000000, -1.000000000000000000 ) ) ;
#21335 = CARTESIAN_POINT ( 'NONE',  ( 22.60000000000000142, 75.89914163091405896, -215.2726746080137445 ) ) ;
#21336 = ORIENTED_EDGE ( 'NONE', *, *, #251827, .F. ) ;
#21337 = CIRCLE ( 'NONE', #12958, 0.09999999999999982514 ) ;
#21338 = CIRCLE ( 'NONE', #17396, 0.1000000000000062367 ) ;
#21339 = VECTOR ( 'NONE', #196594, 1000.000000000000000 ) ;
#21340 = ORIENTED_EDGE ( 'NONE', *, *, #213599, .T. ) ;
#21341 = VECTOR ( 'NONE', #165771, 1000.000000000000000 ) ;
#21342 = ORIENTED_EDGE ( 'NONE', *, *, #183289, .T. ) ;
#21343 = EDGE_CURVE ( 'NONE', #147844, #248466, #232713, .T. ) ;
#21344 = TOROIDAL_SURFACE ( 'NONE', #121125, 0.6000000000000009770, 0.1000000000000000056 ) ;
#21345 = CARTESIAN_POINT ( 'NONE',  ( 21.04999999999959570, 69.65564095796921151, -203.5379631194175261 ) ) ;
#21346 = CARTESIAN_POINT ( 'NONE',  ( -23.15000000000000213, 85.00000000001197975, -112.9170766071766820 ) ) ;
#21347 = EDGE_CURVE ( 'NONE', #155405, #38095, #47553, .T. ) ;
#21348 = DIRECTION ( 'NONE',  ( -0.000000000000000000, -1.000000000000000000, -6.982962677686266711E-15 ) ) ;
#21349 = FACE_OUTER_BOUND ( 'NONE', #73879, .T. ) ;
#21350 = CARTESIAN_POINT ( 'NONE',  ( 20.95512820512820085, 65.37615131630043663, -162.3581939154368285 ) ) ;
#21351 = CIRCLE ( 'NONE', #42018, 0.09999999999999939493 ) ;
#21352 = DIRECTION ( 'NONE',  ( -1.000000000000000000, 0.000000000000000000, 0.000000000000000000 ) ) ;
#21353 = EDGE_CURVE ( 'NONE', #101212, #222175, #16242, .T. ) ;
#21355 = FACE_OUTER_BOUND ( 'NONE', #156614, .T. ) ;
#21354 = CARTESIAN_POINT ( 'NONE',  ( -18.59999999999999787, 11.75000000001115197, -146.1500000000000341 ) ) ;
#21357 = EDGE_CURVE ( 'NONE', #10791, #96147, #209209, .T. ) ;
#21356 = CARTESIAN_POINT ( 'NONE',  ( 5.899999999999997691, -11.34999999999999964, 13.90000000000000213 ) ) ;
#21358 = FACE_OUTER_BOUND ( 'NONE', #607, .T. ) ;
#21359 = CARTESIAN_POINT ( 'NONE',  ( -21.05000000000000071, 33.13294339707397995, -247.6623911921324463 ) ) ;
#21360 = ORIENTED_EDGE ( 'NONE', *, *, #227454, .F. ) ;
#21362 = VERTEX_POINT ( 'NONE', #214356 ) ;
#21361 = CYLINDRICAL_SURFACE ( 'NONE', #257189, 0.1000000000000002554 ) ;
#21363 = EDGE_CURVE ( 'NONE', #23492, #88928, #235209, .T. ) ;
#21364 = CARTESIAN_POINT ( 'NONE',  ( -20.94999999999999929, -11.65000000000000036, -3.000000000000002665 ) ) ;
#21365 = AXIS2_PLACEMENT_3D ( 'NONE', #230593, #169366, #127633 ) ;
#21366 = CARTESIAN_POINT ( 'NONE',  ( -20.85000000000000142, -4.254329952141549853, -236.2118329068272260 ) ) ;
#21367 = ADVANCED_FACE ( 'NONE', ( #211797 ), #14892, .T. ) ;
#21368 = CARTESIAN_POINT ( 'NONE',  ( -22.47886152344871036, 64.14566162948754879, -247.0891211027675070 ) ) ;
#21369 = ORIENTED_EDGE ( 'NONE', *, *, #156647, .F. ) ;
#21370 = CIRCLE ( 'NONE', #250299, 0.1000000000000028644 ) ;
#21371 = PRODUCT_DEFINITION ( 'UNKNOWN', '', #73925, #139182 ) ;
#21372 = CYLINDRICAL_SURFACE ( 'NONE', #4153, 4.000000000000003553 ) ;
#21373 = TOROIDAL_SURFACE ( 'NONE', #238003, 0.4000000000000017431, 0.1000000000000000056 ) ;
#21374 = DIRECTION ( 'NONE',  ( -1.000000000000000000, 0.000000000000000000, 0.000000000000000000 ) ) ;
#21375 = ORIENTED_EDGE ( 'NONE', *, *, #45711, .F. ) ;
#21376 = CARTESIAN_POINT ( 'NONE',  ( -18.57399277249657032, 10.33112638556969465, -206.5901228926974227 ) ) ;
#21377 = DIRECTION ( 'NONE',  ( 0.000000000000000000, 0.2128009952263485993, -0.9770955615653341697 ) ) ;
#21378 = AXIS2_PLACEMENT_3D ( 'NONE', #173814, #91652, #132060 ) ;
#21379 = DIRECTION ( 'NONE',  ( -1.000000000000000000, -2.952720810173289112E-16, 0.000000000000000000 ) ) ;
#21380 = EDGE_CURVE ( 'NONE', #230778, #171007, #153650, .T. ) ;
#21381 = AXIS2_PLACEMENT_3D ( 'NONE', #182444, #32379, #89733 ) ;
#21382 = EDGE_CURVE ( 'NONE', #60760, #177395, #12179, .T. ) ;
#21383 = CARTESIAN_POINT ( 'NONE',  ( 20.95512820512820440, 40.84069494668059264, -237.9516373772122506 ) ) ;
#21385 = ORIENTED_EDGE ( 'NONE', *, *, #3357, .T. ) ;
#21384 = DIRECTION ( 'NONE',  ( 1.000000000000000000, 2.952720810173289112E-16, -0.000000000000000000 ) ) ;
#21386 = EDGE_CURVE ( 'NONE', #21500, #138858, #74534, .T. ) ;
#21388 = ORIENTED_EDGE ( 'NONE', *, *, #141329, .T. ) ;
#21387 = DIRECTION ( 'NONE',  ( -4.448008912761042820E-16, -1.000000000000000000, -7.116814260417668513E-15 ) ) ;
#21389 = DIRECTION ( 'NONE',  ( 1.000000000000000000, 0.000000000000000000, 0.000000000000000000 ) ) ;
#21391 = VECTOR ( 'NONE', #81291, 1000.000000000000000 ) ;
#21390 = DIRECTION ( 'NONE',  ( 0.000000000000000000, 0.000000000000000000, -1.000000000000000000 ) ) ;
#21392 = DIRECTION ( 'NONE',  ( 0.000000000000000000, -1.000000000000000000, 0.000000000000000000 ) ) ;
#21393 = CARTESIAN_POINT ( 'NONE',  ( 20.95512820512820440, 10.62384868372303615, -74.66491356908764487 ) ) ;
#21395 = DIRECTION ( 'NONE',  ( 1.000000000000000000, 0.000000000000000000, 0.000000000000000000 ) ) ;
#21394 = CARTESIAN_POINT ( 'NONE',  ( -18.37013991200266005, 64.50025238379981829, -78.73008447400728471 ) ) ;
#21396 = DIRECTION ( 'NONE',  ( 0.000000000000000000, -6.853228547068871147E-15, 1.000000000000000000 ) ) ;
#21397 = CARTESIAN_POINT ( 'NONE',  ( -21.05000000000000071, 11.65000000001115232, -40.28386566297815108 ) ) ;
#21398 = EDGE_CURVE ( 'NONE', #194806, #44364, #148945, .T. ) ;
#21400 = CARTESIAN_POINT ( 'NONE',  ( -23.25000000000000355, 70.35000000001224407, -149.1731074845243938 ) ) ;
#21399 = VECTOR ( 'NONE', #19608, 1000.000000000000000 ) ;
#21401 = CYLINDRICAL_SURFACE ( 'NONE', #122619, 0.09999999999999939493 ) ;
#21402 = MANIFOLD_SOLID_BREP ( 'Stock-MAS-200-1', #111536 ) ;
#21403 = CARTESIAN_POINT ( 'NONE',  ( 21.08035267497491105, 10.04573058037006028, -228.1122867900675715 ) ) ;
#21404 = CIRCLE ( 'NONE', #217164, 0.09999999999999892308 ) ;
#21405 = ORIENTED_EDGE ( 'NONE', *, *, #152556, .F. ) ;
#21406 = DIRECTION ( 'NONE',  ( 0.000000000000000000, 0.8814952561688429444, -0.4721928772777348460 ) ) ;
#21407 = ORIENTED_EDGE ( 'NONE', *, *, #223, .T. ) ;
#21408 = VECTOR ( 'NONE', #251061, 1000.000000000000000 ) ;
#21409 = ORIENTED_EDGE ( 'NONE', *, *, #134162, .T. ) ;
#21410 = DIRECTION ( 'NONE',  ( -1.000000000000000000, -2.952720810173289112E-16, 0.000000000000000000 ) ) ;
#21411 = CYLINDRICAL_SURFACE ( 'NONE', #198464, 0.09999999999999939493 ) ;
#21412 = EDGE_LOOP ( 'NONE', ( #179093, #54668, #32942, #201880 ) ) ;
#21413 = AXIS2_PLACEMENT_3D ( 'NONE', #137595, #217127, #218416 ) ;
#21415 = EDGE_CURVE ( 'NONE', #242736, #101417, #35746, .T. ) ;
#21414 = ORIENTED_EDGE ( 'NONE', *, *, #35413, .F. ) ;
#21417 = ORIENTED_EDGE ( 'NONE', *, *, #256871, .F. ) ;
#21416 = TOROIDAL_SURFACE ( 'NONE', #175539, 0.2000000000000000111, 0.1000000000000000056 ) ;
#21418 = FACE_OUTER_BOUND ( 'NONE', #134242, .T. ) ;
#21419 = CIRCLE ( 'NONE', #200461, 0.09999999999999635569 ) ;
#21420 = AXIS2_PLACEMENT_3D ( 'NONE', #132390, #15026, #172852 ) ;
#21421 = VERTEX_POINT ( 'NONE', #73592 ) ;
#21422 = AXIS2_PLACEMENT_3D ( 'NONE', #164948, #206646, #223614 ) ;
#21423 = CARTESIAN_POINT ( 'NONE',  ( -21.14999999999999858, -0.1008583690875562017, -88.75043287651064361 ) ) ;
#21424 = CARTESIAN_POINT ( 'NONE',  ( 18.59999999999999076, -1.851617760457748618, -179.1031897196036766 ) ) ;
#21425 = CARTESIAN_POINT ( 'NONE',  ( -23.15000000000000213, 85.60000000001178933, -79.41707660717668205 ) ) ;
#21426 = DIRECTION ( 'NONE',  ( 1.000000000000000000, 0.000000000000000000, 0.000000000000000000 ) ) ;
#21427 = FACE_OUTER_BOUND ( 'NONE', #203772, .T. ) ;
#21428 = EDGE_CURVE ( 'NONE', #39562, #185781, #94750, .T. ) ;
#21429 = CARTESIAN_POINT ( 'NONE',  ( -20.54999999999999716, 76.00000000001155342, -56.54810748452432279 ) ) ;
#21430 = CARTESIAN_POINT ( 'NONE',  ( -21.45000000000000284, 7.708578643762696636, -21.15000000000000213 ) ) ;
#21432 = ORIENTED_EDGE ( 'NONE', *, *, #37330, .F. ) ;
#21431 = DIRECTION ( 'NONE',  ( 3.469446951953728416E-14, -0.8660254037844309360, 0.5000000000000134337 ) ) ;
#21434 = SPHERICAL_SURFACE ( 'NONE', #33658, 0.1000000000000000056 ) ;
#21433 = CARTESIAN_POINT ( 'NONE',  ( -21.05000000000000071, 0.6171228861679354250, -203.8335771285409521 ) ) ;
#21435 = DIRECTION ( 'NONE',  ( 0.000000000000000000, -1.000000000000000000, 0.000000000000000000 ) ) ;
#21436 = ORIENTED_EDGE ( 'NONE', *, *, #21655, .F. ) ;
#21437 = DIRECTION ( 'NONE',  ( -7.304098846218132695E-16, -0.4721928772777346794, -0.8814952561688431665 ) ) ;
#21439 = EDGE_CURVE ( 'NONE', #146445, #163852, #95680, .T. ) ;
#21438 = LINE ( 'NONE', #22722, #195826 ) ;
#21440 = ORIENTED_EDGE ( 'NONE', *, *, #31507, .F. ) ;
#21442 = CARTESIAN_POINT ( 'NONE',  ( -16.93589915522259304, 65.99137474131613601, -115.5825473825640728 ) ) ;
#21441 = FACE_BOUND ( 'NONE', #203036, .T. ) ;
#21443 = FACE_OUTER_BOUND ( 'NONE', #78575, .T. ) ;
#21444 = ORIENTED_EDGE ( 'NONE', *, *, #230399, .F. ) ;
#21445 = EDGE_CURVE ( 'NONE', #232936, #82222, #136418, .T. ) ;
#21446 = CARTESIAN_POINT ( 'NONE',  ( 21.11833042828145324, 6.445644693866474206, -66.99289949094061569 ) ) ;
#21448 = ADVANCED_FACE ( 'NONE', ( #12327 ), #100777, .T. ) ;
#21447 = DIRECTION ( 'NONE',  ( -1.000000000000000000, -7.304098846218133681E-16, 4.217023435051677994E-16 ) ) ;
#21449 = CARTESIAN_POINT ( 'NONE',  ( 20.94999999999999929, 76.00000000001126921, -203.5231074845248997 ) ) ;
#21450 = LINE ( 'NONE', #200066, #240705 ) ;
#21451 = ORIENTED_EDGE ( 'NONE', *, *, #72982, .T. ) ;
#21452 = AXIS2_PLACEMENT_3D ( 'NONE', #5874, #46289, #4593 ) ;
#21453 = CARTESIAN_POINT ( 'NONE',  ( 21.05000005001280172, 67.12872030824165392, -90.84515989627823274 ) ) ;
#21454 = DIRECTION ( 'NONE',  ( 0.000000000000000000, -1.000000000000000000, -6.982962677686265922E-15 ) ) ;
#21455 = DIRECTION ( 'NONE',  ( 0.000000000000000000, 0.9126074666063772600, 0.4088369013363276627 ) ) ;
#21456 = CARTESIAN_POINT ( 'NONE',  ( -18.50000000000000000, -21.97324378644421117, -224.3523082604776562 ) ) ;
#21458 = ADVANCED_FACE ( 'NONE', ( #132249 ), #81239, .T. ) ;
#21457 = LINE ( 'NONE', #98354, #22247 ) ;
#21459 = CIRCLE ( 'NONE', #183937, 0.09999999999999671652 ) ;
#21461 = ORIENTED_EDGE ( 'NONE', *, *, #40094, .F. ) ;
#21460 = CARTESIAN_POINT ( 'NONE',  ( 21.05543885634738643, 8.775771046858691804, -179.6843844707146616 ) ) ;
#21462 = CARTESIAN_POINT ( 'NONE',  ( -21.05000000000000071, 87.48912529308798014, -106.1231074845242262 ) ) ;
#21463 = CARTESIAN_POINT ( 'NONE',  ( -20.94999999999999929, 11.60000000001115517, -93.57179676972454274 ) ) ;
#21464 = DIRECTION ( 'NONE',  ( -1.000000000000000000, 2.952720810173289112E-16, 2.061873921506763405E-30 ) ) ;
#21465 = ADVANCED_FACE ( 'NONE', ( #237770 ), #77393, .T. ) ;
#21466 = CYLINDRICAL_SURFACE ( 'NONE', #241959, 0.09999999999998898659 ) ;
#21468 = VERTEX_POINT ( 'NONE', #82514 ) ;
#21467 = CARTESIAN_POINT ( 'NONE',  ( 21.09706851349342216, 67.22415748653817502, -57.28754126812474112 ) ) ;
#21469 = DIRECTION ( 'NONE',  ( 0.000000000000000000, 0.000000000000000000, 1.000000000000000000 ) ) ;
#21470 = DIRECTION ( 'NONE',  ( 0.000000000000000000, 0.000000000000000000, -1.000000000000000000 ) ) ;
#21471 = LINE ( 'NONE', #239211, #7408 ) ;
#21472 = VERTEX_POINT ( 'NONE', #120430 ) ;
#21473 = CARTESIAN_POINT ( 'NONE',  ( -21.65000000000000213, 68.75000000001188027, -90.37310748452435405 ) ) ;
#21474 = DIRECTION ( 'NONE',  ( 0.000000000000000000, 1.000000000000000000, 6.853228547068871147E-15 ) ) ;
#21475 = ADVANCED_FACE ( 'NONE', ( #156976 ), #11576, .F. ) ;
#21476 = FACE_OUTER_BOUND ( 'NONE', #136572, .T. ) ;
#21477 = EDGE_CURVE ( 'NONE', #164655, #89756, #174099, .T. ) ;
#21479 = AXIS2_PLACEMENT_3D ( 'NONE', #167669, #171529, #91955 ) ;
#21478 = DIRECTION ( 'NONE',  ( 0.000000000000000000, 0.000000000000000000, -1.000000000000000000 ) ) ;
#21481 = AXIS2_PLACEMENT_3D ( 'NONE', #52757, #12388, #132304 ) ;
#21480 = FACE_OUTER_BOUND ( 'NONE', #214458, .T. ) ;
#21482 = ORIENTED_EDGE ( 'NONE', *, *, #168378, .F. ) ;
#21483 = VERTEX_POINT ( 'NONE', #17434 ) ;
#21484 = DIRECTION ( 'NONE',  ( 0.000000000000000000, 0.000000000000000000, -1.000000000000000000 ) ) ;
#21485 = CARTESIAN_POINT ( 'NONE',  ( -21.05000000000000071, -1.851028230140860487, -11.65391326942249428 ) ) ;
#21486 = CARTESIAN_POINT ( 'NONE',  ( 21.00000000000000000, 9.750000000011153745, -54.75000000000000000 ) ) ;
#21487 = DIRECTION ( 'NONE',  ( -0.1538461538461520228, -0.9536447854760599085, 0.2586367802170949082 ) ) ;
#21488 = EDGE_LOOP ( 'NONE', ( #244772, #88870, #187965, #71 ) ) ;
#21489 = EDGE_CURVE ( 'NONE', #28415, #134853, #141240, .T. ) ;
#21490 = ADVANCED_FACE ( 'NONE', ( #220777 ), #121697, .T. ) ;
#21491 = DIRECTION ( 'NONE',  ( 0.000000000000000000, -0.2128009952263604232, 0.9770955615653316162 ) ) ;
#21492 = CARTESIAN_POINT ( 'NONE',  ( -20.00857864376270001, 66.75000000001230660, -157.6731074845244223 ) ) ;
#21493 = AXIS2_PLACEMENT_3D ( 'NONE', #214849, #115754, #34978 ) ;
#21494 = CARTESIAN_POINT ( 'NONE',  ( -22.39999999999999858, 11.75000000001115552, -67.10000000000005116 ) ) ;
#21495 = CARTESIAN_POINT ( 'NONE',  ( 20.95575313997065336, 10.61455330328599089, -108.1212907019448579 ) ) ;
#21496 = CARTESIAN_POINT ( 'NONE',  ( -16.88705144915421030, 9.949999999999981526, -20.56902140528771739 ) ) ;
#21497 = ORIENTED_EDGE ( 'NONE', *, *, #194735, .T. ) ;
#21499 = ORIENTED_EDGE ( 'NONE', *, *, #43939, .T. ) ;
#21498 = CARTESIAN_POINT ( 'NONE',  ( 20.99999999999999645, 66.25000000001153921, -48.67310748452440095 ) ) ;
#21500 = VERTEX_POINT ( 'NONE', #1712 ) ;
#21501 = CARTESIAN_POINT ( 'NONE',  ( -16.81453563122428818, 9.939100205436954383, -20.78825866064531880 ) ) ;
#21502 = EDGE_LOOP ( 'NONE', ( #63227, #27249, #217470, #34133 ) ) ;
#21503 = DIRECTION ( 'NONE',  ( -1.000000000000000000, 0.000000000000000000, -0.000000000000000000 ) ) ;
#21504 = DIRECTION ( 'NONE',  ( 1.000000000000000000, 0.000000000000000000, 0.000000000000000000 ) ) ;
#21505 = DIRECTION ( 'NONE',  ( 1.000000000000000000, 0.000000000000000000, 0.000000000000000000 ) ) ;
#21506 = ORIENTED_EDGE ( 'NONE', *, *, #187639, .F. ) ;
#21507 = DIRECTION ( 'NONE',  ( 1.000000000000000000, 0.000000000000000000, 0.000000000000000000 ) ) ;
#21508 = DIRECTION ( 'NONE',  ( 0.000000000000000000, 0.1455152366551500653, 0.9893560106964507384 ) ) ;
#21509 = ORIENTED_EDGE ( 'NONE', *, *, #166302, .T. ) ;
#21510 = DIRECTION ( 'NONE',  ( 1.000000000000000000, -2.952720810173289112E-16, -2.061873921506763405E-30 ) ) ;
#21512 = EDGE_LOOP ( 'NONE', ( #207023, #251003, #109555, #191976, #160953, #17798 ) ) ;
#21511 = DIRECTION ( 'NONE',  ( 1.734723475976817507E-14, 0.2128009952263604232, -0.9770955615653316162 ) ) ;
#21513 = AXIS2_PLACEMENT_3D ( 'NONE', #57434, #194420, #79561 ) ;
#21514 = AXIS2_PLACEMENT_3D ( 'NONE', #123433, #142964, #8625 ) ;
#21515 = CARTESIAN_POINT ( 'NONE',  ( 18.39999999999999503, 11.74999999999998224, -20.85000000000000142 ) ) ;
#21516 = DIRECTION ( 'NONE',  ( 0.000000000000000000, 0.000000000000000000, 1.000000000000000000 ) ) ;
#21517 = VECTOR ( 'NONE', #221217, 1000.000000000000000 ) ;
#21518 = EDGE_CURVE ( 'NONE', #194746, #72719, #159532, .T. ) ;
#21519 = VERTEX_POINT ( 'NONE', #99512 ) ;
#21520 = CARTESIAN_POINT ( 'NONE',  ( 18.50000000000000000, 86.35479209693758662, -142.7665665014505407 ) ) ;
#21521 = PLANE ( 'NONE',  #196153 ) ;
#21522 = DIRECTION ( 'NONE',  ( 0.000000000000000000, -0.4999999999999088507, 0.8660254037844913322 ) ) ;
#21523 = ORIENTED_EDGE ( 'NONE', *, *, #79968, .F. ) ;
#21524 = DIRECTION ( 'NONE',  ( 1.000000000000000000, 0.000000000000000000, 0.000000000000000000 ) ) ;
#21525 = DIRECTION ( 'NONE',  ( 0.000000000000000000, 0.000000000000000000, 1.000000000000000000 ) ) ;
#21526 = DIRECTION ( 'NONE',  ( 1.000000000000000000, 0.000000000000000000, -0.000000000000000000 ) ) ;
#21527 = CIRCLE ( 'NONE', #42183, 0.2000000000000057288 ) ;
#21528 = VERTEX_POINT ( 'NONE', #136072 ) ;
#21529 = EDGE_CURVE ( 'NONE', #243534, #51864, #183983, .T. ) ;
#21530 = VERTEX_POINT ( 'NONE', #162107 ) ;
#21531 = ORIENTED_EDGE ( 'NONE', *, *, #66157, .F. ) ;
#21532 = CARTESIAN_POINT ( 'NONE',  ( -20.54999999999999716, 76.00000000001142553, -36.02310748452432421 ) ) ;
#21533 = DIRECTION ( 'NONE',  ( -1.000000000000000000, -0.000000000000000000, -0.000000000000000000 ) ) ;
#21534 = AXIS2_PLACEMENT_3D ( 'NONE', #165012, #202848, #46333 ) ;
#21536 = ORIENTED_EDGE ( 'NONE', *, *, #166842, .F. ) ;
#21535 = DIRECTION ( 'NONE',  ( -1.000000000000000000, 9.012599976028471648E-15, 6.882867235861662930E-14 ) ) ;
#21537 = LINE ( 'NONE', #243134, #40968 ) ;
#21538 = CARTESIAN_POINT ( 'NONE',  ( -18.59999999999999787, 22.43030315632513094, -231.3223027016406093 ) ) ;
#21539 = CARTESIAN_POINT ( 'NONE',  ( -21.64999999999999858, 66.65000000001234071, -160.7731074845244166 ) ) ;
#21540 = DIRECTION ( 'NONE',  ( 1.000000000000000000, 0.000000000000000000, 0.000000000000000000 ) ) ;
#21541 = CARTESIAN_POINT ( 'NONE',  ( -23.15000000000000213, 85.50000000001188027, -93.12913836187179584 ) ) ;
#21542 = AXIS2_PLACEMENT_3D ( 'NONE', #250384, #112182, #151307 ) ;
#21543 = DIRECTION ( 'NONE',  ( -1.000000000000000000, -1.652117596168391700E-15, -1.153667551319263085E-29 ) ) ;
#21544 = EDGE_LOOP ( 'NONE', ( #36391, #145440, #143929, #136186, #145637 ) ) ;
#21546 = EDGE_LOOP ( 'NONE', ( #239473, #102087, #127183 ) ) ;
#21545 = CARTESIAN_POINT ( 'NONE',  ( -20.54999999999999716, 74.07476635515199348, -82.25335101765045920 ) ) ;
#21547 = CARTESIAN_POINT ( 'NONE',  ( 18.49999999999999289, 69.35000000001254250, -182.3731074845244109 ) ) ;
#21548 = ORIENTED_EDGE ( 'NONE', *, *, #13305, .T. ) ;
#21549 = CIRCLE ( 'NONE', #175680, 0.1000000000000111355 ) ;
#21550 = ORIENTED_EDGE ( 'NONE', *, *, #97323, .T. ) ;
#21551 = CARTESIAN_POINT ( 'NONE',  ( 18.79999999999999716, 11.49641995933507665, -1.885425182446133663 ) ) ;
#21552 = DIRECTION ( 'NONE',  ( 1.000000000000000000, -0.000000000000000000, -0.000000000000000000 ) ) ;
#21553 = AXIS2_PLACEMENT_3D ( 'NONE', #26251, #245293, #27562 ) ;
#21554 = DIRECTION ( 'NONE',  ( 0.000000000000000000, -6.982962677686266711E-15, 1.000000000000000000 ) ) ;
#21555 = TOROIDAL_SURFACE ( 'NONE', #83484, 0.2000000000000000111, 0.1000000000000000056 ) ;
#21556 = DIRECTION ( 'NONE',  ( 0.000000000000000000, 0.8777080977375072424, -0.4791956752371691608 ) ) ;
#21557 = DIRECTION ( 'NONE',  ( -0.000000000000000000, 1.000000000000000000, 6.982962677686266711E-15 ) ) ;
#21558 = VECTOR ( 'NONE', #123031, 1000.000000000000000 ) ;
#21559 = DIRECTION ( 'NONE',  ( -1.000000000000000000, 0.000000000000000000, 0.000000000000000000 ) ) ;
#21560 = CIRCLE ( 'NONE', #38316, 0.09999999999999469036 ) ;
#21561 = ORIENTED_EDGE ( 'NONE', *, *, #253632, .F. ) ;
#21562 = ORIENTED_EDGE ( 'NONE', *, *, #164320, .T. ) ;
#21563 = LINE ( 'NONE', #180632, #40056 ) ;
#21564 = EDGE_CURVE ( 'NONE', #143423, #231425, #119928, .T. ) ;
#21565 = VECTOR ( 'NONE', #33446, 1000.000000000000000 ) ;
#21566 = ORIENTED_EDGE ( 'NONE', *, *, #158184, .F. ) ;
#21567 = FACE_OUTER_BOUND ( 'NONE', #201873, .T. ) ;
#21568 = AXIS2_PLACEMENT_3D ( 'NONE', #235465, #157255, #232939 ) ;
#21569 = DIRECTION ( 'NONE',  ( 1.000000000000000000, 0.000000000000000000, 0.000000000000000000 ) ) ;
#21570 = CARTESIAN_POINT ( 'NONE',  ( -13.12432614554023225, 66.56923500458923115, -54.29257008977393895 ) ) ;
#21571 = CIRCLE ( 'NONE', #192437, 11.80000000000000426 ) ;
#21572 = DIRECTION ( 'NONE',  ( -1.000000000000000000, 0.000000000000000000, -0.000000000000000000 ) ) ;
#21573 = EDGE_CURVE ( 'NONE', #13818, #207918, #194745, .T. ) ;
#21574 = ORIENTED_EDGE ( 'NONE', *, *, #86400, .T. ) ;
#21575 = CARTESIAN_POINT ( 'NONE',  ( -18.40000000000000213, 11.75000000001113953, -57.75000000000000711 ) ) ;
#21576 = ORIENTED_EDGE ( 'NONE', *, *, #32785, .T. ) ;
#21578 = CIRCLE ( 'NONE', #92294, 0.1000000000000124678 ) ;
#21577 = CARTESIAN_POINT ( 'NONE',  ( -17.22767730082871296, 10.34924421247856863, -89.14242869057068219 ) ) ;
#21579 = ORIENTED_EDGE ( 'NONE', *, *, #149518, .F. ) ;
#21580 = ADVANCED_FACE ( 'NONE', ( #119117 ), #219831, .T. ) ;
#21581 = DIRECTION ( 'NONE',  ( -2.952720810173289112E-16, 1.000000000000000000, 0.000000000000000000 ) ) ;
#21582 = ORIENTED_EDGE ( 'NONE', *, *, #52588, .T. ) ;
#21583 = DIRECTION ( 'NONE',  ( 1.301042606982683418E-14, -0.8660254037844330455, 0.5000000000000096589 ) ) ;
#21584 = ADVANCED_FACE ( 'NONE', ( #18722 ), #98215, .F. ) ;
#21586 = VERTEX_POINT ( 'NONE', #139932 ) ;
#21585 = CARTESIAN_POINT ( 'NONE',  ( 20.94999999999999929, -11.64999999998883595, -200.9999999999999432 ) ) ;
#21587 = AXIS2_PLACEMENT_3D ( 'NONE', #181871, #184427, #99727 ) ;
#21588 = CARTESIAN_POINT ( 'NONE',  ( -22.39999999999999858, 68.20922040163927136, -203.6231074845244109 ) ) ;
#21590 = ORIENTED_EDGE ( 'NONE', *, *, #112158, .F. ) ;
#21589 = VECTOR ( 'NONE', #113480, 1000.000000000000000 ) ;
#21591 =( BOUNDED_SURFACE ( )  B_SPLINE_SURFACE ( 3, 2, ( 
 ( #233785, #193383, #253324 ),
 ( #111263, #51249, #91693 ),
 ( #115110, #75983, #12183 ),
 ( #155554, #214216, #35606 ) ),
 .UNSPECIFIED., .F., .F., .T. ) 
 B_SPLINE_SURFACE_WITH_KNOTS ( ( 4, 4 ),
 ( 3, 3 ),
 ( 0.04058434257139476031, 0.04256401539001599538 ),
 ( 0.000000000000000000, 1.000000000000000000 ),
 .UNSPECIFIED. ) 
 GEOMETRIC_REPRESENTATION_ITEM ( )  RATIONAL_B_SPLINE_SURFACE ( (
 ( 1.000000000000000000, 0.7103081912007810361, 1.000000000000000000),
 ( 1.000000000000000000, 0.7104998333556750145, 1.000000000000000000),
 ( 1.000000000000000000, 0.7107238315754048630, 1.000000000000000000),
 ( 1.000000000000000000, 0.7110073749539779220, 1.000000000000000000) ) ) 
 REPRESENTATION_ITEM ( '' )  SURFACE ( )  );
#21592 = AXIS2_PLACEMENT_3D ( 'NONE', #120928, #143003, #200437 ) ;
#21593 = VECTOR ( 'NONE', #152594, 1000.000000000000000 ) ;
#21594 = CARTESIAN_POINT ( 'NONE',  ( 23.14999999999999858, 4.813084112160684214, -55.05848224347618469 ) ) ;
#21595 = ORIENTED_EDGE ( 'NONE', *, *, #21670, .F. ) ;
#21596 = CARTESIAN_POINT ( 'NONE',  ( 23.25000000000000000, 49.36776662947724503, -253.7196102226803021 ) ) ;
#21597 = EDGE_CURVE ( 'NONE', #207925, #175274, #21321, .T. ) ;
#21598 = CARTESIAN_POINT ( 'NONE',  ( -21.29999999999995808, 76.00000000001165290, -69.52310748452431710 ) ) ;
#21599 = DIRECTION ( 'NONE',  ( 1.000000000000000000, 0.000000000000000000, 0.000000000000000000 ) ) ;
#21600 = CARTESIAN_POINT ( 'NONE',  ( -16.94062896051973865, 66.00728089491089179, -56.92059094240559602 ) ) ;
#21601 = DIRECTION ( 'NONE',  ( -0.000000000000000000, -6.982962677686266711E-15, 1.000000000000000000 ) ) ;
#21602 = ORIENTED_EDGE ( 'NONE', *, *, #171245, .F. ) ;
#21603 = CARTESIAN_POINT ( 'NONE',  ( 18.59999999999999076, 68.59681812508419796, -224.1344059333694361 ) ) ;
#21604 = DIRECTION ( 'NONE',  ( 0.000000000000000000, 0.000000000000000000, -1.000000000000000000 ) ) ;
#21605 = LINE ( 'NONE', #209210, #217717 ) ;
#21606 = ORIENTED_EDGE ( 'NONE', *, *, #224601, .F. ) ;
#21608 = CARTESIAN_POINT ( 'NONE',  ( 20.93302460841143287, 68.06642993404715014, -224.1774859612004036 ) ) ;
#21607 = AXIS2_PLACEMENT_3D ( 'NONE', #115009, #170218, #55009 ) ;
#21609 = ORIENTED_EDGE ( 'NONE', *, *, #81415, .T. ) ;
#21610 = CARTESIAN_POINT ( 'NONE',  ( 20.90000000000000213, -1.885425182446133885, -11.49641995933507843 ) ) ;
#21611 = ORIENTED_EDGE ( 'NONE', *, *, #44350, .F. ) ;
#21612 = CARTESIAN_POINT ( 'NONE',  ( -21.78635804494510708, 68.96433851485950584, -203.6221125500320852 ) ) ;
#21613 = CARTESIAN_POINT ( 'NONE',  ( -16.87036670365547408, 66.01058118071090064, -182.5435473672224305 ) ) ;
#21614 = VERTEX_POINT ( 'NONE', #126811 ) ;
#21616 = ORIENTED_EDGE ( 'NONE', *, *, #88512, .T. ) ;
#21615 = FACE_OUTER_BOUND ( 'NONE', #158364, .T. ) ;
#21617 = CARTESIAN_POINT ( 'NONE',  ( -18.39999999999999858, 13.19494617735151465, -207.6708402378485516 ) ) ;
#21618 = ORIENTED_EDGE ( 'NONE', *, *, #56877, .T. ) ;
#21619 = DIRECTION ( 'NONE',  ( 1.000000000000000000, -0.000000000000000000, -0.000000000000000000 ) ) ;
#21620 = FACE_OUTER_BOUND ( 'NONE', #40657, .T. ) ;
#21621 = ORIENTED_EDGE ( 'NONE', *, *, #210676, .F. ) ;
#21622 = EDGE_LOOP ( 'NONE', ( #60268, #226761, #55929, #40017 ) ) ;
#21623 = FACE_OUTER_BOUND ( 'NONE', #229291, .T. ) ;
#21624 = DIRECTION ( 'NONE',  ( 1.000000000000000000, 0.000000000000000000, 0.000000000000000000 ) ) ;
#21625 = ORIENTED_EDGE ( 'NONE', *, *, #89025, .F. ) ;
#21626 = FACE_OUTER_BOUND ( 'NONE', #152731, .T. ) ;
#21627 = ORIENTED_EDGE ( 'NONE', *, *, #196634, .T. ) ;
#21628 = ORIENTED_EDGE ( 'NONE', *, *, #22438, .T. ) ;
#21629 = ADVANCED_FACE ( 'NONE', ( #223324 ), #157332, .T. ) ;
#21630 = VECTOR ( 'NONE', #139452, 1000.000000000000000 ) ;
#21631 = CYLINDRICAL_SURFACE ( 'NONE', #143074, 0.1000000000000124678 ) ;
#21633 = EDGE_CURVE ( 'NONE', #129900, #146108, #3162, .T. ) ;
#21632 =( BOUNDED_CURVE ( )  B_SPLINE_CURVE ( 3, ( #150677, #88097, #230204, #191106 ),
 .UNSPECIFIED., .F., .F. ) 
 B_SPLINE_CURVE_WITH_KNOTS ( ( 4, 4 ),
 ( -7.815970093361102045E-14, 1.570796326794882125 ),
 .UNSPECIFIED. ) 
 CURVE ( )  GEOMETRIC_REPRESENTATION_ITEM ( )  RATIONAL_B_SPLINE_CURVE ( ( 1.000000000000000000, 0.8047378541243499495, 0.8047378541243499495, 1.000000000000000000 ) ) 
 REPRESENTATION_ITEM ( '' )  );
#21635 = VERTEX_POINT ( 'NONE', #185503 ) ;
#21634 = DIRECTION ( 'NONE',  ( 0.000000000000000000, 6.982962677686266711E-15, -1.000000000000000000 ) ) ;
#21636 = CARTESIAN_POINT ( 'NONE',  ( -18.40000000000000213, 64.52683809665013825, -190.9145288407617613 ) ) ;
#21637 = CARTESIAN_POINT ( 'NONE',  ( 23.25000000000000000, 11.75000000001116263, -188.8499999999999659 ) ) ;
#21638 = DIRECTION ( 'NONE',  ( -0.7071067811865388020, 0.7071067811865561215, 0.000000000000000000 ) ) ;
#21640 = CARTESIAN_POINT ( 'NONE',  ( 21.05000000000000071, 1.115600667400684642E-11, -167.4999999999999716 ) ) ;
#21639 = CARTESIAN_POINT ( 'NONE',  ( -17.29838795458446654, 65.62845014206513383, -125.1278487671420834 ) ) ;
#21642 = EDGE_CURVE ( 'NONE', #141973, #251583, #188072, .T. ) ;
#21641 = DIRECTION ( 'NONE',  ( 0.000000000000000000, 0.9999631594459056361, -0.008583690987128059571 ) ) ;
#21643 = CARTESIAN_POINT ( 'NONE',  ( -21.05000000000000071, 11.65000000000000036, -26.48519422934605316 ) ) ;
#21644 = AXIS2_PLACEMENT_3D ( 'NONE', #238542, #143291, #139423 ) ;
#21645 = CARTESIAN_POINT ( 'NONE',  ( 22.39999999999999503, 30.91424406532124181, -252.0151325879369040 ) ) ;
#21646 = CARTESIAN_POINT ( 'NONE',  ( 22.50000000000000355, -3.119487940400186954, -228.1911993711476043 ) ) ;
#21647 = CIRCLE ( 'NONE', #42475, 0.09999999999999820144 ) ;
#21648 = ORIENTED_EDGE ( 'NONE', *, *, #252186, .T. ) ;
#21649 = ORIENTED_EDGE ( 'NONE', *, *, #84168, .F. ) ;
#21650 = VERTEX_POINT ( 'NONE', #186802 ) ;
#21651 = CARTESIAN_POINT ( 'NONE',  ( -20.85000000000000142, -1.164121893230052995, -141.9148480855716343 ) ) ;
#21652 = EDGE_CURVE ( 'NONE', #37720, #144144, #7453, .T. ) ;
#21653 = VERTEX_POINT ( 'NONE', #83784 ) ;
#21654 = CARTESIAN_POINT ( 'NONE',  ( -16.88815647973234135, 9.950832619326892114, -146.6472170633260248 ) ) ;
#21655 = EDGE_CURVE ( 'NONE', #168071, #146129, #147660, .T. ) ;
#21656 = ADVANCED_FACE ( 'NONE', ( #207651 ), #86541, .T. ) ;
#21657 = EDGE_LOOP ( 'NONE', ( #245248, #49385, #41429, #96026 ) ) ;
#21658 = TOROIDAL_SURFACE ( 'NONE', #200729, 12.97499999999999609, 0.1000000000000000056 ) ;
#21659 = CARTESIAN_POINT ( 'NONE',  ( 20.92356734117541706, 65.68026841930924320, -130.9725740131889893 ) ) ;
#21661 = ORIENTED_EDGE ( 'NONE', *, *, #120290, .T. ) ;
#21660 = ORIENTED_EDGE ( 'NONE', *, *, #257521, .T. ) ;
#21662 = ORIENTED_EDGE ( 'NONE', *, *, #120871, .F. ) ;
#21663 = VERTEX_POINT ( 'NONE', #205036 ) ;
#21664 = EDGE_CURVE ( 'NONE', #62333, #6765, #169819, .T. ) ;
#21665 = DIRECTION ( 'NONE',  ( -0.8049926720990042694, -0.5932847527679310229, 0.000000000000000000 ) ) ;
#21666 = CARTESIAN_POINT ( 'NONE',  ( -23.15000000000000213, 4.350000000011156054, -188.6499999999999488 ) ) ;
#21668 = VERTEX_POINT ( 'NONE', #182950 ) ;
#21667 = DIRECTION ( 'NONE',  ( -0.000000000000000000, 0.4721928772777345684, 0.8814952561688429444 ) ) ;
#21669 = LINE ( 'NONE', #27802, #149314 ) ;
#21670 = EDGE_CURVE ( 'NONE', #241932, #113797, #232341, .T. ) ;
#21671 = CARTESIAN_POINT ( 'NONE',  ( 19.97071067811865674, 11.72071067812981937, -158.6500000000000057 ) ) ;
#21673 = EDGE_LOOP ( 'NONE', ( #133428, #79857, #111775, #59943 ) ) ;
#21672 = CARTESIAN_POINT ( 'NONE',  ( -21.14999999999999858, 1.115600667400684642E-11, -167.4999999999999716 ) ) ;
#21675 = ADVANCED_FACE ( 'NONE', ( #29038, #168559 ), #244171, .T. ) ;
#21674 = ORIENTED_EDGE ( 'NONE', *, *, #35523, .F. ) ;
#21676 = FACE_OUTER_BOUND ( 'NONE', #150336, .T. ) ;
#21678 = EDGE_LOOP ( 'NONE', ( #181864, #181571, #105753, #140725 ) ) ;
#21677 = CARTESIAN_POINT ( 'NONE',  ( -18.59999999999999787, 74.83729825007462466, -195.4231074845243654 ) ) ;
#21679 = CARTESIAN_POINT ( 'NONE',  ( 23.14999999999999503, 64.25000000001199396, -115.2731074845243739 ) ) ;
#21680 = CARTESIAN_POINT ( 'NONE',  ( -15.06720934482788543, 27.56753475832528011, -233.9973862756307312 ) ) ;
#21681 = VECTOR ( 'NONE', #162992, 1000.000000000000000 ) ;
#21682 = AXIS2_PLACEMENT_3D ( 'NONE', #189534, #232526, #231238 ) ;
#21683 = CARTESIAN_POINT ( 'NONE',  ( -20.85000000000000142, 77.13501884592258762, -162.3061306010920362 ) ) ;
#21684 = CIRCLE ( 'NONE', #229781, 0.09999999999998898659 ) ;
#21685 = ORIENTED_EDGE ( 'NONE', *, *, #147453, .F. ) ;
#21687 = DIRECTION ( 'NONE',  ( 0.000000000000000000, 0.9126074666063770380, 0.4088369013363281068 ) ) ;
#21686 = CARTESIAN_POINT ( 'NONE',  ( 20.02499999999999858, 66.25000000001199396, -115.3731074845243683 ) ) ;
#21688 = DIRECTION ( 'NONE',  ( 0.000000000000000000, 0.8814952561688368382, -0.4721928772777462813 ) ) ;
#21689 = DIRECTION ( 'NONE',  ( -1.000000000000000000, -0.000000000000000000, -0.000000000000000000 ) ) ;
#21690 = CARTESIAN_POINT ( 'NONE',  ( 23.14999999999999858, 72.10000000001244302, -170.0231074845243882 ) ) ;
#21691 = DIRECTION ( 'NONE',  ( 0.000000000000000000, -0.9908441862701610203, 0.1350103645451807555 ) ) ;
#21692 = EDGE_LOOP ( 'NONE', ( #239750, #214022, #143484, #20644, #2226 ) ) ;
#21693 = VERTEX_POINT ( 'NONE', #86363 ) ;
#21694 = ORIENTED_EDGE ( 'NONE', *, *, #102054, .T. ) ;
#21695 = DIRECTION ( 'NONE',  ( 0.000000000000000000, -1.000000000000000000, -0.000000000000000000 ) ) ;
#21697 = ORIENTED_EDGE ( 'NONE', *, *, #61779, .F. ) ;
#21696 = EDGE_CURVE ( 'NONE', #203694, #175678, #57326, .T. ) ;
#21698 = DIRECTION ( 'NONE',  ( 0.000000000000000000, 0.000000000000000000, -1.000000000000000000 ) ) ;
#21699 = ORIENTED_EDGE ( 'NONE', *, *, #51324, .F. ) ;
#21700 = EDGE_CURVE ( 'NONE', #84696, #20356, #190646, .T. ) ;
#21701 = CARTESIAN_POINT ( 'NONE',  ( -18.60000000000001208, -7.621793812739404039, -210.0085087240642565 ) ) ;
#21702 = CARTESIAN_POINT ( 'NONE',  ( -21.00023020733502577, 76.00000000001243450, -176.4139767297927222 ) ) ;
#21703 = AXIS2_PLACEMENT_3D ( 'NONE', #198817, #20199, #26631 ) ;
#21705 = ADVANCED_FACE ( 'NONE', ( #66841 ), #88948, .F. ) ;
#21704 = ORIENTED_EDGE ( 'NONE', *, *, #11627, .F. ) ;
#21706 = DIRECTION ( 'NONE',  ( 0.000000000000000000, 2.664535259100315349E-15, -1.000000000000000000 ) ) ;
#21707 = AXIS2_PLACEMENT_3D ( 'NONE', #120154, #118846, #82231 ) ;
#21708 = VERTEX_POINT ( 'NONE', #142503 ) ;
#21709 = ORIENTED_EDGE ( 'NONE', *, *, #4805, .F. ) ;
#21710 = EDGE_LOOP ( 'NONE', ( #209489, #146918, #214353, #205108 ) ) ;
#21711 = DIRECTION ( 'NONE',  ( -4.239556034732055511E-17, -0.3848449534832868446, -0.9229812358755982160 ) ) ;
#21712 = FACE_OUTER_BOUND ( 'NONE', #28908, .T. ) ;
#21713 = LINE ( 'NONE', #226297, #30131 ) ;
#21714 = DIRECTION ( 'NONE',  ( 1.000000000000000000, -7.304098846218135653E-16, 0.000000000000000000 ) ) ;
#21715 = CARTESIAN_POINT ( 'NONE',  ( -21.10257677756357708, 61.04944212076151189, -234.2044117394509044 ) ) ;
#21716 = LINE ( 'NONE', #84182, #26305 ) ;
#21717 = VECTOR ( 'NONE', #179755, 1000.000000000000000 ) ;
#21719 = CARTESIAN_POINT ( 'NONE',  ( -18.59999999999999787, 11.65000000001115232, -74.01480577065404987 ) ) ;
#21718 = CARTESIAN_POINT ( 'NONE',  ( 18.50000000000000000, -9.399999999988843058, -207.8820418481726620 ) ) ;
#21720 = CARTESIAN_POINT ( 'NONE',  ( 20.85000000000000142, -11.64999999998883595, -167.5000000000000000 ) ) ;
#21722 = ORIENTED_EDGE ( 'NONE', *, *, #52655, .T. ) ;
#21721 = LINE ( 'NONE', #159963, #198150 ) ;
#21723 = CARTESIAN_POINT ( 'NONE',  ( -16.92925196614875816, 12.42877699685184112, -211.2056432611043135 ) ) ;
#21724 = CARTESIAN_POINT ( 'NONE',  ( -18.54159361262949801, -9.463132135481945539, -141.0491222162928864 ) ) ;
#21725 = ORIENTED_EDGE ( 'NONE', *, *, #39908, .T. ) ;
#21726 = ORIENTED_EDGE ( 'NONE', *, *, #226467, .F. ) ;
#21727 = CARTESIAN_POINT ( 'NONE',  ( 18.59999999999999787, -11.65000000000000036, 5.900000000000001243 ) ) ;
#21728 = CIRCLE ( 'NONE', #167488, 11.90000000000000213 ) ;
#21729 = CARTESIAN_POINT ( 'NONE',  ( -21.07946286933445279, 69.67096268100397083, -69.59979132778077826 ) ) ;
#21731 = ADVANCED_FACE ( 'NONE', ( #48552 ), #144819, .T. ) ;
#21730 = CYLINDRICAL_SURFACE ( 'NONE', #83142, 0.09999999999999939493 ) ;
#21732 = VERTEX_POINT ( 'NONE', #43424 ) ;
#21733 = CIRCLE ( 'NONE', #150889, 0.1000000000000124678 ) ;
#21734 = CIRCLE ( 'NONE', #84199, 0.09999999999999939493 ) ;
#21735 = EDGE_CURVE ( 'NONE', #101690, #47640, #251560, .T. ) ;
#21736 = AXIS2_PLACEMENT_3D ( 'NONE', #86376, #249353, #190678 ) ;
#21737 = DIRECTION ( 'NONE',  ( 0.000000000000000000, 0.000000000000000000, 1.000000000000000000 ) ) ;
#21738 = AXIS2_PLACEMENT_3D ( 'NONE', #48056, #225395, #29820 ) ;
#21739 = ORIENTED_EDGE ( 'NONE', *, *, #95128, .T. ) ;
#21740 = ORIENTED_EDGE ( 'NONE', *, *, #204991, .F. ) ;
#21741 = EDGE_CURVE ( 'NONE', #138184, #252796, #40811, .T. ) ;
#21743 = EDGE_CURVE ( 'NONE', #5518, #56976, #252045, .T. ) ;
#21742 = CARTESIAN_POINT ( 'NONE',  ( -18.50000000000000000, -9.399999999988850163, -107.3820418481727046 ) ) ;
#21744 = ORIENTED_EDGE ( 'NONE', *, *, #252508, .T. ) ;
#21745 = CARTESIAN_POINT ( 'NONE',  ( -16.93906926870270624, 60.85410600414655136, -221.1186421532144379 ) ) ;
#21746 = DIRECTION ( 'NONE',  ( 0.000000000000000000, 0.000000000000000000, 1.000000000000000000 ) ) ;
#21747 = CYLINDRICAL_SURFACE ( 'NONE', #248921, 0.09999999999998898659 ) ;
#21748 = CARTESIAN_POINT ( 'NONE',  ( -21.05000000000000071, 1.750000000011155743, -179.1695115579016147 ) ) ;
#21749 = EDGE_LOOP ( 'NONE', ( #152439, #86766, #220408, #142154 ) ) ;
#21750 = EDGE_CURVE ( 'NONE', #91227, #197213, #186542, .T. ) ;
#21751 = VECTOR ( 'NONE', #161548, 1000.000000000000000 ) ;
#21753 = AXIS2_PLACEMENT_3D ( 'NONE', #6660, #69235, #27560 ) ;
#21752 = DIRECTION ( 'NONE',  ( -6.938893903907222856E-15, -1.000000000000000000, -6.982962677686266711E-15 ) ) ;
#21754 = DIRECTION ( 'NONE',  ( -1.000000000000000000, -0.000000000000000000, -0.000000000000000000 ) ) ;
#21755 = CIRCLE ( 'NONE', #55037, 0.1999999999999987899 ) ;
#21756 = DIRECTION ( 'NONE',  ( 0.000000000000000000, 0.2128009952263601456, -0.9770955615653316162 ) ) ;
#21757 = CIRCLE ( 'NONE', #200817, 0.1000000000000028644 ) ;
#21758 = EDGE_CURVE ( 'NONE', #68838, #253474, #157525, .T. ) ;
#21759 = ORIENTED_EDGE ( 'NONE', *, *, #196998, .F. ) ;
#21760 = ADVANCED_FACE ( 'NONE', ( #90227 ), #151537, .F. ) ;
#21761 = VECTOR ( 'NONE', #24342, 1000.000000000000000 ) ;
#21763 = ORIENTED_EDGE ( 'NONE', *, *, #207928, .T. ) ;
#21762 = CARTESIAN_POINT ( 'NONE',  ( -18.59999999999999787, 77.16412189325305349, -95.10825939895268277 ) ) ;
#21764 = DIRECTION ( 'NONE',  ( 1.000000000000000000, 0.000000000000000000, -0.000000000000000000 ) ) ;
#21765 = CARTESIAN_POINT ( 'NONE',  ( 18.49713797159830264, 78.19937966003901408, -231.5028605801859385 ) ) ;
#21766 = ADVANCED_FACE ( 'NONE', ( #152827 ), #148961, .F. ) ;
#21767 = VECTOR ( 'NONE', #107825, 1000.000000000000000 ) ;
#21768 = DIRECTION ( 'NONE',  ( -1.000000000000000000, 0.000000000000000000, 0.000000000000000000 ) ) ;
#21769 = DIRECTION ( 'NONE',  ( 0.000000000000000000, -1.000000000000000000, 0.000000000000000000 ) ) ;
#21770 = DIRECTION ( 'NONE',  ( 1.000000000000000000, 0.000000000000000000, 0.000000000000000000 ) ) ;
#21771 = ORIENTED_EDGE ( 'NONE', *, *, #133585, .T. ) ;
#21772 = CARTESIAN_POINT ( 'NONE',  ( -16.89318236219975944, 63.08559331870877429, -213.1222689416267428 ) ) ;
#21773 = CARTESIAN_POINT ( 'NONE',  ( -23.15000000000000213, 76.00000000001168132, -65.52310748452430289 ) ) ;
#21774 = CARTESIAN_POINT ( 'NONE',  ( -18.43459694179565744, 77.15158635572022661, -241.8143376528992405 ) ) ;
#21775 = DIRECTION ( 'NONE',  ( -0.7071067811865487940, 0.7071067811865463515, 0.000000000000000000 ) ) ;
#21776 = ADVANCED_FACE ( 'NONE', ( #52389 ), #69422, .T. ) ;
#21777 = LINE ( 'NONE', #92620, #189915 ) ;
#21778 = AXIS2_PLACEMENT_3D ( 'NONE', #11525, #71509, #151030 ) ;
#21779 = LINE ( 'NONE', #20498, #169924 ) ;
#21780 = AXIS2_PLACEMENT_3D ( 'NONE', #162305, #241820, #146553 ) ;
#21781 = AXIS2_PLACEMENT_3D ( 'NONE', #58571, #1163, #117289 ) ;
#21782 = EDGE_LOOP ( 'NONE', ( #127147, #108894, #28485, #217704 ) ) ;
#21783 = ORIENTED_EDGE ( 'NONE', *, *, #30463, .F. ) ;
#21784 = LINE ( 'NONE', #84248, #166542 ) ;
#21785 = DIRECTION ( 'NONE',  ( 1.000000000000000000, 0.000000000000000000, 0.000000000000000000 ) ) ;
#21786 = ADVANCED_FACE ( 'NONE', ( #54947 ), #240684, .T. ) ;
#21787 = DIRECTION ( 'NONE',  ( 0.000000000000000000, 0.000000000000000000, 1.000000000000000000 ) ) ;
#21788 = ORIENTED_EDGE ( 'NONE', *, *, #201465, .F. ) ;
#21790 = EDGE_CURVE ( 'NONE', #18045, #135942, #3335, .T. ) ;
#21789 = CARTESIAN_POINT ( 'NONE',  ( 23.14999999999999858, 80.00000000001142553, -36.02310748452429578 ) ) ;
#21791 = EDGE_CURVE ( 'NONE', #129045, #52293, #190662, .T. ) ;
#21792 = DIRECTION ( 'NONE',  ( 1.000000000000000000, 0.000000000000000000, 0.000000000000000000 ) ) ;
#21793 = DIRECTION ( 'NONE',  ( 0.000000000000000000, 0.000000000000000000, 1.000000000000000000 ) ) ;
#21794 = LINE ( 'NONE', #97433, #203741 ) ;
#21795 = AXIS2_PLACEMENT_3D ( 'NONE', #32647, #152585, #153890 ) ;
#21796 = VERTEX_POINT ( 'NONE', #194509 ) ;
#21797 = CARTESIAN_POINT ( 'NONE',  ( -18.59999999999999787, 1.115600667400684642E-11, -67.00000000000000000 ) ) ;
#21798 = ORIENTED_EDGE ( 'NONE', *, *, #49334, .T. ) ;
#21799 = EDGE_CURVE ( 'NONE', #163909, #193526, #45054, .T. ) ;
#21800 = DIRECTION ( 'NONE',  ( 1.000000000000000000, 0.000000000000000000, 0.000000000000000000 ) ) ;
#21801 = CARTESIAN_POINT ( 'NONE',  ( -23.15000000000000213, 1.627786319807483340, -244.0021210468063089 ) ) ;
#21802 = CARTESIAN_POINT ( 'NONE',  ( -21.05000000000000071, 10.21728496540351827, -227.9671432372868480 ) ) ;
#21803 = CARTESIAN_POINT ( 'NONE',  ( -20.54999999999999716, 4.350000000011156054, -88.15000000000004832 ) ) ;
#21804 = DIRECTION ( 'NONE',  ( 0.000000000000000000, 0.01562499999998609446, -0.9998779222360101304 ) ) ;
#21805 = DIRECTION ( 'NONE',  ( -1.000000000000000000, 0.000000000000000000, -0.000000000000000000 ) ) ;
#21806 = FACE_OUTER_BOUND ( 'NONE', #106533, .T. ) ;
#21807 = CARTESIAN_POINT ( 'NONE',  ( -18.40000000000000213, 64.66825945288634614, -48.67310748452440805 ) ) ;
#21808 = LINE ( 'NONE', #160049, #108163 ) ;
#21809 = EDGE_CURVE ( 'NONE', #9452, #218469, #146546, .T. ) ;
#21810 = CARTESIAN_POINT ( 'NONE',  ( -22.50000000000000000, 11.65000000001115588, -67.00000000000004263 ) ) ;
#21811 = CARTESIAN_POINT ( 'NONE',  ( -18.69999999999999929, -10.80884033489985363, 5.900000000000001243 ) ) ;
#21812 = MANIFOLD_SOLID_BREP ( 'Stock-MAS-200-1', #178192 ) ;
#21813 = DIRECTION ( 'NONE',  ( 0.000000000000000000, 1.000000000000000000, 0.000000000000000000 ) ) ;
#21814 = FACE_OUTER_BOUND ( 'NONE', #221731, .T. ) ;
#21815 = AXIS2_PLACEMENT_3D ( 'NONE', #112857, #209385, #248511 ) ;
#21816 = ORIENTED_EDGE ( 'NONE', *, *, #167862, .F. ) ;
#21817 = DIRECTION ( 'NONE',  ( 1.000000000000000000, 0.000000000000000000, 0.000000000000000000 ) ) ;
#21818 = DIRECTION ( 'NONE',  ( 0.000000000000000000, 0.000000000000000000, -1.000000000000000000 ) ) ;
#21819 = EDGE_CURVE ( 'NONE', #192257, #113536, #120109, .T. ) ;
#21820 = ORIENTED_EDGE ( 'NONE', *, *, #8766, .F. ) ;
#21821 = CARTESIAN_POINT ( 'NONE',  ( -22.46246831459151494, 0.02191216695058596786, -55.35013543879008324 ) ) ;
#21822 = FACE_OUTER_BOUND ( 'NONE', #23756, .T. ) ;
#21823 = ORIENTED_EDGE ( 'NONE', *, *, #23974, .T. ) ;
#21824 = CARTESIAN_POINT ( 'NONE',  ( -16.88460203013676875, 9.954759003246872240, -188.3658918095381978 ) ) ;
#21825 = DIRECTION ( 'NONE',  ( 0.000000000000000000, 0.000000000000000000, -1.000000000000000000 ) ) ;
#21826 = AXIS2_PLACEMENT_3D ( 'NONE', #4735, #140406, #2172 ) ;
#21827 = ADVANCED_FACE ( 'NONE', ( #254430 ), #215726, .F. ) ;
#21828 = VERTEX_POINT ( 'NONE', #118 ) ;
#21829 = VECTOR ( 'NONE', #162973, 1000.000000000000000 ) ;
#21830 = ORIENTED_EDGE ( 'NONE', *, *, #241961, .T. ) ;
#21831 = CARTESIAN_POINT ( 'NONE',  ( -18.59999999999999787, 79.14291928130900544, -196.3819507745080557 ) ) ;
#21832 = VECTOR ( 'NONE', #27190, 1000.000000000000000 ) ;
#21833 = EDGE_LOOP ( 'NONE', ( #18504, #21461, #159516, #7430 ) ) ;
#21834 = DIRECTION ( 'NONE',  ( -1.000000000000000000, -0.000000000000000000, -0.000000000000000000 ) ) ;
#21835 = CARTESIAN_POINT ( 'NONE',  ( -21.44999999999999929, 7.350000000011155166, -121.7500000000000426 ) ) ;
#21837 = CARTESIAN_POINT ( 'NONE',  ( 21.08621493067296271, 34.01181478797902713, -243.7797238474834387 ) ) ;
#21836 = UNCERTAINTY_MEASURE_WITH_UNIT (LENGTH_MEASURE( 1.000000000000000082E-05 ), #201303, 'distance_accuracy_value', 'NONE');
#21838 = DIRECTION ( 'NONE',  ( -4.448008912761042820E-16, -1.000000000000000000, -7.116814260417668513E-15 ) ) ;
#21839 = DIRECTION ( 'NONE',  ( 0.000000000000000000, 0.1350103645451946055, -0.9908441862701591329 ) ) ;
#21840 = DIRECTION ( 'NONE',  ( 1.000000000000000000, 0.000000000000000000, -0.000000000000000000 ) ) ;
#21841 = AXIS2_PLACEMENT_3D ( 'NONE', #257316, #256030, #235240 ) ;
#21842 = FACE_OUTER_BOUND ( 'NONE', #75070, .T. ) ;
#21844 = FACE_BOUND ( 'NONE', #176956, .T. ) ;
#21843 = AXIS2_PLACEMENT_3D ( 'NONE', #71630, #233282, #14232 ) ;
#21846 = ORIENTED_EDGE ( 'NONE', *, *, #115623, .F. ) ;
#21845 = CARTESIAN_POINT ( 'NONE',  ( -18.49719636458551264, -9.446365359216914115, -40.57161386988322249 ) ) ;
#21847 = ORIENTED_EDGE ( 'NONE', *, *, #177706, .T. ) ;
#21849 = DIRECTION ( 'NONE',  ( 1.000000000000000000, 0.000000000000000000, 0.000000000000000000 ) ) ;
#21848 = CARTESIAN_POINT ( 'NONE',  ( -22.39999999999999858, 1.115600667400684642E-11, -100.4000000000000341 ) ) ;
#21851 = ORIENTED_EDGE ( 'NONE', *, *, #250783, .F. ) ;
#21850 = CARTESIAN_POINT ( 'NONE',  ( 20.95083306685154056, 8.916842641901356004, -108.9773248532583807 ) ) ;
#21852 = ORIENTED_EDGE ( 'NONE', *, *, #241196, .T. ) ;
#21853 = CARTESIAN_POINT ( 'NONE',  ( -16.91776028072577631, 66.03659960638248094, -149.1480834698222964 ) ) ;
#21854 = CARTESIAN_POINT ( 'NONE',  ( -23.25000000000000000, -11.64999999998884483, -97.50000000000004263 ) ) ;
#21855 = CARTESIAN_POINT ( 'NONE',  ( -18.50000000000000000, 11.65000000001115232, -21.75000000000000355 ) ) ;
#21856 = CIRCLE ( 'NONE', #17727, 0.1999999999999893807 ) ;
#21857 = DIRECTION ( 'NONE',  ( 0.000000000000000000, -0.9893560106964500722, 0.1455152366551550613 ) ) ;
#21858 = DIRECTION ( 'NONE',  ( -1.000000000000000000, 0.000000000000000000, 0.000000000000000000 ) ) ;
#21859 = DIRECTION ( 'NONE',  ( 1.000000000000000000, 0.000000000000000000, 0.000000000000000000 ) ) ;
#21860 = TOROIDAL_SURFACE ( 'NONE', #113622, 0.2000000000000000111, 0.1000000000000000056 ) ;
#21861 = AXIS2_PLACEMENT_3D ( 'NONE', #88221, #247316, #111666 ) ;
#21863 = ADVANCED_FACE ( 'NONE', ( #120123 ), #86720, .F. ) ;
#21862 = CIRCLE ( 'NONE', #80259, 0.1000000000000028644 ) ;
#21865 = AXIS2_PLACEMENT_3D ( 'NONE', #38158, #134645, #137235 ) ;
#21864 = CARTESIAN_POINT ( 'NONE',  ( -21.06715728752538652, 11.75000000001115197, -74.01480577065406408 ) ) ;
#21866 = ORIENTED_EDGE ( 'NONE', *, *, #22698, .F. ) ;
#21867 = ORIENTED_EDGE ( 'NONE', *, *, #219268, .T. ) ;
#21868 = PLANE ( 'NONE',  #206432 ) ;
#21869 = ORIENTED_EDGE ( 'NONE', *, *, #162010, .T. ) ;
#21870 = CARTESIAN_POINT ( 'NONE',  ( 21.07928932188134041, 0.09889514566578937182, -27.17148334360129169 ) ) ;
#21871 = VERTEX_POINT ( 'NONE', #19715 ) ;
#21872 = DIRECTION ( 'NONE',  ( 0.000000000000000000, -1.000000000000000000, 0.000000000000000000 ) ) ;
#21873 = CARTESIAN_POINT ( 'NONE',  ( -16.27683809663751191, 41.27791846035903234, -237.2365415511148115 ) ) ;
#21874 = EDGE_CURVE ( 'NONE', #88867, #40828, #224628, .T. ) ;
#21875 = CARTESIAN_POINT ( 'NONE',  ( 21.03670563405603033, 10.62482368933940258, -146.3255468862092528 ) ) ;
#21876 = CARTESIAN_POINT ( 'NONE',  ( -16.87036670365549895, 22.88247411645692253, -230.8391385443351282 ) ) ;
#21877 = ORIENTED_EDGE ( 'NONE', *, *, #40851, .T. ) ;
#21878 = VERTEX_POINT ( 'NONE', #39290 ) ;
#21879 = EDGE_CURVE ( 'NONE', #219752, #205, #121408, .T. ) ;
#21880 = CARTESIAN_POINT ( 'NONE',  ( 22.49066049874202022, 0.05634325154338429287, -122.3499877624829111 ) ) ;
#21881 = DIRECTION ( 'NONE',  ( -0.000000000000000000, 0.9550021345545507412, -0.2965989261549202838 ) ) ;
#21882 = DIRECTION ( 'NONE',  ( 6.938893903907222067E-15, 1.000000000000000000, 6.982962677686266711E-15 ) ) ;
#21883 = CARTESIAN_POINT ( 'NONE',  ( 18.54999999999999716, 8.750000000011182166, -180.1499999999999773 ) ) ;
#21884 = ORIENTED_EDGE ( 'NONE', *, *, #22990, .T. ) ;
#21885 = AXIS2_PLACEMENT_3D ( 'NONE', #39525, #81162, #119036 ) ;
#21886 = CARTESIAN_POINT ( 'NONE',  ( -20.93284271247462058, 36.02367271998545561, -235.8812521208699309 ) ) ;
#21887 = EDGE_CURVE ( 'NONE', #179805, #77787, #140942, .T. ) ;
#21888 = EDGE_LOOP ( 'NONE', ( #90002, #45657, #51790, #117778 ) ) ;
#21891 = ORIENTED_EDGE ( 'NONE', *, *, #73264, .T. ) ;
#21890 = CARTESIAN_POINT ( 'NONE',  ( 21.05000000000000071, 6.477067021135910707, -67.10000000000005116 ) ) ;
#21889 = CARTESIAN_POINT ( 'NONE',  ( 18.59999994388910238, 47.04063701600456682, -255.1605173984034423 ) ) ;
#21892 = AXIS2_PLACEMENT_3D ( 'NONE', #206072, #203506, #65271 ) ;
#21893 = DIRECTION ( 'NONE',  ( 0.000000000000000000, 0.000000000000000000, -1.000000000000000000 ) ) ;
#21894 = ADVANCED_FACE ( 'NONE', ( #195796 ), #144997, .T. ) ;
#21895 = CARTESIAN_POINT ( 'NONE',  ( -23.15000000000000213, 4.350000000011156054, -54.64999999999999858 ) ) ;
#21896 = ORIENTED_EDGE ( 'NONE', *, *, #41256, .F. ) ;
#21897 = CARTESIAN_POINT ( 'NONE',  ( 18.58725287972267637, 85.56662691070442861, -129.7006026787596511 ) ) ;
#21898 = ADVANCED_FACE ( 'NONE', ( #18413 ), #96632, .T. ) ;
#21899 = CIRCLE ( 'NONE', #209318, 0.1000000000000124678 ) ;
#21900 = DIRECTION ( 'NONE',  ( 0.000000000000000000, -1.000000000000000000, -6.982962677686266711E-15 ) ) ;
#21901 = ADVANCED_FACE ( 'NONE', ( #178813 ), #236174, .F. ) ;
#21902 = CARTESIAN_POINT ( 'NONE',  ( -22.47120815636973745, -3.126878263853650530, -228.2062078246864303 ) ) ;
#21904 = ORIENTED_EDGE ( 'NONE', *, *, #168872, .F. ) ;
#21903 = CARTESIAN_POINT ( 'NONE',  ( -21.05000000000000071, 77.83534155023598089, -57.96795619196132776 ) ) ;
#21905 = TOROIDAL_SURFACE ( 'NONE', #184385, 0.2000000000000000111, 0.1000000000000000056 ) ;
#21906 = CARTESIAN_POINT ( 'NONE',  ( -15.55912972643741199, 44.73202778202335139, -236.6305442897015610 ) ) ;
#21908 = EDGE_CURVE ( 'NONE', #70177, #102921, #253344, .T. ) ;
#21907 = AXIS2_PLACEMENT_3D ( 'NONE', #247350, #225203, #128707 ) ;
#21909 = ORIENTED_EDGE ( 'NONE', *, *, #6118, .F. ) ;
#21910 = TOROIDAL_SURFACE ( 'NONE', #138576, 0.2000000000000000111, 0.1000000000000000056 ) ;
#21911 = AXIS2_PLACEMENT_3D ( 'NONE', #153834, #54670, #35158 ) ;
#21912 = DIRECTION ( 'NONE',  ( 0.000000000000000000, 1.000000000000000000, 0.000000000000000000 ) ) ;
#21913 = DIRECTION ( 'NONE',  ( 0.000000000000000000, -0.000000000000000000, 1.000000000000000000 ) ) ;
#21914 = CARTESIAN_POINT ( 'NONE',  ( -18.47130263965439667, -9.471155585952804046, -140.6834047654767801 ) ) ;
#21915 = EDGE_LOOP ( 'NONE', ( #233605, #228488, #44989, #91581 ) ) ;
#21916 = CARTESIAN_POINT ( 'NONE',  ( -16.94107738177415712, 10.01423928514777728, -180.0499999999999545 ) ) ;
#21918 = ORIENTED_EDGE ( 'NONE', *, *, #221157, .F. ) ;
#21917 = AXIS2_PLACEMENT_3D ( 'NONE', #33683, #113167, #149754 ) ;
#21919 = DIRECTION ( 'NONE',  ( 0.000000000000000000, 0.000000000000000000, 1.000000000000000000 ) ) ;
#21920 = AXIS2_PLACEMENT_3D ( 'NONE', #91136, #55825, #192820 ) ;
#21921 = CARTESIAN_POINT ( 'NONE',  ( -20.64999999999999858, 19.73066058418984170, -238.2142830767208466 ) ) ;
#21922 = CARTESIAN_POINT ( 'NONE',  ( 21.05000000000000071, 36.02918351690956200, -236.0543695120161090 ) ) ;
#21923 = EDGE_LOOP ( 'NONE', ( #249870, #137457, #123945, #97521, #220991 ) ) ;
#21924 = CIRCLE ( 'NONE', #9257, 0.09999999999998898659 ) ;
#21925 = EDGE_CURVE ( 'NONE', #144336, #187076, #170014, .T. ) ;
#21926 = DIRECTION ( 'NONE',  ( 0.000000000000000000, 0.000000000000000000, 1.000000000000000000 ) ) ;
#21927 = AXIS2_PLACEMENT_3D ( 'NONE', #22094, #101577, #121219 ) ;
#21928 = DIRECTION ( 'NONE',  ( 0.000000000000000000, -0.9908441862701600211, -0.1350103645451876666 ) ) ;
#21929 = VERTEX_POINT ( 'NONE', #101764 ) ;
#21930 = AXIS2_PLACEMENT_3D ( 'NONE', #192938, #14323, #95113 ) ;
#21931 = DIRECTION ( 'NONE',  ( 0.000000000000000000, 0.000000000000000000, 1.000000000000000000 ) ) ;
#21932 = VERTEX_POINT ( 'NONE', #62685 ) ;
#21933 = DIRECTION ( 'NONE',  ( 1.000000000000000000, -0.000000000000000000, -0.000000000000000000 ) ) ;
#21934 = ORIENTED_EDGE ( 'NONE', *, *, #160921, .F. ) ;
#21935 = CIRCLE ( 'NONE', #9449, 0.09999999999999939493 ) ;
#21936 = EDGE_LOOP ( 'NONE', ( #141099, #165432, #41584, #142019 ) ) ;
#21937 = AXIS2_PLACEMENT_3D ( 'NONE', #82667, #7017, #224769 ) ;
#21938 = EDGE_CURVE ( 'NONE', #185471, #177518, #142208, .T. ) ;
#21939 = DIRECTION ( 'NONE',  ( 0.000000000000000000, -0.9908441862701605762, 0.1350103645451835310 ) ) ;
#21940 = ORIENTED_EDGE ( 'NONE', *, *, #184442, .T. ) ;
#21942 = EDGE_LOOP ( 'NONE', ( #65869, #173096, #57823, #233654 ) ) ;
#21941 = DIRECTION ( 'NONE',  ( -1.000000000000000000, -0.000000000000000000, -0.000000000000000000 ) ) ;
#21943 = VECTOR ( 'NONE', #90599, 1000.000000000000000 ) ;
#21946 = ORIENTED_EDGE ( 'NONE', *, *, #54722, .F. ) ;
#21945 = ORIENTED_EDGE ( 'NONE', *, *, #188834, .F. ) ;
#21944 = CARTESIAN_POINT ( 'NONE',  ( -21.08621493067320429, 0.05619483947604889812, 6.349294291171942106 ) ) ;
#21947 = CARTESIAN_POINT ( 'NONE',  ( -20.54999999999999716, 70.60814576644823148, -215.7631455941064189 ) ) ;
#21948 = CARTESIAN_POINT ( 'NONE',  ( -18.50000000000000000, 64.25000000001269029, -203.4231074845244507 ) ) ;
#21949 = CARTESIAN_POINT ( 'NONE',  ( 13.99999999999999822, 66.15000000001228386, -153.2731074845244450 ) ) ;
#21951 = CYLINDRICAL_SURFACE ( 'NONE', #179432, 0.09999999999999724387 ) ;
#21950 = CARTESIAN_POINT ( 'NONE',  ( -20.54999999999999716, 71.75000000001229239, -157.7731074845243882 ) ) ;
#21953 = EDGE_CURVE ( 'NONE', #31671, #75757, #111363, .T. ) ;
#21952 = FACE_OUTER_BOUND ( 'NONE', #55157, .T. ) ;
#21954 = AXIS2_PLACEMENT_3D ( 'NONE', #247227, #68611, #108998 ) ;
#21955 = CYLINDRICAL_SURFACE ( 'NONE', #138952, 0.09999999999998898659 ) ;
#21956 = AXIS2_PLACEMENT_3D ( 'NONE', #91104, #49414, #151086 ) ;
#21957 = EDGE_CURVE ( 'NONE', #110239, #16537, #34423, .T. ) ;
#21958 = CARTESIAN_POINT ( 'NONE',  ( -21.29999999999995808, 76.00000000001216449, -140.5731074845242858 ) ) ;
#21961 = DIRECTION ( 'NONE',  ( 2.710505431213776862E-16, -0.4721928772777346239, -0.8814952561688430555 ) ) ;
#21960 = FACE_OUTER_BOUND ( 'NONE', #18544, .T. ) ;
#21959 = AXIS2_PLACEMENT_3D ( 'NONE', #167679, #82943, #67266 ) ;
#21962 = EDGE_LOOP ( 'NONE', ( #16914, #90521, #72160, #246736 ) ) ;
#21963 = ORIENTED_EDGE ( 'NONE', *, *, #225802, .F. ) ;
#21964 = CARTESIAN_POINT ( 'NONE',  ( -23.25000000000000000, 1.115600667400684642E-11, -37.65000000000000568 ) ) ;
#21966 = ORIENTED_EDGE ( 'NONE', *, *, #156704, .F. ) ;
#21965 = CARTESIAN_POINT ( 'NONE',  ( 6.000000000000060396, 64.65000000001120384, -25.92310748452479174 ) ) ;
#21967 = ORIENTED_EDGE ( 'NONE', *, *, #200141, .T. ) ;
#21968 = CARTESIAN_POINT ( 'NONE',  ( -16.78055652883087134, 12.41318068003151431, -211.2541194833696068 ) ) ;
#21970 = ADVANCED_FACE ( 'NONE', ( #33149 ), #70027, .T. ) ;
#21969 =( BOUNDED_SURFACE ( )  B_SPLINE_SURFACE ( 3, 2, ( 
 ( #200356, #99938, #834 ),
 ( #159967, #238179, #118250 ),
 ( #216050, #19145, #59522 ),
 ( #139054, #81649, #82936 ),
 ( #178253, #60825, #21724 ),
 ( #257695, #79097, #219913 ),
 ( #218610, #41310, #240773 ),
 ( #185921, #146765, #124675 ) ),
 .UNSPECIFIED., .F., .F., .F. ) 
 B_SPLINE_SURFACE_WITH_KNOTS ( ( 4, 2, 2, 4 ),
 ( 3, 3 ),
 ( 0.0001723339234021422576, 0.0002782939632049988743, 0.0003842540030078555181, 0.0005961740826135687515 ),
 ( 0.000000000000000000, 1.000000000000000000 ),
 .UNSPECIFIED. ) 
 GEOMETRIC_REPRESENTATION_ITEM ( )  RATIONAL_B_SPLINE_SURFACE ( (
 ( 1.000000000000000000, 0.9504532311154454405, 1.000000000000000000),
 ( 1.000000000000000000, 0.9506023220706004695, 1.000000000000000000),
 ( 1.000000000000000000, 0.9395774818186980459, 1.000000000000000000),
 ( 1.000000000000000000, 0.9079328464641933660, 1.000000000000000000),
 ( 1.000000000000000000, 0.8875702416205810685, 1.000000000000000000),
 ( 1.000000000000000000, 0.8205919608039069502, 1.000000000000000000),
 ( 1.000000000000000000, 0.7666842783599246980, 1.000000000000000000),
 ( 1.000000000000000000, 0.7071067811864361063, 1.000000000000000000) ) ) 
 REPRESENTATION_ITEM ( '' )  SURFACE ( )  );
#21971 = ORIENTED_EDGE ( 'NONE', *, *, #44792, .T. ) ;
#21972 = DIRECTION ( 'NONE',  ( 1.000000000000000000, 0.000000000000000000, 0.000000000000000000 ) ) ;
#21973 = EDGE_CURVE ( 'NONE', #213025, #67212, #193482, .T. ) ;
#21974 = ADVANCED_FACE ( 'NONE', ( #171380 ), #172671, .T. ) ;
#21975 = ORIENTED_EDGE ( 'NONE', *, *, #173000, .T. ) ;
#21976 = DIRECTION ( 'NONE',  ( 1.000000000000000000, 0.000000000000000000, 0.000000000000000000 ) ) ;
#21977 = DIRECTION ( 'NONE',  ( 1.000000000000000000, 0.000000000000000000, 0.000000000000000000 ) ) ;
#21978 = TOROIDAL_SURFACE ( 'NONE', #221848, 1.900000000000002576, 0.1000000000000000056 ) ;
#21980 = ORIENTED_EDGE ( 'NONE', *, *, #239232, .T. ) ;
#21979 = VERTEX_POINT ( 'NONE', #150499 ) ;
#21981 = ORIENTED_EDGE ( 'NONE', *, *, #71112, .T. ) ;
#21982 = DIRECTION ( 'NONE',  ( -1.073024830501117725E-15, -6.982962677686266711E-15, 1.000000000000000000 ) ) ;
#21983 = VERTEX_POINT ( 'NONE', #173955 ) ;
#21984 = ORIENTED_EDGE ( 'NONE', *, *, #128327, .F. ) ;
#21985 = EDGE_CURVE ( 'NONE', #135971, #37851, #207579, .T. ) ;
#21986 = CARTESIAN_POINT ( 'NONE',  ( -17.11825945287482753, 12.51174298335651791, -211.2216088517780292 ) ) ;
#21987 = VECTOR ( 'NONE', #22447, 1000.000000000000000 ) ;
#21989 = ORIENTED_EDGE ( 'NONE', *, *, #38278, .F. ) ;
#21988 = FACE_OUTER_BOUND ( 'NONE', #239432, .T. ) ;
#21991 = DIRECTION ( 'NONE',  ( 0.000000000000000000, -0.4999999999999088507, 0.8660254037844913322 ) ) ;
#21990 = FACE_OUTER_BOUND ( 'NONE', #161629, .T. ) ;
#21992 = DIRECTION ( 'NONE',  ( 1.000000000000000000, -0.000000000000000000, 0.000000000000000000 ) ) ;
#21993 = FACE_OUTER_BOUND ( 'NONE', #233261, .T. ) ;
#21994 = DIRECTION ( 'NONE',  ( -6.938893903907222067E-15, 1.000000000000000000, 2.891205793294679805E-16 ) ) ;
#21995 = ORIENTED_EDGE ( 'NONE', *, *, #165108, .F. ) ;
#21996 = VERTEX_POINT ( 'NONE', #13553 ) ;
#21997 = DIRECTION ( 'NONE',  ( -0.000000000000000000, 1.000000000000000000, -0.000000000000000000 ) ) ;
#21998 = CARTESIAN_POINT ( 'NONE',  ( -16.87036670365548474, 66.01058118071060221, -149.0435473672224020 ) ) ;
#21999 = CARTESIAN_POINT ( 'NONE',  ( -21.05000000000000071, 0.09779029131994770863, -60.74218538952393232 ) ) ;
#22000 = ORIENTED_EDGE ( 'NONE', *, *, #166144, .T. ) ;
#22001 = CARTESIAN_POINT ( 'NONE',  ( 20.97468175916167610, 10.62526516438217783, -45.75476143541259688 ) ) ;
#22002 = AXIS2_PLACEMENT_3D ( 'NONE', #104809, #86536, #180542 ) ;
#22003 = CARTESIAN_POINT ( 'NONE',  ( 20.94999999999999929, 1.115600667400684642E-11, -200.9999999999999432 ) ) ;
#22004 = DIRECTION ( 'NONE',  ( -1.000000000000000000, -0.000000000000000000, -0.000000000000000000 ) ) ;
#22005 = ORIENTED_EDGE ( 'NONE', *, *, #167827, .F. ) ;
#22006 = ORIENTED_EDGE ( 'NONE', *, *, #157312, .T. ) ;
#22007 = DIRECTION ( 'NONE',  ( 0.000000000000000000, 0.000000000000000000, -1.000000000000000000 ) ) ;
#22008 = CARTESIAN_POINT ( 'NONE',  ( -20.64999999999999858, -8.999999999988846255, -176.8939691226524076 ) ) ;
#22010 = ORIENTED_EDGE ( 'NONE', *, *, #171325, .T. ) ;
#22009 = ADVANCED_FACE ( 'NONE', ( #252141 ), #214317, .F. ) ;
#22011 = DIRECTION ( 'NONE',  ( -0.7071067811865487940, -0.7071067811865463515, -4.216150419019404490E-15 ) ) ;
#22012 = ORIENTED_EDGE ( 'NONE', *, *, #143911, .F. ) ;
#22013 = EDGE_CURVE ( 'NONE', #44096, #112321, #91798, .T. ) ;
#22014 = LINE ( 'NONE', #1124, #156527 ) ;
#22015 = DIRECTION ( 'NONE',  ( -1.000000000000000000, 3.265361837132813093E-16, 2.280189983783949500E-30 ) ) ;
#22017 = CARTESIAN_POINT ( 'NONE',  ( -21.05000000000000071, 64.40000000001249703, -176.9513107147999449 ) ) ;
#22016 = DIRECTION ( 'NONE',  ( -0.7071067811865474617, -0.6909108974501236844, -0.1504730267678057731 ) ) ;
#22018 = CARTESIAN_POINT ( 'NONE',  ( -16.94107738177415712, 10.01423928514777728, -46.04999999999999716 ) ) ;
#22019 = DIRECTION ( 'NONE',  ( 0.000000000000000000, -6.982962677686266711E-15, 1.000000000000000000 ) ) ;
#22021 = ADVANCED_FACE ( 'NONE', ( #250853 ), #232617, .F. ) ;
#22020 = ORIENTED_EDGE ( 'NONE', *, *, #48335, .T. ) ;
#22022 = VECTOR ( 'NONE', #57985, 1000.000000000000000 ) ;
#22023 = CARTESIAN_POINT ( 'NONE',  ( -20.54999999999999716, 1.999999999999998224, -20.67537807723790166 ) ) ;
#22024 = AXIS2_PLACEMENT_3D ( 'NONE', #226770, #70305, #48132 ) ;
#22025 = B_SPLINE_CURVE_WITH_KNOTS ( 'NONE', 3,
 ( #65425, #144947, #2870, #116732, #45864, #178015, #17617, #155891, #224497, #82392 ),
 .UNSPECIFIED., .F., .F.,
 ( 4, 3, 3, 4 ),
 ( -2.000561356211851792E-06, 0.000000000000000000, 1.787822682428855288E-05, 4.206475347089862486E-05 ),
 .UNSPECIFIED. ) ;
#22027 = ORIENTED_EDGE ( 'NONE', *, *, #57661, .T. ) ;
#22026 = ORIENTED_EDGE ( 'NONE', *, *, #119203, .T. ) ;
#22028 = ORIENTED_EDGE ( 'NONE', *, *, #238390, .T. ) ;
#22029 = EDGE_LOOP ( 'NONE', ( #222995, #82118, #195485, #47375 ) ) ;
#22030 = AXIS2_PLACEMENT_3D ( 'NONE', #113754, #194616, #94187 ) ;
#22031 = CARTESIAN_POINT ( 'NONE',  ( -21.05000000000000071, 1.115600667400684642E-11, -71.29999999999999716 ) ) ;
#22032 = FACE_OUTER_BOUND ( 'NONE', #227349, .T. ) ;
#22033 = DIRECTION ( 'NONE',  ( 0.000000000000000000, 0.000000000000000000, 1.000000000000000000 ) ) ;
#22034 = CARTESIAN_POINT ( 'NONE',  ( -18.59999999999999787, 76.00000000001165290, -69.52310748452431710 ) ) ;
#22035 = LINE ( 'NONE', #24616, #21832 ) ;
#22037 = FACE_OUTER_BOUND ( 'NONE', #140618, .T. ) ;
#22036 = FACE_OUTER_BOUND ( 'NONE', #9579, .T. ) ;
#22039 = EDGE_LOOP ( 'NONE', ( #232880, #100746, #245149, #227658 ) ) ;
#22038 = CARTESIAN_POINT ( 'NONE',  ( 18.44206774312971220, 77.15870146463355184, -241.8076626181645281 ) ) ;
#22040 = DIRECTION ( 'NONE',  ( 0.000000000000000000, -0.9126074666063769270, -0.4088369013363280513 ) ) ;
#22041 = VERTEX_POINT ( 'NONE', #55200 ) ;
#22042 = ORIENTED_EDGE ( 'NONE', *, *, #124653, .F. ) ;
#22043 = EDGE_LOOP ( 'NONE', ( #186158, #186862, #219003, #245460 ) ) ;
#22044 = DIRECTION ( 'NONE',  ( 0.000000000000000000, 0.8814952561688476074, -0.4721928772777262417 ) ) ;
#22046 = AXIS2_PLACEMENT_3D ( 'NONE', #202535, #4319, #83825 ) ;
#22045 = DIRECTION ( 'NONE',  ( 0.000000000000000000, -1.000000000000000000, -6.982962677686266711E-15 ) ) ;
#22047 = CARTESIAN_POINT ( 'NONE',  ( -21.11833042828101625, 75.99289949095337704, -209.9687521783793613 ) ) ;
#22048 = AXIS2_PLACEMENT_3D ( 'NONE', #192538, #129966, #11328 ) ;
#22049 = CARTESIAN_POINT ( 'NONE',  ( -18.59999999999999787, -1.362429037182155023, -208.8888812479211765 ) ) ;
#22050 = EDGE_CURVE ( 'NONE', #29748, #251252, #28470, .T. ) ;
#22051 = LINE ( 'NONE', #242358, #250706 ) ;
#22052 = ORIENTED_EDGE ( 'NONE', *, *, #220856, .F. ) ;
#22053 = ORIENTED_EDGE ( 'NONE', *, *, #196152, .T. ) ;
#22054 = AXIS2_PLACEMENT_3D ( 'NONE', #156096, #98609, #40002 ) ;
#22056 = ADVANCED_FACE ( 'NONE', ( #70981 ), #151797, .T. ) ;
#22055 = CARTESIAN_POINT ( 'NONE',  ( 20.85000000000000142, 76.00000000001244871, -170.0231074845243597 ) ) ;
#22057 = VERTEX_POINT ( 'NONE', #89220 ) ;
#22058 = DIRECTION ( 'NONE',  ( 1.000000000000000000, 0.000000000000000000, 0.000000000000000000 ) ) ;
#22059 = DIRECTION ( 'NONE',  ( 0.000000000000000000, 1.000000000000000000, 6.688090509790097607E-15 ) ) ;
#22060 = CARTESIAN_POINT ( 'NONE',  ( -20.64999999999999858, 7.150000000011155876, -112.8500000000000369 ) ) ;
#22061 = CARTESIAN_POINT ( 'NONE',  ( -17.11825945287482753, 66.05000000001209060, -123.7731074845243597 ) ) ;
#22062 = DIRECTION ( 'NONE',  ( 0.000000000000000000, 5.551115123126393596E-13, -1.000000000000000000 ) ) ;
#22063 = CARTESIAN_POINT ( 'NONE',  ( -23.15000000000000213, 64.35000000001198828, -115.1731074845243796 ) ) ;
#22064 = EDGE_CURVE ( 'NONE', #158940, #106265, #230019, .T. ) ;
#22066 = CARTESIAN_POINT ( 'NONE',  ( 21.05000000000000071, 4.850467289730776344, -155.4657325909983570 ) ) ;
#22065 = AXIS2_PLACEMENT_3D ( 'NONE', #119380, #198903, #52333 ) ;
#22067 = DIRECTION ( 'NONE',  ( 0.000000000000000000, 0.000000000000000000, 1.000000000000000000 ) ) ;
#22068 = TOROIDAL_SURFACE ( 'NONE', #201114, 12.77499999999999858, 0.1000000000000000056 ) ;
#22069 = DIRECTION ( 'NONE',  ( 0.000000000000000000, 0.9654727137038715545, -0.2605042016806676242 ) ) ;
#22070 = EDGE_CURVE ( 'NONE', #200641, #148706, #15868, .T. ) ;
#22071 = DIRECTION ( 'NONE',  ( -1.000000000000000000, -2.952720810173289112E-16, 0.000000000000000000 ) ) ;
#22072 = EDGE_CURVE ( 'NONE', #168194, #161272, #31851, .T. ) ;
#22073 = ORIENTED_EDGE ( 'NONE', *, *, #160038, .T. ) ;
#22075 = EDGE_CURVE ( 'NONE', #214743, #18615, #203278, .T. ) ;
#22074 = EDGE_CURVE ( 'NONE', #169135, #96459, #133491, .T. ) ;
#22076 =( BOUNDED_CURVE ( )  B_SPLINE_CURVE ( 3, ( #218215, #113995, #134824, #235235 ),
 .UNSPECIFIED., .F., .T. ) 
 B_SPLINE_CURVE_WITH_KNOTS ( ( 4, 4 ),
 ( 4.712388980384695003, 6.283185307179586232 ),
 .UNSPECIFIED. ) 
 CURVE ( )  GEOMETRIC_REPRESENTATION_ITEM ( )  RATIONAL_B_SPLINE_CURVE ( ( 1.000000000000000000, 0.8047378541243662697, 0.8047378541243662697, 1.000000000000000000 ) ) 
 REPRESENTATION_ITEM ( '' )  );
#22077 = CARTESIAN_POINT ( 'NONE',  ( 20.95378194480896639, 10.53491199155394220, -41.06505414814786548 ) ) ;
#22078 = ORIENTED_EDGE ( 'NONE', *, *, #22089, .F. ) ;
#22079 = CARTESIAN_POINT ( 'NONE',  ( -20.64999999999999858, 36.65892442174472876, -249.5511627012454596 ) ) ;
#22080 = CARTESIAN_POINT ( 'NONE',  ( 21.05000000000000071, -11.29603075032412640, -97.45210084033617193 ) ) ;
#22081 = DIRECTION ( 'NONE',  ( 1.000000000000000000, 0.000000000000000000, 0.000000000000000000 ) ) ;
#22082 = ORIENTED_EDGE ( 'NONE', *, *, #109820, .T. ) ;
#22083 = DIRECTION ( 'NONE',  ( 0.000000000000000000, 0.000000000000000000, -1.000000000000000000 ) ) ;
#22084 = DIRECTION ( 'NONE',  ( 0.000000000000000000, -6.982962677686266711E-15, 1.000000000000000000 ) ) ;
#22086 = AXIS2_PLACEMENT_3D ( 'NONE', #69493, #149030, #49900 ) ;
#22085 = CARTESIAN_POINT ( 'NONE',  ( 18.59999999999999076, 18.26942912180536638, -237.6183358664095238 ) ) ;
#22087 = EDGE_CURVE ( 'NONE', #199662, #219323, #149335, .T. ) ;
#22088 = DIRECTION ( 'NONE',  ( 0.000000000000000000, -0.9651348961777157509, 0.2617529984165031243 ) ) ;
#22089 = EDGE_CURVE ( 'NONE', #5736, #242867, #180217, .T. ) ;
#22090 = CARTESIAN_POINT ( 'NONE',  ( -16.93294127766158752, 10.00328010296601988, -121.4299072658292715 ) ) ;
#22091 = CARTESIAN_POINT ( 'NONE',  ( -18.59999999999999787, 76.00000000001170974, -69.52310748452431710 ) ) ;
#22092 = ORIENTED_EDGE ( 'NONE', *, *, #157665, .F. ) ;
#22093 = CARTESIAN_POINT ( 'NONE',  ( 20.99999999999999645, 9.749999999999982236, -12.65000000000000568 ) ) ;
#22095 = VERTEX_POINT ( 'NONE', #1550 ) ;
#22094 = CARTESIAN_POINT ( 'NONE',  ( 21.05000000000000071, 1.115600667400684642E-11, -200.9999999999999432 ) ) ;
#22096 = CIRCLE ( 'NONE', #35151, 0.1000000000000070832 ) ;
#22097 = DIRECTION ( 'NONE',  ( 2.694716079187271467E-16, -0.4721928772777345129, -0.8814952561688430555 ) ) ;
#22098 = EDGE_CURVE ( 'NONE', #90063, #116223, #128682, .T. ) ;
#22099 = AXIS2_PLACEMENT_3D ( 'NONE', #172433, #229789, #233659 ) ;
#22100 = CARTESIAN_POINT ( 'NONE',  ( -20.94999999999999929, 76.00000000001142553, -36.02310748452432421 ) ) ;
#22101 = CARTESIAN_POINT ( 'NONE',  ( 21.97500000000000497, 9.750000000011153745, -45.85000000000000142 ) ) ;
#22102 = ORIENTED_EDGE ( 'NONE', *, *, #239506, .F. ) ;
#22103 = DIRECTION ( 'NONE',  ( 1.296989514748957725E-15, -0.5986962832864934914, -0.8009761297185696849 ) ) ;
#22104 = CIRCLE ( 'NONE', #155391, 0.1000000000000028644 ) ;
#22105 = ADVANCED_FACE ( 'NONE', ( #238900 ), #19860, .F. ) ;
#22107 = AXIS2_PLACEMENT_3D ( 'NONE', #206953, #127415, #28353 ) ;
#22106 = DIRECTION ( 'NONE',  ( 1.000000000000000000, -0.000000000000000000, 0.000000000000000000 ) ) ;
#22108 = ORIENTED_EDGE ( 'NONE', *, *, #158899, .T. ) ;
#22109 = AXIS2_PLACEMENT_3D ( 'NONE', #235229, #175292, #137399 ) ;
#22110 = SPHERICAL_SURFACE ( 'NONE', #187755, 0.1000000000000000056 ) ;
#22111 = DIRECTION ( 'NONE',  ( 1.000000000000000000, 0.000000000000000000, 0.000000000000000000 ) ) ;
#22112 = VECTOR ( 'NONE', #214716, 1000.000000000000000 ) ;
#22113 = EDGE_CURVE ( 'NONE', #178566, #79511, #82441, .T. ) ;
#22114 = AXIS2_PLACEMENT_3D ( 'NONE', #179369, #81495, #59359 ) ;
#22115 = CARTESIAN_POINT ( 'NONE',  ( -18.50000000000000000, 76.00000000001142553, -36.02310748452432421 ) ) ;
#22116 = ORIENTED_EDGE ( 'NONE', *, *, #55774, .F. ) ;
#22117 = VERTEX_POINT ( 'NONE', #177668 ) ;
#22118 = EDGE_CURVE ( 'NONE', #165864, #123166, #156823, .T. ) ;
#22119 = CARTESIAN_POINT ( 'NONE',  ( -22.40000000000000213, 76.00000000001203659, -114.7735403769829219 ) ) ;
#22121 = CIRCLE ( 'NONE', #251031, 11.65000000000001457 ) ;
#22120 = CARTESIAN_POINT ( 'NONE',  ( -20.54999999999999716, 8.751106741858205140, -220.7398867978735950 ) ) ;
#22123 = VECTOR ( 'NONE', #201454, 999.9999999999998863 ) ;
#22122 = CARTESIAN_POINT ( 'NONE',  ( 21.05000000000000071, 1.115600667400684642E-11, -112.6500000000000341 ) ) ;
#22124 = CARTESIAN_POINT ( 'NONE',  ( 22.49436431346199683, 64.35004905235922479, -203.5900110142466986 ) ) ;
#22125 = DIRECTION ( 'NONE',  ( 3.469446951953728416E-14, 0.8660254037844343777, -0.5000000000000074385 ) ) ;
#22126 = DIRECTION ( 'NONE',  ( 1.000000000000000000, 0.000000000000000000, 0.000000000000000000 ) ) ;
#22128 = DIRECTION ( 'NONE',  ( -0.000000000000000000, -0.1335171055202901413, -0.9910465087640860649 ) ) ;
#22127 = CARTESIAN_POINT ( 'NONE',  ( 21.05000000000000071, -1.236118717438610792, -194.8647072476872495 ) ) ;
#22129 = EDGE_CURVE ( 'NONE', #91307, #242283, #74516, .T. ) ;
#22130 = CIRCLE ( 'NONE', #72006, 0.09999999999999999167 ) ;
#22131 = CARTESIAN_POINT ( 'NONE',  ( 20.94983749550516450, 65.70233904876961617, -30.54874109119683823 ) ) ;
#22132 = CARTESIAN_POINT ( 'NONE',  ( 19.97071067811864609, 64.27928932189385591, -178.8731074845244393 ) ) ;
#22133 = DIRECTION ( 'NONE',  ( -1.000000000000000000, -0.000000000000000000, -0.000000000000000000 ) ) ;
#22134 = DIRECTION ( 'NONE',  ( 0.7071067811865476838, -0.3338907855510733769, -0.6233112732207617412 ) ) ;
#22135 = ORIENTED_EDGE ( 'NONE', *, *, #202051, .F. ) ;
#22136 = ORIENTED_EDGE ( 'NONE', *, *, #165745, .T. ) ;
#22137 = DIRECTION ( 'NONE',  ( 1.000000000000000000, 0.000000000000000000, 0.000000000000000000 ) ) ;
#22139 = LINE ( 'NONE', #162935, #170283 ) ;
#22138 = CARTESIAN_POINT ( 'NONE',  ( 23.14999999999999858, 5.000000000011153745, -79.40526601891313874 ) ) ;
#22140 = AXIS2_PLACEMENT_3D ( 'NONE', #240208, #23748, #159388 ) ;
#22141 = VECTOR ( 'NONE', #167526, 1000.000000000000000 ) ;
#22143 = TOROIDAL_SURFACE ( 'NONE', #238599, 11.65000000000000036, 0.1000000000000000056 ) ;
#22142 = B_SPLINE_CURVE_WITH_KNOTS ( 'NONE', 3,
 ( #81144, #45884, #180270, #5448, #26334, #181569, #105835, #238966, #42056, #84978, #199849, #40787, #220680, #2890 ),
 .UNSPECIFIED., .F., .F.,
 ( 4, 2, 2, 2, 2, 2, 4 ),
 ( 0.000000000000000000, 2.389617747647320093E-05, 4.779235495294640186E-05, 9.558470990581376537E-05, 0.0001911694198115567594, 0.0003823388396230466778, 0.0007646776792461088598 ),
 .UNSPECIFIED. ) ;
#22144 = CARTESIAN_POINT ( 'NONE',  ( -23.25000000000000000, 1.115600667400684642E-11, -167.5000000000000284 ) ) ;
#22145 = CARTESIAN_POINT ( 'NONE',  ( -21.05000000000000071, 0.000000000000000000, 0.000000000000000000 ) ) ;
#22146 = EDGE_CURVE ( 'NONE', #109222, #79626, #178959, .T. ) ;
#22147 = FACE_BOUND ( 'NONE', #232017, .T. ) ;
#22148 = ORIENTED_EDGE ( 'NONE', *, *, #205331, .F. ) ;
#22149 = FACE_OUTER_BOUND ( 'NONE', #249280, .T. ) ;
#22150 = VERTEX_POINT ( 'NONE', #216753 ) ;
#22151 = CYLINDRICAL_SURFACE ( 'NONE', #234411, 1.749999999999998002 ) ;
#22152 = ORIENTED_EDGE ( 'NONE', *, *, #255960, .F. ) ;
#22153 = FACE_OUTER_BOUND ( 'NONE', #67532, .T. ) ;
#22154 = CIRCLE ( 'NONE', #142726, 0.1000000000000055844 ) ;
#22155 = AXIS2_PLACEMENT_3D ( 'NONE', #150769, #12564, #72533 ) ;
#22156 = CIRCLE ( 'NONE', #67919, 0.1000000000000028644 ) ;
#22157 = VECTOR ( 'NONE', #37669, 1000.000000000000000 ) ;
#22158 = CARTESIAN_POINT ( 'NONE',  ( 18.33996824403505244, 85.56963985944298656, -29.20404184700773698 ) ) ;
#22159 = EDGE_LOOP ( 'NONE', ( #66489, #31347, #49256, #250097 ) ) ;
#22160 = DIRECTION ( 'NONE',  ( 0.000000000000000000, 0.9424537609900496271, 0.3343365196859450217 ) ) ;
#22161 = ORIENTED_EDGE ( 'NONE', *, *, #6271, .T. ) ;
#22162 = CARTESIAN_POINT ( 'NONE',  ( 22.60000000000000142, 55.86495732666938352, -232.8769840133977880 ) ) ;
#22163 = CARTESIAN_POINT ( 'NONE',  ( -21.65000000000000213, 23.06621698515930063, -230.9822826988504119 ) ) ;
#22164 = CARTESIAN_POINT ( 'NONE',  ( -21.55000000000000426, 12.07323165118033614, -220.0163634141040063 ) ) ;
#22165 = DIRECTION ( 'NONE',  ( 0.000000000000000000, 0.000000000000000000, -1.000000000000000000 ) ) ;
#22166 = DIRECTION ( 'NONE',  ( 0.000000000000000000, -0.4999999999999088507, -0.8660254037844913322 ) ) ;
#22168 = CYLINDRICAL_SURFACE ( 'NONE', #12494, 0.5000000000000004441 ) ;
#22167 = CARTESIAN_POINT ( 'NONE',  ( 23.14999999999998437, 1.115600667400684642E-11, -171.5499999999999829 ) ) ;
#22169 = CARTESIAN_POINT ( 'NONE',  ( -18.59999999999999787, 70.05000000001193428, -92.71740517948948934 ) ) ;
#22171 = ORIENTED_EDGE ( 'NONE', *, *, #78336, .F. ) ;
#22170 = CARTESIAN_POINT ( 'NONE',  ( 18.59999999999999432, 18.11150788191476124, -237.7585516551410478 ) ) ;
#22173 = FACE_OUTER_BOUND ( 'NONE', #80954, .T. ) ;
#22172 = CARTESIAN_POINT ( 'NONE',  ( -16.89268316805465986, 9.951721813253337601, -188.3557524785454973 ) ) ;
#22174 = EDGE_LOOP ( 'NONE', ( #88346, #33867, #46568, #71950, #167575, #9880, #24608 ) ) ;
#22176 = ORIENTED_EDGE ( 'NONE', *, *, #86115, .F. ) ;
#22175 = CARTESIAN_POINT ( 'NONE',  ( -23.25000000000000000, 27.77927773649450316, -239.9732258281457860 ) ) ;
#22177 = VERTEX_POINT ( 'NONE', #270 ) ;
#22178 = CARTESIAN_POINT ( 'NONE',  ( 21.05000000000000071, 1.115600667400684642E-11, -102.5000000000000426 ) ) ;
#22179 = CARTESIAN_POINT ( 'NONE',  ( -21.05000000000000071, 77.04701199367727327, -199.6625678998140359 ) ) ;
#22180 = CARTESIAN_POINT ( 'NONE',  ( -21.14999999999999858, 87.75000000001193712, -103.0231074845242318 ) ) ;
#22181 = AXIS2_PLACEMENT_3D ( 'NONE', #22803, #123165, #25367 ) ;
#22182 = ORIENTED_EDGE ( 'NONE', *, *, #54954, .F. ) ;
#22183 = CARTESIAN_POINT ( 'NONE',  ( -22.39999999999999858, 55.89093952297024970, -232.7795287750844579 ) ) ;
#22184 = PLANE ( 'NONE',  #118190 ) ;
#22185 = CARTESIAN_POINT ( 'NONE',  ( 18.44444291854883033, 38.02111363811317091, -261.0467631091868839 ) ) ;
#22186 = VERTEX_POINT ( 'NONE', #201047 ) ;
#22187 = CARTESIAN_POINT ( 'NONE',  ( -18.50000000000000000, 46.32970330538243786, -243.0551226933711746 ) ) ;
#22188 = EDGE_CURVE ( 'NONE', #236062, #216113, #86901, .T. ) ;
#22189 = CARTESIAN_POINT ( 'NONE',  ( -18.50000000000000000, 66.75000000001230660, -157.6731074845244223 ) ) ;
#22190 = EDGE_LOOP ( 'NONE', ( #23055, #161444, #65161, #12617 ) ) ;
#22191 = ORIENTED_EDGE ( 'NONE', *, *, #256332, .T. ) ;
#22192 = CARTESIAN_POINT ( 'NONE',  ( -23.25000000000000000, -8.999999999988844479, -91.20603087734760095 ) ) ;
#22193 = VECTOR ( 'NONE', #106197, 1000.000000000000000 ) ;
#22194 = VECTOR ( 'NONE', #74444, 1000.000000000000114 ) ;
#22195 = ORIENTED_EDGE ( 'NONE', *, *, #186650, .T. ) ;
#22196 = DIRECTION ( 'NONE',  ( 2.895190717381441586E-16, -0.9910465087640865089, 0.1335171055202867274 ) ) ;
#22197 = VERTEX_POINT ( 'NONE', #99355 ) ;
#22198 = DIRECTION ( 'NONE',  ( 0.000000000000000000, 0.03181660087583047802, -0.9994937237965568766 ) ) ;
#22199 = CARTESIAN_POINT ( 'NONE',  ( -20.64999999999999858, 85.00000000001207923, -127.1291383618717816 ) ) ;
#22200 = CARTESIAN_POINT ( 'NONE',  ( -23.15000000000000213, 23.34004772283015328, -229.2004250369967338 ) ) ;
#22201 = CARTESIAN_POINT ( 'NONE',  ( 22.50000000000000000, 1.115600667400684642E-11, -167.4999999999999716 ) ) ;
#22202 = DIRECTION ( 'NONE',  ( 0.000000000000000000, 0.000000000000000000, -1.000000000000000000 ) ) ;
#22203 = EDGE_LOOP ( 'NONE', ( #28089, #190265, #187805, #114897 ) ) ;
#22204 = EDGE_CURVE ( 'NONE', #172421, #183119, #61997, .T. ) ;
#22205 = CARTESIAN_POINT ( 'NONE',  ( 20.94999999999999929, 76.00000000001142553, -36.02310748452432421 ) ) ;
#22207 = AXIS2_PLACEMENT_3D ( 'NONE', #198854, #21526, #99730 ) ;
#22206 = DIRECTION ( 'NONE',  ( 0.000000000000000000, -6.938893903907222067E-15, 1.000000000000000000 ) ) ;
#22208 = CARTESIAN_POINT ( 'NONE',  ( -22.59999970745345976, -0.009356377315827653016, -88.74948679233081350 ) ) ;
#22209 = FACE_OUTER_BOUND ( 'NONE', #242895, .T. ) ;
#22210 = VERTEX_POINT ( 'NONE', #137220 ) ;
#22212 = FACE_OUTER_BOUND ( 'NONE', #120991, .T. ) ;
#22211 = FACE_OUTER_BOUND ( 'NONE', #158243, .T. ) ;
#22214 = ORIENTED_EDGE ( 'NONE', *, *, #95556, .T. ) ;
#22213 = VECTOR ( 'NONE', #257517, 1000.000000000000000 ) ;
#22216 = EDGE_LOOP ( 'NONE', ( #65696, #89565, #211231, #9457 ) ) ;
#22215 = DIRECTION ( 'NONE',  ( -1.000000000000000000, 0.000000000000000000, 0.000000000000000000 ) ) ;
#22217 = ORIENTED_EDGE ( 'NONE', *, *, #237240, .T. ) ;
#22218 = CARTESIAN_POINT ( 'NONE',  ( -20.94999999999999929, 11.65000000001115232, -127.2161343370219413 ) ) ;
#22220 = DIRECTION ( 'NONE',  ( -1.000000000000000000, 0.000000000000000000, 0.000000000000000000 ) ) ;
#22219 = VECTOR ( 'NONE', #175878, 1000.000000000000000 ) ;
#22221 = EDGE_CURVE ( 'NONE', #187737, #195077, #141082, .T. ) ;
#22222 = DIRECTION ( 'NONE',  ( 0.000000000000000000, -1.000000000000000000, -6.982962677686265922E-15 ) ) ;
#22223 = ORIENTED_EDGE ( 'NONE', *, *, #112310, .F. ) ;
#22224 = CARTESIAN_POINT ( 'NONE',  ( 18.49999999999999645, 77.29973367124300410, -146.4949779616548824 ) ) ;
#22225 = EDGE_CURVE ( 'NONE', #91601, #70632, #170190, .T. ) ;
#22226 = CARTESIAN_POINT ( 'NONE',  ( 21.05000000000000071, 71.00000000001151079, -48.42837350343745584 ) ) ;
#22227 = EDGE_CURVE ( 'NONE', #190048, #170518, #49336, .T. ) ;
#22229 = DIRECTION ( 'NONE',  ( 1.000000000000000000, 0.000000000000000000, 0.000000000000000000 ) ) ;
#22228 = CARTESIAN_POINT ( 'NONE',  ( -23.49999999999994316, 77.16254490893143725, -44.02310748452479316 ) ) ;
#22231 = ORIENTED_EDGE ( 'NONE', *, *, #70557, .F. ) ;
#22230 = CARTESIAN_POINT ( 'NONE',  ( 21.78635804494511419, 0.09900506550768010949, 7.035661485153183570 ) ) ;
#22232 = CIRCLE ( 'NONE', #180606, 0.09999999999999130418 ) ;
#22233 = AXIS2_PLACEMENT_3D ( 'NONE', #7151, #230068, #47557 ) ;
#22234 = ADVANCED_FACE ( 'NONE', ( #121546 ), #135920, .F. ) ;
#22235 = EDGE_LOOP ( 'NONE', ( #36136, #254132, #82146, #177422 ) ) ;
#22236 = CARTESIAN_POINT ( 'NONE',  ( -23.25000000000000000, -11.74999999998884448, -170.5999999999999659 ) ) ;
#22237 = LINE ( 'NONE', #118766, #126460 ) ;
#22238 = ORIENTED_EDGE ( 'NONE', *, *, #116565, .F. ) ;
#22239 = CARTESIAN_POINT ( 'NONE',  ( -23.15000000000000213, 80.83132476063475735, -86.05341054232552267 ) ) ;
#22240 = EDGE_CURVE ( 'NONE', #86948, #178818, #22437, .T. ) ;
#22241 = ORIENTED_EDGE ( 'NONE', *, *, #207874, .F. ) ;
#22242 = DIRECTION ( 'NONE',  ( -1.000000000000000000, 1.836970198721029934E-16, 1.282749433769087757E-30 ) ) ;
#22243 = CARTESIAN_POINT ( 'NONE',  ( 22.59999954896768770, 76.00882823225448703, -114.7736161585923043 ) ) ;
#22244 = CARTESIAN_POINT ( 'NONE',  ( 20.94999999999999574, 4.193200906077805712, -212.0298262072164164 ) ) ;
#22245 = ORIENTED_EDGE ( 'NONE', *, *, #239861, .F. ) ;
#22246 = DIRECTION ( 'NONE',  ( -1.000000000000000000, -0.000000000000000000, -0.000000000000000000 ) ) ;
#22247 = VECTOR ( 'NONE', #200076, 1000.000000000000000 ) ;
#22248 = VECTOR ( 'NONE', #104298, 1000.000000000000000 ) ;
#22249 = TOROIDAL_SURFACE ( 'NONE', #155533, 0.2000000000000000111, 0.1000000000000000056 ) ;
#22250 = EDGE_CURVE ( 'NONE', #189878, #603, #65387, .T. ) ;
#22251 = CIRCLE ( 'NONE', #168025, 2.699999999999999289 ) ;
#22252 = MANIFOLD_SOLID_BREP ( 'Stock-MAS-200-1', #70238 ) ;
#22253 = DIRECTION ( 'NONE',  ( 0.000000000000000000, 0.8814952561688476074, -0.4721928772777262417 ) ) ;
#22254 = ORIENTED_EDGE ( 'NONE', *, *, #77312, .T. ) ;
#22255 = ORIENTED_EDGE ( 'NONE', *, *, #56623, .T. ) ;
#22256 = EDGE_LOOP ( 'NONE', ( #46968, #42722, #25951, #93727 ) ) ;
#22257 = CYLINDRICAL_SURFACE ( 'NONE', #228994, 0.09999999999999939493 ) ;
#22258 = EDGE_LOOP ( 'NONE', ( #214335, #13091, #110313, #177689 ) ) ;
#22260 = ORIENTED_EDGE ( 'NONE', *, *, #2673, .T. ) ;
#22259 = CARTESIAN_POINT ( 'NONE',  ( 24.30000000000000071, 3.175288713399624818, 33.00000000000000000 ) ) ;
#22261 = ORIENTED_EDGE ( 'NONE', *, *, #53151, .T. ) ;
#22264 = ORIENTED_EDGE ( 'NONE', *, *, #165632, .T. ) ;
#22263 = ORIENTED_EDGE ( 'NONE', *, *, #134452, .F. ) ;
#22262 = DIRECTION ( 'NONE',  ( 0.000000000000000000, -0.000000000000000000, 1.000000000000000000 ) ) ;
#22265 = AXIS2_PLACEMENT_3D ( 'NONE', #245355, #66713, #71861 ) ;
#22266 = CIRCLE ( 'NONE', #173289, 0.1000000000000028644 ) ;
#22267 = ORIENTED_EDGE ( 'NONE', *, *, #233995, .F. ) ;
#22268 = DIRECTION ( 'NONE',  ( 0.000000000000000000, 0.2128009952263605897, -0.9770955615653315052 ) ) ;
#22269 = AXIS2_PLACEMENT_3D ( 'NONE', #88818, #186677, #247910 ) ;
#22270 = CYLINDRICAL_SURFACE ( 'NONE', #105456, 0.09999999999998898659 ) ;
#22271 = EDGE_CURVE ( 'NONE', #101872, #77834, #121646, .T. ) ;
#22272 = CARTESIAN_POINT ( 'NONE',  ( -16.87998658237740912, 14.11353887542160024, -219.0463262827253459 ) ) ;
#22273 = ORIENTED_EDGE ( 'NONE', *, *, #128198, .T. ) ;
#22274 = CARTESIAN_POINT ( 'NONE',  ( 20.94999999999999929, 18.82290990851282331, -233.3604470821920529 ) ) ;
#22276 = VERTEX_POINT ( 'NONE', #165797 ) ;
#22275 = DIRECTION ( 'NONE',  ( 0.000000000000000000, 0.1575546449569757979, 0.9875102702516471709 ) ) ;
#22277 = DIRECTION ( 'NONE',  ( 0.000000000000000000, -6.467318590049456648E-15, 1.000000000000000000 ) ) ;
#22279 = EDGE_LOOP ( 'NONE', ( #31031, #100730, #42538, #15121 ) ) ;
#22278 = CARTESIAN_POINT ( 'NONE',  ( -18.50000000000000000, 63.86602797976523505, -212.9247947273492514 ) ) ;
#22280 = EDGE_CURVE ( 'NONE', #83831, #252613, #78556, .T. ) ;
#22281 = ADVANCED_FACE ( 'NONE', ( #242729 ), #107074, .T. ) ;
#22282 = ORIENTED_EDGE ( 'NONE', *, *, #48480, .T. ) ;
#22283 = AXIS2_PLACEMENT_3D ( 'NONE', #15377, #36229, #75362 ) ;
#22284 = DIRECTION ( 'NONE',  ( 0.000000000000000000, 0.9998779222360096863, -0.01562500000001061998 ) ) ;
#22285 = DIRECTION ( 'NONE',  ( -0.000000000000000000, 1.000000000000000000, 0.000000000000000000 ) ) ;
#22286 = VECTOR ( 'NONE', #38282, 1000.000000000000114 ) ;
#22287 = ADVANCED_FACE ( 'NONE', ( #25006 ), #4126, .T. ) ;
#22288 = CIRCLE ( 'NONE', #88889, 0.1000000000000028644 ) ;
#22290 = ORIENTED_EDGE ( 'NONE', *, *, #113794, .T. ) ;
#22289 = CIRCLE ( 'NONE', #5673, 0.5000000000000004441 ) ;
#22291 = VERTEX_POINT ( 'NONE', #7997 ) ;
#22292 = VECTOR ( 'NONE', #205082, 1000.000000000000000 ) ;
#22293 = CARTESIAN_POINT ( 'NONE',  ( -20.64999999999999858, 76.00000000001170974, -69.52310748452431710 ) ) ;
#22295 = EDGE_CURVE ( 'NONE', #46773, #20778, #16227, .T. ) ;
#22294 = CARTESIAN_POINT ( 'NONE',  ( 20.84999999999999787, 64.25000000001249134, -176.9422547304831994 ) ) ;
#22296 = ADVANCED_FACE ( 'NONE', ( #167097 ), #83628, .T. ) ;
#22297 = AXIS2_PLACEMENT_3D ( 'NONE', #211759, #112655, #189630 ) ;
#22299 = ORIENTED_EDGE ( 'NONE', *, *, #66446, .F. ) ;
#22298 = ORIENTED_EDGE ( 'NONE', *, *, #49432, .F. ) ;
#22300 = EDGE_LOOP ( 'NONE', ( #10397, #5092, #33876, #157631 ) ) ;
#22301 = DIRECTION ( 'NONE',  ( -1.186688945009010077E-16, -1.000000000000000000, -6.982962677686266711E-15 ) ) ;
#22302 = ORIENTED_EDGE ( 'NONE', *, *, #214526, .T. ) ;
#22303 = VERTEX_POINT ( 'NONE', #163218 ) ;
#22304 = EDGE_CURVE ( 'NONE', #72109, #12777, #207759, .T. ) ;
#22305 = LINE ( 'NONE', #62697, #38652 ) ;
#22307 = VERTEX_POINT ( 'NONE', #45825 ) ;
#22306 = CYLINDRICAL_SURFACE ( 'NONE', #126716, 0.1000000000000055844 ) ;
#22308 = CYLINDRICAL_SURFACE ( 'NONE', #135538, 0.09999999999999530098 ) ;
#22309 = AXIS2_PLACEMENT_3D ( 'NONE', #163183, #178918, #235 ) ;
#22311 = DIRECTION ( 'NONE',  ( 0.000000000000000000, 1.000000000000000000, 6.982962677686266711E-15 ) ) ;
#22310 = CARTESIAN_POINT ( 'NONE',  ( -20.94999999999999929, 10.29270135741298731, -105.9573618871519756 ) ) ;
#22312 = ORIENTED_EDGE ( 'NONE', *, *, #167430, .T. ) ;
#22314 = ORIENTED_EDGE ( 'NONE', *, *, #199964, .F. ) ;
#22313 = VERTEX_POINT ( 'NONE', #223165 ) ;
#22315 = TOROIDAL_SURFACE ( 'NONE', #184591, 0.4000000000000009104, 0.1000000000000000056 ) ;
#22316 = CARTESIAN_POINT ( 'NONE',  ( -21.05000000000000426, 76.10000000001274145, -210.0001745056491131 ) ) ;
#22317 = DIRECTION ( 'NONE',  ( -0.000000000000000000, 1.000000000000000000, -0.000000000000000000 ) ) ;
#22318 = EDGE_CURVE ( 'NONE', #164116, #238428, #20311, .T. ) ;
#22319 = VERTEX_POINT ( 'NONE', #26274 ) ;
#22320 = AXIS2_PLACEMENT_3D ( 'NONE', #122008, #179430, #257598 ) ;
#22321 = AXIS2_PLACEMENT_3D ( 'NONE', #124232, #242878, #201183 ) ;
#22322 = EDGE_CURVE ( 'NONE', #235787, #214842, #161981, .T. ) ;
#22323 = AXIS2_PLACEMENT_3D ( 'NONE', #100610, #101904, #221850 ) ;
#22324 = CARTESIAN_POINT ( 'NONE',  ( -20.65000000000000568, 28.17589918783267322, -238.5974746063260739 ) ) ;
#22325 = ORIENTED_EDGE ( 'NONE', *, *, #129588, .F. ) ;
#22326 = VERTEX_POINT ( 'NONE', #48383 ) ;
#22327 = FACE_OUTER_BOUND ( 'NONE', #131692, .T. ) ;
#22329 = EDGE_CURVE ( 'NONE', #38617, #39343, #127939, .T. ) ;
#22328 = ORIENTED_EDGE ( 'NONE', *, *, #9950, .F. ) ;
#22330 = LINE ( 'NONE', #2721, #47179 ) ;
#22331 = LINE ( 'NONE', #164391, #31280 ) ;
#22332 = VERTEX_POINT ( 'NONE', #92644 ) ;
#22333 = EDGE_CURVE ( 'NONE', #254122, #115263, #30138, .T. ) ;
#22334 = LINE ( 'NONE', #176271, #189450 ) ;
#22335 = DIRECTION ( 'NONE',  ( 0.000000000000000000, -0.9908441862701782288, 0.1350103645450542456 ) ) ;
#22337 = CARTESIAN_POINT ( 'NONE',  ( -16.84981964351497297, 9.917318234109998798, -121.1303983859805697 ) ) ;
#22336 = CARTESIAN_POINT ( 'NONE',  ( -20.54999999999999716, -8.999999999988846255, -43.39396912265245021 ) ) ;
#22338 = DIRECTION ( 'NONE',  ( -1.000000000000000000, 0.000000000000000000, -0.000000000000000000 ) ) ;
#22339 = DIRECTION ( 'NONE',  ( -1.000000000000000000, 0.000000000000000000, 0.000000000000000000 ) ) ;
#22340 = DIRECTION ( 'NONE',  ( 0.000000000000000000, -6.938893903907229955E-15, 1.000000000000000000 ) ) ;
#22341 = DIRECTION ( 'NONE',  ( 1.000000000000000000, 0.000000000000000000, 0.000000000000000000 ) ) ;
#22342 = VECTOR ( 'NONE', #189636, 1000.000000000000000 ) ;
#22343 = VERTEX_POINT ( 'NONE', #150087 ) ;
#22344 = VECTOR ( 'NONE', #252161, 1000.000000000000000 ) ;
#22345 = CIRCLE ( 'NONE', #26428, 0.1000000000000016431 ) ;
#22347 = ORIENTED_EDGE ( 'NONE', *, *, #216363, .F. ) ;
#22346 = ORIENTED_EDGE ( 'NONE', *, *, #201218, .T. ) ;
#22348 = ORIENTED_EDGE ( 'NONE', *, *, #229748, .F. ) ;
#22349 = VERTEX_POINT ( 'NONE', #14433 ) ;
#22350 = DIRECTION ( 'NONE',  ( -1.000000000000000000, -0.000000000000000000, -0.000000000000000000 ) ) ;
#22351 = CARTESIAN_POINT ( 'NONE',  ( -24.30000000000000071, 3.175288713399619045, -347.0000000000001137 ) ) ;
#22353 = CARTESIAN_POINT ( 'NONE',  ( -12.84409460144754433, 9.410682294267951775, -15.43114344194827581 ) ) ;
#22352 = DIRECTION ( 'NONE',  ( 0.000000000000000000, -1.000000000000000000, 0.000000000000000000 ) ) ;
#22354 = CARTESIAN_POINT ( 'NONE',  ( 21.30000000000002558, 36.65892442174472876, -249.5511627012454596 ) ) ;
#22355 = ORIENTED_EDGE ( 'NONE', *, *, #52888, .F. ) ;
#22356 = CARTESIAN_POINT ( 'NONE',  ( -20.88420186297724257, 10.33025634372637391, -106.0870929282639281 ) ) ;
#22357 = PRESENTATION_STYLE_ASSIGNMENT (( #61460 ) ) ;
#22358 = DIRECTION ( 'NONE',  ( -1.000000000000000000, 0.000000000000000000, -0.000000000000000000 ) ) ;
#22359 = DIRECTION ( 'NONE',  ( 0.000000000000000000, 0.000000000000000000, 1.000000000000000000 ) ) ;
#22360 = DIRECTION ( 'NONE',  ( -1.000000000000000000, 0.000000000000000000, 0.000000000000000000 ) ) ;
#22361 = ORIENTED_EDGE ( 'NONE', *, *, #167733, .F. ) ;
#22362 = DIRECTION ( 'NONE',  ( 1.000000000000000000, 0.000000000000000000, -0.000000000000000000 ) ) ;
#22363 = CIRCLE ( 'NONE', #55610, 0.4000000000000045186 ) ;
#22364 = DIRECTION ( 'NONE',  ( -1.000000000000000000, 0.000000000000000000, 0.000000000000000000 ) ) ;
#22365 = EDGE_LOOP ( 'NONE', ( #54090, #90351, #62931, #182255 ) ) ;
#22366 = CARTESIAN_POINT ( 'NONE',  ( -16.89060415895971090, 66.04877923720935939, -56.87718726025393323 ) ) ;
#22367 = CARTESIAN_POINT ( 'NONE',  ( -20.94999999999999929, 76.00000000001179501, -81.22310748452430573 ) ) ;
#22368 = LINE ( 'NONE', #18498, #18706 ) ;
#22369 = CARTESIAN_POINT ( 'NONE',  ( -21.45000000000000284, 68.29142135624935861, -124.2731074845243597 ) ) ;
#22370 = CARTESIAN_POINT ( 'NONE',  ( -16.91256925476569961, 9.985731158128169582, -20.96764248900526439 ) ) ;
#22371 = ORIENTED_EDGE ( 'NONE', *, *, #133395, .F. ) ;
#22372 = LINE ( 'NONE', #23668, #148761 ) ;
#22373 = CARTESIAN_POINT ( 'NONE',  ( -20.94999999999999929, 74.16465844978787914, -158.4679561919613775 ) ) ;
#22374 = FACE_OUTER_BOUND ( 'NONE', #185365, .T. ) ;
#22375 = EDGE_CURVE ( 'NONE', #131987, #161055, #251730, .T. ) ;
#22377 = DIRECTION ( 'NONE',  ( 2.659396599871503240E-15, 0.9858629823651696711, 0.1675535138457361073 ) ) ;
#22376 = CARTESIAN_POINT ( 'NONE',  ( 21.07928932188134397, 69.67148334361908724, -170.1220026301787982 ) ) ;
#22378 = DIRECTION ( 'NONE',  ( -1.000000000000000000, -5.945622153099073960E-16, 5.981866248895714834E-16 ) ) ;
#22379 = DIRECTION ( 'NONE',  ( -0.000000000000000000, -0.9875055080513799322, 0.1575844902526464253 ) ) ;
#22381 = EDGE_CURVE ( 'NONE', #234552, #131734, #66076, .T. ) ;
#22380 = CARTESIAN_POINT ( 'NONE',  ( -20.54999999999999716, 4.349999999999999645, -16.75000000000000000 ) ) ;
#22382 = TOROIDAL_SURFACE ( 'NONE', #134749, 11.65000000000000036, 0.1000000000000000056 ) ;
#22384 = ORIENTED_EDGE ( 'NONE', *, *, #36961, .F. ) ;
#22383 = LINE ( 'NONE', #141036, #136152 ) ;
#22385 = TOROIDAL_SURFACE ( 'NONE', #55631, 4.900000000000000355, 0.1000000000000000056 ) ;
#22386 = VECTOR ( 'NONE', #243940, 1000.000000000000000 ) ;
#22387 = ORIENTED_EDGE ( 'NONE', *, *, #38327, .T. ) ;
#22388 = EDGE_CURVE ( 'NONE', #31578, #81676, #199387, .T. ) ;
#22389 = EDGE_CURVE ( 'NONE', #21421, #254127, #53626, .T. ) ;
#22390 = DIRECTION ( 'NONE',  ( 1.000000000000000000, 0.000000000000000000, 0.000000000000000000 ) ) ;
#22392 = CARTESIAN_POINT ( 'NONE',  ( -18.50000000000000000, 65.70729864260955821, -30.56574559737245167 ) ) ;
#22391 = CIRCLE ( 'NONE', #1508, 2.000000000000001776 ) ;
#22393 = DIRECTION ( 'NONE',  ( 1.000000000000000000, 0.000000000000000000, 0.000000000000000000 ) ) ;
#22394 = ORIENTED_EDGE ( 'NONE', *, *, #53194, .T. ) ;
#22395 = CIRCLE ( 'NONE', #168170, 0.1000000000000028644 ) ;
#22396 = CARTESIAN_POINT ( 'NONE',  ( -22.19999999999999929, -11.64999999999999858, 11.99999999999999645 ) ) ;
#22397 = EDGE_CURVE ( 'NONE', #65006, #21421, #91380, .T. ) ;
#22398 = AXIS2_PLACEMENT_3D ( 'NONE', #78466, #160616, #64052 ) ;
#22399 = CARTESIAN_POINT ( 'NONE',  ( 20.90000000000000213, -1.885425182446133885, -11.49641995933507843 ) ) ;
#22400 = DIRECTION ( 'NONE',  ( 0.000000000000000000, -0.4930308989874729320, -0.8700118002898605818 ) ) ;
#22401 = TOROIDAL_SURFACE ( 'NONE', #226360, 0.2000000000000000111, 0.1000000000000000056 ) ;
#22402 = VERTEX_POINT ( 'NONE', #228324 ) ;
#22403 = DIRECTION ( 'NONE',  ( -0.000000000000000000, 0.000000000000000000, -1.000000000000000000 ) ) ;
#22405 = EDGE_LOOP ( 'NONE', ( #183645, #154834, #80275, #82327 ) ) ;
#22404 = FACE_OUTER_BOUND ( 'NONE', #196344, .T. ) ;
#22407 = CARTESIAN_POINT ( 'NONE',  ( -20.94999999999999929, 75.74389420791943905, -69.55800392619661920 ) ) ;
#22406 = CARTESIAN_POINT ( 'NONE',  ( -16.94107738177415712, 22.92025126680846725, -230.8312174982872591 ) ) ;
#22408 = CARTESIAN_POINT ( 'NONE',  ( -20.65000000000000568, 11.52084357182974195, -219.8296352432475942 ) ) ;
#22409 = DIRECTION ( 'NONE',  ( 0.000000000000000000, 0.000000000000000000, 1.000000000000000000 ) ) ;
#22410 = VERTEX_POINT ( 'NONE', #233475 ) ;
#22411 = AXIS2_PLACEMENT_3D ( 'NONE', #87072, #165355, #6258 ) ;
#22412 = DIRECTION ( 'NONE',  ( 1.000000000000000000, 0.000000000000000000, 0.000000000000000000 ) ) ;
#22414 = SPHERICAL_SURFACE ( 'NONE', #187635, 0.1000000000000000056 ) ;
#22413 = TOROIDAL_SURFACE ( 'NONE', #18289, 0.2000000000000000111, 0.1000000000000000056 ) ;
#22415 = EDGE_CURVE ( 'NONE', #86374, #214176, #124357, .T. ) ;
#22417 = AXIS2_PLACEMENT_3D ( 'NONE', #162003, #207539, #228382 ) ;
#22416 = DIRECTION ( 'NONE',  ( 0.000000000000000000, 0.000000000000000000, 1.000000000000000000 ) ) ;
#22418 = ORIENTED_EDGE ( 'NONE', *, *, #47686, .T. ) ;
#22419 = FACE_OUTER_BOUND ( 'NONE', #94465, .T. ) ;
#22420 = EDGE_CURVE ( 'NONE', #121706, #118654, #57702, .T. ) ;
#22421 = CARTESIAN_POINT ( 'NONE',  ( -22.57320508075687115, 64.35000000001166143, -69.52310748452435973 ) ) ;
#22422 = CIRCLE ( 'NONE', #89021, 2.099999999999995204 ) ;
#22423 = DIRECTION ( 'NONE',  ( 1.000000000000000000, 0.000000000000000000, 0.000000000000000000 ) ) ;
#22424 = FACE_OUTER_BOUND ( 'NONE', #117743, .T. ) ;
#22425 = EDGE_LOOP ( 'NONE', ( #100536, #82314, #126085, #42443 ) ) ;
#22426 = VERTEX_POINT ( 'NONE', #88779 ) ;
#22427 = EDGE_CURVE ( 'NONE', #17857, #136449, #111897, .T. ) ;
#22428 = CIRCLE ( 'NONE', #122186, 0.09999999999999971412 ) ;
#22429 = VECTOR ( 'NONE', #24406, 1000.000000000000000 ) ;
#22430 = EDGE_CURVE ( 'NONE', #208786, #49789, #136816, .T. ) ;
#22431 = VECTOR ( 'NONE', #252680, 1000.000000000000114 ) ;
#22432 = CARTESIAN_POINT ( 'NONE',  ( -21.22070241538126112, 69.53005372714234511, -103.1220265150593889 ) ) ;
#22433 = CARTESIAN_POINT ( 'NONE',  ( -18.59999999999999787, 11.75000000001115197, -122.2500000000000284 ) ) ;
#22434 = DIRECTION ( 'NONE',  ( 0.000000000000000000, 0.1350103645451876666, 0.9908441862701600211 ) ) ;
#22435 = CARTESIAN_POINT ( 'NONE',  ( -20.64999999999999858, -9.399999999988850163, -177.3939691226524076 ) ) ;
#22437 = LINE ( 'NONE', #96778, #186918 ) ;
#22436 = LINE ( 'NONE', #182786, #36698 ) ;
#22438 = EDGE_CURVE ( 'NONE', #56902, #144564, #152663, .T. ) ;
#22439 = CARTESIAN_POINT ( 'NONE',  ( -18.37160782347004329, 58.57697193133546421, -223.9238517115823299 ) ) ;
#22440 = CARTESIAN_POINT ( 'NONE',  ( -16.85939591225059075, 66.09477352162372199, -56.56303923805535305 ) ) ;
#22441 = DIRECTION ( 'NONE',  ( 1.000000000000000000, -0.000000000000000000, 0.000000000000000000 ) ) ;
#22442 = ORIENTED_EDGE ( 'NONE', *, *, #57165, .F. ) ;
#22443 = CYLINDRICAL_SURFACE ( 'NONE', #85630, 0.09999999999999817368 ) ;
#22444 = VERTEX_POINT ( 'NONE', #232189 ) ;
#22445 = CARTESIAN_POINT ( 'NONE',  ( -21.05000000000000071, 64.25000000001209344, -129.7392418215462442 ) ) ;
#22446 = DIRECTION ( 'NONE',  ( 0.000000000000000000, 0.000000000000000000, -1.000000000000000000 ) ) ;
#22448 = CARTESIAN_POINT ( 'NONE',  ( -23.49999999999994316, 64.35000000001120668, -3.123107484524795474 ) ) ;
#22447 = DIRECTION ( 'NONE',  ( 1.000000000000000000, 0.000000000000000000, 0.000000000000000000 ) ) ;
#22449 = ORIENTED_EDGE ( 'NONE', *, *, #174102, .T. ) ;
#22451 = DIRECTION ( 'NONE',  ( 1.000000000000000000, 0.000000000000000000, 0.000000000000000000 ) ) ;
#22450 = CARTESIAN_POINT ( 'NONE',  ( -18.50000000000000000, 76.00000000001170974, -69.52310748452431710 ) ) ;
#22452 = DIRECTION ( 'NONE',  ( 1.000000000000000000, 0.000000000000000000, 0.000000000000000000 ) ) ;
#22453 = EDGE_CURVE ( 'NONE', #30421, #19000, #143317, .T. ) ;
#22454 = LINE ( 'NONE', #101935, #234485 ) ;
#22455 = DIRECTION ( 'NONE',  ( 0.000000000000000000, 0.000000000000000000, 1.000000000000000000 ) ) ;
#22456 = DIRECTION ( 'NONE',  ( 0.000000000000000000, -0.2128009952263603677, 0.9770955615653313941 ) ) ;
#22457 = VERTEX_POINT ( 'NONE', #190501 ) ;
#22458 = CARTESIAN_POINT ( 'NONE',  ( 20.94999999999999929, 1.115600667400684642E-11, -100.5000000000000426 ) ) ;
#22459 = ORIENTED_EDGE ( 'NONE', *, *, #59141, .T. ) ;
#22460 = EDGE_CURVE ( 'NONE', #124544, #222558, #255009, .T. ) ;
#22461 = CIRCLE ( 'NONE', #238922, 0.2000000000000057288 ) ;
#22462 = CIRCLE ( 'NONE', #76594, 0.09999999999999484301 ) ;
#22463 = DIRECTION ( 'NONE',  ( -1.000000000000000000, 0.000000000000000000, -0.000000000000000000 ) ) ;
#22464 = EDGE_LOOP ( 'NONE', ( #135728, #5547, #148841, #124685 ) ) ;
#22465 = DIRECTION ( 'NONE',  ( 1.000000000000000000, -3.265361837132813093E-16, -2.280189983783949500E-30 ) ) ;
#22466 = VECTOR ( 'NONE', #196610, 1000.000000000000000 ) ;
#22467 = ORIENTED_EDGE ( 'NONE', *, *, #138807, .F. ) ;
#22468 = FACE_BOUND ( 'NONE', #45603, .T. ) ;
#22469 = CIRCLE ( 'NONE', #255623, 0.09999999999999939493 ) ;
#22470 = AXIS2_PLACEMENT_3D ( 'NONE', #222747, #7568, #8857 ) ;
#22471 = DIRECTION ( 'NONE',  ( -7.304098846218135653E-16, -0.9770955615653315052, -0.2128009952263603954 ) ) ;
#22472 = EDGE_LOOP ( 'NONE', ( #237729, #178792 ) ) ;
#22473 = CIRCLE ( 'NONE', #168241, 0.09999999999999939493 ) ;
#22474 = CARTESIAN_POINT ( 'NONE',  ( 23.14999999999999503, 17.01923898301590654, -224.3994341343041867 ) ) ;
#22475 = CARTESIAN_POINT ( 'NONE',  ( -20.85000000000000142, 36.65892442174935439, -249.5511627012433848 ) ) ;
#22476 = DIRECTION ( 'NONE',  ( 1.000000000000000000, 0.000000000000000000, 0.000000000000000000 ) ) ;
#22478 = AXIS2_PLACEMENT_3D ( 'NONE', #63474, #42638, #24383 ) ;
#22477 = CARTESIAN_POINT ( 'NONE',  ( -23.15000000000000213, 28.42524210734032053, -258.3567845160494585 ) ) ;
#22479 = CARTESIAN_POINT ( 'NONE',  ( -21.05000000000000071, 70.10000000001193143, -92.80400771986793984 ) ) ;
#22480 = AXIS2_PLACEMENT_3D ( 'NONE', #159276, #103112, #238801 ) ;
#22481 = CARTESIAN_POINT ( 'NONE',  ( 19.80993210785520375, 62.37380685587606166, -208.8759191578901664 ) ) ;
#22482 = ORIENTED_EDGE ( 'NONE', *, *, #29671, .T. ) ;
#22484 = LINE ( 'NONE', #223212, #124229 ) ;
#22483 = DIRECTION ( 'NONE',  ( 1.000000000000000000, 0.000000000000000000, 0.000000000000000000 ) ) ;
#22485 = ORIENTED_EDGE ( 'NONE', *, *, #187398, .T. ) ;
#22487 = EDGE_LOOP ( 'NONE', ( #138303, #242618, #184300, #246209 ) ) ;
#22486 = FACE_OUTER_BOUND ( 'NONE', #176396, .T. ) ;
#22488 = CIRCLE ( 'NONE', #205603, 0.2000000000000005107 ) ;
#22489 = ORIENTED_EDGE ( 'NONE', *, *, #228719, .T. ) ;
#22490 = CYLINDRICAL_SURFACE ( 'NONE', #157229, 12.87499999999999822 ) ;
#22491 = CARTESIAN_POINT ( 'NONE',  ( -21.05000000000000071, 67.23127455305841238, -235.8551265064783991 ) ) ;
#22492 = CARTESIAN_POINT ( 'NONE',  ( 21.08804281139606474, 60.21242112883888353, -221.1554135929782490 ) ) ;
#22493 = DIRECTION ( 'NONE',  ( 1.000000000000000000, 2.885090398161910739E-16, 6.283419270304611573E-17 ) ) ;
#22494 = VERTEX_POINT ( 'NONE', #170965 ) ;
#22495 = DIRECTION ( 'NONE',  ( -0.000000000000000000, 0.1350103645451807555, 0.9908441862701610203 ) ) ;
#22496 = B_SPLINE_CURVE_WITH_KNOTS ( 'NONE', 3,
 ( #232960, #107849, #231672, #129963, #191272, #92138, #112995, #12628, #247354, #227792, #153449, #54283, #171714, #249935, #251197, #72600, #13897, #252483, #93413 ),
 .UNSPECIFIED., .F., .F.,
 ( 4, 3, 3, 3, 3, 3, 4 ),
 ( 0.0001624081864585792971, 0.0001685232196531718575, 0.0001764526673566863891, 0.0001916878551483168600, 0.0002009890782182536747, 0.0002238845907555072430, 0.0002283406619926262157 ),
 .UNSPECIFIED. ) ;
#22498 = DIRECTION ( 'NONE',  ( 0.000000000000000000, -1.000000000000000000, 0.000000000000000000 ) ) ;
#22497 = AXIS2_PLACEMENT_3D ( 'NONE', #238547, #59889, #42923 ) ;
#22499 = ORIENTED_EDGE ( 'NONE', *, *, #81204, .F. ) ;
#22500 = FACE_OUTER_BOUND ( 'NONE', #158968, .T. ) ;
#22501 = AXIS2_PLACEMENT_3D ( 'NONE', #55903, #76774, #19381 ) ;
#22502 = ADVANCED_FACE ( 'NONE', ( #238584 ), #15721, .F. ) ;
#22503 = CARTESIAN_POINT ( 'NONE',  ( -18.59999999999999787, 77.83585931145600512, -158.5186683157258187 ) ) ;
#22504 = ORIENTED_EDGE ( 'NONE', *, *, #8496, .F. ) ;
#22505 = CYLINDRICAL_SURFACE ( 'NONE', #193597, 0.09999999999999939493 ) ;
#22506 = TOROIDAL_SURFACE ( 'NONE', #247320, 1.900000000000002576, 0.1000000000000000056 ) ;
#22507 = AXIS2_PLACEMENT_3D ( 'NONE', #13762, #108993, #170317 ) ;
#22508 = LINE ( 'NONE', #146271, #221374 ) ;
#22509 = EDGE_LOOP ( 'NONE', ( #123737, #24257, #176427, #24129, #167078, #198883, #70180, #212052, #185227, #104237 ) ) ;
#22510 = EDGE_CURVE ( 'NONE', #206239, #141897, #40426, .T. ) ;
#22511 = DIRECTION ( 'NONE',  ( 0.000000000000000000, -1.224646799142185182E-16, 1.000000000000000000 ) ) ;
#22512 = CYLINDRICAL_SURFACE ( 'NONE', #9892, 0.1000000000000028644 ) ;
#22513 = EDGE_CURVE ( 'NONE', #112321, #230038, #153629, .T. ) ;
#22514 = ADVANCED_FACE ( 'NONE', ( #56072 ), #135618, .F. ) ;
#22515 = AXIS2_PLACEMENT_3D ( 'NONE', #196030, #213006, #95621 ) ;
#22516 = DIRECTION ( 'NONE',  ( 0.000000000000000000, 0.4930308989875575865, 0.8700118002898125091 ) ) ;
#22517 = DIRECTION ( 'NONE',  ( 0.000000000000000000, 0.000000000000000000, -1.000000000000000000 ) ) ;
#22518 = STYLED_ITEM ( 'NONE', ( #43559 ), #25658 ) ;
#22519 = AXIS2_PLACEMENT_3D ( 'NONE', #226202, #47589, #127146 ) ;
#22520 = ORIENTED_EDGE ( 'NONE', *, *, #180898, .F. ) ;
#22522 = FACE_OUTER_BOUND ( 'NONE', #203132, .T. ) ;
#22521 = CARTESIAN_POINT ( 'NONE',  ( -21.05000000000000071, 1.115600667400684642E-11, -200.9999999999999432 ) ) ;
#22523 = ORIENTED_EDGE ( 'NONE', *, *, #12353, .T. ) ;
#22524 = CARTESIAN_POINT ( 'NONE',  ( 15.74999999999999645, 66.15000000001185754, -86.27310748452437394 ) ) ;
#22525 = ADVANCED_FACE ( 'NONE', ( #156520 ), #215169, .F. ) ;
#22526 = DIRECTION ( 'NONE',  ( -1.000000000000000000, 2.952720810173289112E-16, 2.061873921506763405E-30 ) ) ;
#22528 = ORIENTED_EDGE ( 'NONE', *, *, #141988, .T. ) ;
#22527 = DIRECTION ( 'NONE',  ( 1.000000000000000000, 0.000000000000000000, 0.000000000000000000 ) ) ;
#22529 = CARTESIAN_POINT ( 'NONE',  ( -18.69999999999999929, 2.168342339202988800, -13.59640602015278432 ) ) ;
#22530 = CARTESIAN_POINT ( 'NONE',  ( 18.60000000000001208, 47.04012343383972450, -255.1614814433716845 ) ) ;
#22531 = CARTESIAN_POINT ( 'NONE',  ( 18.59999999999999787, 46.53760404070597900, -243.0973507280067167 ) ) ;
#22532 = DIRECTION ( 'NONE',  ( 0.000000000000000000, 8.326672684688666480E-14, 1.000000000000000000 ) ) ;
#22533 = CARTESIAN_POINT ( 'NONE',  ( 20.94999999999999574, -11.74999999998883560, -103.4000000000000341 ) ) ;
#22535 = ORIENTED_EDGE ( 'NONE', *, *, #171744, .T. ) ;
#22534 = DIRECTION ( 'NONE',  ( -1.000000000000000000, 0.000000000000000000, 0.000000000000000000 ) ) ;
#22536 = CIRCLE ( 'NONE', #97499, 0.09999999999998898659 ) ;
#22537 = ORIENTED_EDGE ( 'NONE', *, *, #127164, .T. ) ;
#22538 = ADVANCED_FACE ( 'NONE', ( #61232 ), #198171, .F. ) ;
#22539 = ORIENTED_EDGE ( 'NONE', *, *, #108607, .F. ) ;
#22540 = CARTESIAN_POINT ( 'NONE',  ( 21.05000000000000071, 1.115600667400684642E-11, -97.60000000000005116 ) ) ;
#22541 = DIRECTION ( 'NONE',  ( 1.000000000000000000, 0.000000000000000000, 0.000000000000000000 ) ) ;
#22542 = ORIENTED_EDGE ( 'NONE', *, *, #47214, .T. ) ;
#22543 = DIRECTION ( 'NONE',  ( 1.000000000000000000, 0.000000000000000000, 0.000000000000000000 ) ) ;
#22545 = EDGE_CURVE ( 'NONE', #6026, #134468, #119958, .T. ) ;
#22544 = CARTESIAN_POINT ( 'NONE',  ( -16.86337532320262156, 9.979967204235514089, -180.0510755310171476 ) ) ;
#22546 = ORIENTED_EDGE ( 'NONE', *, *, #229832, .F. ) ;
#22547 = AXIS2_PLACEMENT_3D ( 'NONE', #101728, #126455, #143449 ) ;
#22548 = FACE_OUTER_BOUND ( 'NONE', #149635, .T. ) ;
#22549 = CIRCLE ( 'NONE', #93435, 0.1000000000000028644 ) ;
#22550 = CIRCLE ( 'NONE', #139019, 0.1000000000000028644 ) ;
#22551 = LINE ( 'NONE', #110737, #38859 ) ;
#22552 = VECTOR ( 'NONE', #157377, 1000.000000000000000 ) ;
#22553 = ORIENTED_EDGE ( 'NONE', *, *, #85293, .F. ) ;
#22554 = ORIENTED_EDGE ( 'NONE', *, *, #12273, .T. ) ;
#22555 = DIRECTION ( 'NONE',  ( 0.000000000000000000, 0.000000000000000000, 1.000000000000000000 ) ) ;
#22556 = ORIENTED_EDGE ( 'NONE', *, *, #39750, .T. ) ;
#22557 = CARTESIAN_POINT ( 'NONE',  ( -20.64999999999999858, 1.115600667400684642E-11, -167.5000000000000284 ) ) ;
#22558 = ORIENTED_EDGE ( 'NONE', *, *, #30630, .T. ) ;
#22560 = VERTEX_POINT ( 'NONE', #16989 ) ;
#22559 = CARTESIAN_POINT ( 'NONE',  ( 18.59999999999997655, 78.06784868750165174, -195.8985418047209350 ) ) ;
#22561 = ORIENTED_EDGE ( 'NONE', *, *, #201304, .F. ) ;
#22562 = CARTESIAN_POINT ( 'NONE',  ( -18.50000000000000000, -1.835859311432484375, -78.50443916879852679 ) ) ;
#22563 = ORIENTED_EDGE ( 'NONE', *, *, #212869, .T. ) ;
#22565 = VERTEX_POINT ( 'NONE', #160366 ) ;
#22564 = EDGE_LOOP ( 'NONE', ( #193218, #224737, #75319, #132310, #36146 ) ) ;
#22567 = CARTESIAN_POINT ( 'NONE',  ( -18.50000000000000000, -1.835341550213255957, -45.05515129256298223 ) ) ;
#22566 = CIRCLE ( 'NONE', #122527, 12.87499999999999112 ) ;
#22568 = CARTESIAN_POINT ( 'NONE',  ( -20.99551997958471361, 56.17759395754637808, -227.9318432312958294 ) ) ;
#22569 = ORIENTED_EDGE ( 'NONE', *, *, #205139, .T. ) ;
#22570 = VECTOR ( 'NONE', #239752, 1000.000000000000000 ) ;
#22571 = CIRCLE ( 'NONE', #168356, 0.09999999999999939493 ) ;
#22572 = CIRCLE ( 'NONE', #110039, 4.049999999999998046 ) ;
#22573 = ADVANCED_FACE ( 'NONE', ( #20849 ), #174812, .F. ) ;
#22575 = ADVANCED_FACE ( 'NONE', ( #100330 ), #96484, .T. ) ;
#22574 = VECTOR ( 'NONE', #35608, 1000.000000000000114 ) ;
#22576 = ORIENTED_EDGE ( 'NONE', *, *, #215047, .T. ) ;
#22577 = DIRECTION ( 'NONE',  ( -1.000000000000000000, 0.000000000000000000, 0.000000000000000000 ) ) ;
#22578 = CYLINDRICAL_SURFACE ( 'NONE', #113847, 0.5000000000000004441 ) ;
#22580 = ORIENTED_EDGE ( 'NONE', *, *, #188559, .T. ) ;
#22579 = FACE_OUTER_BOUND ( 'NONE', #42947, .T. ) ;
#22581 = PLANE ( 'NONE',  #114723 ) ;
#22582 = VERTEX_POINT ( 'NONE', #155235 ) ;
#22583 = ADVANCED_FACE ( 'NONE', ( #138180 ), #258098, .F. ) ;
#22585 = ADVANCED_FACE ( 'NONE', ( #256805 ), #216101, .F. ) ;
#22584 = PLANE ( 'NONE',  #78652 ) ;
#22586 = LINE ( 'NONE', #162102, #102200 ) ;
#22587 = VERTEX_POINT ( 'NONE', #76937 ) ;
#22588 = CIRCLE ( 'NONE', #118447, 0.09999999999999939493 ) ;
#22589 = DIRECTION ( 'NONE',  ( 0.000000000000000000, 6.577889128801576950E-15, -1.000000000000000000 ) ) ;
#22590 = DIRECTION ( 'NONE',  ( 2.952720810173289112E-16, -1.000000000000000000, 0.000000000000000000 ) ) ;
#22591 = CARTESIAN_POINT ( 'NONE',  ( 21.05000000000000426, 65.43724016256105358, -129.0662935266057900 ) ) ;
#22592 = CIRCLE ( 'NONE', #168374, 0.1000000000000028644 ) ;
#22593 = EDGE_CURVE ( 'NONE', #145347, #185004, #195477, .T. ) ;
#22594 = VERTEX_POINT ( 'NONE', #236011 ) ;
#22595 = CARTESIAN_POINT ( 'NONE',  ( -20.94999999999999929, -11.48912529306490349, -36.60000000000000142 ) ) ;
#22596 = ORIENTED_EDGE ( 'NONE', *, *, #230854, .T. ) ;
#22597 = CIRCLE ( 'NONE', #151603, 0.09999999999999939493 ) ;
#22598 = ADVANCED_FACE ( 'NONE', ( #196883 ), #18256, .T. ) ;
#22600 = EDGE_CURVE ( 'NONE', #232353, #179165, #181988, .T. ) ;
#22599 = ADVANCED_FACE ( 'NONE', ( #237309 ), #191190, .F. ) ;
#22602 = ORIENTED_EDGE ( 'NONE', *, *, #36412, .F. ) ;
#22601 = VECTOR ( 'NONE', #183863, 1000.000000000000000 ) ;
#22603 = ORIENTED_EDGE ( 'NONE', *, *, #44203, .F. ) ;
#22604 = DIRECTION ( 'NONE',  ( 1.000000000000000000, 0.000000000000000000, 0.000000000000000000 ) ) ;
#22605 = ORIENTED_EDGE ( 'NONE', *, *, #79120, .F. ) ;
#22606 = DIRECTION ( 'NONE',  ( 1.000000000000000000, 0.000000000000000000, -0.000000000000000000 ) ) ;
#22607 = ADVANCED_FACE ( 'NONE', ( #200746 ), #126337, .F. ) ;
#22608 = ORIENTED_EDGE ( 'NONE', *, *, #119729, .F. ) ;
#22609 = CARTESIAN_POINT ( 'NONE',  ( -21.05000000000000071, -1.162701749926853712, -108.6000000000000227 ) ) ;
#22610 = B_SPLINE_CURVE_WITH_KNOTS ( 'NONE', 3,
 ( #232301, #114898, #37952, #134434, #191898, #116204, #173648, #36680, #113612, #95336, #15833, #174930, #236127, #255642, #57470, #154074, #53643, #74535, #75780, #137029, #112343, #32837 ),
 .UNSPECIFIED., .F., .F.,
 ( 4, 3, 3, 3, 3, 3, 3, 4 ),
 ( 0.000000000000000000, 7.307836821071800646E-06, 4.161455748548169948E-05, 7.576591810647022036E-05, 0.0001098090429817492279, 0.0001438003617351094759, 0.0001777914035423671713, 0.0002117966137402901058 ),
 .UNSPECIFIED. ) ;
#22611 = CIRCLE ( 'NONE', #47509, 0.09999999999998898659 ) ;
#22612 = CIRCLE ( 'NONE', #251534, 0.1000000000000028644 ) ;
#22613 = FACE_OUTER_BOUND ( 'NONE', #124923, .T. ) ;
#22614 = VECTOR ( 'NONE', #149460, 1000.000000000000000 ) ;
#22615 = ORIENTED_EDGE ( 'NONE', *, *, #224280, .F. ) ;
#22616 = ADVANCED_FACE ( 'NONE', ( #44248 ), #8029, .F. ) ;
#22617 = ORIENTED_EDGE ( 'NONE', *, *, #87980, .F. ) ;
#22618 = EDGE_CURVE ( 'NONE', #74828, #46212, #186325, .T. ) ;
#22619 = EDGE_CURVE ( 'NONE', #246378, #189583, #7692, .T. ) ;
#22620 = ORIENTED_EDGE ( 'NONE', *, *, #201196, .F. ) ;
#22621 = B_SPLINE_CURVE_WITH_KNOTS ( 'NONE', 3,
 ( #154744, #16512, #93447, #173048, #153491, #135134, #36070, #232999, #214684, #195162, #96013, #255032, #129999, #209563, #30956, #170489 ),
 .UNSPECIFIED., .F., .F.,
 ( 4, 3, 3, 3, 3, 4 ),
 ( 0.000000000000000000, 1.810570668010556722E-05, 2.740575833571567380E-05, 4.256816319435758028E-05, 5.213463471025523268E-05, 6.641585710718234082E-05 ),
 .UNSPECIFIED. ) ;
#22622 = EDGE_CURVE ( 'NONE', #219341, #257571, #224484, .T. ) ;
#22623 = CARTESIAN_POINT ( 'NONE',  ( -16.92778301347276582, 65.99905508317655745, -82.09458937655523414 ) ) ;
#22624 = ORIENTED_EDGE ( 'NONE', *, *, #123355, .F. ) ;
#22625 = CARTESIAN_POINT ( 'NONE',  ( 21.03670563405601968, 13.00435671336279064, -210.7822641011882183 ) ) ;
#22626 = DIRECTION ( 'NONE',  ( 0.000000000000000000, -0.9126074666063770380, -0.4088369013363281068 ) ) ;
#22627 = CARTESIAN_POINT ( 'NONE',  ( -21.02374657821588855, 11.60000000083177696, -127.0717967701983326 ) ) ;
#22628 = ADVANCED_FACE ( 'NONE', ( #101600 ), #122503, .T. ) ;
#22629 = CARTESIAN_POINT ( 'NONE',  ( 21.05000000000000071, 26.06832281015329755, -254.4051978787608732 ) ) ;
#22630 = CARTESIAN_POINT ( 'NONE',  ( 23.24999999999997513, 11.75000000001116263, -126.9851942293460922 ) ) ;
#22631 = LINE ( 'NONE', #102112, #93911 ) ;
#22632 = AXIS2_PLACEMENT_3D ( 'NONE', #253243, #211570, #232433 ) ;
#22634 = CARTESIAN_POINT ( 'NONE',  ( -20.64999999999999858, 11.36448785225375602, -246.7787679937655980 ) ) ;
#22633 = LINE ( 'NONE', #102113, #90448 ) ;
#22635 = DIRECTION ( 'NONE',  ( 0.000000000000000000, 0.000000000000000000, -1.000000000000000000 ) ) ;
#22637 = ADVANCED_FACE ( 'NONE', ( #82041 ), #142045, .T. ) ;
#22636 = CARTESIAN_POINT ( 'NONE',  ( 20.00000000000000711, 4.547418889303921574, 21.90000000000000213 ) ) ;
#22638 = CIRCLE ( 'NONE', #10149, 3.970710678118653636 ) ;
#22639 = CARTESIAN_POINT ( 'NONE',  ( -19.89999999999999858, 1.250000000000000000, 16.60000000000000142 ) ) ;
#22641 = CARTESIAN_POINT ( 'NONE',  ( 21.10710606213542206, 44.24183109435373495, -236.5367325923057251 ) ) ;
#22640 = AXIS2_PLACEMENT_3D ( 'NONE', #94632, #55472, #253702 ) ;
#22642 = ORIENTED_EDGE ( 'NONE', *, *, #117083, .T. ) ;
#22643 = VECTOR ( 'NONE', #99135, 999.9999999999998863 ) ;
#22644 = VECTOR ( 'NONE', #213465, 1000.000000000000227 ) ;
#22646 = EDGE_LOOP ( 'NONE', ( #11247, #94298, #179848, #144607 ) ) ;
#22645 = CARTESIAN_POINT ( 'NONE',  ( -23.15000000000000213, 2.272311100394799332, -217.9150152700588592 ) ) ;
#22647 = ORIENTED_EDGE ( 'NONE', *, *, #121668, .F. ) ;
#22648 = EDGE_CURVE ( 'NONE', #139488, #80050, #116183, .T. ) ;
#22649 = DIRECTION ( 'NONE',  ( 1.000000000000000000, 0.000000000000000000, 0.000000000000000000 ) ) ;
#22650 = DIRECTION ( 'NONE',  ( 0.000000000000000000, 0.000000000000000000, 1.000000000000000000 ) ) ;
#22651 = CIRCLE ( 'NONE', #63755, 0.09999999999999939493 ) ;
#22652 = CARTESIAN_POINT ( 'NONE',  ( -22.49072729836729678, 64.12733727798033101, -247.0841716932466738 ) ) ;
#22653 = ORIENTED_EDGE ( 'NONE', *, *, #249770, .T. ) ;
#22654 = AXIS2_PLACEMENT_3D ( 'NONE', #64634, #223692, #45074 ) ;
#22655 =( NAMED_UNIT ( * ) PLANE_ANGLE_UNIT ( ) SI_UNIT ( $, .RADIAN. ) );
#22656 = AXIS2_PLACEMENT_3D ( 'NONE', #50317, #110312, #106433 ) ;
#22657 = CARTESIAN_POINT ( 'NONE',  ( 21.14999999999999858, 56.01362831242965967, -232.7091905853083347 ) ) ;
#22658 = VECTOR ( 'NONE', #205432, 1000.000000000000000 ) ;
#22659 = PRODUCT_DEFINITION_SHAPE ( 'NONE', 'NONE',  #258109 ) ;
#22660 = CARTESIAN_POINT ( 'NONE',  ( -23.15000000000000213, 35.97645343225766368, -235.9694016464868298 ) ) ;
#22661 = ORIENTED_EDGE ( 'NONE', *, *, #43716, .T. ) ;
#22662 = AXIS2_PLACEMENT_3D ( 'NONE', #252493, #235501, #129971 ) ;
#22663 = CARTESIAN_POINT ( 'NONE',  ( -21.03922262424684675, 11.62390063401601381, -140.8592080428932718 ) ) ;
#22664 = DIRECTION ( 'NONE',  ( 1.000000000000000000, 0.000000000000000000, 0.000000000000000000 ) ) ;
#22665 = DIRECTION ( 'NONE',  ( 7.304098846218134667E-16, 1.000000000000000000, 6.982962677686266711E-15 ) ) ;
#22666 = FACE_OUTER_BOUND ( 'NONE', #151256, .T. ) ;
#22668 = VERTEX_POINT ( 'NONE', #42959 ) ;
#22667 = LINE ( 'NONE', #220832, #52021 ) ;
#22669 = AXIS2_PLACEMENT_3D ( 'NONE', #17570, #253611, #155836 ) ;
#22670 = DIRECTION ( 'NONE',  ( -0.000000000000000000, -0.000000000000000000, -1.000000000000000000 ) ) ;
#22672 = ORIENTED_EDGE ( 'NONE', *, *, #82560, .F. ) ;
#22671 = CARTESIAN_POINT ( 'NONE',  ( -21.05000000000000071, 31.98723526783714988, -238.8784020251475511 ) ) ;
#22673 = FACE_OUTER_BOUND ( 'NONE', #116157, .T. ) ;
#22674 = LINE ( 'NONE', #80014, #116616 ) ;
#22675 = CARTESIAN_POINT ( 'NONE',  ( -16.93772744219066340, 66.00645889125993904, -157.4250455125547035 ) ) ;
#22676 = CARTESIAN_POINT ( 'NONE',  ( -12.47155713865591942, 9.375669526436931633, -183.3677900093859705 ) ) ;
#22677 = AXIS2_PLACEMENT_3D ( 'NONE', #214691, #135140, #37366 ) ;
#22678 = EDGE_CURVE ( 'NONE', #203793, #250577, #112077, .T. ) ;
#22680 = CARTESIAN_POINT ( 'NONE',  ( 13.40000000000000036, -8.279289321881350361, 18.97071067811865674 ) ) ;
#22679 = DIRECTION ( 'NONE',  ( -2.940209281316621016E-16, -1.000000000000000000, -7.056502275159890832E-15 ) ) ;
#22681 = CARTESIAN_POINT ( 'NONE',  ( -21.05000000000000071, 34.01125473725046078, -243.8802146427659352 ) ) ;
#22682 = CARTESIAN_POINT ( 'NONE',  ( 20.95512820512820440, 40.84069494668059264, -237.9516373772122222 ) ) ;
#22683 = DIRECTION ( 'NONE',  ( 1.000000000000000000, 0.000000000000000000, 0.000000000000000000 ) ) ;
#22684 = DIRECTION ( 'NONE',  ( 0.000000000000000000, 0.2617529984164915779, 0.9651348961777187485 ) ) ;
#22685 = EDGE_CURVE ( 'NONE', #214983, #182339, #104190, .T. ) ;
#22686 = CARTESIAN_POINT ( 'NONE',  ( 21.08621493067296271, 10.07738939570518255, -228.1092937118111195 ) ) ;
#22688 = ORIENTED_EDGE ( 'NONE', *, *, #117429, .F. ) ;
#22687 = AXIS2_PLACEMENT_3D ( 'NONE', #105907, #129350, #90201 ) ;
#22689 = DIRECTION ( 'NONE',  ( 0.000000000000000000, 0.2128009952263618110, -0.9770955615653312831 ) ) ;
#22690 = CIRCLE ( 'NONE', #47583, 0.3999999999999994671 ) ;
#22691 = VERTEX_POINT ( 'NONE', #182483 ) ;
#22692 = VERTEX_POINT ( 'NONE', #144601 ) ;
#22693 = EDGE_CURVE ( 'NONE', #99386, #194512, #183754, .T. ) ;
#22694 = CARTESIAN_POINT ( 'NONE',  ( -20.99551997958405991, 11.75000000000017941, -26.65165913768950290 ) ) ;
#22695 = EDGE_CURVE ( 'NONE', #4930, #205409, #71765, .T. ) ;
#22696 = DIRECTION ( 'NONE',  ( 0.000000000000000000, -6.982962677686266711E-15, 1.000000000000000000 ) ) ;
#22697 = ORIENTED_EDGE ( 'NONE', *, *, #129500, .T. ) ;
#22698 = EDGE_CURVE ( 'NONE', #67239, #188768, #107969, .T. ) ;
#22699 = ORIENTED_EDGE ( 'NONE', *, *, #137075, .T. ) ;
#22700 =( NAMED_UNIT ( * ) PLANE_ANGLE_UNIT ( ) SI_UNIT ( $, .RADIAN. ) );
#22701 = ORIENTED_EDGE ( 'NONE', *, *, #192464, .F. ) ;
#22702 = CARTESIAN_POINT ( 'NONE',  ( 18.59999999999999076, 7.120270961708750512, -104.1595630418393768 ) ) ;
#22703 = CIRCLE ( 'NONE', #18597, 0.09999999999999971412 ) ;
#22704 = ORIENTED_EDGE ( 'NONE', *, *, #226216, .T. ) ;
#22705 = EDGE_CURVE ( 'NONE', #151216, #91092, #187093, .T. ) ;
#22706 = DIRECTION ( 'NONE',  ( 0.000000000000000000, 0.000000000000000000, 1.000000000000000000 ) ) ;
#22707 = DIRECTION ( 'NONE',  ( -3.265361837132813093E-16, -1.000000000000000000, -6.982962677686266711E-15 ) ) ;
#22708 = DIRECTION ( 'NONE',  ( 2.952720810173289112E-16, -1.000000000000000000, 0.000000000000000000 ) ) ;
#22709 = CARTESIAN_POINT ( 'NONE',  ( 18.50000000000000000, -9.499999999988842703, -174.5320693966996259 ) ) ;
#22710 = CARTESIAN_POINT ( 'NONE',  ( 20.94999999999999929, 20.97908333644147660, -233.6079013178409411 ) ) ;
#22711 = CIRCLE ( 'NONE', #14898, 0.1000000000000124678 ) ;
#22712 =( BOUNDED_CURVE ( )  B_SPLINE_CURVE ( 3, ( #227470, #48840, #207945, #192227 ),
 .UNSPECIFIED., .F., .F. ) 
 B_SPLINE_CURVE_WITH_KNOTS ( ( 4, 4 ),
 ( 1.570796326794885012, 3.141592653589794448 ),
 .UNSPECIFIED. ) 
 CURVE ( )  GEOMETRIC_REPRESENTATION_ITEM ( )  RATIONAL_B_SPLINE_CURVE ( ( 1.000000000000000000, 0.8047378541243619399, 0.8047378541243619399, 1.000000000000000000 ) ) 
 REPRESENTATION_ITEM ( '' )  );
#22713 = DIRECTION ( 'NONE',  ( 1.000000000000000000, 0.000000000000000000, 0.000000000000000000 ) ) ;
#22714 = LINE ( 'NONE', #44818, #116096 ) ;
#22716 = VERTEX_POINT ( 'NONE', #251422 ) ;
#22715 = DIRECTION ( 'NONE',  ( 1.000000000000000000, 0.000000000000000000, 0.000000000000000000 ) ) ;
#22718 = DIRECTION ( 'NONE',  ( -0.000000000000000000, 0.1298341882520054891, 0.9915357197604850459 ) ) ;
#22717 = CARTESIAN_POINT ( 'NONE',  ( 20.95378194480896639, 65.46508800846882536, -61.95805333637653689 ) ) ;
#22719 = CYLINDRICAL_SURFACE ( 'NONE', #15271, 0.5000000000000004441 ) ;
#22720 = EDGE_LOOP ( 'NONE', ( #140434, #254809 ) ) ;
#22721 = CARTESIAN_POINT ( 'NONE',  ( -18.45068461519106151, 8.880466068112633948, -245.4328380456663581 ) ) ;
#22722 = CARTESIAN_POINT ( 'NONE',  ( -23.25000000000000000, -0.1008583690875562017, -155.7504328765105868 ) ) ;
#22723 = ORIENTED_EDGE ( 'NONE', *, *, #52338, .F. ) ;
#22725 = LINE ( 'NONE', #220884, #191557 ) ;
#22724 = DIRECTION ( 'NONE',  ( 0.000000000000000000, 0.000000000000000000, 1.000000000000000000 ) ) ;
#22726 = CARTESIAN_POINT ( 'NONE',  ( -20.54999999999999716, 74.00000000001186606, -89.79848556176222019 ) ) ;
#22727 = EDGE_CURVE ( 'NONE', #203977, #5409, #248862, .T. ) ;
#22728 = ORIENTED_EDGE ( 'NONE', *, *, #254760, .T. ) ;
#22730 = CARTESIAN_POINT ( 'NONE',  ( -21.05000000000000071, -9.519327731081284938, -73.97297637655937308 ) ) ;
#22729 = CIRCLE ( 'NONE', #251657, 11.64999999999999325 ) ;
#22731 = DIRECTION ( 'NONE',  ( -1.000000000000000000, 0.000000000000000000, -0.000000000000000000 ) ) ;
#22732 = CARTESIAN_POINT ( 'NONE',  ( 20.94999999999999574, 77.25000000001263345, -195.5231074845243313 ) ) ;
#22733 = CARTESIAN_POINT ( 'NONE',  ( -22.50000000000088463, 0.04536165659896403135, -122.3494911657900843 ) ) ;
#22734 = ORIENTED_EDGE ( 'NONE', *, *, #230399, .T. ) ;
#22735 = ADVANCED_FACE ( 'NONE', ( #92343 ), #182827, .F. ) ;
#22736 = EDGE_CURVE ( 'NONE', #249506, #146300, #145365, .T. ) ;
#22737 = CARTESIAN_POINT ( 'NONE',  ( -18.59999999999999787, 74.44087353924872730, -232.6253149859214773 ) ) ;
#22738 = CARTESIAN_POINT ( 'NONE',  ( 18.59999999999999076, 29.08883969319483498, -237.9520757887960940 ) ) ;
#22739 = CARTESIAN_POINT ( 'NONE',  ( 23.25000000000000000, 61.47936603916258491, -212.1738987416902376 ) ) ;
#22740 = AXIS2_PLACEMENT_3D ( 'NONE', #54611, #216245, #174627 ) ;
#22741 = DIRECTION ( 'NONE',  ( 1.000000000000000000, 0.000000000000000000, 0.000000000000000000 ) ) ;
#22742 = AXIS2_PLACEMENT_3D ( 'NONE', #70626, #150152, #69325 ) ;
#22743 = FACE_OUTER_BOUND ( 'NONE', #232049, .T. ) ;
#22744 = VECTOR ( 'NONE', #159971, 1000.000000000000000 ) ;
#22745 = AXIS2_PLACEMENT_3D ( 'NONE', #24099, #125731, #7068 ) ;
#22746 = EDGE_CURVE ( 'NONE', #87387, #25027, #137008, .T. ) ;
#22748 = ORIENTED_EDGE ( 'NONE', *, *, #252772, .T. ) ;
#22747 = CARTESIAN_POINT ( 'NONE',  ( 21.08832698747859169, 8.775364393428372267, -179.7287174664641327 ) ) ;
#22749 = DIRECTION ( 'NONE',  ( -1.000000000000000000, -2.885090398161910739E-16, -6.283419270304611573E-17 ) ) ;
#22750 = CARTESIAN_POINT ( 'NONE',  ( 11.60000000000006004, 67.75000000001118394, -21.02310748452479316 ) ) ;
#22751 = FACE_OUTER_BOUND ( 'NONE', #231729, .T. ) ;
#22753 = FACE_OUTER_BOUND ( 'NONE', #248687, .T. ) ;
#22752 = MECHANICAL_DESIGN_GEOMETRIC_PRESENTATION_REPRESENTATION (  '', ( #248145 ), #80968 ) ;
#22754 = CARTESIAN_POINT ( 'NONE',  ( -21.44999999999999929, 68.75000000001253397, -182.3731074845244109 ) ) ;
#22755 = EDGE_CURVE ( 'NONE', #109096, #99184, #24609, .T. ) ;
#22757 = ORIENTED_EDGE ( 'NONE', *, *, #173304, .T. ) ;
#22756 = CARTESIAN_POINT ( 'NONE',  ( -20.94999999999999929, -1.162701749926853712, -41.60000000000000142 ) ) ;
#22758 = CARTESIAN_POINT ( 'NONE',  ( 23.15000000000000213, 86.43238724539048690, -209.5644480942280836 ) ) ;
#22759 = EDGE_CURVE ( 'NONE', #30618, #201330, #8962, .T. ) ;
#22760 = DIRECTION ( 'NONE',  ( 0.000000000000000000, -1.000000000000000000, -6.982962677686265922E-15 ) ) ;
#22761 = CARTESIAN_POINT ( 'NONE',  ( 20.89878130938411616, 67.49249915771264341, -195.4369143829851510 ) ) ;
#22762 = ORIENTED_EDGE ( 'NONE', *, *, #86115, .T. ) ;
#22763 = DIRECTION ( 'NONE',  ( 0.000000000000000000, -1.000000000000000000, 0.000000000000000000 ) ) ;
#22764 = CARTESIAN_POINT ( 'NONE',  ( 21.07954640115206857, 75.93399229287264518, -176.3523951805472905 ) ) ;
#22765 = AXIS2_PLACEMENT_3D ( 'NONE', #192821, #152428, #154988 ) ;
#22766 = EDGE_CURVE ( 'NONE', #39792, #134077, #170367, .T. ) ;
#22767 = AXIS2_PLACEMENT_3D ( 'NONE', #178205, #141611, #42506 ) ;
#22768 = DIRECTION ( 'NONE',  ( 0.000000000000000000, -1.000000000000000000, 0.000000000000000000 ) ) ;
#22770 = ORIENTED_EDGE ( 'NONE', *, *, #13671, .F. ) ;
#22769 = CIRCLE ( 'NONE', #14398, 0.1000000000000028644 ) ;
#22771 = ORIENTED_EDGE ( 'NONE', *, *, #205952, .T. ) ;
#22772 = CARTESIAN_POINT ( 'NONE',  ( 21.95218792049437440, 60.25492730956543852, -234.0656861121678673 ) ) ;
#22773 = CARTESIAN_POINT ( 'NONE',  ( -18.59999999999999787, 64.35000000001208775, -129.5083017138703667 ) ) ;
#22774 = B_SPLINE_CURVE_WITH_KNOTS ( 'NONE', 3,
 ( #79295, #18055, #256611, #158880 ),
 .UNSPECIFIED., .F., .F.,
 ( 4, 4 ),
 ( 3.878959614448864246E-18, 0.0001058379652594393101 ),
 .UNSPECIFIED. ) ;
#22775 = ADVANCED_FACE ( 'NONE', ( #109325 ), #28581, .T. ) ;
#22776 = CARTESIAN_POINT ( 'NONE',  ( 23.24999999999999645, 11.75000000001113953, -121.3500000000000227 ) ) ;
#22777 = CARTESIAN_POINT ( 'NONE',  ( 23.15000000000000213, 85.00000000001149658, -45.41707660717670336 ) ) ;
#22778 = EDGE_LOOP ( 'NONE', ( #112292, #37221, #114318, #8487 ) ) ;
#22779 = CARTESIAN_POINT ( 'NONE',  ( 20.95132126680579887, 10.48994987015794322, -175.0703245384344768 ) ) ;
#22780 = CIRCLE ( 'NONE', #39545, 0.1000000000000028644 ) ;
#22781 = TOROIDAL_SURFACE ( 'NONE', #43420, 4.099999999999999645, 0.1000000000000000056 ) ;
#22782 = AXIS2_PLACEMENT_3D ( 'NONE', #108100, #143361, #83362 ) ;
#22783 = CARTESIAN_POINT ( 'NONE',  ( 21.05000000000000071, 7.128833340093095217, -233.7327013124392749 ) ) ;
#22784 = AXIS2_PLACEMENT_3D ( 'NONE', #86601, #145303, #141460 ) ;
#22785 = DIRECTION ( 'NONE',  ( 0.000000000000000000, 0.000000000000000000, 1.000000000000000000 ) ) ;
#22786 = DIRECTION ( 'NONE',  ( 0.000000000000000000, -1.000000000000000000, -0.000000000000000000 ) ) ;
#22787 = VECTOR ( 'NONE', #226688, 1000.000000000000227 ) ;
#22788 = CARTESIAN_POINT ( 'NONE',  ( -16.84793658983420173, 9.949999999999983302, -20.76635332218982910 ) ) ;
#22789 = DIRECTION ( 'NONE',  ( 0.000000000000000000, 0.000000000000000000, 1.000000000000000000 ) ) ;
#22790 = ORIENTED_EDGE ( 'NONE', *, *, #4532, .T. ) ;
#22792 = ORIENTED_EDGE ( 'NONE', *, *, #25139, .T. ) ;
#22791 = DIRECTION ( 'NONE',  ( -3.787827842127534447E-15, -0.2438576117979244784, 0.9698110461157951612 ) ) ;
#22793 = CIRCLE ( 'NONE', #214309, 0.1000000000000000472 ) ;
#22794 = VERTEX_POINT ( 'NONE', #51911 ) ;
#22795 = CARTESIAN_POINT ( 'NONE',  ( -16.80469485234340610, 9.942151663141038043, -20.80996684393117135 ) ) ;
#22796 = ORIENTED_EDGE ( 'NONE', *, *, #144346, .T. ) ;
#22797 = FACE_OUTER_BOUND ( 'NONE', #99224, .T. ) ;
#22798 = DIRECTION ( 'NONE',  ( -1.000000000000000000, -0.000000000000000000, -0.000000000000000000 ) ) ;
#22799 = DIRECTION ( 'NONE',  ( -1.000000000000000000, 0.000000000000000000, 0.000000000000000000 ) ) ;
#22800 = ORIENTED_EDGE ( 'NONE', *, *, #145280, .T. ) ;
#22802 = AXIS2_PLACEMENT_3D ( 'NONE', #93410, #36031, #112991 ) ;
#22801 = DIRECTION ( 'NONE',  ( 0.000000000000000000, -0.9908441862701420355, -0.1350103645453197554 ) ) ;
#22803 = CARTESIAN_POINT ( 'NONE',  ( -18.59999999999999787, -1.835341550213255957, -78.55515129256302487 ) ) ;
#22804 = AXIS2_PLACEMENT_3D ( 'NONE', #235757, #254035, #196632 ) ;
#22805 = VERTEX_POINT ( 'NONE', #132783 ) ;
#22806 = CARTESIAN_POINT ( 'NONE',  ( 18.39999999999999858, 85.60000000001210196, -129.4910380878245633 ) ) ;
#22808 = ORIENTED_EDGE ( 'NONE', *, *, #214462, .T. ) ;
#22807 = CARTESIAN_POINT ( 'NONE',  ( -21.65000000000000213, 68.29142135624984178, -182.3731074845244109 ) ) ;
#22809 = DIRECTION ( 'NONE',  ( 1.000000000000000000, 0.000000000000000000, 0.000000000000000000 ) ) ;
#22810 = DIRECTION ( 'NONE',  ( 1.000000000000000000, -0.000000000000000000, -0.000000000000000000 ) ) ;
#22811 = EDGE_LOOP ( 'NONE', ( #164033, #138133, #157167, #223721 ) ) ;
#22812 =( BOUNDED_SURFACE ( )  B_SPLINE_SURFACE ( 3, 2, ( 
 ( #50829, #92537, #113403 ),
 ( #15617, #33916, #13042 ),
 ( #189088, #191691, #30039 ),
 ( #172133, #230801, #132979 ),
 ( #95119, #169569, #211214 ),
 ( #247771, #114683, #148691 ),
 ( #71722, #251628, #73029 ),
 ( #249078, #151258, #74309 ),
 ( #52124, #32620, #130383 ),
 ( #152562, #49575, #232083 ) ),
 .UNSPECIFIED., .F., .F., .F. ) 
 B_SPLINE_SURFACE_WITH_KNOTS ( ( 4, 2, 2, 2, 4 ),
 ( 3, 3 ),
 ( 0.0001701955120502345899, 0.0002247052511886083901, 0.0002792149903269822175, 0.0003882344686037298722, 0.0006062734251572251274 ),
 ( 0.000000000000000000, 1.000000000000000000 ),
 .UNSPECIFIED. ) 
 GEOMETRIC_REPRESENTATION_ITEM ( )  RATIONAL_B_SPLINE_SURFACE ( (
 ( 1.000000000000000000, 0.2966190024560962923, 1.000000000000000000),
 ( 1.000000000000000000, 0.2964522492710705004, 1.000000000000000000),
 ( 1.000000000000000000, 0.3059923531883924630, 1.000000000000000000),
 ( 1.000000000000000000, 0.3355751146944598862, 1.000000000000000000),
 ( 1.000000000000000000, 0.3550672384962806349, 1.000000000000000000),
 ( 1.000000000000000000, 0.4157034672182661761, 1.000000000000000000),
 ( 1.000000000000000000, 0.4588031877658533819, 1.000000000000000000),
 ( 1.000000000000000000, 0.5771441759652413683, 1.000000000000000000),
 ( 1.000000000000000000, 0.6469377121778552286, 1.000000000000000000),
 ( 1.000000000000000000, 0.7071067811865475727, 1.000000000000000000) ) ) 
 REPRESENTATION_ITEM ( '' )  SURFACE ( )  );
#22813 = SPHERICAL_SURFACE ( 'NONE', #114490, 0.1000000000000000056 ) ;
#22814 = DIRECTION ( 'NONE',  ( 0.000000000000000000, -6.982962677686266711E-15, 1.000000000000000000 ) ) ;
#22815 = DIRECTION ( 'NONE',  ( -0.000000000000000000, 0.000000000000000000, 1.000000000000000000 ) ) ;
#22816 = VERTEX_POINT ( 'NONE', #108068 ) ;
#22817 = DIRECTION ( 'NONE',  ( 1.000000000000000000, 1.836970198721029934E-16, 0.000000000000000000 ) ) ;
#22818 = EDGE_CURVE ( 'NONE', #175744, #238381, #236964, .T. ) ;
#22819 = CARTESIAN_POINT ( 'NONE',  ( 12.93279065517211457, 49.36478519392532149, -233.5395520442455961 ) ) ;
#22820 = CARTESIAN_POINT ( 'NONE',  ( -22.50000000000000000, 11.75000000001115552, -167.4999999999999716 ) ) ;
#22821 = AXIS2_PLACEMENT_3D ( 'NONE', #247617, #48126, #171976 ) ;
#22822 = EDGE_CURVE ( 'NONE', #34176, #100484, #220412, .T. ) ;
#22823 = ORIENTED_EDGE ( 'NONE', *, *, #224414, .F. ) ;
#22824 = ADVANCED_FACE ( 'NONE', ( #88471 ), #247570, .F. ) ;
#22825 = CIRCLE ( 'NONE', #147706, 12.87500000000000000 ) ;
#22826 = ORIENTED_EDGE ( 'NONE', *, *, #124257, .F. ) ;
#22827 = AXIS2_PLACEMENT_3D ( 'NONE', #254677, #189628, #35709 ) ;
#22828 = AXIS2_PLACEMENT_3D ( 'NONE', #19795, #99289, #120201 ) ;
#22829 = ORIENTED_EDGE ( 'NONE', *, *, #257539, .T. ) ;
#22830 = CARTESIAN_POINT ( 'NONE',  ( 18.50000324121758055, 10.29307482167976318, -38.95864214669396119 ) ) ;
#22831 = ADVANCED_FACE ( 'NONE', ( #208470 ), #29840, .F. ) ;
#22832 = CARTESIAN_POINT ( 'NONE',  ( 21.05000005001280172, 8.871279691782060439, -45.67794758824611279 ) ) ;
#22834 = ORIENTED_EDGE ( 'NONE', *, *, #126242, .T. ) ;
#22833 = CARTESIAN_POINT ( 'NONE',  ( -16.87372386987899375, 9.880600233647912845, -147.1492698718664940 ) ) ;
#22835 = CARTESIAN_POINT ( 'NONE',  ( 20.85000000000000142, -1.851617760468904805, -45.10318971960366241 ) ) ;
#22836 = DIRECTION ( 'NONE',  ( 0.000000000000000000, -1.000000000000000000, 0.000000000000000000 ) ) ;
#22837 = DIRECTION ( 'NONE',  ( 0.000000000000000000, 1.000000000000000000, 1.734723475976807292E-15 ) ) ;
#22838 = CARTESIAN_POINT ( 'NONE',  ( -16.89268316805465986, 51.62340874627276577, -231.9425458505251072 ) ) ;
#22839 = DIRECTION ( 'NONE',  ( 0.000000000000000000, -1.000000000000000000, 0.000000000000000000 ) ) ;
#22840 = CIRCLE ( 'NONE', #135230, 0.09999999999999939493 ) ;
#22841 = DIRECTION ( 'NONE',  ( -1.000000000000000000, -3.190570557967288949E-16, -6.948722487160392945E-17 ) ) ;
#22842 = CIRCLE ( 'NONE', #213792, 0.09999999999999939493 ) ;
#22844 = ORIENTED_EDGE ( 'NONE', *, *, #154202, .T. ) ;
#22843 = CARTESIAN_POINT ( 'NONE',  ( -16.87683809663752399, 66.15000000001259650, -190.1207434663281219 ) ) ;
#22846 = VERTEX_POINT ( 'NONE', #11546 ) ;
#22845 = CARTESIAN_POINT ( 'NONE',  ( -21.05000000000000071, 1.835341550235567887, -145.6551512925629766 ) ) ;
#22847 = CARTESIAN_POINT ( 'NONE',  ( 22.50497660315937409, -0.07871793021434789206, -55.25020449510461162 ) ) ;
#22848 = AXIS2_PLACEMENT_3D ( 'NONE', #209851, #108183, #231991 ) ;
#22849 = ORIENTED_EDGE ( 'NONE', *, *, #49668, .T. ) ;
#22850 = ORIENTED_EDGE ( 'NONE', *, *, #53712, .T. ) ;
#22851 = CARTESIAN_POINT ( 'NONE',  ( -20.00857864376270001, 66.85000000001180354, -81.77310748452437394 ) ) ;
#22852 = DIRECTION ( 'NONE',  ( 0.000000000000000000, -0.000000000000000000, -1.000000000000000000 ) ) ;
#22853 = CARTESIAN_POINT ( 'NONE',  ( -23.15000000000000213, 0.8831241302008846494, -205.0549465804976421 ) ) ;
#22854 = ADVANCED_FACE ( 'NONE', ( #169363 ), #50633, .T. ) ;
#22855 = EDGE_CURVE ( 'NONE', #25903, #166513, #190178, .T. ) ;
#22856 = CARTESIAN_POINT ( 'NONE',  ( -17.11825945287482753, 10.04999999999998295, -12.65000000000000213 ) ) ;
#22857 = CIRCLE ( 'NONE', #81072, 0.1000000000000007133 ) ;
#22858 = CARTESIAN_POINT ( 'NONE',  ( 20.13684514580103624, 66.50414460725998822, -195.3800757988351506 ) ) ;
#22859 = ORIENTED_EDGE ( 'NONE', *, *, #164497, .F. ) ;
#22860 = FACE_OUTER_BOUND ( 'NONE', #198017, .T. ) ;
#22861 = AXIS2_PLACEMENT_3D ( 'NONE', #110154, #69769, #50171 ) ;
#22862 = ORIENTED_EDGE ( 'NONE', *, *, #121865, .T. ) ;
#22863 = ORIENTED_EDGE ( 'NONE', *, *, #235168, .F. ) ;
#22864 = SURFACE_SIDE_STYLE ('',( #240597 ) ) ;
#22865 = EDGE_CURVE ( 'NONE', #79905, #132946, #253879, .T. ) ;
#22866 = ORIENTED_EDGE ( 'NONE', *, *, #32888, .F. ) ;
#22867 = VECTOR ( 'NONE', #233016, 1000.000000000000114 ) ;
#22868 = CARTESIAN_POINT ( 'NONE',  ( 22.00411653889200991, 75.90096189422573048, -177.2765503521646622 ) ) ;
#22869 = CIRCLE ( 'NONE', #118729, 0.1000000000000001860 ) ;
#22870 = FACE_OUTER_BOUND ( 'NONE', #236129, .T. ) ;
#22871 = ORIENTED_EDGE ( 'NONE', *, *, #250390, .F. ) ;
#22872 = DIRECTION ( 'NONE',  ( 0.2834754621636358385, -0.4719347312574445619, 0.8348169091388102370 ) ) ;
#22873 = VERTEX_POINT ( 'NONE', #119628 ) ;
#22874 = CARTESIAN_POINT ( 'NONE',  ( -15.15766958671843589, 9.410538608540020888, -48.93268799714089567 ) ) ;
#22875 = ORIENTED_EDGE ( 'NONE', *, *, #163616, .F. ) ;
#22876 = DIRECTION ( 'NONE',  ( -2.915501640297154283E-16, 1.000000000000000000, 0.000000000000000000 ) ) ;
#22877 = EDGE_CURVE ( 'NONE', #15592, #168233, #38804, .T. ) ;
#22878 = CARTESIAN_POINT ( 'NONE',  ( 14.56326696814970845, 9.446648990640015953, -182.5891632959231288 ) ) ;
#22879 = ORIENTED_EDGE ( 'NONE', *, *, #151809, .T. ) ;
#22880 = DIRECTION ( 'NONE',  ( 1.000000000000000000, 0.000000000000000000, 0.000000000000000000 ) ) ;
#22882 = ORIENTED_EDGE ( 'NONE', *, *, #154566, .T. ) ;
#22881 = DIRECTION ( 'NONE',  ( 0.000000000000000000, 0.000000000000000000, -1.000000000000000000 ) ) ;
#22883 = CARTESIAN_POINT ( 'NONE',  ( -22.50000000000088463, 75.95463834342507425, -215.1736163187297564 ) ) ;
#22884 = AXIS2_PLACEMENT_3D ( 'NONE', #99884, #2087, #235568 ) ;
#22885 = ORIENTED_EDGE ( 'NONE', *, *, #49141, .F. ) ;
#22886 = EDGE_CURVE ( 'NONE', #29706, #56434, #166446, .T. ) ;
#22887 = AXIS2_PLACEMENT_3D ( 'NONE', #229610, #249178, #49679 ) ;
#22888 = CARTESIAN_POINT ( 'NONE',  ( -16.97048326478264357, 66.05000000001264482, -190.3820006043973194 ) ) ;
#22889 = ORIENTED_EDGE ( 'NONE', *, *, #165970, .F. ) ;
#22890 = DIRECTION ( 'NONE',  ( 0.000000000000000000, 0.4088369013363322146, -0.9126074666063751506 ) ) ;
#22891 = DIRECTION ( 'NONE',  ( 0.000000000000000000, 0.000000000000000000, 1.000000000000000000 ) ) ;
#22892 = LINE ( 'NONE', #204060, #149472 ) ;
#22893 = DIRECTION ( 'NONE',  ( 0.000000000000000000, 6.982962677686266711E-15, -1.000000000000000000 ) ) ;
#22894 = EDGE_CURVE ( 'NONE', #148706, #218484, #154922, .T. ) ;
#22895 = EDGE_CURVE ( 'NONE', #191564, #98792, #94903, .T. ) ;
#22896 = DIRECTION ( 'NONE',  ( -1.000000000000000000, 0.000000000000000000, 0.000000000000000000 ) ) ;
#22897 = PLANE ( 'NONE',  #33928 ) ;
#22898 = ORIENTED_EDGE ( 'NONE', *, *, #5265, .F. ) ;
#22899 = DIRECTION ( 'NONE',  ( 0.000000000000000000, -0.8164989248600462712, 0.5773469543544753613 ) ) ;
#22900 = CARTESIAN_POINT ( 'NONE',  ( -23.15000000000000213, 17.01923898301589944, -224.3994341343041867 ) ) ;
#22901 = DIRECTION ( 'NONE',  ( 1.000000000000000000, -2.952720810173289112E-16, -2.061873921506763405E-30 ) ) ;
#22902 = CARTESIAN_POINT ( 'NONE',  ( -18.59999999999999787, 11.76393579169289083, -211.0774408799668720 ) ) ;
#22903 = ORIENTED_EDGE ( 'NONE', *, *, #192163, .F. ) ;
#22904 = FACE_OUTER_BOUND ( 'NONE', #142100, .T. ) ;
#22905 = ORIENTED_EDGE ( 'NONE', *, *, #131256, .F. ) ;
#22906 = ORIENTED_EDGE ( 'NONE', *, *, #65866, .T. ) ;
#22907 = EDGE_CURVE ( 'NONE', #493, #135423, #59608, .T. ) ;
#22908 = AXIS2_PLACEMENT_3D ( 'NONE', #219797, #119438, #238076 ) ;
#22909 = AXIS2_PLACEMENT_3D ( 'NONE', #81998, #118618, #159036 ) ;
#22910 = EDGE_CURVE ( 'NONE', #43174, #134638, #75382, .T. ) ;
#22911 = LINE ( 'NONE', #141537, #235037 ) ;
#22912 = CARTESIAN_POINT ( 'NONE',  ( -17.80356949364066566, 65.12326860300937881, -180.3100344602943039 ) ) ;
#22913 = ORIENTED_EDGE ( 'NONE', *, *, #126748, .T. ) ;
#22914 = ORIENTED_EDGE ( 'NONE', *, *, #216849, .F. ) ;
#22915 = DIRECTION ( 'NONE',  ( 1.000000000000000000, 0.000000000000000000, 0.000000000000000000 ) ) ;
#22916 = EDGE_LOOP ( 'NONE', ( #2600, #246476, #214072, #221351 ) ) ;
#22917 = ADVANCED_FACE ( 'NONE', ( #177046 ), #135307, .F. ) ;
#22918 = DIRECTION ( 'NONE',  ( 0.000000000000000000, -6.982962677686266711E-15, 1.000000000000000000 ) ) ;
#22919 = DIRECTION ( 'NONE',  ( 0.000000000000000000, 0.000000000000000000, -1.000000000000000000 ) ) ;
#22920 = VERTEX_POINT ( 'NONE', #98723 ) ;
#22921 = ORIENTED_EDGE ( 'NONE', *, *, #71831, .F. ) ;
#22922 = EDGE_CURVE ( 'NONE', #81295, #122312, #174841, .T. ) ;
#22923 = DIRECTION ( 'NONE',  ( 0.000000000000000000, 0.000000000000000000, -1.000000000000000000 ) ) ;
#22924 = CARTESIAN_POINT ( 'NONE',  ( 21.05000000000000071, 76.10000000001272724, -210.0001538663142640 ) ) ;
#22925 = CARTESIAN_POINT ( 'NONE',  ( -16.86379686415369861, 66.02478224075890978, -123.9564973736146527 ) ) ;
#22926 = AXIS2_PLACEMENT_3D ( 'NONE', #96248, #175822, #114549 ) ;
#22927 = EDGE_CURVE ( 'NONE', #24913, #148383, #3923, .T. ) ;
#22928 = ADVANCED_FACE ( 'NONE', ( #178331 ), #199152, .T. ) ;
#22929 = ORIENTED_EDGE ( 'NONE', *, *, #219576, .F. ) ;
#22930 = ORIENTED_EDGE ( 'NONE', *, *, #210402, .T. ) ;
#22931 = AXIS2_PLACEMENT_3D ( 'NONE', #188489, #244609, #205477 ) ;
#22932 = AXIS2_PLACEMENT_3D ( 'NONE', #52616, #211720, #132162 ) ;
#22933 = CARTESIAN_POINT ( 'NONE',  ( 18.39999999999999503, 65.06382255409391746, -210.1412732845728897 ) ) ;
#22934 = EDGE_CURVE ( 'NONE', #14366, #217036, #179607, .T. ) ;
#22936 = ORIENTED_EDGE ( 'NONE', *, *, #237325, .T. ) ;
#22935 = CARTESIAN_POINT ( 'NONE',  ( 20.94999999999999929, 28.50120599808395028, -258.2149742250584268 ) ) ;
#22937 = EDGE_CURVE ( 'NONE', #239104, #147282, #16680, .T. ) ;
#22938 = CARTESIAN_POINT ( 'NONE',  ( -18.50000000000000000, 76.00000000001170974, -69.52310748452431710 ) ) ;
#22939 = CARTESIAN_POINT ( 'NONE',  ( -22.44366136229477249, 75.99065843052565583, -81.17282604199823481 ) ) ;
#22940 = EDGE_CURVE ( 'NONE', #147657, #11395, #139142, .T. ) ;
#22941 = CARTESIAN_POINT ( 'NONE',  ( -23.25000000000000355, 64.25000000001159606, -56.87310748452440379 ) ) ;
#22943 = DIRECTION ( 'NONE',  ( 1.000000000000000000, 0.000000000000000000, 0.000000000000000000 ) ) ;
#22942 = CARTESIAN_POINT ( 'NONE',  ( -16.94180778212363236, 66.00755694427971321, -90.41892391399113649 ) ) ;
#22944 = CARTESIAN_POINT ( 'NONE',  ( -21.05000000000000071, 75.94867256767049923, -142.8232908207915273 ) ) ;
#22946 = EDGE_CURVE ( 'NONE', #239004, #77358, #15398, .T. ) ;
#22945 = CARTESIAN_POINT ( 'NONE',  ( -21.05000000000000071, 77.25000000001159606, -61.52310748452431710 ) ) ;
#22947 = CARTESIAN_POINT ( 'NONE',  ( 23.14999999999999858, 76.00000000001190870, -103.0231074845243029 ) ) ;
#22948 = CARTESIAN_POINT ( 'NONE',  ( -20.94999999999999929, 87.65000000001192859, -100.0231074845242318 ) ) ;
#22949 = CIRCLE ( 'NONE', #243495, 0.09999999999999939493 ) ;
#22950 = VERTEX_POINT ( 'NONE', #214858 ) ;
#22951 = AXIS2_PLACEMENT_3D ( 'NONE', #122200, #201724, #102590 ) ;
#22952 = VERTEX_POINT ( 'NONE', #195330 ) ;
#22953 = DIRECTION ( 'NONE',  ( 1.000000000000000000, 0.000000000000000000, 0.000000000000000000 ) ) ;
#22954 = VERTEX_POINT ( 'NONE', #256491 ) ;
#22955 = EDGE_CURVE ( 'NONE', #227928, #187942, #162326, .T. ) ;
#22956 = ADVANCED_FACE ( 'NONE', ( #100013 ), #195662, .T. ) ;
#22957 = CARTESIAN_POINT ( 'NONE',  ( -16.87851181299898329, 9.950042924018893231, -146.6498564846331192 ) ) ;
#22958 = CIRCLE ( 'NONE', #98099, 0.09999999999999810429 ) ;
#22959 = VECTOR ( 'NONE', #221286, 1000.000000000000114 ) ;
#22960 = AXIS2_PLACEMENT_3D ( 'NONE', #253485, #71032, #214370 ) ;
#22961 = ORIENTED_EDGE ( 'NONE', *, *, #180464, .T. ) ;
#22962 = VECTOR ( 'NONE', #16110, 1000.000000000000114 ) ;
#22963 = DIRECTION ( 'NONE',  ( 1.000000000000000000, 0.000000000000000000, 0.000000000000000000 ) ) ;
#22965 = ORIENTED_EDGE ( 'NONE', *, *, #94487, .T. ) ;
#22964 = ORIENTED_EDGE ( 'NONE', *, *, #4076, .T. ) ;
#22966 = CARTESIAN_POINT ( 'NONE',  ( -21.13614978966381841, 6.350246358321663287, -199.6169840513710483 ) ) ;
#22967 = EDGE_LOOP ( 'NONE', ( #168073, #196341, #148766, #228189 ) ) ;
#22968 = VERTEX_POINT ( 'NONE', #196573 ) ;
#22970 = DIRECTION ( 'NONE',  ( 0.000000000000000000, -1.000000000000000000, -6.982962677686265922E-15 ) ) ;
#22969 = CIRCLE ( 'NONE', #97745, 0.09999999999999609201 ) ;
#22971 = CARTESIAN_POINT ( 'NONE',  ( -21.08078803292166725, 75.92081401285429365, -109.3561204489614482 ) ) ;
#22973 = ORIENTED_EDGE ( 'NONE', *, *, #214730, .T. ) ;
#22972 = DIRECTION ( 'NONE',  ( 0.000000000000000000, -0.9654727137038715545, 0.2605042016806676242 ) ) ;
#22974 = CIRCLE ( 'NONE', #127006, 11.65000000000000036 ) ;
#22975 = CARTESIAN_POINT ( 'NONE',  ( -20.85000000000000142, 70.15623657602074559, -198.0563205710787713 ) ) ;
#22976 = CARTESIAN_POINT ( 'NONE',  ( 19.80993210785717551, 11.75000000001116263, -158.7671177488815317 ) ) ;
#22978 = VERTEX_POINT ( 'NONE', #40112 ) ;
#22977 = CARTESIAN_POINT ( 'NONE',  ( 11.60000000000006004, 67.75000000001118394, -18.42310748452479530 ) ) ;
#22979 = CARTESIAN_POINT ( 'NONE',  ( -23.25000000000000000, 76.10000000001222986, -148.1726782920690937 ) ) ;
#22980 = EDGE_LOOP ( 'NONE', ( #9351, #70023, #243865, #215088 ) ) ;
#22981 = AXIS2_PLACEMENT_3D ( 'NONE', #53671, #206333, #51060 ) ;
#22982 = CARTESIAN_POINT ( 'NONE',  ( 20.94999999999999929, 84.73084112150785074, -179.6211822035086527 ) ) ;
#22983 = AXIS2_PLACEMENT_3D ( 'NONE', #252751, #212375, #255274 ) ;
#22985 = VERTEX_POINT ( 'NONE', #216135 ) ;
#22984 = CARTESIAN_POINT ( 'NONE',  ( -18.59999999999999787, 77.14957036958705316, -28.20719500002235236 ) ) ;
#22986 = CARTESIAN_POINT ( 'NONE',  ( 21.14999999999999858, 6.650000000011155876, -179.6499999999999773 ) ) ;
#22987 = CARTESIAN_POINT ( 'NONE',  ( -20.54999999999999716, 1.940186915887853303, -12.82911921105332631 ) ) ;
#22988 = LINE ( 'NONE', #241998, #36029 ) ;
#22989 = ORIENTED_EDGE ( 'NONE', *, *, #126178, .T. ) ;
#22990 = EDGE_CURVE ( 'NONE', #142483, #83831, #37523, .T. ) ;
#22992 = CARTESIAN_POINT ( 'NONE',  ( 20.77526135991775291, 8.932009016633136511, -108.9685685427243698 ) ) ;
#22991 = FACE_OUTER_BOUND ( 'NONE', #21300, .T. ) ;
#22993 = CARTESIAN_POINT ( 'NONE',  ( -13.54036565897075484, 66.54845833862633242, -84.56923198569380418 ) ) ;
#22994 = CARTESIAN_POINT ( 'NONE',  ( 21.13461538461538325, 65.38541703798675542, -157.6731074845244223 ) ) ;
#22995 = EDGE_CURVE ( 'NONE', #43436, #14594, #80444, .T. ) ;
#22996 = DIRECTION ( 'NONE',  ( 0.000000000000000000, -0.9999631594459056361, -0.008583690987124413183 ) ) ;
#22997 = CARTESIAN_POINT ( 'NONE',  ( -20.54999999999999716, 76.00000000001213607, -136.5231074845242745 ) ) ;
#22998 = ORIENTED_EDGE ( 'NONE', *, *, #183258, .T. ) ;
#22999 = EDGE_LOOP ( 'NONE', ( #29684, #57804, #81188, #28338 ) ) ;
#23000 = EDGE_LOOP ( 'NONE', ( #140608, #219223, #246836, #216217 ) ) ;
#23001 = ORIENTED_EDGE ( 'NONE', *, *, #128538, .T. ) ;
#23002 = CARTESIAN_POINT ( 'NONE',  ( 20.94999999999999574, 0.6656436123793491033, -212.6810495496487476 ) ) ;
#23003 = ORIENTED_EDGE ( 'NONE', *, *, #243872, .T. ) ;
#23004 = CARTESIAN_POINT ( 'NONE',  ( 18.52928932188133970, 10.27928932189250411, -91.65000000000004832 ) ) ;
#23005 = CARTESIAN_POINT ( 'NONE',  ( -18.59999999999999787, 11.65000000001115232, -141.0148057706540214 ) ) ;
#23006 = AXIS2_PLACEMENT_3D ( 'NONE', #83055, #60957, #183488 ) ;
#23007 = AXIS2_PLACEMENT_3D ( 'NONE', #135080, #229082, #251178 ) ;
#23008 = ORIENTED_EDGE ( 'NONE', *, *, #138298, .T. ) ;
#23009 = FACE_OUTER_BOUND ( 'NONE', #213478, .T. ) ;
#23010 = EDGE_CURVE ( 'NONE', #90665, #61807, #21808, .T. ) ;
#23011 = CIRCLE ( 'NONE', #64845, 0.09999999999999939493 ) ;
#23012 = ORIENTED_EDGE ( 'NONE', *, *, #235109, .T. ) ;
#23013 = ORIENTED_EDGE ( 'NONE', *, *, #248898, .F. ) ;
#23014 = ORIENTED_EDGE ( 'NONE', *, *, #71245, .F. ) ;
#23015 = VECTOR ( 'NONE', #142469, 1000.000000000000000 ) ;
#23016 = CARTESIAN_POINT ( 'NONE',  ( -21.14999999999999858, 1.115600667400684642E-11, -160.9593430482987344 ) ) ;
#23017 = CARTESIAN_POINT ( 'NONE',  ( 22.39999999999999503, 76.00000000001276135, -215.1726782920691505 ) ) ;
#23018 = VECTOR ( 'NONE', #22058, 1000.000000000000000 ) ;
#23019 = DIRECTION ( 'NONE',  ( -1.000000000000000000, 0.000000000000000000, 0.000000000000000000 ) ) ;
#23020 = CARTESIAN_POINT ( 'NONE',  ( -18.50000000000000000, 69.15387683765879956, -32.28538121767450519 ) ) ;
#23021 = DIRECTION ( 'NONE',  ( -2.557131231893036985E-16, 0.8660254037844384856, -0.5000000000000002220 ) ) ;
#23022 = DIRECTION ( 'NONE',  ( 2.952720810173289112E-16, -1.000000000000000000, 0.000000000000000000 ) ) ;
#23024 = CARTESIAN_POINT ( 'NONE',  ( -23.15000000000000213, 2.000000000011154189, -46.72462192276210402 ) ) ;
#23023 = DIRECTION ( 'NONE',  ( 0.000000000000000000, 0.000000000000000000, -1.000000000000000000 ) ) ;
#23025 = CARTESIAN_POINT ( 'NONE',  ( -17.71734398241073549, 10.84235722847571637, -56.72513825300558921 ) ) ;
#23026 = ORIENTED_EDGE ( 'NONE', *, *, #8264, .T. ) ;
#23027 = CARTESIAN_POINT ( 'NONE',  ( 21.08376601933332495, 69.65805272873629406, -103.0868834954543587 ) ) ;
#23028 = DIRECTION ( 'NONE',  ( -0.000000000000000000, 0.9908441862701591329, 0.1350103645451946055 ) ) ;
#23029 = ORIENTED_EDGE ( 'NONE', *, *, #158767, .T. ) ;
#23030 = CARTESIAN_POINT ( 'NONE',  ( -18.79999999999999716, -1.901609089591594470, -11.59510167572422112 ) ) ;
#23031 = AXIS2_PLACEMENT_3D ( 'NONE', #203222, #181116, #77170 ) ;
#23032 = DIRECTION ( 'NONE',  ( 0.000000000000000000, 0.000000000000000000, 1.000000000000000000 ) ) ;
#23033 = CARTESIAN_POINT ( 'NONE',  ( 18.49999999999999645, 1.115600667400684642E-11, -134.0000000000000284 ) ) ;
#23034 = ORIENTED_EDGE ( 'NONE', *, *, #136536, .T. ) ;
#23035 = VECTOR ( 'NONE', #45638, 1000.000000000000000 ) ;
#23036 = CYLINDRICAL_SURFACE ( 'NONE', #173307, 0.09999999999999724387 ) ;
#23037 = DIRECTION ( 'NONE',  ( 1.000000000000000000, 0.000000000000000000, 0.000000000000000000 ) ) ;
#23038 = ORIENTED_EDGE ( 'NONE', *, *, #84330, .F. ) ;
#23039 = ORIENTED_EDGE ( 'NONE', *, *, #26354, .F. ) ;
#23040 = FACE_OUTER_BOUND ( 'NONE', #19659, .T. ) ;
#23041 = EDGE_LOOP ( 'NONE', ( #211208, #133668, #95370, #39099 ) ) ;
#23042 = DIRECTION ( 'NONE',  ( 0.000000000000000000, 0.1335171055202901413, 0.9910465087640860649 ) ) ;
#23043 = CARTESIAN_POINT ( 'NONE',  ( -18.50000000000001066, -9.480686695267808162, -174.4411151687578752 ) ) ;
#23044 = AXIS2_PLACEMENT_3D ( 'NONE', #13594, #50127, #111403 ) ;
#23045 = DIRECTION ( 'NONE',  ( 0.000000000000000000, -0.8700118002898321601, 0.4930308989875230030 ) ) ;
#23046 = DIRECTION ( 'NONE',  ( -3.469446951953635015E-14, -1.000000000000000000, 0.000000000000000000 ) ) ;
#23047 = ORIENTED_EDGE ( 'NONE', *, *, #24882, .T. ) ;
#23048 = EDGE_CURVE ( 'NONE', #153127, #122858, #153994, .T. ) ;
#23049 = LINE ( 'NONE', #860, #154521 ) ;
#23050 = DIRECTION ( 'NONE',  ( 1.000000000000000000, 0.000000000000000000, -0.000000000000000000 ) ) ;
#23051 = ADVANCED_FACE ( 'NONE', ( #45205 ), #24384, .F. ) ;
#23052 = CYLINDRICAL_SURFACE ( 'NONE', #20285, 0.09999999999999939493 ) ;
#23053 = CARTESIAN_POINT ( 'NONE',  ( -22.49756042579671700, 25.99526245069998254, -254.2428317230260291 ) ) ;
#23054 = AXIS2_PLACEMENT_3D ( 'NONE', #245829, #86725, #155439 ) ;
#23055 = ORIENTED_EDGE ( 'NONE', *, *, #57285, .F. ) ;
#23056 = AXIS2_PLACEMENT_3D ( 'NONE', #37223, #134995, #175458 ) ;
#23057 = EDGE_CURVE ( 'NONE', #189831, #140297, #29080, .T. ) ;
#23059 = VERTEX_POINT ( 'NONE', #140445 ) ;
#23058 = CARTESIAN_POINT ( 'NONE',  ( 23.24999999999999289, 11.75000000000000711, -12.15000000000000036 ) ) ;
#23060 = FACE_OUTER_BOUND ( 'NONE', #23623, .T. ) ;
#23061 = CARTESIAN_POINT ( 'NONE',  ( -21.05000000000000071, 34.07086262126583875, -243.8523844785541428 ) ) ;
#23062 = CARTESIAN_POINT ( 'NONE',  ( -22.39999999999999858, 7.790779598384560245, -100.4000000000000341 ) ) ;
#23063 = ADVANCED_FACE ( 'NONE', ( #165160 ), #64765, .T. ) ;
#23064 = DIRECTION ( 'NONE',  ( -2.915501640297152804E-16, -1.000000000000000000, -6.997203936713167125E-15 ) ) ;
#23065 = DIRECTION ( 'NONE',  ( -0.8660254037843277963, 0.000000000000000000, -0.5000000000001921796 ) ) ;
#23066 = CARTESIAN_POINT ( 'NONE',  ( -16.87851181299898684, 66.04995707600431842, -123.8732509998912832 ) ) ;
#23067 = ORIENTED_EDGE ( 'NONE', *, *, #148070, .T. ) ;
#23068 = CARTESIAN_POINT ( 'NONE',  ( 21.05000000000000071, 18.56623428888383387, -239.8594038951179073 ) ) ;
#23069 = CARTESIAN_POINT ( 'NONE',  ( -16.77977881697927032, 9.946601933544062746, -146.6613785731150585 ) ) ;
#23070 = DIRECTION ( 'NONE',  ( -0.000000000000000000, 0.9651348961777157509, -0.2617529984165031243 ) ) ;
#23071 = CARTESIAN_POINT ( 'NONE',  ( 20.95000000000005969, 65.27857539272349641, -29.97167177764265844 ) ) ;
#23072 = EDGE_CURVE ( 'NONE', #190117, #28056, #241434, .T. ) ;
#23073 = AXIS2_PLACEMENT_3D ( 'NONE', #245853, #183313, #67211 ) ;
#23074 = CARTESIAN_POINT ( 'NONE',  ( -0.8999999999999437339, 66.35000000001119247, -7.423107484524793520 ) ) ;
#23075 = DIRECTION ( 'NONE',  ( 0.000000000000000000, -1.000000000000000000, 0.000000000000000000 ) ) ;
#23076 = ORIENTED_EDGE ( 'NONE', *, *, #77298, .T. ) ;
#23077 = ORIENTED_EDGE ( 'NONE', *, *, #208937, .T. ) ;
#23078 = DIRECTION ( 'NONE',  ( 0.000000000000000000, -1.000000000000000000, 0.000000000000000000 ) ) ;
#23079 = FACE_OUTER_BOUND ( 'NONE', #102954, .T. ) ;
#23081 = DIRECTION ( 'NONE',  ( 1.000000000000000000, 0.000000000000000000, 0.000000000000000000 ) ) ;
#23080 = VECTOR ( 'NONE', #51913, 1000.000000000000000 ) ;
#23082 = CARTESIAN_POINT ( 'NONE',  ( 20.99780126800945368, 16.99738886486927569, -224.5087459288183993 ) ) ;
#23083 = EDGE_CURVE ( 'NONE', #131694, #167228, #187278, .T. ) ;
#23084 = ORIENTED_EDGE ( 'NONE', *, *, #14254, .T. ) ;
#23085 = CARTESIAN_POINT ( 'NONE',  ( -18.49499033040906681, 47.08667629969059476, -255.2216170810507947 ) ) ;
#23086 = DIRECTION ( 'NONE',  ( 1.000000000000000000, 0.000000000000000000, 0.000000000000000000 ) ) ;
#23087 = DIRECTION ( 'NONE',  ( 0.000000000000000000, 0.2617529984165152257, 0.9651348961777124202 ) ) ;
#23088 = CARTESIAN_POINT ( 'NONE',  ( -18.50000000000000000, 36.65892442174472876, -249.5511627012454596 ) ) ;
#23089 = AXIS2_PLACEMENT_3D ( 'NONE', #197665, #19037, #164972 ) ;
#23090 = CIRCLE ( 'NONE', #77222, 0.09999999999998898659 ) ;
#23091 = ORIENTED_EDGE ( 'NONE', *, *, #81305, .F. ) ;
#23092 = LINE ( 'NONE', #103861, #139993 ) ;
#23093 = ORIENTED_EDGE ( 'NONE', *, *, #165346, .T. ) ;
#23094 = LINE ( 'NONE', #102571, #31004 ) ;
#23095 = CARTESIAN_POINT ( 'NONE',  ( -18.40000000000000213, 64.52683809665005299, -182.5731074845244279 ) ) ;
#23096 = CARTESIAN_POINT ( 'NONE',  ( -20.54999999999999716, 82.48249193998721296, -215.5326005316167084 ) ) ;
#23097 = CARTESIAN_POINT ( 'NONE',  ( 18.56579813702275317, 65.66974365629644694, -63.93601455626049557 ) ) ;
#23098 = CARTESIAN_POINT ( 'NONE',  ( -21.65000000000000213, 65.35370752038342346, -213.3282663891675952 ) ) ;
#23099 = LINE ( 'NONE', #63472, #160353 ) ;
#23100 = DIRECTION ( 'NONE',  ( 0.000000000000000000, 1.000000000000000000, -0.000000000000000000 ) ) ;
#23101 = CARTESIAN_POINT ( 'NONE',  ( -20.64999999999999858, 74.05981308412367525, -48.85222669557766295 ) ) ;
#23102 = CARTESIAN_POINT ( 'NONE',  ( 22.39999999999999503, 1.115541036281197940E-11, -92.70922040162665212 ) ) ;
#23103 = CARTESIAN_POINT ( 'NONE',  ( -20.94999999999999929, 1.835341550235569663, -179.0551512925629538 ) ) ;
#23104 = CYLINDRICAL_SURFACE ( 'NONE', #77379, 0.1000000000000118433 ) ;
#23105 = CARTESIAN_POINT ( 'NONE',  ( -21.45000000000000284, 68.29142135624930177, -115.3731074845243540 ) ) ;
#23106 = CIRCLE ( 'NONE', #147985, 0.1000000000000028644 ) ;
#23107 = CIRCLE ( 'NONE', #168877, 0.1000000000000028644 ) ;
#23108 = CARTESIAN_POINT ( 'NONE',  ( -21.05000000000000426, 69.52295361822181974, -69.42310748452437963 ) ) ;
#23110 = CARTESIAN_POINT ( 'NONE',  ( 18.39999999999999858, 85.68240343348880117, -163.3662641071115047 ) ) ;
#23109 = AXIS2_PLACEMENT_3D ( 'NONE', #123089, #202614, #227307 ) ;
#23111 = AXIS2_PLACEMENT_3D ( 'NONE', #186466, #46924, #67791 ) ;
#23112 = EDGE_CURVE ( 'NONE', #56338, #207268, #3500, .T. ) ;
#23113 = ORIENTED_EDGE ( 'NONE', *, *, #171032, .T. ) ;
#23115 = DIRECTION ( 'NONE',  ( 0.000000000000000000, -0.4999999999999088507, 0.8660254037844913322 ) ) ;
#23114 = PRESENTATION_LAYER_ASSIGNMENT (  '', '', ( #235458 ) ) ;
#23116 = EDGE_CURVE ( 'NONE', #38982, #165098, #82981, .T. ) ;
#23117 = ORIENTED_EDGE ( 'NONE', *, *, #164826, .T. ) ;
#23118 = LINE ( 'NONE', #42654, #138902 ) ;
#23119 = CARTESIAN_POINT ( 'NONE',  ( 20.97462148592293119, 11.27926720595585230, -211.0854055964561553 ) ) ;
#23120 = CARTESIAN_POINT ( 'NONE',  ( -18.44085059012132177, 11.51401249349496325, -191.7403053191215179 ) ) ;
#23121 = ADVANCED_FACE ( 'NONE', ( #124754 ), #90097, .F. ) ;
#23122 = EDGE_LOOP ( 'NONE', ( #157606, #222379, #62144, #94582 ) ) ;
#23124 = ADVANCED_FACE ( 'NONE', ( #122193 ), #38814, .F. ) ;
#23123 = DIRECTION ( 'NONE',  ( 0.000000000000000000, 0.8412123295017488456, 0.5407049257166434142 ) ) ;
#23125 = FACE_OUTER_BOUND ( 'NONE', #6447, .T. ) ;
#23126 = ORIENTED_EDGE ( 'NONE', *, *, #104446, .T. ) ;
#23127 =( BOUNDED_SURFACE ( )  B_SPLINE_SURFACE ( 3, 2, ( 
 ( #17873, #37466, #199091 ),
 ( #218635, #197796, #157436 ),
 ( #116987, #19164, #82952 ),
 ( #2154, #239510, #81667 ) ),
 .UNSPECIFIED., .F., .F., .T. ) 
 B_SPLINE_SURFACE_WITH_KNOTS ( ( 4, 4 ),
 ( 3, 3 ),
 ( 0.0006461284895273780972, 0.0007503702773985577784 ),
 ( 0.000000000000000000, 1.000000000000000000 ),
 .UNSPECIFIED. ) 
 GEOMETRIC_REPRESENTATION_ITEM ( )  RATIONAL_B_SPLINE_SURFACE ( (
 ( 1.000000000000000000, 0.7071067811865475727, 1.000000000000000000),
 ( 1.000000000000000000, 0.7076476444648740483, 1.000000000000000000),
 ( 1.000000000000000000, 0.7075727925191939160, 1.000000000000000000),
 ( 1.000000000000000000, 0.7071067811865475727, 1.000000000000000000) ) ) 
 REPRESENTATION_ITEM ( '' )  SURFACE ( )  );
#23128 = STYLED_ITEM ( 'NONE', ( #158620 ), #73277 ) ;
#23129 = CIRCLE ( 'NONE', #85603, 0.09999999999999939493 ) ;
#23130 = ORIENTED_EDGE ( 'NONE', *, *, #187435, .F. ) ;
#23131 = DIRECTION ( 'NONE',  ( 0.000000000000000000, 0.1350103645451904977, -0.9908441862701596881 ) ) ;
#23132 = VERTEX_POINT ( 'NONE', #7361 ) ;
#23133 = EDGE_CURVE ( 'NONE', #203922, #2197, #52903, .T. ) ;
#23134 = CARTESIAN_POINT ( 'NONE',  ( 21.05000000000000071, 5.500000000011153745, -188.5947339810868755 ) ) ;
#23135 = DIRECTION ( 'NONE',  ( 0.000000000000000000, 0.000000000000000000, -1.000000000000000000 ) ) ;
#23137 = TOROIDAL_SURFACE ( 'NONE', #181542, 11.65000000000000036, 0.1000000000000000056 ) ;
#23136 = CARTESIAN_POINT ( 'NONE',  ( 21.07971444708685738, 33.99092351726255856, -243.8104526470560813 ) ) ;
#23138 = EDGE_CURVE ( 'NONE', #45997, #128875, #33178, .T. ) ;
#23140 = DIRECTION ( 'NONE',  ( 0.000000000000000000, 0.000000000000000000, -1.000000000000000000 ) ) ;
#23139 = VECTOR ( 'NONE', #63876, 1000.000000000000000 ) ;
#23141 = VECTOR ( 'NONE', #108546, 1000.000000000000000 ) ;
#23142 = CARTESIAN_POINT ( 'NONE',  ( -16.88705144915433110, 66.05000000001230376, -157.0921288898123578 ) ) ;
#23143 = DIRECTION ( 'NONE',  ( 0.000000000000000000, 0.9126074666063545004, 0.4088369013363783999 ) ) ;
#23144 = CARTESIAN_POINT ( 'NONE',  ( 22.50000000000000000, 65.09550114356429162, -243.3481044654562879 ) ) ;
#23145 = CARTESIAN_POINT ( 'NONE',  ( -22.94999999999999929, -1.467286812112899463, 33.00000000000000000 ) ) ;
#23147 = ORIENTED_EDGE ( 'NONE', *, *, #146560, .T. ) ;
#23146 = CARTESIAN_POINT ( 'NONE',  ( -18.43599941264909603, -9.519327428583617134, -40.47297678952136124 ) ) ;
#23148 = VERTEX_POINT ( 'NONE', #226389 ) ;
#23150 = CARTESIAN_POINT ( 'NONE',  ( -18.59999999999999787, 53.17902629910250312, -234.2060907248186368 ) ) ;
#23149 = CARTESIAN_POINT ( 'NONE',  ( 23.14999999999999858, 20.66107731230508548, -234.7421556583769302 ) ) ;
#23152 = ORIENTED_EDGE ( 'NONE', *, *, #194020, .F. ) ;
#23151 = CARTESIAN_POINT ( 'NONE',  ( -16.89935556175730724, 61.06753202229781152, -220.5691239899323648 ) ) ;
#23153 = EDGE_LOOP ( 'NONE', ( #240828, #65203, #101227, #186971 ) ) ;
#23154 = FACE_OUTER_BOUND ( 'NONE', #63300, .T. ) ;
#23155 = CARTESIAN_POINT ( 'NONE',  ( -20.64999999999999858, 25.30967299857550401, -243.4716794062925374 ) ) ;
#23156 = AXIS2_PLACEMENT_3D ( 'NONE', #7142, #43717, #85370 ) ;
#23157 = AXIS2_PLACEMENT_3D ( 'NONE', #108521, #88942, #248025 ) ;
#23159 = EDGE_CURVE ( 'NONE', #208387, #123814, #245530, .T. ) ;
#23158 = CARTESIAN_POINT ( 'NONE',  ( 21.05000000000005400, 89.48413628383013929, -38.12477508515532065 ) ) ;
#23160 = CARTESIAN_POINT ( 'NONE',  ( -20.94999999999999929, 14.05000000001115623, -139.5136950707610026 ) ) ;
#23161 = EDGE_CURVE ( 'NONE', #179534, #215487, #249834, .T. ) ;
#23162 = EDGE_CURVE ( 'NONE', #190881, #62787, #248541, .T. ) ;
#23163 = VECTOR ( 'NONE', #76632, 1000.000000000000000 ) ;
#23164 = DIRECTION ( 'NONE',  ( 0.000000000000000000, -0.1350103645451974088, 0.9908441862701587999 ) ) ;
#23165 = DIRECTION ( 'NONE',  ( 0.000000000000000000, 0.4999999999999929501, -0.8660254037844427044 ) ) ;
#23166 = DIRECTION ( 'NONE',  ( -1.000000000000000000, -0.000000000000000000, -0.000000000000000000 ) ) ;
#23167 = ORIENTED_EDGE ( 'NONE', *, *, #92751, .T. ) ;
#23168 = ORIENTED_EDGE ( 'NONE', *, *, #59914, .T. ) ;
#23169 = DIRECTION ( 'NONE',  ( 0.7071067811865127117, 0.7071067811865821007, 0.000000000000000000 ) ) ;
#23170 = ORIENTED_EDGE ( 'NONE', *, *, #49973, .T. ) ;
#23171 = B_SPLINE_CURVE_WITH_KNOTS ( 'NONE', 3,
 ( #227611, #204194, #183371, #85501 ),
 .UNSPECIFIED., .F., .F.,
 ( 4, 4 ),
 ( 0.000000000000000000, 0.001767853679387121216 ),
 .UNSPECIFIED. ) ;
#23172 = CARTESIAN_POINT ( 'NONE',  ( -18.50000000000000000, 68.97833521811233481, -166.1895420826271277 ) ) ;
#23173 = ORIENTED_EDGE ( 'NONE', *, *, #237921, .T. ) ;
#23174 = CARTESIAN_POINT ( 'NONE',  ( -16.81453563122428818, 9.939100205448108127, -154.7882586606453401 ) ) ;
#23175 = EDGE_CURVE ( 'NONE', #14355, #104087, #171612, .T. ) ;
#23176 = LINE ( 'NONE', #102654, #5126 ) ;
#23177 = CARTESIAN_POINT ( 'NONE',  ( 18.49999999999999289, 65.75000000001148237, -44.87310748452439668 ) ) ;
#23178 = CARTESIAN_POINT ( 'NONE',  ( -16.89797118371617302, 22.91357555947262981, -230.8705896228633776 ) ) ;
#23179 = ORIENTED_EDGE ( 'NONE', *, *, #245256, .T. ) ;
#23180 = CARTESIAN_POINT ( 'NONE',  ( -20.94684162621883061, 11.74999999999999467, -6.841644000359353939 ) ) ;
#23181 = VERTEX_POINT ( 'NONE', #107745 ) ;
#23182 = VECTOR ( 'NONE', #113589, 1000.000000000000000 ) ;
#23183 = CARTESIAN_POINT ( 'NONE',  ( 22.39999999999999503, 1.115600667400684642E-11, -122.3504291924552234 ) ) ;
#23184 = CARTESIAN_POINT ( 'NONE',  ( -22.39999999999999503, 29.54900078958453236, -252.7363208912387620 ) ) ;
#23185 = CIRCLE ( 'NONE', #231464, 0.09999999999999520384 ) ;
#23186 = EDGE_CURVE ( 'NONE', #5246, #155129, #248600, .T. ) ;
#23187 = CARTESIAN_POINT ( 'NONE',  ( 18.50000000000000000, -7.631834139421004970, -210.1304494778856053 ) ) ;
#23188 = CARTESIAN_POINT ( 'NONE',  ( 23.14999999999999503, 13.96869538424789070, -210.3925794786331949 ) ) ;
#23189 = TOROIDAL_SURFACE ( 'NONE', #168956, 0.2000000000000000111, 0.1000000000000000056 ) ;
#23190 = ORIENTED_EDGE ( 'NONE', *, *, #53760, .F. ) ;
#23191 = FACE_OUTER_BOUND ( 'NONE', #34389, .T. ) ;
#23192 = ORIENTED_EDGE ( 'NONE', *, *, #126282, .T. ) ;
#23195 = EDGE_LOOP ( 'NONE', ( #245697, #251295, #807, #105704 ) ) ;
#23194 = CARTESIAN_POINT ( 'NONE',  ( -22.39999999999999858, 12.54173083476182526, -223.4160622903444846 ) ) ;
#23193 = CARTESIAN_POINT ( 'NONE',  ( 18.50000000000000000, 47.16152503674115337, -255.1462838189583806 ) ) ;
#23196 = DIRECTION ( 'NONE',  ( 0.000000000000000000, 0.2617529984164856383, 0.9651348961777204138 ) ) ;
#23197 = VERTEX_POINT ( 'NONE', #167752 ) ;
#23198 = AXIS2_PLACEMENT_3D ( 'NONE', #103032, #143455, #125192 ) ;
#23199 = DIRECTION ( 'NONE',  ( -1.000000000000000000, 0.000000000000000000, -0.000000000000000000 ) ) ;
#23200 = ORIENTED_EDGE ( 'NONE', *, *, #187309, .F. ) ;
#23201 = CARTESIAN_POINT ( 'NONE',  ( -23.15000000000000213, 1.115600667400684642E-11, -134.0000000000000284 ) ) ;
#23202 = EDGE_CURVE ( 'NONE', #246412, #220499, #91409, .T. ) ;
#23203 = SPHERICAL_SURFACE ( 'NONE', #236233, 0.1000000000000000056 ) ;
#23204 = CARTESIAN_POINT ( 'NONE',  ( 21.97500000000000497, 61.05385884576949707, -221.3836188041226762 ) ) ;
#23205 = AXIS2_PLACEMENT_3D ( 'NONE', #157007, #139962, #18751 ) ;
#23206 = CARTESIAN_POINT ( 'NONE',  ( 20.85000000000000142, 68.92903212821357783, -166.2765432626560766 ) ) ;
#23207 = VECTOR ( 'NONE', #25575, 1000.000000000000227 ) ;
#23208 = EDGE_CURVE ( 'NONE', #74533, #144474, #169048, .T. ) ;
#23209 = DIRECTION ( 'NONE',  ( -1.000000000000000000, -0.000000000000000000, -0.000000000000000000 ) ) ;
#23210 = CIRCLE ( 'NONE', #168981, 0.4999999999999970024 ) ;
#23211 = EDGE_LOOP ( 'NONE', ( #159291, #50543, #35795, #10708, #28136, #168586, #238435, #59772 ) ) ;
#23212 = ADVANCED_FACE ( 'NONE', ( #69933 ), #228780, .F. ) ;
#23213 = CARTESIAN_POINT ( 'NONE',  ( -16.87036670365548474, 14.22508806334145959, -219.3732768077300932 ) ) ;
#23214 = CYLINDRICAL_SURFACE ( 'NONE', #132563, 11.80000000000000426 ) ;
#23215 = DIRECTION ( 'NONE',  ( 1.000000000000000000, 0.000000000000000000, 0.000000000000000000 ) ) ;
#23216 = ORIENTED_EDGE ( 'NONE', *, *, #58608, .T. ) ;
#23217 = CARTESIAN_POINT ( 'NONE',  ( -18.50000000000000000, 63.83985267992358104, -213.0213082169670145 ) ) ;
#23218 = VERTEX_POINT ( 'NONE', #129866 ) ;
#23219 = DIRECTION ( 'NONE',  ( 1.000000000000000000, 0.000000000000000000, 0.000000000000000000 ) ) ;
#23220 = EDGE_CURVE ( 'NONE', #71443, #248210, #124722, .T. ) ;
#23221 = EDGE_CURVE ( 'NONE', #150237, #56745, #208156, .T. ) ;
#23222 = FACE_OUTER_BOUND ( 'NONE', #33433, .T. ) ;
#23223 = DIRECTION ( 'NONE',  ( 1.000000000000000000, -0.000000000000000000, -0.000000000000000000 ) ) ;
#23224 = TOROIDAL_SURFACE ( 'NONE', #189796, 0.2000000000000000111, 0.1000000000000000056 ) ;
#23226 = EDGE_LOOP ( 'NONE', ( #103309, #245918, #122690, #104024 ) ) ;
#23225 = CARTESIAN_POINT ( 'NONE',  ( -20.85000000000000142, -11.74999999998884448, -167.5000000000000000 ) ) ;
#23227 = CARTESIAN_POINT ( 'NONE',  ( -20.54999999999999716, 71.75000000001186606, -90.67310748452433700 ) ) ;
#23228 = DIRECTION ( 'NONE',  ( 0.000000000000000000, 0.000000000000000000, -1.000000000000000000 ) ) ;
#23229 = DIRECTION ( 'NONE',  ( 0.000000000000000000, -0.5000683049008606273, -0.8659859643398268858 ) ) ;
#23230 = EDGE_LOOP ( 'NONE', ( #123035, #162328, #157062, #15254 ) ) ;
#23231 = CARTESIAN_POINT ( 'NONE',  ( 20.95512820512820795, 8.876151316288117599, -12.20017285912874883 ) ) ;
#23232 = FACE_OUTER_BOUND ( 'NONE', #219466, .T. ) ;
#23233 = ORIENTED_EDGE ( 'NONE', *, *, #87811, .T. ) ;
#23234 = CARTESIAN_POINT ( 'NONE',  ( -21.07094088545368749, 65.48150606888252412, -241.9290547188616074 ) ) ;
#23235 = AXIS2_PLACEMENT_3D ( 'NONE', #189486, #51218, #10848 ) ;
#23236 = CIRCLE ( 'NONE', #44057, 0.1000000000000014488 ) ;
#23237 = EDGE_CURVE ( 'NONE', #192913, #45256, #110314, .T. ) ;
#23238 = VECTOR ( 'NONE', #96845, 1000.000000000000227 ) ;
#23239 = AXIS2_PLACEMENT_3D ( 'NONE', #104760, #184321, #164776 ) ;
#23240 = EDGE_CURVE ( 'NONE', #69711, #110939, #230256, .T. ) ;
#23241 = ORIENTED_EDGE ( 'NONE', *, *, #205482, .F. ) ;
#23242 = DIRECTION ( 'NONE',  ( 0.000000000000000000, -0.9908441862701782288, -0.1350103645450539402 ) ) ;
#23243 = VERTEX_POINT ( 'NONE', #232855 ) ;
#23245 = VERTEX_POINT ( 'NONE', #54186 ) ;
#23244 = CARTESIAN_POINT ( 'NONE',  ( -20.94999999999999929, 5.850000000011160495, -157.3675027757221017 ) ) ;
#23246 = EDGE_CURVE ( 'NONE', #219544, #140091, #252375, .T. ) ;
#23249 = EDGE_LOOP ( 'NONE', ( #31604, #75251, #204849, #87713 ) ) ;
#23248 = EDGE_LOOP ( 'NONE', ( #108853, #165569, #123906, #167153 ) ) ;
#23247 = DIRECTION ( 'NONE',  ( 0.000000000000000000, -0.8660254037844459241, -0.4999999999999873990 ) ) ;
#23250 = LINE ( 'NONE', #42784, #158016 ) ;
#23251 = DIRECTION ( 'NONE',  ( 1.000000000000000000, 2.952720810173289112E-16, -0.000000000000000000 ) ) ;
#23253 = DIRECTION ( 'NONE',  ( 0.000000000000000000, 0.000000000000000000, -1.000000000000000000 ) ) ;
#23252 = DIRECTION ( 'NONE',  ( 0.000000000000000000, 0.000000000000000000, -1.000000000000000000 ) ) ;
#23254 = CARTESIAN_POINT ( 'NONE',  ( -23.25000000000000000, 70.05000000001149374, -46.32880978955918039 ) ) ;
#23255 = ADVANCED_FACE ( 'NONE', ( #133724 ), #112889, .T. ) ;
#23256 = CIRCLE ( 'NONE', #106405, 0.09999999999998898659 ) ;
#23257 = CARTESIAN_POINT ( 'NONE',  ( -16.90257928357875272, 44.12128666712435177, -235.3007907132581522 ) ) ;
#23258 = CARTESIAN_POINT ( 'NONE',  ( -20.65000000000000568, 5.649999999999983480, -9.250000000000001776 ) ) ;
#23260 = CARTESIAN_POINT ( 'NONE',  ( -23.25000000000000355, 41.03261631955726330, -236.6889770711509584 ) ) ;
#23259 = DIRECTION ( 'NONE',  ( 0.000000000000000000, 0.000000000000000000, -1.000000000000000000 ) ) ;
#23261 = ORIENTED_EDGE ( 'NONE', *, *, #167173, .T. ) ;
#23262 = ORIENTED_EDGE ( 'NONE', *, *, #53258, .T. ) ;
#23263 = ADVANCED_FACE ( 'NONE', ( #178017 ), #17619, .T. ) ;
#23264 = CARTESIAN_POINT ( 'NONE',  ( -21.04999999999994387, 74.83745509109094485, -43.82310748452479743 ) ) ;
#23265 = AXIS2_PLACEMENT_3D ( 'NONE', #911, #178333, #120930 ) ;
#23267 = EDGE_LOOP ( 'NONE', ( #21548, #108253, #221185, #33459, #34787, #125301, #213278, #207014, #76, #157364, #208564, #120178, #73910, #93161, #22558, #27944, #71878, #37934, #151114, #21482, #217801, #79406, #179593 ) ) ;
#23266 = SPHERICAL_SURFACE ( 'NONE', #136958, 0.1000000000000000056 ) ;
#23268 = ORIENTED_EDGE ( 'NONE', *, *, #66475, .F. ) ;
#23269 = CARTESIAN_POINT ( 'NONE',  ( -21.44999999999999929, 68.85000000001205933, -124.2731074845243455 ) ) ;
#23270 = EDGE_LOOP ( 'NONE', ( #133120, #39655, #110593 ) ) ;
#23271 = CARTESIAN_POINT ( 'NONE',  ( -21.05000000000000071, 69.74115727647293284, -136.5551211777123797 ) ) ;
#23272 = EDGE_CURVE ( 'NONE', #71686, #148851, #55443, .T. ) ;
#23273 = EDGE_LOOP ( 'NONE', ( #26077, #218139, #51448, #140965 ) ) ;
#23274 = DIRECTION ( 'NONE',  ( 2.952720810173289112E-16, 1.000000000000000000, -6.088138035986627436E-46 ) ) ;
#23275 = CARTESIAN_POINT ( 'NONE',  ( 18.59999999999999076, 10.20857864377385127, -58.15000000000000568 ) ) ;
#23278 = ORIENTED_EDGE ( 'NONE', *, *, #166741, .T. ) ;
#23277 = EDGE_LOOP ( 'NONE', ( #80222, #82992, #107605, #4677 ) ) ;
#23276 = AXIS2_PLACEMENT_3D ( 'NONE', #112411, #73304, #111113 ) ;
#23279 = VECTOR ( 'NONE', #173186, 1000.000000000000000 ) ;
#23280 = ORIENTED_EDGE ( 'NONE', *, *, #230827, .T. ) ;
#23281 = CARTESIAN_POINT ( 'NONE',  ( 19.90000000000000924, 1.350000000000000089, 22.00000000000000355 ) ) ;
#23282 = ORIENTED_EDGE ( 'NONE', *, *, #19049, .T. ) ;
#23283 = ORIENTED_EDGE ( 'NONE', *, *, #250888, .T. ) ;
#23284 = FACE_OUTER_BOUND ( 'NONE', #17533, .T. ) ;
#23286 = ORIENTED_EDGE ( 'NONE', *, *, #201265, .T. ) ;
#23285 = CARTESIAN_POINT ( 'NONE',  ( -20.15000000000000568, 66.70857864377492774, -148.8731074845244393 ) ) ;
#23288 = DIRECTION ( 'NONE',  ( 1.000000000000000000, 0.000000000000000000, 0.000000000000000000 ) ) ;
#23287 = DIRECTION ( 'NONE',  ( 0.000000000000000000, 0.9209589331071758034, -0.3896596508879157650 ) ) ;
#23289 = DIRECTION ( 'NONE',  ( -1.000000000000000000, -2.952720810173289112E-16, 0.000000000000000000 ) ) ;
#23290 = FACE_OUTER_BOUND ( 'NONE', #114693, .T. ) ;
#23291 = CARTESIAN_POINT ( 'NONE',  ( -21.12642695952773764, 6.375659922046319927, -66.90109671681068448 ) ) ;
#23292 = ORIENTED_EDGE ( 'NONE', *, *, #141443, .F. ) ;
#23293 = VERTEX_POINT ( 'NONE', #192428 ) ;
#23294 = CARTESIAN_POINT ( 'NONE',  ( 20.94999999999999574, 46.45388641681647357, -243.1520440498138385 ) ) ;
#23295 = CARTESIAN_POINT ( 'NONE',  ( -22.59999999999999787, 75.90000000001276703, -215.1726782920691505 ) ) ;
#23296 = CIRCLE ( 'NONE', #160669, 0.09999999999998898659 ) ;
#23297 = ORIENTED_EDGE ( 'NONE', *, *, #115565, .F. ) ;
#23298 = CARTESIAN_POINT ( 'NONE',  ( -20.94999999999999929, 13.54362637910787370, -238.4879411198429580 ) ) ;
#23299 = AXIS2_PLACEMENT_3D ( 'NONE', #218445, #159792, #63229 ) ;
#23300 = CIRCLE ( 'NONE', #10809, 0.09999999999999609201 ) ;
#23301 = AXIS2_PLACEMENT_3D ( 'NONE', #119783, #197996, #233311 ) ;
#23302 = FACE_OUTER_BOUND ( 'NONE', #81284, .T. ) ;
#23303 = CARTESIAN_POINT ( 'NONE',  ( 18.59999999999999076, 7.783179459866048866, -245.3643104511423019 ) ) ;
#23304 = VERTEX_POINT ( 'NONE', #234107 ) ;
#23305 = EDGE_LOOP ( 'NONE', ( #81453, #224277, #221447, #219782 ) ) ;
#23306 = STYLED_ITEM ( 'NONE', ( #148067 ), #194461 ) ;
#23307 = CARTESIAN_POINT ( 'NONE',  ( 21.05000000000000071, 1.115600667400684642E-11, -71.00000000000001421 ) ) ;
#23308 = EDGE_CURVE ( 'NONE', #96826, #215608, #34658, .T. ) ;
#23309 = CARTESIAN_POINT ( 'NONE',  ( -22.10000000000000142, -11.75000000000000000, -15.00000000000000000 ) ) ;
#23310 = ORIENTED_EDGE ( 'NONE', *, *, #177808, .F. ) ;
#23311 = CARTESIAN_POINT ( 'NONE',  ( 23.14999999999999503, 56.06656052939784729, -228.0911609752645290 ) ) ;
#23312 = ORIENTED_EDGE ( 'NONE', *, *, #138350, .F. ) ;
#23313 = FACE_OUTER_BOUND ( 'NONE', #237816, .T. ) ;
#23314 = CARTESIAN_POINT ( 'NONE',  ( -21.55000000000000071, 21.39776787615277343, -233.0380739262505472 ) ) ;
#23316 = FACE_OUTER_BOUND ( 'NONE', #203653, .T. ) ;
#23315 = CARTESIAN_POINT ( 'NONE',  ( -21.33487959338958007, 10.30459399514276164, -227.8041537064418662 ) ) ;
#23317 = DIRECTION ( 'NONE',  ( 0.000000000000000000, -0.9126074666063844765, -0.4088369013363114535 ) ) ;
#23318 = B_SPLINE_CURVE_WITH_KNOTS ( 'NONE', 3,
 ( #222048, #42178, #44741, #139956, #43449, #219500 ),
 .UNSPECIFIED., .F., .F.,
 ( 4, 2, 4 ),
 ( 0.000000000000000000, 0.0001568709654583421050, 0.0003137419309166842099 ),
 .UNSPECIFIED. ) ;
#23319 = DIRECTION ( 'NONE',  ( 0.000000000000000000, -0.9915357197604792727, 0.1298341882520475943 ) ) ;
#23320 = ORIENTED_EDGE ( 'NONE', *, *, #152203, .T. ) ;
#23321 = DIRECTION ( 'NONE',  ( 4.239556034732056127E-17, 0.3848449534832867891, 0.9229812358755983270 ) ) ;
#23322 = EDGE_CURVE ( 'NONE', #174781, #103006, #4091, .T. ) ;
#23323 = AXIS2_PLACEMENT_3D ( 'NONE', #8463, #87960, #28048 ) ;
#23325 = ORIENTED_EDGE ( 'NONE', *, *, #253044, .F. ) ;
#23324 = ORIENTED_EDGE ( 'NONE', *, *, #111867, .F. ) ;
#23326 = VERTEX_POINT ( 'NONE', #77582 ) ;
#23327 = CIRCLE ( 'NONE', #40077, 0.9750000000000036415 ) ;
#23328 = ORIENTED_EDGE ( 'NONE', *, *, #114492, .F. ) ;
#23329 = DIRECTION ( 'NONE',  ( -3.469446951953515108E-14, -1.000000000000000000, 0.000000000000000000 ) ) ;
#23330 = CARTESIAN_POINT ( 'NONE',  ( -20.12071067811865888, 9.320710678129810134, -146.3500000000000227 ) ) ;
#23331 = DIRECTION ( 'NONE',  ( 0.000000000000000000, 0.000000000000000000, 1.000000000000000000 ) ) ;
#23332 = DIRECTION ( 'NONE',  ( -0.000000000000000000, 1.000000000000000000, -0.000000000000000000 ) ) ;
#23333 = VECTOR ( 'NONE', #105821, 1000.000000000000000 ) ;
#23334 = CARTESIAN_POINT ( 'NONE',  ( 21.14999999999999858, 11.65000000000000391, -0.1000000000000028644 ) ) ;
#23336 = CARTESIAN_POINT ( 'NONE',  ( 21.04999999999999716, 58.97995181213600091, -225.7513643067558746 ) ) ;
#23335 = DIRECTION ( 'NONE',  ( -1.000000000000000000, 0.000000000000000000, 0.000000000000000000 ) ) ;
#23338 = EDGE_LOOP ( 'NONE', ( #61652, #102377, #66347, #95758 ) ) ;
#23337 = CARTESIAN_POINT ( 'NONE',  ( 18.47135592147650840, 77.20290371986166633, -241.7660124468425522 ) ) ;
#23339 = CARTESIAN_POINT ( 'NONE',  ( -21.04999999999998295, 6.344723404101382691, -167.4852821434760131 ) ) ;
#23340 = EDGE_LOOP ( 'NONE', ( #60228, #47772, #756, #600 ) ) ;
#23341 = CIRCLE ( 'NONE', #15114, 0.1000000000000017680 ) ;
#23342 = CARTESIAN_POINT ( 'NONE',  ( -22.50000000000000000, 11.64987090377452184, -66.91748010912704103 ) ) ;
#23343 = CIRCLE ( 'NONE', #69116, 0.1000000000000028644 ) ;
#23344 = ORIENTED_EDGE ( 'NONE', *, *, #98781, .F. ) ;
#23345 = VERTEX_POINT ( 'NONE', #172909 ) ;
#23346 = DIRECTION ( 'NONE',  ( 0.000000000000000000, 0.000000000000000000, -1.000000000000000000 ) ) ;
#23347 = LINE ( 'NONE', #44175, #56016 ) ;
#23348 = CARTESIAN_POINT ( 'NONE',  ( -16.77431908686106610, 66.05419424549353380, -48.68726826687415610 ) ) ;
#23349 = CARTESIAN_POINT ( 'NONE',  ( 15.70340296795548518, 9.355888454513701546, -83.28864289677805743 ) ) ;
#23350 = CIRCLE ( 'NONE', #2453, 6.258578643762710669 ) ;
#23351 = CARTESIAN_POINT ( 'NONE',  ( -23.15000000000000213, -8.663551401858001100, -124.4758988819327215 ) ) ;
#23352 = ORIENTED_EDGE ( 'NONE', *, *, #204837, .T. ) ;
#23353 = VERTEX_POINT ( 'NONE', #115445 ) ;
#23354 = CIRCLE ( 'NONE', #98115, 0.3999999999999975797 ) ;
#23355 = CARTESIAN_POINT ( 'NONE',  ( -21.05000000000000071, 64.25000000001176659, -76.53791325517833855 ) ) ;
#23356 = ORIENTED_EDGE ( 'NONE', *, *, #137013, .F. ) ;
#23357 = DIRECTION ( 'NONE',  ( 1.000000000000000000, 0.000000000000000000, -0.000000000000000000 ) ) ;
#23358 = CARTESIAN_POINT ( 'NONE',  ( -18.40000000000000213, 64.51332499825430489, -112.2731074845243739 ) ) ;
#23359 = AXIS2_PLACEMENT_3D ( 'NONE', #224471, #246606, #67975 ) ;
#23360 = DIRECTION ( 'NONE',  ( 1.000000000000000000, 0.000000000000000000, 0.000000000000000000 ) ) ;
#23361 = LINE ( 'NONE', #117297, #212679 ) ;
#23362 = VECTOR ( 'NONE', #246564, 1000.000000000000000 ) ;
#23363 = DIRECTION ( 'NONE',  ( 1.000000000000000000, 0.000000000000000000, 0.000000000000000000 ) ) ;
#23364 = CARTESIAN_POINT ( 'NONE',  ( 18.49999999999999645, 1.115600667400684642E-11, -134.0000000000000000 ) ) ;
#23365 = LINE ( 'NONE', #220264, #58615 ) ;
#23366 = CARTESIAN_POINT ( 'NONE',  ( -18.39999999999999858, -9.519327731081281385, -140.9729763765593589 ) ) ;
#23368 = EDGE_CURVE ( 'NONE', #214472, #109031, #208302, .T. ) ;
#23367 = CARTESIAN_POINT ( 'NONE',  ( 20.94999999999999929, 71.00000000001180922, -81.52837350343745015 ) ) ;
#23369 = CARTESIAN_POINT ( 'NONE',  ( 18.49999999999999289, 65.76093837589102975, -178.7687100499267672 ) ) ;
#23370 = DIRECTION ( 'NONE',  ( 1.000000000000000000, 0.000000000000000000, 0.000000000000000000 ) ) ;
#23371 = CARTESIAN_POINT ( 'NONE',  ( 22.39999999999999503, 12.54173083476182882, -223.4160622903444562 ) ) ;
#23372 = ORIENTED_EDGE ( 'NONE', *, *, #57165, .T. ) ;
#23373 = EDGE_CURVE ( 'NONE', #7826, #65719, #112444, .T. ) ;
#23374 = CARTESIAN_POINT ( 'NONE',  ( -16.87331047859649757, 30.20632856012693424, -234.8070450048000737 ) ) ;
#23375 = ORIENTED_EDGE ( 'NONE', *, *, #122302, .T. ) ;
#23376 = DIRECTION ( 'NONE',  ( 0.000000000000000000, 0.000000000000000000, -1.000000000000000000 ) ) ;
#23377 = EDGE_CURVE ( 'NONE', #80091, #77103, #157177, .T. ) ;
#23379 = CIRCLE ( 'NONE', #56617, 12.87499999999999467 ) ;
#23378 = DIRECTION ( 'NONE',  ( 1.000000000000000000, 0.000000000000000000, 0.000000000000000000 ) ) ;
#23380 = DIRECTION ( 'NONE',  ( -1.000000000000000000, 2.952720810173289112E-16, 2.061873921506763405E-30 ) ) ;
#23382 = VERTEX_POINT ( 'NONE', #75076 ) ;
#23381 = CIRCLE ( 'NONE', #198130, 0.09999999999999939493 ) ;
#23383 = CARTESIAN_POINT ( 'NONE',  ( -20.64999999999999858, 74.00000000001199396, -116.2477294072864140 ) ) ;
#23384 = CIRCLE ( 'NONE', #148239, 0.09999999999999530098 ) ;
#23385 = CONICAL_SURFACE ( 'NONE', #56624, 6.249999999999998224, 0.7853981633974431720 ) ;
#23386 = CARTESIAN_POINT ( 'NONE',  ( 18.59999999999999787, 1.148907358139439339E-11, -201.0000000000015064 ) ) ;
#23387 = CARTESIAN_POINT ( 'NONE',  ( -23.15000000000000213, 76.00000000001237765, -170.0231074845243597 ) ) ;
#23388 = EDGE_CURVE ( 'NONE', #125075, #110138, #41712, .T. ) ;
#23389 = DIRECTION ( 'NONE',  ( 0.000000000000000000, 1.000000000000000000, 0.000000000000000000 ) ) ;
#23390 = DIRECTION ( 'NONE',  ( 0.000000000000000000, 0.000000000000000000, 1.000000000000000000 ) ) ;
#23391 = DIRECTION ( 'NONE',  ( -1.000000000000000000, -0.000000000000000000, 0.000000000000000000 ) ) ;
#23392 = AXIS2_PLACEMENT_3D ( 'NONE', #10055, #148287, #111730 ) ;
#23393 = B_SPLINE_CURVE_WITH_KNOTS ( 'NONE', 3,
 ( #127806, #249046, #49545, #30008, #109499, #207348 ),
 .UNSPECIFIED., .F., .F.,
 ( 4, 2, 4 ),
 ( 0.000000000000000000, 0.0001895189928937402997, 0.0003790379857874805994 ),
 .UNSPECIFIED. ) ;
#23394 = ORIENTED_EDGE ( 'NONE', *, *, #205574, .F. ) ;
#23395 = CARTESIAN_POINT ( 'NONE',  ( 21.51976009735019346, 69.08954155835293420, -136.5231074845243313 ) ) ;
#23397 = EDGE_LOOP ( 'NONE', ( #77009, #81858, #13393, #39493 ) ) ;
#23396 = CARTESIAN_POINT ( 'NONE',  ( -20.64999999999999858, 38.33376540847015690, -250.4483291680710693 ) ) ;
#23398 = DIRECTION ( 'NONE',  ( -0.000000000000000000, -0.000000000000000000, -1.000000000000000000 ) ) ;
#23399 = CARTESIAN_POINT ( 'NONE',  ( -23.25000000000000000, -9.682403433465239573, -140.6568433774128266 ) ) ;
#23400 = EDGE_CURVE ( 'NONE', #56194, #224530, #220759, .T. ) ;
#23401 = DIRECTION ( 'NONE',  ( 0.000000000000000000, -0.2617529984164506107, -0.9651348961777299618 ) ) ;
#23402 = ORIENTED_EDGE ( 'NONE', *, *, #48133, .T. ) ;
#23403 = DIRECTION ( 'NONE',  ( 0.000000000000000000, 0.8814952561688476074, -0.4721928772777262417 ) ) ;
#23404 = ITEM_DEFINED_TRANSFORMATION ( 'NONE', 'NONE', #181865,  #2425 ) ;
#23406 = EDGE_CURVE ( 'NONE', #70151, #155284, #141641, .T. ) ;
#23405 = CARTESIAN_POINT ( 'NONE',  ( -21.14999999999994174, 77.85126707825561709, -47.62635315998165453 ) ) ;
#23407 = CIRCLE ( 'NONE', #48313, 0.09999999999999741040 ) ;
#23408 = ORIENTED_EDGE ( 'NONE', *, *, #112642, .T. ) ;
#23409 = CARTESIAN_POINT ( 'NONE',  ( 20.94999999999999929, 85.00000000001232081, -160.1291383618718385 ) ) ;
#23410 = FACE_BOUND ( 'NONE', #201613, .T. ) ;
#23411 = DIRECTION ( 'NONE',  ( 0.000000000000000000, 8.896017825522085641E-15, -1.000000000000000000 ) ) ;
#23412 = ORIENTED_EDGE ( 'NONE', *, *, #121748, .F. ) ;
#23413 = AXIS2_PLACEMENT_3D ( 'NONE', #229128, #203138, #24529 ) ;
#23414 = ORIENTED_EDGE ( 'NONE', *, *, #113626, .T. ) ;
#23415 = CARTESIAN_POINT ( 'NONE',  ( 21.05000000000000071, 10.47338541492405639, -74.57865446424858646 ) ) ;
#23416 = CARTESIAN_POINT ( 'NONE',  ( 20.85000000000000142, -1.135018845899022466, -141.7169768834323520 ) ) ;
#23417 = EDGE_CURVE ( 'NONE', #243619, #212843, #137348, .T. ) ;
#23418 = CYLINDRICAL_SURFACE ( 'NONE', #136235, 11.75000000000000000 ) ;
#23419 = CARTESIAN_POINT ( 'NONE',  ( 21.05000000000000071, 5.500000000011153745, -146.4052660189131245 ) ) ;
#23420 = CARTESIAN_POINT ( 'NONE',  ( -21.05000000000000071, -11.64999999998884306, -198.0999999999999659 ) ) ;
#23421 = FACE_OUTER_BOUND ( 'NONE', #163247, .T. ) ;
#23423 = CARTESIAN_POINT ( 'NONE',  ( 20.04142135623730070, 11.65000000001115943, -54.85000000000000142 ) ) ;
#23422 = DIRECTION ( 'NONE',  ( 0.000000000000000000, -0.1495327102803180597, 0.9887567792719412774 ) ) ;
#23424 = DIRECTION ( 'NONE',  ( -0.7071067811865389130, -0.1850873201762232578, -0.6824534298470456006 ) ) ;
#23425 = DIRECTION ( 'NONE',  ( -1.000000000000000000, -0.000000000000000000, -0.000000000000000000 ) ) ;
#23426 = DIRECTION ( 'NONE',  ( 1.000000000000000000, -0.000000000000000000, 0.000000000000000000 ) ) ;
#23427 = AXIS2_PLACEMENT_3D ( 'NONE', #103781, #120841, #165068 ) ;
#23428 = ORIENTED_EDGE ( 'NONE', *, *, #80674, .F. ) ;
#23429 = VECTOR ( 'NONE', #205762, 1000.000000000000000 ) ;
#23430 = VERTEX_POINT ( 'NONE', #197552 ) ;
#23431 = CIRCLE ( 'NONE', #35883, 11.80000000000000426 ) ;
#23432 = CARTESIAN_POINT ( 'NONE',  ( -18.50000000000000355, -1.263275465206102233, -74.90186466674640542 ) ) ;
#23433 = VECTOR ( 'NONE', #251636, 1000.000000000000000 ) ;
#23434 = DIRECTION ( 'NONE',  ( 0.000000000000000000, 0.000000000000000000, 1.000000000000000000 ) ) ;
#23436 = CARTESIAN_POINT ( 'NONE',  ( 21.05543885634738643, 67.22422895316505276, -191.3387230138097266 ) ) ;
#23435 = DIRECTION ( 'NONE',  ( -1.000000000000000000, -0.000000000000000000, 0.000000000000000000 ) ) ;
#23437 = EDGE_CURVE ( 'NONE', #203363, #31535, #58755, .T. ) ;
#23438 = FACE_OUTER_BOUND ( 'NONE', #58694, .T. ) ;
#23439 = DIRECTION ( 'NONE',  ( 0.000000000000000000, 1.000000000000000000, 0.000000000000000000 ) ) ;
#23440 = CARTESIAN_POINT ( 'NONE',  ( -18.50000000000000000, -1.162701749926853712, -175.5999999999999659 ) ) ;
#23441 = ORIENTED_EDGE ( 'NONE', *, *, #30319, .T. ) ;
#23442 = DIRECTION ( 'NONE',  ( 3.469446951953243109E-14, 0.4999999999999608646, 0.8660254037844612451 ) ) ;
#23443 = EDGE_CURVE ( 'NONE', #69524, #101132, #37431, .T. ) ;
#23444 = VERTEX_POINT ( 'NONE', #243101 ) ;
#23445 = CARTESIAN_POINT ( 'NONE',  ( -14.77538296656415184, 9.436662931799085996, -18.32303673229489149 ) ) ;
#23446 = CIRCLE ( 'NONE', #65102, 0.09999999999999810429 ) ;
#23447 = VERTEX_POINT ( 'NONE', #183149 ) ;
#23448 = EDGE_CURVE ( 'NONE', #256296, #68040, #39804, .T. ) ;
#23449 = DIRECTION ( 'NONE',  ( 0.000000000000000000, -6.938893903907222067E-15, 1.000000000000000000 ) ) ;
#23450 = AXIS2_PLACEMENT_3D ( 'NONE', #47023, #206123, #13079 ) ;
#23451 = EDGE_CURVE ( 'NONE', #125402, #76326, #121892, .T. ) ;
#23452 = CARTESIAN_POINT ( 'NONE',  ( -23.15000000000000213, 4.150000000011156764, -88.15000000000004832 ) ) ;
#23453 = CIRCLE ( 'NONE', #31826, 12.77499999999999503 ) ;
#23454 = ORIENTED_EDGE ( 'NONE', *, *, #131347, .T. ) ;
#23455 = CARTESIAN_POINT ( 'NONE',  ( -16.91049119928363353, 66.05000000001263061, -190.9048278777152632 ) ) ;
#23456 = ADVANCED_FACE ( 'NONE', ( #85288 ), #73394, .T. ) ;
#23457 = ORIENTED_EDGE ( 'NONE', *, *, #90332, .F. ) ;
#23458 = FACE_OUTER_BOUND ( 'NONE', #19781, .T. ) ;
#23459 = LINE ( 'NONE', #125110, #7649 ) ;
#23460 = CYLINDRICAL_SURFACE ( 'NONE', #153318, 0.1000000000000028644 ) ;
#23461 = EDGE_CURVE ( 'NONE', #59785, #83634, #42342, .T. ) ;
#23462 = DIRECTION ( 'NONE',  ( -0.000000000000000000, 0.1350103645451859180, 0.9908441862701603542 ) ) ;
#23463 = EDGE_CURVE ( 'NONE', #654, #66129, #175024, .T. ) ;
#23464 = LINE ( 'NONE', #102943, #180470 ) ;
#23466 = CYLINDRICAL_SURFACE ( 'NONE', #58418, 0.09999999999999609201 ) ;
#23465 = DIRECTION ( 'NONE',  ( -0.5932847527679298016, -0.8049926720990051576, -5.621233785078291429E-15 ) ) ;
#23467 = CYLINDRICAL_SURFACE ( 'NONE', #224558, 0.1000000000000028644 ) ;
#23469 = EDGE_LOOP ( 'NONE', ( #138010, #2053, #122836, #34254 ) ) ;
#23468 = CARTESIAN_POINT ( 'NONE',  ( 21.05563370358598263, 65.27576964416608973, -191.3400166685613328 ) ) ;
#23471 = DIRECTION ( 'NONE',  ( -0.7071067811865475727, -0.7071067811865475727, 0.000000000000000000 ) ) ;
#23470 = DIRECTION ( 'NONE',  ( 1.000000000000000000, 0.000000000000000000, 0.000000000000000000 ) ) ;
#23472 = ORIENTED_EDGE ( 'NONE', *, *, #27689, .F. ) ;
#23474 = ORIENTED_EDGE ( 'NONE', *, *, #155622, .T. ) ;
#23473 = CYLINDRICAL_SURFACE ( 'NONE', #15105, 0.1000000000000053763 ) ;
#23475 = AXIS2_PLACEMENT_3D ( 'NONE', #45695, #103080, #203494 ) ;
#23476 = ORIENTED_EDGE ( 'NONE', *, *, #219166, .F. ) ;
#23477 = CARTESIAN_POINT ( 'NONE',  ( 18.43565242384934066, 85.51932773110407027, -62.55013110796493692 ) ) ;
#23478 = DIRECTION ( 'NONE',  ( 0.000000000000000000, 1.000000000000000000, 0.000000000000000000 ) ) ;
#23479 = DIRECTION ( 'NONE',  ( 0.000000000000000000, 0.2617529984165031243, 0.9651348961777157509 ) ) ;
#23480 = EDGE_CURVE ( 'NONE', #131288, #199985, #15386, .T. ) ;
#23481 = ORIENTED_EDGE ( 'NONE', *, *, #254008, .T. ) ;
#23482 = CARTESIAN_POINT ( 'NONE',  ( 21.05000000000000071, -0.09999999998884512298, -127.4593430482987912 ) ) ;
#23483 = DIRECTION ( 'NONE',  ( -1.000000000000000000, 0.000000000000000000, 0.000000000000000000 ) ) ;
#23484 = LINE ( 'NONE', #63859, #64798 ) ;
#23485 = EDGE_CURVE ( 'NONE', #225917, #79334, #158259, .T. ) ;
#23486 = EDGE_CURVE ( 'NONE', #105957, #227500, #154171, .T. ) ;
#23487 = CARTESIAN_POINT ( 'NONE',  ( 18.59999999999999076, 10.20857864377385127, -121.8500000000000369 ) ) ;
#23488 = DIRECTION ( 'NONE',  ( 0.000000000000000000, 0.9908441862701791170, 0.1350103645450472789 ) ) ;
#23490 = AXIS2_PLACEMENT_3D ( 'NONE', #110935, #31438, #74419 ) ;
#23489 = CARTESIAN_POINT ( 'NONE',  ( 23.15000000000000213, -11.64999999999999147, -30.39999999999999503 ) ) ;
#23491 = ORIENTED_EDGE ( 'NONE', *, *, #110843, .F. ) ;
#23492 = VERTEX_POINT ( 'NONE', #93969 ) ;
#23493 = DIRECTION ( 'NONE',  ( 0.000000000000000000, 0.1397316906016290161, -0.9901894034181595305 ) ) ;
#23494 = VECTOR ( 'NONE', #193677, 1000.000000000000000 ) ;
#23495 = AXIS2_PLACEMENT_3D ( 'NONE', #232023, #151192, #53366 ) ;
#23496 = ORIENTED_EDGE ( 'NONE', *, *, #121789, .F. ) ;
#23497 = DIRECTION ( 'NONE',  ( 1.000000000000000000, 0.000000000000000000, 0.000000000000000000 ) ) ;
#23498 = VERTEX_POINT ( 'NONE', #86572 ) ;
#23499 = FACE_OUTER_BOUND ( 'NONE', #80613, .T. ) ;
#23500 = MECHANICAL_DESIGN_GEOMETRIC_PRESENTATION_REPRESENTATION (  '', ( #115046 ), #152677 ) ;
#23501 = EDGE_CURVE ( 'NONE', #40232, #124932, #233267, .T. ) ;
#23502 = FACE_OUTER_BOUND ( 'NONE', #184526, .T. ) ;
#23503 = CARTESIAN_POINT ( 'NONE',  ( 23.24999999999999645, 58.75092140306929167, -245.7296447454341148 ) ) ;
#23504 = EDGE_CURVE ( 'NONE', #185121, #1805, #91583, .T. ) ;
#23505 = CARTESIAN_POINT ( 'NONE',  ( -20.64999999999999858, 68.85000000001259934, -191.1731074845243938 ) ) ;
#23506 = DIRECTION ( 'NONE',  ( -1.000000000000000000, 0.000000000000000000, 0.000000000000000000 ) ) ;
#23507 = EDGE_LOOP ( 'NONE', ( #57717, #253160, #179128, #59181 ) ) ;
#23508 = CARTESIAN_POINT ( 'NONE',  ( -16.87036670365548474, 9.989418819312801290, -87.97956011730209980 ) ) ;
#23509 = EDGE_CURVE ( 'NONE', #98142, #92818, #58240, .T. ) ;
#23510 = FACE_OUTER_BOUND ( 'NONE', #108039, .T. ) ;
#23511 = CARTESIAN_POINT ( 'NONE',  ( -21.08035267497491816, 0.08268862478717949049, -27.16829316021696172 ) ) ;
#23512 = SPHERICAL_SURFACE ( 'NONE', #89243, 0.1000000000000000056 ) ;
#23513 = ORIENTED_EDGE ( 'NONE', *, *, #221889, .F. ) ;
#23515 = DIRECTION ( 'NONE',  ( -1.000000000000000000, 0.000000000000000000, -0.000000000000000000 ) ) ;
#23514 = LINE ( 'NONE', #83416, #12425 ) ;
#23516 = VECTOR ( 'NONE', #182828, 1000.000000000000000 ) ;
#23517 = EDGE_LOOP ( 'NONE', ( #115143, #118785, #241302, #113242 ) ) ;
#23520 = ORIENTED_EDGE ( 'NONE', *, *, #197703, .F. ) ;
#23519 = CARTESIAN_POINT ( 'NONE',  ( -18.59999999999999787, 13.96869538424787649, -210.3925794786331949 ) ) ;
#23518 = CARTESIAN_POINT ( 'NONE',  ( -20.54999999999999716, 1.115600667400684642E-11, -134.0000000000000000 ) ) ;
#23521 = EDGE_LOOP ( 'NONE', ( #8114, #137354, #137297, #166954 ) ) ;
#23522 = DIRECTION ( 'NONE',  ( 0.000000000000000000, 0.000000000000000000, -1.000000000000000000 ) ) ;
#23523 = AXIS2_PLACEMENT_3D ( 'NONE', #76088, #253434, #36995 ) ;
#23524 = DIRECTION ( 'NONE',  ( 1.000000000000000000, 0.000000000000000000, 0.000000000000000000 ) ) ;
#23525 = DIRECTION ( 'NONE',  ( 0.000000000000000000, -0.9910465087640861759, 0.1335171055202901691 ) ) ;
#23526 = EDGE_LOOP ( 'NONE', ( #50340, #42499, #40478 ) ) ;
#23527 = CARTESIAN_POINT ( 'NONE',  ( 19.97071067811865674, 16.69779891432240859, -222.5912266955230621 ) ) ;
#23529 = DIRECTION ( 'NONE',  ( -0.000000000000000000, -0.000000000000000000, 1.000000000000000000 ) ) ;
#23528 =( BOUNDED_CURVE ( )  B_SPLINE_CURVE ( 3, ( #163172, #116638, #55336, #155792 ),
 .UNSPECIFIED., .F., .F. ) 
 B_SPLINE_CURVE_WITH_KNOTS ( ( 4, 4 ),
 ( 3.141592653589706519, 4.712388980384571546 ),
 .UNSPECIFIED. ) 
 CURVE ( )  GEOMETRIC_REPRESENTATION_ITEM ( )  RATIONAL_B_SPLINE_CURVE ( ( 1.000000000000000000, 0.8047378541243723760, 0.8047378541243723760, 1.000000000000000000 ) ) 
 REPRESENTATION_ITEM ( '' )  );
#23530 = CIRCLE ( 'NONE', #202369, 0.09999999999998807065 ) ;
#23532 = DIRECTION ( 'NONE',  ( 1.000000000000000000, 0.000000000000000000, 0.000000000000000000 ) ) ;
#23531 = FACE_OUTER_BOUND ( 'NONE', #188053, .T. ) ;
#23533 = VECTOR ( 'NONE', #116591, 1000.000000000000000 ) ;
#23535 = ORIENTED_EDGE ( 'NONE', *, *, #199981, .T. ) ;
#23534 = DIRECTION ( 'NONE',  ( -1.000000000000000000, -0.000000000000000000, 0.000000000000000000 ) ) ;
#23536 = EDGE_CURVE ( 'NONE', #37861, #186401, #212408, .T. ) ;
#23537 = ORIENTED_EDGE ( 'NONE', *, *, #167891, .T. ) ;
#23538 = EDGE_CURVE ( 'NONE', #23245, #47350, #68333, .T. ) ;
#23539 = DIRECTION ( 'NONE',  ( 0.000000000000000000, -0.1350103645451904977, -0.9908441862701596881 ) ) ;
#23540 = LINE ( 'NONE', #142157, #18723 ) ;
#23541 = AXIS2_PLACEMENT_3D ( 'NONE', #4615, #26793, #84108 ) ;
#23542 = LINE ( 'NONE', #224259, #105580 ) ;
#23543 = ORIENTED_EDGE ( 'NONE', *, *, #115004, .F. ) ;
#23545 = AXIS2_PLACEMENT_3D ( 'NONE', #14980, #54083, #252274 ) ;
#23544 = DIRECTION ( 'NONE',  ( 1.000000000000000000, -7.304098846218133681E-16, -2.111765289898285610E-31 ) ) ;
#23546 = ORIENTED_EDGE ( 'NONE', *, *, #230789, .F. ) ;
#23547 = AXIS2_PLACEMENT_3D ( 'NONE', #101262, #201701, #123455 ) ;
#23548 = LINE ( 'NONE', #171706, #76741 ) ;
#23549 = EDGE_CURVE ( 'NONE', #155597, #255663, #108340, .T. ) ;
#23550 = CARTESIAN_POINT ( 'NONE',  ( 20.94999999999999574, 65.52661458509918191, -128.9444530202758301 ) ) ;
#23551 = CARTESIAN_POINT ( 'NONE',  ( 21.07016717456946253, 6.320940838111409832, -33.50000000000000711 ) ) ;
#23553 = ORIENTED_EDGE ( 'NONE', *, *, #217480, .F. ) ;
#23552 = CIRCLE ( 'NONE', #35990, 0.09999999999999939493 ) ;
#23554 = CARTESIAN_POINT ( 'NONE',  ( -20.94999999999999929, 68.97833521811179480, -99.18954208262705663 ) ) ;
#23555 = EDGE_CURVE ( 'NONE', #233092, #111434, #113544, .T. ) ;
#23556 = EDGE_CURVE ( 'NONE', #85964, #176232, #120830, .T. ) ;
#23557 = VECTOR ( 'NONE', #255036, 1000.000000000000114 ) ;
#23558 = LINE ( 'NONE', #105585, #68987 ) ;
#23559 = EDGE_CURVE ( 'NONE', #2690, #127766, #166626, .T. ) ;
#23560 = ORIENTED_EDGE ( 'NONE', *, *, #90255, .F. ) ;
#23561 = ORIENTED_EDGE ( 'NONE', *, *, #130024, .T. ) ;
#23563 = EDGE_CURVE ( 'NONE', #221934, #226856, #108736, .T. ) ;
#23562 = ADVANCED_FACE ( 'NONE', ( #254316 ), #233512, .T. ) ;
#23564 = ORIENTED_EDGE ( 'NONE', *, *, #151707, .T. ) ;
#23565 = CARTESIAN_POINT ( 'NONE',  ( 18.59999999999998721, 6.933893972137497030, -204.7856458343735255 ) ) ;
#23566 = ORIENTED_EDGE ( 'NONE', *, *, #84798, .F. ) ;
#23568 = ORIENTED_EDGE ( 'NONE', *, *, #23770, .T. ) ;
#23567 = DIRECTION ( 'NONE',  ( -0.000000000000000000, 1.000000000000000000, -0.000000000000000000 ) ) ;
#23569 = ORIENTED_EDGE ( 'NONE', *, *, #112902, .T. ) ;
#23570 = AXIS2_PLACEMENT_3D ( 'NONE', #29613, #93394, #8738 ) ;
#23571 = CIRCLE ( 'NONE', #56805, 0.09999999999999739653 ) ;
#23574 = EDGE_LOOP ( 'NONE', ( #57058, #59760, #110394 ) ) ;
#23573 = EDGE_LOOP ( 'NONE', ( #87331, #234560, #23441, #202511 ) ) ;
#23572 = DIRECTION ( 'NONE',  ( 1.000000000000000000, 0.000000000000000000, 0.000000000000000000 ) ) ;
#23575 = CIRCLE ( 'NONE', #144297, 14.20833333333333748 ) ;
#23576 = VECTOR ( 'NONE', #102056, 1000.000000000000000 ) ;
#23577 = EDGE_LOOP ( 'NONE', ( #22762, #87887, #254692, #100399 ) ) ;
#23578 = LINE ( 'NONE', #3968, #193981 ) ;
#23579 = EDGE_CURVE ( 'NONE', #26810, #224301, #20879, .T. ) ;
#23580 = EDGE_CURVE ( 'NONE', #230427, #182014, #254070, .T. ) ;
#23581 = DIRECTION ( 'NONE',  ( 1.000000000000000000, 3.265361837132813093E-16, -0.000000000000000000 ) ) ;
#23582 = CARTESIAN_POINT ( 'NONE',  ( -18.33981767444424804, 87.02086759565104046, -199.4465615830173135 ) ) ;
#23583 = ORIENTED_EDGE ( 'NONE', *, *, #142070, .T. ) ;
#23584 = ADVANCED_FACE ( 'NONE', ( #26653 ), #75715, .T. ) ;
#23585 = LINE ( 'NONE', #103055, #120519 ) ;
#23587 = ORIENTED_EDGE ( 'NONE', *, *, #236833, .T. ) ;
#23586 = DIRECTION ( 'NONE',  ( 0.000000000000000000, 0.8814952561688428334, -0.4721928772777349570 ) ) ;
#23588 = CARTESIAN_POINT ( 'NONE',  ( -16.77683809663752257, 9.945835743215301505, -180.1639490191041943 ) ) ;
#23590 = ORIENTED_EDGE ( 'NONE', *, *, #40458, .T. ) ;
#23589 = DIRECTION ( 'NONE',  ( 0.000000000000000000, -0.5000000000000016653, 0.8660254037844377084 ) ) ;
#23591 = ORIENTED_EDGE ( 'NONE', *, *, #145650, .F. ) ;
#23592 = EDGE_CURVE ( 'NONE', #34034, #244396, #7058, .T. ) ;
#23593 = VECTOR ( 'NONE', #234063, 1000.000000000000000 ) ;
#23594 = EDGE_CURVE ( 'NONE', #83134, #156105, #87467, .T. ) ;
#23595 = ORIENTED_EDGE ( 'NONE', *, *, #141500, .T. ) ;
#23596 = EDGE_LOOP ( 'NONE', ( #75673, #89368, #212440, #165551 ) ) ;
#23597 = CARTESIAN_POINT ( 'NONE',  ( -33.80000000000000426, 3.175288713399618601, -347.0000000000001137 ) ) ;
#23598 = DIRECTION ( 'NONE',  ( -1.000000000000000000, 0.000000000000000000, 0.000000000000000000 ) ) ;
#23600 = ORIENTED_EDGE ( 'NONE', *, *, #255632, .F. ) ;
#23599 = ORIENTED_EDGE ( 'NONE', *, *, #36171, .T. ) ;
#23601 = VERTEX_POINT ( 'NONE', #29244 ) ;
#23602 = ORIENTED_EDGE ( 'NONE', *, *, #123869, .T. ) ;
#23603 = ORIENTED_EDGE ( 'NONE', *, *, #112417, .T. ) ;
#23604 = CARTESIAN_POINT ( 'NONE',  ( -23.49999999999994316, 87.51781941433023349, -37.75951082105083145 ) ) ;
#23605 = CIRCLE ( 'NONE', #65254, 0.09999999999999892308 ) ;
#23607 = VERTEX_POINT ( 'NONE', #188269 ) ;
#23606 = DIRECTION ( 'NONE',  ( 1.000000000000000000, -0.000000000000000000, -0.000000000000000000 ) ) ;
#23608 = EDGE_CURVE ( 'NONE', #234652, #245055, #116531, .T. ) ;
#23609 = DIRECTION ( 'NONE',  ( 0.000000000000000000, -0.1335171055202901413, 0.9910465087640860649 ) ) ;
#23610 = CARTESIAN_POINT ( 'NONE',  ( -21.65000000000000213, 9.950000000011140600, -46.25000000000000711 ) ) ;
#23611 = VERTEX_POINT ( 'NONE', #14472 ) ;
#23613 = ORIENTED_EDGE ( 'NONE', *, *, #63703, .T. ) ;
#23612 = ORIENTED_EDGE ( 'NONE', *, *, #216250, .T. ) ;
#23614 = ADVANCED_FACE ( 'NONE', ( #157852 ), #195679, .T. ) ;
#23615 = CARTESIAN_POINT ( 'NONE',  ( 18.59999999999999076, 74.16465844978715438, -57.96795619196135618 ) ) ;
#23616 = EDGE_LOOP ( 'NONE', ( #169857, #250289, #180348, #74402 ) ) ;
#23617 = CIRCLE ( 'NONE', #169368, 4.149999999999999467 ) ;
#23618 = VECTOR ( 'NONE', #28138, 1000.000000000000000 ) ;
#23619 = TOROIDAL_SURFACE ( 'NONE', #219383, 4.099999999999999645, 0.1000000000000000056 ) ;
#23620 = CIRCLE ( 'NONE', #15215, 0.6000000000000064171 ) ;
#23621 = DIRECTION ( 'NONE',  ( 1.000000000000000000, -0.000000000000000000, 0.000000000000000000 ) ) ;
#23622 = ORIENTED_EDGE ( 'NONE', *, *, #172451, .T. ) ;
#23623 = EDGE_LOOP ( 'NONE', ( #183859, #88486, #168353, #61897 ) ) ;
#23624 = CARTESIAN_POINT ( 'NONE',  ( -16.97683809663752186, 66.05000000001187743, -89.62074346632789457 ) ) ;
#23625 = ADVANCED_FACE ( 'NONE', ( #135657 ), #129189, .T. ) ;
#23626 = VERTEX_POINT ( 'NONE', #176112 ) ;
#23627 = DIRECTION ( 'NONE',  ( 0.000000000000000000, -0.8814952561688444987, 0.4721928772777320149 ) ) ;
#23628 = CARTESIAN_POINT ( 'NONE',  ( 21.05000000000000071, 75.90220970870321082, -109.2809220950004345 ) ) ;
#23629 = ORIENTED_EDGE ( 'NONE', *, *, #105893, .T. ) ;
#23630 = DIRECTION ( 'NONE',  ( 1.000000000000000000, 0.000000000000000000, 0.000000000000000000 ) ) ;
#23631 = LINE ( 'NONE', #86097, #73773 ) ;
#23632 = CARTESIAN_POINT ( 'NONE',  ( -23.25000000000000000, 54.26389919992384137, -237.1169412515656632 ) ) ;
#23633 = CARTESIAN_POINT ( 'NONE',  ( 20.90000000000000213, 1.786320531569725478, -11.50977166988710820 ) ) ;
#23634 = CARTESIAN_POINT ( 'NONE',  ( -18.50000000000000000, 72.02722222756958104, -225.1832529173024398 ) ) ;
#23635 = CARTESIAN_POINT ( 'NONE',  ( -23.15000000000000213, 11.65000000000000036, -26.48519422934605672 ) ) ;
#23636 = LINE ( 'NONE', #199697, #209910 ) ;
#23637 = CIRCLE ( 'NONE', #135997, 0.09999999999999939493 ) ;
#23638 = VECTOR ( 'NONE', #87132, 1000.000000000000000 ) ;
#23639 = AXIS2_PLACEMENT_3D ( 'NONE', #83425, #142142, #20950 ) ;
#23640 = ORIENTED_EDGE ( 'NONE', *, *, #45784, .F. ) ;
#23641 = ADVANCED_FACE ( 'NONE', ( #219047 ), #22168, .F. ) ;
#23643 = ORIENTED_EDGE ( 'NONE', *, *, #106886, .F. ) ;
#23642 = ORIENTED_EDGE ( 'NONE', *, *, #240347, .T. ) ;
#23644 = CIRCLE ( 'NONE', #215141, 0.2000000000000057288 ) ;
#23645 = VERTEX_POINT ( 'NONE', #56115 ) ;
#23646 = LINE ( 'NONE', #2743, #16100 ) ;
#23647 = CARTESIAN_POINT ( 'NONE',  ( -18.59999999999999787, -1.164121893230052995, -108.3148480855716542 ) ) ;
#23649 = CARTESIAN_POINT ( 'NONE',  ( -15.06774609480955363, 9.417651958841000592, -15.35878739244043345 ) ) ;
#23648 = CYLINDRICAL_SURFACE ( 'NONE', #32815, 0.09999999999999939493 ) ;
#23650 = CARTESIAN_POINT ( 'NONE',  ( -21.13498764882296044, 75.99834360528086563, -143.0187256279982364 ) ) ;
#23651 = EDGE_LOOP ( 'NONE', ( #40309, #156661, #30934, #133444 ) ) ;
#23652 = CARTESIAN_POINT ( 'NONE',  ( -23.25000000000000000, 4.350000000011156054, -79.15000000000004832 ) ) ;
#23653 = CYLINDRICAL_SURFACE ( 'NONE', #162578, 0.09999999999999939493 ) ;
#23654 = CARTESIAN_POINT ( 'NONE',  ( 19.75857864376268935, 64.35000000001197407, -111.6731074845243796 ) ) ;
#23655 = DIRECTION ( 'NONE',  ( 0.000000000000000000, 0.000000000000000000, 1.000000000000000000 ) ) ;
#23656 = VERTEX_POINT ( 'NONE', #58679 ) ;
#23657 = AXIS2_PLACEMENT_3D ( 'NONE', #31945, #111453, #192289 ) ;
#23658 = DIRECTION ( 'NONE',  ( -1.000000000000000000, 0.000000000000000000, 0.000000000000000000 ) ) ;
#23659 = CARTESIAN_POINT ( 'NONE',  ( 18.39999999999999147, 8.822561741666397950, -9.250000000000001776 ) ) ;
#23660 = ORIENTED_EDGE ( 'NONE', *, *, #151970, .T. ) ;
#23661 = CARTESIAN_POINT ( 'NONE',  ( -16.87383368123029825, 66.05000000001157900, -56.87310748452438958 ) ) ;
#23662 = CARTESIAN_POINT ( 'NONE',  ( 20.73486653747088937, 68.25000000001251976, -182.6731074845244223 ) ) ;
#23663 = DIRECTION ( 'NONE',  ( 1.000000000000000000, 0.000000000000000000, 0.000000000000000000 ) ) ;
#23664 = CARTESIAN_POINT ( 'NONE',  ( -2.995603634470891112E-16, -11.74999999998884448, -179.7499999999999716 ) ) ;
#23665 = CIRCLE ( 'NONE', #7055, 0.1999999999999987899 ) ;
#23666 = CARTESIAN_POINT ( 'NONE',  ( -18.41431012584568805, 11.48747202920817223, -24.27323601310168399 ) ) ;
#23667 = VERTEX_POINT ( 'NONE', #100369 ) ;
#23668 = CARTESIAN_POINT ( 'NONE',  ( 20.94999999999999574, 74.25000000001229239, -158.3535959266227451 ) ) ;
#23669 = CARTESIAN_POINT ( 'NONE',  ( -21.64999999999999858, 66.65000000001158753, -56.87310748452438958 ) ) ;
#23670 = CARTESIAN_POINT ( 'NONE',  ( -21.04999999999999716, 0.05132743235275089716, -60.69981666373099216 ) ) ;
#23671 = DIRECTION ( 'NONE',  ( -0.000000000000000000, -0.1350103645451904977, 0.9908441862701596881 ) ) ;
#23673 = EDGE_CURVE ( 'NONE', #87546, #69800, #50062, .T. ) ;
#23672 = DIRECTION ( 'NONE',  ( 1.000000000000000000, -0.000000000000000000, -0.000000000000000000 ) ) ;
#23674 = VECTOR ( 'NONE', #52885, 1000.000000000000000 ) ;
#23675 = DIRECTION ( 'NONE',  ( 0.000000000000000000, -0.4088369013363783999, 0.9126074666063545004 ) ) ;
#23676 = DIRECTION ( 'NONE',  ( 0.000000000000000000, 0.000000000000000000, -1.000000000000000000 ) ) ;
#23677 = CARTESIAN_POINT ( 'NONE',  ( 18.44444291854882678, -9.490101180932073888, -207.6289039648910091 ) ) ;
#23678 = VECTOR ( 'NONE', #115821, 1000.000000000000000 ) ;
#23680 = ORIENTED_EDGE ( 'NONE', *, *, #45774, .T. ) ;
#23679 = FACE_OUTER_BOUND ( 'NONE', #144545, .T. ) ;
#23682 = ORIENTED_EDGE ( 'NONE', *, *, #118094, .T. ) ;
#23681 = AXIS2_PLACEMENT_3D ( 'NONE', #206167, #224432, #103190 ) ;
#23683 = EDGE_CURVE ( 'NONE', #71927, #107433, #17029, .T. ) ;
#23684 = CARTESIAN_POINT ( 'NONE',  ( -20.85000000000000142, 76.00000000001244871, -170.0231074845243597 ) ) ;
#23685 = EDGE_CURVE ( 'NONE', #166580, #228001, #59964, .T. ) ;
#23686 = CARTESIAN_POINT ( 'NONE',  ( -20.54999999999999716, 1.148907358139439339E-11, -201.0000000000015064 ) ) ;
#23687 = CARTESIAN_POINT ( 'NONE',  ( 18.49999999999999289, 64.25000000001202238, -114.7731074845243882 ) ) ;
#23689 = ADVANCED_FACE ( 'NONE', ( #255569 ), #108510, .T. ) ;
#23688 = VECTOR ( 'NONE', #86199, 1000.000000000000000 ) ;
#23690 = ORIENTED_EDGE ( 'NONE', *, *, #60606, .F. ) ;
#23691 = CIRCLE ( 'NONE', #102736, 2.000000000000002220 ) ;
#23692 = CARTESIAN_POINT ( 'NONE',  ( 21.08489834409762054, 65.37767610527603779, -57.17310748452440805 ) ) ;
#23693 = CARTESIAN_POINT ( 'NONE',  ( 22.39999999999999503, 11.65000000001116298, -33.40000000000000568 ) ) ;
#23694 = ADVANCED_FACE ( 'NONE', ( #179949 ), #156559, .F. ) ;
#23695 = CIRCLE ( 'NONE', #102931, 0.09999999999999999167 ) ;
#23697 = ORIENTED_EDGE ( 'NONE', *, *, #228776, .F. ) ;
#23696 = ADVANCED_FACE ( 'NONE', ( #2566 ), #234777, .T. ) ;
#23698 = CARTESIAN_POINT ( 'NONE',  ( -20.64999999999999858, 74.00000000001186606, -89.79848556176222019 ) ) ;
#23701 = VERTEX_POINT ( 'NONE', #198210 ) ;
#23700 = CARTESIAN_POINT ( 'NONE',  ( -16.77308656112215601, 9.950000000011133494, -188.3498068082976431 ) ) ;
#23699 = PRESENTATION_LAYER_ASSIGNMENT (  '', '', ( #231784 ) ) ;
#23703 = CARTESIAN_POINT ( 'NONE',  ( -23.15000000000000213, 87.48912529308749697, -39.02310748452423894 ) ) ;
#23702 = CARTESIAN_POINT ( 'NONE',  ( -21.05000000000000071, 3.338403738567107926, -231.7022719401450388 ) ) ;
#23704 = AXIS2_PLACEMENT_3D ( 'NONE', #37275, #153396, #116790 ) ;
#23705 = EDGE_CURVE ( 'NONE', #159849, #79539, #248001, .T. ) ;
#23706 =( LENGTH_UNIT ( ) NAMED_UNIT ( * ) SI_UNIT ( .MILLI., .METRE. ) );
#23708 = ORIENTED_EDGE ( 'NONE', *, *, #34887, .T. ) ;
#23707 = CIRCLE ( 'NONE', #136066, 0.1000000000000076522 ) ;
#23709 =( NAMED_UNIT ( * ) PLANE_ANGLE_UNIT ( ) SI_UNIT ( $, .RADIAN. ) );
#23710 = FACE_OUTER_BOUND ( 'NONE', #199621, .T. ) ;
#23711 = CARTESIAN_POINT ( 'NONE',  ( 21.05000000000000071, 67.18479819544440090, -128.1025699878376827 ) ) ;
#23712 = ADVANCED_FACE ( 'NONE', ( #241211 ), #23466, .F. ) ;
#23713 = VERTEX_POINT ( 'NONE', #161681 ) ;
#23714 = CARTESIAN_POINT ( 'NONE',  ( -21.05000000000000071, 0.000000000000000000, -33.50000000000000000 ) ) ;
#23715 = AXIS2_PLACEMENT_3D ( 'NONE', #199975, #184244, #164692 ) ;
#23716 = FACE_OUTER_BOUND ( 'NONE', #53170, .T. ) ;
#23717 = CIRCLE ( 'NONE', #240175, 0.1000000000000028644 ) ;
#23718 = VECTOR ( 'NONE', #206841, 1000.000000000000000 ) ;
#23719 = DIRECTION ( 'NONE',  ( 0.000000000000000000, 0.2617529984164955192, 0.9651348961777177493 ) ) ;
#23720 = DIRECTION ( 'NONE',  ( 1.000000000000000000, 0.000000000000000000, -0.000000000000000000 ) ) ;
#23721 = VERTEX_POINT ( 'NONE', #142082 ) ;
#23722 = EDGE_CURVE ( 'NONE', #204034, #146220, #150228, .T. ) ;
#23723 = VERTEX_POINT ( 'NONE', #102945 ) ;
#23724 = SPHERICAL_SURFACE ( 'NONE', #196498, 0.1000000000000000056 ) ;
#23725 = EDGE_CURVE ( 'NONE', #206012, #124831, #121020, .T. ) ;
#23726 = DIRECTION ( 'NONE',  ( -0.000000000000000000, 0.8700118002898356018, -0.4930308989875170078 ) ) ;
#23727 = DIRECTION ( 'NONE',  ( 0.000000000000000000, 0.000000000000000000, 1.000000000000000000 ) ) ;
#23728 = LINE ( 'NONE', #104480, #228514 ) ;
#23729 = CARTESIAN_POINT ( 'NONE',  ( 17.74533788810829904, 65.18150020854101001, -79.83673015947196916 ) ) ;
#23730 = AXIS2_PLACEMENT_3D ( 'NONE', #8500, #87998, #247082 ) ;
#23731 = FACE_OUTER_BOUND ( 'NONE', #93064, .T. ) ;
#23732 = DIRECTION ( 'NONE',  ( -1.284434275755705789E-16, 0.7071067811865472397, -0.7071067811865479058 ) ) ;
#23733 = CARTESIAN_POINT ( 'NONE',  ( 21.97500000000000497, 22.53103078161933936, -230.9224853114453140 ) ) ;
#23734 = CARTESIAN_POINT ( 'NONE',  ( 18.47688499308726406, -9.464855950272974994, -107.2013477531374406 ) ) ;
#23735 = EDGE_LOOP ( 'NONE', ( #58433, #167495, #115406, #215906 ) ) ;
#23736 = DIRECTION ( 'NONE',  ( 0.000000000000000000, 0.9908441862701782288, 0.1350103645450542456 ) ) ;
#23738 = ORIENTED_EDGE ( 'NONE', *, *, #55589, .F. ) ;
#23737 = CARTESIAN_POINT ( 'NONE',  ( 23.14999999999999503, 38.38020821401235594, -234.4776589466471819 ) ) ;
#23739 = CARTESIAN_POINT ( 'NONE',  ( -20.94999999999999929, 64.25000000001209344, -129.5083017138703667 ) ) ;
#23740 = DIRECTION ( 'NONE',  ( 1.000000000000000000, 0.000000000000000000, 0.000000000000000000 ) ) ;
#23742 = CARTESIAN_POINT ( 'NONE',  ( 23.24999999999997513, 17.01923898301590654, -224.3994341343041867 ) ) ;
#23741 = CARTESIAN_POINT ( 'NONE',  ( 21.05000000000000071, 11.75000000001116263, -193.9851942293460070 ) ) ;
#23743 = EDGE_CURVE ( 'NONE', #140330, #220964, #72133, .T. ) ;
#23744 = EDGE_LOOP ( 'NONE', ( #250062, #175573, #167220, #201461 ) ) ;
#23746 = DIRECTION ( 'NONE',  ( 0.000000000000000000, 0.2617529984164915779, 0.9651348961777189706 ) ) ;
#23745 = CARTESIAN_POINT ( 'NONE',  ( -23.25000000000000000, -0.09999999998884338825, -55.35042919245524473 ) ) ;
#23747 = CARTESIAN_POINT ( 'NONE',  ( 21.05000000000005400, 76.00000000001119815, -36.02310748452479316 ) ) ;
#23748 = DIRECTION ( 'NONE',  ( 0.000000000000000000, -0.2617529984165031243, -0.9651348961777157509 ) ) ;
#23749 = FACE_OUTER_BOUND ( 'NONE', #126832, .T. ) ;
#23750 = CARTESIAN_POINT ( 'NONE',  ( -12.48127053791144725, 66.62341902196861554, -185.8961612375124446 ) ) ;
#23751 = VERTEX_POINT ( 'NONE', #211638 ) ;
#23752 = EDGE_LOOP ( 'NONE', ( #157790, #202216, #116557, #164669 ) ) ;
#23753 = CIRCLE ( 'NONE', #169499, 0.09999999999999939493 ) ;
#23754 = VECTOR ( 'NONE', #191393, 1000.000000000000000 ) ;
#23755 = FACE_OUTER_BOUND ( 'NONE', #232277, .T. ) ;
#23756 = EDGE_LOOP ( 'NONE', ( #77803, #50328, #103182, #165089, #111690 ) ) ;
#23757 = DIRECTION ( 'NONE',  ( -1.000000000000000000, 0.000000000000000000, 0.000000000000000000 ) ) ;
#23758 = VERTEX_POINT ( 'NONE', #74727 ) ;
#23759 = ADVANCED_FACE ( 'NONE', ( #130798 ), #29442, .F. ) ;
#23760 = FACE_OUTER_BOUND ( 'NONE', #7549, .T. ) ;
#23761 = DIRECTION ( 'NONE',  ( 0.000000000000000000, -0.000000000000000000, -1.000000000000000000 ) ) ;
#23762 = EDGE_LOOP ( 'NONE', ( #37477, #40612, #63650 ) ) ;
#23764 = EDGE_CURVE ( 'NONE', #165453, #60977, #90381, .T. ) ;
#23763 = VECTOR ( 'NONE', #237844, 1000.000000000000000 ) ;
#23765 = FACE_OUTER_BOUND ( 'NONE', #144898, .T. ) ;
#23767 = CIRCLE ( 'NONE', #11260, 0.5000000000000007772 ) ;
#23766 = CARTESIAN_POINT ( 'NONE',  ( -16.92507428761700439, 66.05000000001201954, -115.7365049441459490 ) ) ;
#23768 = DIRECTION ( 'NONE',  ( 0.000000000000000000, 0.1298341882520022694, 0.9915357197604852679 ) ) ;
#23769 = AXIS2_PLACEMENT_3D ( 'NONE', #178640, #116079, #239878 ) ;
#23770 = EDGE_CURVE ( 'NONE', #221704, #239471, #229331, .T. ) ;
#23771 = LINE ( 'NONE', #215811, #191559 ) ;
#23772 = EDGE_CURVE ( 'NONE', #14564, #56338, #216664, .T. ) ;
#23773 = CARTESIAN_POINT ( 'NONE',  ( -23.15000000000000213, 74.00000000001156764, -56.79848556176223440 ) ) ;
#23774 = FACE_OUTER_BOUND ( 'NONE', #78388, .T. ) ;
#23775 = CYLINDRICAL_SURFACE ( 'NONE', #90446, 0.1000000000000013933 ) ;
#23776 = ORIENTED_EDGE ( 'NONE', *, *, #226570, .F. ) ;
#23779 = EDGE_CURVE ( 'NONE', #200909, #62075, #241785, .T. ) ;
#23778 = CARTESIAN_POINT ( 'NONE',  ( -22.50000000000000000, 75.90000000001276703, -215.1726782920691505 ) ) ;
#23777 = CARTESIAN_POINT ( 'NONE',  ( -21.59142135623730852, 21.63386431479164784, -232.5973262981661094 ) ) ;
#23780 = ORIENTED_EDGE ( 'NONE', *, *, #15108, .F. ) ;
#23782 = ORIENTED_EDGE ( 'NONE', *, *, #219485, .F. ) ;
#23781 = CARTESIAN_POINT ( 'NONE',  ( -21.05000000000000071, 77.25000000001189449, -95.02310748452430289 ) ) ;
#23783 = AXIS2_PLACEMENT_3D ( 'NONE', #74778, #250797, #34354 ) ;
#23784 = EDGE_LOOP ( 'NONE', ( #231979, #24575, #160742, #180064 ) ) ;
#23785 = DIRECTION ( 'NONE',  ( 2.879366945564059217E-14, 0.9875055080513762684, -0.1575844902526679081 ) ) ;
#23786 = CARTESIAN_POINT ( 'NONE',  ( 21.05000000000005400, 67.85000000001119247, -3.023107484524792277 ) ) ;
#23787 = DIRECTION ( 'NONE',  ( 1.000000000000000000, 0.000000000000000000, 0.000000000000000000 ) ) ;
#23788 = EDGE_CURVE ( 'NONE', #47449, #214318, #173836, .T. ) ;
#23789 = DIRECTION ( 'NONE',  ( -1.000000000000000000, -0.000000000000000000, -0.000000000000000000 ) ) ;
#23790 = ORIENTED_EDGE ( 'NONE', *, *, #27924, .F. ) ;
#23791 = DIRECTION ( 'NONE',  ( 1.000000000000000000, 0.000000000000000000, 0.000000000000000000 ) ) ;
#23792 = DIRECTION ( 'NONE',  ( -1.000000000000000000, -7.304098846218134667E-16, 0.000000000000000000 ) ) ;
#23793 = EDGE_LOOP ( 'NONE', ( #192427, #103359, #38538, #255459 ) ) ;
#23794 = DIRECTION ( 'NONE',  ( -0.000000000000000000, -6.982962677686266711E-15, 1.000000000000000000 ) ) ;
#23795 = DIRECTION ( 'NONE',  ( -1.000000000000000000, -1.836970198721029934E-16, 0.000000000000000000 ) ) ;
#23796 = AXIS2_PLACEMENT_3D ( 'NONE', #187888, #168358, #47056 ) ;
#23797 = ORIENTED_EDGE ( 'NONE', *, *, #106100, .F. ) ;
#23798 = AXIS2_PLACEMENT_3D ( 'NONE', #61796, #1800, #145163 ) ;
#23799 = CARTESIAN_POINT ( 'NONE',  ( -16.77431908686106254, 9.945805754529134290, -146.6641607823497964 ) ) ;
#23800 = AXIS2_PLACEMENT_3D ( 'NONE', #98162, #17386, #177764 ) ;
#23801 = AXIS2_PLACEMENT_3D ( 'NONE', #209306, #131059, #188465 ) ;
#23802 = EDGE_CURVE ( 'NONE', #90690, #82095, #172554, .T. ) ;
#23803 = DIRECTION ( 'NONE',  ( -0.000000000000000000, 1.000000000000000000, -0.000000000000000000 ) ) ;
#23804 = ORIENTED_EDGE ( 'NONE', *, *, #187803, .F. ) ;
#23805 = CARTESIAN_POINT ( 'NONE',  ( -18.59999999999999787, -1.149570369564537842, -74.81591248450196474 ) ) ;
#23806 = EDGE_CURVE ( 'NONE', #111193, #245252, #154354, .T. ) ;
#23807 = CARTESIAN_POINT ( 'NONE',  ( 21.14999999999999503, 36.65892442174472876, -249.5511627012454596 ) ) ;
#23808 = CARTESIAN_POINT ( 'NONE',  ( 5.899999999999995914, -11.25000000000000000, 10.10000000000000142 ) ) ;
#23809 = EDGE_CURVE ( 'NONE', #95921, #100505, #79270, .T. ) ;
#23810 = CARTESIAN_POINT ( 'NONE',  ( 18.59999999999998721, 56.14960075277809182, -67.24280442672311153 ) ) ;
#23811 = AXIS2_PLACEMENT_3D ( 'NONE', #14722, #12152, #91662 ) ;
#23812 = VECTOR ( 'NONE', #14716, 1000.000000000000114 ) ;
#23813 = TOROIDAL_SURFACE ( 'NONE', #94496, 0.2000000000000000111, 0.1000000000000000056 ) ;
#23814 = CARTESIAN_POINT ( 'NONE',  ( -21.14999999999999858, 87.65000000001266756, -200.6231074845242688 ) ) ;
#23815 = CARTESIAN_POINT ( 'NONE',  ( 18.59999999999999076, -1.835859311432481045, -78.50443916879852679 ) ) ;
#23816 = CYLINDRICAL_SURFACE ( 'NONE', #156288, 0.09999999999998898659 ) ;
#23817 = ORIENTED_EDGE ( 'NONE', *, *, #163792, .F. ) ;
#23818 = CARTESIAN_POINT ( 'NONE',  ( -20.94999999999999929, 2.859758780633683273, -208.6670499591424459 ) ) ;
#23819 = AXIS2_PLACEMENT_3D ( 'NONE', #148198, #90777, #128653 ) ;
#23820 = VERTEX_POINT ( 'NONE', #149102 ) ;
#23821 = FACE_OUTER_BOUND ( 'NONE', #47217, .T. ) ;
#23822 = DIRECTION ( 'NONE',  ( -1.000000000000000000, -0.000000000000000000, 0.000000000000000000 ) ) ;
#23824 = ORIENTED_EDGE ( 'NONE', *, *, #174058, .T. ) ;
#23823 = DIRECTION ( 'NONE',  ( -1.000000000000000000, 0.000000000000000000, 0.000000000000000000 ) ) ;
#23826 = EDGE_LOOP ( 'NONE', ( #149908, #110448 ) ) ;
#23825 = LINE ( 'NONE', #121634, #249513 ) ;
#23827 = CARTESIAN_POINT ( 'NONE',  ( -23.15000000000000213, 68.66552716081216090, -214.3300732090495444 ) ) ;
#23828 = CARTESIAN_POINT ( 'NONE',  ( -18.59999999999999787, -9.399999999988787991, -74.29725975966333351 ) ) ;
#23829 = DIRECTION ( 'NONE',  ( 0.000000000000000000, -6.982962677686267499E-15, 1.000000000000000000 ) ) ;
#23832 = EDGE_CURVE ( 'NONE', #172414, #170581, #208659, .T. ) ;
#23831 = ORIENTED_EDGE ( 'NONE', *, *, #147397, .F. ) ;
#23830 = CARTESIAN_POINT ( 'NONE',  ( -21.05000000000000071, 1.115600667400684642E-11, -134.0000000000000000 ) ) ;
#23833 = AXIS2_PLACEMENT_3D ( 'NONE', #31651, #109852, #212835 ) ;
#23834 = CARTESIAN_POINT ( 'NONE',  ( -21.05000000000000071, 5.850000000011156942, -157.3675027757221017 ) ) ;
#23835 = ORIENTED_EDGE ( 'NONE', *, *, #81866, .F. ) ;
#23836 = ORIENTED_EDGE ( 'NONE', *, *, #64973, .T. ) ;
#23837 = CARTESIAN_POINT ( 'NONE',  ( -18.45140287520618472, 85.48607773954091726, -29.38258435783816225 ) ) ;
#23838 = FACE_OUTER_BOUND ( 'NONE', #246311, .T. ) ;
#23839 = CIRCLE ( 'NONE', #40604, 0.1000000000000052097 ) ;
#23840 = EDGE_LOOP ( 'NONE', ( #16308, #99363 ) ) ;
#23841 = DIRECTION ( 'NONE',  ( 0.000000000000000000, -0.9770955615653316162, -0.2128009952263604232 ) ) ;
#23842 = EDGE_CURVE ( 'NONE', #238290, #167205, #52538, .T. ) ;
#23843 = CARTESIAN_POINT ( 'NONE',  ( -23.25000000000000355, 5.649999999999983480, -20.85000000000000142 ) ) ;
#23844 = AXIS2_PLACEMENT_3D ( 'NONE', #177713, #219362, #78568 ) ;
#23845 = EDGE_CURVE ( 'NONE', #88893, #65641, #91765, .T. ) ;
#23846 = VERTEX_POINT ( 'NONE', #132089 ) ;
#23847 = AXIS2_PLACEMENT_3D ( 'NONE', #220195, #237192, #16871 ) ;
#23848 = CARTESIAN_POINT ( 'NONE',  ( 21.08621493067296271, 6.191908953220322864, -199.5939561276201459 ) ) ;
#23849 = CARTESIAN_POINT ( 'NONE',  ( 22.50000000000000000, 0.09999999999999939493, 7.790779598373383408 ) ) ;
#23850 = CIRCLE ( 'NONE', #33182, 11.64999999999999325 ) ;
#23851 = EDGE_CURVE ( 'NONE', #172217, #113945, #45968, .T. ) ;
#23852 = ORIENTED_EDGE ( 'NONE', *, *, #172448, .F. ) ;
#23853 = ORIENTED_EDGE ( 'NONE', *, *, #92770, .F. ) ;
#23856 = EDGE_CURVE ( 'NONE', #217484, #167927, #175201, .T. ) ;
#23855 = CARTESIAN_POINT ( 'NONE',  ( -21.15000000000000213, 60.91865828504416669, -234.1430899377568551 ) ) ;
#23854 = AXIS2_PLACEMENT_3D ( 'NONE', #217575, #158938, #119807 ) ;
#23857 = ORIENTED_EDGE ( 'NONE', *, *, #207576, .T. ) ;
#23858 = CARTESIAN_POINT ( 'NONE',  ( -16.77683809663752257, 22.98839712131283974, -230.9453208111996503 ) ) ;
#23859 = VECTOR ( 'NONE', #199086, 1000.000000000000000 ) ;
#23860 = EDGE_LOOP ( 'NONE', ( #140501, #95111, #198916, #131935, #123014 ) ) ;
#23862 = ORIENTED_EDGE ( 'NONE', *, *, #133298, .T. ) ;
#23861 = DIRECTION ( 'NONE',  ( 1.000000000000000000, -1.335000415235278971E-16, 2.979993593738921214E-16 ) ) ;
#23863 = FACE_OUTER_BOUND ( 'NONE', #251869, .T. ) ;
#23864 = VERTEX_POINT ( 'NONE', #154272 ) ;
#23865 = CARTESIAN_POINT ( 'NONE',  ( -20.64999999999999858, 70.60814576644823148, -215.7631455941064189 ) ) ;
#23866 = ORIENTED_EDGE ( 'NONE', *, *, #30190, .F. ) ;
#23868 = VERTEX_POINT ( 'NONE', #150383 ) ;
#23867 = ORIENTED_EDGE ( 'NONE', *, *, #207160, .F. ) ;
#23869 = CARTESIAN_POINT ( 'NONE',  ( 20.04142135623730070, 62.34315093393704643, -208.9889535843037720 ) ) ;
#23870 = CARTESIAN_POINT ( 'NONE',  ( -21.04386569057474432, 56.16954312985654241, -227.9354499029107046 ) ) ;
#23872 = EDGE_LOOP ( 'NONE', ( #158148, #106260, #33210, #29767 ) ) ;
#23871 = VECTOR ( 'NONE', #23726, 1000.000000000000114 ) ;
#23873 = ADVANCED_FACE ( 'NONE', ( #51236 ), #210353, .T. ) ;
#23875 = EDGE_CURVE ( 'NONE', #139949, #92460, #187645, .T. ) ;
#23874 = AXIS2_PLACEMENT_3D ( 'NONE', #37333, #253774, #256287 ) ;
#23876 = ORIENTED_EDGE ( 'NONE', *, *, #179472, .T. ) ;
#23877 = CIRCLE ( 'NONE', #140356, 0.09999999999999939493 ) ;
#23878 = DIRECTION ( 'NONE',  ( 0.000000000000000000, 0.2128009952263604232, -0.9770955615653316162 ) ) ;
#23879 = DIRECTION ( 'NONE',  ( 0.000000000000000000, -0.9651348961777157509, 0.2617529984165031243 ) ) ;
#23881 = ORIENTED_EDGE ( 'NONE', *, *, #239800, .F. ) ;
#23880 = CARTESIAN_POINT ( 'NONE',  ( -20.94999999999999929, 16.44800918141279666, -240.8068063186265135 ) ) ;
#23882 = FACE_OUTER_BOUND ( 'NONE', #182960, .T. ) ;
#23883 = ORIENTED_EDGE ( 'NONE', *, *, #6983, .T. ) ;
#23884 = CIRCLE ( 'NONE', #57143, 0.09999999999999939493 ) ;
#23885 = DIRECTION ( 'NONE',  ( 0.000000000000000000, 0.9999631594459056361, -0.008583690987128059571 ) ) ;
#23886 = CARTESIAN_POINT ( 'NONE',  ( 18.69999999999999929, 11.49641995933507843, -1.885425182446135661 ) ) ;
#23887 = ORIENTED_EDGE ( 'NONE', *, *, #94759, .T. ) ;
#23889 = EDGE_CURVE ( 'NONE', #122770, #203779, #50228, .T. ) ;
#23888 = DIRECTION ( 'NONE',  ( 0.000000000000000000, 0.000000000000000000, -1.000000000000000000 ) ) ;
#23890 = VERTEX_POINT ( 'NONE', #27679 ) ;
#23891 = ADVANCED_FACE ( 'NONE', ( #225807 ), #86295, .T. ) ;
#23892 = CARTESIAN_POINT ( 'NONE',  ( 21.05000000000000071, 11.75000000001116263, -59.98519422934605672 ) ) ;
#23893 = ORIENTED_EDGE ( 'NONE', *, *, #105148, .F. ) ;
#23894 = AXIS2_PLACEMENT_3D ( 'NONE', #38045, #215363, #77138 ) ;
#23895 = AXIS2_PLACEMENT_3D ( 'NONE', #6703, #221874, #2834 ) ;
#23896 = AXIS2_PLACEMENT_3D ( 'NONE', #25908, #226650, #84533 ) ;
#23898 = ORIENTED_EDGE ( 'NONE', *, *, #32116, .F. ) ;
#23897 = ORIENTED_EDGE ( 'NONE', *, *, #235188, .F. ) ;
#23899 = ORIENTED_EDGE ( 'NONE', *, *, #204444, .F. ) ;
#23900 = CARTESIAN_POINT ( 'NONE',  ( -16.81744102076749314, 9.950000000011142376, -79.65000000000004832 ) ) ;
#23901 = ORIENTED_EDGE ( 'NONE', *, *, #93525, .T. ) ;
#23902 = DIRECTION ( 'NONE',  ( -1.020425574104003999E-15, -0.2128009952263603677, 0.9770955615653313941 ) ) ;
#23903 = VERTEX_POINT ( 'NONE', #102000 ) ;
#23904 = ADVANCED_FACE ( 'NONE', ( #236712 ), #2920, .F. ) ;
#23905 = FACE_OUTER_BOUND ( 'NONE', #218932, .T. ) ;
#23906 = DIRECTION ( 'NONE',  ( 0.000000000000000000, 0.000000000000000000, 1.000000000000000000 ) ) ;
#23907 = ORIENTED_EDGE ( 'NONE', *, *, #58608, .F. ) ;
#23908 = CIRCLE ( 'NONE', #173954, 0.2000000000000048683 ) ;
#23909 = VERTEX_POINT ( 'NONE', #223253 ) ;
#23910 = ADVANCED_FACE ( 'NONE', ( #202419 ), #66770, .F. ) ;
#23911 = ORIENTED_EDGE ( 'NONE', *, *, #144941, .F. ) ;
#23912 = CIRCLE ( 'NONE', #227896, 0.09999999999998898659 ) ;
#23913 = CARTESIAN_POINT ( 'NONE',  ( -16.92973740335360944, 66.00749618554500842, -82.11704844932265246 ) ) ;
#23914 = ORIENTED_EDGE ( 'NONE', *, *, #143237, .F. ) ;
#23915 = CARTESIAN_POINT ( 'NONE',  ( 18.44364597020197039, 85.49048731717461180, -162.9651295948404481 ) ) ;
#23916 = EDGE_CURVE ( 'NONE', #91428, #80096, #249981, .T. ) ;
#23917 = CYLINDRICAL_SURFACE ( 'NONE', #26188, 0.09999999999999939493 ) ;
#23918 = DIRECTION ( 'NONE',  ( -0.000000000000000000, -1.000000000000000000, -6.982962677686266711E-15 ) ) ;
#23919 = VECTOR ( 'NONE', #180349, 1000.000000000000000 ) ;
#23920 = CARTESIAN_POINT ( 'NONE',  ( -23.15000000000000213, 0.000000000000000000, -33.50000000000000000 ) ) ;
#23921 = DIRECTION ( 'NONE',  ( 0.000000000000000000, 0.9126074666063772600, 0.4088369013363274407 ) ) ;
#23922 = VECTOR ( 'NONE', #44716, 1000.000000000000000 ) ;
#23923 = DIRECTION ( 'NONE',  ( 0.000000000000000000, -7.545205021724366615E-15, 1.000000000000000000 ) ) ;
#23925 = CARTESIAN_POINT ( 'NONE',  ( -20.64999999999999858, -9.400000000000002132, -23.60603087734756045 ) ) ;
#23924 = DIRECTION ( 'NONE',  ( 0.000000000000000000, 0.000000000000000000, -1.000000000000000000 ) ) ;
#23926 = DIRECTION ( 'NONE',  ( 0.000000000000000000, 6.982962677686266711E-15, -1.000000000000000000 ) ) ;
#23927 = CIRCLE ( 'NONE', #40693, 0.09999999999999961697 ) ;
#23928 = DIRECTION ( 'NONE',  ( 1.000000000000000000, 3.265361837132813093E-16, -0.000000000000000000 ) ) ;
#23929 = FACE_OUTER_BOUND ( 'NONE', #19716, .T. ) ;
#23930 = CARTESIAN_POINT ( 'NONE',  ( -23.15000000000000213, 76.00000000001234923, -165.9731074845243768 ) ) ;
#23932 = ORIENTED_EDGE ( 'NONE', *, *, #106728, .T. ) ;
#23931 = CIRCLE ( 'NONE', #173806, 0.1000000000000013933 ) ;
#23934 = ORIENTED_EDGE ( 'NONE', *, *, #10382, .F. ) ;
#23933 = DIRECTION ( 'NONE',  ( 0.000000000000000000, 0.8814952561688430555, -0.4721928772777346239 ) ) ;
#23935 = EDGE_LOOP ( 'NONE', ( #20658, #216973, #158050 ) ) ;
#23936 = CARTESIAN_POINT ( 'NONE',  ( 21.14999999999999858, -0.09999999999999939493, 0.000000000000000000 ) ) ;
#23937 = CYLINDRICAL_SURFACE ( 'NONE', #223559, 0.5000000000000004441 ) ;
#23938 = CARTESIAN_POINT ( 'NONE',  ( -21.05000000000000071, -1.835341550213257733, -145.5551512925629822 ) ) ;
#23939 = EDGE_LOOP ( 'NONE', ( #100458, #198427, #257947, #205974, #37849, #139673, #114242, #143402, #80822, #197168, #206052, #132137 ) ) ;
#23940 = AXIS2_PLACEMENT_3D ( 'NONE', #191479, #29836, #50629 ) ;
#23941 = LINE ( 'NONE', #83840, #195894 ) ;
#23942 = DIRECTION ( 'NONE',  ( 0.000000000000000000, -1.000000000000000000, -6.982962677686266711E-15 ) ) ;
#23943 = ORIENTED_EDGE ( 'NONE', *, *, #215986, .F. ) ;
#23944 = VECTOR ( 'NONE', #250151, 1000.000000000000000 ) ;
#23945 = DIRECTION ( 'NONE',  ( 0.000000000000000000, 0.000000000000000000, -1.000000000000000000 ) ) ;
#23946 = DIRECTION ( 'NONE',  ( 0.000000000000000000, -7.272083257015735086E-15, 1.000000000000000000 ) ) ;
#23947 = CARTESIAN_POINT ( 'NONE',  ( 21.05000000000000071, 67.70174932746996888, -211.7710791003628401 ) ) ;
#23949 = ORIENTED_EDGE ( 'NONE', *, *, #101799, .T. ) ;
#23948 = CARTESIAN_POINT ( 'NONE',  ( -20.65000000000000568, 68.75000000001161027, -60.27310748452437394 ) ) ;
#23950 = DIRECTION ( 'NONE',  ( 0.000000000000000000, -0.9654727137038715545, 0.2605042016806676242 ) ) ;
#23952 = EDGE_LOOP ( 'NONE', ( #30840, #169071, #169210, #3231 ) ) ;
#23951 = CARTESIAN_POINT ( 'NONE',  ( -0.8999999999999993561, -8.250000000000005329, 28.60000000000000142 ) ) ;
#23953 = DIRECTION ( 'NONE',  ( 8.673617379884087537E-15, 6.982962677686266711E-15, -1.000000000000000000 ) ) ;
#23954 = DIRECTION ( 'NONE',  ( 0.000000000000000000, 0.000000000000000000, -1.000000000000000000 ) ) ;
#23955 = ORIENTED_EDGE ( 'NONE', *, *, #15608, .F. ) ;
#23956 = LINE ( 'NONE', #142576, #2795 ) ;
#23957 = DIRECTION ( 'NONE',  ( 0.000000000000000000, -6.982962677686266711E-15, 1.000000000000000000 ) ) ;
#23959 = DIRECTION ( 'NONE',  ( 1.000000000000000000, 2.952720810173289112E-16, -0.000000000000000000 ) ) ;
#23958 = FACE_OUTER_BOUND ( 'NONE', #215628, .T. ) ;
#23961 = ADVANCED_FACE ( 'NONE', ( #22522 ), #137607, .T. ) ;
#23960 = PLANE ( 'NONE',  #112128 ) ;
#23962 = CARTESIAN_POINT ( 'NONE',  ( -16.87331047859651179, 22.97806745954242302, -230.9350634111226270 ) ) ;
#23963 = FACE_OUTER_BOUND ( 'NONE', #125830, .T. ) ;
#23964 = CARTESIAN_POINT ( 'NONE',  ( -18.50000000000000000, 19.02280865327213277, -233.3540837620168986 ) ) ;
#23965 = VECTOR ( 'NONE', #70528, 1000.000000000000000 ) ;
#23966 = CIRCLE ( 'NONE', #19675, 0.1000000000000033501 ) ;
#23967 = CARTESIAN_POINT ( 'NONE',  ( -20.94999999999999929, 69.15387683765952431, -132.7853812176745407 ) ) ;
#23968 = CIRCLE ( 'NONE', #11495, 0.09999999999999939493 ) ;
#23969 = EDGE_LOOP ( 'NONE', ( #124859, #138386, #194941, #97185 ) ) ;
#23970 = CARTESIAN_POINT ( 'NONE',  ( -20.65000000000000568, 45.89348038176515843, -239.2231437130149061 ) ) ;
#23971 = ORIENTED_EDGE ( 'NONE', *, *, #15570, .T. ) ;
#23972 = ORIENTED_EDGE ( 'NONE', *, *, #36727, .F. ) ;
#23973 = CARTESIAN_POINT ( 'NONE',  ( 20.85000000000000142, -11.64999999999999147, -33.50000000000000000 ) ) ;
#23974 = EDGE_CURVE ( 'NONE', #25027, #50700, #33547, .T. ) ;
#23975 = DIRECTION ( 'NONE',  ( 0.000000000000000000, -0.4721928772777346239, -0.8814952561688430555 ) ) ;
#23976 = ORIENTED_EDGE ( 'NONE', *, *, #81123, .F. ) ;
#23977 = ADVANCED_FACE ( 'NONE', ( #217139 ), #38536, .T. ) ;
#23978 = ORIENTED_EDGE ( 'NONE', *, *, #158782, .F. ) ;
#23979 = AXIS2_PLACEMENT_3D ( 'NONE', #216531, #2610, #82131 ) ;
#23980 = AXIS2_PLACEMENT_3D ( 'NONE', #220943, #63154, #22789 ) ;
#23981 = ORIENTED_EDGE ( 'NONE', *, *, #38248, .T. ) ;
#23982 = DIRECTION ( 'NONE',  ( 2.840903330521633255E-16, 0.8700118002898357128, -0.4930308989875171188 ) ) ;
#23983 = ORIENTED_EDGE ( 'NONE', *, *, #20313, .T. ) ;
#23984 = DIRECTION ( 'NONE',  ( -1.000000000000000000, 1.836970198721029934E-16, 1.282749433769087757E-30 ) ) ;
#23985 = CARTESIAN_POINT ( 'NONE',  ( 23.14999999999999858, 70.05000000001251692, -180.3288097895592159 ) ) ;
#23986 = AXIS2_PLACEMENT_3D ( 'NONE', #246989, #68372, #44953 ) ;
#23987 = FACE_OUTER_BOUND ( 'NONE', #200468, .T. ) ;
#23988 = CARTESIAN_POINT ( 'NONE',  ( 13.99999999999999822, 13.18880795147152618, -215.2702608532411830 ) ) ;
#23989 = CARTESIAN_POINT ( 'NONE',  ( -23.25000000000000000, 11.65000000001115588, -55.25000000000004974 ) ) ;
#23990 = EDGE_CURVE ( 'NONE', #157381, #77718, #66824, .T. ) ;
#23991 = DIRECTION ( 'NONE',  ( 1.000000000000000000, 0.000000000000000000, 0.000000000000000000 ) ) ;
#23992 = EDGE_CURVE ( 'NONE', #122268, #113211, #212584, .T. ) ;
#23993 = CARTESIAN_POINT ( 'NONE',  ( -23.15000000000000213, 76.00000000001205080, -123.6481074845242887 ) ) ;
#23995 = ORIENTED_EDGE ( 'NONE', *, *, #60824, .T. ) ;
#23994 = CARTESIAN_POINT ( 'NONE',  ( 21.00000000000000000, 30.46448808713892831, -235.1722212069449256 ) ) ;
#23997 = CARTESIAN_POINT ( 'NONE',  ( -22.39999999999999858, 64.35000000001238618, -169.9231074845244507 ) ) ;
#23996 = DIRECTION ( 'NONE',  ( 0.000000000000000000, -1.000000000000000000, -6.982962677686266711E-15 ) ) ;
#23998 = CARTESIAN_POINT ( 'NONE',  ( 21.05000000000000071, -11.39257802169451139, -97.42605042016811012 ) ) ;
#23999 = ORIENTED_EDGE ( 'NONE', *, *, #48663, .T. ) ;
#24001 = EDGE_CURVE ( 'NONE', #166612, #146108, #245889, .T. ) ;
#24000 = CARTESIAN_POINT ( 'NONE',  ( 18.59999999999999076, 1.835341550235567887, -179.0551512925629538 ) ) ;
#24002 = CARTESIAN_POINT ( 'NONE',  ( -23.49999999999994316, 87.60324567546805952, -34.17184040628037422 ) ) ;
#24003 = EDGE_LOOP ( 'NONE', ( #96415, #1704, #21909, #848 ) ) ;
#24005 = CARTESIAN_POINT ( 'NONE',  ( -16.93234230245721861, 66.00189262946491908, -115.6054172028581206 ) ) ;
#24004 = DIRECTION ( 'NONE',  ( 1.000000000000000000, 7.492892343619937423E-30, -1.073024830501117725E-15 ) ) ;
#24006 = CIRCLE ( 'NONE', #119876, 0.09999999999999986677 ) ;
#24007 = CARTESIAN_POINT ( 'NONE',  ( 18.59999999999999076, 30.68102565639535939, -234.7679863078877531 ) ) ;
#24008 = ORIENTED_EDGE ( 'NONE', *, *, #151227, .T. ) ;
#24009 = AXIS2_PLACEMENT_3D ( 'NONE', #248333, #8447, #185791 ) ;
#24010 = CARTESIAN_POINT ( 'NONE',  ( 21.04999999999999716, 6.300183336278585955, -66.94867256765833474 ) ) ;
#24011 = ADVANCED_FACE ( 'NONE', ( #105861 ), #21064, .T. ) ;
#24012 = CARTESIAN_POINT ( 'NONE',  ( -22.50875500270928598, -0.1008579137641475443, -21.75043287260211144 ) ) ;
#24013 = DIRECTION ( 'NONE',  ( 1.000000000000000000, 0.000000000000000000, 0.000000000000000000 ) ) ;
#24014 = EDGE_LOOP ( 'NONE', ( #29055, #86739, #158169, #6802 ) ) ;
#24015 = AXIS2_PLACEMENT_3D ( 'NONE', #193673, #215776, #35899 ) ;
#24016 = EDGE_CURVE ( 'NONE', #10221, #168616, #200100, .T. ) ;
#24017 = AXIS2_PLACEMENT_3D ( 'NONE', #37885, #79531, #117398 ) ;
#24018 = DIRECTION ( 'NONE',  ( 0.000000000000000000, 0.9371753822965315228, -0.3488585713686133682 ) ) ;
#24019 = CARTESIAN_POINT ( 'NONE',  ( 21.14999999999999858, 1.115600667400684642E-11, -134.0000000000000000 ) ) ;
#24020 = DIRECTION ( 'NONE',  ( -0.7071067811865487940, 0.7071067811865463515, -7.215498431451184074E-16 ) ) ;
#24021 = DIRECTION ( 'NONE',  ( 0.000000000000000000, 6.982962677686266711E-15, -1.000000000000000000 ) ) ;
#24022 = AXIS2_PLACEMENT_3D ( 'NONE', #170090, #252136, #12276 ) ;
#24024 = CARTESIAN_POINT ( 'NONE',  ( -21.14999999999999858, 11.38316329224760004, -198.5208684056144079 ) ) ;
#24023 = VECTOR ( 'NONE', #199033, 1000.000000000000000 ) ;
#24025 = CARTESIAN_POINT ( 'NONE',  ( 15.74999999999999645, 9.350000000011139178, -83.75000000000004263 ) ) ;
#24027 = VERTEX_POINT ( 'NONE', #242823 ) ;
#24026 = DIRECTION ( 'NONE',  ( 1.000000000000000000, 0.000000000000000000, 0.000000000000000000 ) ) ;
#24028 = CARTESIAN_POINT ( 'NONE',  ( 21.05000000000000071, 87.48912529308852015, -172.9231074845242802 ) ) ;
#24029 = VECTOR ( 'NONE', #239107, 1000.000000000000000 ) ;
#24030 = DIRECTION ( 'NONE',  ( 1.000000000000000000, 0.000000000000000000, 0.000000000000000000 ) ) ;
#24031 = DIRECTION ( 'NONE',  ( 0.000000000000000000, 0.000000000000000000, -1.000000000000000000 ) ) ;
#24032 = CARTESIAN_POINT ( 'NONE',  ( -18.59999999999999787, -1.637172712970379918, -11.58215336547201701 ) ) ;
#24033 = TOROIDAL_SURFACE ( 'NONE', #236398, 0.2000000000000000111, 0.1000000000000000056 ) ;
#24034 = CARTESIAN_POINT ( 'NONE',  ( 23.14999999999999503, 6.650000000011155876, -188.6499999999999488 ) ) ;
#24036 = ORIENTED_EDGE ( 'NONE', *, *, #71783, .F. ) ;
#24035 = CARTESIAN_POINT ( 'NONE',  ( 21.12802099929860944, 67.21944740978935329, -57.27491749959277456 ) ) ;
#24037 = FACE_OUTER_BOUND ( 'NONE', #29350, .T. ) ;
#24038 = CARTESIAN_POINT ( 'NONE',  ( -18.51024323315077424, 65.68895814178293335, -164.5026557862138645 ) ) ;
#24039 = CARTESIAN_POINT ( 'NONE',  ( -17.05016517656147101, 63.07979108456520123, -213.1495282149433308 ) ) ;
#24040 = CARTESIAN_POINT ( 'NONE',  ( 21.05000000000000071, 1.115650877919449575E-11, -163.4000000000000341 ) ) ;
#24041 = EDGE_LOOP ( 'NONE', ( #76796, #232849, #228378, #112131 ) ) ;
#24042 = CARTESIAN_POINT ( 'NONE',  ( -13.54036565897074240, 66.54845833862674453, -151.5692319856938184 ) ) ;
#24043 = CARTESIAN_POINT ( 'NONE',  ( -16.97683809663752186, 66.05000000001201954, -116.4254715027206828 ) ) ;
#24044 = CARTESIAN_POINT ( 'NONE',  ( 18.59999999999999432, -1.162701749926853712, -175.5999999999999659 ) ) ;
#24045 = CARTESIAN_POINT ( 'NONE',  ( 18.59999999999999432, 77.26178616857765746, -195.4366085209788935 ) ) ;
#24046 = CIRCLE ( 'NONE', #78174, 11.64999999999999325 ) ;
#24047 = VERTEX_POINT ( 'NONE', #185428 ) ;
#24048 = CIRCLE ( 'NONE', #169816, 0.1000000000000028644 ) ;
#24049 = VERTEX_POINT ( 'NONE', #6786 ) ;
#24050 = EDGE_CURVE ( 'NONE', #144670, #11990, #64201, .T. ) ;
#24051 = CIRCLE ( 'NONE', #94926, 11.65000000000000746 ) ;
#24052 = FACE_OUTER_BOUND ( 'NONE', #73482, .T. ) ;
#24055 = EDGE_CURVE ( 'NONE', #190429, #27504, #65471, .T. ) ;
#24054 = FACE_OUTER_BOUND ( 'NONE', #81944, .T. ) ;
#24053 = AXIS2_PLACEMENT_3D ( 'NONE', #197349, #216909, #38295 ) ;
#24056 = PRESENTATION_LAYER_ASSIGNMENT (  '', '', ( #136421 ) ) ;
#24057 = DIRECTION ( 'NONE',  ( -3.469446951953352918E-14, 0.4721928772776973204, 0.8814952561688629284 ) ) ;
#24058 = ORIENTED_EDGE ( 'NONE', *, *, #139310, .F. ) ;
#24059 = CIRCLE ( 'NONE', #98823, 0.09999999999999939493 ) ;
#24060 = EDGE_CURVE ( 'NONE', #255384, #222829, #87586, .T. ) ;
#24061 = ADVANCED_FACE ( 'NONE', ( #112323 ), #71306, .T. ) ;
#24062 = CARTESIAN_POINT ( 'NONE',  ( -18.50000000000000000, 1.340746217944851715, -23.22713749457881960 ) ) ;
#24063 = EDGE_CURVE ( 'NONE', #251832, #19019, #183534, .T. ) ;
#24064 = CARTESIAN_POINT ( 'NONE',  ( 21.09551895715215153, 12.98223157744519618, -210.6965877634172841 ) ) ;
#24065 = LINE ( 'NONE', #5734, #24583 ) ;
#24066 = FACE_OUTER_BOUND ( 'NONE', #182662, .T. ) ;
#24067 = EDGE_CURVE ( 'NONE', #86393, #50999, #188002, .T. ) ;
#24068 = VECTOR ( 'NONE', #97660, 1000.000000000000000 ) ;
#24072 = ADVANCED_FACE ( 'NONE', ( #191878 ), #151455, .T. ) ;
#24071 = ADVANCED_FACE ( 'NONE', ( #230994 ), #108459, .F. ) ;
#24070 = AXIS2_PLACEMENT_3D ( 'NONE', #230438, #51777, #12702 ) ;
#24069 = CARTESIAN_POINT ( 'NONE',  ( -18.59999999999999787, 30.27561093622783517, -235.5248193094124645 ) ) ;
#24073 = ORIENTED_EDGE ( 'NONE', *, *, #38507, .F. ) ;
#24075 = ORIENTED_EDGE ( 'NONE', *, *, #61602, .T. ) ;
#24074 = DIRECTION ( 'NONE',  ( 0.000000000000000000, 0.000000000000000000, 1.000000000000000000 ) ) ;
#24076 = ORIENTED_EDGE ( 'NONE', *, *, #103688, .F. ) ;
#24077 = DIRECTION ( 'NONE',  ( 0.000000000000000000, 0.000000000000000000, -1.000000000000000000 ) ) ;
#24078 = ORIENTED_EDGE ( 'NONE', *, *, #185552, .F. ) ;
#24079 = CARTESIAN_POINT ( 'NONE',  ( -18.40000000000000213, 64.25000000001159606, -56.87310748452440379 ) ) ;
#24080 = CARTESIAN_POINT ( 'NONE',  ( -21.07928932188134041, 6.328516656409859387, -100.4011048543454052 ) ) ;
#24081 = DIRECTION ( 'NONE',  ( -1.000000000000000000, 0.000000000000000000, 0.000000000000000000 ) ) ;
#24082 = ORIENTED_EDGE ( 'NONE', *, *, #122929, .T. ) ;
#24083 = CARTESIAN_POINT ( 'NONE',  ( 23.15000000000000213, -4.259020970815407203, -226.0869574510824123 ) ) ;
#24084 = CARTESIAN_POINT ( 'NONE',  ( 21.05000000000000071, 67.22371710471961137, -127.9644784893834100 ) ) ;
#24085 = ORIENTED_EDGE ( 'NONE', *, *, #144499, .F. ) ;
#24086 = CARTESIAN_POINT ( 'NONE',  ( -15.15564720441980207, 9.410708747058237122, -152.0692084058441367 ) ) ;
#24087 = AXIS2_PLACEMENT_3D ( 'NONE', #225323, #70156, #10159 ) ;
#24088 = EDGE_CURVE ( 'NONE', #203545, #109174, #111025, .T. ) ;
#24090 = ORIENTED_EDGE ( 'NONE', *, *, #142546, .T. ) ;
#24089 = DIRECTION ( 'NONE',  ( 0.000000000000000000, -0.4088369013363283289, 0.9126074666063768159 ) ) ;
#24091 = DIRECTION ( 'NONE',  ( 1.000000000000000000, 0.000000000000000000, 0.000000000000000000 ) ) ;
#24092 = CIRCLE ( 'NONE', #132393, 4.049999999999998934 ) ;
#24093 = DIRECTION ( 'NONE',  ( 1.000000000000000000, 0.000000000000000000, 0.000000000000000000 ) ) ;
#24094 = AXIS2_PLACEMENT_3D ( 'NONE', #49992, #9574, #73440 ) ;
#24095 = EDGE_CURVE ( 'NONE', #95308, #165343, #150420, .T. ) ;
#24096 = EDGE_CURVE ( 'NONE', #14875, #139556, #137709, .T. ) ;
#24097 = ORIENTED_EDGE ( 'NONE', *, *, #167061, .F. ) ;
#24098 = CIRCLE ( 'NONE', #128125, 0.1000000000000028644 ) ;
#24099 = CARTESIAN_POINT ( 'NONE',  ( 21.05000000000000071, 36.65892442174935439, -249.5511627012433848 ) ) ;
#24101 = EDGE_CURVE ( 'NONE', #26294, #5985, #69347, .T. ) ;
#24100 = DIRECTION ( 'NONE',  ( 0.000000000000000000, 1.000000000000000000, 6.982962677686266711E-15 ) ) ;
#24102 = CARTESIAN_POINT ( 'NONE',  ( 21.05000000000000426, 39.14562251533264003, -236.8628884932207654 ) ) ;
#24103 = VERTEX_POINT ( 'NONE', #130575 ) ;
#24104 = CYLINDRICAL_SURFACE ( 'NONE', #175728, 0.09999999999999939493 ) ;
#24105 = DIRECTION ( 'NONE',  ( 0.000000000000000000, 1.000000000000000000, -6.308085367188393199E-16 ) ) ;
#24106 = EDGE_CURVE ( 'NONE', #216121, #163280, #246080, .T. ) ;
#24107 = CIRCLE ( 'NONE', #94803, 0.09999999999999939493 ) ;
#24108 = VERTEX_POINT ( 'NONE', #73213 ) ;
#24109 = AXIS2_PLACEMENT_3D ( 'NONE', #79110, #158704, #162545 ) ;
#24110 = AXIS2_PLACEMENT_3D ( 'NONE', #119226, #115356, #158379 ) ;
#24111 = VECTOR ( 'NONE', #248281, 1000.000000000000000 ) ;
#24112 = ORIENTED_EDGE ( 'NONE', *, *, #86433, .F. ) ;
#24113 = EDGE_LOOP ( 'NONE', ( #123098, #97470, #232666 ) ) ;
#24114 = CYLINDRICAL_SURFACE ( 'NONE', #14416, 4.049999999999998046 ) ;
#24115 = CARTESIAN_POINT ( 'NONE',  ( -16.77431908686106965, 66.05419424549457119, -182.6872682668742129 ) ) ;
#24117 = VERTEX_POINT ( 'NONE', #211412 ) ;
#24116 = FACE_OUTER_BOUND ( 'NONE', #81539, .T. ) ;
#24118 = CARTESIAN_POINT ( 'NONE',  ( -23.25000000000000000, -1.851617760468904805, -45.10318971960366241 ) ) ;
#24119 = DIRECTION ( 'NONE',  ( 0.000000000000000000, 0.000000000000000000, 1.000000000000000000 ) ) ;
#24120 = CARTESIAN_POINT ( 'NONE',  ( -23.25000000000000000, 87.75000000001222134, -148.2731074845242176 ) ) ;
#24121 = FACE_OUTER_BOUND ( 'NONE', #232614, .T. ) ;
#24122 = VECTOR ( 'NONE', #207861, 1000.000000000000114 ) ;
#24123 = CARTESIAN_POINT ( 'NONE',  ( 21.05000000000005400, 65.15000000001120384, -3.123107484524795474 ) ) ;
#24125 = ORIENTED_EDGE ( 'NONE', *, *, #78888, .F. ) ;
#24124 = DIRECTION ( 'NONE',  ( -1.000000000000000000, -3.265361837132813093E-16, 0.000000000000000000 ) ) ;
#24127 = ORIENTED_EDGE ( 'NONE', *, *, #17139, .T. ) ;
#24126 = LINE ( 'NONE', #243145, #127639 ) ;
#24128 = DIRECTION ( 'NONE',  ( 0.000000000000000000, 0.000000000000000000, -1.000000000000000000 ) ) ;
#24129 = ORIENTED_EDGE ( 'NONE', *, *, #208678, .F. ) ;
#24130 = CARTESIAN_POINT ( 'NONE',  ( 20.95512820512820085, 65.37615131629998189, -90.82294546509999122 ) ) ;
#24131 = VECTOR ( 'NONE', #58990, 1000.000000000000000 ) ;
#24132 = CARTESIAN_POINT ( 'NONE',  ( 23.50000000000005684, 82.84256550613280012, -26.34830530078816935 ) ) ;
#24133 = CYLINDRICAL_SURFACE ( 'NONE', #98442, 0.1000000000000064587 ) ;
#24134 = CARTESIAN_POINT ( 'NONE',  ( -23.15000000000000213, 1.115600667400684642E-11, -134.0000000000000284 ) ) ;
#24135 = ORIENTED_EDGE ( 'NONE', *, *, #3089, .T. ) ;
#24136 = CARTESIAN_POINT ( 'NONE',  ( 21.05000000000000071, 10.38143492858865891, -207.4255871593388463 ) ) ;
#24138 = ORIENTED_EDGE ( 'NONE', *, *, #104441, .T. ) ;
#24137 = EDGE_CURVE ( 'NONE', #191970, #37506, #228420, .T. ) ;
#24139 = CARTESIAN_POINT ( 'NONE',  ( 23.25000000000000000, -13.88357498613435048, -191.9982587459959689 ) ) ;
#24140 = AXIS2_PLACEMENT_3D ( 'NONE', #89735, #169331, #134003 ) ;
#24141 = AXIS2_PLACEMENT_3D ( 'NONE', #204210, #62150, #43868 ) ;
#24142 = EDGE_CURVE ( 'NONE', #208786, #106358, #33735, .T. ) ;
#24143 = ORIENTED_EDGE ( 'NONE', *, *, #101636, .F. ) ;
#24144 = AXIS2_PLACEMENT_3D ( 'NONE', #201659, #199097, #81673 ) ;
#24145 = CARTESIAN_POINT ( 'NONE',  ( 21.15000000000005187, 64.25000000001119815, -6.023107484524794941 ) ) ;
#24146 = EDGE_CURVE ( 'NONE', #63679, #203031, #169755, .T. ) ;
#24147 = EDGE_LOOP ( 'NONE', ( #140484, #13528, #248617, #230484 ) ) ;
#24149 = ADVANCED_FACE ( 'NONE', ( #208844 ), #204360, .F. ) ;
#24148 = CARTESIAN_POINT ( 'NONE',  ( -23.15000000000000213, 76.00000000001213607, -136.5231074845243313 ) ) ;
#24150 = EDGE_LOOP ( 'NONE', ( #75488, #237638, #225570, #108314, #138746, #81317, #228112, #44932, #150568, #69400, #127830, #189165, #20633, #131309, #134520, #15252, #84051, #81321, #23282, #172223, #4019, #175651, #30293, #154807, #243769 ) ) ;
#24151 = CYLINDRICAL_SURFACE ( 'NONE', #113123, 0.09999999999999939493 ) ;
#24152 = EDGE_LOOP ( 'NONE', ( #187907, #214322, #241127, #61713 ) ) ;
#24153 = DIRECTION ( 'NONE',  ( -3.265361837132813093E-16, -1.000000000000000000, 7.445645354460596589E-46 ) ) ;
#24154 = CARTESIAN_POINT ( 'NONE',  ( 12.84233041328156766, 9.410538608540022665, -182.9326879971409028 ) ) ;
#24155 = VECTOR ( 'NONE', #244759, 1000.000000000000000 ) ;
#24156 = VERTEX_POINT ( 'NONE', #30218 ) ;
#24158 = CYLINDRICAL_SURFACE ( 'NONE', #32106, 2.000000000000001776 ) ;
#24157 = AXIS2_PLACEMENT_3D ( 'NONE', #180257, #103252, #78570 ) ;
#24160 = ORIENTED_EDGE ( 'NONE', *, *, #164698, .T. ) ;
#24159 = DIRECTION ( 'NONE',  ( 1.000000000000000000, 0.000000000000000000, 0.000000000000000000 ) ) ;
#24161 = CARTESIAN_POINT ( 'NONE',  ( -22.45354308602447801, 75.99999978014568569, -215.2735403749861689 ) ) ;
#24162 = ORIENTED_EDGE ( 'NONE', *, *, #13681, .T. ) ;
#24163 = EDGE_CURVE ( 'NONE', #234900, #49525, #249260, .T. ) ;
#24164 = AXIS2_PLACEMENT_3D ( 'NONE', #178512, #135485, #175946 ) ;
#24165 = EDGE_CURVE ( 'NONE', #86684, #213775, #71115, .T. ) ;
#24166 = ORIENTED_EDGE ( 'NONE', *, *, #209091, .T. ) ;
#24167 = CARTESIAN_POINT ( 'NONE',  ( -20.54999999999999716, 75.50266930301991408, -205.3568637872625686 ) ) ;
#24168 = CARTESIAN_POINT ( 'NONE',  ( 22.44352723754030166, 26.02350891930491272, -254.3055323313045903 ) ) ;
#24169 = CARTESIAN_POINT ( 'NONE',  ( -18.59999999999999787, 74.75000000001207923, -128.5231074845243029 ) ) ;
#24170 = FACE_OUTER_BOUND ( 'NONE', #187347, .T. ) ;
#24171 = DIRECTION ( 'NONE',  ( -0.000000000000000000, 1.000000000000000000, -0.000000000000000000 ) ) ;
#24172 = ORIENTED_EDGE ( 'NONE', *, *, #100580, .F. ) ;
#24173 = CARTESIAN_POINT ( 'NONE',  ( -16.94389599337535657, 66.00880201025582039, -182.6307522863228314 ) ) ;
#24174 = EDGE_CURVE ( 'NONE', #153695, #46950, #159168, .T. ) ;
#24175 = DIRECTION ( 'NONE',  ( 1.000000000000000000, 0.000000000000000000, 0.000000000000000000 ) ) ;
#24176 = CARTESIAN_POINT ( 'NONE',  ( -20.85000000000000142, 87.24382154048164750, -206.5725299160771726 ) ) ;
#24177 = AXIS2_PLACEMENT_3D ( 'NONE', #156436, #58558, #39035 ) ;
#24178 = ORIENTED_EDGE ( 'NONE', *, *, #81161, .F. ) ;
#24179 = EDGE_CURVE ( 'NONE', #113797, #235011, #125277, .T. ) ;
#24180 = FACE_OUTER_BOUND ( 'NONE', #175439, .T. ) ;
#24181 = ORIENTED_EDGE ( 'NONE', *, *, #70841, .T. ) ;
#24182 = CARTESIAN_POINT ( 'NONE',  ( -18.39999999999999858, -7.792936614629570435, -209.8606550935952271 ) ) ;
#24183 = VECTOR ( 'NONE', #141230, 1000.000000000000000 ) ;
#24184 = ORIENTED_EDGE ( 'NONE', *, *, #148106, .F. ) ;
#24185 = CARTESIAN_POINT ( 'NONE',  ( -21.14999999999999858, -0.09999999998884338825, -55.35042919245524473 ) ) ;
#24186 = CARTESIAN_POINT ( 'NONE',  ( 21.05000000000000071, 65.69992488703364586, -222.9708107233114163 ) ) ;
#24187 = EDGE_LOOP ( 'NONE', ( #56263, #230378, #133390, #83051 ) ) ;
#24189 = ORIENTED_EDGE ( 'NONE', *, *, #4053, .F. ) ;
#24188 = DIRECTION ( 'NONE',  ( -1.000000000000000000, -0.000000000000000000, -0.000000000000000000 ) ) ;
#24190 = CARTESIAN_POINT ( 'NONE',  ( -18.39999999999999858, 64.52683809664941350, -93.72327823605837693 ) ) ;
#24191 = ORIENTED_EDGE ( 'NONE', *, *, #28495, .T. ) ;
#24192 = AXIS2_PLACEMENT_3D ( 'NONE', #193388, #190836, #214222 ) ;
#24193 = EDGE_CURVE ( 'NONE', #241192, #14385, #91934, .T. ) ;
#24194 = FACE_OUTER_BOUND ( 'NONE', #49728, .T. ) ;
#24195 = DIRECTION ( 'NONE',  ( -1.000000000000000000, -1.836970198721029934E-16, 0.000000000000000000 ) ) ;
#24196 = EDGE_CURVE ( 'NONE', #214744, #161687, #187833, .T. ) ;
#24197 = ORIENTED_EDGE ( 'NONE', *, *, #43363, .T. ) ;
#24198 = VERTEX_POINT ( 'NONE', #254361 ) ;
#24199 = CARTESIAN_POINT ( 'NONE',  ( 20.94999999999999574, 4.252251777740764460, -211.8999245327126744 ) ) ;
#24200 = CARTESIAN_POINT ( 'NONE',  ( 23.15000000000000213, -9.500000000000001776, -9.893969122652443104 ) ) ;
#24201 = DIRECTION ( 'NONE',  ( -2.952720810173289112E-16, -1.000000000000000000, -6.982962677686266711E-15 ) ) ;
#24202 = ADVANCED_FACE ( 'NONE', ( #173623 ), #216539, .T. ) ;
#24203 = AXIS2_PLACEMENT_3D ( 'NONE', #64219, #246698, #225826 ) ;
#24204 = VECTOR ( 'NONE', #81302, 1000.000000000000000 ) ;
#24206 = ORIENTED_EDGE ( 'NONE', *, *, #213297, .T. ) ;
#24205 = AXIS2_PLACEMENT_3D ( 'NONE', #248574, #69964, #205580 ) ;
#24207 = ORIENTED_EDGE ( 'NONE', *, *, #161533, .F. ) ;
#24209 = CARTESIAN_POINT ( 'NONE',  ( 18.59999999999999076, 53.33306769324366314, -234.7945388949160872 ) ) ;
#24208 = VECTOR ( 'NONE', #64109, 1000.000000000000000 ) ;
#24210 = APPLICATION_CONTEXT ( 'automotive_design' ) ;
#24211 = EDGE_CURVE ( 'NONE', #58156, #111921, #129559, .T. ) ;
#24213 = ORIENTED_EDGE ( 'NONE', *, *, #156055, .F. ) ;
#24212 = DIRECTION ( 'NONE',  ( 1.000000000000000000, -0.000000000000000000, -0.000000000000000000 ) ) ;
#24214 = PLANE ( 'NONE',  #15972 ) ;
#24215 = CARTESIAN_POINT ( 'NONE',  ( -22.43310005002225438, 75.99436305787085644, -81.17276961165872251 ) ) ;
#24216 = DIRECTION ( 'NONE',  ( 0.000000000000000000, -6.517943393102682774E-15, 1.000000000000000000 ) ) ;
#24217 = EDGE_CURVE ( 'NONE', #221299, #156630, #94014, .T. ) ;
#24219 = DIRECTION ( 'NONE',  ( 1.000000000000000000, 0.000000000000000000, 0.000000000000000000 ) ) ;
#24218 = DIRECTION ( 'NONE',  ( 1.000000000000000000, 0.000000000000000000, 0.000000000000000000 ) ) ;
#24220 = CARTESIAN_POINT ( 'NONE',  ( 21.05000000000000071, 10.48459288120601229, -107.9567135705844265 ) ) ;
#24221 = CARTESIAN_POINT ( 'NONE',  ( 18.79999999999999716, 7.986648289447971116, 1.311673547813416718 ) ) ;
#24222 = AXIS2_PLACEMENT_3D ( 'NONE', #214241, #238940, #55124 ) ;
#24223 = CARTESIAN_POINT ( 'NONE',  ( -21.05000000000000071, 68.17695920783671681, -227.9262201573640141 ) ) ;
#24224 = DIRECTION ( 'NONE',  ( 0.000000000000000000, -8.881784197001832136E-16, -1.000000000000000000 ) ) ;
#24225 = AXIS2_PLACEMENT_3D ( 'NONE', #1722, #39619, #20038 ) ;
#24226 = ORIENTED_EDGE ( 'NONE', *, *, #157505, .F. ) ;
#24227 = AXIS2_PLACEMENT_3D ( 'NONE', #155103, #16857, #57223 ) ;
#24228 = AXIS2_PLACEMENT_3D ( 'NONE', #233876, #209168, #30561 ) ;
#24229 = AXIS2_PLACEMENT_3D ( 'NONE', #88566, #209827, #149864 ) ;
#24230 = ORIENTED_EDGE ( 'NONE', *, *, #51420, .F. ) ;
#24231 = EDGE_CURVE ( 'NONE', #30937, #17857, #117453, .T. ) ;
#24232 = CYLINDRICAL_SURFACE ( 'NONE', #231162, 0.09999999999999954758 ) ;
#24233 =( BOUNDED_SURFACE ( )  B_SPLINE_SURFACE ( 3, 2, ( 
 ( #77237, #173840, #156825 ),
 ( #55088, #175121, #135922 ),
 ( #36882, #118962, #236322 ),
 ( #57670, #92956, #137223 ),
 ( #117661, #197192, #18569 ),
 ( #98061, #177671, #172557 ) ),
 .UNSPECIFIED., .F., .F., .F. ) 
 B_SPLINE_SURFACE_WITH_KNOTS ( ( 4, 2, 4 ),
 ( 3, 3 ),
 ( 0.0001342700090130014186, 0.0002909192928057377698, 0.0004475685765984741210 ),
 ( 0.000000000000000000, 1.000000000000000000 ),
 .UNSPECIFIED. ) 
 GEOMETRIC_REPRESENTATION_ITEM ( )  RATIONAL_B_SPLINE_SURFACE ( (
 ( 1.000000000000000000, 0.7250110520819876836, 1.000000000000000000),
 ( 1.000000000000000000, 0.7257599279120965363, 1.000000000000000000),
 ( 1.000000000000000000, 0.7137594617301571409, 1.000000000000000000),
 ( 1.000000000000000000, 0.6959270178792876793, 1.000000000000000000),
 ( 1.000000000000000000, 0.6919879549351505288, 1.000000000000000000),
 ( 1.000000000000000000, 0.7071067811865494601, 1.000000000000000000) ) ) 
 REPRESENTATION_ITEM ( '' )  SURFACE ( )  );
#24234 = EDGE_LOOP ( 'NONE', ( #39587, #32908, #79339, #126250 ) ) ;
#24235 = CIRCLE ( 'NONE', #36725, 0.1000000000000028644 ) ;
#24236 = DIRECTION ( 'NONE',  ( 0.000000000000000000, 0.9908441862701791170, -0.1350103645450472789 ) ) ;
#24237 = ORIENTED_EDGE ( 'NONE', *, *, #248993, .F. ) ;
#24238 = DIRECTION ( 'NONE',  ( 0.000000000000000000, 0.2128009952263605065, -0.9770955615653315052 ) ) ;
#24239 = ORIENTED_EDGE ( 'NONE', *, *, #115787, .T. ) ;
#24240 = B_SPLINE_CURVE_WITH_KNOTS ( 'NONE', 3,
 ( #257220, #251688, #32694, #36529, #91348, #213848 ),
 .UNSPECIFIED., .F., .F.,
 ( 4, 2, 4 ),
 ( 0.000000000000000000, 0.0001496588209255839900, 0.0002993176418511679800 ),
 .UNSPECIFIED. ) ;
#24241 = CYLINDRICAL_SURFACE ( 'NONE', #100597, 0.09999999999998898659 ) ;
#24242 = EDGE_LOOP ( 'NONE', ( #240204, #192585, #189296, #207550 ) ) ;
#24243 = AXIS2_PLACEMENT_3D ( 'NONE', #36360, #254082, #96285 ) ;
#24244 = AXIS2_PLACEMENT_3D ( 'NONE', #207791, #227321, #52527 ) ;
#24245 = ORIENTED_EDGE ( 'NONE', *, *, #36135, .F. ) ;
#24246 = CARTESIAN_POINT ( 'NONE',  ( -21.14999999999999858, -2.598867842139046314, -189.5410128746472083 ) ) ;
#24247 = CYLINDRICAL_SURFACE ( 'NONE', #201012, 0.1000000000000028644 ) ;
#24249 = VERTEX_POINT ( 'NONE', #196967 ) ;
#24248 = DIRECTION ( 'NONE',  ( 0.000000000000000000, 0.000000000000000000, -1.000000000000000000 ) ) ;
#24250 = CARTESIAN_POINT ( 'NONE',  ( -23.15000000000000213, 4.250000000011156409, -79.35000000000005116 ) ) ;
#24252 = ORIENTED_EDGE ( 'NONE', *, *, #169881, .F. ) ;
#24251 = CARTESIAN_POINT ( 'NONE',  ( 18.69999999999999929, 1.212568896937007645, -8.000000000000000000 ) ) ;
#24253 = CARTESIAN_POINT ( 'NONE',  ( 19.90621891164687440, 11.75000000001116263, -125.3284452778770373 ) ) ;
#24254 = VERTEX_POINT ( 'NONE', #54 ) ;
#24255 = CARTESIAN_POINT ( 'NONE',  ( -16.89208623190940273, 9.951577948986638944, -121.3552722032183055 ) ) ;
#24257 = ORIENTED_EDGE ( 'NONE', *, *, #245413, .T. ) ;
#24256 = CARTESIAN_POINT ( 'NONE',  ( -20.94999999999999929, 43.35377423437995503, -245.1717807829448930 ) ) ;
#24258 = AXIS2_PLACEMENT_3D ( 'NONE', #257683, #240762, #141646 ) ;
#24259 = CARTESIAN_POINT ( 'NONE',  ( 23.14999999999999503, 64.35000000001222986, -148.6731074845244507 ) ) ;
#24260 = CARTESIAN_POINT ( 'NONE',  ( -13.77083647240106679, 27.90214353194706476, -234.1315669640961801 ) ) ;
#24261 = CARTESIAN_POINT ( 'NONE',  ( 20.85000000000000142, 11.75000000001115907, -60.21613433702191287 ) ) ;
#24262 = VERTEX_POINT ( 'NONE', #14522 ) ;
#24264 = CARTESIAN_POINT ( 'NONE',  ( -21.09610168723073187, 69.62104428478792784, -203.5566969914158904 ) ) ;
#24263 = DIRECTION ( 'NONE',  ( 0.7071067811865489050, -0.6824534298470359417, 0.1850873201762213704 ) ) ;
#24265 = DIRECTION ( 'NONE',  ( 1.000000000000000000, 0.000000000000000000, 0.000000000000000000 ) ) ;
#24266 = AXIS2_PLACEMENT_3D ( 'NONE', #138487, #116399, #218028 ) ;
#24267 = FACE_OUTER_BOUND ( 'NONE', #203365, .T. ) ;
#24268 = FACE_OUTER_BOUND ( 'NONE', #178149, .T. ) ;
#24269 = DIRECTION ( 'NONE',  ( -0.000000000000000000, -0.000000000000000000, 1.000000000000000000 ) ) ;
#24270 = ORIENTED_EDGE ( 'NONE', *, *, #250133, .T. ) ;
#24271 = VERTEX_POINT ( 'NONE', #114876 ) ;
#24273 = ORIENTED_EDGE ( 'NONE', *, *, #56675, .F. ) ;
#24272 = VECTOR ( 'NONE', #189395, 1000.000000000000000 ) ;
#24274 = LINE ( 'NONE', #184604, #72301 ) ;
#24275 = VERTEX_POINT ( 'NONE', #134413 ) ;
#24276 = CARTESIAN_POINT ( 'NONE',  ( -23.25000000000000000, 69.20602499728043711, -247.8456586332460176 ) ) ;
#24277 = ORIENTED_EDGE ( 'NONE', *, *, #204205, .F. ) ;
#24278 = FACE_OUTER_BOUND ( 'NONE', #113620, .T. ) ;
#24279 = EDGE_CURVE ( 'NONE', #203821, #226489, #74512, .T. ) ;
#24280 = CARTESIAN_POINT ( 'NONE',  ( -16.87036670365548474, 14.22508806334146492, -219.3732768077300932 ) ) ;
#24281 = VECTOR ( 'NONE', #31647, 1000.000000000000000 ) ;
#24282 = EDGE_CURVE ( 'NONE', #170827, #189189, #21246, .T. ) ;
#24283 = EDGE_CURVE ( 'NONE', #107106, #245608, #37991, .T. ) ;
#24284 = ORIENTED_EDGE ( 'NONE', *, *, #191991, .T. ) ;
#24285 = AXIS2_PLACEMENT_3D ( 'NONE', #41173, #140218, #101060 ) ;
#24286 = DIRECTION ( 'NONE',  ( 1.000000000000000000, 0.000000000000000000, 0.000000000000000000 ) ) ;
#24287 = SURFACE_SIDE_STYLE ('',( #124657 ) ) ;
#24288 = AXIS2_PLACEMENT_3D ( 'NONE', #37677, #196718, #32560 ) ;
#24289 = ORIENTED_EDGE ( 'NONE', *, *, #210086, .F. ) ;
#24290 = ORIENTED_EDGE ( 'NONE', *, *, #107805, .T. ) ;
#24291 = VERTEX_POINT ( 'NONE', #58724 ) ;
#24292 = DIRECTION ( 'NONE',  ( -0.7071067811865389130, 8.659560562355038861E-17, -0.7071067811865561215 ) ) ;
#24293 =( NAMED_UNIT ( * ) PLANE_ANGLE_UNIT ( ) SI_UNIT ( $, .RADIAN. ) );
#24294 = FACE_OUTER_BOUND ( 'NONE', #234149, .T. ) ;
#24295 = CARTESIAN_POINT ( 'NONE',  ( 15.73863059295127442, 26.51187484352280421, -233.5070971077067554 ) ) ;
#24296 = CYLINDRICAL_SURFACE ( 'NONE', #27539, 0.1000000000000028644 ) ;
#24297 = DIRECTION ( 'NONE',  ( -0.7071067811865487940, -0.7071067811865463515, -4.937700262164522799E-15 ) ) ;
#24298 = EDGE_CURVE ( 'NONE', #153949, #57412, #158606, .T. ) ;
#24300 = DIRECTION ( 'NONE',  ( 1.000000000000000000, 0.000000000000000000, -0.000000000000000000 ) ) ;
#24299 = CARTESIAN_POINT ( 'NONE',  ( 20.85000000000000142, 80.78317333349157536, -192.9003134612048882 ) ) ;
#24301 = CARTESIAN_POINT ( 'NONE',  ( -16.87036670365549895, 10.08494996325527460, -12.55000000000000249 ) ) ;
#24303 = ORIENTED_EDGE ( 'NONE', *, *, #22438, .F. ) ;
#24302 = DIRECTION ( 'NONE',  ( 0.000000000000000000, 0.8814952561688430555, -0.4721928772777346239 ) ) ;
#24305 = CARTESIAN_POINT ( 'NONE',  ( 21.30000000000002558, 76.00000000001264766, -199.4731074845243484 ) ) ;
#24304 = CARTESIAN_POINT ( 'NONE',  ( -20.94684162641900116, 11.75000000001115374, -40.34164400167171038 ) ) ;
#24306 = CARTESIAN_POINT ( 'NONE',  ( -23.25000000000000000, 11.75000000001115552, -167.4999999999999716 ) ) ;
#24307 = ORIENTED_EDGE ( 'NONE', *, *, #206006, .T. ) ;
#24308 = FACE_OUTER_BOUND ( 'NONE', #71397, .T. ) ;
#24309 = TOROIDAL_SURFACE ( 'NONE', #111769, 0.2000000000000000111, 0.1000000000000000056 ) ;
#24310 = CYLINDRICAL_SURFACE ( 'NONE', #139412, 0.1000000000000035305 ) ;
#24311 = DIRECTION ( 'NONE',  ( 0.000000000000000000, 0.000000000000000000, -1.000000000000000000 ) ) ;
#24312 = ORIENTED_EDGE ( 'NONE', *, *, #118295, .F. ) ;
#24313 = CARTESIAN_POINT ( 'NONE',  ( 21.08134388332231879, 69.66531941949473605, -203.5989264020314238 ) ) ;
#24314 = CARTESIAN_POINT ( 'NONE',  ( 18.59999999999998721, 19.85039924723355398, -2.280303057801358335 ) ) ;
#24315 = ORIENTED_EDGE ( 'NONE', *, *, #49065, .F. ) ;
#24316 = EDGE_LOOP ( 'NONE', ( #9412, #192261, #31789, #5166 ) ) ;
#24317 = CARTESIAN_POINT ( 'NONE',  ( 23.14999999999999503, 6.650000000011155876, -188.7499999999999716 ) ) ;
#24319 = ORIENTED_EDGE ( 'NONE', *, *, #87929, .T. ) ;
#24318 = ADVANCED_FACE ( 'NONE', ( #256903 ), #46154, .F. ) ;
#24320 = CARTESIAN_POINT ( 'NONE',  ( 21.07016717456946253, 6.320940838111409832, -67.00000000000004263 ) ) ;
#24321 = EDGE_CURVE ( 'NONE', #102057, #156378, #95602, .T. ) ;
#24322 = CARTESIAN_POINT ( 'NONE',  ( 20.94999999999999574, 77.16270174994961906, -61.52310748452431710 ) ) ;
#24323 = CARTESIAN_POINT ( 'NONE',  ( -20.64999999999999858, 68.85000000001186038, -90.77310748452435973 ) ) ;
#24324 = CARTESIAN_POINT ( 'NONE',  ( -22.50000000000000000, 64.18196446391819165, -247.0985338183330668 ) ) ;
#24325 = ORIENTED_EDGE ( 'NONE', *, *, #135882, .F. ) ;
#24326 = CARTESIAN_POINT ( 'NONE',  ( -16.87036670365549895, 12.42497885867826390, -211.1079079717509046 ) ) ;
#24327 = LINE ( 'NONE', #183389, #191695 ) ;
#24328 = EDGE_CURVE ( 'NONE', #244346, #84318, #77024, .T. ) ;
#24329 = CARTESIAN_POINT ( 'NONE',  ( 18.50000000000281730, 10.44006789215406705, -192.2671177488813896 ) ) ;
#24330 = CIRCLE ( 'NONE', #203379, 11.75000000000000355 ) ;
#24332 = CIRCLE ( 'NONE', #115306, 0.09999999999999939493 ) ;
#24331 = CARTESIAN_POINT ( 'NONE',  ( -20.64999999999999858, 7.150000000000000355, -21.15000000000000213 ) ) ;
#24333 = CIRCLE ( 'NONE', #253254, 0.09999999999999489853 ) ;
#24334 = EDGE_LOOP ( 'NONE', ( #75925, #218159, #81647, #83394 ) ) ;
#24335 =( BOUNDED_CURVE ( )  B_SPLINE_CURVE ( 3, ( #6799, #165901, #27692, #186742 ),
 .UNSPECIFIED., .F., .F. ) 
 B_SPLINE_CURVE_WITH_KNOTS ( ( 4, 4 ),
 ( 4.937700262164173333E-15, 1.570796326794912323 ),
 .UNSPECIFIED. ) 
 CURVE ( )  GEOMETRIC_REPRESENTATION_ITEM ( )  RATIONAL_B_SPLINE_CURVE ( ( 1.000000000000000000, 0.8047378541243623840, 0.8047378541243623840, 1.000000000000000000 ) ) 
 REPRESENTATION_ITEM ( '' )  );
#24337 = ORIENTED_EDGE ( 'NONE', *, *, #217303, .F. ) ;
#24336 = FACE_BOUND ( 'NONE', #30311, .T. ) ;
#24338 = LINE ( 'NONE', #85532, #110035 ) ;
#24339 = CARTESIAN_POINT ( 'NONE',  ( 18.45036689428365051, 78.22617660076507207, -231.5710132021329173 ) ) ;
#24340 = PLANE ( 'NONE',  #179444 ) ;
#24341 = DIRECTION ( 'NONE',  ( 1.000000000000000000, -3.265361837132813093E-16, -2.280189983783949500E-30 ) ) ;
#24342 = DIRECTION ( 'NONE',  ( 1.000000000000000000, 0.000000000000000000, -0.000000000000000000 ) ) ;
#24343 = CARTESIAN_POINT ( 'NONE',  ( 20.02499999999999858, 9.750000000011153745, -155.1500000000000057 ) ) ;
#24344 = ORIENTED_EDGE ( 'NONE', *, *, #145629, .F. ) ;
#24345 = EDGE_CURVE ( 'NONE', #92979, #243059, #83710, .T. ) ;
#24346 = DIRECTION ( 'NONE',  ( -0.000000000000000000, 1.000000000000000000, 6.982962677686266711E-15 ) ) ;
#24347 = DIRECTION ( 'NONE',  ( 0.000000000000000000, 1.897661533703519897E-16, -1.000000000000000000 ) ) ;
#24348 = AXIS2_PLACEMENT_3D ( 'NONE', #256121, #59226, #39744 ) ;
#24349 = FACE_OUTER_BOUND ( 'NONE', #123937, .T. ) ;
#24350 = CARTESIAN_POINT ( 'NONE',  ( 22.47007471830799474, 7.720710651937603863, -134.0000000000000000 ) ) ;
#24351 = AXIS2_PLACEMENT_3D ( 'NONE', #154014, #134372, #17034 ) ;
#24352 = DIRECTION ( 'NONE',  ( 1.000000000000000000, 0.000000000000000000, 0.000000000000000000 ) ) ;
#24353 = CARTESIAN_POINT ( 'NONE',  ( -17.29158576265543346, 10.36474766602906961, -189.5827582447921600 ) ) ;
#24354 = AXIS2_PLACEMENT_3D ( 'NONE', #166655, #246159, #226572 ) ;
#24355 = VERTEX_POINT ( 'NONE', #144694 ) ;
#24356 = EDGE_LOOP ( 'NONE', ( #41788, #67222, #19848, #182333 ) ) ;
#24357 = LINE ( 'NONE', #119606, #71040 ) ;
#24358 = CARTESIAN_POINT ( 'NONE',  ( -21.05000000000000071, 1.835341550224411922, -11.55515129256298046 ) ) ;
#24359 = EDGE_CURVE ( 'NONE', #151535, #148073, #161735, .T. ) ;
#24360 = CARTESIAN_POINT ( 'NONE',  ( 22.49806830649814060, 11.64988965483908068, 0.07746431632550301871 ) ) ;
#24361 = CARTESIAN_POINT ( 'NONE',  ( -20.64999999999999858, 1.115600667400684642E-11, -167.4999999999999716 ) ) ;
#24362 = ORIENTED_EDGE ( 'NONE', *, *, #88738, .F. ) ;
#24363 = CARTESIAN_POINT ( 'NONE',  ( 23.24999999999999289, 6.550000000011156231, -188.8499999999999659 ) ) ;
#24364 = ADVANCED_FACE ( 'NONE', ( #105543 ), #224237, .F. ) ;
#24365 = ADVANCED_FACE ( 'NONE', ( #180002 ), #239972, .T. ) ;
#24366 = DIRECTION ( 'NONE',  ( -0.000000000000000000, 0.4721928772777345684, 0.8814952561688429444 ) ) ;
#24367 = CYLINDRICAL_SURFACE ( 'NONE', #38266, 0.09999999999998898659 ) ;
#24368 = DIRECTION ( 'NONE',  ( 0.000000000000000000, 0.1350103645451876666, 0.9908441862701600211 ) ) ;
#24369 = AXIS2_PLACEMENT_3D ( 'NONE', #23024, #45124, #199066 ) ;
#24370 = AXIS2_PLACEMENT_3D ( 'NONE', #152509, #251570, #110775 ) ;
#24371 = ADVANCED_FACE ( 'NONE', ( #5165 ), #102998, .F. ) ;
#24372 = EDGE_CURVE ( 'NONE', #88769, #40263, #355, .T. ) ;
#24373 = EDGE_LOOP ( 'NONE', ( #176205, #221795, #112777, #28502, #214268, #62990, #87756, #85945, #75121 ) ) ;
#24374 = DIRECTION ( 'NONE',  ( -1.000000000000000000, 0.000000000000000000, 0.000000000000000000 ) ) ;
#24375 = VERTEX_POINT ( 'NONE', #45616 ) ;
#24376 = CARTESIAN_POINT ( 'NONE',  ( -23.25000000000000000, 6.982009704867601307, -171.1961521182563217 ) ) ;
#24377 = CARTESIAN_POINT ( 'NONE',  ( 23.14999999999999503, 64.25000000001202238, -114.7731074845243882 ) ) ;
#24378 = CIRCLE ( 'NONE', #107738, 12.77499999999999503 ) ;
#24379 = EDGE_CURVE ( 'NONE', #103201, #218583, #154520, .T. ) ;
#24380 = CARTESIAN_POINT ( 'NONE',  ( -22.50000000000000000, 1.115600667400684642E-11, -67.00000000000004263 ) ) ;
#24381 = DIRECTION ( 'NONE',  ( -1.000000000000000000, -3.265361837132813093E-16, 0.000000000000000000 ) ) ;
#24382 = CARTESIAN_POINT ( 'NONE',  ( -18.50000000000000355, -9.399999999999973710, -7.297259759663287326 ) ) ;
#24383 = DIRECTION ( 'NONE',  ( 0.000000000000000000, -0.1568667991644355497, -0.9876197685951332295 ) ) ;
#24384 = CYLINDRICAL_SURFACE ( 'NONE', #141454, 2.000000000000001776 ) ;
#24385 = EDGE_CURVE ( 'NONE', #167246, #236853, #204666, .T. ) ;
#24386 = FACE_OUTER_BOUND ( 'NONE', #220934, .T. ) ;
#24387 = DIRECTION ( 'NONE',  ( 1.000000000000000000, -0.000000000000000000, -0.000000000000000000 ) ) ;
#24388 = DIRECTION ( 'NONE',  ( 0.7071067811865487940, 0.7071067811865462405, -7.215498431451186046E-16 ) ) ;
#24390 = MANIFOLD_SOLID_BREP ( 'Stock-MAS-200-1', #57530 ) ;
#24389 = AXIS2_PLACEMENT_3D ( 'NONE', #130740, #171201, #125598 ) ;
#24391 = EDGE_CURVE ( 'NONE', #234881, #232370, #121394, .T. ) ;
#24392 = EDGE_CURVE ( 'NONE', #176500, #253862, #254606, .T. ) ;
#24393 = VECTOR ( 'NONE', #35684, 1000.000000000000000 ) ;
#24394 = FACE_OUTER_BOUND ( 'NONE', #174250, .T. ) ;
#24395 = CIRCLE ( 'NONE', #195276, 11.70000000000001528 ) ;
#24396 = ORIENTED_EDGE ( 'NONE', *, *, #11514, .T. ) ;
#24397 = CARTESIAN_POINT ( 'NONE',  ( 18.39999999999999858, 85.50000000001209344, -129.9229180933022576 ) ) ;
#24399 = EDGE_CURVE ( 'NONE', #50227, #122858, #145984, .T. ) ;
#24398 = DIRECTION ( 'NONE',  ( 0.000000000000000000, 0.000000000000000000, 1.000000000000000000 ) ) ;
#24400 = ORIENTED_EDGE ( 'NONE', *, *, #231825, .F. ) ;
#24401 = CARTESIAN_POINT ( 'NONE',  ( -22.50000000000000000, 0.1000000000111554016, -55.35042919245524473 ) ) ;
#24402 = DIRECTION ( 'NONE',  ( 1.000000000000000000, 0.000000000000000000, 0.000000000000000000 ) ) ;
#24403 = EDGE_CURVE ( 'NONE', #66389, #116798, #133812, .T. ) ;
#24404 = VECTOR ( 'NONE', #108374, 1000.000000000000114 ) ;
#24405 = EDGE_CURVE ( 'NONE', #147767, #32779, #242140, .T. ) ;
#24406 = DIRECTION ( 'NONE',  ( -0.000000000000000000, 0.000000000000000000, -1.000000000000000000 ) ) ;
#24407 = ORIENTED_EDGE ( 'NONE', *, *, #103123, .T. ) ;
#24408 = DIRECTION ( 'NONE',  ( -0.000000000000000000, 0.1298341882520009927, 0.9915357197604854900 ) ) ;
#24409 = FACE_OUTER_BOUND ( 'NONE', #154435, .T. ) ;
#24410 = EDGE_CURVE ( 'NONE', #76299, #171611, #112982, .T. ) ;
#24411 = VECTOR ( 'NONE', #9302, 1000.000000000000000 ) ;
#24412 = ORIENTED_EDGE ( 'NONE', *, *, #10190, .F. ) ;
#24413 = CIRCLE ( 'NONE', #186728, 0.1000000000000028644 ) ;
#24414 = AXIS2_PLACEMENT_3D ( 'NONE', #179916, #114788, #217716 ) ;
#24415 = CIRCLE ( 'NONE', #57703, 0.09999999999999892308 ) ;
#24417 = ORIENTED_EDGE ( 'NONE', *, *, #82479, .F. ) ;
#24416 = AXIS2_PLACEMENT_3D ( 'NONE', #58819, #197060, #234926 ) ;
#24418 = CARTESIAN_POINT ( 'NONE',  ( -20.54999999999999716, 71.65000000001155911, -57.17310748452435121 ) ) ;
#24419 = ORIENTED_EDGE ( 'NONE', *, *, #206019, .F. ) ;
#24420 = EDGE_CURVE ( 'NONE', #75871, #104039, #246261, .T. ) ;
#24421 = AXIS2_PLACEMENT_3D ( 'NONE', #84111, #125850, #140269 ) ;
#24422 = CYLINDRICAL_SURFACE ( 'NONE', #112890, 0.09999999999999939493 ) ;
#24423 = FACE_OUTER_BOUND ( 'NONE', #39579, .T. ) ;
#24424 = DIRECTION ( 'NONE',  ( 0.000000000000000000, 0.000000000000000000, -1.000000000000000000 ) ) ;
#24426 = CARTESIAN_POINT ( 'NONE',  ( 18.59999999999999787, -1.736705739456431807, -179.0174225876237415 ) ) ;
#24425 = UNCERTAINTY_MEASURE_WITH_UNIT (LENGTH_MEASURE( 1.000000000000000082E-05 ), #216032, 'distance_accuracy_value', 'NONE');
#24427 = LINE ( 'NONE', #205584, #129347 ) ;
#24428 = CARTESIAN_POINT ( 'NONE',  ( -16.96982749440685012, 66.05000000001230376, -156.8983290757135194 ) ) ;
#24429 = CYLINDRICAL_SURFACE ( 'NONE', #208479, 0.09999999999999939493 ) ;
#24430 = DIRECTION ( 'NONE',  ( 0.000000000000000000, 6.982962677686266711E-15, -1.000000000000000000 ) ) ;
#24431 = DIRECTION ( 'NONE',  ( -1.000000000000000000, -0.000000000000000000, -0.000000000000000000 ) ) ;
#24433 = ORIENTED_EDGE ( 'NONE', *, *, #31493, .F. ) ;
#24432 = CARTESIAN_POINT ( 'NONE',  ( 18.43466021071410310, 86.89521045040650904, -199.6218833434545843 ) ) ;
#24434 = ORIENTED_EDGE ( 'NONE', *, *, #84952, .F. ) ;
#24436 = DIRECTION ( 'NONE',  ( 0.000000000000000000, 1.000000000000000000, 0.000000000000000000 ) ) ;
#24435 = CARTESIAN_POINT ( 'NONE',  ( 23.15000000000000213, 78.08573236070779444, -228.9307947190811774 ) ) ;
#24438 = VERTEX_POINT ( 'NONE', #152445 ) ;
#24437 = CARTESIAN_POINT ( 'NONE',  ( -16.80621392010904813, 60.95724664626749956, -221.0055571468712401 ) ) ;
#24439 = ORIENTED_EDGE ( 'NONE', *, *, #227057, .F. ) ;
#24440 = DIRECTION ( 'NONE',  ( 1.000000000000000000, 2.952720810173289112E-16, -0.000000000000000000 ) ) ;
#24441 = VECTOR ( 'NONE', #63588, 1000.000000000000114 ) ;
#24442 = AXIS2_PLACEMENT_3D ( 'NONE', #98048, #118950, #19852 ) ;
#24443 = CARTESIAN_POINT ( 'NONE',  ( -21.52071067811865746, 7.779289321892505882, -155.1500000000000057 ) ) ;
#24444 = CLOSED_SHELL ( 'NONE', ( #93514, #231899, #33585, #223638, #74734, #90628, #232417, #255096, #257586, #97914, #165410, #200576, #127157, #116588, #142229, #84628, #136428, #11208 ) ) ;
#24445 = CARTESIAN_POINT ( 'NONE',  ( 22.39999999999999503, 12.58895012248959944, -223.3279127647275857 ) ) ;
#24446 = DIRECTION ( 'NONE',  ( 0.000000000000000000, -0.9126074666063770380, -0.4088369013363281068 ) ) ;
#24447 = CARTESIAN_POINT ( 'NONE',  ( 20.94999999999999929, 74.63912941281984104, -94.95010955743335046 ) ) ;
#24448 = DIRECTION ( 'NONE',  ( 1.000000000000000000, 0.000000000000000000, 0.000000000000000000 ) ) ;
#24449 = VECTOR ( 'NONE', #40987, 1000.000000000000000 ) ;
#24450 = AXIS2_PLACEMENT_3D ( 'NONE', #200536, #21912, #254081 ) ;
#24451 = CARTESIAN_POINT ( 'NONE',  ( 23.14999999999999858, 34.81737220036618652, -252.9889942003018461 ) ) ;
#24453 = ORIENTED_EDGE ( 'NONE', *, *, #240644, .F. ) ;
#24452 = EDGE_CURVE ( 'NONE', #70684, #256630, #45713, .T. ) ;
#24454 = VERTEX_POINT ( 'NONE', #186422 ) ;
#24455 = FACE_OUTER_BOUND ( 'NONE', #70495, .T. ) ;
#24456 = CIRCLE ( 'NONE', #11983, 0.09999999999999351075 ) ;
#24457 = EDGE_CURVE ( 'NONE', #137090, #236044, #142195, .T. ) ;
#24458 = ORIENTED_EDGE ( 'NONE', *, *, #47582, .T. ) ;
#24459 = CARTESIAN_POINT ( 'NONE',  ( 21.07954640115348965, 0.06600770715080908624, -27.17071230397564463 ) ) ;
#24460 = ORIENTED_EDGE ( 'NONE', *, *, #101457, .T. ) ;
#24461 = DIRECTION ( 'NONE',  ( -0.000000000000000000, -0.000000000000000000, -1.000000000000000000 ) ) ;
#24462 = AXIS2_PLACEMENT_3D ( 'NONE', #43812, #123351, #202873 ) ;
#24463 = CARTESIAN_POINT ( 'NONE',  ( 19.97071067811864609, 11.72071067812981404, -88.35000000000003695 ) ) ;
#24464 = CARTESIAN_POINT ( 'NONE',  ( 20.95512820512820795, 10.62384868372303615, -146.2001620194244538 ) ) ;
#24465 = CARTESIAN_POINT ( 'NONE',  ( -20.00857864376270001, 66.65000000001180069, -81.77310748452437394 ) ) ;
#24466 = ORIENTED_EDGE ( 'NONE', *, *, #92462, .T. ) ;
#24467 = LINE ( 'NONE', #103947, #196135 ) ;
#24468 = ORIENTED_EDGE ( 'NONE', *, *, #86827, .T. ) ;
#24469 = CARTESIAN_POINT ( 'NONE',  ( 22.49999999999999645, 0.08880997639808871358, -122.3502370819681033 ) ) ;
#24470 = AXIS2_PLACEMENT_3D ( 'NONE', #222159, #18845, #120546 ) ;
#24472 = FACE_OUTER_BOUND ( 'NONE', #254375, .T. ) ;
#24471 = VECTOR ( 'NONE', #52851, 1000.000000000000000 ) ;
#24473 = CARTESIAN_POINT ( 'NONE',  ( -21.55000000000000426, 68.25000000001199396, -115.2731074845243455 ) ) ;
#24474 = AXIS2_PLACEMENT_3D ( 'NONE', #138918, #81518, #22890 ) ;
#24475 = EDGE_CURVE ( 'NONE', #63272, #104591, #198256, .T. ) ;
#24476 = ORIENTED_EDGE ( 'NONE', *, *, #151863, .T. ) ;
#24477 = DIRECTION ( 'NONE',  ( 1.000000000000000000, 0.000000000000000000, 0.000000000000000000 ) ) ;
#24478 = VERTEX_POINT ( 'NONE', #112021 ) ;
#24481 = ORIENTED_EDGE ( 'NONE', *, *, #49121, .T. ) ;
#24480 = DIRECTION ( 'NONE',  ( 0.000000000000000000, -0.2868887416115947775, 0.9579639084728169829 ) ) ;
#24479 = CYLINDRICAL_SURFACE ( 'NONE', #145183, 0.09999999999998898659 ) ;
#24482 = ORIENTED_EDGE ( 'NONE', *, *, #194135, .F. ) ;
#24483 = DIRECTION ( 'NONE',  ( 0.000000000000000000, 1.084202172485623868E-14, 1.000000000000000000 ) ) ;
#24484 = ORIENTED_EDGE ( 'NONE', *, *, #120290, .F. ) ;
#24485 = CARTESIAN_POINT ( 'NONE',  ( -17.29158576265543346, 65.63525233399438719, -158.6058657293166050 ) ) ;
#24486 = B_SPLINE_CURVE_WITH_KNOTS ( 'NONE', 3,
 ( #219838, #200287, #21654, #101121, #180731, #22957, #63322, #222377, #85427, #243246 ),
 .UNSPECIFIED., .F., .F.,
 ( 4, 3, 3, 4 ),
 ( 1.950915401637565782E-15, 8.145022132839031210E-06, 1.905645951092651034E-05, 2.061107371226032482E-05 ),
 .UNSPECIFIED. ) ;
#24487 = FACE_OUTER_BOUND ( 'NONE', #49530, .T. ) ;
#24488 = CARTESIAN_POINT ( 'NONE',  ( -18.50000000000000000, 76.00000000001267608, -203.5231074845243597 ) ) ;
#24489 = DIRECTION ( 'NONE',  ( -0.000000000000000000, -0.1332476588733589318, -0.9910827722268049644 ) ) ;
#24490 = CARTESIAN_POINT ( 'NONE',  ( -16.89060415895971090, 9.951220762802197584, -12.64592022427046203 ) ) ;
#24491 = ORIENTED_EDGE ( 'NONE', *, *, #89995, .F. ) ;
#24492 = DIRECTION ( 'NONE',  ( 0.000000000000000000, 0.000000000000000000, 1.000000000000000000 ) ) ;
#24493 = DIRECTION ( 'NONE',  ( 1.000000000000000000, -0.000000000000000000, -0.000000000000000000 ) ) ;
#24494 = CARTESIAN_POINT ( 'NONE',  ( 21.14999999999999503, 1.115600667400684642E-11, -134.0000000000000000 ) ) ;
#24495 = ORIENTED_EDGE ( 'NONE', *, *, #41741, .T. ) ;
#24496 = ORIENTED_EDGE ( 'NONE', *, *, #25515, .F. ) ;
#24497 = CARTESIAN_POINT ( 'NONE',  ( -23.25000000000000000, 11.75000000001115552, -134.0000000000000000 ) ) ;
#24498 = CARTESIAN_POINT ( 'NONE',  ( 19.75857864376268935, 34.53503747617446606, -235.1972745784239578 ) ) ;
#24499 = DIRECTION ( 'NONE',  ( 1.000000000000000000, 0.000000000000000000, 0.000000000000000000 ) ) ;
#24501 = ORIENTED_EDGE ( 'NONE', *, *, #152657, .F. ) ;
#24500 = CARTESIAN_POINT ( 'NONE',  ( 18.60000000000000142, -7.567701079425715349, -210.0537230116848946 ) ) ;
#24502 = EDGE_CURVE ( 'NONE', #24275, #76825, #33580, .T. ) ;
#24503 = PLANE ( 'NONE',  #106695 ) ;
#24504 = CARTESIAN_POINT ( 'NONE',  ( -18.50000000000000000, -9.499999999988849808, -142.1000000000000227 ) ) ;
#24505 = EDGE_CURVE ( 'NONE', #33031, #213499, #21419, .T. ) ;
#24506 = ORIENTED_EDGE ( 'NONE', *, *, #30944, .T. ) ;
#24507 = TOROIDAL_SURFACE ( 'NONE', #149413, 6.258578643762712446, 0.1000000000000000056 ) ;
#24509 = CIRCLE ( 'NONE', #224211, 0.6000000000000033085 ) ;
#24508 = CARTESIAN_POINT ( 'NONE',  ( -20.64999999999999858, 74.00000000001156764, -56.79848556176223440 ) ) ;
#24510 = CARTESIAN_POINT ( 'NONE',  ( -20.64999999999999858, 2.500000000011156409, -46.72462192276210402 ) ) ;
#24511 = VERTEX_POINT ( 'NONE', #7778 ) ;
#24512 = TOROIDAL_SURFACE ( 'NONE', #36991, 0.4000000000000012990, 0.1000000000000000056 ) ;
#24513 = DIRECTION ( 'NONE',  ( 0.000000000000000000, 1.000000000000000000, 6.982962677686266711E-15 ) ) ;
#24514 = ORIENTED_EDGE ( 'NONE', *, *, #215165, .T. ) ;
#24515 = EDGE_CURVE ( 'NONE', #244889, #109657, #76932, .T. ) ;
#24516 = CARTESIAN_POINT ( 'NONE',  ( -23.15000000000000213, 1.115600667400684642E-11, -67.00000000000004263 ) ) ;
#24517 = AXIS2_PLACEMENT_3D ( 'NONE', #215731, #239167, #180482 ) ;
#24519 = ORIENTED_EDGE ( 'NONE', *, *, #228726, .T. ) ;
#24518 = CARTESIAN_POINT ( 'NONE',  ( 23.14999999999999858, 71.22429906543244726, -91.17433938047835795 ) ) ;
#24520 = EDGE_CURVE ( 'NONE', #5002, #18671, #28669, .T. ) ;
#24521 = EDGE_CURVE ( 'NONE', #90604, #50990, #241815, .T. ) ;
#24524 = ORIENTED_EDGE ( 'NONE', *, *, #108814, .T. ) ;
#24523 = ORIENTED_EDGE ( 'NONE', *, *, #9637, .F. ) ;
#24522 = DIRECTION ( 'NONE',  ( 0.000000000000000000, 0.000000000000000000, 1.000000000000000000 ) ) ;
#24526 = VECTOR ( 'NONE', #142499, 1000.000000000000000 ) ;
#24525 = CARTESIAN_POINT ( 'NONE',  ( -21.98333005346336932, 29.92928821712972720, -252.5659568089976403 ) ) ;
#24527 = AXIS2_PLACEMENT_3D ( 'NONE', #206100, #67865, #225629 ) ;
#24528 = FACE_OUTER_BOUND ( 'NONE', #29959, .T. ) ;
#24529 = DIRECTION ( 'NONE',  ( 0.000000000000000000, 0.000000000000000000, 1.000000000000000000 ) ) ;
#24530 = AXIS2_PLACEMENT_3D ( 'NONE', #213616, #35028, #31180 ) ;
#24531 = EDGE_CURVE ( 'NONE', #255306, #159190, #158795, .T. ) ;
#24533 = CYLINDRICAL_SURFACE ( 'NONE', #208668, 0.1000000000000028644 ) ;
#24532 = DIRECTION ( 'NONE',  ( 0.000000000000000000, -0.9126074666063660468, -0.4088369013363524762 ) ) ;
#24534 = CARTESIAN_POINT ( 'NONE',  ( -21.05000000000000071, -0.09999999998884338825, -155.8499999999999659 ) ) ;
#24535 = CYLINDRICAL_SURFACE ( 'NONE', #63986, 0.1000000000000055844 ) ;
#24536 = CARTESIAN_POINT ( 'NONE',  ( 23.15000000000000213, -8.663551401858002876, -76.52410111806734960 ) ) ;
#24537 = AXIS2_PLACEMENT_3D ( 'NONE', #175326, #77447, #233974 ) ;
#24538 = CARTESIAN_POINT ( 'NONE',  ( -22.50000000000094147, 75.90000000001231228, -148.1726782920691221 ) ) ;
#24539 = ORIENTED_EDGE ( 'NONE', *, *, #168346, .T. ) ;
#24540 = ORIENTED_EDGE ( 'NONE', *, *, #172587, .F. ) ;
#24541 = DIRECTION ( 'NONE',  ( 1.000000000000000000, -3.265361837132813093E-16, -2.280189983783949500E-30 ) ) ;
#24543 = ORIENTED_EDGE ( 'NONE', *, *, #55293, .F. ) ;
#24542 = CARTESIAN_POINT ( 'NONE',  ( -22.39999999999999858, 64.25000000001165290, -69.42310748452440805 ) ) ;
#24544 = ORIENTED_EDGE ( 'NONE', *, *, #249303, .F. ) ;
#24545 = EDGE_CURVE ( 'NONE', #42982, #186477, #187997, .T. ) ;
#24546 = CARTESIAN_POINT ( 'NONE',  ( -22.00356870141645871, 7.254242362487164364, -2.206487650916222969E-12 ) ) ;
#24547 = VERTEX_POINT ( 'NONE', #115856 ) ;
#24548 = DIRECTION ( 'NONE',  ( 0.000000000000000000, 0.000000000000000000, -1.000000000000000000 ) ) ;
#24549 = EDGE_LOOP ( 'NONE', ( #127219, #183059, #94665, #146334 ) ) ;
#24550 = FACE_OUTER_BOUND ( 'NONE', #217626, .T. ) ;
#24551 = CARTESIAN_POINT ( 'NONE',  ( -18.54270223418606989, -9.624105502871749707, -174.2409350504074723 ) ) ;
#24552 = VECTOR ( 'NONE', #192896, 1000.000000000000000 ) ;
#24553 = AXIS2_PLACEMENT_3D ( 'NONE', #30175, #26309, #67991 ) ;
#24555 = ORIENTED_EDGE ( 'NONE', *, *, #18595, .T. ) ;
#24554 = ORIENTED_EDGE ( 'NONE', *, *, #256244, .T. ) ;
#24556 = ORIENTED_EDGE ( 'NONE', *, *, #132492, .F. ) ;
#24557 = DIRECTION ( 'NONE',  ( 1.000000000000000000, 0.000000000000000000, 0.000000000000000000 ) ) ;
#24558 = ORIENTED_EDGE ( 'NONE', *, *, #40442, .T. ) ;
#24559 = EDGE_LOOP ( 'NONE', ( #179470, #31265, #180473, #215496 ) ) ;
#24560 = DIRECTION ( 'NONE',  ( 0.000000000000000000, -0.2128009952263982818, 0.9770955615653232895 ) ) ;
#24561 = DIRECTION ( 'NONE',  ( 0.000000000000000000, 0.9126074666064177832, 0.4088369013362369020 ) ) ;
#24563 = VERTEX_POINT ( 'NONE', #14213 ) ;
#24562 = CYLINDRICAL_SURFACE ( 'NONE', #185157, 0.09999999999999939493 ) ;
#24565 = CARTESIAN_POINT ( 'NONE',  ( -22.50000000000000000, 75.90000000001245439, -181.6726782920691505 ) ) ;
#24564 = CARTESIAN_POINT ( 'NONE',  ( 23.24999999999999289, 11.65000000001116298, -167.4999999999999716 ) ) ;
#24566 = DIRECTION ( 'NONE',  ( -2.578261006436900068E-14, 0.1350103645451904977, -0.9908441862701597991 ) ) ;
#24568 = ORIENTED_EDGE ( 'NONE', *, *, #89942, .T. ) ;
#24567 = CARTESIAN_POINT ( 'NONE',  ( -20.64999999999999858, 7.250000000011155521, -146.2500000000000284 ) ) ;
#24569 = CARTESIAN_POINT ( 'NONE',  ( -20.54999999999999716, -9.000000000000001776, -24.00603087734755903 ) ) ;
#24570 = ORIENTED_EDGE ( 'NONE', *, *, #33437, .F. ) ;
#24571 = CARTESIAN_POINT ( 'NONE',  ( -20.85000000000000142, -1.135018845899022466, -208.7169768834322952 ) ) ;
#24572 = ORIENTED_EDGE ( 'NONE', *, *, #33837, .T. ) ;
#24573 = CARTESIAN_POINT ( 'NONE',  ( 22.47071067811865319, 75.90090754530939421, -110.7431822290223522 ) ) ;
#24574 = CARTESIAN_POINT ( 'NONE',  ( 20.85000000000000142, 77.16412189325258453, -28.10825939895270764 ) ) ;
#24575 = ORIENTED_EDGE ( 'NONE', *, *, #196421, .T. ) ;
#24576 = AXIS2_PLACEMENT_3D ( 'NONE', #167542, #210499, #91829 ) ;
#24578 = DIRECTION ( 'NONE',  ( 0.000000000000000000, 0.000000000000000000, 1.000000000000000000 ) ) ;
#24577 = AXIS2_PLACEMENT_3D ( 'NONE', #64696, #47685, #258041 ) ;
#24579 = AXIS2_PLACEMENT_3D ( 'NONE', #31216, #226795, #7305 ) ;
#24580 = EDGE_CURVE ( 'NONE', #107664, #200718, #167180, .T. ) ;
#24581 = CARTESIAN_POINT ( 'NONE',  ( -23.15000000000000213, 64.40000000001147384, -42.95131071479990936 ) ) ;
#24582 = CARTESIAN_POINT ( 'NONE',  ( 21.05000000000000071, 18.65488991999774271, -228.0822300706204544 ) ) ;
#24583 = VECTOR ( 'NONE', #85264, 1000.000000000000000 ) ;
#24584 = ORIENTED_EDGE ( 'NONE', *, *, #143849, .T. ) ;
#24585 = ORIENTED_EDGE ( 'NONE', *, *, #126410, .T. ) ;
#24586 = CARTESIAN_POINT ( 'NONE',  ( 21.14999999999999858, 1.115600667400684642E-11, -179.6499999999999773 ) ) ;
#24587 = PLANE ( 'NONE',  #98312 ) ;
#24588 = EDGE_LOOP ( 'NONE', ( #62027, #181013, #233855, #208870 ) ) ;
#24589 = DIRECTION ( 'NONE',  ( -1.000000000000000000, 0.000000000000000000, 0.000000000000000000 ) ) ;
#24590 = ORIENTED_EDGE ( 'NONE', *, *, #147256, .F. ) ;
#24591 = CYLINDRICAL_SURFACE ( 'NONE', #131538, 0.09999999999999939493 ) ;
#24593 = ADVANCED_FACE ( 'NONE', ( #93721 ), #75473, .F. ) ;
#24592 = CARTESIAN_POINT ( 'NONE',  ( -23.25000000000000000, 5.950000000011163692, -56.69429769496518645 ) ) ;
#24595 = DIRECTION ( 'NONE',  ( 1.000000000000000000, 0.000000000000000000, 0.000000000000000000 ) ) ;
#24594 = CARTESIAN_POINT ( 'NONE',  ( 22.10000000000000142, -11.65000000000000036, 12.09999999999999609 ) ) ;
#24596 = AXIS2_PLACEMENT_3D ( 'NONE', #197127, #257059, #78460 ) ;
#24597 = VECTOR ( 'NONE', #74103, 1000.000000000000000 ) ;
#24598 = CARTESIAN_POINT ( 'NONE',  ( 22.49999999999999645, 0.08880997639808872746, -55.35023708196812464 ) ) ;
#24599 = CARTESIAN_POINT ( 'NONE',  ( -22.94999999999999929, 11.50977166988710820, -1.786320531569725478 ) ) ;
#24600 = EDGE_CURVE ( 'NONE', #138276, #192532, #96391, .T. ) ;
#24601 = ADVANCED_FACE ( 'NONE', ( #16772 ), #195417, .T. ) ;
#24602 = ORIENTED_EDGE ( 'NONE', *, *, #48278, .T. ) ;
#24603 = AXIS2_PLACEMENT_3D ( 'NONE', #130207, #209768, #32447 ) ;
#24604 = CARTESIAN_POINT ( 'NONE',  ( -16.77683809663752257, 63.08610022504904435, -213.1421742787362064 ) ) ;
#24607 = EDGE_LOOP ( 'NONE', ( #135595, #171131, #188932, #200305 ) ) ;
#24606 = VERTEX_POINT ( 'NONE', #256590 ) ;
#24605 = CIRCLE ( 'NONE', #216100, 0.09999999999998898659 ) ;
#24608 = ORIENTED_EDGE ( 'NONE', *, *, #104895, .F. ) ;
#24609 = CIRCLE ( 'NONE', #241266, 0.09999999999998898659 ) ;
#24610 = VECTOR ( 'NONE', #251634, 1000.000000000000000 ) ;
#24611 = ORIENTED_EDGE ( 'NONE', *, *, #203258, .T. ) ;
#24612 = CARTESIAN_POINT ( 'NONE',  ( -21.29999999999995808, 1.115600667400684642E-11, -33.50000000000000000 ) ) ;
#24613 = CARTESIAN_POINT ( 'NONE',  ( -21.44999999999999929, 11.50825441376376901, -220.2417535673963300 ) ) ;
#24614 = CARTESIAN_POINT ( 'NONE',  ( -21.05000000000000071, 1.115600667400684642E-11, -67.00000000000000000 ) ) ;
#24615 = DIRECTION ( 'NONE',  ( -0.000000000000000000, -6.982962677686266711E-15, 1.000000000000000000 ) ) ;
#24616 = CARTESIAN_POINT ( 'NONE',  ( -21.00000000000000000, 7.900000000000000355, -1.212568896937008089 ) ) ;
#24617 = EDGE_CURVE ( 'NONE', #74571, #18045, #212944, .T. ) ;
#24618 = AXIS2_PLACEMENT_3D ( 'NONE', #57863, #197385, #137410 ) ;
#24620 = CARTESIAN_POINT ( 'NONE',  ( -22.39999999999999503, 1.115541036281197940E-11, -159.7092204016265384 ) ) ;
#24619 = CARTESIAN_POINT ( 'NONE',  ( 21.97500000000000497, 12.13349391679638778, -210.8946109257198032 ) ) ;
#24622 = ORIENTED_EDGE ( 'NONE', *, *, #70628, .F. ) ;
#24621 = CARTESIAN_POINT ( 'NONE',  ( 18.46163235739467368, 77.18289512160934862, -241.7849060539989807 ) ) ;
#24623 = DIRECTION ( 'NONE',  ( 0.000000000000000000, 1.000000000000000000, -0.000000000000000000 ) ) ;
#24624 = VERTEX_POINT ( 'NONE', #212404 ) ;
#24625 = EDGE_CURVE ( 'NONE', #56847, #208658, #36338, .T. ) ;
#24626 = CARTESIAN_POINT ( 'NONE',  ( 21.07928932188134397, 33.98134083355422774, -243.8161431329846778 ) ) ;
#24627 = ORIENTED_EDGE ( 'NONE', *, *, #7479, .F. ) ;
#24628 = ORIENTED_EDGE ( 'NONE', *, *, #193568, .F. ) ;
#24629 = CARTESIAN_POINT ( 'NONE',  ( 21.05000000000000071, 69.74218538953603286, -136.6208977758331287 ) ) ;
#24630 = DIRECTION ( 'NONE',  ( 0.000000000000000000, 0.9126074666063771490, 0.4088369013363281623 ) ) ;
#24631 = CARTESIAN_POINT ( 'NONE',  ( -16.80070461187883879, 66.05000000001155058, -48.67007131368379191 ) ) ;
#24632 = CARTESIAN_POINT ( 'NONE',  ( -18.40000000000000213, 53.98582189624753624, -228.9137301112145622 ) ) ;
#24633 = PRODUCT_RELATED_PRODUCT_CATEGORY ( 'part', '', ( #211859 ) ) ;
#24634 = AXIS2_PLACEMENT_3D ( 'NONE', #237939, #37199, #140107 ) ;
#24635 = EDGE_LOOP ( 'NONE', ( #96474, #205634, #177585, #244611 ) ) ;
#24636 = ORIENTED_EDGE ( 'NONE', *, *, #81845, .F. ) ;
#24637 = EDGE_CURVE ( 'NONE', #253340, #183881, #252781, .T. ) ;
#24638 = CARTESIAN_POINT ( 'NONE',  ( 23.14999999999999503, 6.450000000011156587, -121.6500000000000341 ) ) ;
#24640 = ORIENTED_EDGE ( 'NONE', *, *, #11665, .F. ) ;
#24639 = EDGE_CURVE ( 'NONE', #241144, #176862, #125458, .T. ) ;
#24641 = DIRECTION ( 'NONE',  ( -1.000000000000000000, 0.000000000000000000, -0.000000000000000000 ) ) ;
#24642 = CARTESIAN_POINT ( 'NONE',  ( -16.91247567987037925, 9.959082683680399839, -46.12872445853733439 ) ) ;
#24643 = EDGE_CURVE ( 'NONE', #224755, #102331, #175541, .T. ) ;
#24644 = CARTESIAN_POINT ( 'NONE',  ( -23.25000000000000000, 71.85000000001186038, -90.67310748452433700 ) ) ;
#24645 = DIRECTION ( 'NONE',  ( 1.000000000000000000, 0.000000000000000000, 0.000000000000000000 ) ) ;
#24646 = DIRECTION ( 'NONE',  ( -0.000000000000000000, 1.000000000000000000, 6.982962677686266711E-15 ) ) ;
#24647 = CARTESIAN_POINT ( 'NONE',  ( 21.93642651522410603, 7.327166239336949438, -67.00000000000004263 ) ) ;
#24648 = DIRECTION ( 'NONE',  ( 0.000000000000000000, 1.000000000000000000, 6.982962677686266711E-15 ) ) ;
#24649 = CIRCLE ( 'NONE', #41198, 0.5000000000000004441 ) ;
#24650 = DIRECTION ( 'NONE',  ( -1.000000000000000000, 0.000000000000000000, 0.000000000000000000 ) ) ;
#24651 = CARTESIAN_POINT ( 'NONE',  ( 20.94999999999999929, 42.88650567345842290, -254.4176359484683871 ) ) ;
#24652 = VECTOR ( 'NONE', #168159, 1000.000000000000000 ) ;
#24653 = DIRECTION ( 'NONE',  ( -3.265361837132813093E-16, 1.000000000000000000, 0.000000000000000000 ) ) ;
#24654 = FACE_OUTER_BOUND ( 'NONE', #17220, .T. ) ;
#24655 = CIRCLE ( 'NONE', #16264, 0.09999999999999939493 ) ;
#24656 = DIRECTION ( 'NONE',  ( 1.000000000000000000, 0.000000000000000000, 0.000000000000000000 ) ) ;
#24657 = AXIS2_PLACEMENT_3D ( 'NONE', #65623, #46061, #9502 ) ;
#24658 = EDGE_LOOP ( 'NONE', ( #167349, #35286, #183783, #195604 ) ) ;
#24659 = CARTESIAN_POINT ( 'NONE',  ( -20.94999999999999929, 47.95459712139159336, -246.5019368548292675 ) ) ;
#24660 = VERTEX_POINT ( 'NONE', #33794 ) ;
#24661 = FACE_BOUND ( 'NONE', #176978, .T. ) ;
#24662 = DIRECTION ( 'NONE',  ( 1.000000000000000000, 0.000000000000000000, -0.000000000000000000 ) ) ;
#24663 = FACE_OUTER_BOUND ( 'NONE', #49884, .T. ) ;
#24664 = CIRCLE ( 'NONE', #41220, 0.4000000000000114575 ) ;
#24665 = VERTEX_POINT ( 'NONE', #214951 ) ;
#24666 = EDGE_CURVE ( 'NONE', #15533, #127486, #104568, .T. ) ;
#24667 = CYLINDRICAL_SURFACE ( 'NONE', #229933, 0.09999999999998898659 ) ;
#24668 = CIRCLE ( 'NONE', #16281, 4.049999999999998046 ) ;
#24669 = CARTESIAN_POINT ( 'NONE',  ( 20.94999999999999929, 87.48912529308852015, -172.9231074845242802 ) ) ;
#24670 = CARTESIAN_POINT ( 'NONE',  ( -23.25000000000000000, 11.75000000001115552, -88.75000000000004263 ) ) ;
#24671 = DIRECTION ( 'NONE',  ( 0.000000000000000000, 6.982962677686266711E-15, -1.000000000000000000 ) ) ;
#24672 = TOROIDAL_SURFACE ( 'NONE', #49588, 0.2000000000000000111, 0.1000000000000000056 ) ;
#24673 = DIRECTION ( 'NONE',  ( 1.000000000000000000, -7.136802563874199107E-16, -1.554319503706929991E-16 ) ) ;
#24674 = ORIENTED_EDGE ( 'NONE', *, *, #151628, .F. ) ;
#24675 = DIRECTION ( 'NONE',  ( -1.000000000000000000, 0.000000000000000000, 0.000000000000000000 ) ) ;
#24677 = ORIENTED_EDGE ( 'NONE', *, *, #33221, .T. ) ;
#24676 = CARTESIAN_POINT ( 'NONE',  ( 0.8999999999999993561, -8.250000000000005329, 26.00000000000000355 ) ) ;
#24678 = ADVANCED_FACE ( 'NONE', ( #76711 ), #192115, .T. ) ;
#24679 = DIRECTION ( 'NONE',  ( 0.000000000000000000, 0.000000000000000000, -1.000000000000000000 ) ) ;
#24680 =( NAMED_UNIT ( * ) SI_UNIT ( $, .STERADIAN. ) SOLID_ANGLE_UNIT ( ) );
#24681 = ORIENTED_EDGE ( 'NONE', *, *, #171742, .F. ) ;
#24682 = CARTESIAN_POINT ( 'NONE',  ( -22.45372860728439690, 75.98507938046373056, -148.1729046192281771 ) ) ;
#24683 = EDGE_CURVE ( 'NONE', #92040, #211799, #5539, .T. ) ;
#24684 = FACE_OUTER_BOUND ( 'NONE', #50029, .T. ) ;
#24685 = ORIENTED_EDGE ( 'NONE', *, *, #39610, .T. ) ;
#24687 = ADVANCED_FACE ( 'NONE', ( #57133 ), #117142, .T. ) ;
#24686 = CARTESIAN_POINT ( 'NONE',  ( -20.94999999999999929, -1.162701749926853712, -108.5000000000000426 ) ) ;
#24688 = CYLINDRICAL_SURFACE ( 'NONE', #130131, 0.09999999999999939493 ) ;
#24689 = CIRCLE ( 'NONE', #37322, 0.09999999999999939493 ) ;
#24690 = EDGE_CURVE ( 'NONE', #246496, #4373, #213671, .T. ) ;
#24691 = EDGE_CURVE ( 'NONE', #227218, #18809, #76283, .T. ) ;
#24692 = LINE ( 'NONE', #228969, #33025 ) ;
#24693 = ORIENTED_EDGE ( 'NONE', *, *, #61789, .T. ) ;
#24694 = ORIENTED_EDGE ( 'NONE', *, *, #14664, .F. ) ;
#24695 = CARTESIAN_POINT ( 'NONE',  ( 21.05000000000000071, 10.72371681401022592, -74.59439923588408305 ) ) ;
#24696 = LINE ( 'NONE', #125062, #225639 ) ;
#24697 = DIRECTION ( 'NONE',  ( 1.000000000000000000, 2.885090398161910739E-16, 6.283419270304611573E-17 ) ) ;
#24698 = DIRECTION ( 'NONE',  ( 0.000000000000000000, -5.956132106358139644E-15, 1.000000000000000000 ) ) ;
#24699 = CARTESIAN_POINT ( 'NONE',  ( 21.14999999999999503, 79.33069327855442054, -236.1318330389568985 ) ) ;
#24700 = FACE_OUTER_BOUND ( 'NONE', #256720, .T. ) ;
#24701 = DIRECTION ( 'NONE',  ( -1.000000000000000000, 0.000000000000000000, -0.000000000000000000 ) ) ;
#24703 = DIRECTION ( 'NONE',  ( 0.000000000000000000, 0.000000000000000000, 1.000000000000000000 ) ) ;
#24702 = CARTESIAN_POINT ( 'NONE',  ( 20.95325940946048249, 65.47660992931560031, -95.45864535528430395 ) ) ;
#24704 = AXIS2_PLACEMENT_3D ( 'NONE', #221266, #137877, #197864 ) ;
#24706 = CARTESIAN_POINT ( 'NONE',  ( -21.05000000000000071, 77.83534155023671985, -158.4679561919613491 ) ) ;
#24705 = TOROIDAL_SURFACE ( 'NONE', #224398, 11.65000000000000036, 0.1000000000000000056 ) ;
#24707 = CARTESIAN_POINT ( 'NONE',  ( -20.64999999999999858, 0.000000000000000000, 0.000000000000000000 ) ) ;
#24708 = DIRECTION ( 'NONE',  ( -1.000000000000000000, -2.952720810173289112E-16, 0.000000000000000000 ) ) ;
#24709 = CIRCLE ( 'NONE', #57966, 0.09999999999999939493 ) ;
#24711 = CARTESIAN_POINT ( 'NONE',  ( 21.05000000000000071, 55.59258605799641373, -234.6589115948038966 ) ) ;
#24710 = VECTOR ( 'NONE', #132311, 1000.000000000000000 ) ;
#24712 = ORIENTED_EDGE ( 'NONE', *, *, #177706, .F. ) ;
#24713 = ADVANCED_FACE ( 'NONE', ( #79266 ), #184618, .F. ) ;
#24714 = ORIENTED_EDGE ( 'NONE', *, *, #6404, .F. ) ;
#24715 = DIRECTION ( 'NONE',  ( 0.000000000000000000, -0.6728971962616412394, -0.7397360091703134577 ) ) ;
#24716 = ADVANCED_FACE ( 'NONE', ( #218784 ), #40197, .T. ) ;
#24718 = LINE ( 'NONE', #147197, #211942 ) ;
#24717 = DIRECTION ( 'NONE',  ( -0.000000000000000000, 1.000000000000000000, -0.000000000000000000 ) ) ;
#24719 = CIRCLE ( 'NONE', #74606, 12.97499999999999964 ) ;
#24720 = FACE_BOUND ( 'NONE', #133502, .T. ) ;
#24722 = ADVANCED_FACE ( 'NONE', ( #100106 ), #13758, .F. ) ;
#24721 = CARTESIAN_POINT ( 'NONE',  ( 20.94999999999999574, 87.48912529308798014, -100.1231074845242262 ) ) ;
#24723 = FACE_OUTER_BOUND ( 'NONE', #244364, .T. ) ;
#24724 = FACE_OUTER_BOUND ( 'NONE', #163104, .T. ) ;
#24725 = ORIENTED_EDGE ( 'NONE', *, *, #126357, .F. ) ;
#24726 = CIRCLE ( 'NONE', #91343, 0.09999999999999868716 ) ;
#24727 = AXIS2_PLACEMENT_3D ( 'NONE', #179860, #177312, #218959 ) ;
#24728 = EDGE_CURVE ( 'NONE', #26254, #250075, #123555, .T. ) ;
#24730 = TOROIDAL_SURFACE ( 'NONE', #141395, 1.900000000000002576, 0.1000000000000000056 ) ;
#24729 = LINE ( 'NONE', #5095, #13851 ) ;
#24731 = ORIENTED_EDGE ( 'NONE', *, *, #86765, .T. ) ;
#24732 = DIRECTION ( 'NONE',  ( 2.915501640297156255E-16, 1.000000000000000000, 6.997203936713175802E-15 ) ) ;
#24733 = EDGE_CURVE ( 'NONE', #45688, #108560, #222014, .T. ) ;
#24734 = AXIS2_PLACEMENT_3D ( 'NONE', #190738, #167315, #86430 ) ;
#24735 = CARTESIAN_POINT ( 'NONE',  ( 18.44208962362734638, 85.55234049691893006, -29.18093442906062407 ) ) ;
#24736 = EDGE_CURVE ( 'NONE', #81658, #196598, #163788, .T. ) ;
#24737 = ORIENTED_EDGE ( 'NONE', *, *, #66674, .F. ) ;
#24738 = DIRECTION ( 'NONE',  ( -0.000000000000000000, 0.1298341882519735979, 0.9915357197604890427 ) ) ;
#24739 = EDGE_LOOP ( 'NONE', ( #50791, #35786, #182866, #219446 ) ) ;
#24740 = EDGE_CURVE ( 'NONE', #244509, #135741, #213673, .T. ) ;
#24741 = CARTESIAN_POINT ( 'NONE',  ( 18.59999999999998721, 69.06610602788505560, -32.23746165015079868 ) ) ;
#24742 = ADVANCED_FACE ( 'NONE', ( #42727 ), #63832, .F. ) ;
#24743 = CARTESIAN_POINT ( 'NONE',  ( 20.94999999999999929, 74.16465844978765176, -124.9679561919613207 ) ) ;
#24744 = DIRECTION ( 'NONE',  ( 0.000000000000000000, 0.2128009952263582305, -0.9770955615653319493 ) ) ;
#24745 = DIRECTION ( 'NONE',  ( 0.000000000000000000, 1.000000000000000000, 6.982962677686266711E-15 ) ) ;
#24746 = DIRECTION ( 'NONE',  ( 1.000000000000000000, -0.000000000000000000, 0.000000000000000000 ) ) ;
#24747 = DIRECTION ( 'NONE',  ( -1.000000000000000000, 0.000000000000000000, 0.000000000000000000 ) ) ;
#24748 = CARTESIAN_POINT ( 'NONE',  ( -18.59999999999999787, 68.87972903831409610, -65.86354444268503983 ) ) ;
#24750 = EDGE_LOOP ( 'NONE', ( #171132, #198588, #190561, #249444 ) ) ;
#24749 = CARTESIAN_POINT ( 'NONE',  ( -20.54999999999999716, 2.400000000011155432, -87.27537807723794572 ) ) ;
#24752 = DIRECTION ( 'NONE',  ( 1.000000000000000000, 0.000000000000000000, 0.000000000000000000 ) ) ;
#24751 = DIRECTION ( 'NONE',  ( -1.000000000000000000, 0.000000000000000000, 0.000000000000000000 ) ) ;
#24753 = ORIENTED_EDGE ( 'NONE', *, *, #123184, .T. ) ;
#24755 = EDGE_LOOP ( 'NONE', ( #34145, #69048, #197816, #64236 ) ) ;
#24754 = CARTESIAN_POINT ( 'NONE',  ( -20.95000000000000284, 64.35000000001195986, -110.0379132551783243 ) ) ;
#24756 = AXIS2_PLACEMENT_3D ( 'NONE', #251452, #74135, #191516 ) ;
#24757 = EDGE_LOOP ( 'NONE', ( #181875, #22299, #18452, #21726, #157025 ) ) ;
#24758 = LINE ( 'NONE', #6437, #53332 ) ;
#24759 = DIRECTION ( 'NONE',  ( 0.000000000000000000, 0.000000000000000000, -1.000000000000000000 ) ) ;
#24760 = CARTESIAN_POINT ( 'NONE',  ( -21.05000000000000071, 1.162701749949165642, -108.5000000000000426 ) ) ;
#24761 = VERTEX_POINT ( 'NONE', #105219 ) ;
#24762 = CARTESIAN_POINT ( 'NONE',  ( 21.04999999999999716, -0.01454569055791622018, -127.5029822135672077 ) ) ;
#24763 = DIRECTION ( 'NONE',  ( -1.000000000000000000, -0.000000000000000000, -0.000000000000000000 ) ) ;
#24764 = AXIS2_PLACEMENT_3D ( 'NONE', #98273, #20077, #77441 ) ;
#24765 = CARTESIAN_POINT ( 'NONE',  ( 18.47688499308725341, 38.09689311189373484, -261.0587169989327663 ) ) ;
#24766 = CARTESIAN_POINT ( 'NONE',  ( -16.87036670365548474, 9.989418819312801290, -154.9795601173020714 ) ) ;
#24767 = CARTESIAN_POINT ( 'NONE',  ( -20.94999999999999929, 4.288595810029049993, -211.9930862808554934 ) ) ;
#24768 = PLANE ( 'NONE',  #230900 ) ;
#24769 = ORIENTED_EDGE ( 'NONE', *, *, #43636, .T. ) ;
#24770 = EDGE_LOOP ( 'NONE', ( #249025, #22485, #152576, #53106 ) ) ;
#24771 = AXIS2_PLACEMENT_3D ( 'NONE', #72424, #211928, #112816 ) ;
#24772 = DIRECTION ( 'NONE',  ( 2.710505431213777355E-16, -0.9770955615653316162, -0.2128009952263604232 ) ) ;
#24773 = AXIS2_PLACEMENT_3D ( 'NONE', #166134, #66992, #163527 ) ;
#24774 = EDGE_CURVE ( 'NONE', #47997, #124622, #185945, .T. ) ;
#24775 = ORIENTED_EDGE ( 'NONE', *, *, #149438, .T. ) ;
#24776 = DIRECTION ( 'NONE',  ( 0.000000000000000000, 0.000000000000000000, -1.000000000000000000 ) ) ;
#24778 = ORIENTED_EDGE ( 'NONE', *, *, #146667, .T. ) ;
#24777 = VECTOR ( 'NONE', #26316, 1000.000000000000000 ) ;
#24779 = CARTESIAN_POINT ( 'NONE',  ( -20.54999999999999716, 73.60000000001149090, -45.91707660717678152 ) ) ;
#24780 = LINE ( 'NONE', #246366, #117588 ) ;
#24781 = DIRECTION ( 'NONE',  ( 0.000000000000000000, 0.000000000000000000, -1.000000000000000000 ) ) ;
#24782 = CARTESIAN_POINT ( 'NONE',  ( -21.14250536705909056, 30.71039182449740679, -252.2160320164180689 ) ) ;
#24783 = FACE_OUTER_BOUND ( 'NONE', #225504, .T. ) ;
#24784 = VERTEX_POINT ( 'NONE', #201795 ) ;
#24785 = AXIS2_PLACEMENT_3D ( 'NONE', #170909, #206132, #91324 ) ;
#24786 = CIRCLE ( 'NONE', #257918, 0.8750000000000007772 ) ;
#24787 = CARTESIAN_POINT ( 'NONE',  ( 23.14999999999999503, 2.319530388122574394, -217.8268657444419887 ) ) ;
#24788 = CARTESIAN_POINT ( 'NONE',  ( 21.05000000000000071, 43.39316802731212874, -245.2602608822587342 ) ) ;
#24789 = CARTESIAN_POINT ( 'NONE',  ( -23.15000000000000213, 11.75000000001115552, -21.75000000000000355 ) ) ;
#24791 = EDGE_CURVE ( 'NONE', #238120, #84325, #105483, .T. ) ;
#24790 = DIRECTION ( 'NONE',  ( 0.000000000000000000, -1.000000000000000000, -6.982962677686265922E-15 ) ) ;
#24792 = ORIENTED_EDGE ( 'NONE', *, *, #180367, .T. ) ;
#24794 = CARTESIAN_POINT ( 'NONE',  ( -23.25000000000000000, 49.61306877027904250, -254.2671747026441551 ) ) ;
#24793 = DIRECTION ( 'NONE',  ( -1.000000000000000000, 0.000000000000000000, 0.000000000000000000 ) ) ;
#24795 = ORIENTED_EDGE ( 'NONE', *, *, #39886, .T. ) ;
#24798 = ORIENTED_EDGE ( 'NONE', *, *, #165273, .F. ) ;
#24797 = CARTESIAN_POINT ( 'NONE',  ( -20.94999999999999929, 7.128833340094563376, -233.7327013124401276 ) ) ;
#24796 = CARTESIAN_POINT ( 'NONE',  ( -22.39999999999999858, 1.115600667400684642E-11, -161.2499999999999716 ) ) ;
#24799 = AXIS2_PLACEMENT_3D ( 'NONE', #17842, #159961, #59515 ) ;
#24800 = ORIENTED_EDGE ( 'NONE', *, *, #110919, .T. ) ;
#24801 = CARTESIAN_POINT ( 'NONE',  ( -17.11825945287483108, 9.950000000011124612, -113.1500000000000483 ) ) ;
#24802 = AXIS2_PLACEMENT_3D ( 'NONE', #20535, #255218, #156203 ) ;
#24803 = AXIS2_PLACEMENT_3D ( 'NONE', #27176, #45416, #85787 ) ;
#24804 = CIRCLE ( 'NONE', #41361, 0.09999999999998898659 ) ;
#24805 = DIRECTION ( 'NONE',  ( 0.000000000000000000, -0.9889818879709272315, -0.1480365673253073999 ) ) ;
#24806 = PLANE ( 'NONE',  #133364 ) ;
#24807 = ORIENTED_EDGE ( 'NONE', *, *, #120097, .T. ) ;
#24808 = DIRECTION ( 'NONE',  ( 0.000000000000000000, -0.1298341882520022694, -0.9915357197604853789 ) ) ;
#24809 = VECTOR ( 'NONE', #17193, 1000.000000000000000 ) ;
#24810 = DIRECTION ( 'NONE',  ( 1.000000000000000000, -3.265361837132813093E-16, -2.280189983783949500E-30 ) ) ;
#24812 = DIRECTION ( 'NONE',  ( 0.000000000000000000, 0.000000000000000000, 1.000000000000000000 ) ) ;
#24811 = CARTESIAN_POINT ( 'NONE',  ( 22.39999999999999503, 64.35000000001164722, -69.62310748452439668 ) ) ;
#24814 = ORIENTED_EDGE ( 'NONE', *, *, #214868, .F. ) ;
#24813 = CARTESIAN_POINT ( 'NONE',  ( 21.07928932188134397, 0.09889514565439641580, 6.328516656393307294 ) ) ;
#24815 = EDGE_LOOP ( 'NONE', ( #202486, #8406, #109703, #164949 ) ) ;
#24816 = CARTESIAN_POINT ( 'NONE',  ( 19.99999999738052736, 64.25000000001179501, -78.33593553489176031 ) ) ;
#24817 = VECTOR ( 'NONE', #226927, 1000.000000000000000 ) ;
#24818 = LINE ( 'NONE', #182592, #164485 ) ;
#24819 = CARTESIAN_POINT ( 'NONE',  ( 18.49999999999999645, 76.00000000001213607, -136.5231074845243313 ) ) ;
#24820 = ORIENTED_EDGE ( 'NONE', *, *, #93551, .T. ) ;
#24821 = CARTESIAN_POINT ( 'NONE',  ( -21.14999999999999858, 26.06832281015329755, -254.4051978787608732 ) ) ;
#24822 = VERTEX_POINT ( 'NONE', #158854 ) ;
#24823 = LINE ( 'NONE', #72593, #134799 ) ;
#24824 = DIRECTION ( 'NONE',  ( 0.000000000000000000, 0.8814952561694257005, -0.4721928772766468829 ) ) ;
#24825 = CARTESIAN_POINT ( 'NONE',  ( 18.39999999999999503, 70.35000000001181775, -82.17310748452435121 ) ) ;
#24826 = ORIENTED_EDGE ( 'NONE', *, *, #150147, .T. ) ;
#24827 = DIRECTION ( 'NONE',  ( -1.000000000000000000, 0.000000000000000000, 0.000000000000000000 ) ) ;
#24828 = AXIS2_PLACEMENT_3D ( 'NONE', #164276, #207258, #202110 ) ;
#24829 = AXIS2_PLACEMENT_3D ( 'NONE', #47312, #51157, #75601 ) ;
#24830 = EDGE_CURVE ( 'NONE', #51736, #176751, #244750, .T. ) ;
#24831 = CARTESIAN_POINT ( 'NONE',  ( -18.40000000000000213, 64.51332499825412015, -78.77310748452438816 ) ) ;
#24832 = AXIS2_PLACEMENT_3D ( 'NONE', #58885, #21101, #138420 ) ;
#24833 = EDGE_LOOP ( 'NONE', ( #6944, #251897, #2346, #234155 ) ) ;
#24834 = VERTEX_POINT ( 'NONE', #144366 ) ;
#24835 = ORIENTED_EDGE ( 'NONE', *, *, #37352, .T. ) ;
#24836 = ADVANCED_FACE ( 'NONE', ( #220089 ), #201193, .T. ) ;
#24837 = CARTESIAN_POINT ( 'NONE',  ( -20.90000000000000213, 6.356682116888462630, 11.91686199900910381 ) ) ;
#24838 = ORIENTED_EDGE ( 'NONE', *, *, #219789, .T. ) ;
#24840 = EDGE_LOOP ( 'NONE', ( #53075, #107350, #136682, #35365 ) ) ;
#24839 = CARTESIAN_POINT ( 'NONE',  ( -21.05000000000000071, 5.900000000011102586, -177.7190997646563915 ) ) ;
#24841 = EDGE_CURVE ( 'NONE', #250992, #129355, #30526, .T. ) ;
#24842 = ORIENTED_EDGE ( 'NONE', *, *, #161503, .T. ) ;
#24843 = CIRCLE ( 'NONE', #132984, 0.09999999999999854838 ) ;
#24846 = EDGE_LOOP ( 'NONE', ( #160640, #23039, #104951, #127790, #218200, #28777, #194708, #108388, #150183, #46639, #14090, #237592, #40136, #86424 ) ) ;
#24845 = ORIENTED_EDGE ( 'NONE', *, *, #187643, .T. ) ;
#24844 = CARTESIAN_POINT ( 'NONE',  ( -16.77977881697927032, 9.946601933544062746, -113.1613785731150870 ) ) ;
#24847 = VECTOR ( 'NONE', #18402, 1000.000000000000000 ) ;
#24848 = CARTESIAN_POINT ( 'NONE',  ( -20.85000000000000142, 77.26327546522863088, -28.12124281777790813 ) ) ;
#24850 = ADVANCED_FACE ( 'NONE', ( #41473 ), #200520, .T. ) ;
#24849 = ORIENTED_EDGE ( 'NONE', *, *, #184261, .T. ) ;
#24851 = CARTESIAN_POINT ( 'NONE',  ( -18.59999999999999787, 68.87972903831379767, -32.36354444268504693 ) ) ;
#24852 = B_SPLINE_CURVE_WITH_KNOTS ( 'NONE', 3,
 ( #86926, #166522, #50368, #227741, #187356, #8704 ),
 .UNSPECIFIED., .F., .F.,
 ( 4, 2, 4 ),
 ( 0.000000000000000000, 0.0001496588209255877576, 0.0002993176418511755152 ),
 .UNSPECIFIED. ) ;
#24853 = AXIS2_PLACEMENT_3D ( 'NONE', #98272, #218236, #80001 ) ;
#24854 = CARTESIAN_POINT ( 'NONE',  ( 20.95429402530550433, 67.12380584891043611, -195.0000207865866173 ) ) ;
#24855 = DIRECTION ( 'NONE',  ( 0.000000000000000000, -6.467318590049456648E-15, 1.000000000000000000 ) ) ;
#24856 = ORIENTED_EDGE ( 'NONE', *, *, #110927, .T. ) ;
#24857 = FACE_OUTER_BOUND ( 'NONE', #181639, .T. ) ;
#24859 = VERTEX_POINT ( 'NONE', #221342 ) ;
#24858 = LINE ( 'NONE', #249028, #219976 ) ;
#24860 = CARTESIAN_POINT ( 'NONE',  ( -16.80438519320023616, 9.949779096479501206, -180.1507382809212743 ) ) ;
#24862 = ORIENTED_EDGE ( 'NONE', *, *, #207836, .T. ) ;
#24861 = CARTESIAN_POINT ( 'NONE',  ( -20.94999999999999929, 44.09392520544991356, -258.8097135244738638 ) ) ;
#24863 = EDGE_CURVE ( 'NONE', #218506, #176897, #185656, .T. ) ;
#24864 = VERTEX_POINT ( 'NONE', #210788 ) ;
#24865 = VERTEX_POINT ( 'NONE', #109106 ) ;
#24866 = ORIENTED_EDGE ( 'NONE', *, *, #143309, .T. ) ;
#24867 = AXIS2_PLACEMENT_3D ( 'NONE', #157541, #80485, #76665 ) ;
#24868 = DIRECTION ( 'NONE',  ( 0.000000000000000000, 0.000000000000000000, -1.000000000000000000 ) ) ;
#24869 = DIRECTION ( 'NONE',  ( 0.000000000000000000, 1.000000000000000000, -1.224646799147353207E-16 ) ) ;
#24871 = VERTEX_POINT ( 'NONE', #107836 ) ;
#24870 = EDGE_LOOP ( 'NONE', ( #218649, #218131, #124842, #171679 ) ) ;
#24872 = ORIENTED_EDGE ( 'NONE', *, *, #248413, .T. ) ;
#24873 = DIRECTION ( 'NONE',  ( -1.073024830501117725E-15, 0.000000000000000000, 1.000000000000000000 ) ) ;
#24874 = ORIENTED_EDGE ( 'NONE', *, *, #120389, .T. ) ;
#24875 = VERTEX_POINT ( 'NONE', #145667 ) ;
#24876 = CARTESIAN_POINT ( 'NONE',  ( 18.50000000000000000, 85.40000000001239755, -163.1410656363516125 ) ) ;
#24878 = EDGE_LOOP ( 'NONE', ( #180737, #93788, #64240, #17542 ) ) ;
#24877 = DIRECTION ( 'NONE',  ( 0.000000000000000000, 0.2128009952263485993, -0.9770955615653341697 ) ) ;
#24879 = FACE_OUTER_BOUND ( 'NONE', #2685, .T. ) ;
#24881 = CARTESIAN_POINT ( 'NONE',  ( 18.48536876927967754, -9.463527249856181101, -107.5486182650831495 ) ) ;
#24880 = CARTESIAN_POINT ( 'NONE',  ( -16.91247567987037215, 22.96360194920584163, -230.9170109094160068 ) ) ;
#24882 = EDGE_CURVE ( 'NONE', #22560, #38351, #47052, .T. ) ;
#24883 = ORIENTED_EDGE ( 'NONE', *, *, #757, .F. ) ;
#24885 = EDGE_LOOP ( 'NONE', ( #94883, #113306, #39417, #158944 ) ) ;
#24884 = EDGE_LOOP ( 'NONE', ( #87712, #84736, #46534, #88040 ) ) ;
#24886 = CARTESIAN_POINT ( 'NONE',  ( -18.59999999999999787, 14.05000000001115623, -173.0136950707609458 ) ) ;
#24887 = CARTESIAN_POINT ( 'NONE',  ( 18.69999999999999574, -9.749999999999994671, 30.09999999999999076 ) ) ;
#24888 = VECTOR ( 'NONE', #2415, 1000.000000000000000 ) ;
#24889 = CIRCLE ( 'NONE', #187191, 3.999999999999999112 ) ;
#24890 = VERTEX_POINT ( 'NONE', #225192 ) ;
#24891 = EDGE_CURVE ( 'NONE', #2430, #159306, #34628, .T. ) ;
#24892 = AXIS2_PLACEMENT_3D ( 'NONE', #237281, #18231, #235977 ) ;
#24893 = EDGE_LOOP ( 'NONE', ( #100243, #234357, #70137, #172000 ) ) ;
#24894 = VERTEX_POINT ( 'NONE', #88244 ) ;
#24895 = FACE_OUTER_BOUND ( 'NONE', #77151, .T. ) ;
#24896 = ORIENTED_EDGE ( 'NONE', *, *, #17750, .F. ) ;
#24897 = CARTESIAN_POINT ( 'NONE',  ( 20.85000000000000142, 79.28756800457986742, -196.2274082906208434 ) ) ;
#24898 = CARTESIAN_POINT ( 'NONE',  ( 21.04999999999999716, 76.08561306081597309, -109.4368672183345836 ) ) ;
#24899 = VERTEX_POINT ( 'NONE', #46561 ) ;
#24900 = CARTESIAN_POINT ( 'NONE',  ( 20.94999999999999929, 70.15000000001198543, -113.1556047088022581 ) ) ;
#24902 = EDGE_CURVE ( 'NONE', #231942, #28671, #85664, .T. ) ;
#24901 = CARTESIAN_POINT ( 'NONE',  ( 23.15000000000000213, 85.00000000001222134, -146.4170766071767389 ) ) ;
#24904 = DIRECTION ( 'NONE',  ( 0.000000000000000000, -1.000000000000000000, -6.982962677686265922E-15 ) ) ;
#24903 = LINE ( 'NONE', #181406, #82098 ) ;
#24905 = DIRECTION ( 'NONE',  ( -0.7071067811865474617, 0.7071067811865474617, 4.937700262164531476E-15 ) ) ;
#24906 = DIRECTION ( 'NONE',  ( 1.000000000000000000, 0.000000000000000000, 0.000000000000000000 ) ) ;
#24907 = CARTESIAN_POINT ( 'NONE',  ( 21.14999999999999858, 64.25000000001156764, -57.37310748452440379 ) ) ;
#24908 = AXIS2_PLACEMENT_3D ( 'NONE', #145320, #185750, #144034 ) ;
#24909 = DIRECTION ( 'NONE',  ( 0.000000000000000000, -0.1455152366551721865, -0.9893560106964475187 ) ) ;
#24910 = EDGE_CURVE ( 'NONE', #20990, #129691, #7445, .T. ) ;
#24911 = ORIENTED_EDGE ( 'NONE', *, *, #12659, .T. ) ;
#24912 = CIRCLE ( 'NONE', #258067, 0.09999999999999939493 ) ;
#24914 = ORIENTED_EDGE ( 'NONE', *, *, #140895, .T. ) ;
#24913 = VERTEX_POINT ( 'NONE', #27051 ) ;
#24915 = VERTEX_POINT ( 'NONE', #169134 ) ;
#24916 = CARTESIAN_POINT ( 'NONE',  ( -17.11825945287482753, 10.05000000001113847, -79.65000000000004832 ) ) ;
#24917 = ADVANCED_FACE ( 'NONE', ( #128698 ), #106528, .T. ) ;
#24919 = LINE ( 'NONE', #186551, #257158 ) ;
#24918 = PLANE ( 'NONE',  #95315 ) ;
#24920 = CARTESIAN_POINT ( 'NONE',  ( -21.11927991906891222, 75.99091632053830381, -142.9716006030158155 ) ) ;
#24921 = VERTEX_POINT ( 'NONE', #148245 ) ;
#24922 = EDGE_CURVE ( 'NONE', #187354, #206992, #22156, .T. ) ;
#24923 = CARTESIAN_POINT ( 'NONE',  ( -20.94403535211772294, 10.30632246271647467, -106.0041836778896283 ) ) ;
#24924 = EDGE_CURVE ( 'NONE', #27371, #155708, #192838, .T. ) ;
#24925 = DIRECTION ( 'NONE',  ( 1.000000000000000000, 0.000000000000000000, -0.000000000000000000 ) ) ;
#24926 = LINE ( 'NONE', #62750, #218143 ) ;
#24927 = DIRECTION ( 'NONE',  ( 0.000000000000000000, 6.982962677686266711E-15, -1.000000000000000000 ) ) ;
#24928 = ORIENTED_EDGE ( 'NONE', *, *, #138984, .F. ) ;
#24929 = CIRCLE ( 'NONE', #203780, 0.1000000000000028644 ) ;
#24930 = CARTESIAN_POINT ( 'NONE',  ( 18.46858270002952551, -9.474202674710566541, -7.102021934703857120 ) ) ;
#24931 = EDGE_CURVE ( 'NONE', #99200, #256904, #1264, .T. ) ;
#24932 = FACE_OUTER_BOUND ( 'NONE', #182929, .T. ) ;
#24933 = ORIENTED_EDGE ( 'NONE', *, *, #124110, .T. ) ;
#24934 = FACE_OUTER_BOUND ( 'NONE', #175623, .T. ) ;
#24935 = DIRECTION ( 'NONE',  ( -1.000000000000000000, -0.000000000000000000, -0.000000000000000000 ) ) ;
#24936 = AXIS2_PLACEMENT_3D ( 'NONE', #142562, #23942, #83842 ) ;
#24937 = DIRECTION ( 'NONE',  ( 1.000000000000000000, 0.000000000000000000, 0.000000000000000000 ) ) ;
#24938 = EDGE_CURVE ( 'NONE', #187424, #206683, #225373, .T. ) ;
#24939 = CARTESIAN_POINT ( 'NONE',  ( 20.95512820512820440, 67.12384868372348024, -60.96447848938343839 ) ) ;
#24940 = LINE ( 'NONE', #44493, #94140 ) ;
#24941 = ADVANCED_FACE ( 'NONE', ( #146944 ), #206942, .T. ) ;
#24942 = DIRECTION ( 'NONE',  ( -1.000000000000000000, -0.000000000000000000, -0.000000000000000000 ) ) ;
#24943 = VERTEX_POINT ( 'NONE', #127408 ) ;
#24944 = DIRECTION ( 'NONE',  ( 1.000000000000000000, 2.952720810173289112E-16, -0.000000000000000000 ) ) ;
#24945 = DIRECTION ( 'NONE',  ( 0.7071067811865475727, -0.7071067811865475727, 0.000000000000000000 ) ) ;
#24946 = CARTESIAN_POINT ( 'NONE',  ( -21.05000000000000071, -0.02110330804785563383, -60.69548367073601725 ) ) ;
#24948 = CARTESIAN_POINT ( 'NONE',  ( -20.54999999999999716, -8.999999999988846255, -42.89396912265245021 ) ) ;
#24947 = FACE_OUTER_BOUND ( 'NONE', #217778, .T. ) ;
#24949 = CARTESIAN_POINT ( 'NONE',  ( -18.58735405345342429, 85.56647862034900243, -163.2003928382583808 ) ) ;
#24950 = CARTESIAN_POINT ( 'NONE',  ( 21.13461538461538325, 67.11458296203782936, -157.6731074845244223 ) ) ;
#24951 = CARTESIAN_POINT ( 'NONE',  ( -22.94999999999999929, 1.786320531569725478, -11.50977166988710820 ) ) ;
#24952 = CARTESIAN_POINT ( 'NONE',  ( 23.25000000000000000, 84.59626168225447884, -45.47323500167454569 ) ) ;
#24953 = AXIS2_PLACEMENT_3D ( 'NONE', #70575, #1252, #116098 ) ;
#24955 = ORIENTED_EDGE ( 'NONE', *, *, #144634, .T. ) ;
#24954 = DIRECTION ( 'NONE',  ( 0.000000000000000000, 0.000000000000000000, 1.000000000000000000 ) ) ;
#24956 = VECTOR ( 'NONE', #91103, 1000.000000000000000 ) ;
#24957 = EDGE_CURVE ( 'NONE', #197965, #86957, #196350, .T. ) ;
#24958 = CIRCLE ( 'NONE', #108708, 0.2000000000000057288 ) ;
#24959 = EDGE_CURVE ( 'NONE', #206404, #183689, #180354, .T. ) ;
#24960 = AXIS2_PLACEMENT_3D ( 'NONE', #38412, #150989, #217027 ) ;
#24961 = VECTOR ( 'NONE', #114822, 1000.000000000000000 ) ;
#24962 = CARTESIAN_POINT ( 'NONE',  ( 23.14999999999998437, 76.00000000001267608, -203.5231074845243597 ) ) ;
#24963 = ADVANCED_FACE ( 'NONE', ( #118105 ), #18032, .F. ) ;
#24964 = CYLINDRICAL_SURFACE ( 'NONE', #71358, 12.87499999999999467 ) ;
#24965 = FACE_OUTER_BOUND ( 'NONE', #169317, .T. ) ;
#24966 = ORIENTED_EDGE ( 'NONE', *, *, #132005, .T. ) ;
#24967 = AXIS2_PLACEMENT_3D ( 'NONE', #46387, #23023, #183361 ) ;
#24968 = SPHERICAL_SURFACE ( 'NONE', #180507, 0.1000000000000000056 ) ;
#24969 = AXIS2_PLACEMENT_3D ( 'NONE', #22806, #102272, #82710 ) ;
#24970 = CIRCLE ( 'NONE', #225008, 0.5000000000000014433 ) ;
#24971 = DIRECTION ( 'NONE',  ( -1.000000000000000000, 0.000000000000000000, 0.000000000000000000 ) ) ;
#24972 = DIRECTION ( 'NONE',  ( 0.000000000000000000, -0.2617529984165152257, -0.9651348961777124202 ) ) ;
#24973 = TOROIDAL_SURFACE ( 'NONE', #174844, 11.65000000000000036, 0.1000000000000000056 ) ;
#24974 = AXIS2_PLACEMENT_3D ( 'NONE', #171981, #251465, #72872 ) ;
#24975 = ORIENTED_EDGE ( 'NONE', *, *, #37800, .T. ) ;
#24976 = DIRECTION ( 'NONE',  ( -1.000000000000000000, -0.000000000000000000, -0.000000000000000000 ) ) ;
#24978 = ORIENTED_EDGE ( 'NONE', *, *, #69913, .T. ) ;
#24977 = DIRECTION ( 'NONE',  ( -0.000000000000000000, -0.000000000000000000, -1.000000000000000000 ) ) ;
#24979 = CARTESIAN_POINT ( 'NONE',  ( -16.79140778683509794, 66.05505840115722549, -82.19337025075358838 ) ) ;
#24980 = CIRCLE ( 'NONE', #178930, 0.1000000000000108025 ) ;
#24981 = DIRECTION ( 'NONE',  ( 0.000000000000000000, 0.000000000000000000, 1.000000000000000000 ) ) ;
#24982 = VERTEX_POINT ( 'NONE', #192511 ) ;
#24983 = LINE ( 'NONE', #124072, #171963 ) ;
#24984 = ADVANCED_FACE ( 'NONE', ( #17703 ), #72581, .F. ) ;
#24985 = CARTESIAN_POINT ( 'NONE',  ( -22.39999999999999858, 55.86476422312859569, -232.8760422647022494 ) ) ;
#24986 = CARTESIAN_POINT ( 'NONE',  ( 21.05000000000000071, 67.22371710471961137, -127.9644784893834100 ) ) ;
#24987 = EDGE_LOOP ( 'NONE', ( #244915, #6202, #233455, #229139 ) ) ;
#24989 = EDGE_CURVE ( 'NONE', #150875, #150463, #126366, .T. ) ;
#24988 = DIRECTION ( 'NONE',  ( -1.000000000000000000, 3.265361837132813093E-16, 2.280189983783949500E-30 ) ) ;
#24990 = DIRECTION ( 'NONE',  ( -2.940209281316621016E-16, -1.000000000000000000, -9.408669700213187250E-15 ) ) ;
#24991 = EDGE_CURVE ( 'NONE', #216036, #44045, #55411, .T. ) ;
#24992 = CARTESIAN_POINT ( 'NONE',  ( -21.64999999999999858, 68.75000000001199396, -115.2731074845243455 ) ) ;
#24993 = EDGE_CURVE ( 'NONE', #5675, #72740, #167908, .T. ) ;
#24994 = CARTESIAN_POINT ( 'NONE',  ( -23.15000000000000213, 74.00000000001205080, -123.2984855617622060 ) ) ;
#24995 = ORIENTED_EDGE ( 'NONE', *, *, #33509, .T. ) ;
#24996 = ORIENTED_EDGE ( 'NONE', *, *, #152647, .F. ) ;
#24997 = EDGE_CURVE ( 'NONE', #152757, #936, #153429, .T. ) ;
#24998 = DIRECTION ( 'NONE',  ( 1.000000000000000000, 0.000000000000000000, 0.000000000000000000 ) ) ;
#24999 = VECTOR ( 'NONE', #118418, 1000.000000000000000 ) ;
#25000 = LINE ( 'NONE', #1544, #19380 ) ;
#25001 = CARTESIAN_POINT ( 'NONE',  ( -21.14999999999999858, 76.00000000001267608, -203.5231074845243597 ) ) ;
#25002 = CARTESIAN_POINT ( 'NONE',  ( -21.05000000000000071, -1.249999999988843369, -142.0000000000000284 ) ) ;
#25003 = CARTESIAN_POINT ( 'NONE',  ( -18.40000000000000213, 11.41458325961093756, -79.65000000000004832 ) ) ;
#25004 = AXIS2_PLACEMENT_3D ( 'NONE', #256944, #220453, #142181 ) ;
#25006 = FACE_OUTER_BOUND ( 'NONE', #50276, .T. ) ;
#25005 = CARTESIAN_POINT ( 'NONE',  ( -16.80100426158789872, 12.41435172007160403, -211.2765376762438052 ) ) ;
#25007 = DIRECTION ( 'NONE',  ( 2.952720810173289112E-16, 1.000000000000000000, 6.938893903907229955E-15 ) ) ;
#25008 = CARTESIAN_POINT ( 'NONE',  ( -22.59999999999999787, 12.61936297652653316, -223.3443501630868298 ) ) ;
#25009 = CARTESIAN_POINT ( 'NONE',  ( -20.64999999999999858, 7.250000000011155521, -155.1500000000000057 ) ) ;
#25010 = LINE ( 'NONE', #124102, #218943 ) ;
#25011 = CIRCLE ( 'NONE', #195883, 0.1999999999999987899 ) ;
#25012 = EDGE_CURVE ( 'NONE', #153832, #15171, #52987, .T. ) ;
#25014 = ORIENTED_EDGE ( 'NONE', *, *, #85453, .T. ) ;
#25013 = DIRECTION ( 'NONE',  ( -0.000000000000000000, -0.000000000000000000, 1.000000000000000000 ) ) ;
#25015 = CARTESIAN_POINT ( 'NONE',  ( -21.14999999893415250, 64.25000000001209344, -129.6786121409976715 ) ) ;
#25016 = ADVANCED_FACE ( 'NONE', ( #155975 ), #97099, .T. ) ;
#25017 = DIRECTION ( 'NONE',  ( 1.000000000000000000, 0.000000000000000000, 0.000000000000000000 ) ) ;
#25019 = SPHERICAL_SURFACE ( 'NONE', #57613, 0.1000000000000000056 ) ;
#25018 = CARTESIAN_POINT ( 'NONE',  ( 20.94999999999999929, 54.32225538558144962, -236.1594012422037281 ) ) ;
#25020 = VERTEX_POINT ( 'NONE', #176813 ) ;
#25021 = CARTESIAN_POINT ( 'NONE',  ( -16.87683809663752754, 66.13411015068078314, -56.25568067745533796 ) ) ;
#25023 = ADVANCED_FACE ( 'NONE', ( #172988 ), #77670, .F. ) ;
#25022 = CARTESIAN_POINT ( 'NONE',  ( -17.71734398241073905, 10.84235722847571814, -110.7748617469944605 ) ) ;
#25024 = DIRECTION ( 'NONE',  ( 0.000000000000000000, 0.000000000000000000, -1.000000000000000000 ) ) ;
#25025 = CARTESIAN_POINT ( 'NONE',  ( -20.85000000000000142, -1.851617760457748618, -78.60318971960367662 ) ) ;
#25026 = DIRECTION ( 'NONE',  ( 1.000000000000000000, 0.000000000000000000, 0.000000000000000000 ) ) ;
#25027 = VERTEX_POINT ( 'NONE', #213339 ) ;
#25029 = ORIENTED_EDGE ( 'NONE', *, *, #4331, .F. ) ;
#25028 = AXIS2_PLACEMENT_3D ( 'NONE', #129843, #209390, #230239 ) ;
#25030 = LINE ( 'NONE', #122839, #226011 ) ;
#25031 = ORIENTED_EDGE ( 'NONE', *, *, #220105, .T. ) ;
#25032 = FACE_OUTER_BOUND ( 'NONE', #140293, .T. ) ;
#25033 = ADVANCED_FACE ( 'NONE', ( #34744 ), #174280, .F. ) ;
#25035 = EDGE_CURVE ( 'NONE', #195135, #201670, #188355, .T. ) ;
#25034 = AXIS2_PLACEMENT_3D ( 'NONE', #105993, #220823, #46037 ) ;
#25036 = ORIENTED_EDGE ( 'NONE', *, *, #22759, .F. ) ;
#25037 = CARTESIAN_POINT ( 'NONE',  ( -18.40000000000000213, 64.52132590001188817, -78.79780070086499677 ) ) ;
#25038 = FACE_OUTER_BOUND ( 'NONE', #219925, .T. ) ;
#25039 = EDGE_CURVE ( 'NONE', #94857, #238735, #51318, .T. ) ;
#25040 = LINE ( 'NONE', #182832, #147141 ) ;
#25041 = ORIENTED_EDGE ( 'NONE', *, *, #193395, .T. ) ;
#25042 =( BOUNDED_CURVE ( )  B_SPLINE_CURVE ( 3, ( #246374, #26054, #185114, #145974 ),
 .UNSPECIFIED., .F., .F. ) 
 B_SPLINE_CURVE_WITH_KNOTS ( ( 4, 4 ),
 ( 3.752122642744639691, 4.712388980384671022 ),
 .UNSPECIFIED. ) 
 CURVE ( )  GEOMETRIC_REPRESENTATION_ITEM ( )  RATIONAL_B_SPLINE_CURVE ( ( 1.000000000000000000, 0.9246222802177307409, 0.9246222802177307409, 1.000000000000000000 ) ) 
 REPRESENTATION_ITEM ( '' )  );
#25043 = EDGE_CURVE ( 'NONE', #160911, #31617, #109784, .T. ) ;
#25044 = CARTESIAN_POINT ( 'NONE',  ( 20.94999999999999574, 79.33069327855442054, -236.1318330389568985 ) ) ;
#25045 = CARTESIAN_POINT ( 'NONE',  ( 22.14074124539698829, 68.60992214896839414, -136.6221603803684275 ) ) ;
#25046 = EDGE_CURVE ( 'NONE', #67597, #196307, #101050, .T. ) ;
#25047 = CARTESIAN_POINT ( 'NONE',  ( 23.25000000000000000, -11.64999999998883595, -155.7499999999999716 ) ) ;
#25048 = DIRECTION ( 'NONE',  ( -0.7071067811865462405, -0.6909108974501250167, -0.1504730267678050515 ) ) ;
#25049 = FACE_OUTER_BOUND ( 'NONE', #170476, .T. ) ;
#25051 = AXIS2_PLACEMENT_3D ( 'NONE', #220700, #42082, #103290 ) ;
#25050 = CARTESIAN_POINT ( 'NONE',  ( -18.59999999999999787, -10.64999999999999325, 32.89999999999999858 ) ) ;
#25052 = AXIS2_PLACEMENT_3D ( 'NONE', #53926, #210450, #190904 ) ;
#25053 = DIRECTION ( 'NONE',  ( 1.000000000000000000, 0.000000000000000000, -0.000000000000000000 ) ) ;
#25054 = ORIENTED_EDGE ( 'NONE', *, *, #183512, .T. ) ;
#25056 = LINE ( 'NONE', #62868, #86777 ) ;
#25055 = DIRECTION ( 'NONE',  ( 0.000000000000000000, 0.000000000000000000, -1.000000000000000000 ) ) ;
#25057 = EDGE_LOOP ( 'NONE', ( #229854, #5160, #239264, #128705 ) ) ;
#25059 = ORIENTED_EDGE ( 'NONE', *, *, #150494, .T. ) ;
#25058 = LINE ( 'NONE', #168448, #23333 ) ;
#25060 = ORIENTED_EDGE ( 'NONE', *, *, #89287, .T. ) ;
#25061 = FACE_OUTER_BOUND ( 'NONE', #78470, .T. ) ;
#25062 = CYLINDRICAL_SURFACE ( 'NONE', #88249, 0.09999999999999939493 ) ;
#25063 =( BOUNDED_SURFACE ( )  B_SPLINE_SURFACE ( 3, 2, ( 
 ( #110080, #84371, #33160 ),
 ( #12295, #91810, #171389 ),
 ( #124850, #63573, #72257 ),
 ( #163981, #143104, #112663 ) ),
 .UNSPECIFIED., .F., .F., .F. ) 
 B_SPLINE_SURFACE_WITH_KNOTS ( ( 4, 4 ),
 ( 3, 3 ),
 ( -3.469446951953614189E-18, 0.001979672783031532438 ),
 ( 0.000000000000000000, 1.000000000000000000 ),
 .UNSPECIFIED. ) 
 GEOMETRIC_REPRESENTATION_ITEM ( )  RATIONAL_B_SPLINE_SURFACE ( (
 ( 1.000000000000000000, 0.7103081912008384347, 1.000000000000000000),
 ( 1.000000000000000000, 0.7104998333558356638, 1.000000000000000000),
 ( 1.000000000000000000, 0.7107238315755363134, 1.000000000000000000),
 ( 1.000000000000000000, 0.7110073749539295163, 1.000000000000000000) ) ) 
 REPRESENTATION_ITEM ( '' )  SURFACE ( )  );
#25064 = LINE ( 'NONE', #220673, #242953 ) ;
#25065 = CARTESIAN_POINT ( 'NONE',  ( 18.79999999999999716, -1.212568896937008089, -7.900000000000000355 ) ) ;
#25066 = ORIENTED_EDGE ( 'NONE', *, *, #178440, .F. ) ;
#25067 = EDGE_CURVE ( 'NONE', #38015, #189087, #97276, .T. ) ;
#25068 = CARTESIAN_POINT ( 'NONE',  ( 21.30000000000002558, 76.00000000001213607, -136.5231074845242745 ) ) ;
#25069 = CARTESIAN_POINT ( 'NONE',  ( 23.24999999999999645, 76.00000000001195133, -103.0231074845243171 ) ) ;
#25070 = ORIENTED_EDGE ( 'NONE', *, *, #10542, .F. ) ;
#25071 = CARTESIAN_POINT ( 'NONE',  ( -20.89878130938411616, 10.32747123226657493, -39.07740328502492844 ) ) ;
#25072 = ADVANCED_FACE ( 'NONE', ( #218465 ), #159814, .T. ) ;
#25073 = CIRCLE ( 'NONE', #29177, 0.1000000000000040579 ) ;
#25074 = VECTOR ( 'NONE', #164731, 1000.000000000000000 ) ;
#25075 = TOROIDAL_SURFACE ( 'NONE', #129103, 14.20833333333334103, 0.1000000000000000056 ) ;
#25077 = CIRCLE ( 'NONE', #66749, 4.050000000000003375 ) ;
#25076 = CARTESIAN_POINT ( 'NONE',  ( -20.94999999999999929, 87.48912529308798014, -100.1231074845242262 ) ) ;
#25078 = ORIENTED_EDGE ( 'NONE', *, *, #79689, .F. ) ;
#25079 = LINE ( 'NONE', #66751, #206069 ) ;
#25080 =( BOUNDED_SURFACE ( )  B_SPLINE_SURFACE ( 3, 2, ( 
 ( #155245, #153977, #35304 ),
 ( #194365, #254287, #234745 ),
 ( #56080, #135632, #156532 ),
 ( #236023, #1245, #83338 ) ),
 .UNSPECIFIED., .F., .F., .F. ) 
 B_SPLINE_SURFACE_WITH_KNOTS ( ( 4, 4 ),
 ( 3, 3 ),
 ( 0.3000847527772363410, 0.5552748953338753068 ),
 ( 0.000000000000000000, 1.000000000000000000 ),
 .UNSPECIFIED. ) 
 GEOMETRIC_REPRESENTATION_ITEM ( )  RATIONAL_B_SPLINE_SURFACE ( (
 ( 1.000000000000000000, 0.9152888060719485130, 1.000000000000000000),
 ( 1.000000000000000000, 0.9104333467450272943, 1.000000000000000000),
 ( 1.000000000000000000, 0.9035312726220733337, 1.000000000000000000),
 ( 1.000000000000000000, 0.8946697475932141597, 1.000000000000000000) ) ) 
 REPRESENTATION_ITEM ( '' )  SURFACE ( )  );
#25081 = ORIENTED_EDGE ( 'NONE', *, *, #163516, .T. ) ;
#25082 = VECTOR ( 'NONE', #128892, 1000.000000000000114 ) ;
#25083 = CARTESIAN_POINT ( 'NONE',  ( -20.94999999999999929, 0.6656436123793473270, -212.6810495496487476 ) ) ;
#25084 = ORIENTED_EDGE ( 'NONE', *, *, #83187, .F. ) ;
#25085 = FACE_OUTER_BOUND ( 'NONE', #115869, .T. ) ;
#25086 = ADVANCED_FACE ( 'NONE', ( #141512 ), #72400, .F. ) ;
#25087 = CARTESIAN_POINT ( 'NONE',  ( -20.64999999999999858, 76.00000000001142553, -36.02310748452432421 ) ) ;
#25088 = CARTESIAN_POINT ( 'NONE',  ( 18.49999999999998934, 8.433899723187009201, -209.4150263691077782 ) ) ;
#25089 = DIRECTION ( 'NONE',  ( 0.000000000000000000, 0.000000000000000000, -1.000000000000000000 ) ) ;
#25090 = AXIS2_PLACEMENT_3D ( 'NONE', #234049, #252318, #110252 ) ;
#25091 = AXIS2_PLACEMENT_3D ( 'NONE', #135177, #204136, #105001 ) ;
#25092 = CARTESIAN_POINT ( 'NONE',  ( -20.64999999999999858, -8.999999999988846255, -76.39396912265249284 ) ) ;
#25094 = EDGE_CURVE ( 'NONE', #76299, #42612, #39877, .T. ) ;
#25093 = CARTESIAN_POINT ( 'NONE',  ( -23.25000000000000000, 1.115600667400684642E-11, -67.00000000000000000 ) ) ;
#25095 = DIRECTION ( 'NONE',  ( 0.000000000000000000, 0.000000000000000000, -1.000000000000000000 ) ) ;
#25096 = VERTEX_POINT ( 'NONE', #1990 ) ;
#25098 = DIRECTION ( 'NONE',  ( 0.000000000000000000, -0.9126074666063660468, -0.4088369013363524762 ) ) ;
#25097 = CARTESIAN_POINT ( 'NONE',  ( -21.05000000000000071, 69.50298221358124806, -170.0085617939582505 ) ) ;
#25099 = ORIENTED_EDGE ( 'NONE', *, *, #36101, .T. ) ;
#25100 = CARTESIAN_POINT ( 'NONE',  ( -18.49513951962167368, 85.43772502669008873, -163.2450349094951321 ) ) ;
#25101 = DIRECTION ( 'NONE',  ( 1.000000000000000000, 0.000000000000000000, 0.000000000000000000 ) ) ;
#25103 = ORIENTED_EDGE ( 'NONE', *, *, #129431, .T. ) ;
#25102 = CARTESIAN_POINT ( 'NONE',  ( -23.15000000000000213, -9.000000000000001776, -23.60603087734756045 ) ) ;
#25105 = ORIENTED_EDGE ( 'NONE', *, *, #128872, .T. ) ;
#25104 = CARTESIAN_POINT ( 'NONE',  ( 20.94999999999999574, -11.41227409413852989, -69.90000000000004832 ) ) ;
#25106 = DIRECTION ( 'NONE',  ( 0.000000000000000000, -6.982962677686266711E-15, 1.000000000000000000 ) ) ;
#25107 = CARTESIAN_POINT ( 'NONE',  ( 21.07928932188134397, 0.09889514565439641580, 6.328516656393307294 ) ) ;
#25108 = CARTESIAN_POINT ( 'NONE',  ( -18.59999999999999787, 1.115600667400684642E-11, -67.00000000000004263 ) ) ;
#25109 = DIRECTION ( 'NONE',  ( 3.265361837132813093E-16, 0.9651348961777157509, -0.2617529984165031243 ) ) ;
#25111 = ORIENTED_EDGE ( 'NONE', *, *, #236449, .T. ) ;
#25110 = CARTESIAN_POINT ( 'NONE',  ( 21.05000005001280172, 67.12872030824209446, -157.8451598962784317 ) ) ;
#25112 = CIRCLE ( 'NONE', #199891, 0.5000000000000004441 ) ;
#25113 = CARTESIAN_POINT ( 'NONE',  ( 21.05000000000000071, -1.360870587180885716, -41.57299792709095954 ) ) ;
#25114 = ORIENTED_EDGE ( 'NONE', *, *, #233140, .T. ) ;
#25115 = ORIENTED_EDGE ( 'NONE', *, *, #234676, .F. ) ;
#25116 = CARTESIAN_POINT ( 'NONE',  ( -2.995603634470884209E-16, 6.650000000011155876, -54.75000000000000000 ) ) ;
#25117 = CARTESIAN_POINT ( 'NONE',  ( -20.64999999999999858, 20.06933876993645782, -235.7297789824848451 ) ) ;
#25118 = ORIENTED_EDGE ( 'NONE', *, *, #194218, .T. ) ;
#25119 = DIRECTION ( 'NONE',  ( 0.000000000000000000, 0.000000000000000000, -1.000000000000000000 ) ) ;
#25120 = EDGE_CURVE ( 'NONE', #106745, #200735, #18225, .T. ) ;
#25121 = DIRECTION ( 'NONE',  ( 1.000000000000000000, 0.000000000000000000, -0.000000000000000000 ) ) ;
#25122 = ORIENTED_EDGE ( 'NONE', *, *, #122800, .F. ) ;
#25123 = CARTESIAN_POINT ( 'NONE',  ( -2.995603634470891112E-16, 69.35000000001151932, -48.37310748452436826 ) ) ;
#25124 = CIRCLE ( 'NONE', #58217, 7.791421356237317575 ) ;
#25125 = LINE ( 'NONE', #189003, #192981 ) ;
#25126 = B_SPLINE_CURVE_WITH_KNOTS ( 'NONE', 3,
 ( #212727, #35402, #174931, #131893 ),
 .UNSPECIFIED., .F., .F.,
 ( 4, 4 ),
 ( 0.000000000000000000, 0.001767853679387140298 ),
 .UNSPECIFIED. ) ;
#25127 = ORIENTED_EDGE ( 'NONE', *, *, #16654, .F. ) ;
#25128 = ORIENTED_EDGE ( 'NONE', *, *, #129878, .T. ) ;
#25129 = DIRECTION ( 'NONE',  ( 1.000000000000000000, 0.000000000000000000, 0.000000000000000000 ) ) ;
#25130 = AXIS2_PLACEMENT_3D ( 'NONE', #141355, #4402, #163491 ) ;
#25131 = ORIENTED_EDGE ( 'NONE', *, *, #200286, .F. ) ;
#25132 = EDGE_CURVE ( 'NONE', #139340, #114526, #251447, .T. ) ;
#25133 = CYLINDRICAL_SURFACE ( 'NONE', #129629, 0.1000000000000033362 ) ;
#25134 = ORIENTED_EDGE ( 'NONE', *, *, #156333, .T. ) ;
#25136 = ORIENTED_EDGE ( 'NONE', *, *, #155118, .T. ) ;
#25135 = CARTESIAN_POINT ( 'NONE',  ( 22.39999999999999503, 7.790779598384535376, -167.4999999999999716 ) ) ;
#25137 = AXIS2_PLACEMENT_3D ( 'NONE', #183787, #121287, #5108 ) ;
#25139 = EDGE_CURVE ( 'NONE', #109188, #253865, #42282, .T. ) ;
#25138 = LINE ( 'NONE', #143763, #52741 ) ;
#25140 = ORIENTED_EDGE ( 'NONE', *, *, #71541, .F. ) ;
#25141 = DIRECTION ( 'NONE',  ( 1.000000000000000000, 0.000000000000000000, 0.000000000000000000 ) ) ;
#25142 = EDGE_LOOP ( 'NONE', ( #257027, #200407, #177844, #59229, #7583, #182004, #131561 ) ) ;
#25144 = VERTEX_POINT ( 'NONE', #4558 ) ;
#25143 = ORIENTED_EDGE ( 'NONE', *, *, #22225, .F. ) ;
#25145 = CARTESIAN_POINT ( 'NONE',  ( 21.05000000000000071, 69.52244781751869596, -136.4231075192252547 ) ) ;
#25146 = CARTESIAN_POINT ( 'NONE',  ( -18.79999999999999716, -8.150000000000005684, 33.00000000000000000 ) ) ;
#25148 = EDGE_CURVE ( 'NONE', #117008, #246109, #88934, .T. ) ;
#25147 = VERTEX_POINT ( 'NONE', #179383 ) ;
#25149 = AXIS2_PLACEMENT_3D ( 'NONE', #163481, #202606, #26554 ) ;
#25150 = VECTOR ( 'NONE', #16020, 1000.000000000000114 ) ;
#25151 = CIRCLE ( 'NONE', #58419, 0.09999999999998898659 ) ;
#25152 = CIRCLE ( 'NONE', #54159, 7.800000000000001599 ) ;
#25153 = EDGE_CURVE ( 'NONE', #37046, #257664, #76463, .T. ) ;
#25154 = EDGE_CURVE ( 'NONE', #9680, #211904, #138978, .T. ) ;
#25155 = ORIENTED_EDGE ( 'NONE', *, *, #150339, .T. ) ;
#25156 = FACE_OUTER_BOUND ( 'NONE', #153148, .T. ) ;
#25157 = FACE_OUTER_BOUND ( 'NONE', #114589, .T. ) ;
#25159 = EDGE_LOOP ( 'NONE', ( #84881, #227115, #173546, #234364 ) ) ;
#25158 = CARTESIAN_POINT ( 'NONE',  ( -18.50000000000000000, 11.65000000001115232, -146.1500000000000341 ) ) ;
#25160 = DIRECTION ( 'NONE',  ( 0.000000000000000000, -0.6410630849193120762, 0.7674881895858300940 ) ) ;
#25161 = ORIENTED_EDGE ( 'NONE', *, *, #38107, .T. ) ;
#25162 = EDGE_CURVE ( 'NONE', #171376, #255434, #218106, .T. ) ;
#25163 = DIRECTION ( 'NONE',  ( 1.000000000000000000, 2.952720810173289112E-16, -0.000000000000000000 ) ) ;
#25164 = DIRECTION ( 'NONE',  ( 0.000000000000000000, -7.172728831056617961E-15, 1.000000000000000000 ) ) ;
#25165 = ORIENTED_EDGE ( 'NONE', *, *, #78451, .T. ) ;
#25166 = CARTESIAN_POINT ( 'NONE',  ( -22.39999999999999858, 68.20922040163824818, -69.62310748452438247 ) ) ;
#25167 = CIRCLE ( 'NONE', #229345, 0.1000000000000028644 ) ;
#25168 = DIRECTION ( 'NONE',  ( 0.000000000000000000, -0.9651348961777157509, 0.2617529984165031243 ) ) ;
#25169 = EDGE_CURVE ( 'NONE', #7171, #183348, #105675, .T. ) ;
#25170 = ORIENTED_EDGE ( 'NONE', *, *, #254398, .T. ) ;
#25171 = DIRECTION ( 'NONE',  ( -1.000000000000000000, 0.000000000000000000, 0.000000000000000000 ) ) ;
#25172 = ORIENTED_EDGE ( 'NONE', *, *, #214869, .T. ) ;
#25174 = ORIENTED_EDGE ( 'NONE', *, *, #229030, .T. ) ;
#25173 = VERTEX_POINT ( 'NONE', #42416 ) ;
#25175 = ORIENTED_EDGE ( 'NONE', *, *, #10285, .F. ) ;
#25176 = LINE ( 'NONE', #100789, #40808 ) ;
#25177 = ORIENTED_EDGE ( 'NONE', *, *, #85815, .F. ) ;
#25178 = CARTESIAN_POINT ( 'NONE',  ( -17.11825945287481687, 66.05000000001153637, -48.77310748452439526 ) ) ;
#25179 = ORIENTED_EDGE ( 'NONE', *, *, #113169, .T. ) ;
#25180 = CARTESIAN_POINT ( 'NONE',  ( -23.15000000000000213, 71.75000000001186606, -90.77310748452434552 ) ) ;
#25181 = DIRECTION ( 'NONE',  ( 0.000000000000000000, -1.000000000000000000, -8.717686153663073805E-15 ) ) ;
#25182 = VECTOR ( 'NONE', #211439, 1000.000000000000000 ) ;
#25183 = EDGE_CURVE ( 'NONE', #152840, #37872, #188911, .T. ) ;
#25184 = EDGE_LOOP ( 'NONE', ( #234187, #81864, #42268, #175693, #4708, #230029, #158670, #130065 ) ) ;
#25185 = AXIS2_PLACEMENT_3D ( 'NONE', #7492, #183575, #105275 ) ;
#25186 = EDGE_LOOP ( 'NONE', ( #249833, #9952 ) ) ;
#25187 = ORIENTED_EDGE ( 'NONE', *, *, #54465, .F. ) ;
#25188 = AXIS2_PLACEMENT_3D ( 'NONE', #43720, #22899, #166271 ) ;
#25189 = EDGE_CURVE ( 'NONE', #109469, #84065, #222304, .T. ) ;
#25190 = FACE_OUTER_BOUND ( 'NONE', #68593, .T. ) ;
#25191 = EDGE_LOOP ( 'NONE', ( #196562, #92235, #201866, #40888 ) ) ;
#25192 = FACE_OUTER_BOUND ( 'NONE', #92816, .T. ) ;
#25193 = DIRECTION ( 'NONE',  ( -2.602085213965227050E-14, -0.9126074666063771490, -0.4088369013363281623 ) ) ;
#25194 = FACE_OUTER_BOUND ( 'NONE', #16589, .T. ) ;
#25195 = CARTESIAN_POINT ( 'NONE',  ( -23.15000000000000213, 87.41227409416143246, -72.52310748452423184 ) ) ;
#25196 = CARTESIAN_POINT ( 'NONE',  ( 21.05000000000000071, 5.850000000011156942, -190.8675027757220448 ) ) ;
#25197 = CARTESIAN_POINT ( 'NONE',  ( 22.39999999999999503, 11.75000000001116263, -33.60000000000000142 ) ) ;
#25198 = DIRECTION ( 'NONE',  ( 1.000000000000000000, 0.000000000000000000, 0.000000000000000000 ) ) ;
#25199 = AXIS2_PLACEMENT_3D ( 'NONE', #47915, #164035, #46621 ) ;
#25201 = DIRECTION ( 'NONE',  ( 0.000000000000000000, -0.8814952561688430555, 0.4721928772777346239 ) ) ;
#25200 = CARTESIAN_POINT ( 'NONE',  ( -16.80939487329395021, 66.05000000001224691, -149.1731074845235696 ) ) ;
#25202 = CARTESIAN_POINT ( 'NONE',  ( 23.14999999999999858, 2.100000000011158274, -134.0000000000000284 ) ) ;
#25203 = CARTESIAN_POINT ( 'NONE',  ( -18.79999999999999716, 0.000000000000000000, 32.89999999999999858 ) ) ;
#25204 = DIRECTION ( 'NONE',  ( 0.000000000000000000, 0.000000000000000000, -1.000000000000000000 ) ) ;
#25205 = DIRECTION ( 'NONE',  ( -2.602085213965226419E-14, -6.982962677686266711E-15, 1.000000000000000000 ) ) ;
#25206 = AXIS2_PLACEMENT_3D ( 'NONE', #250370, #151287, #230830 ) ;
#25207 = ORIENTED_EDGE ( 'NONE', *, *, #15947, .F. ) ;
#25208 = EDGE_CURVE ( 'NONE', #231547, #143070, #64544, .T. ) ;
#25209 = AXIS2_PLACEMENT_3D ( 'NONE', #54099, #181460, #193624 ) ;
#25210 = AXIS2_PLACEMENT_3D ( 'NONE', #88976, #250624, #205070 ) ;
#25212 = EDGE_LOOP ( 'NONE', ( #86945, #162648, #184139, #57728 ) ) ;
#25211 = FACE_OUTER_BOUND ( 'NONE', #7152, .T. ) ;
#25213 = VERTEX_POINT ( 'NONE', #230046 ) ;
#25214 = EDGE_CURVE ( 'NONE', #226065, #147930, #172390, .T. ) ;
#25215 = DIRECTION ( 'NONE',  ( 1.000000000000000000, 0.000000000000000000, 0.000000000000000000 ) ) ;
#25216 = CARTESIAN_POINT ( 'NONE',  ( 21.05000000000000071, 1.115600667400684642E-11, -200.9999999999999432 ) ) ;
#25217 = VERTEX_POINT ( 'NONE', #29318 ) ;
#25218 = EDGE_CURVE ( 'NONE', #35875, #121315, #176458, .T. ) ;
#25219 = EDGE_CURVE ( 'NONE', #37447, #75338, #46257, .T. ) ;
#25221 = AXIS2_PLACEMENT_3D ( 'NONE', #77759, #219850, #157356 ) ;
#25220 = CARTESIAN_POINT ( 'NONE',  ( 18.49999999999999289, 65.79142135624927334, -111.8731074845243683 ) ) ;
#25222 = AXIS2_PLACEMENT_3D ( 'NONE', #173631, #210145, #31532 ) ;
#25223 = DIRECTION ( 'NONE',  ( -1.000000000000000000, -0.000000000000000000, -0.000000000000000000 ) ) ;
#25224 = ORIENTED_EDGE ( 'NONE', *, *, #240691, .T. ) ;
#25225 = CARTESIAN_POINT ( 'NONE',  ( 22.39999999999999503, 1.115600667400684642E-11, -59.25000000000003553 ) ) ;
#25226 = DIRECTION ( 'NONE',  ( 0.000000000000000000, 0.9126074666063660468, 0.4088369013363524762 ) ) ;
#25227 = EDGE_CURVE ( 'NONE', #55518, #48144, #47236, .T. ) ;
#25228 = CARTESIAN_POINT ( 'NONE',  ( -16.97683809663752186, 9.850000000011137402, -180.9023640181964652 ) ) ;
#25230 = ORIENTED_EDGE ( 'NONE', *, *, #248462, .F. ) ;
#25229 = CARTESIAN_POINT ( 'NONE',  ( -16.92989143108097849, 66.05000000001230376, -157.1406236097677152 ) ) ;
#25231 = DIRECTION ( 'NONE',  ( 1.000000000000000000, 0.000000000000000000, 0.000000000000000000 ) ) ;
#25232 = ORIENTED_EDGE ( 'NONE', *, *, #81431, .T. ) ;
#25233 = DIRECTION ( 'NONE',  ( 1.000000000000000000, 0.000000000000000000, 0.000000000000000000 ) ) ;
#25234 = DIRECTION ( 'NONE',  ( 0.000000000000000000, 0.000000000000000000, -1.000000000000000000 ) ) ;
#25235 = ORIENTED_EDGE ( 'NONE', *, *, #161274, .T. ) ;
#25236 = CARTESIAN_POINT ( 'NONE',  ( -16.93226657140833069, 66.00045617728787306, -157.4443943735508071 ) ) ;
#25237 = DIRECTION ( 'NONE',  ( -1.652117596168391700E-15, -1.000000000000000000, 0.000000000000000000 ) ) ;
#25238 = VECTOR ( 'NONE', #56131, 1000.000000000000000 ) ;
#25241 = DIRECTION ( 'NONE',  ( -1.000000000000000000, -0.000000000000000000, -0.000000000000000000 ) ) ;
#25240 = CIRCLE ( 'NONE', #225106, 1.899999999999999023 ) ;
#25239 = DIRECTION ( 'NONE',  ( -1.000000000000000000, 3.265361837132813093E-16, 2.280189983783949500E-30 ) ) ;
#25242 = DIRECTION ( 'NONE',  ( 0.000000000000000000, -1.000000000000000000, 0.000000000000000000 ) ) ;
#25243 = LINE ( 'NONE', #166045, #90868 ) ;
#25244 = AXIS2_PLACEMENT_3D ( 'NONE', #41000, #141351, #241735 ) ;
#25246 = B_SPLINE_CURVE_WITH_KNOTS ( 'NONE', 3,
 ( #156723, #237519, #138381, #193257, #212821, #217919, #14633, #92851 ),
 .UNSPECIFIED., .F., .F.,
 ( 4, 2, 2, 4 ),
 ( 0.000000000000000000, 0.0002114466876442108679, 0.0003171700314663126563, 0.0004228933752884144175 ),
 .UNSPECIFIED. ) ;
#25245 = CARTESIAN_POINT ( 'NONE',  ( -18.40000000000000213, 11.48667500176882328, -143.2500000000000284 ) ) ;
#25247 = CARTESIAN_POINT ( 'NONE',  ( 21.05000000000000071, 76.00000000001195133, -103.0231074845243171 ) ) ;
#25248 = MANIFOLD_SOLID_BREP ( 'Stock-MAS-200-1', #140757 ) ;
#25249 = CYLINDRICAL_SURFACE ( 'NONE', #143366, 0.09999999999999854838 ) ;
#25250 = VERTEX_POINT ( 'NONE', #127091 ) ;
#25251 = CARTESIAN_POINT ( 'NONE',  ( -18.50000000000000000, 55.32469252163839712, -244.8004216010555183 ) ) ;
#25252 = ORIENTED_EDGE ( 'NONE', *, *, #29094, .T. ) ;
#25253 = ORIENTED_EDGE ( 'NONE', *, *, #32517, .T. ) ;
#25254 = CARTESIAN_POINT ( 'NONE',  ( -20.94560253601877164, 11.74999999999999645, -26.51008351251536865 ) ) ;
#25255 = FACE_OUTER_BOUND ( 'NONE', #76323, .T. ) ;
#25256 = EDGE_CURVE ( 'NONE', #126699, #201739, #69708, .T. ) ;
#25257 = ORIENTED_EDGE ( 'NONE', *, *, #79567, .F. ) ;
#25258 = EDGE_CURVE ( 'NONE', #233936, #189246, #222199, .T. ) ;
#25259 = AXIS2_PLACEMENT_3D ( 'NONE', #95805, #178939, #185323 ) ;
#25260 = ORIENTED_EDGE ( 'NONE', *, *, #205937, .F. ) ;
#25261 = EDGE_CURVE ( 'NONE', #132417, #27454, #10995, .T. ) ;
#25262 = ORIENTED_EDGE ( 'NONE', *, *, #138459, .F. ) ;
#25263 = LINE ( 'NONE', #65645, #37774 ) ;
#25264 = ORIENTED_EDGE ( 'NONE', *, *, #165682, .T. ) ;
#25265 = DIRECTION ( 'NONE',  ( 0.000000000000000000, -7.086529944415886769E-15, 1.000000000000000000 ) ) ;
#25266 = DIRECTION ( 'NONE',  ( 0.000000000000000000, -1.000000000000000000, 0.000000000000000000 ) ) ;
#25267 = CARTESIAN_POINT ( 'NONE',  ( 23.14999999999999503, 64.25000000001244871, -181.7731074845244450 ) ) ;
#25268 = DIRECTION ( 'NONE',  ( 0.000000000000000000, 0.000000000000000000, 1.000000000000000000 ) ) ;
#25269 = CARTESIAN_POINT ( 'NONE',  ( -22.50000000000000000, 1.115600667400684642E-11, -60.75000000000004974 ) ) ;
#25270 = CARTESIAN_POINT ( 'NONE',  ( -20.64999999999999858, 68.56901367119438362, -214.3038979092079046 ) ) ;
#25271 = DIRECTION ( 'NONE',  ( 0.000000000000000000, 1.000000000000000000, -0.000000000000000000 ) ) ;
#25273 = ORIENTED_EDGE ( 'NONE', *, *, #10052, .T. ) ;
#25272 = CARTESIAN_POINT ( 'NONE',  ( -21.05000000000000071, 0.000000000000000000, -29.50000000000000355 ) ) ;
#25275 = CARTESIAN_POINT ( 'NONE',  ( 18.59999999999999076, 64.25000000001202238, -114.7731074845243882 ) ) ;
#25274 = CARTESIAN_POINT ( 'NONE',  ( -21.05000000000000071, 88.41227409416184457, -139.4231074845242802 ) ) ;
#25277 = CARTESIAN_POINT ( 'NONE',  ( -21.46681500597872727, 76.00000000001170974, -76.38061864395214684 ) ) ;
#25276 = AXIS2_PLACEMENT_3D ( 'NONE', #160980, #243062, #202653 ) ;
#25278 = ORIENTED_EDGE ( 'NONE', *, *, #86129, .F. ) ;
#25279 = DIRECTION ( 'NONE',  ( 1.020425574104004196E-15, 1.210927747993693964E-31, -1.000000000000000000 ) ) ;
#25280 = DIRECTION ( 'NONE',  ( -1.000000000000000000, 0.000000000000000000, 0.000000000000000000 ) ) ;
#25281 = ORIENTED_EDGE ( 'NONE', *, *, #143257, .F. ) ;
#25282 = VECTOR ( 'NONE', #219946, 1000.000000000000000 ) ;
#25284 = DIRECTION ( 'NONE',  ( 0.000000000000000000, -0.9887567792719351711, 0.1495327102803594987 ) ) ;
#25283 = FACE_BOUND ( 'NONE', #225769, .T. ) ;
#25285 = AXIS2_PLACEMENT_3D ( 'NONE', #227420, #206580, #48784 ) ;
#25286 = EDGE_CURVE ( 'NONE', #227367, #201931, #20588, .T. ) ;
#25287 = CARTESIAN_POINT ( 'NONE',  ( -16.77431908686106610, 66.05419424549383223, -82.18726826687414189 ) ) ;
#25288 = ORIENTED_EDGE ( 'NONE', *, *, #79664, .F. ) ;
#25289 = DIRECTION ( 'NONE',  ( -1.000000000000000000, 0.000000000000000000, 0.000000000000000000 ) ) ;
#25290 = CARTESIAN_POINT ( 'NONE',  ( -18.59999999999999787, 63.76951449014745066, -212.8986194275075832 ) ) ;
#25292 = DIRECTION ( 'NONE',  ( 0.000000000000000000, -0.1350103645451807555, -0.9908441862701610203 ) ) ;
#25291 = AXIS2_PLACEMENT_3D ( 'NONE', #114408, #192669, #193955 ) ;
#25293 = EDGE_CURVE ( 'NONE', #172262, #155744, #213044, .T. ) ;
#25294 = FACE_BOUND ( 'NONE', #231470, .T. ) ;
#25295 = VERTEX_POINT ( 'NONE', #250879 ) ;
#25296 = VERTEX_POINT ( 'NONE', #231349 ) ;
#25297 = EDGE_CURVE ( 'NONE', #170273, #231806, #64014, .T. ) ;
#25298 = SPHERICAL_SURFACE ( 'NONE', #35956, 0.1000000000000000056 ) ;
#25299 = CARTESIAN_POINT ( 'NONE',  ( 21.15000000000005542, 74.16448838626246243, -47.52760213295649550 ) ) ;
#25300 = DIRECTION ( 'NONE',  ( 1.000000000000000000, 0.000000000000000000, 0.000000000000000000 ) ) ;
#25301 = CARTESIAN_POINT ( 'NONE',  ( 18.59999999999999076, 65.79142135624951493, -145.3731074845244109 ) ) ;
#25302 = ADVANCED_FACE ( 'NONE', ( #133511 ), #1458, .F. ) ;
#25303 = AXIS2_PLACEMENT_3D ( 'NONE', #139157, #58338, #178342 ) ;
#25304 = DIRECTION ( 'NONE',  ( -1.000000000000000000, -0.000000000000000000, -0.000000000000000000 ) ) ;
#25306 = FACE_OUTER_BOUND ( 'NONE', #43156, .T. ) ;
#25305 = CIRCLE ( 'NONE', #171083, 0.1999999999999996503 ) ;
#25307 = ORIENTED_EDGE ( 'NONE', *, *, #238884, .F. ) ;
#25308 = DIRECTION ( 'NONE',  ( 1.000000000000000000, 0.000000000000000000, 0.000000000000000000 ) ) ;
#25309 = EDGE_CURVE ( 'NONE', #193140, #68295, #134720, .T. ) ;
#25310 = CIRCLE ( 'NONE', #129534, 0.1000000000000028644 ) ;
#25312 = ORIENTED_EDGE ( 'NONE', *, *, #200995, .F. ) ;
#25311 = CARTESIAN_POINT ( 'NONE',  ( 21.12802099929860589, 8.780552590233368093, -179.7481899849315994 ) ) ;
#25313 = CARTESIAN_POINT ( 'NONE',  ( -21.05000000000000426, 6.440770893673126274, -33.51759718700845525 ) ) ;
#25315 = ADVANCED_FACE ( 'NONE', ( #192220 ), #172692, .T. ) ;
#25314 = EDGE_CURVE ( 'NONE', #162626, #112086, #171399, .T. ) ;
#25316 = CARTESIAN_POINT ( 'NONE',  ( 18.49999999999999289, 2.319530388122574394, -217.8268657444419887 ) ) ;
#25317 = FACE_OUTER_BOUND ( 'NONE', #191524, .T. ) ;
#25318 = AXIS2_PLACEMENT_3D ( 'NONE', #124070, #104462, #26253 ) ;
#25319 = DIRECTION ( 'NONE',  ( 0.000000000000000000, -0.1350103645451904977, -0.9908441862701596881 ) ) ;
#25320 = DIRECTION ( 'NONE',  ( 0.000000000000000000, 0.1686199900910313187, -0.9856811345164828708 ) ) ;
#25322 = ORIENTED_EDGE ( 'NONE', *, *, #184216, .T. ) ;
#25321 = CARTESIAN_POINT ( 'NONE',  ( -20.94999999999999929, 68.22930980752001062, -227.7331931781284879 ) ) ;
#25323 = DIRECTION ( 'NONE',  ( -2.489438768765009500E-17, 0.1686199900910313187, -0.9856811345164828708 ) ) ;
#25324 = CARTESIAN_POINT ( 'NONE',  ( 21.07888907270776002, 10.72506921352637654, -179.7211935868331807 ) ) ;
#25325 = SPHERICAL_SURFACE ( 'NONE', #1248, 0.1000000000000000056 ) ;
#25326 = CYLINDRICAL_SURFACE ( 'NONE', #178135, 0.09999999999999181766 ) ;
#25327 = AXIS2_PLACEMENT_3D ( 'NONE', #187340, #244711, #46510 ) ;
#25328 = ORIENTED_EDGE ( 'NONE', *, *, #91523, .F. ) ;
#25329 = CARTESIAN_POINT ( 'NONE',  ( -15.39126916658603150, 66.61042836546582180, -152.2054667721552050 ) ) ;
#25330 = DIRECTION ( 'NONE',  ( 0.000000000000000000, 0.000000000000000000, 1.000000000000000000 ) ) ;
#25331 = DIRECTION ( 'NONE',  ( -0.000000000000000000, 0.9594490217226103734, 0.2818822000686205254 ) ) ;
#25332 = CARTESIAN_POINT ( 'NONE',  ( 22.50000000000000000, 0.1000000000111554016, -21.85042919245520210 ) ) ;
#25333 = ORIENTED_EDGE ( 'NONE', *, *, #161069, .F. ) ;
#25334 = CARTESIAN_POINT ( 'NONE',  ( -18.59999999999999787, 77.83534155023700407, -191.8679561919613832 ) ) ;
#25335 = ADVANCED_FACE ( 'NONE', ( #154402 ), #147212, .T. ) ;
#25337 = EDGE_CURVE ( 'NONE', #200535, #142216, #27083, .T. ) ;
#25336 = VECTOR ( 'NONE', #49764, 1000.000000000000000 ) ;
#25338 = VECTOR ( 'NONE', #226655, 1000.000000000000000 ) ;
#25339 = EDGE_LOOP ( 'NONE', ( #208788, #184426, #19206, #199297 ) ) ;
#25340 = CIRCLE ( 'NONE', #87831, 0.09999999999999939493 ) ;
#25341 = DIRECTION ( 'NONE',  ( 1.000000000000000000, -0.000000000000000000, -0.000000000000000000 ) ) ;
#25342 = CARTESIAN_POINT ( 'NONE',  ( -21.10257677756356998, 34.02025961620756078, -243.7221525359516079 ) ) ;
#25343 = EDGE_CURVE ( 'NONE', #190169, #158009, #130641, .T. ) ;
#25344 = DIRECTION ( 'NONE',  ( 0.000000000000000000, 1.000000000000000000, 0.000000000000000000 ) ) ;
#25345 = DIRECTION ( 'NONE',  ( -1.000000000000000000, -0.000000000000000000, 0.000000000000000000 ) ) ;
#25346 = ORIENTED_EDGE ( 'NONE', *, *, #177185, .F. ) ;
#25347 = CYLINDRICAL_SURFACE ( 'NONE', #183635, 0.5000000000000004441 ) ;
#25348 = ADVANCED_FACE ( 'NONE', ( #83056 ), #65456, .F. ) ;
#25349 = AXIS2_PLACEMENT_3D ( 'NONE', #92500, #149938, #251577 ) ;
#25350 = DIRECTION ( 'NONE',  ( 6.938893903907991995E-14, 0.000000000000000000, 1.000000000000000000 ) ) ;
#25351 = EDGE_CURVE ( 'NONE', #161541, #81489, #168111, .T. ) ;
#25352 = CARTESIAN_POINT ( 'NONE',  ( -21.14999999999999858, 69.74218538953583391, -103.1208977758331571 ) ) ;
#25353 = DIRECTION ( 'NONE',  ( 1.000000000000000000, 0.000000000000000000, 0.000000000000000000 ) ) ;
#25354 = CARTESIAN_POINT ( 'NONE',  ( 23.24999999999999645, 36.65892442174472876, -249.5511627012454596 ) ) ;
#25355 = ORIENTED_EDGE ( 'NONE', *, *, #130906, .F. ) ;
#25357 = EDGE_LOOP ( 'NONE', ( #151001, #204439, #225467, #167651, #184226 ) ) ;
#25356 = DIRECTION ( 'NONE',  ( 0.2834754621636439431, 0.2834754621636471628, 0.9161240771326858434 ) ) ;
#25358 = ORIENTED_EDGE ( 'NONE', *, *, #23083, .F. ) ;
#25359 = FACE_OUTER_BOUND ( 'NONE', #234333, .T. ) ;
#25360 = VERTEX_POINT ( 'NONE', #4815 ) ;
#25361 = CARTESIAN_POINT ( 'NONE',  ( 21.05000000000000071, 61.18232994059686547, -234.2475056001613325 ) ) ;
#25362 = CARTESIAN_POINT ( 'NONE',  ( 21.05000000000000071, 44.34387878855809362, -247.3824414791181994 ) ) ;
#25363 = SPHERICAL_SURFACE ( 'NONE', #162246, 0.1000000000000000056 ) ;
#25364 = EDGE_LOOP ( 'NONE', ( #111507, #126472, #244930, #190723, #91811, #153143, #255414, #194345, #40492, #114627, #184096, #221703, #33288, #56259, #191304, #90518 ) ) ;
#25365 = EDGE_CURVE ( 'NONE', #10892, #77390, #205638, .T. ) ;
#25366 = DIRECTION ( 'NONE',  ( -1.073024830501117725E-15, -0.2128009952263603954, 0.9770955615653315052 ) ) ;
#25367 = DIRECTION ( 'NONE',  ( 0.000000000000000000, 0.000000000000000000, 1.000000000000000000 ) ) ;
#25368 = CARTESIAN_POINT ( 'NONE',  ( 20.77766267348356166, 10.44904239062990570, -41.09270891587767238 ) ) ;
#25370 = VERTEX_POINT ( 'NONE', #100064 ) ;
#25369 = AXIS2_PLACEMENT_3D ( 'NONE', #151492, #250556, #234863 ) ;
#25371 = CARTESIAN_POINT ( 'NONE',  ( -16.87786941232801041, 9.958154714156124854, -54.37718579979401312 ) ) ;
#25373 = ORIENTED_EDGE ( 'NONE', *, *, #48533, .F. ) ;
#25372 = DIRECTION ( 'NONE',  ( 0.000000000000000000, 0.000000000000000000, -1.000000000000000000 ) ) ;
#25374 = DIRECTION ( 'NONE',  ( -0.000000000000000000, 0.8496786552930076786, 0.5273008465188218086 ) ) ;
#25375 = EDGE_CURVE ( 'NONE', #191992, #62719, #226478, .T. ) ;
#25376 = AXIS2_PLACEMENT_3D ( 'NONE', #33192, #31892, #9719 ) ;
#25377 = VERTEX_POINT ( 'NONE', #60958 ) ;
#25378 = CARTESIAN_POINT ( 'NONE',  ( 21.05000000000000426, 69.58617371119942163, -169.9373665474910240 ) ) ;
#25379 = DIRECTION ( 'NONE',  ( 0.000000000000000000, -0.5000000000000016653, 0.8660254037844377084 ) ) ;
#25380 = AXIS2_PLACEMENT_3D ( 'NONE', #157403, #114387, #193936 ) ;
#25381 = DIRECTION ( 'NONE',  ( 0.000000000000000000, 0.000000000000000000, -1.000000000000000000 ) ) ;
#25382 = EDGE_LOOP ( 'NONE', ( #153236, #114768, #238855, #253472 ) ) ;
#25383 = CARTESIAN_POINT ( 'NONE',  ( 22.60000000000000142, 75.89914163091376054, -181.7726746080137445 ) ) ;
#25384 = EDGE_CURVE ( 'NONE', #37547, #128905, #176633, .T. ) ;
#25385 = DIRECTION ( 'NONE',  ( 0.000000000000000000, -0.9908441862701782288, -0.1350103645450542456 ) ) ;
#25386 = AXIS2_PLACEMENT_3D ( 'NONE', #90258, #224640, #165997 ) ;
#25387 = ORIENTED_EDGE ( 'NONE', *, *, #42030, .F. ) ;
#25388 = CIRCLE ( 'NONE', #175425, 0.1000000000000028644 ) ;
#25390 = ORIENTED_EDGE ( 'NONE', *, *, #232777, .F. ) ;
#25389 = CIRCLE ( 'NONE', #112861, 0.1000000000000028644 ) ;
#25391 = DIRECTION ( 'NONE',  ( 0.000000000000000000, 0.2128009952263604510, -0.9770955615653315052 ) ) ;
#25392 = ORIENTED_EDGE ( 'NONE', *, *, #75402, .T. ) ;
#25393 = CARTESIAN_POINT ( 'NONE',  ( 18.52643265882457868, 10.31973158070287333, -39.05053347133544861 ) ) ;
#25394 = FACE_OUTER_BOUND ( 'NONE', #28441, .T. ) ;
#25396 = ORIENTED_EDGE ( 'NONE', *, *, #25746, .T. ) ;
#25395 = DIRECTION ( 'NONE',  ( 0.000000000000000000, 1.000000000000000000, -6.308085367188393199E-16 ) ) ;
#25397 = DIRECTION ( 'NONE',  ( 0.000000000000000000, 0.000000000000000000, -1.000000000000000000 ) ) ;
#25398 = DIRECTION ( 'NONE',  ( 1.000000000000000000, 0.000000000000000000, 1.073024830501117725E-15 ) ) ;
#25399 = DIRECTION ( 'NONE',  ( 0.000000000000000000, 0.5283051335750404975, -0.8490545835446967615 ) ) ;
#25400 = DIRECTION ( 'NONE',  ( -1.000000000000000000, 0.000000000000000000, 0.000000000000000000 ) ) ;
#25401 = CARTESIAN_POINT ( 'NONE',  ( 23.14999999999999858, 69.35000000001259934, -191.1731074845243938 ) ) ;
#25402 = DIRECTION ( 'NONE',  ( -0.000000000000000000, 7.109473446599835262E-15, -1.000000000000000000 ) ) ;
#25403 = DIRECTION ( 'NONE',  ( -1.000000000000000000, -0.000000000000000000, -0.000000000000000000 ) ) ;
#25404 = CARTESIAN_POINT ( 'NONE',  ( -18.46946985241266859, -9.509317228700410851, -107.4866625654996852 ) ) ;
#25406 = ORIENTED_EDGE ( 'NONE', *, *, #213135, .F. ) ;
#25405 = DIRECTION ( 'NONE',  ( 1.000000000000000000, 1.836970198721029934E-16, 0.000000000000000000 ) ) ;
#25407 = DIRECTION ( 'NONE',  ( -1.000000000000000000, 0.000000000000000000, 0.000000000000000000 ) ) ;
#25408 = CIRCLE ( 'NONE', #58681, 0.1000000000000028644 ) ;
#25409 = ORIENTED_EDGE ( 'NONE', *, *, #85021, .T. ) ;
#25410 = DIRECTION ( 'NONE',  ( -1.000000000000000000, -0.000000000000000000, -0.000000000000000000 ) ) ;
#25411 = DIRECTION ( 'NONE',  ( 0.000000000000000000, 0.000000000000000000, 1.000000000000000000 ) ) ;
#25412 = CARTESIAN_POINT ( 'NONE',  ( 23.14999999999999147, 76.00000000001165290, -69.52310748452431710 ) ) ;
#25413 = CARTESIAN_POINT ( 'NONE',  ( -21.05000000000000071, 43.57568952063339651, -245.1784935019914826 ) ) ;
#25414 = DIRECTION ( 'NONE',  ( 0.000000000000000000, 0.000000000000000000, -1.000000000000000000 ) ) ;
#25415 = VERTEX_POINT ( 'NONE', #38854 ) ;
#25416 = DIRECTION ( 'NONE',  ( -1.000000000000000000, 3.265361837132813093E-16, 2.280189983783949500E-30 ) ) ;
#25417 = AXIS2_PLACEMENT_3D ( 'NONE', #54742, #235944, #71769 ) ;
#25419 = EDGE_CURVE ( 'NONE', #85377, #143803, #244554, .T. ) ;
#25418 = CIRCLE ( 'NONE', #109151, 0.09999999999999739653 ) ;
#25420 = DIRECTION ( 'NONE',  ( 0.000000000000000000, 0.000000000000000000, 1.000000000000000000 ) ) ;
#25421 = CIRCLE ( 'NONE', #8845, 0.09999999999999939493 ) ;
#25422 = ORIENTED_EDGE ( 'NONE', *, *, #51710, .F. ) ;
#25423 = VECTOR ( 'NONE', #222179, 1000.000000000000000 ) ;
#25424 = CARTESIAN_POINT ( 'NONE',  ( -16.84421487269768392, 60.94446250508437402, -221.0229055566649663 ) ) ;
#25425 = ORIENTED_EDGE ( 'NONE', *, *, #98448, .F. ) ;
#25426 = CARTESIAN_POINT ( 'NONE',  ( -16.93294127766158752, 65.99671989705738895, -149.0932002186951877 ) ) ;
#25427 = VERTEX_POINT ( 'NONE', #248591 ) ;
#25428 = DIRECTION ( 'NONE',  ( 1.000000000000000000, 0.000000000000000000, 0.000000000000000000 ) ) ;
#25429 = VERTEX_POINT ( 'NONE', #244721 ) ;
#25431 = ADVANCED_FACE ( 'NONE', ( #25697 ), #51685, .T. ) ;
#25430 = VECTOR ( 'NONE', #27265, 1000.000000000000000 ) ;
#25433 = EDGE_CURVE ( 'NONE', #10751, #49099, #180723, .T. ) ;
#25432 = CYLINDRICAL_SURFACE ( 'NONE', #144125, 0.1000000000000124678 ) ;
#25434 = CARTESIAN_POINT ( 'NONE',  ( 12.25000000000000178, 9.350000000011142731, -184.0215193718251214 ) ) ;
#25435 = ORIENTED_EDGE ( 'NONE', *, *, #66318, .T. ) ;
#25436 = DIRECTION ( 'NONE',  ( 1.000000000000000000, -0.000000000000000000, -0.000000000000000000 ) ) ;
#25438 = ORIENTED_EDGE ( 'NONE', *, *, #48135, .T. ) ;
#25437 = CARTESIAN_POINT ( 'NONE',  ( -21.05000000000000071, 87.65000000001266756, -200.5231074845242745 ) ) ;
#25439 = DIRECTION ( 'NONE',  ( 0.000000000000000000, 0.9770955615653316162, 0.2128009952263604232 ) ) ;
#25440 = ORIENTED_EDGE ( 'NONE', *, *, #218853, .T. ) ;
#25441 = EDGE_CURVE ( 'NONE', #130340, #159456, #151718, .T. ) ;
#25442 = ADVANCED_FACE ( 'NONE', ( #6110 ), #80738, .T. ) ;
#25443 = VERTEX_POINT ( 'NONE', #165204 ) ;
#25444 = CARTESIAN_POINT ( 'NONE',  ( 21.07928932188134397, 6.328516656404459262, -167.4011048543455615 ) ) ;
#25446 = DIRECTION ( 'NONE',  ( -1.000000000000000000, -0.000000000000000000, 0.000000000000000000 ) ) ;
#25445 = CIRCLE ( 'NONE', #50537, 0.1000000000000000472 ) ;
#25447 = CYLINDRICAL_SURFACE ( 'NONE', #111465, 0.09999999999999939493 ) ;
#25448 = ADVANCED_FACE ( 'NONE', ( #49095 ), #223871, .F. ) ;
#25449 = DIRECTION ( 'NONE',  ( 0.000000000000000000, 0.000000000000000000, 1.000000000000000000 ) ) ;
#25450 = CARTESIAN_POINT ( 'NONE',  ( -14.77738660682464911, 66.56344716000816675, -188.3451520117640996 ) ) ;
#25451 = CARTESIAN_POINT ( 'NONE',  ( 23.14999999999999503, 9.083217576421224848, -211.4565844547649931 ) ) ;
#25452 = AXIS2_PLACEMENT_3D ( 'NONE', #35598, #133389, #212920 ) ;
#25453 = ORIENTED_EDGE ( 'NONE', *, *, #6271, .F. ) ;
#25454 = CYLINDRICAL_SURFACE ( 'NONE', #246115, 0.09999999999998898659 ) ;
#25455 = DIRECTION ( 'NONE',  ( 0.000000000000000000, 0.000000000000000000, -1.000000000000000000 ) ) ;
#25456 = LINE ( 'NONE', #103666, #95334 ) ;
#25457 = EDGE_CURVE ( 'NONE', #14829, #153040, #66099, .T. ) ;
#25458 = CARTESIAN_POINT ( 'NONE',  ( 21.14999999999999858, 36.65892442174472876, -249.5511627012454596 ) ) ;
#25459 = AXIS2_PLACEMENT_3D ( 'NONE', #137951, #217485, #42716 ) ;
#25460 = EDGE_LOOP ( 'NONE', ( #113551, #53638, #209785, #61153 ) ) ;
#25461 = DIRECTION ( 'NONE',  ( 0.000000000000000000, -1.000000000000000000, 0.000000000000000000 ) ) ;
#25462 = ORIENTED_EDGE ( 'NONE', *, *, #53876, .F. ) ;
#25463 = CARTESIAN_POINT ( 'NONE',  ( -20.85000000000000142, 64.25000000001176659, -76.30697314750248950 ) ) ;
#25464 = ORIENTED_EDGE ( 'NONE', *, *, #57608, .T. ) ;
#25465 = CIRCLE ( 'NONE', #121361, 0.1000000000000028644 ) ;
#25466 = EDGE_CURVE ( 'NONE', #43854, #226150, #209961, .T. ) ;
#25467 = FACE_OUTER_BOUND ( 'NONE', #116091, .T. ) ;
#25468 = DIRECTION ( 'NONE',  ( -3.440080580676165868E-14, 0.1298341882520054891, 0.9915357197604850459 ) ) ;
#25469 = EDGE_LOOP ( 'NONE', ( #135038, #166176, #98378, #74125, #66885 ) ) ;
#25470 = CIRCLE ( 'NONE', #146066, 0.1000000000000028644 ) ;
#25472 = ORIENTED_EDGE ( 'NONE', *, *, #185533, .T. ) ;
#25471 = DIRECTION ( 'NONE',  ( 1.000000000000000000, 0.000000000000000000, 0.000000000000000000 ) ) ;
#25473 = CARTESIAN_POINT ( 'NONE',  ( -20.54999999999999716, 76.00000000001244871, -170.0231074845243597 ) ) ;
#25474 = EDGE_LOOP ( 'NONE', ( #220724, #120115, #32362, #245121 ) ) ;
#25475 = DIRECTION ( 'NONE',  ( -0.7071067811865475727, -0.7071067811865475727, 0.000000000000000000 ) ) ;
#25476 = CARTESIAN_POINT ( 'NONE',  ( -18.59117750673696889, 65.66751761918648356, -63.92826094061123143 ) ) ;
#25477 = EDGE_CURVE ( 'NONE', #84754, #114211, #243239, .T. ) ;
#25478 = ORIENTED_EDGE ( 'NONE', *, *, #79344, .T. ) ;
#25479 = DIRECTION ( 'NONE',  ( 0.000000000000000000, -1.224646799147358384E-16, 1.000000000000000000 ) ) ;
#25480 = DIRECTION ( 'NONE',  ( 1.000000000000000000, 0.000000000000000000, 0.000000000000000000 ) ) ;
#25481 = AXIS2_PLACEMENT_3D ( 'NONE', #56736, #39814, #58033 ) ;
#25482 = CIRCLE ( 'NONE', #166981, 4.099999999999992539 ) ;
#25483 = ORIENTED_EDGE ( 'NONE', *, *, #66715, .F. ) ;
#25484 = ORIENTED_EDGE ( 'NONE', *, *, #170319, .F. ) ;
#25485 = CIRCLE ( 'NONE', #79444, 0.1000000000000124678 ) ;
#25486 = CIRCLE ( 'NONE', #58774, 7.800000000000000711 ) ;
#25487 = TOROIDAL_SURFACE ( 'NONE', #42240, 12.97499999999999609, 0.1000000000000000056 ) ;
#25488 = CARTESIAN_POINT ( 'NONE',  ( -21.13614978966382196, 6.499104701844945708, -67.00000000000004263 ) ) ;
#25490 = ORIENTED_EDGE ( 'NONE', *, *, #127172, .T. ) ;
#25489 = DIRECTION ( 'NONE',  ( 3.469446951953635015E-14, -0.000000000000000000, 1.000000000000000000 ) ) ;
#25491 = DIRECTION ( 'NONE',  ( -0.000000000000000000, -0.000000000000000000, -1.000000000000000000 ) ) ;
#25492 = CARTESIAN_POINT ( 'NONE',  ( 21.00000000000000000, 9.750000000011153745, -188.7499999999999716 ) ) ;
#25493 = CARTESIAN_POINT ( 'NONE',  ( -16.85718274719421217, 9.976142314632896912, -121.4366536678175663 ) ) ;
#25495 = CARTESIAN_POINT ( 'NONE',  ( -21.14999999999994174, 77.75000000001119815, -47.64205752314703801 ) ) ;
#25494 = CARTESIAN_POINT ( 'NONE',  ( -16.93658211146646408, 66.00589133767067551, -90.42740255448006792 ) ) ;
#25496 = CARTESIAN_POINT ( 'NONE',  ( 21.05000000000002558, 39.30856869743859505, -236.7176136696176627 ) ) ;
#25497 = CARTESIAN_POINT ( 'NONE',  ( -21.05000000000000071, 76.00000000001199396, -114.7231074845243057 ) ) ;
#25498 = CARTESIAN_POINT ( 'NONE',  ( 13.99999999999999822, 13.18880795147152618, -215.2702608532411830 ) ) ;
#25499 = VECTOR ( 'NONE', #111562, 1000.000000000000000 ) ;
#25500 = CARTESIAN_POINT ( 'NONE',  ( -20.54999999999999716, 6.724511449164476851, -231.8762197454659884 ) ) ;
#25501 = VECTOR ( 'NONE', #202936, 1000.000000000000000 ) ;
#25503 = ORIENTED_EDGE ( 'NONE', *, *, #74632, .F. ) ;
#25502 = AXIS2_PLACEMENT_3D ( 'NONE', #103662, #85371, #124550 ) ;
#25504 = EDGE_CURVE ( 'NONE', #113635, #59420, #1630, .T. ) ;
#25505 = EDGE_CURVE ( 'NONE', #240643, #61134, #68300, .T. ) ;
#25506 = ORIENTED_EDGE ( 'NONE', *, *, #60511, .T. ) ;
#25507 = DIRECTION ( 'NONE',  ( 1.000000000000000000, 0.000000000000000000, 0.000000000000000000 ) ) ;
#25508 = ORIENTED_EDGE ( 'NONE', *, *, #103494, .T. ) ;
#25509 = EDGE_CURVE ( 'NONE', #183971, #177551, #227735, .T. ) ;
#25510 = EDGE_CURVE ( 'NONE', #160408, #85652, #106480, .T. ) ;
#25511 = CARTESIAN_POINT ( 'NONE',  ( 20.94999999999999929, -9.399999999988844834, -191.1060308773475072 ) ) ;
#25512 = ORIENTED_EDGE ( 'NONE', *, *, #70279, .T. ) ;
#25513 = ADVANCED_FACE ( 'NONE', ( #186054 ), #76652, .T. ) ;
#25514 = FACE_OUTER_BOUND ( 'NONE', #223137, .T. ) ;
#25515 = EDGE_CURVE ( 'NONE', #250000, #61108, #164159, .T. ) ;
#25516 = ORIENTED_EDGE ( 'NONE', *, *, #184264, .T. ) ;
#25517 = CARTESIAN_POINT ( 'NONE',  ( -21.09610168723072121, 6.225701436283752166, -199.6097317171979171 ) ) ;
#25518 = ORIENTED_EDGE ( 'NONE', *, *, #139279, .F. ) ;
#25519 = EDGE_CURVE ( 'NONE', #208882, #202160, #184999, .T. ) ;
#25520 = EDGE_LOOP ( 'NONE', ( #99856, #7419, #122305, #155810, #211536 ) ) ;
#25521 = DIRECTION ( 'NONE',  ( -1.000000000000000000, 6.938893903907270030E-14, 0.000000000000000000 ) ) ;
#25522 = CARTESIAN_POINT ( 'NONE',  ( -21.14250536705909411, 76.00000000001200817, -109.5412796614050563 ) ) ;
#25524 = ORIENTED_EDGE ( 'NONE', *, *, #180090, .T. ) ;
#25523 = CARTESIAN_POINT ( 'NONE',  ( -18.59999999999999787, 43.57281345108133053, -239.9888335660389487 ) ) ;
#25525 = ADVANCED_FACE ( 'NONE', ( #88200 ), #109975, .F. ) ;
#25526 = CARTESIAN_POINT ( 'NONE',  ( 20.86777300164945004, 65.66799936921530900, -97.42993998886008455 ) ) ;
#25528 = EDGE_LOOP ( 'NONE', ( #169349, #243508, #248005, #10608 ) ) ;
#25527 = DIRECTION ( 'NONE',  ( 0.000000000000000000, 0.9915357197604792727, -0.1298341882520475943 ) ) ;
#25529 = LINE ( 'NONE', #158638, #204106 ) ;
#25530 = CARTESIAN_POINT ( 'NONE',  ( -18.50000000000000000, 63.74333919030581086, -212.9951329171253747 ) ) ;
#25532 = ORIENTED_EDGE ( 'NONE', *, *, #200332, .T. ) ;
#25531 = CARTESIAN_POINT ( 'NONE',  ( -20.54999999999999716, 66.65000000001198543, -115.3731074845243683 ) ) ;
#25533 = CARTESIAN_POINT ( 'NONE',  ( 18.50596464788227280, 10.30632246271648889, -173.0041836778896140 ) ) ;
#25535 = ADVANCED_FACE ( 'NONE', ( #68678 ), #64196, .F. ) ;
#25534 = CARTESIAN_POINT ( 'NONE',  ( -14.11361717019516249, 27.90226189425600367, -234.1316127586030120 ) ) ;
#25536 = CARTESIAN_POINT ( 'NONE',  ( -16.90137573187933029, 12.44348879280447129, -211.3781360020290379 ) ) ;
#25537 = ORIENTED_EDGE ( 'NONE', *, *, #189107, .F. ) ;
#25539 = CARTESIAN_POINT ( 'NONE',  ( 21.05000000000000071, 69.65000000001231228, -160.1792853948412869 ) ) ;
#25538 = DIRECTION ( 'NONE',  ( -1.020425574104004196E-15, 0.2617529984165031243, 0.9651348961777157509 ) ) ;
#25540 = DIRECTION ( 'NONE',  ( -1.000000000000000000, -2.952720810173289112E-16, 0.000000000000000000 ) ) ;
#25541 = EDGE_CURVE ( 'NONE', #36614, #250601, #33439, .T. ) ;
#25542 = EDGE_CURVE ( 'NONE', #7829, #20356, #234153, .T. ) ;
#25543 = DIRECTION ( 'NONE',  ( -1.000000000000000000, 0.000000000000000000, 0.000000000000000000 ) ) ;
#25544 = DIRECTION ( 'NONE',  ( 1.000000000000000000, -0.000000000000000000, -0.000000000000000000 ) ) ;
#25545 = DIRECTION ( 'NONE',  ( 0.000000000000000000, -0.9876197685951263461, 0.1568667991644794590 ) ) ;
#25546 = ORIENTED_EDGE ( 'NONE', *, *, #181391, .T. ) ;
#25547 = ORIENTED_EDGE ( 'NONE', *, *, #77097, .T. ) ;
#25548 = ORIENTED_EDGE ( 'NONE', *, *, #221357, .F. ) ;
#25549 = EDGE_CURVE ( 'NONE', #94057, #13123, #17820, .T. ) ;
#25551 = CIRCLE ( 'NONE', #221325, 0.1999999999999987899 ) ;
#25550 = DIRECTION ( 'NONE',  ( -4.336808689942053235E-15, -0.8660254037844482555, -0.4999999999999836797 ) ) ;
#25552 = ORIENTED_EDGE ( 'NONE', *, *, #128540, .F. ) ;
#25553 = DIRECTION ( 'NONE',  ( -1.000000000000000000, 0.000000000000000000, 0.000000000000000000 ) ) ;
#25554 = ORIENTED_EDGE ( 'NONE', *, *, #106627, .F. ) ;
#25555 = CARTESIAN_POINT ( 'NONE',  ( 23.14999999999999858, 76.00000000001172396, -71.52310748452431710 ) ) ;
#25556 = CARTESIAN_POINT ( 'NONE',  ( -17.80356949365270580, 15.56737101418502967, -221.3668113561435860 ) ) ;
#25557 = EDGE_CURVE ( 'NONE', #73589, #12219, #172584, .T. ) ;
#25558 = ADVANCED_FACE ( 'NONE', ( #172951 ), #153369, .F. ) ;
#25559 = EDGE_LOOP ( 'NONE', ( #6130, #188189, #113366, #144589 ) ) ;
#25560 = CARTESIAN_POINT ( 'NONE',  ( 13.12229106158772218, 9.430637101707896264, -152.2682606180609639 ) ) ;
#25561 =( NAMED_UNIT ( * ) SI_UNIT ( $, .STERADIAN. ) SOLID_ANGLE_UNIT ( ) );
#25563 = VERTEX_POINT ( 'NONE', #135037 ) ;
#25562 = AXIS2_PLACEMENT_3D ( 'NONE', #79030, #98578, #97303 ) ;
#25564 = ORIENTED_EDGE ( 'NONE', *, *, #206006, .F. ) ;
#25565 = ORIENTED_EDGE ( 'NONE', *, *, #89279, .F. ) ;
#25566 = CONICAL_SURFACE ( 'NONE', #17370, 4.000000000000000000, 0.7853981633974489451 ) ;
#25567 = CARTESIAN_POINT ( 'NONE',  ( -18.39999999999999858, 85.51932773110434027, -96.05013110796491560 ) ) ;
#25568 = DIRECTION ( 'NONE',  ( 7.304098846218134667E-16, -1.000000000000000000, 0.000000000000000000 ) ) ;
#25569 = CARTESIAN_POINT ( 'NONE',  ( 14.45963434102923983, 27.85878770204270083, -234.1150007431636766 ) ) ;
#25570 = DIRECTION ( 'NONE',  ( -1.000000000000000000, -0.000000000000000000, -0.000000000000000000 ) ) ;
#25571 = CARTESIAN_POINT ( 'NONE',  ( 18.49999999999999645, 77.63717271298267519, -158.4409541190523214 ) ) ;
#25573 = DIRECTION ( 'NONE',  ( -1.000000000000000000, -3.265361837132813093E-16, 0.000000000000000000 ) ) ;
#25572 = CARTESIAN_POINT ( 'NONE',  ( 20.73486653747088937, 7.750000000000025757, -9.250000000000001776 ) ) ;
#25574 = DIRECTION ( 'NONE',  ( 0.000000000000000000, -6.982962677686266711E-15, 1.000000000000000000 ) ) ;
#25576 = ORIENTED_EDGE ( 'NONE', *, *, #101765, .T. ) ;
#25575 = DIRECTION ( 'NONE',  ( 0.000000000000000000, 0.9770955615653310611, 0.2128009952263620608 ) ) ;
#25578 = CARTESIAN_POINT ( 'NONE',  ( 21.11101077988997332, 69.57631526528589916, -103.0383927534386714 ) ) ;
#25577 = CARTESIAN_POINT ( 'NONE',  ( -21.05000000000000071, 11.75000000001115197, -40.28386566297815108 ) ) ;
#25579 = DIRECTION ( 'NONE',  ( 1.000000000000000000, -0.000000000000000000, -0.000000000000000000 ) ) ;
#25580 = ORIENTED_EDGE ( 'NONE', *, *, #69326, .T. ) ;
#25581 = CARTESIAN_POINT ( 'NONE',  ( 20.95561247346651967, 10.59500736521470721, -74.59378276698168975 ) ) ;
#25582 = DIRECTION ( 'NONE',  ( 1.000000000000000000, 0.000000000000000000, 0.000000000000000000 ) ) ;
#25583 = FACE_OUTER_BOUND ( 'NONE', #103893, .T. ) ;
#25584 = ORIENTED_EDGE ( 'NONE', *, *, #115315, .F. ) ;
#25585 = AXIS2_PLACEMENT_3D ( 'NONE', #185470, #68089, #94058 ) ;
#25586 = LINE ( 'NONE', #125942, #53600 ) ;
#25587 = CARTESIAN_POINT ( 'NONE',  ( -18.59999999999999787, 64.18627039993180006, -224.3513032416919089 ) ) ;
#25588 = DIRECTION ( 'NONE',  ( 0.000000000000000000, -0.1350103645451904977, -0.9908441862701596881 ) ) ;
#25589 = ORIENTED_EDGE ( 'NONE', *, *, #167222, .F. ) ;
#25590 = ORIENTED_EDGE ( 'NONE', *, *, #7003, .T. ) ;
#25591 = CARTESIAN_POINT ( 'NONE',  ( -16.97683809663752186, 44.82209472663103611, -234.9913374327310578 ) ) ;
#25592 = ORIENTED_EDGE ( 'NONE', *, *, #24545, .F. ) ;
#25593 = CARTESIAN_POINT ( 'NONE',  ( -22.94999999999999929, -1.800000000000000044, -11.61130914238355771 ) ) ;
#25594 = CARTESIAN_POINT ( 'NONE',  ( -18.54260524012587297, -9.624219390062703994, -174.2407730457707089 ) ) ;
#25595 = DIRECTION ( 'NONE',  ( -0.000000000000000000, 0.8660254037844424824, 0.4999999999999934497 ) ) ;
#25596 = DIRECTION ( 'NONE',  ( -0.7071067811865475727, 0.6824534298470373850, -0.1850873201762210096 ) ) ;
#25597 = ORIENTED_EDGE ( 'NONE', *, *, #145722, .F. ) ;
#25598 = ADVANCED_FACE ( 'NONE', ( #131202 ), #133772, .F. ) ;
#25599 = AXIS2_PLACEMENT_3D ( 'NONE', #224900, #168847, #87947 ) ;
#25601 = CARTESIAN_POINT ( 'NONE',  ( -20.54999999999999716, 74.00000000001151079, -48.84772940728643675 ) ) ;
#25600 = AXIS2_PLACEMENT_3D ( 'NONE', #97471, #195350, #152373 ) ;
#25602 = CARTESIAN_POINT ( 'NONE',  ( 18.49999999999996447, 10.49142135624846439, -192.2499999999999716 ) ) ;
#25603 = DIRECTION ( 'NONE',  ( 1.000000000000000000, 7.304098846218133681E-16, 4.639676173203992654E-30 ) ) ;
#25604 = EDGE_CURVE ( 'NONE', #136568, #238120, #35012, .T. ) ;
#25605 = VERTEX_POINT ( 'NONE', #253711 ) ;
#25606 = EDGE_CURVE ( 'NONE', #105012, #13011, #56772, .T. ) ;
#25608 = ORIENTED_EDGE ( 'NONE', *, *, #22822, .F. ) ;
#25607 = DIRECTION ( 'NONE',  ( 0.000000000000000000, 7.026728003956683390E-15, -1.000000000000000000 ) ) ;
#25609 = ADVANCED_FACE ( 'NONE', ( #35979 ), #72542, .F. ) ;
#25610 = DIRECTION ( 'NONE',  ( -1.000000000000000000, 0.000000000000000000, 0.000000000000000000 ) ) ;
#25611 = DIRECTION ( 'NONE',  ( 1.000000000000000000, 8.855395344894292773E-17, 1.653135691717061729E-16 ) ) ;
#25612 = DIRECTION ( 'NONE',  ( 0.000000000000000000, -1.000000000000000000, -6.982962677686266711E-15 ) ) ;
#25613 = DIRECTION ( 'NONE',  ( 1.000000000000000000, -0.000000000000000000, -0.000000000000000000 ) ) ;
#25614 = DIRECTION ( 'NONE',  ( 1.000000000000000000, 0.000000000000000000, 0.000000000000000000 ) ) ;
#25615 = VECTOR ( 'NONE', #40091, 1000.000000000000000 ) ;
#25616 = VERTEX_POINT ( 'NONE', #174233 ) ;
#25617 = DIRECTION ( 'NONE',  ( 0.000000000000000000, -0.2617529984165034018, -0.9651348961777157509 ) ) ;
#25618 = DIRECTION ( 'NONE',  ( 0.000000000000000000, -0.01562499999996560217, -0.9998779222360102414 ) ) ;
#25619 = LINE ( 'NONE', #122151, #163205 ) ;
#25620 = PLANE ( 'NONE',  #213021 ) ;
#25621 = DIRECTION ( 'NONE',  ( -0.7071067811865489050, -0.6824534298470359417, 0.1850873201762213704 ) ) ;
#25622 = EDGE_CURVE ( 'NONE', #98792, #127648, #251638, .T. ) ;
#25623 = VERTEX_POINT ( 'NONE', #196310 ) ;
#25624 = ORIENTED_EDGE ( 'NONE', *, *, #46370, .T. ) ;
#25625 = CARTESIAN_POINT ( 'NONE',  ( 20.90000000000000213, -1.212568896937008089, -7.900000000000000355 ) ) ;
#25626 = CARTESIAN_POINT ( 'NONE',  ( -23.25000000000000000, 76.00000000001207923, -128.6231074845243540 ) ) ;
#25627 = CARTESIAN_POINT ( 'NONE',  ( -23.49999999999994316, 87.75000000001119815, -51.02310748452479316 ) ) ;
#25628 = AXIS2_PLACEMENT_3D ( 'NONE', #12840, #251427, #226715 ) ;
#25629 = FACE_OUTER_BOUND ( 'NONE', #139328, .T. ) ;
#25630 = CARTESIAN_POINT ( 'NONE',  ( -23.49999999999994316, 74.16448838626247664, -47.52760213295649550 ) ) ;
#25631 = DIRECTION ( 'NONE',  ( -5.603264701231743991E-32, 1.897661533703519897E-16, -1.000000000000000000 ) ) ;
#25632 = EDGE_CURVE ( 'NONE', #106883, #113112, #209366, .T. ) ;
#25633 = CARTESIAN_POINT ( 'NONE',  ( -20.85000000000000142, 17.16609282392353464, -224.6038045889790453 ) ) ;
#25634 = VECTOR ( 'NONE', #88231, 1000.000000000000000 ) ;
#25635 = EDGE_CURVE ( 'NONE', #3044, #188675, #97169, .T. ) ;
#25636 = AXIS2_PLACEMENT_3D ( 'NONE', #100595, #221837, #257089 ) ;
#25637 = VERTEX_POINT ( 'NONE', #76354 ) ;
#25638 = LINE ( 'NONE', #63464, #206659 ) ;
#25639 = CIRCLE ( 'NONE', #233757, 7.720710678118692272 ) ;
#25640 = ORIENTED_EDGE ( 'NONE', *, *, #43795, .T. ) ;
#25641 = CARTESIAN_POINT ( 'NONE',  ( -21.05000000000000071, 70.10000000001220144, -146.7422072491807796 ) ) ;
#25642 = CARTESIAN_POINT ( 'NONE',  ( -18.59999999999999787, -14.27107483842559610, -0.5438473119858301397 ) ) ;
#25643 = DIRECTION ( 'NONE',  ( 1.000000000000000000, 0.000000000000000000, 0.000000000000000000 ) ) ;
#25644 = EDGE_CURVE ( 'NONE', #237434, #173330, #176778, .T. ) ;
#25645 = DIRECTION ( 'NONE',  ( -0.000000000000000000, 0.2128009952263603677, -0.9770955615653313941 ) ) ;
#25646 = DIRECTION ( 'NONE',  ( -1.000000000000000000, 1.772924042024179204E-16, -4.808324575169892332E-17 ) ) ;
#25647 = CARTESIAN_POINT ( 'NONE',  ( 15.74999999999999645, 66.15000000001155911, -52.77310748452440237 ) ) ;
#25649 = CARTESIAN_POINT ( 'NONE',  ( -18.49719636458550553, -9.446365359228076741, -7.071613869883250914 ) ) ;
#25648 = CIRCLE ( 'NONE', #34068, 0.09999999999999939493 ) ;
#25650 = FACE_OUTER_BOUND ( 'NONE', #82181, .T. ) ;
#25651 = EDGE_CURVE ( 'NONE', #61093, #149809, #134887, .T. ) ;
#25652 = CARTESIAN_POINT ( 'NONE',  ( -21.07016717456946608, 6.320940838111406279, -67.00000000000004263 ) ) ;
#25653 = CARTESIAN_POINT ( 'NONE',  ( -20.00857864376270001, 9.150000000011157653, -155.2500000000000284 ) ) ;
#25654 = FACE_OUTER_BOUND ( 'NONE', #169502, .T. ) ;
#25655 = CYLINDRICAL_SURFACE ( 'NONE', #256116, 0.5000000000000004441 ) ;
#25657 = ADVANCED_FACE ( 'NONE', ( #82639 ), #63444, .T. ) ;
#25656 = AXIS2_PLACEMENT_3D ( 'NONE', #960, #75437, #137925 ) ;
#25658 = MANIFOLD_SOLID_BREP ( 'Stock-MAS-200-1', #136839 ) ;
#25659 = AXIS2_PLACEMENT_3D ( 'NONE', #52000, #213663, #112013 ) ;
#25660 = CARTESIAN_POINT ( 'NONE',  ( 18.39999999999999503, 5.650000000011139001, -146.6500000000000341 ) ) ;
#25661 = FACE_OUTER_BOUND ( 'NONE', #137684, .T. ) ;
#25662 = ORIENTED_EDGE ( 'NONE', *, *, #212096, .F. ) ;
#25663 = CIRCLE ( 'NONE', #233782, 0.1000000000000124678 ) ;
#25664 = LINE ( 'NONE', #107755, #156227 ) ;
#25665 = DIRECTION ( 'NONE',  ( 0.000000000000000000, -1.000000000000000000, 0.000000000000000000 ) ) ;
#25666 = ADVANCED_FACE ( 'NONE', ( #124383 ), #13736, .F. ) ;
#25667 = AXIS2_PLACEMENT_3D ( 'NONE', #124196, #83726, #244115 ) ;
#25668 = VERTEX_POINT ( 'NONE', #183074 ) ;
#25669 = DIRECTION ( 'NONE',  ( -3.035766082959430717E-14, 0.2617529984165031243, 0.9651348961777157509 ) ) ;
#25670 = CARTESIAN_POINT ( 'NONE',  ( 21.04999999999908411, 67.22371710472162931, -157.8651984818719143 ) ) ;
#25671 = CARTESIAN_POINT ( 'NONE',  ( 23.24999999999999645, 76.00000000001213607, -136.5231074845242745 ) ) ;
#25672 = EDGE_CURVE ( 'NONE', #167145, #72511, #4411, .T. ) ;
#25673 = ORIENTED_EDGE ( 'NONE', *, *, #76762, .F. ) ;
#25674 = DIRECTION ( 'NONE',  ( -1.000000000000000000, -0.000000000000000000, 0.000000000000000000 ) ) ;
#25675 = DIRECTION ( 'NONE',  ( 0.000000000000000000, -0.9126074666063660468, -0.4088369013363524762 ) ) ;
#25676 = CIRCLE ( 'NONE', #183892, 0.5000000000000147660 ) ;
#25677 = VERTEX_POINT ( 'NONE', #80065 ) ;
#25678 = CIRCLE ( 'NONE', #88003, 0.09999999999999939493 ) ;
#25679 = VECTOR ( 'NONE', #47756, 999.9999999999998863 ) ;
#25680 = AXIS2_PLACEMENT_3D ( 'NONE', #16913, #14364, #55996 ) ;
#25681 = DIRECTION ( 'NONE',  ( 0.000000000000000000, 0.9910465087640861759, -0.1335171055202901691 ) ) ;
#25682 = VERTEX_POINT ( 'NONE', #203902 ) ;
#25683 = CARTESIAN_POINT ( 'NONE',  ( 23.14999999999999503, 11.75000000001115552, -188.7499999999999716 ) ) ;
#25684 = CARTESIAN_POINT ( 'NONE',  ( 22.49999999999999645, 0.04562336060752137518, -21.84949566144972621 ) ) ;
#25685 = CARTESIAN_POINT ( 'NONE',  ( -20.94999999999999929, 2.817198581588411077, -208.4716308468294130 ) ) ;
#25686 = DIRECTION ( 'NONE',  ( 1.000000000000000000, 0.000000000000000000, 0.000000000000000000 ) ) ;
#25687 = CARTESIAN_POINT ( 'NONE',  ( -21.05000000000000071, 1.162701749949165642, -142.1000000000000227 ) ) ;
#25688 = DIRECTION ( 'NONE',  ( 0.000000000000000000, 0.4088369013363283289, -0.9126074666063768159 ) ) ;
#25689 = DIRECTION ( 'NONE',  ( 0.000000000000000000, 0.8149014228131981064, -0.5795995782408966956 ) ) ;
#25690 = DIRECTION ( 'NONE',  ( 1.000000000000000000, 0.000000000000000000, 0.000000000000000000 ) ) ;
#25691 = CARTESIAN_POINT ( 'NONE',  ( 20.85000000000000142, 69.06610602788535402, -65.73746165015079157 ) ) ;
#25693 = ORIENTED_EDGE ( 'NONE', *, *, #96158, .F. ) ;
#25692 = CARTESIAN_POINT ( 'NONE',  ( 18.33996824403804737, 87.02090424921982503, -199.4466712054037885 ) ) ;
#25694 = EDGE_LOOP ( 'NONE', ( #54353, #39795, #153817, #174846 ) ) ;
#25696 = DIRECTION ( 'NONE',  ( -1.000000000000000000, 0.000000000000000000, 0.000000000000000000 ) ) ;
#25695 = DIRECTION ( 'NONE',  ( 1.000000000000000000, 0.000000000000000000, 0.000000000000000000 ) ) ;
#25698 = ORIENTED_EDGE ( 'NONE', *, *, #8298, .T. ) ;
#25697 = FACE_OUTER_BOUND ( 'NONE', #27746, .T. ) ;
#25699 = ORIENTED_EDGE ( 'NONE', *, *, #110298, .T. ) ;
#25700 = DIRECTION ( 'NONE',  ( 0.000000000000000000, -1.000000000000000000, 0.000000000000000000 ) ) ;
#25701 = AXIS2_PLACEMENT_3D ( 'NONE', #199711, #122739, #217939 ) ;
#25702 = FACE_OUTER_BOUND ( 'NONE', #251338, .T. ) ;
#25703 = DIRECTION ( 'NONE',  ( -1.000000000000000000, -0.000000000000000000, -0.000000000000000000 ) ) ;
#25704 = DIRECTION ( 'NONE',  ( -1.000000000000000000, 0.000000000000000000, 0.000000000000000000 ) ) ;
#25705 = CARTESIAN_POINT ( 'NONE',  ( 18.60000000000000497, 1.115600667400684642E-11, -167.4999999999999716 ) ) ;
#25706 = CARTESIAN_POINT ( 'NONE',  ( -23.25000000000000000, 68.11287320386161070, -224.1382462126928488 ) ) ;
#25707 = CIRCLE ( 'NONE', #4825, 0.1000000000000028644 ) ;
#25708 = LINE ( 'NONE', #199221, #35468 ) ;
#25709 = ORIENTED_EDGE ( 'NONE', *, *, #194990, .F. ) ;
#25710 = EDGE_LOOP ( 'NONE', ( #239487, #229734, #102080 ) ) ;
#25711 = EDGE_CURVE ( 'NONE', #68580, #256608, #60530, .T. ) ;
#25712 = CARTESIAN_POINT ( 'NONE',  ( -20.15000000000000568, 9.291421356248463326, -88.25000000000005684 ) ) ;
#25713 = ORIENTED_EDGE ( 'NONE', *, *, #206290, .T. ) ;
#25714 = CARTESIAN_POINT ( 'NONE',  ( 22.59999999999999432, 64.25012875563587045, -170.0885370755381132 ) ) ;
#25715 = EDGE_LOOP ( 'NONE', ( #253750, #193825, #84515, #195190 ) ) ;
#25716 = DIRECTION ( 'NONE',  ( 1.000000000000000000, 0.000000000000000000, 0.000000000000000000 ) ) ;
#25717 = AXIS2_PLACEMENT_3D ( 'NONE', #108363, #187904, #235994 ) ;
#25718 = SPHERICAL_SURFACE ( 'NONE', #113488, 0.1000000000000000056 ) ;
#25719 = ADVANCED_FACE ( 'NONE', ( #180502 ), #160947, .T. ) ;
#25720 = DIRECTION ( 'NONE',  ( 1.000000000000000000, 0.000000000000000000, 0.000000000000000000 ) ) ;
#25721 = DIRECTION ( 'NONE',  ( -1.000000000000000000, 0.000000000000000000, 0.000000000000000000 ) ) ;
#25722 = ORIENTED_EDGE ( 'NONE', *, *, #58888, .F. ) ;
#25723 = APPLICATION_CONTEXT ( 'automotive_design' ) ;
#25724 = DIRECTION ( 'NONE',  ( 0.000000000000000000, 7.056502275159890832E-15, -1.000000000000000000 ) ) ;
#25725 = ORIENTED_EDGE ( 'NONE', *, *, #219455, .T. ) ;
#25726 = ADVANCED_FACE ( 'NONE', ( #81356 ), #231199, .F. ) ;
#25727 = CARTESIAN_POINT ( 'NONE',  ( -20.54999999999999716, -8.999999999988844479, -124.1060308773475924 ) ) ;
#25728 = EDGE_CURVE ( 'NONE', #177863, #49440, #9646, .T. ) ;
#25729 = DIRECTION ( 'NONE',  ( -0.000000000000000000, 0.8660254037844377084, 0.5000000000000016653 ) ) ;
#25730 = DIRECTION ( 'NONE',  ( 1.000000000000000000, -1.186688945009009831E-16, -8.286604613020806758E-31 ) ) ;
#25731 = DIRECTION ( 'NONE',  ( 1.000000000000000000, 0.000000000000000000, 0.000000000000000000 ) ) ;
#25732 = ORIENTED_EDGE ( 'NONE', *, *, #72592, .F. ) ;
#25734 = DIRECTION ( 'NONE',  ( 0.000000000000000000, -0.9910465087640860649, 0.1335171055202901413 ) ) ;
#25733 = CIRCLE ( 'NONE', #88240, 0.1000000000000013933 ) ;
#25735 = ORIENTED_EDGE ( 'NONE', *, *, #215812, .T. ) ;
#25738 = EDGE_LOOP ( 'NONE', ( #255660, #203485, #109182, #243584 ) ) ;
#25737 = CARTESIAN_POINT ( 'NONE',  ( -18.59999999999999787, 67.23127455305835554, -235.8551265064784559 ) ) ;
#25736 = CARTESIAN_POINT ( 'NONE',  ( 18.45036689428352616, 46.93870047321756545, -255.3449267777946829 ) ) ;
#25739 = AXIS2_PLACEMENT_3D ( 'NONE', #95733, #76174, #114018 ) ;
#25740 = CYLINDRICAL_SURFACE ( 'NONE', #181221, 11.75000000000001066 ) ;
#25741 = ORIENTED_EDGE ( 'NONE', *, *, #137292, .T. ) ;
#25742 = CIRCLE ( 'NONE', #75811, 2.000000000000001776 ) ;
#25743 = CARTESIAN_POINT ( 'NONE',  ( -18.50000000000000000, 9.350000000011156942, -112.6500000000000341 ) ) ;
#25744 = ORIENTED_EDGE ( 'NONE', *, *, #21072, .T. ) ;
#25745 = DIRECTION ( 'NONE',  ( 1.000000000000000000, 0.000000000000000000, 0.000000000000000000 ) ) ;
#25746 = EDGE_CURVE ( 'NONE', #170888, #152148, #27875, .T. ) ;
#25747 =( BOUNDED_CURVE ( )  B_SPLINE_CURVE ( 3, ( #87730, #228560, #90303, #69496 ),
 .UNSPECIFIED., .F., .F. ) 
 B_SPLINE_CURVE_WITH_KNOTS ( ( 4, 4 ),
 ( 1.570796326794895448, 3.141592653589791784 ),
 .UNSPECIFIED. ) 
 CURVE ( )  GEOMETRIC_REPRESENTATION_ITEM ( )  RATIONAL_B_SPLINE_CURVE ( ( 1.000000000000000000, 0.8047378541243650485, 0.8047378541243650485, 1.000000000000000000 ) ) 
 REPRESENTATION_ITEM ( '' )  );
#25748 = DIRECTION ( 'NONE',  ( 0.000000000000000000, -1.000000000000000000, 0.000000000000000000 ) ) ;
#25749 = PLANE ( 'NONE',  #214312 ) ;
#25750 = AXIS2_PLACEMENT_3D ( 'NONE', #188877, #143320, #8953 ) ;
#25751 = VERTEX_POINT ( 'NONE', #47382 ) ;
#25752 = LINE ( 'NONE', #63586, #231645 ) ;
#25753 = CARTESIAN_POINT ( 'NONE',  ( -16.81453563122428108, 14.13521282870534357, -219.1970648546185885 ) ) ;
#25754 = CARTESIAN_POINT ( 'NONE',  ( -15.52965525596988527, 66.62446189796426665, -154.1532316035335555 ) ) ;
#25755 = ORIENTED_EDGE ( 'NONE', *, *, #212473, .F. ) ;
#25756 = DIRECTION ( 'NONE',  ( -0.000000000000000000, 0.4721928772777345684, 0.8814952561688429444 ) ) ;
#25757 = ORIENTED_EDGE ( 'NONE', *, *, #119405, .T. ) ;
#25758 = LINE ( 'NONE', #105250, #35623 ) ;
#25759 = EDGE_CURVE ( 'NONE', #223637, #46965, #80342, .T. ) ;
#25760 = CARTESIAN_POINT ( 'NONE',  ( 18.49999999999999289, 64.25000000001196554, -111.6731074845243796 ) ) ;
#25761 = CARTESIAN_POINT ( 'NONE',  ( 21.04999999999999716, 36.17635217701701578, -235.9630383263116187 ) ) ;
#25762 = EDGE_CURVE ( 'NONE', #213598, #126780, #227317, .T. ) ;
#25764 = EDGE_LOOP ( 'NONE', ( #14597, #236378, #187817, #24058 ) ) ;
#25763 = CARTESIAN_POINT ( 'NONE',  ( -20.64999999999999858, 84.66355140188063899, -45.54720860259156723 ) ) ;
#25765 = FACE_OUTER_BOUND ( 'NONE', #59118, .T. ) ;
#25766 = CARTESIAN_POINT ( 'NONE',  ( -12.92414019175886253, 62.89253001998297776, -215.8738493471900028 ) ) ;
#25767 = B_SPLINE_CURVE_WITH_KNOTS ( 'NONE', 3,
 ( #119940, #84571, #143308, #179893, #1212, #222838, #58624, #140747, #101583, #203290, #24682, #178623, #138158, #39105, #239860, #161625 ),
 .UNSPECIFIED., .F., .F.,
 ( 4, 3, 3, 3, 3, 4 ),
 ( 0.000000000000000000, 2.209075297431620268E-05, 5.594258369009776820E-05, 8.979524372341989448E-05, 0.0001236472815274614490, 0.0001574990747609543082 ),
 .UNSPECIFIED. ) ;
#25768 = TOROIDAL_SURFACE ( 'NONE', #171550, 0.6000000000000004219, 0.1000000000000000056 ) ;
#25769 = CONICAL_SURFACE ( 'NONE', #167273, 4.299999999999956302, 0.7853981633974466137 ) ;
#25770 = CARTESIAN_POINT ( 'NONE',  ( -18.59999999999999787, 65.66751761918692409, -130.9282609406112670 ) ) ;
#25772 = EDGE_CURVE ( 'NONE', #192398, #8323, #245609, .T. ) ;
#25771 = ORIENTED_EDGE ( 'NONE', *, *, #122440, .F. ) ;
#25773 = VECTOR ( 'NONE', #82666, 999.9999999999998863 ) ;
#25774 = DIRECTION ( 'NONE',  ( -0.000000000000000000, -1.000000000000000000, -6.982962677686266711E-15 ) ) ;
#25775 = CARTESIAN_POINT ( 'NONE',  ( -18.40000000000000213, 54.02969457822032950, -229.1974241798695004 ) ) ;
#25776 = ORIENTED_EDGE ( 'NONE', *, *, #166640, .F. ) ;
#25777 = FACE_OUTER_BOUND ( 'NONE', #154684, .T. ) ;
#25778 = ORIENTED_EDGE ( 'NONE', *, *, #126757, .T. ) ;
#25779 = DIRECTION ( 'NONE',  ( 0.000000000000000000, 0.2617529984165027912, 0.9651348961777157509 ) ) ;
#25781 = EDGE_LOOP ( 'NONE', ( #199942, #124515, #255965, #239378 ) ) ;
#25780 = CARTESIAN_POINT ( 'NONE',  ( -21.04999999999994387, 64.35000000001120668, -3.123107484524795474 ) ) ;
#25782 = AXIS2_PLACEMENT_3D ( 'NONE', #71193, #192408, #251078 ) ;
#25785 = ORIENTED_EDGE ( 'NONE', *, *, #251746, .T. ) ;
#25784 = EDGE_LOOP ( 'NONE', ( #81497, #105633, #256559, #198364, #128077, #112117, #54102, #213460, #210791, #146171, #25490 ) ) ;
#25783 = CYLINDRICAL_SURFACE ( 'NONE', #213675, 1.500000000000001332 ) ;
#25786 = CARTESIAN_POINT ( 'NONE',  ( -18.40000000000000213, 11.33174054713631662, -79.65000000000004832 ) ) ;
#25787 = FACE_OUTER_BOUND ( 'NONE', #247418, .T. ) ;
#25788 = CARTESIAN_POINT ( 'NONE',  ( 21.05000000000000071, 76.00000000001205080, -124.3731074845242972 ) ) ;
#25790 = CARTESIAN_POINT ( 'NONE',  ( 18.59999999999999432, 1.162701749938009677, -8.099999999999999645 ) ) ;
#25789 = CARTESIAN_POINT ( 'NONE',  ( 23.14999999999999503, 69.45000000001252261, -182.2731074845244166 ) ) ;
#25791 = DIRECTION ( 'NONE',  ( 0.000000000000000000, 0.000000000000000000, 1.000000000000000000 ) ) ;
#25792 = CARTESIAN_POINT ( 'NONE',  ( -16.91256925476572093, 66.01426884188337851, -56.99074997352967387 ) ) ;
#25793 = CARTESIAN_POINT ( 'NONE',  ( -21.14999999999994174, 74.83745509109094485, -43.82310748452479743 ) ) ;
#25794 = DIRECTION ( 'NONE',  ( 0.000000000000000000, 0.9126074666063769270, 0.4088369013363280513 ) ) ;
#25795 = EDGE_LOOP ( 'NONE', ( #191251, #9367, #60859, #221843 ) ) ;
#25796 = VERTEX_POINT ( 'NONE', #186942 ) ;
#25797 = EDGE_CURVE ( 'NONE', #1620, #82189, #251047, .T. ) ;
#25798 = CARTESIAN_POINT ( 'NONE',  ( -20.85000000000000142, 64.25000000001175238, -76.30697314750248950 ) ) ;
#25799 = EDGE_CURVE ( 'NONE', #211613, #86491, #172005, .T. ) ;
#25801 = EDGE_LOOP ( 'NONE', ( #210344, #19332, #213487 ) ) ;
#25800 = CARTESIAN_POINT ( 'NONE',  ( -22.50000000000000000, 1.115600667400684642E-11, -21.85042919245520210 ) ) ;
#25802 = ORIENTED_EDGE ( 'NONE', *, *, #247500, .T. ) ;
#25804 = LINE ( 'NONE', #105300, #64363 ) ;
#25803 = CIRCLE ( 'NONE', #179940, 0.1000000000000028644 ) ;
#25805 = VERTEX_POINT ( 'NONE', #48675 ) ;
#25806 = EDGE_CURVE ( 'NONE', #7738, #113603, #112522, .T. ) ;
#25807 = ADVANCED_FACE ( 'NONE', ( #190801 ), #8290, .T. ) ;
#25808 = AXIS2_PLACEMENT_3D ( 'NONE', #56004, #234675, #215110 ) ;
#25809 = EDGE_LOOP ( 'NONE', ( #51057, #44422, #253029, #255023, #102770, #152214, #85431, #234827, #186789, #164004 ) ) ;
#25810 = CIRCLE ( 'NONE', #217512, 0.09999999999999609201 ) ;
#25811 = EDGE_CURVE ( 'NONE', #45832, #256245, #47043, .T. ) ;
#25813 = AXIS2_PLACEMENT_3D ( 'NONE', #167085, #83617, #245312 ) ;
#25812 = DIRECTION ( 'NONE',  ( 1.000000000000000000, 0.000000000000000000, 0.000000000000000000 ) ) ;
#25814 = CARTESIAN_POINT ( 'NONE',  ( -18.50000000000000000, 5.950000000011100632, -110.8057023050348988 ) ) ;
#25816 = VECTOR ( 'NONE', #2699, 1000.000000000000000 ) ;
#25815 = B_SPLINE_CURVE_WITH_KNOTS ( 'NONE', 3,
 ( #170039, #189566, #27945, #29240, #255562, #135653, #70923, #51292, #87855, #215208 ),
 .UNSPECIFIED., .F., .F.,
 ( 4, 3, 3, 4 ),
 ( 1.891637802867244836E-15, 3.877043166999269576E-05, 7.336897548475566824E-05, 7.659383120239756379E-05 ),
 .UNSPECIFIED. ) ;
#25817 = ADVANCED_FACE ( 'NONE', ( #246876 ), #255286, .F. ) ;
#25819 = EDGE_LOOP ( 'NONE', ( #45338, #125956, #172459, #1007 ) ) ;
#25818 = VERTEX_POINT ( 'NONE', #189491 ) ;
#25820 = ORIENTED_EDGE ( 'NONE', *, *, #52596, .F. ) ;
#25824 = ADVANCED_FACE ( 'NONE', ( #188201 ), #221992, .T. ) ;
#25823 = ADVANCED_FACE ( 'NONE', ( #250730 ), #188700, .T. ) ;
#25822 = DIRECTION ( 'NONE',  ( 0.000000000000000000, 0.000000000000000000, 1.000000000000000000 ) ) ;
#25821 = VECTOR ( 'NONE', #108043, 1000.000000000000000 ) ;
#25825 = EDGE_LOOP ( 'NONE', ( #157068, #67976, #250781, #127409 ) ) ;
#25826 = ORIENTED_EDGE ( 'NONE', *, *, #138172, .T. ) ;
#25827 = DIRECTION ( 'NONE',  ( 0.000000000000000000, 0.000000000000000000, -1.000000000000000000 ) ) ;
#25828 = DIRECTION ( 'NONE',  ( 0.000000000000000000, -0.9126074666063660468, -0.4088369013363524762 ) ) ;
#25829 = CIRCLE ( 'NONE', #17443, 0.09999999999998898659 ) ;
#25831 = ORIENTED_EDGE ( 'NONE', *, *, #138813, .T. ) ;
#25830 = DIRECTION ( 'NONE',  ( 0.000000000000000000, -0.9126074666063770380, -0.4088369013363281068 ) ) ;
#25832 = EDGE_CURVE ( 'NONE', #202242, #204776, #84612, .T. ) ;
#25833 = DIRECTION ( 'NONE',  ( 7.304098846218134667E-16, -1.000000000000000000, 0.000000000000000000 ) ) ;
#25834 = DIRECTION ( 'NONE',  ( 1.000000000000000000, -0.000000000000000000, -0.000000000000000000 ) ) ;
#25836 = EDGE_LOOP ( 'NONE', ( #242179, #1367, #135468, #151353 ) ) ;
#25835 = CARTESIAN_POINT ( 'NONE',  ( -11.59999999999994458, 67.75000000001118394, -21.02310748452479316 ) ) ;
#25837 = CARTESIAN_POINT ( 'NONE',  ( -16.94107738177415357, 10.01423928514777728, -180.0499999999999545 ) ) ;
#25838 = ORIENTED_EDGE ( 'NONE', *, *, #68350, .T. ) ;
#25839 = FACE_OUTER_BOUND ( 'NONE', #143418, .T. ) ;
#25840 = CIRCLE ( 'NONE', #121538, 6.258578643762724880 ) ;
#25841 = EDGE_LOOP ( 'NONE', ( #239221, #248234, #73881, #84631, #150600, #82985, #5231, #130720, #93174, #69596, #218813, #61290, #92360, #50469 ) ) ;
#25842 = CIRCLE ( 'NONE', #63225, 0.1000000000000089567 ) ;
#25843 = FACE_OUTER_BOUND ( 'NONE', #233355, .T. ) ;
#25845 = ADVANCED_FACE ( 'NONE', ( #10851 ), #5339, .F. ) ;
#25844 = CARTESIAN_POINT ( 'NONE',  ( 21.05000000000000071, 62.82351852614503684, -207.2177435922979214 ) ) ;
#25847 = ORIENTED_EDGE ( 'NONE', *, *, #4678, .T. ) ;
#25846 = AXIS2_PLACEMENT_3D ( 'NONE', #178384, #220051, #41435 ) ;
#25849 = DIRECTION ( 'NONE',  ( 1.000000000000000000, -2.849773892568378313E-16, 7.728835255496647986E-17 ) ) ;
#25848 = CARTESIAN_POINT ( 'NONE',  ( 21.78635804494511419, 0.09900506551883611617, -26.46433851484681909 ) ) ;
#25850 = ADVANCED_FACE ( 'NONE', ( #150369 ), #55076, .T. ) ;
#25852 = EDGE_CURVE ( 'NONE', #156652, #203538, #109594, .T. ) ;
#25851 = CIRCLE ( 'NONE', #129872, 0.1999999999999987899 ) ;
#25853 = CARTESIAN_POINT ( 'NONE',  ( 22.39999999999999503, 76.10000000001203091, -114.6726782920691079 ) ) ;
#25854 = LINE ( 'NONE', #105335, #205883 ) ;
#25855 = VERTEX_POINT ( 'NONE', #16008 ) ;
#25856 = ORIENTED_EDGE ( 'NONE', *, *, #194515, .F. ) ;
#25858 =( BOUNDED_CURVE ( )  B_SPLINE_CURVE ( 3, ( #174866, #254326, #112288, #114838 ),
 .UNSPECIFIED., .F., .F. ) 
 B_SPLINE_CURVE_WITH_KNOTS ( ( 4, 4 ),
 ( 3.141592653589793116, 4.712388980384689674 ),
 .UNSPECIFIED. ) 
 CURVE ( )  GEOMETRIC_REPRESENTATION_ITEM ( )  RATIONAL_B_SPLINE_CURVE ( ( 1.000000000000000000, 0.8047378541243649375, 0.8047378541243649375, 1.000000000000000000 ) ) 
 REPRESENTATION_ITEM ( '' )  );
#25857 = AXIS2_PLACEMENT_3D ( 'NONE', #124711, #162569, #204233 ) ;
#25859 = EDGE_CURVE ( 'NONE', #130019, #227981, #95511, .T. ) ;
#25860 = DIRECTION ( 'NONE',  ( 0.7071359030027593029, 0.7070776581709197206, 0.000000000000000000 ) ) ;
#25861 = CARTESIAN_POINT ( 'NONE',  ( 21.05000000000000071, -4.557064143889601127, -233.1584191572127622 ) ) ;
#25862 = VERTEX_POINT ( 'NONE', #17277 ) ;
#25863 = PLANE ( 'NONE',  #22470 ) ;
#25864 = ORIENTED_EDGE ( 'NONE', *, *, #97644, .T. ) ;
#25865 = DIRECTION ( 'NONE',  ( 0.000000000000000000, 6.982962677686266711E-15, -1.000000000000000000 ) ) ;
#25866 = TOROIDAL_SURFACE ( 'NONE', #59123, 0.2000000000000000111, 0.1000000000000000056 ) ;
#25867 = DIRECTION ( 'NONE',  ( 1.000000000000000000, 0.000000000000000000, 0.000000000000000000 ) ) ;
#25868 = ADVANCED_FACE ( 'NONE', ( #73417 ), #254556, .T. ) ;
#25869 = CARTESIAN_POINT ( 'NONE',  ( -20.64999999999999858, -8.999999999988844479, -124.1060308773475924 ) ) ;
#25870 = DIRECTION ( 'NONE',  ( 0.000000000000000000, -0.2128009952263602567, 0.9770955615653315052 ) ) ;
#25871 = EDGE_CURVE ( 'NONE', #140969, #65925, #226097, .T. ) ;
#25872 = EDGE_LOOP ( 'NONE', ( #69429, #47215, #111462, #26766 ) ) ;
#25873 = CARTESIAN_POINT ( 'NONE',  ( 18.44206774312977259, -9.491027357528896147, -207.6262275046982211 ) ) ;
#25874 = VECTOR ( 'NONE', #241832, 1000.000000000000000 ) ;
#25875 = AXIS2_PLACEMENT_3D ( 'NONE', #128899, #127613, #207154 ) ;
#25876 = VECTOR ( 'NONE', #183150, 1000.000000000000000 ) ;
#25877 = EDGE_LOOP ( 'NONE', ( #109433, #108807, #125141, #200957 ) ) ;
#25879 = EDGE_LOOP ( 'NONE', ( #110430, #115190, #69627, #33630 ) ) ;
#25878 = CIRCLE ( 'NONE', #17478, 7.800000000000001599 ) ;
#25880 = ORIENTED_EDGE ( 'NONE', *, *, #110373, .T. ) ;
#25881 = CARTESIAN_POINT ( 'NONE',  ( 22.48660254037843842, 64.25000000001213607, -136.5731074845243995 ) ) ;
#25882 = FACE_OUTER_BOUND ( 'NONE', #198597, .T. ) ;
#25883 = CARTESIAN_POINT ( 'NONE',  ( -18.59999999999999787, 12.85464084203975155, -205.2772944332067766 ) ) ;
#25884 = CARTESIAN_POINT ( 'NONE',  ( 22.94999999999999929, 0.000000000000000000, 0.000000000000000000 ) ) ;
#25885 = DIRECTION ( 'NONE',  ( 1.000000000000000000, 0.000000000000000000, 0.000000000000000000 ) ) ;
#25886 = EDGE_CURVE ( 'NONE', #219487, #226256, #142888, .T. ) ;
#25888 = LINE ( 'NONE', #201948, #186681 ) ;
#25887 = CARTESIAN_POINT ( 'NONE',  ( 22.42357213249528769, 68.32706761365174941, -69.62219444852593142 ) ) ;
#25890 = ORIENTED_EDGE ( 'NONE', *, *, #255178, .F. ) ;
#25889 = DIRECTION ( 'NONE',  ( 0.000000000000000000, -0.01562499999996560217, -0.9998779222360102414 ) ) ;
#25891 = CARTESIAN_POINT ( 'NONE',  ( -21.11825140030082792, 6.445407565431271024, -167.4927963793673200 ) ) ;
#25892 = ORIENTED_EDGE ( 'NONE', *, *, #197278, .T. ) ;
#25893 = FACE_OUTER_BOUND ( 'NONE', #171226, .T. ) ;
#25894 = ORIENTED_EDGE ( 'NONE', *, *, #103570, .T. ) ;
#25895 = ORIENTED_EDGE ( 'NONE', *, *, #201300, .F. ) ;
#25896 = DIRECTION ( 'NONE',  ( 0.000000000000000000, -0.4088369013363296611, 0.9126074666063762608 ) ) ;
#25897 = LINE ( 'NONE', #105376, #150230 ) ;
#25898 = CARTESIAN_POINT ( 'NONE',  ( 15.06592377766031809, 9.417789466963361278, -82.35738454397692010 ) ) ;
#25899 = DIRECTION ( 'NONE',  ( 0.000000000000000000, -0.4721928772777346239, -0.8814952561688430555 ) ) ;
#25900 = EDGE_LOOP ( 'NONE', ( #197043, #182394, #25143 ) ) ;
#25901 = ORIENTED_EDGE ( 'NONE', *, *, #144006, .F. ) ;
#25902 = DIRECTION ( 'NONE',  ( 0.000000000000000000, 1.000000000000000000, 6.982962677686266711E-15 ) ) ;
#25903 = VERTEX_POINT ( 'NONE', #233756 ) ;
#25904 = CARTESIAN_POINT ( 'NONE',  ( 20.94999999999999929, -4.892732937820623462, -233.2805462221312496 ) ) ;
#25905 = CARTESIAN_POINT ( 'NONE',  ( -21.55000000000000071, 44.92467540951147953, -237.7943620901849613 ) ) ;
#25906 = CYLINDRICAL_SURFACE ( 'NONE', #202998, 0.1000000000000028644 ) ;
#25907 = CARTESIAN_POINT ( 'NONE',  ( 21.07928932188134397, -1.250084634896337255, -194.7953894783290423 ) ) ;
#25908 = CARTESIAN_POINT ( 'NONE',  ( -21.14999999999999858, 76.10000000001222986, -148.1726782920690937 ) ) ;
#25909 = LINE ( 'NONE', #10200, #59087 ) ;
#25910 = EDGE_LOOP ( 'NONE', ( #235028, #61536, #238740 ) ) ;
#25911 = DIRECTION ( 'NONE',  ( 1.000000000000000000, -0.000000000000000000, 0.000000000000000000 ) ) ;
#25912 = FACE_OUTER_BOUND ( 'NONE', #157589, .T. ) ;
#25913 = DIRECTION ( 'NONE',  ( 1.000000000000000000, -0.000000000000000000, -0.000000000000000000 ) ) ;
#25914 = CARTESIAN_POINT ( 'NONE',  ( 18.49999999999999289, 10.49142135623730709, -24.85000000000000142 ) ) ;
#25915 = EDGE_CURVE ( 'NONE', #22985, #180615, #113691, .T. ) ;
#25916 = LINE ( 'NONE', #49314, #87215 ) ;
#25917 = DIRECTION ( 'NONE',  ( 0.000000000000000000, 0.000000000000000000, 1.000000000000000000 ) ) ;
#25918 = EDGE_CURVE ( 'NONE', #77679, #110820, #176359, .T. ) ;
#25920 = ORIENTED_EDGE ( 'NONE', *, *, #50190, .F. ) ;
#25919 = VECTOR ( 'NONE', #179276, 1000.000000000000000 ) ;
#25921 = ADVANCED_FACE ( 'NONE', ( #212901 ), #22143, .T. ) ;
#25922 = FACE_OUTER_BOUND ( 'NONE', #242830, .T. ) ;
#25923 = EDGE_CURVE ( 'NONE', #133253, #219149, #1250, .T. ) ;
#25924 = VERTEX_POINT ( 'NONE', #18554 ) ;
#25925 = DIRECTION ( 'NONE',  ( 1.000000000000000000, 0.000000000000000000, 0.000000000000000000 ) ) ;
#25926 = CYLINDRICAL_SURFACE ( 'NONE', #173071, 0.09999999999998898659 ) ;
#25927 = DIRECTION ( 'NONE',  ( 0.000000000000000000, -1.000000000000000000, 0.000000000000000000 ) ) ;
#25928 = ORIENTED_EDGE ( 'NONE', *, *, #31723, .T. ) ;
#25929 = DIRECTION ( 'NONE',  ( -0.000000000000000000, 0.8814952561688430555, -0.4721928772777346239 ) ) ;
#25930 = FACE_OUTER_BOUND ( 'NONE', #64146, .T. ) ;
#25931 = LINE ( 'NONE', #144567, #89691 ) ;
#25932 = CARTESIAN_POINT ( 'NONE',  ( 22.88900146558018989, 8.703904791123973084, -180.1499999999999773 ) ) ;
#25933 = CIRCLE ( 'NONE', #217611, 0.1000000000000022676 ) ;
#25934 = CARTESIAN_POINT ( 'NONE',  ( -20.15000000000000568, 44.03968997137859986, -236.0634901547873312 ) ) ;
#25935 = VECTOR ( 'NONE', #75727, 1000.000000000000000 ) ;
#25936 = EDGE_CURVE ( 'NONE', #34168, #72701, #201171, .T. ) ;
#25937 = EDGE_LOOP ( 'NONE', ( #207143, #140432, #202548, #152228 ) ) ;
#25938 = EDGE_LOOP ( 'NONE', ( #12544, #149152, #84362, #95821 ) ) ;
#25939 = CARTESIAN_POINT ( 'NONE',  ( -18.50000000000000711, 11.75000000001115197, -40.51480577065400013 ) ) ;
#25941 = ORIENTED_EDGE ( 'NONE', *, *, #107506, .F. ) ;
#25940 = DIRECTION ( 'NONE',  ( -0.000000000000000000, 0.9651348961777158619, -0.2617529984165030132 ) ) ;
#25943 = DIRECTION ( 'NONE',  ( -1.000000000000000000, -0.000000000000000000, -0.000000000000000000 ) ) ;
#25942 = AXIS2_PLACEMENT_3D ( 'NONE', #123696, #85800, #4993 ) ;
#25944 = DIRECTION ( 'NONE',  ( 0.000000000000000000, 0.000000000000000000, -1.000000000000000000 ) ) ;
#25945 = EDGE_LOOP ( 'NONE', ( #53007, #211515, #94727, #39584 ) ) ;
#25946 = DIRECTION ( 'NONE',  ( -1.000000000000000000, 0.000000000000000000, 0.000000000000000000 ) ) ;
#25947 = ITEM_DEFINED_TRANSFORMATION ( 'NONE', 'NONE', #206984,  #2425 ) ;
#25948 = B_SPLINE_CURVE_WITH_KNOTS ( 'NONE', 3,
 ( #132064, #34283, #252004, #246863, #248162, #207774, #73407, #49950, #209035, #150357, #229887, #152949, #30412, #232471, #147788, #189479, #133356, #212891, #227305, #48667, #51209, #90358, #130775, #210331, #31715, #254544 ),
 .UNSPECIFIED., .F., .F.,
 ( 4, 2, 2, 2, 2, 2, 2, 2, 2, 2, 2, 2, 4 ),
 ( 0.005476422646581347378, 0.006160811967703578272, 0.006845201288825809166, 0.007187395949386910302, 0.007529590609948011437, 0.007871785270509112573, 0.008213979931070213708, 0.008556174591631314844, 0.008898369252192415979, 0.009240563912753515380, 0.009582758573314618250, 0.01026714789443681879, 0.01095153721555902106 ),
 .UNSPECIFIED. ) ;
#25949 = CARTESIAN_POINT ( 'NONE',  ( -21.37071067811865532, 8.070710678129811910, -179.7499999999999716 ) ) ;
#25950 = CIRCLE ( 'NONE', #204980, 7.900000000000003908 ) ;
#25951 = ORIENTED_EDGE ( 'NONE', *, *, #176024, .F. ) ;
#25952 = VECTOR ( 'NONE', #229413, 1000.000000000000000 ) ;
#25953 = DIRECTION ( 'NONE',  ( 0.000000000000000000, 0.8814952561688437216, -0.4721928772777334582 ) ) ;
#25954 = ADVANCED_FACE ( 'NONE', ( #193350 ), #130449, .T. ) ;
#25955 = DIRECTION ( 'NONE',  ( 0.000000000000000000, 0.000000000000000000, -1.000000000000000000 ) ) ;
#25956 = ORIENTED_EDGE ( 'NONE', *, *, #41216, .T. ) ;
#25957 = ORIENTED_EDGE ( 'NONE', *, *, #216098, .T. ) ;
#25958 = CARTESIAN_POINT ( 'NONE',  ( -20.94999999999999929, 16.44800918141279666, -240.8068063186265135 ) ) ;
#25959 = DIRECTION ( 'NONE',  ( 0.000000000000000000, 0.000000000000000000, 1.000000000000000000 ) ) ;
#25960 = CARTESIAN_POINT ( 'NONE',  ( -18.59999999999999787, 14.80545736607782814, -235.9842437978701639 ) ) ;
#25961 = EDGE_CURVE ( 'NONE', #147896, #117855, #237602, .T. ) ;
#25962 = CARTESIAN_POINT ( 'NONE',  ( -21.09610168723073187, 69.62104428478716045, -103.0566969914158477 ) ) ;
#25963 = CARTESIAN_POINT ( 'NONE',  ( 22.10000000000000497, 10.21702379168713115, -11.24211197275198160 ) ) ;
#25965 = DIRECTION ( 'NONE',  ( 1.000000000000000000, 0.000000000000000000, 0.000000000000000000 ) ) ;
#25964 = CIRCLE ( 'NONE', #229968, 0.1000000000000013933 ) ;
#25966 = VECTOR ( 'NONE', #60568, 999.9999999999998863 ) ;
#25967 = CARTESIAN_POINT ( 'NONE',  ( -11.59999999999994458, 64.35000000001120668, -18.32310748452479388 ) ) ;
#25968 = EDGE_CURVE ( 'NONE', #168616, #38453, #235038, .T. ) ;
#25971 = DIRECTION ( 'NONE',  ( -1.000000000000000000, 0.000000000000000000, 0.000000000000000000 ) ) ;
#25970 = AXIS2_PLACEMENT_3D ( 'NONE', #81099, #22451, #240206 ) ;
#25969 = CARTESIAN_POINT ( 'NONE',  ( -20.64999999999999858, 82.22731448072437388, -214.9453318841612486 ) ) ;
#25972 = DIRECTION ( 'NONE',  ( 0.000000000000000000, 0.000000000000000000, -1.000000000000000000 ) ) ;
#25973 = CARTESIAN_POINT ( 'NONE',  ( -23.25000000000000355, 5.650000000011139001, -46.15000000000000568 ) ) ;
#25974 = DIRECTION ( 'NONE',  ( 0.000000000000000000, 0.000000000000000000, 1.000000000000000000 ) ) ;
#25975 = ORIENTED_EDGE ( 'NONE', *, *, #9101, .F. ) ;
#25976 = VERTEX_POINT ( 'NONE', #94221 ) ;
#25977 = CARTESIAN_POINT ( 'NONE',  ( 23.14999999999999858, 38.42191493408704872, -250.4955484557988541 ) ) ;
#25978 = CARTESIAN_POINT ( 'NONE',  ( -18.50000000000000000, 45.53758419368699606, -241.2860287061636768 ) ) ;
#25980 = FACE_OUTER_BOUND ( 'NONE', #6990, .T. ) ;
#25979 = CARTESIAN_POINT ( 'NONE',  ( -21.05000000000000426, 69.52295361822210396, -102.9231074845243512 ) ) ;
#25981 = ADVANCED_FACE ( 'NONE', ( #56368 ), #47158, .T. ) ;
#25982 = CARTESIAN_POINT ( 'NONE',  ( 20.95568717954149562, 39.26254392658486125, -236.7675178030809207 ) ) ;
#25983 = CARTESIAN_POINT ( 'NONE',  ( -20.94999999999999929, 1.736257131597397585, -11.56865232901749962 ) ) ;
#25984 = LINE ( 'NONE', #7709, #94048 ) ;
#25985 = EDGE_CURVE ( 'NONE', #26858, #72558, #217731, .T. ) ;
#25986 = EDGE_CURVE ( 'NONE', #6078, #191026, #144895, .T. ) ;
#25987 = VERTEX_POINT ( 'NONE', #40719 ) ;
#25988 = ORIENTED_EDGE ( 'NONE', *, *, #66503, .T. ) ;
#25989 = CARTESIAN_POINT ( 'NONE',  ( -12.30589683808040391, 9.356746017078247490, -17.20335972136419400 ) ) ;
#25990 = ADVANCED_FACE ( 'NONE', ( #203601 ), #82336, .F. ) ;
#25991 = EDGE_LOOP ( 'NONE', ( #188133, #126825, #126216, #40834 ) ) ;
#25992 = DIRECTION ( 'NONE',  ( 0.000000000000000000, 0.000000000000000000, 1.000000000000000000 ) ) ;
#25993 = AXIS2_PLACEMENT_3D ( 'NONE', #113394, #252893, #33905 ) ;
#25994 = DIRECTION ( 'NONE',  ( 1.186688945009010077E-16, 1.000000000000000000, 6.982962677686266711E-15 ) ) ;
#25995 = ORIENTED_EDGE ( 'NONE', *, *, #214896, .F. ) ;
#25996 = DIRECTION ( 'NONE',  ( 0.000000000000000000, 0.2617529984164980728, 0.9651348961777171942 ) ) ;
#25997 = EDGE_CURVE ( 'NONE', #92780, #44979, #101172, .T. ) ;
#25998 = AXIS2_PLACEMENT_3D ( 'NONE', #100808, #20052, #81265 ) ;
#25999 = ORIENTED_EDGE ( 'NONE', *, *, #55270, .F. ) ;
#26000 = CARTESIAN_POINT ( 'NONE',  ( -18.60000000000001563, 85.36424052760324344, -162.8428589026835311 ) ) ;
#26001 = DIRECTION ( 'NONE',  ( -1.000000000000000000, 0.000000000000000000, 0.000000000000000000 ) ) ;
#26003 = TOROIDAL_SURFACE ( 'NONE', #121867, 14.20833333333334103, 0.1000000000000000056 ) ;
#26002 = CARTESIAN_POINT ( 'NONE',  ( 20.04142135623730070, 62.43966442355481661, -209.0151288841454118 ) ) ;
#26004 = CARTESIAN_POINT ( 'NONE',  ( 18.59999994388910238, -9.363566187060129664, -141.1811172368007590 ) ) ;
#26005 = DIRECTION ( 'NONE',  ( 0.000000000000000000, 0.000000000000000000, -1.000000000000000000 ) ) ;
#26006 = DIRECTION ( 'NONE',  ( 0.000000000000000000, 6.938893903907030216E-14, -1.000000000000000000 ) ) ;
#26007 = AXIS2_PLACEMENT_3D ( 'NONE', #56181, #236118, #60037 ) ;
#26008 = FACE_OUTER_BOUND ( 'NONE', #125155, .T. ) ;
#26010 = DIRECTION ( 'NONE',  ( 0.000000000000000000, 0.000000000000000000, -1.000000000000000000 ) ) ;
#26009 = CIRCLE ( 'NONE', #184203, 7.791421356237304252 ) ;
#26011 = AXIS2_PLACEMENT_3D ( 'NONE', #97627, #177225, #52092 ) ;
#26013 = ORIENTED_EDGE ( 'NONE', *, *, #142777, .T. ) ;
#26012 = CARTESIAN_POINT ( 'NONE',  ( 18.31325810956367661, -0.7275186016206726114, -242.4731767114571142 ) ) ;
#26015 = DIRECTION ( 'NONE',  ( 0.000000000000000000, -0.9908441862701605762, 0.1350103645451835310 ) ) ;
#26014 = DIRECTION ( 'NONE',  ( 0.000000000000000000, -0.9126074666063660468, -0.4088369013363524762 ) ) ;
#26016 = ORIENTED_EDGE ( 'NONE', *, *, #142093, .T. ) ;
#26018 = EDGE_LOOP ( 'NONE', ( #163896, #203149, #73598, #62250 ) ) ;
#26017 = FACE_OUTER_BOUND ( 'NONE', #249224, .T. ) ;
#26019 = EDGE_LOOP ( 'NONE', ( #254521, #234828, #73886, #90759 ) ) ;
#26020 = CARTESIAN_POINT ( 'NONE',  ( -18.50000000000000000, 97.49741144064424248, -225.2667035127916790 ) ) ;
#26021 = AXIS2_PLACEMENT_3D ( 'NONE', #59572, #139107, #218667 ) ;
#26022 = CARTESIAN_POINT ( 'NONE',  ( -18.50000000000000000, 70.05000000001236060, -159.7174051794895320 ) ) ;
#26023 = AXIS2_PLACEMENT_3D ( 'NONE', #217788, #39204, #200823 ) ;
#26024 = CARTESIAN_POINT ( 'NONE',  ( -21.98333005346336932, 0.6286209188979320350, -230.2507154655492627 ) ) ;
#26025 = DIRECTION ( 'NONE',  ( 0.000000000000000000, 0.000000000000000000, 1.000000000000000000 ) ) ;
#26026 = DIRECTION ( 'NONE',  ( 1.000000000000000000, 0.000000000000000000, 0.000000000000000000 ) ) ;
#26027 = ORIENTED_EDGE ( 'NONE', *, *, #117857, .F. ) ;
#26028 = VECTOR ( 'NONE', #85485, 1000.000000000000000 ) ;
#26029 = DIRECTION ( 'NONE',  ( 0.000000000000000000, -1.000000000000000000, -1.734723475976807292E-15 ) ) ;
#26030 = CIRCLE ( 'NONE', #246580, 0.09999999999999939493 ) ;
#26031 = CARTESIAN_POINT ( 'NONE',  ( 21.05000000000000071, 87.65000000001235492, -167.1231074845242688 ) ) ;
#26032 = CIRCLE ( 'NONE', #9266, 0.3999999999999975797 ) ;
#26033 = AXIS2_PLACEMENT_3D ( 'NONE', #119835, #40312, #58533 ) ;
#26034 = ORIENTED_EDGE ( 'NONE', *, *, #610, .T. ) ;
#26035 = ORIENTED_EDGE ( 'NONE', *, *, #43006, .F. ) ;
#26036 = CARTESIAN_POINT ( 'NONE',  ( -20.94999999999999929, 87.41227409416133298, -66.52310748452423184 ) ) ;
#26037 = AXIS2_PLACEMENT_3D ( 'NONE', #171267, #89102, #90380 ) ;
#26038 = EDGE_CURVE ( 'NONE', #198003, #28211, #160658, .T. ) ;
#26039 = EDGE_LOOP ( 'NONE', ( #178469, #59495 ) ) ;
#26040 = DIRECTION ( 'NONE',  ( 0.000000000000000000, 1.000000000000000000, 1.156482317317864980E-14 ) ) ;
#26041 = ORIENTED_EDGE ( 'NONE', *, *, #231747, .F. ) ;
#26043 = AXIS2_PLACEMENT_3D ( 'NONE', #145047, #159502, #99482 ) ;
#26042 = CARTESIAN_POINT ( 'NONE',  ( 18.59999999999999076, 69.45000000001206786, -126.5060803140843291 ) ) ;
#26044 = AXIS2_PLACEMENT_3D ( 'NONE', #129828, #211961, #33351 ) ;
#26045 = DIRECTION ( 'NONE',  ( 0.000000000000000000, -0.000000000000000000, -1.000000000000000000 ) ) ;
#26046 = DIRECTION ( 'NONE',  ( 0.000000000000000000, -0.1350103645451876944, -0.9908441862701601321 ) ) ;
#26048 = ADVANCED_FACE ( 'NONE', ( #23716 ), #72012, .T. ) ;
#26047 = TOROIDAL_SURFACE ( 'NONE', #100989, 14.20833333333334103, 0.1000000000000000056 ) ;
#26049 = DIRECTION ( 'NONE',  ( 0.000000000000000000, 0.000000000000000000, 1.000000000000000000 ) ) ;
#26050 = DIRECTION ( 'NONE',  ( 1.000000000000000000, 0.000000000000000000, 0.000000000000000000 ) ) ;
#26051 = VERTEX_POINT ( 'NONE', #224441 ) ;
#26052 = EDGE_CURVE ( 'NONE', #187198, #85045, #80519, .T. ) ;
#26053 = ADVANCED_FACE ( 'NONE', ( #83612 ), #104472, .F. ) ;
#26054 = CARTESIAN_POINT ( 'NONE',  ( -16.98495255085917321, 51.61018462143365326, -231.8894715066228116 ) ) ;
#26055 = CARTESIAN_POINT ( 'NONE',  ( 18.59999999999999787, 85.32100840337291459, -62.28716923544639172 ) ) ;
#26056 = CARTESIAN_POINT ( 'NONE',  ( -23.25000000000000000, 1.115600667400684642E-11, -67.00000000000004263 ) ) ;
#26057 = ORIENTED_EDGE ( 'NONE', *, *, #700, .T. ) ;
#26059 = LINE ( 'NONE', #101692, #193852 ) ;
#26058 = FACE_OUTER_BOUND ( 'NONE', #94109, .T. ) ;
#26060 = ORIENTED_EDGE ( 'NONE', *, *, #158614, .F. ) ;
#26062 = ORIENTED_EDGE ( 'NONE', *, *, #175817, .F. ) ;
#26061 = SURFACE_STYLE_FILL_AREA ( #202122 ) ;
#26063 = AXIS2_PLACEMENT_3D ( 'NONE', #187663, #33749, #248908 ) ;
#26064 = VERTEX_POINT ( 'NONE', #120258 ) ;
#26065 = DIRECTION ( 'NONE',  ( 0.000000000000000000, -0.6728971962617388280, 0.7397360091702248619 ) ) ;
#26066 = CIRCLE ( 'NONE', #167723, 0.09999999999999939493 ) ;
#26067 = DIRECTION ( 'NONE',  ( 0.000000000000000000, 0.4088369013363281623, -0.9126074666063771490 ) ) ;
#26068 = FACE_OUTER_BOUND ( 'NONE', #39914, .T. ) ;
#26069 = ORIENTED_EDGE ( 'NONE', *, *, #210771, .T. ) ;
#26070 = DIRECTION ( 'NONE',  ( 1.000000000000000000, -7.304098846218163263E-16, 4.217023435051626718E-16 ) ) ;
#26071 = EDGE_CURVE ( 'NONE', #100213, #181223, #65373, .T. ) ;
#26072 = CARTESIAN_POINT ( 'NONE',  ( -16.89268316805466341, 9.951721813253341153, -113.1442475214544885 ) ) ;
#26073 = EDGE_CURVE ( 'NONE', #135203, #6205, #122256, .T. ) ;
#26075 = CARTESIAN_POINT ( 'NONE',  ( -21.05000000000000071, -11.48912529306489994, -97.40000000000004832 ) ) ;
#26074 = CARTESIAN_POINT ( 'NONE',  ( -22.49544290803771318, 11.74987023785715934, 0.06531195925749262721 ) ) ;
#26077 = ORIENTED_EDGE ( 'NONE', *, *, #104139, .T. ) ;
#26076 = FACE_OUTER_BOUND ( 'NONE', #204314, .T. ) ;
#26078 = ORIENTED_EDGE ( 'NONE', *, *, #108852, .T. ) ;
#26079 = CARTESIAN_POINT ( 'NONE',  ( -16.88815647973234135, 9.950832619326893891, -79.64721706332603901 ) ) ;
#26080 = AXIS2_PLACEMENT_3D ( 'NONE', #3380, #162493, #123358 ) ;
#26081 = PLANE ( 'NONE',  #127060 ) ;
#26082 = LINE ( 'NONE', #164310, #251355 ) ;
#26083 = VERTEX_POINT ( 'NONE', #159360 ) ;
#26084 = DIRECTION ( 'NONE',  ( -0.000000000000000000, -0.000000000000000000, -1.000000000000000000 ) ) ;
#26085 = ORIENTED_EDGE ( 'NONE', *, *, #34149, .T. ) ;
#26086 = EDGE_CURVE ( 'NONE', #113219, #256686, #5699, .T. ) ;
#26087 = DIRECTION ( 'NONE',  ( 0.000000000000000000, -6.982962677686266711E-15, 1.000000000000000000 ) ) ;
#26088 = AXIS2_PLACEMENT_3D ( 'NONE', #90082, #168407, #191799 ) ;
#26090 = EDGE_CURVE ( 'NONE', #255448, #221704, #88912, .T. ) ;
#26089 = DIRECTION ( 'NONE',  ( 1.000000000000000000, 0.000000000000000000, 0.000000000000000000 ) ) ;
#26091 = CARTESIAN_POINT ( 'NONE',  ( 21.05000000000000071, 70.15000000001192859, -92.89061026024637613 ) ) ;
#26092 = EDGE_CURVE ( 'NONE', #222344, #15852, #30701, .T. ) ;
#26093 = ORIENTED_EDGE ( 'NONE', *, *, #155266, .F. ) ;
#26094 = CARTESIAN_POINT ( 'NONE',  ( -23.15000000000000213, 11.65000000001115588, -59.98519422934605672 ) ) ;
#26096 = EDGE_CURVE ( 'NONE', #248002, #55604, #151502, .T. ) ;
#26095 = ORIENTED_EDGE ( 'NONE', *, *, #228834, .T. ) ;
#26097 = MANIFOLD_SOLID_BREP ( 'Stock-MAS-200-1', #223943 ) ;
#26098 = CARTESIAN_POINT ( 'NONE',  ( 20.94999999999999929, 87.48912529308749697, -39.02310748452423894 ) ) ;
#26100 = ORIENTED_EDGE ( 'NONE', *, *, #7181, .F. ) ;
#26099 = AXIS2_PLACEMENT_3D ( 'NONE', #188539, #172880, #249801 ) ;
#26101 = ORIENTED_EDGE ( 'NONE', *, *, #48804, .T. ) ;
#26102 = VERTEX_POINT ( 'NONE', #132756 ) ;
#26103 = CARTESIAN_POINT ( 'NONE',  ( -23.15000000000000213, 11.65000000001115588, -45.75000000000000000 ) ) ;
#26104 = EDGE_LOOP ( 'NONE', ( #191098, #134889, #24362, #128907 ) ) ;
#26106 = ORIENTED_EDGE ( 'NONE', *, *, #62238, .F. ) ;
#26105 = CARTESIAN_POINT ( 'NONE',  ( -22.24259225415828567, 7.491937870565431368, 0.09906588345283832975 ) ) ;
#26107 = EDGE_LOOP ( 'NONE', ( #67551, #227466, #210412, #220654 ) ) ;
#26110 = ADVANCED_FACE ( 'NONE', ( #212290 ), #167081, .T. ) ;
#26109 = VERTEX_POINT ( 'NONE', #81066 ) ;
#26108 = ORIENTED_EDGE ( 'NONE', *, *, #200067, .T. ) ;
#26111 = CARTESIAN_POINT ( 'NONE',  ( -18.36527282682037310, -9.500000599987968641, -107.4221489644983905 ) ) ;
#26112 = CIRCLE ( 'NONE', #151190, 0.1000000000000000472 ) ;
#26113 = VERTEX_POINT ( 'NONE', #45811 ) ;
#26114 = DIRECTION ( 'NONE',  ( 0.000000000000000000, 0.000000000000000000, -1.000000000000000000 ) ) ;
#26115 = CARTESIAN_POINT ( 'NONE',  ( 15.74999999999999645, 66.65000000001185754, -86.27310748452437394 ) ) ;
#26116 = AXIS2_PLACEMENT_3D ( 'NONE', #203673, #184101, #245378 ) ;
#26117 = CARTESIAN_POINT ( 'NONE',  ( 20.94999999999999929, 4.999999999999997335, -21.59473398108690390 ) ) ;
#26118 = VERTEX_POINT ( 'NONE', #252664 ) ;
#26119 = ORIENTED_EDGE ( 'NONE', *, *, #173029, .F. ) ;
#26120 = AXIS2_PLACEMENT_3D ( 'NONE', #47989, #192655, #70159 ) ;
#26121 = ADVANCED_FACE ( 'NONE', ( #54472 ), #146187, .T. ) ;
#26122 = DIRECTION ( 'NONE',  ( 0.000000000000000000, 6.982962677686266711E-15, -1.000000000000000000 ) ) ;
#26124 = ORIENTED_EDGE ( 'NONE', *, *, #153269, .T. ) ;
#26123 = CARTESIAN_POINT ( 'NONE',  ( -16.93433913041102912, 65.99402157848859929, -182.5877420571292760 ) ) ;
#26125 = CARTESIAN_POINT ( 'NONE',  ( -16.87786941232800686, 14.17275468830522556, -219.2799003491669225 ) ) ;
#26127 = ORIENTED_EDGE ( 'NONE', *, *, #237002, .F. ) ;
#26126 = DIRECTION ( 'NONE',  ( 0.000000000000000000, 0.2617529984165031243, 0.9651348961777157509 ) ) ;
#26128 = EDGE_LOOP ( 'NONE', ( #236561, #128336, #103187 ) ) ;
#26129 = DIRECTION ( 'NONE',  ( 0.000000000000000000, 0.000000000000000000, -1.000000000000000000 ) ) ;
#26130 = ADVANCED_FACE ( 'NONE', ( #213542 ), #246571, .T. ) ;
#26131 = CIRCLE ( 'NONE', #213549, 12.97499999999999964 ) ;
#26132 = CIRCLE ( 'NONE', #171908, 0.1000000000000054040 ) ;
#26133 = ORIENTED_EDGE ( 'NONE', *, *, #114491, .T. ) ;
#26134 = ORIENTED_EDGE ( 'NONE', *, *, #142171, .F. ) ;
#26135 = CARTESIAN_POINT ( 'NONE',  ( -16.89935556175703368, 9.950000000011137047, -180.6396763628857514 ) ) ;
#26136 = CARTESIAN_POINT ( 'NONE',  ( -21.13422380239137510, 1.115580863182033025E-11, -161.0066734851942556 ) ) ;
#26137 = EDGE_CURVE ( 'NONE', #49363, #200563, #131446, .T. ) ;
#26139 = ORIENTED_EDGE ( 'NONE', *, *, #156993, .T. ) ;
#26138 = ORIENTED_EDGE ( 'NONE', *, *, #8410, .F. ) ;
#26140 = EDGE_LOOP ( 'NONE', ( #94462, #93458, #242591, #144337 ) ) ;
#26142 = EDGE_CURVE ( 'NONE', #103174, #254691, #147200, .T. ) ;
#26141 = CARTESIAN_POINT ( 'NONE',  ( -22.50000000000094147, 64.08545097430051385, -247.0723585184914555 ) ) ;
#26143 = ORIENTED_EDGE ( 'NONE', *, *, #36546, .F. ) ;
#26144 = ORIENTED_EDGE ( 'NONE', *, *, #136555, .F. ) ;
#26146 = LINE ( 'NONE', #66548, #71984 ) ;
#26145 = CIRCLE ( 'NONE', #88455, 0.09999999999998898659 ) ;
#26148 = VERTEX_POINT ( 'NONE', #174486 ) ;
#26147 = CARTESIAN_POINT ( 'NONE',  ( -20.94999999999999929, 40.27305497204160645, -251.4871534980821082 ) ) ;
#26149 = DIRECTION ( 'NONE',  ( -1.000000000000000000, -0.000000000000000000, -0.000000000000000000 ) ) ;
#26151 = CARTESIAN_POINT ( 'NONE',  ( 18.47073956224755875, -9.471729412460639708, -107.6086857528181753 ) ) ;
#26150 = CARTESIAN_POINT ( 'NONE',  ( -18.59999999999999787, 44.10700160683882132, -235.9691471569721841 ) ) ;
#26152 = CARTESIAN_POINT ( 'NONE',  ( 18.46947024752525479, 85.50929715716861779, -196.5364180358262161 ) ) ;
#26153 = CARTESIAN_POINT ( 'NONE',  ( -14.45443560709636621, 62.05118075326794980, -218.8501529344108008 ) ) ;
#26154 = ORIENTED_EDGE ( 'NONE', *, *, #236306, .F. ) ;
#26155 = AXIS2_PLACEMENT_3D ( 'NONE', #76258, #193659, #15036 ) ;
#26156 = AXIS2_PLACEMENT_3D ( 'NONE', #94975, #179667, #143071 ) ;
#26157 = VECTOR ( 'NONE', #130511, 1000.000000000000000 ) ;
#26158 = ORIENTED_EDGE ( 'NONE', *, *, #155311, .F. ) ;
#26159 = TOROIDAL_SURFACE ( 'NONE', #142638, 4.149999999999999467, 0.1000000000000000056 ) ;
#26160 = DIRECTION ( 'NONE',  ( 1.000000000000000000, 0.000000000000000000, 0.000000000000000000 ) ) ;
#26161 = ADVANCED_FACE ( 'NONE', ( #51889 ), #32387, .F. ) ;
#26162 = ORIENTED_EDGE ( 'NONE', *, *, #188336, .T. ) ;
#26163 = EDGE_CURVE ( 'NONE', #232311, #120786, #68085, .T. ) ;
#26164 = DIRECTION ( 'NONE',  ( 0.000000000000000000, 1.000000000000000000, 0.000000000000000000 ) ) ;
#26165 = ORIENTED_EDGE ( 'NONE', *, *, #235985, .T. ) ;
#26166 = ORIENTED_EDGE ( 'NONE', *, *, #79899, .F. ) ;
#26167 = ADVANCED_FACE ( 'NONE', ( #231854 ), #126352, .F. ) ;
#26168 = ORIENTED_EDGE ( 'NONE', *, *, #103265, .F. ) ;
#26169 = DIRECTION ( 'NONE',  ( 0.000000000000000000, 0.000000000000000000, 1.000000000000000000 ) ) ;
#26170 = CARTESIAN_POINT ( 'NONE',  ( 18.59999999999999076, 46.02130280899747561, -256.6489974955837852 ) ) ;
#26171 = ORIENTED_EDGE ( 'NONE', *, *, #210310, .F. ) ;
#26172 = CARTESIAN_POINT ( 'NONE',  ( 20.04142135391667168, 64.25000000001220712, -145.3206006188949004 ) ) ;
#26173 = DIRECTION ( 'NONE',  ( 1.000000000000000000, 0.000000000000000000, 0.000000000000000000 ) ) ;
#26175 = CARTESIAN_POINT ( 'NONE',  ( -18.40000000000000213, 70.35000000001153353, -48.67310748452436542 ) ) ;
#26174 = DIRECTION ( 'NONE',  ( -0.000000000000000000, -0.2814428106787469908, -0.9595780032479106492 ) ) ;
#26176 = FACE_OUTER_BOUND ( 'NONE', #136874, .T. ) ;
#26177 = CARTESIAN_POINT ( 'NONE',  ( -21.14999999999999858, -3.187427350888460076, -228.3200064793908837 ) ) ;
#26179 = ADVANCED_FACE ( 'NONE', ( #225701 ), #171900, .F. ) ;
#26178 = FACE_OUTER_BOUND ( 'NONE', #78469, .T. ) ;
#26180 = DIRECTION ( 'NONE',  ( 0.000000000000000000, 0.000000000000000000, 1.000000000000000000 ) ) ;
#26181 = EDGE_CURVE ( 'NONE', #178795, #217944, #111906, .T. ) ;
#26182 = AXIS2_PLACEMENT_3D ( 'NONE', #72214, #34383, #214279 ) ;
#26183 = ORIENTED_EDGE ( 'NONE', *, *, #102992, .T. ) ;
#26185 = ORIENTED_EDGE ( 'NONE', *, *, #164164, .T. ) ;
#26184 = ORIENTED_EDGE ( 'NONE', *, *, #116472, .T. ) ;
#26186 = EDGE_LOOP ( 'NONE', ( #167203, #205061, #38641, #144411 ) ) ;
#26187 = CARTESIAN_POINT ( 'NONE',  ( -21.05000000000000071, 16.44800918141279311, -240.8068063186265135 ) ) ;
#26188 = AXIS2_PLACEMENT_3D ( 'NONE', #39635, #179141, #198668 ) ;
#26189 = DIRECTION ( 'NONE',  ( 0.000000000000000000, 0.9770955615653548199, 0.2128009952262535920 ) ) ;
#26190 = ADVANCED_FACE ( 'NONE', ( #77878 ), #76447, .T. ) ;
#26192 = DIRECTION ( 'NONE',  ( -1.000000000000000000, 1.207181226542539700E-16, -2.694675058168174199E-16 ) ) ;
#26191 = CARTESIAN_POINT ( 'NONE',  ( -20.54999999999999716, 63.74333919030581086, -212.9951329171253747 ) ) ;
#26193 = EDGE_CURVE ( 'NONE', #91448, #209114, #101346, .T. ) ;
#26194 = DIRECTION ( 'NONE',  ( 0.000000000000000000, -0.4088369013363494231, 0.9126074666063672680 ) ) ;
#26195 = ORIENTED_EDGE ( 'NONE', *, *, #12046, .F. ) ;
#26196 = VECTOR ( 'NONE', #230883, 1000.000000000000000 ) ;
#26197 = CARTESIAN_POINT ( 'NONE',  ( -21.45000000000000284, 68.29142135624952914, -148.8731074845244109 ) ) ;
#26198 = DIRECTION ( 'NONE',  ( 0.000000000000000000, -6.938893903907222067E-15, 1.000000000000000000 ) ) ;
#26199 = CIRCLE ( 'NONE', #151085, 0.5000000000000004441 ) ;
#26200 = DIRECTION ( 'NONE',  ( -1.040834085586090694E-13, 0.1568667991644355497, 0.9876197685951332295 ) ) ;
#26201 = VECTOR ( 'NONE', #48231, 1000.000000000000000 ) ;
#26202 = AXIS2_PLACEMENT_3D ( 'NONE', #57220, #93796, #134201 ) ;
#26203 = CARTESIAN_POINT ( 'NONE',  ( -16.94275863006528482, 9.989496048678669027, -87.89169738207662874 ) ) ;
#26204 = ORIENTED_EDGE ( 'NONE', *, *, #104628, .F. ) ;
#26205 = CARTESIAN_POINT ( 'NONE',  ( -21.45000000000000284, 7.708578643773852157, -146.3500000000000227 ) ) ;
#26206 = AXIS2_PLACEMENT_3D ( 'NONE', #111671, #12599, #152110 ) ;
#26207 = CARTESIAN_POINT ( 'NONE',  ( 20.94999999999999574, 1.115600667400684642E-11, -67.00000000000004263 ) ) ;
#26208 = ORIENTED_EDGE ( 'NONE', *, *, #117136, .T. ) ;
#26209 = VERTEX_POINT ( 'NONE', #57014 ) ;
#26210 = CARTESIAN_POINT ( 'NONE',  ( -16.88593481969334320, 9.950560090095464716, -54.35187225694449609 ) ) ;
#26211 = DIRECTION ( 'NONE',  ( 0.000000000000000000, 0.000000000000000000, 1.000000000000000000 ) ) ;
#26212 = CARTESIAN_POINT ( 'NONE',  ( -23.25000000000000000, -1.249999999999999334, -41.30048075441507649 ) ) ;
#26213 = CARTESIAN_POINT ( 'NONE',  ( -18.59999999999999787, 77.83534155023646406, -124.8679561919613121 ) ) ;
#26214 = DIRECTION ( 'NONE',  ( 1.000000000000000000, 0.000000000000000000, 0.000000000000000000 ) ) ;
#26215 = B_SPLINE_CURVE_WITH_KNOTS ( 'NONE', 3,
 ( #185126, #245100, #225505, #46879 ),
 .UNSPECIFIED., .F., .F.,
 ( 4, 4 ),
 ( 0.000000000000000000, 0.0002118541922231706302 ),
 .UNSPECIFIED. ) ;
#26217 = VECTOR ( 'NONE', #74979, 1000.000000000000000 ) ;
#26216 = DIRECTION ( 'NONE',  ( 0.000000000000000000, -1.000000000000000000, 0.000000000000000000 ) ) ;
#26218 = VERTEX_POINT ( 'NONE', #236972 ) ;
#26219 = DIRECTION ( 'NONE',  ( 0.000000000000000000, 0.000000000000000000, 1.000000000000000000 ) ) ;
#26220 = CARTESIAN_POINT ( 'NONE',  ( 21.05000000000000071, 6.650000000011155876, -77.01702717044007329 ) ) ;
#26221 = CARTESIAN_POINT ( 'NONE',  ( 21.04999999999999716, 12.01637667977029267, -206.2275507673361403 ) ) ;
#26222 = VECTOR ( 'NONE', #53503, 1000.000000000000000 ) ;
#26224 = CARTESIAN_POINT ( 'NONE',  ( -21.00250684356849362, 11.75000000001115197, -174.5148057687579808 ) ) ;
#26223 = CARTESIAN_POINT ( 'NONE',  ( 23.14999999999999503, 8.980461154494404852, -187.0187154576991304 ) ) ;
#26225 = CARTESIAN_POINT ( 'NONE',  ( 20.12500000000000355, 65.75804927292995217, -195.6629037574383290 ) ) ;
#26226 = VECTOR ( 'NONE', #87955, 1000.000000000000000 ) ;
#26227 = DIRECTION ( 'NONE',  ( 0.000000000000000000, -0.9274965247785555977, 0.3738317757009190223 ) ) ;
#26228 = FACE_OUTER_BOUND ( 'NONE', #209504, .T. ) ;
#26230 = VERTEX_POINT ( 'NONE', #239541 ) ;
#26229 = LINE ( 'NONE', #30096, #144556 ) ;
#26231 = EDGE_CURVE ( 'NONE', #43859, #19722, #158633, .T. ) ;
#26232 = VECTOR ( 'NONE', #221698, 1000.000000000000000 ) ;
#26233 = VECTOR ( 'NONE', #109966, 1000.000000000000227 ) ;
#26234 = AXIS2_PLACEMENT_3D ( 'NONE', #215274, #92743, #114891 ) ;
#26235 = VECTOR ( 'NONE', #78504, 1000.000000000000114 ) ;
#26236 = DIRECTION ( 'NONE',  ( -1.000000000000000000, 2.952720810173289112E-16, 2.061873921506763405E-30 ) ) ;
#26237 = DIRECTION ( 'NONE',  ( -1.000000000000000000, 0.000000000000000000, 0.000000000000000000 ) ) ;
#26238 = ADVANCED_FACE ( 'NONE', ( #20508 ), #36225, .T. ) ;
#26239 = CARTESIAN_POINT ( 'NONE',  ( -20.54999999999999716, 85.00000000001251976, -179.9170766071767389 ) ) ;
#26240 = AXIS2_PLACEMENT_3D ( 'NONE', #129020, #88577, #188986 ) ;
#26241 = ORIENTED_EDGE ( 'NONE', *, *, #142104, .T. ) ;
#26242 = AXIS2_PLACEMENT_3D ( 'NONE', #85617, #244714, #66092 ) ;
#26244 = DIRECTION ( 'NONE',  ( -1.000000000000000000, -0.000000000000000000, -0.000000000000000000 ) ) ;
#26243 = AXIS2_PLACEMENT_3D ( 'NONE', #11681, #129053, #54631 ) ;
#26245 = CARTESIAN_POINT ( 'NONE',  ( -18.40000000000000213, 55.18266668263805030, -231.5853321237989633 ) ) ;
#26246 = CYLINDRICAL_SURFACE ( 'NONE', #148675, 0.09999999999998898659 ) ;
#26247 = VERTEX_POINT ( 'NONE', #199126 ) ;
#26248 = DIRECTION ( 'NONE',  ( -0.000000000000000000, 1.000000000000000000, 2.891205793294679805E-16 ) ) ;
#26250 = ORIENTED_EDGE ( 'NONE', *, *, #143541, .F. ) ;
#26249 = CARTESIAN_POINT ( 'NONE',  ( -16.77180007708461318, 9.950000000011137047, -188.3643858810451377 ) ) ;
#26252 = CARTESIAN_POINT ( 'NONE',  ( 23.24999999999999645, 5.600000000011153389, -146.4052660189131245 ) ) ;
#26251 = CARTESIAN_POINT ( 'NONE',  ( 18.54999999999999716, 8.750000000011182166, -143.2500000000000284 ) ) ;
#26253 = DIRECTION ( 'NONE',  ( 0.000000000000000000, 0.1332476588733589318, -0.9910827722268049644 ) ) ;
#26254 = VERTEX_POINT ( 'NONE', #197831 ) ;
#26255 = CARTESIAN_POINT ( 'NONE',  ( -18.59999999999999787, 64.35000000001230092, -157.7731074845244450 ) ) ;
#26256 = DIRECTION ( 'NONE',  ( 0.000000000000000000, 0.000000000000000000, 1.000000000000000000 ) ) ;
#26257 = CARTESIAN_POINT ( 'NONE',  ( -23.25000000000000000, 74.00000000001223555, -149.7477294072864709 ) ) ;
#26258 = CARTESIAN_POINT ( 'NONE',  ( 21.05000000000000071, 67.12338541492499644, -128.1380270056797031 ) ) ;
#26259 = CARTESIAN_POINT ( 'NONE',  ( -18.79999999999999716, 8.000000000000000000, -1.212568896937008089 ) ) ;
#26260 = ORIENTED_EDGE ( 'NONE', *, *, #29561, .T. ) ;
#26261 = DIRECTION ( 'NONE',  ( 0.000000000000000000, 0.000000000000000000, -1.000000000000000000 ) ) ;
#26262 = PLANE ( 'NONE',  #92353 ) ;
#26263 = AXIS2_PLACEMENT_3D ( 'NONE', #206115, #27520, #106995 ) ;
#26264 = CARTESIAN_POINT ( 'NONE',  ( -22.50000000000000000, 0.09263750062063520752, -122.3503027929592690 ) ) ;
#26265 = VERTEX_POINT ( 'NONE', #80417 ) ;
#26266 = ORIENTED_EDGE ( 'NONE', *, *, #202074, .F. ) ;
#26267 = SPHERICAL_SURFACE ( 'NONE', #250655, 0.1000000000000000056 ) ;
#26268 = FACE_OUTER_BOUND ( 'NONE', #233151, .T. ) ;
#26269 = CARTESIAN_POINT ( 'NONE',  ( -21.05000000000000071, 87.41227409416205774, -167.0231074845242745 ) ) ;
#26270 = DIRECTION ( 'NONE',  ( 0.7070776581709139474, 0.7071359030027652981, 2.946958787807621248E-14 ) ) ;
#26271 = CARTESIAN_POINT ( 'NONE',  ( 21.05000000000000071, 5.400000000011154988, -124.1060308773475924 ) ) ;
#26272 = EDGE_CURVE ( 'NONE', #58764, #76100, #118154, .T. ) ;
#26274 = CARTESIAN_POINT ( 'NONE',  ( -20.54999999999999716, 76.00000000001215028, -138.4231074845243654 ) ) ;
#26273 = CARTESIAN_POINT ( 'NONE',  ( 20.94999999999999929, -9.499999999988844479, -90.60603087734760663 ) ) ;
#26275 = CARTESIAN_POINT ( 'NONE',  ( -20.64999999999999858, 68.56901367119438362, -214.3038979092079046 ) ) ;
#26276 = CARTESIAN_POINT ( 'NONE',  ( -16.89268316805466341, 9.951721813253341153, -113.1442475214544885 ) ) ;
#26277 = DIRECTION ( 'NONE',  ( -0.000000000000000000, 1.000000000000000000, -0.000000000000000000 ) ) ;
#26278 = CARTESIAN_POINT ( 'NONE',  ( 18.59999999999999076, 6.550000000011156231, -43.51702717044002355 ) ) ;
#26279 = AXIS2_PLACEMENT_3D ( 'NONE', #130830, #168726, #129558 ) ;
#26281 = ORIENTED_EDGE ( 'NONE', *, *, #194516, .F. ) ;
#26280 = CYLINDRICAL_SURFACE ( 'NONE', #228068, 0.09999999999999939493 ) ;
#26282 = CARTESIAN_POINT ( 'NONE',  ( -22.57320508075687115, 11.75000000001115552, -67.00000000000004263 ) ) ;
#26283 = CARTESIAN_POINT ( 'NONE',  ( -20.85000000000000142, 87.65000000001143121, -36.02310748452423894 ) ) ;
#26285 = CARTESIAN_POINT ( 'NONE',  ( 21.15000000000005187, 77.83551161375991967, -47.52760213295649550 ) ) ;
#26284 = DIRECTION ( 'NONE',  ( 1.000000000000000000, 3.265361837132813093E-16, -0.000000000000000000 ) ) ;
#26286 = EDGE_CURVE ( 'NONE', #139066, #56206, #243046, .T. ) ;
#26287 = VERTEX_POINT ( 'NONE', #137846 ) ;
#26288 = CARTESIAN_POINT ( 'NONE',  ( -21.05000000000000071, 1.835341550235567887, -112.0551512925630249 ) ) ;
#26289 = DIRECTION ( 'NONE',  ( -4.408576920032448588E-17, 0.1350103645451876944, -0.9908441862701601321 ) ) ;
#26290 = DIRECTION ( 'NONE',  ( 1.000000000000000000, 0.000000000000000000, 0.000000000000000000 ) ) ;
#26291 = CARTESIAN_POINT ( 'NONE',  ( -23.15000000000000213, 1.115600667400684642E-11, -113.2750000000000341 ) ) ;
#26292 = FACE_OUTER_BOUND ( 'NONE', #13297, .T. ) ;
#26293 = EDGE_CURVE ( 'NONE', #95570, #99741, #255186, .T. ) ;
#26294 = VERTEX_POINT ( 'NONE', #60884 ) ;
#26295 = EDGE_LOOP ( 'NONE', ( #26562, #124446, #207243, #9178 ) ) ;
#26297 = AXIS2_PLACEMENT_3D ( 'NONE', #240499, #200094, #117983 ) ;
#26296 = CARTESIAN_POINT ( 'NONE',  ( 21.05000000000000071, 61.94127660284455317, -221.8315191551248517 ) ) ;
#26298 = ADVANCED_FACE ( 'NONE', ( #115739 ), #2186, .T. ) ;
#26299 = ORIENTED_EDGE ( 'NONE', *, *, #17279, .F. ) ;
#26300 = LINE ( 'NONE', #66706, #30567 ) ;
#26301 = EDGE_LOOP ( 'NONE', ( #144035, #17981, #81912, #245528 ) ) ;
#26302 = AXIS2_PLACEMENT_3D ( 'NONE', #180926, #63526, #179655 ) ;
#26303 = DIRECTION ( 'NONE',  ( -1.836970198721029934E-16, -1.000000000000000000, -6.982962677686266711E-15 ) ) ;
#26304 = DIRECTION ( 'NONE',  ( 0.000000000000000000, 1.000000000000000000, 6.982962677686266711E-15 ) ) ;
#26305 = VECTOR ( 'NONE', #85488, 1000.000000000000000 ) ;
#26306 = DIRECTION ( 'NONE',  ( 0.000000000000000000, 0.000000000000000000, -1.000000000000000000 ) ) ;
#26307 = ORIENTED_EDGE ( 'NONE', *, *, #130286, .F. ) ;
#26308 = EDGE_CURVE ( 'NONE', #232039, #142689, #220954, .T. ) ;
#26309 = DIRECTION ( 'NONE',  ( -1.000000000000000000, 0.000000000000000000, 0.000000000000000000 ) ) ;
#26310 = CARTESIAN_POINT ( 'NONE',  ( -23.25000000000000000, 87.65000000001246860, -173.0231074845243029 ) ) ;
#26311 = CARTESIAN_POINT ( 'NONE',  ( 23.14999999999999503, 69.35000000001186038, -90.87310748452435405 ) ) ;
#26312 = VECTOR ( 'NONE', #212509, 1000.000000000000000 ) ;
#26314 = DIRECTION ( 'NONE',  ( 1.000000000000000000, 0.000000000000000000, 0.000000000000000000 ) ) ;
#26313 = CIRCLE ( 'NONE', #59583, 3.899999999999999467 ) ;
#26315 = CARTESIAN_POINT ( 'NONE',  ( 23.14999999999999858, 63.58084468663284383, -237.4904741118237723 ) ) ;
#26317 = AXIS2_PLACEMENT_3D ( 'NONE', #104831, #22798, #102264 ) ;
#26316 = DIRECTION ( 'NONE',  ( 0.000000000000000000, -1.000000000000000000, 0.000000000000000000 ) ) ;
#26319 = CARTESIAN_POINT ( 'NONE',  ( 21.05281448260627641, 11.16554581325007334, -211.0271857082375391 ) ) ;
#26318 = ADVANCED_BREP_SHAPE_REPRESENTATION ( '', ( #194237, #2425 ), #127326 ) ;
#26320 = EDGE_LOOP ( 'NONE', ( #228500, #22449, #203016, #229326 ) ) ;
#26322 = CARTESIAN_POINT ( 'NONE',  ( -21.65000000000000213, 68.29142135624984178, -182.2731074845244166 ) ) ;
#26321 = CARTESIAN_POINT ( 'NONE',  ( -21.55000000000000426, 7.750000000011155521, -45.85000000000000142 ) ) ;
#26323 = ORIENTED_EDGE ( 'NONE', *, *, #7762, .T. ) ;
#26325 = EDGE_LOOP ( 'NONE', ( #54399, #161812, #175639, #56904 ) ) ;
#26324 = CARTESIAN_POINT ( 'NONE',  ( -20.64999999999999858, -3.770473190032741062, -225.9805569534692324 ) ) ;
#26326 = EDGE_LOOP ( 'NONE', ( #126224, #101712, #31268, #245920 ) ) ;
#26327 = PLANE ( 'NONE',  #19849 ) ;
#26328 = CARTESIAN_POINT ( 'NONE',  ( -20.85000000000000142, 11.75000000001115552, -100.5000000000000426 ) ) ;
#26329 = CARTESIAN_POINT ( 'NONE',  ( 21.05000012384897801, 60.16074777168594068, -221.3196362128388159 ) ) ;
#26330 = VECTOR ( 'NONE', #210901, 1000.000000000000000 ) ;
#26331 = CARTESIAN_POINT ( 'NONE',  ( -18.39999999999999858, 85.60000000001210196, -129.8229180933022633 ) ) ;
#26332 = ORIENTED_EDGE ( 'NONE', *, *, #3743, .T. ) ;
#26333 = CARTESIAN_POINT ( 'NONE',  ( 23.14999999999998437, 76.00000000001264766, -199.4731074845243484 ) ) ;
#26334 = CARTESIAN_POINT ( 'NONE',  ( -16.80468759584937644, 66.05784632487818442, -157.3330886183227904 ) ) ;
#26335 = TOROIDAL_SURFACE ( 'NONE', #42900, 0.2000000000000000111, 0.1000000000000000056 ) ;
#26336 = ORIENTED_EDGE ( 'NONE', *, *, #237175, .F. ) ;
#26337 = VECTOR ( 'NONE', #87608, 1000.000000000000000 ) ;
#26338 = CIRCLE ( 'NONE', #255214, 4.000000000000003553 ) ;
#26339 = AXIS2_PLACEMENT_3D ( 'NONE', #18865, #235339, #56677 ) ;
#26340 = DIRECTION ( 'NONE',  ( -0.7071067811865475727, -0.7071067811865475727, 0.000000000000000000 ) ) ;
#26341 = ORIENTED_EDGE ( 'NONE', *, *, #240170, .T. ) ;
#26342 = DIRECTION ( 'NONE',  ( 0.000000000000000000, 1.000000000000000000, -0.000000000000000000 ) ) ;
#26343 = ADVANCED_FACE ( 'NONE', ( #235670 ), #234388, .F. ) ;
#26344 = ORIENTED_EDGE ( 'NONE', *, *, #224199, .F. ) ;
#26345 = DIRECTION ( 'NONE',  ( 1.000000000000000000, 0.000000000000000000, 0.000000000000000000 ) ) ;
#26346 = ORIENTED_EDGE ( 'NONE', *, *, #141038, .F. ) ;
#26347 = CARTESIAN_POINT ( 'NONE',  ( 21.05000000000000071, 1.360870587203197646, -41.57299792709095954 ) ) ;
#26348 = CARTESIAN_POINT ( 'NONE',  ( -20.94999999999999929, 5.850000000000004086, -23.36750277572207324 ) ) ;
#26349 = CYLINDRICAL_SURFACE ( 'NONE', #247389, 0.1000000000000054040 ) ;
#26350 = EDGE_CURVE ( 'NONE', #156593, #234500, #51485, .T. ) ;
#26351 = CARTESIAN_POINT ( 'NONE',  ( 23.14999999999999858, 4.775700934590584090, -45.34876810404598046 ) ) ;
#26352 = AXIS2_PLACEMENT_3D ( 'NONE', #136608, #91413, #216149 ) ;
#26353 = EDGE_CURVE ( 'NONE', #6520, #236406, #196549, .T. ) ;
#26354 = EDGE_CURVE ( 'NONE', #108079, #57171, #59574, .T. ) ;
#26355 = CIRCLE ( 'NONE', #122020, 0.1000000000000106498 ) ;
#26356 = DIRECTION ( 'NONE',  ( 0.000000000000000000, -7.056502275159890043E-15, 1.000000000000000000 ) ) ;
#26357 = CARTESIAN_POINT ( 'NONE',  ( -19.95447128016622429, 4.513204987603615770, 22.00000000000000355 ) ) ;
#26358 = CARTESIAN_POINT ( 'NONE',  ( -21.14999999999999858, 1.115600667400684642E-11, -26.95934304829875927 ) ) ;
#26359 = ORIENTED_EDGE ( 'NONE', *, *, #49713, .T. ) ;
#26361 = DIRECTION ( 'NONE',  ( -1.000000000000000000, 0.000000000000000000, 0.000000000000000000 ) ) ;
#26360 = CARTESIAN_POINT ( 'NONE',  ( 18.59999999999999076, 64.35000000001147669, -44.67310748452440095 ) ) ;
#26362 = DIRECTION ( 'NONE',  ( 0.000000000000000000, -0.2128009952263604232, 0.9770955615653316162 ) ) ;
#26363 = AXIS2_PLACEMENT_3D ( 'NONE', #94406, #35753, #90549 ) ;
#26364 = CARTESIAN_POINT ( 'NONE',  ( -20.85000000000000142, 7.576017155224048061, -241.7224044826512284 ) ) ;
#26365 = AXIS2_PLACEMENT_3D ( 'NONE', #244199, #107270, #10752 ) ;
#26368 = ADVANCED_FACE ( 'NONE', ( #123441 ), #205527, .T. ) ;
#26367 = EDGE_LOOP ( 'NONE', ( #127040, #160237, #174950, #99860 ) ) ;
#26366 = DIRECTION ( 'NONE',  ( 0.000000000000000000, 0.000000000000000000, -1.000000000000000000 ) ) ;
#26370 = ORIENTED_EDGE ( 'NONE', *, *, #61506, .F. ) ;
#26369 = CARTESIAN_POINT ( 'NONE',  ( -21.05000000000000071, 6.540656951712397138, -167.5999999999999659 ) ) ;
#26371 = ADVANCED_FACE ( 'NONE', ( #63452 ), #20545, .F. ) ;
#26372 = DIRECTION ( 'NONE',  ( 0.000000000000000000, -0.9126074666063660468, -0.4088369013363524762 ) ) ;
#26373 = CARTESIAN_POINT ( 'NONE',  ( 20.94999999999999929, 70.22659352830977753, -197.9852579278363578 ) ) ;
#26374 = VECTOR ( 'NONE', #147160, 1000.000000000000000 ) ;
#26375 = ADVANCED_FACE ( 'NONE', ( #223807 ), #85551, .T. ) ;
#26376 = DIRECTION ( 'NONE',  ( 0.000000000000000000, 0.2868887416115947775, -0.9579639084728169829 ) ) ;
#26378 = VERTEX_POINT ( 'NONE', #225078 ) ;
#26377 = CARTESIAN_POINT ( 'NONE',  ( 20.95512820512820440, 67.12384868372417657, -157.8731074845244109 ) ) ;
#26379 = AXIS2_PLACEMENT_3D ( 'NONE', #90528, #249631, #170128 ) ;
#26380 = AXIS2_PLACEMENT_3D ( 'NONE', #221401, #187139, #147993 ) ;
#26381 = AXIS2_PLACEMENT_3D ( 'NONE', #64936, #6239, #25827 ) ;
#26382 = PRODUCT ( 'Injection Molded Chain Links 15', 'Injection Molded Chain Links 15', '', ( #235988 ) ) ;
#26383 = VECTOR ( 'NONE', #203743, 1000.000000000000000 ) ;
#26385 = EDGE_CURVE ( 'NONE', #124376, #97342, #251227, .T. ) ;
#26384 = FACE_OUTER_BOUND ( 'NONE', #139021, .T. ) ;
#26386 = CARTESIAN_POINT ( 'NONE',  ( 21.05000000000000071, 4.813084112149527805, -21.55848224347618114 ) ) ;
#26387 = ORIENTED_EDGE ( 'NONE', *, *, #109691, .T. ) ;
#26388 = FACE_OUTER_BOUND ( 'NONE', #32493, .T. ) ;
#26389 = VERTEX_POINT ( 'NONE', #64743 ) ;
#26390 = ADVANCED_FACE ( 'NONE', ( #125996 ), #162585, .T. ) ;
#26392 = EDGE_CURVE ( 'NONE', #185736, #191967, #26407, .T. ) ;
#26391 = CYLINDRICAL_SURFACE ( 'NONE', #24203, 12.87499999999999822 ) ;
#26393 = DIRECTION ( 'NONE',  ( -1.000000000000000000, 0.000000000000000000, 0.000000000000000000 ) ) ;
#26394 = EDGE_CURVE ( 'NONE', #52759, #218080, #13929, .T. ) ;
#26395 = AXIS2_PLACEMENT_3D ( 'NONE', #169945, #49938, #27853 ) ;
#26396 = ORIENTED_EDGE ( 'NONE', *, *, #101500, .T. ) ;
#26397 = FACE_OUTER_BOUND ( 'NONE', #131974, .T. ) ;
#26398 = AXIS2_PLACEMENT_3D ( 'NONE', #133782, #34713, #195073 ) ;
#26399 = CARTESIAN_POINT ( 'NONE',  ( -21.05000000000000071, 74.73821383144705521, -128.4366085209788366 ) ) ;
#26400 = CIRCLE ( 'NONE', #88906, 0.1000000000000002554 ) ;
#26401 = ORIENTED_EDGE ( 'NONE', *, *, #157424, .F. ) ;
#26402 = CARTESIAN_POINT ( 'NONE',  ( -16.89081410710458542, 66.04868147016441071, -48.66870156468802833 ) ) ;
#26403 = AXIS2_PLACEMENT_3D ( 'NONE', #58459, #78039, #63619 ) ;
#26404 = AXIS2_PLACEMENT_3D ( 'NONE', #167111, #129238, #33705 ) ;
#26405 = VECTOR ( 'NONE', #59370, 1000.000000000000000 ) ;
#26406 = EDGE_LOOP ( 'NONE', ( #239318, #526, #68548, #50027, #44718, #196489, #115273, #79757, #215176 ) ) ;
#26407 = CIRCLE ( 'NONE', #172202, 12.97499999999999609 ) ;
#26408 = ORIENTED_EDGE ( 'NONE', *, *, #29729, .F. ) ;
#26409 = CYLINDRICAL_SURFACE ( 'NONE', #256829, 0.1000000000000054040 ) ;
#26410 = ADVANCED_FACE ( 'NONE', ( #122163 ), #8633, .T. ) ;
#26411 = VERTEX_POINT ( 'NONE', #142972 ) ;
#26412 = EDGE_CURVE ( 'NONE', #1074, #243492, #82989, .T. ) ;
#26413 = DIRECTION ( 'NONE',  ( -0.000000000000000000, 0.1298341882519953583, 0.9915357197604862671 ) ) ;
#26414 = ORIENTED_EDGE ( 'NONE', *, *, #219105, .T. ) ;
#26416 = VERTEX_POINT ( 'NONE', #201686 ) ;
#26415 = DIRECTION ( 'NONE',  ( 1.000000000000000000, 0.000000000000000000, 0.000000000000000000 ) ) ;
#26417 = CARTESIAN_POINT ( 'NONE',  ( -21.00448002041592943, 11.75000000001115552, -73.84834086231086303 ) ) ;
#26418 = ORIENTED_EDGE ( 'NONE', *, *, #142171, .T. ) ;
#26419 = DIRECTION ( 'NONE',  ( -1.000000000000000000, 3.265361837132813093E-16, 2.280189983783949500E-30 ) ) ;
#26420 = ORIENTED_EDGE ( 'NONE', *, *, #114369, .T. ) ;
#26423 = EDGE_CURVE ( 'NONE', #102134, #88943, #255077, .T. ) ;
#26422 = VERTEX_POINT ( 'NONE', #102550 ) ;
#26421 = VERTEX_POINT ( 'NONE', #182137 ) ;
#26424 = DIRECTION ( 'NONE',  ( 0.000000000000000000, 0.000000000000000000, -1.000000000000000000 ) ) ;
#26425 = CARTESIAN_POINT ( 'NONE',  ( -16.93935632781549572, 14.20137645198545862, -219.2864342127633961 ) ) ;
#26426 = ORIENTED_EDGE ( 'NONE', *, *, #160132, .F. ) ;
#26427 = VECTOR ( 'NONE', #217497, 999.9999999999998863 ) ;
#26428 = AXIS2_PLACEMENT_3D ( 'NONE', #178156, #234239, #198974 ) ;
#26429 = ORIENTED_EDGE ( 'NONE', *, *, #96420, .T. ) ;
#26430 = CARTESIAN_POINT ( 'NONE',  ( 18.79999999999999716, -11.65000000000000036, 33.00000000000000000 ) ) ;
#26431 = DIRECTION ( 'NONE',  ( 1.000000000000000000, 0.000000000000000000, 0.000000000000000000 ) ) ;
#26433 = ORIENTED_EDGE ( 'NONE', *, *, #36139, .T. ) ;
#26432 = LINE ( 'NONE', #48542, #207344 ) ;
#26434 = ORIENTED_EDGE ( 'NONE', *, *, #253302, .F. ) ;
#26435 = DIRECTION ( 'NONE',  ( 0.000000000000000000, 0.8814952561688438326, -0.4721928772777331806 ) ) ;
#26436 = CARTESIAN_POINT ( 'NONE',  ( 18.39999999999997371, 58.31215475832291162, -223.8520309854405923 ) ) ;
#26438 = ORIENTED_EDGE ( 'NONE', *, *, #230616, .T. ) ;
#26437 = EDGE_CURVE ( 'NONE', #158699, #44711, #204247, .T. ) ;
#26439 = CYLINDRICAL_SURFACE ( 'NONE', #40505, 0.1000000000000001443 ) ;
#26440 = EDGE_CURVE ( 'NONE', #221298, #241136, #3779, .T. ) ;
#26441 = ORIENTED_EDGE ( 'NONE', *, *, #81482, .F. ) ;
#26442 = CARTESIAN_POINT ( 'NONE',  ( 18.49999999999999645, 77.86671491006960366, -158.2704322382423356 ) ) ;
#26443 = ORIENTED_EDGE ( 'NONE', *, *, #221047, .F. ) ;
#26444 = EDGE_CURVE ( 'NONE', #258034, #241107, #114045, .T. ) ;
#26446 = ORIENTED_EDGE ( 'NONE', *, *, #163341, .F. ) ;
#26445 = ORIENTED_EDGE ( 'NONE', *, *, #64176, .T. ) ;
#26447 = TOROIDAL_SURFACE ( 'NONE', #168137, 2.100000000000002309, 0.1000000000000000056 ) ;
#26448 = ORIENTED_EDGE ( 'NONE', *, *, #40824, .F. ) ;
#26450 = ADVANCED_FACE ( 'NONE', ( #34632 ), #152017, .F. ) ;
#26449 = CARTESIAN_POINT ( 'NONE',  ( -16.94445028196807002, 66.00793639031481064, -182.6304376629428816 ) ) ;
#26451 = ORIENTED_EDGE ( 'NONE', *, *, #209548, .T. ) ;
#26452 = DIRECTION ( 'NONE',  ( 0.000000000000000000, 0.9889818879709272315, 0.1480365673253073999 ) ) ;
#26453 = ORIENTED_EDGE ( 'NONE', *, *, #98787, .F. ) ;
#26454 = LINE ( 'NONE', #27759, #160714 ) ;
#26455 = EDGE_CURVE ( 'NONE', #130308, #251611, #134874, .T. ) ;
#26456 = CARTESIAN_POINT ( 'NONE',  ( 21.13461538461538325, 43.58999342716158765, -234.8150793036844846 ) ) ;
#26457 = ORIENTED_EDGE ( 'NONE', *, *, #71435, .T. ) ;
#26458 = VERTEX_POINT ( 'NONE', #112863 ) ;
#26459 = VECTOR ( 'NONE', #93063, 1000.000000000000227 ) ;
#26460 = ORIENTED_EDGE ( 'NONE', *, *, #148111, .F. ) ;
#26461 = EDGE_CURVE ( 'NONE', #178866, #250208, #226456, .T. ) ;
#26462 = AXIS2_PLACEMENT_3D ( 'NONE', #108402, #10588, #148821 ) ;
#26463 = ADVANCED_FACE ( 'NONE', ( #189835 ), #243221, .T. ) ;
#26464 = AXIS2_PLACEMENT_3D ( 'NONE', #75885, #38068, #215390 ) ;
#26465 = CARTESIAN_POINT ( 'NONE',  ( 18.79999999999999716, 1.311673547813416718, -7.986648289447971116 ) ) ;
#26466 = ORIENTED_EDGE ( 'NONE', *, *, #130824, .F. ) ;
#26467 = EDGE_CURVE ( 'NONE', #189027, #113973, #52831, .T. ) ;
#26468 = FACE_OUTER_BOUND ( 'NONE', #172690, .T. ) ;
#26470 = ORIENTED_EDGE ( 'NONE', *, *, #98361, .F. ) ;
#26469 = CYLINDRICAL_SURFACE ( 'NONE', #41963, 0.09999999999999684142 ) ;
#26471 = CARTESIAN_POINT ( 'NONE',  ( 19.75857864376268935, 64.35000000001251408, -178.7731074845244450 ) ) ;
#26472 = CYLINDRICAL_SURFACE ( 'NONE', #118368, 0.09999999999999939493 ) ;
#26473 = DIRECTION ( 'NONE',  ( 1.000000000000000000, -0.000000000000000000, 0.000000000000000000 ) ) ;
#26474 = DIRECTION ( 'NONE',  ( -0.7071067811865463515, -0.7071067811865487940, 7.587431340288849180E-16 ) ) ;
#26475 = FACE_OUTER_BOUND ( 'NONE', #227144, .T. ) ;
#26477 = DIRECTION ( 'NONE',  ( 1.000000000000000000, 0.000000000000000000, 0.000000000000000000 ) ) ;
#26476 = CARTESIAN_POINT ( 'NONE',  ( -21.05000000000000426, -0.09999999998884340213, -60.52293297887530343 ) ) ;
#26478 = DIRECTION ( 'NONE',  ( -0.000000000000000000, 0.9594490217226113726, 0.2818822000686178608 ) ) ;
#26479 = CARTESIAN_POINT ( 'NONE',  ( 19.90000000000000924, 4.611773100472912112, 22.11686199900910665 ) ) ;
#26480 = VECTOR ( 'NONE', #248211, 1000.000000000000000 ) ;
#26481 = CARTESIAN_POINT ( 'NONE',  ( -20.64999999999999858, 54.34471204062663219, -239.4366250215122420 ) ) ;
#26482 = DIRECTION ( 'NONE',  ( 0.000000000000000000, -0.09425075112713271475, -0.9955484899852801162 ) ) ;
#26483 = EDGE_CURVE ( 'NONE', #3677, #97821, #49031, .T. ) ;
#26484 = AXIS2_PLACEMENT_3D ( 'NONE', #249881, #126062, #106485 ) ;
#26485 = ORIENTED_EDGE ( 'NONE', *, *, #144457, .F. ) ;
#26486 = AXIS2_PLACEMENT_3D ( 'NONE', #232443, #151627, #113744 ) ;
#26487 = AXIS2_PLACEMENT_3D ( 'NONE', #42762, #141851, #102704 ) ;
#26488 = EDGE_CURVE ( 'NONE', #142241, #52160, #14132, .T. ) ;
#26490 = ORIENTED_EDGE ( 'NONE', *, *, #161803, .F. ) ;
#26489 = DIRECTION ( 'NONE',  ( 1.000000000000000000, 5.603460673774840016E-17, 1.046060675573451769E-16 ) ) ;
#26491 = ORIENTED_EDGE ( 'NONE', *, *, #75077, .T. ) ;
#26492 = CARTESIAN_POINT ( 'NONE',  ( -20.94999999999999929, 87.39257802171813694, -173.0970570643562212 ) ) ;
#26493 = EDGE_CURVE ( 'NONE', #49226, #129819, #9902, .T. ) ;
#26494 = FACE_OUTER_BOUND ( 'NONE', #182766, .T. ) ;
#26495 = CYLINDRICAL_SURFACE ( 'NONE', #73899, 4.000000000000002665 ) ;
#26496 = EDGE_CURVE ( 'NONE', #189309, #64533, #122453, .T. ) ;
#26497 = VERTEX_POINT ( 'NONE', #11199 ) ;
#26498 = AXIS2_PLACEMENT_3D ( 'NONE', #25853, #127512, #145770 ) ;
#26499 = TOROIDAL_SURFACE ( 'NONE', #101257, 0.2000000000000000111, 0.1000000000000000056 ) ;
#26501 = AXIS2_PLACEMENT_3D ( 'NONE', #135975, #233821, #133431 ) ;
#26500 = FACE_OUTER_BOUND ( 'NONE', #243447, .T. ) ;
#26502 = CARTESIAN_POINT ( 'NONE',  ( 23.24999999999999645, 76.00000000001142553, -36.02310748452432421 ) ) ;
#26503 = EDGE_LOOP ( 'NONE', ( #117513, #185381, #61329, #222043 ) ) ;
#26504 = DIRECTION ( 'NONE',  ( 0.000000000000000000, 0.000000000000000000, -1.000000000000000000 ) ) ;
#26505 = CARTESIAN_POINT ( 'NONE',  ( -16.80100426158789872, 9.943150520407291637, -180.1829457528340015 ) ) ;
#26506 = DIRECTION ( 'NONE',  ( 0.000000000000000000, -0.9126074666063770380, -0.4088369013363281068 ) ) ;
#26507 = AXIS2_PLACEMENT_3D ( 'NONE', #213152, #114044, #14975 ) ;
#26508 = EDGE_CURVE ( 'NONE', #222464, #155345, #120347, .T. ) ;
#26509 = DIRECTION ( 'NONE',  ( -1.000000000000000000, 0.000000000000000000, 0.000000000000000000 ) ) ;
#26511 = VERTEX_POINT ( 'NONE', #73760 ) ;
#26510 = CARTESIAN_POINT ( 'NONE',  ( -16.89020380669786192, 66.05000000001230376, -157.2656963364138676 ) ) ;
#26512 = CARTESIAN_POINT ( 'NONE',  ( -18.59999999999999787, 77.83534155023627932, -91.46795619196132066 ) ) ;
#26513 = DIRECTION ( 'NONE',  ( 0.000000000000000000, -1.000000000000000000, -6.982962677686266711E-15 ) ) ;
#26514 = AXIS2_PLACEMENT_3D ( 'NONE', #220326, #80775, #178654 ) ;
#26516 = DIRECTION ( 'NONE',  ( -1.000000000000000000, -0.000000000000000000, 0.000000000000000000 ) ) ;
#26515 = AXIS2_PLACEMENT_3D ( 'NONE', #63914, #243825, #205991 ) ;
#26518 = ORIENTED_EDGE ( 'NONE', *, *, #219294, .T. ) ;
#26517 = CIRCLE ( 'NONE', #209863, 12.87499999999999822 ) ;
#26519 = FACE_OUTER_BOUND ( 'NONE', #118575, .T. ) ;
#26520 = FACE_OUTER_BOUND ( 'NONE', #52391, .T. ) ;
#26521 = CIRCLE ( 'NONE', #238894, 0.09999999999999939493 ) ;
#26523 = DIRECTION ( 'NONE',  ( -1.000000000000000000, 0.000000000000000000, 0.000000000000000000 ) ) ;
#26522 = CARTESIAN_POINT ( 'NONE',  ( 18.59999999999999432, 77.16270174995010223, -128.4231074845242802 ) ) ;
#26524 = FACE_OUTER_BOUND ( 'NONE', #104992, .T. ) ;
#26525 = DIRECTION ( 'NONE',  ( -3.265361837132813093E-16, 1.000000000000000000, -0.000000000000000000 ) ) ;
#26526 = CARTESIAN_POINT ( 'NONE',  ( -21.00250684356850073, 64.25000000001233502, -163.0083017157664358 ) ) ;
#26527 = DIRECTION ( 'NONE',  ( 0.000000000000000000, 0.2617529984165027912, 0.9651348961777157509 ) ) ;
#26528 = CARTESIAN_POINT ( 'NONE',  ( 18.58685178364169843, 85.40673308381636275, -129.3986870154365363 ) ) ;
#26529 = LINE ( 'NONE', #222112, #230884 ) ;
#26530 = ORIENTED_EDGE ( 'NONE', *, *, #38779, .F. ) ;
#26531 = DIRECTION ( 'NONE',  ( 1.000000000000000000, 0.000000000000000000, 0.000000000000000000 ) ) ;
#26532 = VERTEX_POINT ( 'NONE', #153310 ) ;
#26533 = VERTEX_POINT ( 'NONE', #248517 ) ;
#26534 = ADVANCED_FACE ( 'NONE', ( #71187, #54161 ), #51564, .F. ) ;
#26535 = CARTESIAN_POINT ( 'NONE',  ( -20.99780126800938262, 11.60538868787665301, -26.58735257170532762 ) ) ;
#26536 = DIRECTION ( 'NONE',  ( 0.000000000000000000, 0.8814952561688476074, -0.4721928772777262417 ) ) ;
#26537 = VERTEX_POINT ( 'NONE', #129842 ) ;
#26538 = ORIENTED_EDGE ( 'NONE', *, *, #142306, .F. ) ;
#26539 = CIRCLE ( 'NONE', #118100, 0.1000000000000091788 ) ;
#26540 =( NAMED_UNIT ( * ) PLANE_ANGLE_UNIT ( ) SI_UNIT ( $, .RADIAN. ) );
#26541 = VECTOR ( 'NONE', #97995, 1000.000000000000000 ) ;
#26542 = ADVANCED_FACE ( 'NONE', ( #210674 ), #218354, .T. ) ;
#26543 = ORIENTED_EDGE ( 'NONE', *, *, #227215, .F. ) ;
#26544 = AXIS2_PLACEMENT_3D ( 'NONE', #114517, #136629, #37563 ) ;
#26545 = CYLINDRICAL_SURFACE ( 'NONE', #104357, 0.1000000000000118433 ) ;
#26546 = ORIENTED_EDGE ( 'NONE', *, *, #135677, .F. ) ;
#26547 = DIRECTION ( 'NONE',  ( 0.000000000000000000, 0.8879235499942239596, 0.4599910535713220838 ) ) ;
#26548 = DIRECTION ( 'NONE',  ( -1.000000000000000000, 0.000000000000000000, -0.000000000000000000 ) ) ;
#26549 = DIRECTION ( 'NONE',  ( 0.000000000000000000, 0.008583690987124697677, -0.9999631594459055250 ) ) ;
#26550 = DIRECTION ( 'NONE',  ( 0.000000000000000000, 0.3738317757009345654, 0.9274965247785492695 ) ) ;
#26551 = CARTESIAN_POINT ( 'NONE',  ( -20.54999999999999361, 11.64999999999999680, -21.35000000000000142 ) ) ;
#26552 = AXIS2_PLACEMENT_3D ( 'NONE', #241543, #126731, #104566 ) ;
#26553 = AXIS2_PLACEMENT_3D ( 'NONE', #117547, #60127, #100516 ) ;
#26554 = DIRECTION ( 'NONE',  ( 1.000000000000000000, 0.000000000000000000, 0.000000000000000000 ) ) ;
#26555 = CARTESIAN_POINT ( 'NONE',  ( 20.90000000000000213, -1.786320531569725478, -11.50977166988710820 ) ) ;
#26557 = VERTEX_POINT ( 'NONE', #157145 ) ;
#26556 = CARTESIAN_POINT ( 'NONE',  ( 20.85000000000000142, 11.65000000001115943, -200.9999999999999432 ) ) ;
#26559 = PLANE ( 'NONE',  #191858 ) ;
#26558 = FACE_OUTER_BOUND ( 'NONE', #166427, .T. ) ;
#26560 = CARTESIAN_POINT ( 'NONE',  ( -22.00356870070283577, 76.00000000002545164, -76.77734984626648895 ) ) ;
#26561 =( BOUNDED_SURFACE ( )  B_SPLINE_SURFACE ( 3, 2, ( 
 ( #162445, #103705, #222361 ),
 ( #63309, #198979, #81566 ),
 ( #21639, #20371, #161150 ),
 ( #99848, #2046, #141573 ) ),
 .UNSPECIFIED., .F., .F., .F. ) 
 B_SPLINE_SURFACE_WITH_KNOTS ( ( 4, 4 ),
 ( 3, 3 ),
 ( 5.727910411845712702, 5.983100554402349225 ),
 ( 0.000000000000000000, 1.000000000000000000 ),
 .UNSPECIFIED. ) 
 GEOMETRIC_REPRESENTATION_ITEM ( )  RATIONAL_B_SPLINE_SURFACE ( (
 ( 1.000000000000000000, 0.8946697475932141597, 1.000000000000000000),
 ( 1.000000000000000000, 0.9035312726220684487, 1.000000000000000000),
 ( 1.000000000000000000, 0.9104333467450373973, 1.000000000000000000),
 ( 1.000000000000000000, 0.9152888060719408525, 1.000000000000000000) ) ) 
 REPRESENTATION_ITEM ( '' )  SURFACE ( )  );
#26562 = ORIENTED_EDGE ( 'NONE', *, *, #103501, .F. ) ;
#26563 = DIRECTION ( 'NONE',  ( 0.7071067811865475727, 0.7071067811865475727, 0.000000000000000000 ) ) ;
#26564 = AXIS2_PLACEMENT_3D ( 'NONE', #115742, #57018, #192720 ) ;
#26565 = CARTESIAN_POINT ( 'NONE',  ( 22.50000000000000000, 0.1000000000111554016, -55.25000000000004974 ) ) ;
#26566 = CARTESIAN_POINT ( 'NONE',  ( 18.59999999999999076, 14.05000000001116689, -173.0136950707609458 ) ) ;
#26567 = ORIENTED_EDGE ( 'NONE', *, *, #205053, .F. ) ;
#26568 = CIRCLE ( 'NONE', #172351, 0.09999999999999771572 ) ;
#26569 = CARTESIAN_POINT ( 'NONE',  ( -16.93521499325732549, 66.00521388020847269, -115.6159989434308244 ) ) ;
#26570 = VECTOR ( 'NONE', #136741, 1000.000000000000114 ) ;
#26571 = AXIS2_PLACEMENT_3D ( 'NONE', #200949, #43169, #142256 ) ;
#26572 = CARTESIAN_POINT ( 'NONE',  ( -21.44999999999999929, 7.350000000011155166, -112.7500000000000284 ) ) ;
#26573 = VERTEX_POINT ( 'NONE', #39775 ) ;
#26574 = CIRCLE ( 'NONE', #101533, 0.1000000000000028644 ) ;
#26575 = SURFACE_SIDE_STYLE ('',( #239182 ) ) ;
#26576 = DIRECTION ( 'NONE',  ( 0.000000000000000000, -1.000000000000000000, -6.982962677686265922E-15 ) ) ;
#26577 =( BOUNDED_SURFACE ( )  B_SPLINE_SURFACE ( 3, 2, ( 
 ( #197242, #160719, #81126 ),
 ( #121592, #22481, #79834 ),
 ( #237658, #19905, #58982 ),
 ( #77282, #43313, #159416 ),
 ( #141131, #179005, #122854 ),
 ( #101959, #18608, #99401 ) ),
 .UNSPECIFIED., .F., .F., .F. ) 
 B_SPLINE_SURFACE_WITH_KNOTS ( ( 4, 2, 4 ),
 ( 3, 3 ),
 ( 4.712388980384689674, 5.497787143782137953, 6.283185307179586232 ),
 ( 0.000000000000000000, 1.000000000000000000 ),
 .UNSPECIFIED. ) 
 GEOMETRIC_REPRESENTATION_ITEM ( )  RATIONAL_B_SPLINE_SURFACE ( (
 ( 1.000000000000000000, 0.7071067811865819897, 1.000000000000000000),
 ( 1.000000000000000000, 0.7727932973487859902, 1.000000000000000000),
 ( 1.000000000000000000, 0.8282379607655473430, 1.000000000000000000),
 ( 1.000000000000000000, 0.9038128468033935770, 1.000000000000000000),
 ( 1.000000000000000000, 0.9240297172247979862, 1.000000000000000000),
 ( 1.000000000000000000, 0.9238795325112969525, 1.000000000000000000) ) ) 
 REPRESENTATION_ITEM ( '' )  SURFACE ( )  );
#26578 = CARTESIAN_POINT ( 'NONE',  ( -18.40904629823846506, -0.7490475871975608158, -242.2033266940802889 ) ) ;
#26579 = VERTEX_POINT ( 'NONE', #174165 ) ;
#26580 = CIRCLE ( 'NONE', #184769, 0.1000000000000028644 ) ;
#26581 = ORIENTED_EDGE ( 'NONE', *, *, #196586, .F. ) ;
#26582 = ADVANCED_FACE ( 'NONE', ( #55416 ), #119290, .T. ) ;
#26583 = CARTESIAN_POINT ( 'NONE',  ( 21.14999999999999858, 12.71802988599559470, -223.5105008658000258 ) ) ;
#26585 = VECTOR ( 'NONE', #130005, 1000.000000000000000 ) ;
#26584 = CARTESIAN_POINT ( 'NONE',  ( 20.94999999999999929, 61.88149656937974896, -248.1136133839584090 ) ) ;
#26586 = FACE_OUTER_BOUND ( 'NONE', #77724, .T. ) ;
#26587 = CARTESIAN_POINT ( 'NONE',  ( 18.59999999999999076, 64.35000000001177511, -78.17310748452437963 ) ) ;
#26588 = DIRECTION ( 'NONE',  ( 0.000000000000000000, 1.000000000000000000, 0.000000000000000000 ) ) ;
#26589 = CARTESIAN_POINT ( 'NONE',  ( -18.59999999999999787, 66.65000000001253966, -182.3731074845244393 ) ) ;
#26590 = AXIS2_PLACEMENT_3D ( 'NONE', #94421, #213090, #248372 ) ;
#26591 = ORIENTED_EDGE ( 'NONE', *, *, #151440, .T. ) ;
#26593 =( BOUNDED_SURFACE ( )  B_SPLINE_SURFACE ( 3, 2, ( 
 ( #238103, #119467, #101112 ),
 ( #21646, #217245, #102419 ),
 ( #240679, #256322, #56874 ),
 ( #37367, #62060, #201548 ) ),
 .UNSPECIFIED., .F., .F., .F. ) 
 B_SPLINE_SURFACE_WITH_KNOTS ( ( 4, 4 ),
 ( 3, 3 ),
 ( -2.087089182034596035E-18, 0.0003124336600439759455 ),
 ( 0.000000000000000000, 1.000000000000000000 ),
 .UNSPECIFIED. ) 
 GEOMETRIC_REPRESENTATION_ITEM ( )  RATIONAL_B_SPLINE_SURFACE ( (
 ( 1.000000000000000000, 0.7071067811865205943, 1.000000000000000000),
 ( 1.000000000000000000, 0.7089187706049330240, 1.000000000000000000),
 ( 1.000000000000000000, 0.7039288185051130187, 1.000000000000000000),
 ( 1.000000000000000000, 0.7040654476016154906, 1.000000000000000000) ) ) 
 REPRESENTATION_ITEM ( '' )  SURFACE ( )  );
#26592 = CARTESIAN_POINT ( 'NONE',  ( -18.40000000000000213, 5.650000000011139001, -79.65000000000004832 ) ) ;
#26594 = CIRCLE ( 'NONE', #97259, 0.2000000000000057288 ) ;
#26596 = ORIENTED_EDGE ( 'NONE', *, *, #134048, .T. ) ;
#26595 = CARTESIAN_POINT ( 'NONE',  ( -20.64999999999999858, 4.389020526555173163, -221.1525959572864792 ) ) ;
#26597 = AXIS2_PLACEMENT_3D ( 'NONE', #169026, #211978, #33367 ) ;
#26598 = CARTESIAN_POINT ( 'NONE',  ( -21.09107601085566586, 6.363877975371106999, -33.46069283528267846 ) ) ;
#26599 = CARTESIAN_POINT ( 'NONE',  ( 21.07928932188134397, 10.02993822722304351, -228.1074463178677263 ) ) ;
#26600 = CARTESIAN_POINT ( 'NONE',  ( -21.09316766718153247, 75.96073659769703568, -75.89326079699904426 ) ) ;
#26601 = DIRECTION ( 'NONE',  ( 7.589415207398576792E-15, -1.000000000000000000, -0.000000000000000000 ) ) ;
#26602 = ADVANCED_FACE ( 'NONE', ( #17592 ), #116709, .T. ) ;
#26603 = DIRECTION ( 'NONE',  ( -1.000000000000000000, 0.000000000000000000, -0.000000000000000000 ) ) ;
#26605 = ORIENTED_EDGE ( 'NONE', *, *, #257419, .F. ) ;
#26604 = PLANE ( 'NONE',  #235927 ) ;
#26606 = DIRECTION ( 'NONE',  ( 0.000000000000000000, -0.4558084472153119959, 0.8900778951570285091 ) ) ;
#26607 = CARTESIAN_POINT ( 'NONE',  ( -15.75000000000000355, 9.849999999999978328, -16.75000000000000355 ) ) ;
#26608 = CYLINDRICAL_SURFACE ( 'NONE', #13732, 0.09999999999999939493 ) ;
#26609 = CYLINDRICAL_SURFACE ( 'NONE', #98975, 0.09999999999999950595 ) ;
#26610 = EDGE_CURVE ( 'NONE', #110468, #43374, #257443, .T. ) ;
#26611 = ORIENTED_EDGE ( 'NONE', *, *, #97300, .F. ) ;
#26612 = CARTESIAN_POINT ( 'NONE',  ( 20.94999999999999929, 77.13501884592203339, -95.30613060109196510 ) ) ;
#26613 = CARTESIAN_POINT ( 'NONE',  ( -23.15000000000000213, 64.35000000001180354, -81.67310748452439384 ) ) ;
#26614 = LINE ( 'NONE', #8332, #71242 ) ;
#26615 = CARTESIAN_POINT ( 'NONE',  ( 23.25000000000000000, -3.770473190032740174, -225.9805569534692324 ) ) ;
#26617 = ADVANCED_FACE ( 'NONE', ( #97105 ), #209939, .F. ) ;
#26616 = VECTOR ( 'NONE', #176199, 1000.000000000000114 ) ;
#26619 = ORIENTED_EDGE ( 'NONE', *, *, #92914, .F. ) ;
#26618 = AXIS2_PLACEMENT_3D ( 'NONE', #127054, #206588, #106182 ) ;
#26620 = CARTESIAN_POINT ( 'NONE',  ( -16.77180007708460963, 9.950000000011137047, -87.86438588104522296 ) ) ;
#26621 = VECTOR ( 'NONE', #22881, 1000.000000000000000 ) ;
#26622 = VECTOR ( 'NONE', #26790, 1000.000000000000114 ) ;
#26623 = ORIENTED_EDGE ( 'NONE', *, *, #44908, .T. ) ;
#26624 = ADVANCED_BREP_SHAPE_REPRESENTATION ( '', ( #192084, #2425 ), #239393 ) ;
#26625 = CYLINDRICAL_SURFACE ( 'NONE', #39259, 12.87499999999999822 ) ;
#26626 = CARTESIAN_POINT ( 'NONE',  ( 20.94999999999999929, 76.00000000001227818, -157.0481074845243938 ) ) ;
#26627 = CYLINDRICAL_SURFACE ( 'NONE', #183009, 0.09999999999999939493 ) ;
#26628 = CARTESIAN_POINT ( 'NONE',  ( 18.60000000000000497, -9.364236010355609707, -174.6802544007245501 ) ) ;
#26629 = VERTEX_POINT ( 'NONE', #179283 ) ;
#26630 = EDGE_CURVE ( 'NONE', #61748, #54081, #75053, .T. ) ;
#26631 = DIRECTION ( 'NONE',  ( 0.000000000000000000, -0.008583690987162452199, -0.9999631594459053030 ) ) ;
#26632 = EDGE_CURVE ( 'NONE', #18265, #68090, #139846, .T. ) ;
#26633 = CARTESIAN_POINT ( 'NONE',  ( -21.05000000000000071, 7.872214528623318053, -209.6555322433423498 ) ) ;
#26634 = DIRECTION ( 'NONE',  ( 0.000000000000000000, -0.9770955615653316162, -0.2128009952263604232 ) ) ;
#26635 = FACE_OUTER_BOUND ( 'NONE', #176204, .T. ) ;
#26636 = DIRECTION ( 'NONE',  ( -0.000000000000000000, -0.000000000000000000, 1.000000000000000000 ) ) ;
#26637 = VERTEX_POINT ( 'NONE', #590 ) ;
#26639 = ORIENTED_EDGE ( 'NONE', *, *, #47376, .T. ) ;
#26638 = DIRECTION ( 'NONE',  ( 0.000000000000000000, 0.000000000000000000, -1.000000000000000000 ) ) ;
#26640 = VERTEX_POINT ( 'NONE', #77554 ) ;
#26641 =( GEOMETRIC_REPRESENTATION_CONTEXT ( 3 ) GLOBAL_UNCERTAINTY_ASSIGNED_CONTEXT ( ( #170380 ) ) GLOBAL_UNIT_ASSIGNED_CONTEXT ( ( #57419, #53592, #96539 ) ) REPRESENTATION_CONTEXT ( 'NONE', 'WORKASPACE' ) );
#26642 = DIRECTION ( 'NONE',  ( 1.000000000000000000, 0.000000000000000000, 0.000000000000000000 ) ) ;
#26643 = ORIENTED_EDGE ( 'NONE', *, *, #254348, .F. ) ;
#26644 = CARTESIAN_POINT ( 'NONE',  ( 21.05193202509564543, 65.27606398031487345, -124.3505728811986017 ) ) ;
#26645 = CARTESIAN_POINT ( 'NONE',  ( -23.25000000000000000, 7.128833340093095217, -233.7327013124392749 ) ) ;
#26646 = DIRECTION ( 'NONE',  ( 0.000000000000000000, -0.9654727137038715545, -0.2605042016806676242 ) ) ;
#26647 = VERTEX_POINT ( 'NONE', #80106 ) ;
#26648 = CARTESIAN_POINT ( 'NONE',  ( 23.25000000000000000, -9.000000000000000000, -23.60603087734755690 ) ) ;
#26649 = DIRECTION ( 'NONE',  ( 0.000000000000000000, 0.000000000000000000, 1.000000000000000000 ) ) ;
#26650 = CARTESIAN_POINT ( 'NONE',  ( 20.13684514580102913, 9.495855392761558988, -41.64303168568470426 ) ) ;
#26651 = EDGE_LOOP ( 'NONE', ( #186739, #200918, #169687 ) ) ;
#26652 = EDGE_CURVE ( 'NONE', #175343, #215740, #155785, .T. ) ;
#26653 = FACE_OUTER_BOUND ( 'NONE', #22174, .T. ) ;
#26655 = ORIENTED_EDGE ( 'NONE', *, *, #65177, .F. ) ;
#26654 = CYLINDRICAL_SURFACE ( 'NONE', #146636, 0.09999999999999961697 ) ;
#26656 = DIRECTION ( 'NONE',  ( 0.000000000000000000, 0.9770955615653548199, 0.2128009952262535920 ) ) ;
#26657 = DIRECTION ( 'NONE',  ( 0.000000000000000000, -1.000000000000000000, 0.000000000000000000 ) ) ;
#26658 = VECTOR ( 'NONE', #65197, 1000.000000000000000 ) ;
#26659 = AXIS2_PLACEMENT_3D ( 'NONE', #96209, #36273, #175781 ) ;
#26660 = EDGE_LOOP ( 'NONE', ( #118270, #223598, #84733, #40495, #150949, #77498, #154174, #71609 ) ) ;
#26661 = AXIS2_PLACEMENT_3D ( 'NONE', #250371, #146127, #144832 ) ;
#26662 = DIRECTION ( 'NONE',  ( 0.000000000000000000, -7.304098846218085561E-15, 1.000000000000000000 ) ) ;
#26664 = ADVANCED_FACE ( 'NONE', ( #239225 ), #214516, .F. ) ;
#26663 = CARTESIAN_POINT ( 'NONE',  ( -13.54795643572458097, 66.54933111084451980, -121.4675609943170116 ) ) ;
#26665 = DIRECTION ( 'NONE',  ( 0.000000000000000000, 0.1350103645451946055, -0.9908441862701591329 ) ) ;
#26666 = ORIENTED_EDGE ( 'NONE', *, *, #113984, .T. ) ;
#26667 = CARTESIAN_POINT ( 'NONE',  ( -21.14999999999999858, 64.35000000001268461, -203.5231074845244166 ) ) ;
#26668 = DIRECTION ( 'NONE',  ( -1.000000000000000000, -0.000000000000000000, -0.000000000000000000 ) ) ;
#26669 = EDGE_CURVE ( 'NONE', #146715, #39843, #120586, .T. ) ;
#26670 = ORIENTED_EDGE ( 'NONE', *, *, #141181, .F. ) ;
#26671 = EDGE_CURVE ( 'NONE', #10810, #176282, #180705, .T. ) ;
#26672 = VECTOR ( 'NONE', #209686, 1000.000000000000000 ) ;
#26673 = ADVANCED_FACE ( 'NONE', ( #38456 ), #30450, .F. ) ;
#26674 = AXIS2_PLACEMENT_3D ( 'NONE', #146924, #167825, #184779 ) ;
#26675 = ORIENTED_EDGE ( 'NONE', *, *, #69637, .F. ) ;
#26676 = DIRECTION ( 'NONE',  ( 0.000000000000000000, 1.000000000000000000, 1.734723475976817507E-14 ) ) ;
#26677 = CIRCLE ( 'NONE', #59952, 0.1000000000000028644 ) ;
#26678 = ORIENTED_EDGE ( 'NONE', *, *, #2894, .T. ) ;
#26679 = CARTESIAN_POINT ( 'NONE',  ( 21.05000000000000071, 87.65000000001215597, -139.4231074845242802 ) ) ;
#26680 = CARTESIAN_POINT ( 'NONE',  ( 21.05000000000000071, -8.999999999988842703, -124.1060308773475924 ) ) ;
#26683 = EDGE_CURVE ( 'NONE', #123176, #102761, #109957, .T. ) ;
#26682 = ORIENTED_EDGE ( 'NONE', *, *, #196042, .F. ) ;
#26681 = DIRECTION ( 'NONE',  ( 1.000000000000000000, -0.000000000000000000, -0.000000000000000000 ) ) ;
#26684 = DIRECTION ( 'NONE',  ( 0.000000000000000000, 0.000000000000000000, -1.000000000000000000 ) ) ;
#26685 = DIRECTION ( 'NONE',  ( 0.000000000000000000, 0.000000000000000000, -1.000000000000000000 ) ) ;
#26686 = SURFACE_STYLE_USAGE ( .BOTH. , #238322 ) ;
#26687 = DIRECTION ( 'NONE',  ( -1.000000000000000000, -0.000000000000000000, 0.000000000000000000 ) ) ;
#26688 = PLANE ( 'NONE',  #97783 ) ;
#26689 = DIRECTION ( 'NONE',  ( 1.000000000000000000, 0.000000000000000000, 0.000000000000000000 ) ) ;
#26690 = CIRCLE ( 'NONE', #64081, 0.09999999999999939493 ) ;
#26691 = ADVANCED_FACE ( 'NONE', ( #180547 ), #222202, .T. ) ;
#26692 = FACE_OUTER_BOUND ( 'NONE', #25879, .T. ) ;
#26693 = AXIS2_PLACEMENT_3D ( 'NONE', #137574, #159737, #82723 ) ;
#26694 = EDGE_CURVE ( 'NONE', #152864, #246882, #143282, .T. ) ;
#26695 = CYLINDRICAL_SURFACE ( 'NONE', #236356, 0.1000000000000028644 ) ;
#26697 = ORIENTED_EDGE ( 'NONE', *, *, #63806, .T. ) ;
#26696 = CARTESIAN_POINT ( 'NONE',  ( 21.05000000000000071, 1.115600667400684642E-11, -146.1500000000000341 ) ) ;
#26699 = DIRECTION ( 'NONE',  ( 0.000000000000000000, -1.000000000000000000, 0.000000000000000000 ) ) ;
#26698 = AXIS2_PLACEMENT_3D ( 'NONE', #203369, #202087, #222914 ) ;
#26700 = ORIENTED_EDGE ( 'NONE', *, *, #256157, .F. ) ;
#26701 = CARTESIAN_POINT ( 'NONE',  ( -18.59999999999999787, 64.35000000001198828, -115.1731074845243796 ) ) ;
#26702 = AXIS2_PLACEMENT_3D ( 'NONE', #89209, #70973, #147922 ) ;
#26704 = ADVANCED_FACE ( 'NONE', ( #85251 ), #81397, .F. ) ;
#26703 = CYLINDRICAL_SURFACE ( 'NONE', #171800, 0.5000000000000004441 ) ;
#26705 = DIRECTION ( 'NONE',  ( 0.000000000000000000, -8.905812670947865054E-15, 1.000000000000000000 ) ) ;
#26706 = CARTESIAN_POINT ( 'NONE',  ( 20.84451136049616338, 65.37985808520433295, -196.0291829250029991 ) ) ;
#26707 = CARTESIAN_POINT ( 'NONE',  ( -21.05000000000000071, 1.750000000011155743, -45.16951155790164307 ) ) ;
#26708 = EDGE_CURVE ( 'NONE', #87352, #35875, #44883, .T. ) ;
#26709 = AXIS2_PLACEMENT_3D ( 'NONE', #131579, #136696, #92434 ) ;
#26711 = ORIENTED_EDGE ( 'NONE', *, *, #243435, .T. ) ;
#26710 = CIRCLE ( 'NONE', #93314, 0.09999999999998898659 ) ;
#26713 = TOROIDAL_SURFACE ( 'NONE', #35107, 0.2000000000000000111, 0.1000000000000000056 ) ;
#26712 = CARTESIAN_POINT ( 'NONE',  ( 18.59999999999999787, 76.00000000001195133, -103.0231074845243171 ) ) ;
#26714 = ORIENTED_EDGE ( 'NONE', *, *, #40228, .T. ) ;
#26715 = DIRECTION ( 'NONE',  ( 0.000000000000000000, -0.9550021345545507412, 0.2965989261549202283 ) ) ;
#26716 = CARTESIAN_POINT ( 'NONE',  ( 22.57856590037848576, -0.004128330053175033321, -21.74994153732456326 ) ) ;
#26717 = ORIENTED_EDGE ( 'NONE', *, *, #51948, .T. ) ;
#26718 = CARTESIAN_POINT ( 'NONE',  ( -21.04999999999999716, 6.497017786443340270, -67.01454569057010247 ) ) ;
#26719 = EDGE_CURVE ( 'NONE', #211733, #19150, #155412, .T. ) ;
#26720 = EDGE_LOOP ( 'NONE', ( #204655, #177233, #234310, #92934 ) ) ;
#26721 = EDGE_CURVE ( 'NONE', #32241, #161437, #224781, .T. ) ;
#26722 = DIRECTION ( 'NONE',  ( 2.952720810173289112E-16, -1.000000000000000000, 0.000000000000000000 ) ) ;
#26723 = EDGE_LOOP ( 'NONE', ( #55297, #170434, #134199, #26829 ) ) ;
#26724 = LINE ( 'NONE', #128377, #52563 ) ;
#26725 = CIRCLE ( 'NONE', #230729, 0.09999999999999939493 ) ;
#26726 = SPHERICAL_SURFACE ( 'NONE', #18007, 0.1000000000000000056 ) ;
#26727 = ORIENTED_EDGE ( 'NONE', *, *, #34071, .F. ) ;
#26728 = CIRCLE ( 'NONE', #1747, 0.09999999999999939493 ) ;
#26730 = EDGE_CURVE ( 'NONE', #79286, #139556, #61880, .T. ) ;
#26729 = ORIENTED_EDGE ( 'NONE', *, *, #86968, .F. ) ;
#26731 = DIRECTION ( 'NONE',  ( -1.000000000000000000, 0.000000000000000000, 0.000000000000000000 ) ) ;
#26733 = ORIENTED_EDGE ( 'NONE', *, *, #43193, .F. ) ;
#26732 = CARTESIAN_POINT ( 'NONE',  ( 14.77516762759921498, 9.436674251854011430, -48.67686193099920899 ) ) ;
#26734 = AXIS2_PLACEMENT_3D ( 'NONE', #15116, #114203, #195048 ) ;
#26735 = CARTESIAN_POINT ( 'NONE',  ( -20.64999999999999858, 8.751106741858205140, -220.7398867978736234 ) ) ;
#26736 = EDGE_LOOP ( 'NONE', ( #65313, #113511, #229067, #173693 ) ) ;
#26737 = AXIS2_PLACEMENT_3D ( 'NONE', #241255, #24790, #104271 ) ;
#26738 = AXIS2_PLACEMENT_3D ( 'NONE', #53105, #72706, #94799 ) ;
#26739 = ORIENTED_EDGE ( 'NONE', *, *, #182785, .F. ) ;
#26740 = DIRECTION ( 'NONE',  ( -0.000000000000000000, 0.8660254037844502539, 0.4999999999999799605 ) ) ;
#26741 = DIRECTION ( 'NONE',  ( 0.7071067811865388020, 0.6909108974501111389, 0.1504730267679034728 ) ) ;
#26742 = CARTESIAN_POINT ( 'NONE',  ( -20.94999999999999929, 68.92903212821357783, -166.2765432626560766 ) ) ;
#26743 = AXIS2_PLACEMENT_3D ( 'NONE', #54164, #172888, #112867 ) ;
#26744 = PLANE ( 'NONE',  #237961 ) ;
#26745 = CARTESIAN_POINT ( 'NONE',  ( 20.04999999999999716, 12.98648691417777101, -219.5104337504080263 ) ) ;
#26746 = LINE ( 'NONE', #245775, #4624 ) ;
#26747 = VECTOR ( 'NONE', #82064, 1000.000000000000114 ) ;
#26749 = VERTEX_POINT ( 'NONE', #102241 ) ;
#26748 = ADVANCED_FACE ( 'NONE', ( #121859 ), #26625, .T. ) ;
#26750 = CARTESIAN_POINT ( 'NONE',  ( -16.93935632781549572, 66.01526950028744523, -182.6334467358141467 ) ) ;
#26751 = AXIS2_PLACEMENT_3D ( 'NONE', #214857, #117051, #234412 ) ;
#26752 = DIRECTION ( 'NONE',  ( 1.000000000000000000, 0.000000000000000000, 0.000000000000000000 ) ) ;
#26753 = CARTESIAN_POINT ( 'NONE',  ( 20.95159278453404283, 67.09210366206302467, -128.0383872994151204 ) ) ;
#26755 = CARTESIAN_POINT ( 'NONE',  ( -20.54999999999999716, 6.268811756569107274, -220.3853799378769622 ) ) ;
#26754 = AXIS2_PLACEMENT_3D ( 'NONE', #137753, #156090, #159928 ) ;
#26756 = EDGE_CURVE ( 'NONE', #216892, #250368, #193187, .T. ) ;
#26757 = ORIENTED_EDGE ( 'NONE', *, *, #236881, .T. ) ;
#26758 = DIRECTION ( 'NONE',  ( 0.000000000000000000, 0.000000000000000000, -1.000000000000000000 ) ) ;
#26759 = ORIENTED_EDGE ( 'NONE', *, *, #8710, .T. ) ;
#26760 = CYLINDRICAL_SURFACE ( 'NONE', #2424, 0.1000000000000028644 ) ;
#26762 = VERTEX_POINT ( 'NONE', #226046 ) ;
#26761 = AXIS2_PLACEMENT_3D ( 'NONE', #36043, #33507, #94709 ) ;
#26763 = DIRECTION ( 'NONE',  ( 0.000000000000000000, -0.6728971962616697722, -0.7397360091702875895 ) ) ;
#26764 = CARTESIAN_POINT ( 'NONE',  ( -23.15000000000000213, 4.150000000011156764, -88.75000000000004263 ) ) ;
#26765 = VERTEX_POINT ( 'NONE', #3161 ) ;
#26766 = ORIENTED_EDGE ( 'NONE', *, *, #129542, .T. ) ;
#26769 = ORIENTED_EDGE ( 'NONE', *, *, #202223, .F. ) ;
#26768 = ADVANCED_FACE ( 'NONE', ( #183120 ), #47429, .F. ) ;
#26767 = CARTESIAN_POINT ( 'NONE',  ( -22.50000000000000000, 11.75000000001115552, -67.00000000000004263 ) ) ;
#26770 = CARTESIAN_POINT ( 'NONE',  ( -18.39999999999999858, 64.52132590001261292, -93.74841426818372270 ) ) ;
#26771 = ORIENTED_EDGE ( 'NONE', *, *, #17494, .F. ) ;
#26772 = AXIS2_PLACEMENT_3D ( 'NONE', #86515, #166128, #183095 ) ;
#26773 = CARTESIAN_POINT ( 'NONE',  ( 23.14999999999999858, 36.65892442174472876, -249.5511627012454596 ) ) ;
#26774 = EDGE_CURVE ( 'NONE', #38351, #153545, #164149, .T. ) ;
#26775 = CYLINDRICAL_SURFACE ( 'NONE', #35572, 4.049999999999998046 ) ;
#26776 = ORIENTED_EDGE ( 'NONE', *, *, #151865, .F. ) ;
#26777 = AXIS2_PLACEMENT_3D ( 'NONE', #235534, #56873, #36079 ) ;
#26778 = CYLINDRICAL_SURFACE ( 'NONE', #31160, 0.09999999999999892308 ) ;
#26779 = ADVANCED_FACE ( 'NONE', ( #24052 ), #4457, .T. ) ;
#26780 = CARTESIAN_POINT ( 'NONE',  ( -20.85000000000000142, 7.633102355717365839, -241.5185714324494484 ) ) ;
#26782 = ORIENTED_EDGE ( 'NONE', *, *, #135045, .F. ) ;
#26781 = AXIS2_PLACEMENT_3D ( 'NONE', #28753, #109504, #230769 ) ;
#26783 = CIRCLE ( 'NONE', #193374, 3.900000000000000799 ) ;
#26784 = EDGE_CURVE ( 'NONE', #81112, #206635, #51669, .T. ) ;
#26785 = VECTOR ( 'NONE', #212948, 1000.000000000000000 ) ;
#26788 = ADVANCED_FACE ( 'NONE', ( #27918 ), #80724, .T. ) ;
#26787 = EDGE_CURVE ( 'NONE', #78569, #139340, #230791, .T. ) ;
#26786 = DIRECTION ( 'NONE',  ( 0.000000000000000000, -7.086529944415893080E-15, 1.000000000000000000 ) ) ;
#26789 = CARTESIAN_POINT ( 'NONE',  ( 18.49999999999999289, 15.22030141505243961, -222.9130098973476777 ) ) ;
#26791 = ORIENTED_EDGE ( 'NONE', *, *, #135447, .F. ) ;
#26790 = DIRECTION ( 'NONE',  ( -0.000000000000000000, -0.1332476588733589318, 0.9910827722268049644 ) ) ;
#26792 = DIRECTION ( 'NONE',  ( 1.000000000000000000, 0.000000000000000000, 0.000000000000000000 ) ) ;
#26793 = DIRECTION ( 'NONE',  ( -0.000000000000000000, 0.4721928772777346239, 0.8814952561688430555 ) ) ;
#26794 = DIRECTION ( 'NONE',  ( -1.000000000000000000, 0.000000000000000000, 0.000000000000000000 ) ) ;
#26796 = DIRECTION ( 'NONE',  ( 1.000000000000000000, 0.000000000000000000, 0.000000000000000000 ) ) ;
#26795 = CARTESIAN_POINT ( 'NONE',  ( -17.04761207306819770, 10.02645087340893149, -154.8500000000000512 ) ) ;
#26797 = CARTESIAN_POINT ( 'NONE',  ( 20.95595624212449692, 39.27834562703553445, -236.7364447859425525 ) ) ;
#26798 = CARTESIAN_POINT ( 'NONE',  ( 21.05000000000000071, 8.776282895303632259, -109.0586289951409924 ) ) ;
#26799 = CARTESIAN_POINT ( 'NONE',  ( 23.24999999999999289, 11.65000000001116298, -93.48519422934610645 ) ) ;
#26800 = AXIS2_PLACEMENT_3D ( 'NONE', #154067, #75774, #151472 ) ;
#26801 = DIRECTION ( 'NONE',  ( 0.000000000000000000, -0.5826443254699606999, -0.8127272543711416830 ) ) ;
#26803 = EDGE_CURVE ( 'NONE', #247138, #93424, #89114, .T. ) ;
#26802 = AXIS2_PLACEMENT_3D ( 'NONE', #175496, #152084, #16422 ) ;
#26804 = AXIS2_PLACEMENT_3D ( 'NONE', #90262, #128134, #47278 ) ;
#26805 = EDGE_CURVE ( 'NONE', #59500, #214176, #72565, .T. ) ;
#26806 = ORIENTED_EDGE ( 'NONE', *, *, #24515, .T. ) ;
#26807 = ORIENTED_EDGE ( 'NONE', *, *, #10707, .F. ) ;
#26808 = EDGE_CURVE ( 'NONE', #28183, #116722, #68305, .T. ) ;
#26809 = FACE_OUTER_BOUND ( 'NONE', #116459, .T. ) ;
#26810 = VERTEX_POINT ( 'NONE', #211677 ) ;
#26811 = ADVANCED_FACE ( 'NONE', ( #72164 ), #170013, .F. ) ;
#26812 = DIRECTION ( 'NONE',  ( 1.000000000000000000, -0.000000000000000000, -0.000000000000000000 ) ) ;
#26813 = EDGE_CURVE ( 'NONE', #16688, #78593, #8338, .T. ) ;
#26814 = ORIENTED_EDGE ( 'NONE', *, *, #163057, .T. ) ;
#26815 =( LENGTH_UNIT ( ) NAMED_UNIT ( * ) SI_UNIT ( .MILLI., .METRE. ) );
#26816 = CARTESIAN_POINT ( 'NONE',  ( 20.91682497891423154, 65.67736539654967487, -130.9625116876572406 ) ) ;
#26817 = CARTESIAN_POINT ( 'NONE',  ( -20.54999999999999716, 68.75000000001185185, -90.77310748452435973 ) ) ;
#26818 = VERTEX_POINT ( 'NONE', #107416 ) ;
#26819 = CARTESIAN_POINT ( 'NONE',  ( -20.94999999999994245, 67.65000000001118963, -3.023107484524792277 ) ) ;
#26820 = ORIENTED_EDGE ( 'NONE', *, *, #82869, .F. ) ;
#26821 = ORIENTED_EDGE ( 'NONE', *, *, #90139, .F. ) ;
#26822 = CARTESIAN_POINT ( 'NONE',  ( -16.89268316805466341, 9.951721813253341153, -46.14424752145445296 ) ) ;
#26823 = CARTESIAN_POINT ( 'NONE',  ( 23.24999999999997513, 11.65000000001116298, -126.9851942293460922 ) ) ;
#26825 = ORIENTED_EDGE ( 'NONE', *, *, #2905, .T. ) ;
#26824 = FACE_OUTER_BOUND ( 'NONE', #133687, .T. ) ;
#26826 = ADVANCED_FACE ( 'NONE', ( #87832 ), #150424, .T. ) ;
#26827 = CARTESIAN_POINT ( 'NONE',  ( 20.04142135623731136, 11.75000000001116263, -158.6500000000000057 ) ) ;
#26829 = ORIENTED_EDGE ( 'NONE', *, *, #155562, .F. ) ;
#26828 = CARTESIAN_POINT ( 'NONE',  ( 20.94999999999999929, 77.36242903720540198, -128.6342262366031548 ) ) ;
#26830 = DIRECTION ( 'NONE',  ( 0.000000000000000000, 0.4721928772777344019, 0.8814952561688432775 ) ) ;
#26831 = CARTESIAN_POINT ( 'NONE',  ( 21.05000000000000071, 4.898587196589410857E-16, -29.50000000000000355 ) ) ;
#26833 = ORIENTED_EDGE ( 'NONE', *, *, #3552, .F. ) ;
#26832 = DIRECTION ( 'NONE',  ( 0.000000000000000000, 0.2128009952263601456, -0.9770955615653316162 ) ) ;
#26834 = DIRECTION ( 'NONE',  ( 1.000000000000000000, 2.952720810173289112E-16, -0.000000000000000000 ) ) ;
#26835 = CARTESIAN_POINT ( 'NONE',  ( -18.50211644919735576, 10.30207779525983014, -72.48955207167824710 ) ) ;
#26836 = CARTESIAN_POINT ( 'NONE',  ( -18.59999999999999787, 85.32100840337361092, -162.7871692354464130 ) ) ;
#26837 = EDGE_CURVE ( 'NONE', #217779, #67383, #167421, .T. ) ;
#26839 = CARTESIAN_POINT ( 'NONE',  ( -17.29158576265543346, 10.36474766601791586, -22.08275824479217775 ) ) ;
#26838 = CARTESIAN_POINT ( 'NONE',  ( -17.11825945287481687, 10.05000000001113847, -121.3500000000000227 ) ) ;
#26840 = DIRECTION ( 'NONE',  ( 0.000000000000000000, 0.9654727137038726648, -0.2605042016806632943 ) ) ;
#26841 = AXIS2_PLACEMENT_3D ( 'NONE', #248989, #70368, #71636 ) ;
#26842 = CARTESIAN_POINT ( 'NONE',  ( 18.33996824403475756, 85.56963985944447870, -163.2040418470076588 ) ) ;
#26843 = VECTOR ( 'NONE', #126036, 1000.000000000000000 ) ;
#26844 = DIRECTION ( 'NONE',  ( -1.000000000000000000, 0.000000000000000000, 0.000000000000000000 ) ) ;
#26845 = DIRECTION ( 'NONE',  ( 0.000000000000000000, -0.1568667991644355497, -0.9876197685951332295 ) ) ;
#26846 = EDGE_LOOP ( 'NONE', ( #81622, #45470, #84061, #223428 ) ) ;
#26848 = EDGE_LOOP ( 'NONE', ( #53504, #108058, #104179, #253478 ) ) ;
#26847 = VECTOR ( 'NONE', #187547, 1000.000000000000114 ) ;
#26849 = VERTEX_POINT ( 'NONE', #90416 ) ;
#26850 = AXIS2_PLACEMENT_3D ( 'NONE', #138068, #79377, #241053 ) ;
#26851 = DIRECTION ( 'NONE',  ( 0.000000000000000000, -0.9998779222360097974, 0.01562500000000363945 ) ) ;
#26852 = ORIENTED_EDGE ( 'NONE', *, *, #221831, .T. ) ;
#26853 = FACE_OUTER_BOUND ( 'NONE', #52820, .T. ) ;
#26854 = ORIENTED_EDGE ( 'NONE', *, *, #215785, .T. ) ;
#26855 = EDGE_CURVE ( 'NONE', #34297, #207268, #35179, .T. ) ;
#26856 = CARTESIAN_POINT ( 'NONE',  ( -22.47007471830798764, 7.720710651937634061, -100.5000000000000426 ) ) ;
#26857 = DIRECTION ( 'NONE',  ( 0.000000000000000000, 0.000000000000000000, -1.000000000000000000 ) ) ;
#26858 = VERTEX_POINT ( 'NONE', #229938 ) ;
#26859 = AXIS2_PLACEMENT_3D ( 'NONE', #62896, #142430, #185418 ) ;
#26860 = CARTESIAN_POINT ( 'NONE',  ( 14.45963434102924694, 9.451541661396669625, -152.4538754988305982 ) ) ;
#26861 = CIRCLE ( 'NONE', #114127, 0.09999999999998898659 ) ;
#26862 = ORIENTED_EDGE ( 'NONE', *, *, #121659, .F. ) ;
#26863 = EDGE_LOOP ( 'NONE', ( #248958, #49567, #20085, #20430 ) ) ;
#26864 = EDGE_LOOP ( 'NONE', ( #160576, #197352, #91400, #128655 ) ) ;
#26865 = AXIS2_PLACEMENT_3D ( 'NONE', #50440, #129984, #255021 ) ;
#26866 = DIRECTION ( 'NONE',  ( 7.304098846218134667E-16, -1.000000000000000000, 0.000000000000000000 ) ) ;
#26867 = CARTESIAN_POINT ( 'NONE',  ( -22.39999999999999858, 76.10000000001245724, -181.6726782920691505 ) ) ;
#26868 = CARTESIAN_POINT ( 'NONE',  ( -21.44999999999999929, 7.350000000011155166, -54.65000000000000568 ) ) ;
#26869 = AXIS2_PLACEMENT_3D ( 'NONE', #135936, #36894, #116404 ) ;
#26870 = CARTESIAN_POINT ( 'NONE',  ( -21.07928932188134041, 69.67148334361836248, -69.62200263017875557 ) ) ;
#26871 = CYLINDRICAL_SURFACE ( 'NONE', #19105, 0.1000000000000055844 ) ;
#26872 = DIRECTION ( 'NONE',  ( 1.186688945009009831E-16, 1.000000000000000000, 6.982962677686266711E-15 ) ) ;
#26874 = DIRECTION ( 'NONE',  ( 1.000000000000000000, 0.000000000000000000, 0.000000000000000000 ) ) ;
#26873 = CARTESIAN_POINT ( 'NONE',  ( 21.05000000000000071, 11.75000000001116263, -193.9851942293460070 ) ) ;
#26876 = ORIENTED_EDGE ( 'NONE', *, *, #77921, .T. ) ;
#26875 = CARTESIAN_POINT ( 'NONE',  ( -18.50000000000000000, 43.07541598710462694, -233.9110336739111631 ) ) ;
#26878 = DIRECTION ( 'NONE',  ( 1.000000000000000000, 0.000000000000000000, 0.000000000000000000 ) ) ;
#26877 = CARTESIAN_POINT ( 'NONE',  ( -18.59999999999999787, -1.835859311432481045, -112.1044391687985780 ) ) ;
#26879 = FACE_OUTER_BOUND ( 'NONE', #240717, .T. ) ;
#26880 = ORIENTED_EDGE ( 'NONE', *, *, #205937, .T. ) ;
#26881 = CARTESIAN_POINT ( 'NONE',  ( 20.95512820512820440, 10.62384868372303615, -74.66491356908764487 ) ) ;
#26883 = VECTOR ( 'NONE', #164744, 1000.000000000000000 ) ;
#26882 = DIRECTION ( 'NONE',  ( 1.000000000000000000, -0.000000000000000000, 0.000000000000000000 ) ) ;
#26884 = CARTESIAN_POINT ( 'NONE',  ( 19.83283456528359423, 64.25000000001148237, -44.67310748510406171 ) ) ;
#26885 = VECTOR ( 'NONE', #136944, 1000.000000000000000 ) ;
#26886 = ORIENTED_EDGE ( 'NONE', *, *, #912, .F. ) ;
#26887 = AXIS2_PLACEMENT_3D ( 'NONE', #153371, #149499, #129896 ) ;
#26888 = CYLINDRICAL_SURFACE ( 'NONE', #257530, 0.1000000000000028644 ) ;
#26889 = VECTOR ( 'NONE', #235669, 1000.000000000000000 ) ;
#26890 = DIRECTION ( 'NONE',  ( 0.000000000000000000, 1.000000000000000000, 0.000000000000000000 ) ) ;
#26891 = CARTESIAN_POINT ( 'NONE',  ( 21.05000000000000071, -1.162701749926853712, -142.1000000000000227 ) ) ;
#26892 = ORIENTED_EDGE ( 'NONE', *, *, #16946, .T. ) ;
#26893 = ORIENTED_EDGE ( 'NONE', *, *, #21132, .T. ) ;
#26894 = AXIS2_PLACEMENT_3D ( 'NONE', #19333, #96281, #237100 ) ;
#26895 = DIRECTION ( 'NONE',  ( 0.000000000000000000, 0.1568667991644863147, -0.9876197685951252359 ) ) ;
#26896 = ORIENTED_EDGE ( 'NONE', *, *, #152057, .F. ) ;
#26897 = DIRECTION ( 'NONE',  ( 0.000000000000000000, -0.1575844902526687130, -0.9875055080513762684 ) ) ;
#26898 = LINE ( 'NONE', #221199, #198900 ) ;
#26899 = CARTESIAN_POINT ( 'NONE',  ( 18.39999999999999858, 85.50000000001166711, -62.92291809330220786 ) ) ;
#26900 = LINE ( 'NONE', #208095, #34400 ) ;
#26901 = ORIENTED_EDGE ( 'NONE', *, *, #8801, .F. ) ;
#26902 = AXIS2_PLACEMENT_3D ( 'NONE', #187400, #227788, #105233 ) ;
#26903 = VECTOR ( 'NONE', #222923, 1000.000000000000000 ) ;
#26904 = AXIS2_PLACEMENT_3D ( 'NONE', #228981, #232845, #54175 ) ;
#26905 = CARTESIAN_POINT ( 'NONE',  ( -15.57281606413133979, 9.370655051134635372, -118.0258232559809244 ) ) ;
#26907 = EDGE_CURVE ( 'NONE', #237038, #123700, #251617, .T. ) ;
#26906 = CARTESIAN_POINT ( 'NONE',  ( -18.40000000000000213, 64.25000000001153921, -48.67310748452440805 ) ) ;
#26908 = FACE_OUTER_BOUND ( 'NONE', #109476, .T. ) ;
#26909 = DIRECTION ( 'NONE',  ( 0.000000000000000000, -1.000000000000000000, 0.000000000000000000 ) ) ;
#26910 = ORIENTED_EDGE ( 'NONE', *, *, #174835, .T. ) ;
#26911 = DIRECTION ( 'NONE',  ( 0.000000000000000000, -0.4999999999999088507, -0.8660254037844913322 ) ) ;
#26913 = ORIENTED_EDGE ( 'NONE', *, *, #184992, .T. ) ;
#26912 = DIRECTION ( 'NONE',  ( 1.000000000000000000, 0.000000000000000000, 0.000000000000000000 ) ) ;
#26914 = DIRECTION ( 'NONE',  ( 0.000000000000000000, 0.000000000000000000, -1.000000000000000000 ) ) ;
#26915 = CARTESIAN_POINT ( 'NONE',  ( -21.05000000000000071, 62.00000000001195133, -108.4502000149068834 ) ) ;
#26916 = EDGE_CURVE ( 'NONE', #40901, #11972, #139154, .T. ) ;
#26917 = CARTESIAN_POINT ( 'NONE',  ( -21.05000000000000071, 72.93748991853819064, -214.8151857698041738 ) ) ;
#26918 = LINE ( 'NONE', #141688, #34008 ) ;
#26919 = DIRECTION ( 'NONE',  ( 0.000000000000000000, -5.214354714482146219E-14, 1.000000000000000000 ) ) ;
#26920 = CARTESIAN_POINT ( 'NONE',  ( -21.37071067811865532, 12.38659663131667976, -219.9481158626206252 ) ) ;
#26921 = ADVANCED_FACE ( 'NONE', ( #52570 ), #48722, .F. ) ;
#26922 = ORIENTED_EDGE ( 'NONE', *, *, #128599, .F. ) ;
#26923 = DIRECTION ( 'NONE',  ( 0.000000000000000000, 0.9910465087640866200, -0.1335171055202867274 ) ) ;
#26924 = DIRECTION ( 'NONE',  ( 0.000000000000000000, -0.6728388485993177515, 0.7397890806274072251 ) ) ;
#26926 = VECTOR ( 'NONE', #106854, 1000.000000000000000 ) ;
#26925 = FACE_OUTER_BOUND ( 'NONE', #157205, .T. ) ;
#26927 = AXIS2_PLACEMENT_3D ( 'NONE', #188302, #107483, #187052 ) ;
#26928 = DIRECTION ( 'NONE',  ( -0.000000000000000000, 0.7397890806274223241, 0.6728388485993012091 ) ) ;
#26929 = DIRECTION ( 'NONE',  ( 0.000000000000000000, 1.000000000000000000, 6.982962677686266711E-15 ) ) ;
#26930 = ORIENTED_EDGE ( 'NONE', *, *, #251875, .F. ) ;
#26931 = ORIENTED_EDGE ( 'NONE', *, *, #70916, .F. ) ;
#26932 = CIRCLE ( 'NONE', #243375, 0.4000000000000114575 ) ;
#26933 = ADVANCED_FACE ( 'NONE', ( #192119 ), #13467, .T. ) ;
#26934 = CARTESIAN_POINT ( 'NONE',  ( -20.54999999999999716, 85.50000000001149658, -45.91707660717669626 ) ) ;
#26935 = AXIS2_PLACEMENT_3D ( 'NONE', #169251, #192633, #208360 ) ;
#26936 = DIRECTION ( 'NONE',  ( 0.000000000000000000, 0.2128009952263601456, -0.9770955615653316162 ) ) ;
#26937 = EDGE_CURVE ( 'NONE', #216189, #66123, #164327, .T. ) ;
#26938 = CARTESIAN_POINT ( 'NONE',  ( 20.94999999999999929, 10.29270135741298731, -139.4573618871519614 ) ) ;
#26939 = EDGE_CURVE ( 'NONE', #173551, #9426, #239146, .T. ) ;
#26941 = CONICAL_SURFACE ( 'NONE', #64327, 4.299999999999945643, 0.7853981633974466137 ) ;
#26940 = FACE_OUTER_BOUND ( 'NONE', #58524, .T. ) ;
#26942 = CYLINDRICAL_SURFACE ( 'NONE', #54985, 14.30833333333333890 ) ;
#26943 = CIRCLE ( 'NONE', #6052, 0.1000000000000028644 ) ;
#26944 = B_SPLINE_CURVE_WITH_KNOTS ( 'NONE', 3,
 ( #120160, #181402, #24898, #21045, #82239, #161841, #202229, #23628 ),
 .UNSPECIFIED., .F., .F.,
 ( 4, 2, 2, 4 ),
 ( 0.000000000000000000, 0.0001881495939909255417, 0.0002822243909863809941, 0.0003762991879818364466 ),
 .UNSPECIFIED. ) ;
#26945 = EDGE_CURVE ( 'NONE', #188354, #52356, #56414, .T. ) ;
#26946 = CIRCLE ( 'NONE', #18550, 0.09999999999999939493 ) ;
#26947 = CARTESIAN_POINT ( 'NONE',  ( -21.05315837326133632, 17.15379753644537075, -224.5473496284387522 ) ) ;
#26948 = EDGE_CURVE ( 'NONE', #242965, #39036, #43521, .T. ) ;
#26949 = ORIENTED_EDGE ( 'NONE', *, *, #110871, .F. ) ;
#26950 = DIRECTION ( 'NONE',  ( 1.000000000000000000, 0.000000000000000000, 0.000000000000000000 ) ) ;
#26951 = VERTEX_POINT ( 'NONE', #237647 ) ;
#26952 = CARTESIAN_POINT ( 'NONE',  ( -21.14999999999999858, 76.00000000001170974, -76.06376443622556849 ) ) ;
#26953 = DIRECTION ( 'NONE',  ( -0.000000000000000000, 0.4856429311786307212, 0.8741572761215384846 ) ) ;
#26955 = AXIS2_PLACEMENT_3D ( 'NONE', #187925, #151377, #8007 ) ;
#26954 = DIRECTION ( 'NONE',  ( 0.000000000000000000, -1.000000000000000000, 0.000000000000000000 ) ) ;
#26956 = CARTESIAN_POINT ( 'NONE',  ( -16.80438519320023616, 9.949779096479501206, -46.15073828092127428 ) ) ;
#26957 = DIRECTION ( 'NONE',  ( 0.000000000000000000, 0.000000000000000000, 1.000000000000000000 ) ) ;
#26958 = CARTESIAN_POINT ( 'NONE',  ( -21.14999999999999858, -0.09999999999999939493, 11.64957080754479968 ) ) ;
#26959 = DIRECTION ( 'NONE',  ( -1.000000000000000000, 0.000000000000000000, 0.000000000000000000 ) ) ;
#26960 = ADVANCED_FACE ( 'NONE', ( #135957 ), #195965, .F. ) ;
#26961 = CARTESIAN_POINT ( 'NONE',  ( 21.46681500597533798, 1.115541036281197940E-11, -93.64248884056873123 ) ) ;
#26962 = AXIS2_PLACEMENT_3D ( 'NONE', #98254, #138671, #137413 ) ;
#26963 = CARTESIAN_POINT ( 'NONE',  ( -23.25000000000000000, 82.25348978056602789, -214.8488183945435139 ) ) ;
#26964 = LINE ( 'NONE', #146855, #148136 ) ;
#26965 = DIRECTION ( 'NONE',  ( 0.000000000000000000, 0.000000000000000000, -1.000000000000000000 ) ) ;
#26966 = VECTOR ( 'NONE', #134202, 1000.000000000000000 ) ;
#26967 = CARTESIAN_POINT ( 'NONE',  ( -16.94445028196807002, 14.20918193489391790, -219.2878138714100373 ) ) ;
#26968 = LINE ( 'NONE', #242124, #82890 ) ;
#26969 = AXIS2_PLACEMENT_3D ( 'NONE', #17771, #19070, #98566 ) ;
#26970 = AXIS2_PLACEMENT_3D ( 'NONE', #48413, #187943, #208791 ) ;
#26971 = ORIENTED_EDGE ( 'NONE', *, *, #17066, .F. ) ;
#26972 = LINE ( 'NONE', #84283, #85422 ) ;
#26973 = CARTESIAN_POINT ( 'NONE',  ( 21.00000000000000000, -1.410778198689825347, -7.973296578895943121 ) ) ;
#26974 = SHAPE_REPRESENTATION ( 'Drag Chain Support Tray Channel', ( #2425 ), #147622 ) ;
#26975 = ORIENTED_EDGE ( 'NONE', *, *, #137943, .T. ) ;
#26976 = CARTESIAN_POINT ( 'NONE',  ( -0.8999999999999993561, -11.65000000000000036, 23.30000000000000426 ) ) ;
#26977 = DIRECTION ( 'NONE',  ( 0.000000000000000000, -0.9654727137038715545, 0.2605042016806676242 ) ) ;
#26978 = ORIENTED_EDGE ( 'NONE', *, *, #111463, .T. ) ;
#26979 = FACE_OUTER_BOUND ( 'NONE', #205445, .T. ) ;
#26980 = DIRECTION ( 'NONE',  ( 6.938893903907224433E-15, 1.000000000000000000, 7.272083257015735086E-15 ) ) ;
#26981 = ORIENTED_EDGE ( 'NONE', *, *, #211806, .F. ) ;
#26982 = AXIS2_PLACEMENT_3D ( 'NONE', #40627, #200939, #143526 ) ;
#26983 = ADVANCED_FACE ( 'NONE', ( #253343 ), #58969, .F. ) ;
#26984 = CYLINDRICAL_SURFACE ( 'NONE', #252070, 0.09999999999999990841 ) ;
#26985 = CIRCLE ( 'NONE', #151889, 0.09999999999998898659 ) ;
#26986 = ORIENTED_EDGE ( 'NONE', *, *, #225238, .F. ) ;
#26987 = LINE ( 'NONE', #68662, #183447 ) ;
#26988 = ADVANCED_FACE ( 'NONE', ( #18599 ), #14319, .T. ) ;
#26990 = EDGE_CURVE ( 'NONE', #99338, #117682, #178995, .T. ) ;
#26989 = CYLINDRICAL_SURFACE ( 'NONE', #254025, 11.80000000000000426 ) ;
#26991 = CARTESIAN_POINT ( 'NONE',  ( -23.15000000000000213, -11.75000000000000000, 11.75000000000000000 ) ) ;
#26993 = CARTESIAN_POINT ( 'NONE',  ( -21.05000000000000071, 40.18490544642472884, -251.4399342103543233 ) ) ;
#26992 = UNCERTAINTY_MEASURE_WITH_UNIT (LENGTH_MEASURE( 1.000000000000000082E-05 ), #34825, 'distance_accuracy_value', 'NONE');
#26994 = DIRECTION ( 'NONE',  ( -0.000000000000000000, -0.000000000000000000, -1.000000000000000000 ) ) ;
#26995 = FACE_OUTER_BOUND ( 'NONE', #145307, .T. ) ;
#26996 = DIRECTION ( 'NONE',  ( 1.000000000000000000, 0.000000000000000000, 0.000000000000000000 ) ) ;
#26997 = EDGE_CURVE ( 'NONE', #90910, #257108, #77268, .T. ) ;
#26998 = CARTESIAN_POINT ( 'NONE',  ( -18.59999999999999787, 11.65000000001115232, -88.35000000000003695 ) ) ;
#26999 = CARTESIAN_POINT ( 'NONE',  ( -18.40000000000000213, 64.25000000001256240, -182.6731074845244507 ) ) ;
#27000 = EDGE_CURVE ( 'NONE', #227815, #67400, #51865, .T. ) ;
#27002 = ORIENTED_EDGE ( 'NONE', *, *, #117044, .F. ) ;
#27001 = CARTESIAN_POINT ( 'NONE',  ( 18.44208962363008197, 87.01025646670076696, -199.4198412699713003 ) ) ;
#27003 = EDGE_LOOP ( 'NONE', ( #137174, #36550, #169492, #149323, #42560, #206822, #25224, #22020, #175978, #204501, #112490, #31720, #177135, #24778 ) ) ;
#27005 = CARTESIAN_POINT ( 'NONE',  ( -14.11361717019515893, 9.457426452500060421, -85.50004186840004650 ) ) ;
#27004 = CARTESIAN_POINT ( 'NONE',  ( 23.15000000000000213, -11.64999999998884483, -134.0000000000000000 ) ) ;
#27007 = VERTEX_POINT ( 'NONE', #34335 ) ;
#27006 = DIRECTION ( 'NONE',  ( 0.000000000000000000, -0.9274965247785323941, -0.3738317757009769760 ) ) ;
#27008 = EDGE_CURVE ( 'NONE', #26118, #30618, #22690, .T. ) ;
#27009 = ORIENTED_EDGE ( 'NONE', *, *, #133785, .T. ) ;
#27010 = B_SPLINE_CURVE_WITH_KNOTS ( 'NONE', 3,
 ( #202855, #62076, #25526, #183307, #142860, #200301, #5923, #4641, #185864, #85444, #7215, #182024, #141603, #82877, #86746, #46343, #243258, #81595, #162473 ),
 .UNSPECIFIED., .F., .F.,
 ( 4, 3, 3, 3, 3, 3, 4 ),
 ( 1.387778780781445676E-17, 2.646747978909012316E-05, 5.271166642128706850E-05, 9.008788829884963154E-05, 0.0001426648776560992193, 0.0001897378458659761016, 0.0001917382627806360094 ),
 .UNSPECIFIED. ) ;
#27011 = DIRECTION ( 'NONE',  ( -1.020425574104004196E-15, 0.2617529984165031243, 0.9651348961777157509 ) ) ;
#27012 = EDGE_CURVE ( 'NONE', #42929, #246745, #189271, .T. ) ;
#27013 = CARTESIAN_POINT ( 'NONE',  ( -14.00000000000000178, 66.15000000001228386, -153.2731074845244166 ) ) ;
#27014 = AXIS2_PLACEMENT_3D ( 'NONE', #246108, #150848, #232975 ) ;
#27016 = EDGE_CURVE ( 'NONE', #196712, #215838, #86986, .T. ) ;
#27015 = DIRECTION ( 'NONE',  ( 0.000000000000000000, 0.9915357197604804940, -0.1298341882520397950 ) ) ;
#27017 = DIRECTION ( 'NONE',  ( 1.000000000000000000, 0.000000000000000000, 0.000000000000000000 ) ) ;
#27018 = DIRECTION ( 'NONE',  ( -0.000000000000000000, 0.1350103645451876666, 0.9908441862701600211 ) ) ;
#27019 = DIRECTION ( 'NONE',  ( -0.000000000000000000, 0.9910827722268049644, -0.1332476588733589318 ) ) ;
#27020 = DIRECTION ( 'NONE',  ( 0.000000000000000000, 0.000000000000000000, 1.000000000000000000 ) ) ;
#27021 = ORIENTED_EDGE ( 'NONE', *, *, #237852, .F. ) ;
#27022 = EDGE_LOOP ( 'NONE', ( #118967, #26518, #158540, #114645 ) ) ;
#27023 = CYLINDRICAL_SURFACE ( 'NONE', #160672, 0.09999999999999939493 ) ;
#27024 = B_SPLINE_CURVE_WITH_KNOTS ( 'NONE', 3,
 ( #141577, #162449, #103709, #205386, #3331, #161156, #221104, #4621, #241958, #63314 ),
 .UNSPECIFIED., .F., .F.,
 ( 4, 3, 3, 4 ),
 ( 0.000000000000000000, 4.874959354402766518E-05, 9.785140065120894143E-05, 0.0001360444631936018149 ),
 .UNSPECIFIED. ) ;
#27025 = CIRCLE ( 'NONE', #85397, 4.000000000000003553 ) ;
#27026 = VECTOR ( 'NONE', #49744, 1000.000000000000000 ) ;
#27027 = EDGE_LOOP ( 'NONE', ( #192512, #209647, #254644, #81028 ) ) ;
#27028 = LINE ( 'NONE', #52969, #176014 ) ;
#27029 = ORIENTED_EDGE ( 'NONE', *, *, #20288, .T. ) ;
#27030 = CARTESIAN_POINT ( 'NONE',  ( 20.85000000000000142, 11.75000000000000355, -33.50000000000000000 ) ) ;
#27031 = CIRCLE ( 'NONE', #22931, 0.09999999999999939493 ) ;
#27032 = TOROIDAL_SURFACE ( 'NONE', #22745, 1.900000000000002576, 0.1000000000000000056 ) ;
#27033 = EDGE_CURVE ( 'NONE', #21223, #20798, #156853, .T. ) ;
#27034 = MECHANICAL_DESIGN_GEOMETRIC_PRESENTATION_REPRESENTATION (  '', ( #43754 ), #131232 ) ;
#27035 = PLANE ( 'NONE',  #10828 ) ;
#27036 = EDGE_CURVE ( 'NONE', #6886, #186491, #114240, .T. ) ;
#27037 = LINE ( 'NONE', #144349, #245562 ) ;
#27038 = VERTEX_POINT ( 'NONE', #19895 ) ;
#27039 = EDGE_CURVE ( 'NONE', #236288, #13140, #1797, .T. ) ;
#27040 = DIRECTION ( 'NONE',  ( 5.603264701231745086E-32, 7.172728831056619538E-15, -1.000000000000000000 ) ) ;
#27041 = ORIENTED_EDGE ( 'NONE', *, *, #125190, .T. ) ;
#27042 = DIRECTION ( 'NONE',  ( -0.000000000000000000, 0.1686199900910463068, -0.9856811345164802063 ) ) ;
#27043 = DIRECTION ( 'NONE',  ( 0.000000000000000000, -0.000000000000000000, 1.000000000000000000 ) ) ;
#27044 = DIRECTION ( 'NONE',  ( -1.000000000000000000, 0.000000000000000000, 0.000000000000000000 ) ) ;
#27045 = CYLINDRICAL_SURFACE ( 'NONE', #107337, 0.1000000000000013933 ) ;
#27046 = ORIENTED_EDGE ( 'NONE', *, *, #92523, .F. ) ;
#27047 = DIRECTION ( 'NONE',  ( 0.000000000000000000, -0.2617529984165031243, -0.9651348961777157509 ) ) ;
#27049 = ORIENTED_EDGE ( 'NONE', *, *, #255904, .T. ) ;
#27048 = AXIS2_PLACEMENT_3D ( 'NONE', #253847, #94784, #53090 ) ;
#27052 = VERTEX_POINT ( 'NONE', #113836 ) ;
#27051 = CARTESIAN_POINT ( 'NONE',  ( 20.94999999999999929, 74.73788286442776041, -233.7359682632885267 ) ) ;
#27050 = CARTESIAN_POINT ( 'NONE',  ( 18.48536876927967398, 46.96058523626525272, -255.3059130797066985 ) ) ;
#27053 = DIRECTION ( 'NONE',  ( 0.000000000000000000, 8.881784197000696176E-16, -1.000000000000000000 ) ) ;
#27055 = ORIENTED_EDGE ( 'NONE', *, *, #84122, .F. ) ;
#27054 = AXIS2_PLACEMENT_3D ( 'NONE', #24821, #27398, #147298 ) ;
#27056 = CIRCLE ( 'NONE', #10289, 0.2000000000000057288 ) ;
#27057 = ORIENTED_EDGE ( 'NONE', *, *, #174087, .T. ) ;
#27058 = LINE ( 'NONE', #105229, #211479 ) ;
#27059 = DIRECTION ( 'NONE',  ( 0.000000000000000000, -0.9908441862701420355, -0.1350103645453197554 ) ) ;
#27060 = DIRECTION ( 'NONE',  ( -0.000000000000000000, -0.000000000000000000, 1.000000000000000000 ) ) ;
#27061 = AXIS2_PLACEMENT_3D ( 'NONE', #157512, #160063, #60922 ) ;
#27062 = CIRCLE ( 'NONE', #97738, 0.1000000000000055705 ) ;
#27063 = DIRECTION ( 'NONE',  ( 0.000000000000000000, 0.9126074666063791474, 0.4088369013363231663 ) ) ;
#27064 = CIRCLE ( 'NONE', #47857, 0.09999999999998898659 ) ;
#27065 = EDGE_LOOP ( 'NONE', ( #93464, #166277, #116353, #113668 ) ) ;
#27066 = DIRECTION ( 'NONE',  ( 0.000000000000000000, 0.000000000000000000, 1.000000000000000000 ) ) ;
#27067 = CARTESIAN_POINT ( 'NONE',  ( -16.83794479845801462, 14.10322380767677863, -219.1100655228689220 ) ) ;
#27068 = TOROIDAL_SURFACE ( 'NONE', #238858, 0.2000000000000000111, 0.1000000000000000056 ) ;
#27069 = CARTESIAN_POINT ( 'NONE',  ( -18.44232395689893877, -9.552282557039065480, -140.8422519848076888 ) ) ;
#27070 = EDGE_LOOP ( 'NONE', ( #9176, #229075, #195769, #120195 ) ) ;
#27071 = DIRECTION ( 'NONE',  ( 1.000000000000000000, 0.000000000000000000, 0.000000000000000000 ) ) ;
#27072 = VERTEX_POINT ( 'NONE', #55117 ) ;
#27073 = DIRECTION ( 'NONE',  ( 0.000000000000000000, 0.000000000000000000, 1.000000000000000000 ) ) ;
#27074 = AXIS2_PLACEMENT_3D ( 'NONE', #118119, #198930, #197645 ) ;
#27075 = CIRCLE ( 'NONE', #39557, 1.900000000000005906 ) ;
#27076 = DIRECTION ( 'NONE',  ( 1.000000000000000000, 0.000000000000000000, 0.000000000000000000 ) ) ;
#27077 = CARTESIAN_POINT ( 'NONE',  ( -22.45354308602760796, 75.99999978012890267, -181.7735403749906595 ) ) ;
#27079 = ORIENTED_EDGE ( 'NONE', *, *, #98305, .F. ) ;
#27078 = CARTESIAN_POINT ( 'NONE',  ( -16.92132318717937522, 9.966070024017081863, -146.6224066303520885 ) ) ;
#27080 = FACE_OUTER_BOUND ( 'NONE', #14447, .T. ) ;
#27081 = AXIS2_PLACEMENT_3D ( 'NONE', #215306, #37984, #18390 ) ;
#27083 = B_SPLINE_CURVE_WITH_KNOTS ( 'NONE', 3,
 ( #13578, #53970, #73572, #233896, #151818, #190947, #55224, #12307, #59654, #98768, #122234, #180922, #201755, #158816, #197902, #240897 ),
 .UNSPECIFIED., .F., .F.,
 ( 4, 3, 3, 3, 3, 4 ),
 ( 0.000000000000000000, 3.357088238232317244E-05, 6.714213034886757942E-05, 0.0001007408646120921551, 0.0001343627955914185768, 0.0001573956632895995484 ),
 .UNSPECIFIED. ) ;
#27082 = CIRCLE ( 'NONE', #172851, 0.1000000000000068751 ) ;
#27084 = CARTESIAN_POINT ( 'NONE',  ( -14.87770893841227249, 62.91120958565418420, -215.7552931531716354 ) ) ;
#27085 = ADVANCED_FACE ( 'NONE', ( #35625 ), #194698, .F. ) ;
#27086 = CARTESIAN_POINT ( 'NONE',  ( 21.05000000000000071, 0.000000000000000000, -0.09999999999999592548 ) ) ;
#27087 = ORIENTED_EDGE ( 'NONE', *, *, #117469, .F. ) ;
#27088 = DIRECTION ( 'NONE',  ( 0.000000000000000000, 0.000000000000000000, -1.000000000000000000 ) ) ;
#27090 = EDGE_CURVE ( 'NONE', #250150, #101654, #64141, .T. ) ;
#27089 = DIRECTION ( 'NONE',  ( 0.000000000000000000, 6.982962677686266711E-15, -1.000000000000000000 ) ) ;
#27091 = ORIENTED_EDGE ( 'NONE', *, *, #37158, .F. ) ;
#27092 = CARTESIAN_POINT ( 'NONE',  ( -22.39999999999999503, 65.19201463318204048, -243.3742797652979277 ) ) ;
#27093 = EDGE_LOOP ( 'NONE', ( #59531, #179494, #154095, #92731 ) ) ;
#27094 = EDGE_CURVE ( 'NONE', #116632, #51707, #147567, .T. ) ;
#27095 = CARTESIAN_POINT ( 'NONE',  ( -16.80468759584941196, 44.17521108926469964, -235.2897310320125825 ) ) ;
#27098 = EDGE_CURVE ( 'NONE', #84395, #73566, #201722, .T. ) ;
#27097 = ORIENTED_EDGE ( 'NONE', *, *, #194826, .F. ) ;
#27096 = DIRECTION ( 'NONE',  ( 0.000000000000000000, -0.9126074666063771490, -0.4088369013363281623 ) ) ;
#27101 = ORIENTED_EDGE ( 'NONE', *, *, #235263, .T. ) ;
#27100 = EDGE_LOOP ( 'NONE', ( #96839, #248408, #162742 ) ) ;
#27099 = DIRECTION ( 'NONE',  ( -1.000000000000000000, -0.000000000000000000, -0.000000000000000000 ) ) ;
#27102 = CARTESIAN_POINT ( 'NONE',  ( -20.64999999999999858, 70.71284696581484752, -215.3770916356353382 ) ) ;
#27103 = CARTESIAN_POINT ( 'NONE',  ( 21.05000000000000071, 1.115600667400684642E-11, -67.00000000000000000 ) ) ;
#27104 = TOROIDAL_SURFACE ( 'NONE', #210256, 0.2000000000000000111, 0.1000000000000000056 ) ;
#27105 = DIRECTION ( 'NONE',  ( 0.000000000000000000, -0.8777080977375132376, 0.4791956752371582251 ) ) ;
#27107 = CARTESIAN_POINT ( 'NONE',  ( -12.33960340485504226, 66.63925083009645789, -52.20853734391712919 ) ) ;
#27106 = CARTESIAN_POINT ( 'NONE',  ( 20.90851465518106167, 46.44433919924416898, -243.0795225066946159 ) ) ;
#27108 = CARTESIAN_POINT ( 'NONE',  ( 15.48841904831874849, 52.18649987366221410, -233.2135506059238139 ) ) ;
#27109 = AXIS2_PLACEMENT_3D ( 'NONE', #112012, #91144, #130259 ) ;
#27110 = DIRECTION ( 'NONE',  ( 0.000000000000000000, -0.2128009952263485993, 0.9770955615653341697 ) ) ;
#27111 = DIRECTION ( 'NONE',  ( 0.000000000000000000, 0.000000000000000000, 1.000000000000000000 ) ) ;
#27112 = DIRECTION ( 'NONE',  ( -4.391705002472927119E-16, -1.000000000000000000, -7.026728003956683390E-15 ) ) ;
#27113 = EDGE_CURVE ( 'NONE', #34297, #229408, #43297, .T. ) ;
#27114 = CARTESIAN_POINT ( 'NONE',  ( 23.15000000000000213, 87.48912529308822172, -139.6231074845242688 ) ) ;
#27115 = EDGE_CURVE ( 'NONE', #185405, #19000, #2861, .T. ) ;
#27116 = ORIENTED_EDGE ( 'NONE', *, *, #147406, .F. ) ;
#27118 = ORIENTED_EDGE ( 'NONE', *, *, #44275, .T. ) ;
#27117 = VECTOR ( 'NONE', #59056, 1000.000000000000000 ) ;
#27119 = FACE_OUTER_BOUND ( 'NONE', #66142, .T. ) ;
#27120 = AXIS2_PLACEMENT_3D ( 'NONE', #203552, #49612, #129159 ) ;
#27122 = ORIENTED_EDGE ( 'NONE', *, *, #43279, .T. ) ;
#27121 = PLANE ( 'NONE',  #132882 ) ;
#27123 = ORIENTED_EDGE ( 'NONE', *, *, #179764, .F. ) ;
#27124 = CARTESIAN_POINT ( 'NONE',  ( -16.81095280782811230, 12.41403342719979719, -211.2428889512998467 ) ) ;
#27125 = ORIENTED_EDGE ( 'NONE', *, *, #64526, .F. ) ;
#27126 = CARTESIAN_POINT ( 'NONE',  ( 23.15000000000000213, 85.00000000001149658, -45.91707660717670336 ) ) ;
#27127 = CIRCLE ( 'NONE', #193697, 0.09999999999999939493 ) ;
#27128 = EDGE_CURVE ( 'NONE', #123899, #192971, #180887, .T. ) ;
#27129 = ORIENTED_EDGE ( 'NONE', *, *, #254845, .T. ) ;
#27130 = AXIS2_PLACEMENT_3D ( 'NONE', #143875, #81309, #164741 ) ;
#27131 = CARTESIAN_POINT ( 'NONE',  ( 18.55857864376267941, 10.36715728753653565, -125.2500000000000284 ) ) ;
#27132 = CARTESIAN_POINT ( 'NONE',  ( -18.52328366898031931, -9.642321089030097880, -174.2148193375701055 ) ) ;
#27133 = EDGE_CURVE ( 'NONE', #59699, #24915, #122643, .T. ) ;
#27135 = ORIENTED_EDGE ( 'NONE', *, *, #129702, .F. ) ;
#27134 = ORIENTED_EDGE ( 'NONE', *, *, #12353, .F. ) ;
#27136 = ORIENTED_EDGE ( 'NONE', *, *, #94184, .T. ) ;
#27137 = FACE_OUTER_BOUND ( 'NONE', #37114, .T. ) ;
#27138 = ORIENTED_EDGE ( 'NONE', *, *, #102861, .T. ) ;
#27139 = ORIENTED_EDGE ( 'NONE', *, *, #105775, .T. ) ;
#27140 = CARTESIAN_POINT ( 'NONE',  ( -16.88005004766534967, 14.15917131436227372, -219.2553795824229610 ) ) ;
#27141 = CARTESIAN_POINT ( 'NONE',  ( 18.47149038651510722, -9.671457157995549281, -73.67278633473839022 ) ) ;
#27143 = ORIENTED_EDGE ( 'NONE', *, *, #16127, .T. ) ;
#27142 = CARTESIAN_POINT ( 'NONE',  ( 20.94999999999999929, 84.73084112150721126, -93.42503276553991043 ) ) ;
#27144 = VECTOR ( 'NONE', #37852, 1000.000000000000114 ) ;
#27145 = DIRECTION ( 'NONE',  ( 1.000000000000000000, -0.000000000000000000, -0.000000000000000000 ) ) ;
#27146 = EDGE_CURVE ( 'NONE', #227067, #48315, #76823, .T. ) ;
#27147 = DIRECTION ( 'NONE',  ( 0.000000000000000000, -1.000000000000000000, 0.000000000000000000 ) ) ;
#27149 = ORIENTED_EDGE ( 'NONE', *, *, #140754, .F. ) ;
#27148 = DIRECTION ( 'NONE',  ( 0.000000000000000000, 0.9651348961777157509, -0.2617529984165031243 ) ) ;
#27150 = CARTESIAN_POINT ( 'NONE',  ( 20.73486653747088582, 7.250000000000026645, -9.250000000000001776 ) ) ;
#27151 = ORIENTED_EDGE ( 'NONE', *, *, #157892, .T. ) ;
#27152 = DIRECTION ( 'NONE',  ( 0.000000000000000000, 3.552713678800493041E-15, -1.000000000000000000 ) ) ;
#27153 = EDGE_CURVE ( 'NONE', #179129, #155241, #197616, .T. ) ;
#27154 = ORIENTED_EDGE ( 'NONE', *, *, #184749, .F. ) ;
#27155 = DIRECTION ( 'NONE',  ( 0.000000000000000000, 0.000000000000000000, -1.000000000000000000 ) ) ;
#27157 = EDGE_CURVE ( 'NONE', #122573, #62691, #124127, .T. ) ;
#27156 = EDGE_LOOP ( 'NONE', ( #254889, #26543, #118272, #157676 ) ) ;
#27159 = LINE ( 'NONE', #204463, #245358 ) ;
#27158 = CARTESIAN_POINT ( 'NONE',  ( 21.14999999999999858, 10.71339244341104013, -45.75000000000000000 ) ) ;
#27160 = VECTOR ( 'NONE', #231104, 1000.000000000000114 ) ;
#27161 = CARTESIAN_POINT ( 'NONE',  ( 18.49999999999999289, 69.55000000001203375, -114.7731074845243455 ) ) ;
#27162 = CIRCLE ( 'NONE', #110505, 0.1000000000000000472 ) ;
#27163 = CARTESIAN_POINT ( 'NONE',  ( -20.15000000000000568, 22.40264273797979655, -231.3739394982302429 ) ) ;
#27164 = ORIENTED_EDGE ( 'NONE', *, *, #121516, .F. ) ;
#27165 = ORIENTED_EDGE ( 'NONE', *, *, #254563, .F. ) ;
#27166 = FACE_OUTER_BOUND ( 'NONE', #87862, .T. ) ;
#27167 = LINE ( 'NONE', #106639, #144124 ) ;
#27168 = VERTEX_POINT ( 'NONE', #199821 ) ;
#27169 = SPHERICAL_SURFACE ( 'NONE', #230745, 0.1000000000000000056 ) ;
#27170 = ORIENTED_EDGE ( 'NONE', *, *, #171744, .F. ) ;
#27171 = ADVANCED_FACE ( 'NONE', ( #81114 ), #163254, .T. ) ;
#27172 = DIRECTION ( 'NONE',  ( 0.000000000000000000, -6.982962677686266711E-15, 1.000000000000000000 ) ) ;
#27173 = ORIENTED_EDGE ( 'NONE', *, *, #194171, .T. ) ;
#27174 = DIRECTION ( 'NONE',  ( 1.000000000000000000, -0.000000000000000000, 0.000000000000000000 ) ) ;
#27175 = DIRECTION ( 'NONE',  ( 0.000000000000000000, -0.4999999999999088507, -0.8660254037844913322 ) ) ;
#27177 = EDGE_CURVE ( 'NONE', #105430, #231806, #204915, .T. ) ;
#27176 = CARTESIAN_POINT ( 'NONE',  ( 18.59999999999999076, 64.25000000001188027, -94.92310748452439384 ) ) ;
#27178 = ORIENTED_EDGE ( 'NONE', *, *, #78623, .T. ) ;
#27179 = CARTESIAN_POINT ( 'NONE',  ( 18.37172112093692888, -9.570961652232536920, -207.8167344534829510 ) ) ;
#27180 = SURFACE_SIDE_STYLE ('',( #180136 ) ) ;
#27181 = AXIS2_PLACEMENT_3D ( 'NONE', #192302, #54059, #34525 ) ;
#27182 = ORIENTED_EDGE ( 'NONE', *, *, #213058, .T. ) ;
#27183 = ORIENTED_EDGE ( 'NONE', *, *, #32302, .F. ) ;
#27184 = VERTEX_POINT ( 'NONE', #104513 ) ;
#27185 = CARTESIAN_POINT ( 'NONE',  ( -20.64999999999999858, 25.94586868676353575, -241.5435999122864530 ) ) ;
#27186 = DIRECTION ( 'NONE',  ( 1.000000000000000000, 0.000000000000000000, 0.000000000000000000 ) ) ;
#27187 = CIRCLE ( 'NONE', #23265, 0.1000000000000028644 ) ;
#27188 = DIRECTION ( 'NONE',  ( 0.000000000000000000, 6.982962677686266711E-15, -1.000000000000000000 ) ) ;
#27189 = FACE_OUTER_BOUND ( 'NONE', #184696, .T. ) ;
#27190 = DIRECTION ( 'NONE',  ( -1.000000000000000000, 0.000000000000000000, -0.000000000000000000 ) ) ;
#27192 = CARTESIAN_POINT ( 'NONE',  ( -20.85000000000000142, -1.263275465206102233, -175.4018646667464338 ) ) ;
#27191 = DIRECTION ( 'NONE',  ( 0.000000000000000000, -0.9651348961777379554, 0.2617529984164210233 ) ) ;
#27194 = ORIENTED_EDGE ( 'NONE', *, *, #71887, .T. ) ;
#27193 = CARTESIAN_POINT ( 'NONE',  ( 21.05000000000000071, 1.115600667400684642E-11, -167.5000000000000284 ) ) ;
#27195 = CARTESIAN_POINT ( 'NONE',  ( -21.05000000000000071, 6.300179817925902981, -167.4485171181181897 ) ) ;
#27196 = ORIENTED_EDGE ( 'NONE', *, *, #189097, .F. ) ;
#27197 = CARTESIAN_POINT ( 'NONE',  ( 21.14999999999999503, 76.10000000001245724, -181.6726782920691505 ) ) ;
#27198 = ORIENTED_EDGE ( 'NONE', *, *, #235822, .T. ) ;
#27199 = ORIENTED_EDGE ( 'NONE', *, *, #87112, .T. ) ;
#27200 = FACE_OUTER_BOUND ( 'NONE', #152400, .T. ) ;
#27201 = FACE_OUTER_BOUND ( 'NONE', #175977, .T. ) ;
#27202 = CARTESIAN_POINT ( 'NONE',  ( -21.07954763557471267, 75.93412408139434433, -209.8523984745624205 ) ) ;
#27203 = DIRECTION ( 'NONE',  ( 1.000000000000000000, 0.000000000000000000, 0.000000000000000000 ) ) ;
#27204 = VECTOR ( 'NONE', #239845, 1000.000000000000000 ) ;
#27205 = CARTESIAN_POINT ( 'NONE',  ( 21.05000000000000071, 76.00000000001229239, -157.1481074845243882 ) ) ;
#27206 = EDGE_LOOP ( 'NONE', ( #163321, #137463, #250823, #70220 ) ) ;
#27207 = EDGE_LOOP ( 'NONE', ( #213639, #76160, #254074, #12217 ) ) ;
#27208 = CARTESIAN_POINT ( 'NONE',  ( -16.98495255085916966, 10.00556436600592214, -188.3653827937794745 ) ) ;
#27209 = ORIENTED_EDGE ( 'NONE', *, *, #3250, .F. ) ;
#27210 = CARTESIAN_POINT ( 'NONE',  ( -20.94999999999999929, -11.64999999998884483, -97.50000000000004263 ) ) ;
#27211 = DIRECTION ( 'NONE',  ( 1.000000000000000000, 0.000000000000000000, 0.000000000000000000 ) ) ;
#27212 = CARTESIAN_POINT ( 'NONE',  ( 18.59999999999999787, -11.65000000000000036, 6.000000000000001776 ) ) ;
#27213 = CARTESIAN_POINT ( 'NONE',  ( 21.14999999999999858, 76.00000000001165290, -69.52310748452431710 ) ) ;
#27214 = CARTESIAN_POINT ( 'NONE',  ( -23.15000000000000213, 76.00000000001142553, -36.02310748452432421 ) ) ;
#27215 = LINE ( 'NONE', #149723, #138211 ) ;
#27216 = VERTEX_POINT ( 'NONE', #6725 ) ;
#27217 = DIRECTION ( 'NONE',  ( 1.000000000000000000, 0.000000000000000000, -0.000000000000000000 ) ) ;
#27218 = DIRECTION ( 'NONE',  ( 1.000000000000000000, 0.000000000000000000, 0.000000000000000000 ) ) ;
#27219 = DIRECTION ( 'NONE',  ( -1.000000000000000000, -3.265361837132813093E-16, 0.000000000000000000 ) ) ;
#27220 = DIRECTION ( 'NONE',  ( 0.000000000000000000, 0.9126074666063844765, 0.4088369013363114535 ) ) ;
#27222 = EDGE_CURVE ( 'NONE', #214984, #223215, #240225, .T. ) ;
#27221 = CYLINDRICAL_SURFACE ( 'NONE', #4025, 0.09999999999999939493 ) ;
#27223 = AXIS2_PLACEMENT_3D ( 'NONE', #96627, #219161, #197028 ) ;
#27224 = CARTESIAN_POINT ( 'NONE',  ( -21.14999999999994174, 87.50449464844290048, -37.85861909827351468 ) ) ;
#27225 = AXIS2_PLACEMENT_3D ( 'NONE', #28647, #31203, #88540 ) ;
#27226 = VECTOR ( 'NONE', #184322, 1000.000000000000000 ) ;
#27227 = AXIS2_PLACEMENT_3D ( 'NONE', #11799, #135551, #152598 ) ;
#27228 = EDGE_LOOP ( 'NONE', ( #234782, #65753, #23091 ) ) ;
#27229 = PRESENTATION_LAYER_ASSIGNMENT (  '', '', ( #185591 ) ) ;
#27230 = CARTESIAN_POINT ( 'NONE',  ( -17.11825945287482753, 65.95000000001232365, -157.3731074845244109 ) ) ;
#27231 = ADVANCED_FACE ( 'NONE', ( #139805 ), #242757, .T. ) ;
#27232 = ORIENTED_EDGE ( 'NONE', *, *, #13809, .T. ) ;
#27233 = DIRECTION ( 'NONE',  ( -3.265361837132813093E-16, 1.000000000000000000, 0.000000000000000000 ) ) ;
#27234 = LINE ( 'NONE', #246251, #243761 ) ;
#27236 = EDGE_CURVE ( 'NONE', #86432, #175343, #223195, .T. ) ;
#27235 = CARTESIAN_POINT ( 'NONE',  ( 21.11345278033240191, 61.86426160980555977, -221.7111410851087498 ) ) ;
#27237 = DIRECTION ( 'NONE',  ( 0.2834754621636358940, 0.03379383663320500997, -0.9583838682682015442 ) ) ;
#27238 = ADVANCED_FACE ( 'NONE', ( #201078, #22468, #23760 ), #103240, .F. ) ;
#27239 = ORIENTED_EDGE ( 'NONE', *, *, #127036, .T. ) ;
#27240 = DIRECTION ( 'NONE',  ( 1.000000000000000000, 0.000000000000000000, 0.000000000000000000 ) ) ;
#27241 = CARTESIAN_POINT ( 'NONE',  ( -23.15000000000000213, -9.499999999988848032, -110.3939691226524786 ) ) ;
#27242 = DIRECTION ( 'NONE',  ( 0.000000000000000000, 0.000000000000000000, 1.000000000000000000 ) ) ;
#27243 = DIRECTION ( 'NONE',  ( 0.000000000000000000, 0.000000000000000000, -1.000000000000000000 ) ) ;
#27244 = CARTESIAN_POINT ( 'NONE',  ( -21.13614978966382196, 69.50089529817859102, -170.0231074845243882 ) ) ;
#27245 = CIRCLE ( 'NONE', #10644, 0.09999999999999061029 ) ;
#27246 = DIRECTION ( 'NONE',  ( 1.000000000000000000, 0.000000000000000000, 0.000000000000000000 ) ) ;
#27247 = AXIS2_PLACEMENT_3D ( 'NONE', #216298, #135471, #78071 ) ;
#27248 = AXIS2_PLACEMENT_3D ( 'NONE', #182174, #237012, #196584 ) ;
#27249 = ORIENTED_EDGE ( 'NONE', *, *, #92092, .T. ) ;
#27250 = EDGE_LOOP ( 'NONE', ( #115617, #145014, #8516, #173070 ) ) ;
#27251 = CARTESIAN_POINT ( 'NONE',  ( 21.05000000000000071, 76.00000000001170974, -69.52310748452431710 ) ) ;
#27252 = FACE_OUTER_BOUND ( 'NONE', #207353, .T. ) ;
#27253 = DIRECTION ( 'NONE',  ( -1.000000000000000000, -0.000000000000000000, -0.000000000000000000 ) ) ;
#27254 = EDGE_CURVE ( 'NONE', #139587, #162722, #257837, .T. ) ;
#27255 = CARTESIAN_POINT ( 'NONE',  ( -21.00023020733438628, 69.60913075474465472, -170.0231074845244166 ) ) ;
#27256 = EDGE_CURVE ( 'NONE', #204622, #52856, #1975, .T. ) ;
#27257 = EDGE_LOOP ( 'NONE', ( #24127, #31391, #38612, #170986 ) ) ;
#27258 = DIRECTION ( 'NONE',  ( 0.000000000000000000, 0.000000000000000000, 1.000000000000000000 ) ) ;
#27259 = VECTOR ( 'NONE', #23792, 1000.000000000000000 ) ;
#27260 = CONTEXT_DEPENDENT_SHAPE_REPRESENTATION ( #110643, #95331 ) ;
#27261 = AXIS2_PLACEMENT_3D ( 'NONE', #109048, #12551, #216826 ) ;
#27262 = AXIS2_PLACEMENT_3D ( 'NONE', #170156, #51409, #192258 ) ;
#27263 = CARTESIAN_POINT ( 'NONE',  ( -18.59999999999999787, -9.480686695278977894, -40.44111516875783963 ) ) ;
#27264 = ORIENTED_EDGE ( 'NONE', *, *, #123570, .F. ) ;
#27265 = DIRECTION ( 'NONE',  ( -1.000000000000000000, 0.000000000000000000, 0.000000000000000000 ) ) ;
#27266 = EDGE_CURVE ( 'NONE', #86605, #27579, #164514, .T. ) ;
#27268 = ORIENTED_EDGE ( 'NONE', *, *, #7011, .F. ) ;
#27267 = CIRCLE ( 'NONE', #89755, 0.09999999999999735489 ) ;
#27269 = EDGE_LOOP ( 'NONE', ( #22267, #77698, #14267 ) ) ;
#27270 = DIRECTION ( 'NONE',  ( 1.000000000000000000, 0.000000000000000000, 0.000000000000000000 ) ) ;
#27271 = AXIS2_PLACEMENT_3D ( 'NONE', #23105, #4772, #242120 ) ;
#27272 = FACE_OUTER_BOUND ( 'NONE', #79804, .T. ) ;
#27273 = DIRECTION ( 'NONE',  ( 2.940209281316622002E-16, -0.9770955615653309501, -0.2128009952263629490 ) ) ;
#27274 = CIRCLE ( 'NONE', #106312, 0.2000000000000057288 ) ;
#27275 = CARTESIAN_POINT ( 'NONE',  ( 18.50000000000000000, -9.399999999988843058, -140.8820418481727188 ) ) ;
#27276 = CARTESIAN_POINT ( 'NONE',  ( 21.05000000000000071, 64.35000000001267040, -203.4231074845244507 ) ) ;
#27277 = DIRECTION ( 'NONE',  ( 0.2834754621636358940, 0.2834754621636501049, -0.9161240771326873977 ) ) ;
#27278 = SPHERICAL_SURFACE ( 'NONE', #55730, 0.1000000000000000056 ) ;
#27279 = EDGE_CURVE ( 'NONE', #157975, #134789, #143643, .T. ) ;
#27281 = CARTESIAN_POINT ( 'NONE',  ( 19.58285714285715073, 11.77074044182232448, -206.2449930062242629 ) ) ;
#27280 = FACE_OUTER_BOUND ( 'NONE', #49231, .T. ) ;
#27282 = CARTESIAN_POINT ( 'NONE',  ( 21.05000000000000426, -1.267579133596468122, -194.8710457894447927 ) ) ;
#27283 = CARTESIAN_POINT ( 'NONE',  ( -16.87435696428308063, 9.950002462943377424, -113.1499917651666038 ) ) ;
#27284 = FACE_BOUND ( 'NONE', #27743, .T. ) ;
#27285 = DIRECTION ( 'NONE',  ( -1.186688945009010077E-16, 1.000000000000000000, 0.000000000000000000 ) ) ;
#27286 = ORIENTED_EDGE ( 'NONE', *, *, #26496, .T. ) ;
#27287 = ORIENTED_EDGE ( 'NONE', *, *, #178761, .F. ) ;
#27288 = CARTESIAN_POINT ( 'NONE',  ( -18.50000000000000000, 12.87592094156238609, -205.3750039893633073 ) ) ;
#27289 = CYLINDRICAL_SURFACE ( 'NONE', #103515, 0.09999999999998898659 ) ;
#27291 = DIRECTION ( 'NONE',  ( 0.000000000000000000, 0.000000000000000000, 1.000000000000000000 ) ) ;
#27290 = DIRECTION ( 'NONE',  ( -1.000000000000000000, -1.476360405086644309E-16, 0.000000000000000000 ) ) ;
#27292 = FACE_OUTER_BOUND ( 'NONE', #104339, .T. ) ;
#27293 = CARTESIAN_POINT ( 'NONE',  ( -20.94999999999999929, -0.2561057920810652089, -167.4651035583276553 ) ) ;
#27294 = CARTESIAN_POINT ( 'NONE',  ( -20.64999999999999858, 68.85000000001222986, -148.8731074845244109 ) ) ;
#27295 = ORIENTED_EDGE ( 'NONE', *, *, #225532, .F. ) ;
#27296 = ORIENTED_EDGE ( 'NONE', *, *, #131669, .T. ) ;
#27297 = AXIS2_PLACEMENT_3D ( 'NONE', #118744, #199575, #56164 ) ;
#27298 = EDGE_CURVE ( 'NONE', #8107, #224679, #22869, .T. ) ;
#27299 = AXIS2_PLACEMENT_3D ( 'NONE', #248323, #230048, #170123 ) ;
#27300 = CARTESIAN_POINT ( 'NONE',  ( -23.15000000000000213, 11.75000000001115552, -197.8999999999999773 ) ) ;
#27301 = ORIENTED_EDGE ( 'NONE', *, *, #132632, .T. ) ;
#27302 = CARTESIAN_POINT ( 'NONE',  ( -20.94999999999999929, 70.53171716061257257, -228.4612385850772682 ) ) ;
#27303 = CIRCLE ( 'NONE', #256319, 0.1999999999999997335 ) ;
#27304 = CARTESIAN_POINT ( 'NONE',  ( -18.59999999999999787, 9.150000000000002132, -12.34999999999999964 ) ) ;
#27305 = VECTOR ( 'NONE', #238398, 1000.000000000000000 ) ;
#27306 = B_SPLINE_CURVE_WITH_KNOTS ( 'NONE', 3,
 ( #149105, #164802, #65689, #146493, #46121, #125662, #106073, #185647, #47397, #166120, #126954, #107378, #8308, #167391, #254573, #112539, #173839, #70866, #253311 ),
 .UNSPECIFIED., .F., .F.,
 ( 4, 3, 3, 3, 3, 3, 4 ),
 ( 0.000000000000000000, 7.110282409890013474E-05, 0.0001508797727291402539, 0.0002027344179858551164, 0.0002343294522349084557, 0.0002454816334821245888, 0.0002619873080085767438 ),
 .UNSPECIFIED. ) ;
#27307 = EDGE_CURVE ( 'NONE', #202658, #197481, #46342, .T. ) ;
#27308 = TOROIDAL_SURFACE ( 'NONE', #143778, 0.2000000000000000111, 0.1000000000000000056 ) ;
#27309 = EDGE_CURVE ( 'NONE', #159302, #249063, #218645, .T. ) ;
#27310 = ORIENTED_EDGE ( 'NONE', *, *, #256074, .F. ) ;
#27311 = DIRECTION ( 'NONE',  ( 1.000000000000000000, 0.000000000000000000, 0.000000000000000000 ) ) ;
#27312 =( BOUNDED_SURFACE ( )  B_SPLINE_SURFACE ( 3, 2, ( 
 ( #135184, #37404, #193907 ),
 ( #39983, #34848, #15275 ),
 ( #153534, #156084, #192614 ),
 ( #234290, #96058, #13985 ) ),
 .UNSPECIFIED., .F., .F., .F. ) 
 B_SPLINE_SURFACE_WITH_KNOTS ( ( 4, 4 ),
 ( 3, 3 ),
 ( 0.0008258556059633777964, 0.0009616864997632737413 ),
 ( 0.000000000000000000, 1.000000000000000000 ),
 .UNSPECIFIED. ) 
 GEOMETRIC_REPRESENTATION_ITEM ( )  RATIONAL_B_SPLINE_SURFACE ( (
 ( 1.000000000000000000, 0.9152888060719349683, 1.000000000000000000),
 ( 1.000000000000000000, 0.9327727094138091868, 1.000000000000000000),
 ( 1.000000000000000000, 0.9369023509258495030, 1.000000000000000000),
 ( 1.000000000000000000, 0.9246339933864486937, 1.000000000000000000) ) ) 
 REPRESENTATION_ITEM ( '' )  SURFACE ( )  );
#27313 = ORIENTED_EDGE ( 'NONE', *, *, #177474, .T. ) ;
#27314 = ADVANCED_FACE ( 'NONE', ( #108407 ), #211358, .T. ) ;
#27317 = EDGE_CURVE ( 'NONE', #53973, #105004, #122823, .T. ) ;
#27316 = CIRCLE ( 'NONE', #177150, 0.1000000000000116629 ) ;
#27315 = LINE ( 'NONE', #247603, #158045 ) ;
#27319 = CIRCLE ( 'NONE', #18895, 0.9000000000000014655 ) ;
#27318 = CARTESIAN_POINT ( 'NONE',  ( -23.15000000000000213, 11.75000000001115552, -164.4000000000000057 ) ) ;
#27320 = CARTESIAN_POINT ( 'NONE',  ( 15.74999999999999645, 66.65000000001258229, -186.7731074845244166 ) ) ;
#27321 = CARTESIAN_POINT ( 'NONE',  ( -20.12071067811865888, 9.320710678118654613, -12.34999999999999964 ) ) ;
#27322 = DIRECTION ( 'NONE',  ( 0.000000000000000000, 0.000000000000000000, -1.000000000000000000 ) ) ;
#27323 = LINE ( 'NONE', #162961, #91561 ) ;
#27324 = CIRCLE ( 'NONE', #56487, 0.1000000000000124678 ) ;
#27325 = ADVANCED_FACE ( 'NONE', ( #8028 ), #109665, .T. ) ;
#27326 = PLANE ( 'NONE',  #254923 ) ;
#27327 = FACE_OUTER_BOUND ( 'NONE', #50114, .T. ) ;
#27329 = VERTEX_POINT ( 'NONE', #250466 ) ;
#27328 = CARTESIAN_POINT ( 'NONE',  ( 18.33996824403354609, -0.7705153381573188742, -242.4320089669257356 ) ) ;
#27331 = DIRECTION ( 'NONE',  ( 0.000000000000000000, 0.000000000000000000, 1.000000000000000000 ) ) ;
#27330 = CARTESIAN_POINT ( 'NONE',  ( -18.50000000000000000, -11.78281952876890060, -191.5407366062592871 ) ) ;
#27332 = ORIENTED_EDGE ( 'NONE', *, *, #42473, .T. ) ;
#27333 = EDGE_LOOP ( 'NONE', ( #252121, #1190, #170431, #230798, #99315 ) ) ;
#27334 = EDGE_CURVE ( 'NONE', #48376, #79572, #177003, .T. ) ;
#27335 = EDGE_LOOP ( 'NONE', ( #155686, #2683, #208275, #26451 ) ) ;
#27336 = DIRECTION ( 'NONE',  ( 0.000000000000000000, -6.982962677686266711E-15, 1.000000000000000000 ) ) ;
#27338 = EDGE_CURVE ( 'NONE', #74869, #220667, #13157, .T. ) ;
#27337 = ADVANCED_FACE ( 'NONE', ( #148824 ), #246615, .F. ) ;
#27339 = CARTESIAN_POINT ( 'NONE',  ( -22.32929514600008503, 29.70208827356600523, -252.5591762845882329 ) ) ;
#27340 = DIRECTION ( 'NONE',  ( 0.000000000000000000, 0.000000000000000000, 1.000000000000000000 ) ) ;
#27341 = CARTESIAN_POINT ( 'NONE',  ( 23.14999999999999858, 1.115600667400684642E-11, -100.5000000000000426 ) ) ;
#27343 = DIRECTION ( 'NONE',  ( 1.000000000000000000, -1.836970198721029934E-16, -1.282749433769087582E-30 ) ) ;
#27342 = AXIS2_PLACEMENT_3D ( 'NONE', #214995, #14260, #75519 ) ;
#27344 = CARTESIAN_POINT ( 'NONE',  ( 21.00000000000000000, 22.53103078161933936, -230.9224853114453140 ) ) ;
#27345 = CARTESIAN_POINT ( 'NONE',  ( 23.14999999999999858, 64.35000000001146248, -43.03791325517834565 ) ) ;
#27346 = DIRECTION ( 'NONE',  ( 0.000000000000000000, -0.2965989261549489275, -0.9550021345545417484 ) ) ;
#27347 = EDGE_CURVE ( 'NONE', #118647, #36019, #31264, .T. ) ;
#27348 = CARTESIAN_POINT ( 'NONE',  ( -18.50000000000000000, 9.122720154857367092, -245.4644708025848558 ) ) ;
#27349 = EDGE_LOOP ( 'NONE', ( #42808, #174363, #196948, #176358 ) ) ;
#27350 = ORIENTED_EDGE ( 'NONE', *, *, #253920, .F. ) ;
#27351 = CARTESIAN_POINT ( 'NONE',  ( 18.39999999999997371, 64.52683809665003878, -179.2731074845244450 ) ) ;
#27352 = ADVANCED_FACE ( 'NONE', ( #88808 ), #18743, .T. ) ;
#27353 = EDGE_CURVE ( 'NONE', #36405, #3656, #222739, .T. ) ;
#27354 = TOROIDAL_SURFACE ( 'NONE', #10744, 12.97499999999999787, 0.1000000000000000056 ) ;
#27355 = ORIENTED_EDGE ( 'NONE', *, *, #194644, .F. ) ;
#27356 = AXIS2_PLACEMENT_3D ( 'NONE', #119318, #58027, #94599 ) ;
#27357 = CARTESIAN_POINT ( 'NONE',  ( 20.04142135623730070, 15.92646454033040015, -219.3818586450342423 ) ) ;
#27358 = VERTEX_POINT ( 'NONE', #30167 ) ;
#27359 = DIRECTION ( 'NONE',  ( 1.000000000000000000, -0.000000000000000000, -0.000000000000000000 ) ) ;
#27360 = ADVANCED_FACE ( 'NONE', ( #10591 ), #214377, .F. ) ;
#27361 = CARTESIAN_POINT ( 'NONE',  ( 20.01093837587850288, 11.75000000000000711, -24.75439743459708808 ) ) ;
#27362 = DIRECTION ( 'NONE',  ( 0.000000000000000000, 0.000000000000000000, 1.000000000000000000 ) ) ;
#27363 = CARTESIAN_POINT ( 'NONE',  ( -21.05000000000000071, 1.627596811821301115, -230.7476853162787052 ) ) ;
#27364 = CARTESIAN_POINT ( 'NONE',  ( 21.05000000000000071, 10.72371711693665652, -179.6762396011382066 ) ) ;
#27365 = ORIENTED_EDGE ( 'NONE', *, *, #69037, .F. ) ;
#27366 = ADVANCED_FACE ( 'NONE', ( #169703 ), #93582, .T. ) ;
#27367 = CARTESIAN_POINT ( 'NONE',  ( 18.59999999999999076, 1.250000000011167511, -108.5000000000000426 ) ) ;
#27368 = CARTESIAN_POINT ( 'NONE',  ( -23.25000000000000000, 1.148907358139439339E-11, -201.0000000000015064 ) ) ;
#27369 = CARTESIAN_POINT ( 'NONE',  ( 18.54147908293623459, 85.46326165793961138, -62.47415858776833630 ) ) ;
#27370 = DIRECTION ( 'NONE',  ( 1.000000000000000000, 0.000000000000000000, 0.000000000000000000 ) ) ;
#27371 = VERTEX_POINT ( 'NONE', #153993 ) ;
#27372 = CIRCLE ( 'NONE', #214756, 0.09999999999999939493 ) ;
#27374 = LINE ( 'NONE', #106848, #119212 ) ;
#27373 = CARTESIAN_POINT ( 'NONE',  ( -20.64999999999999858, 74.00000000001180922, -82.74772940728641402 ) ) ;
#27375 = VERTEX_POINT ( 'NONE', #233502 ) ;
#27378 = VERTEX_POINT ( 'NONE', #56096 ) ;
#27377 = CARTESIAN_POINT ( 'NONE',  ( -17.29158576265543346, 10.36474766602906783, -55.58275824479218130 ) ) ;
#27376 = FACE_OUTER_BOUND ( 'NONE', #19341, .T. ) ;
#27379 = ORIENTED_EDGE ( 'NONE', *, *, #47782, .F. ) ;
#27380 = CARTESIAN_POINT ( 'NONE',  ( -21.64999999999999858, 7.250000000011148416, -54.75000000000000000 ) ) ;
#27381 = FACE_OUTER_BOUND ( 'NONE', #33335, .T. ) ;
#27382 = CARTESIAN_POINT ( 'NONE',  ( -20.54999999999999716, 6.759468328187065111, -212.0650163994647812 ) ) ;
#27383 = TOROIDAL_SURFACE ( 'NONE', #173130, 2.100000000000002309, 0.1000000000000000056 ) ;
#27384 = EDGE_LOOP ( 'NONE', ( #17414, #230155, #20218, #238816 ) ) ;
#27385 = CARTESIAN_POINT ( 'NONE',  ( -18.59999999999999787, 77.16412189325305349, -95.20825939895267709 ) ) ;
#27386 = DIRECTION ( 'NONE',  ( 0.000000000000000000, -0.9910465087640866200, -0.1335171055202867274 ) ) ;
#27388 = CARTESIAN_POINT ( 'NONE',  ( 18.49999999999999645, 8.006782298343173565, -209.8034900594678618 ) ) ;
#27387 = DIRECTION ( 'NONE',  ( 7.304098846218134667E-16, 1.000000000000000000, 6.982962677686267499E-15 ) ) ;
#27390 = ORIENTED_EDGE ( 'NONE', *, *, #207102, .T. ) ;
#27389 = CARTESIAN_POINT ( 'NONE',  ( 20.94999999999999574, 11.75000000001115552, -93.71613433702195550 ) ) ;
#27391 = ORIENTED_EDGE ( 'NONE', *, *, #141565, .F. ) ;
#27392 = CARTESIAN_POINT ( 'NONE',  ( -16.87435696428308063, 9.950002462943377424, -79.64999176516661805 ) ) ;
#27393 = CARTESIAN_POINT ( 'NONE',  ( 22.60000000000000142, -2.453693327374942612, -189.5089294449251724 ) ) ;
#27394 = VECTOR ( 'NONE', #179131, 1000.000000000000000 ) ;
#27395 = VECTOR ( 'NONE', #49982, 999.9999999999998863 ) ;
#27396 = DIRECTION ( 'NONE',  ( -1.000000000000000000, 3.265361837132813093E-16, 2.280189983783949500E-30 ) ) ;
#27397 = ORIENTED_EDGE ( 'NONE', *, *, #153653, .T. ) ;
#27398 = DIRECTION ( 'NONE',  ( 0.000000000000000000, 0.4166553800442402977, -0.9090645160164321226 ) ) ;
#27399 = DIRECTION ( 'NONE',  ( 0.000000000000000000, -1.000000000000000000, -6.982962677686266711E-15 ) ) ;
#27400 = DIRECTION ( 'NONE',  ( 0.000000000000000000, -1.000000000000000000, 6.308085367188393199E-16 ) ) ;
#27401 = ORIENTED_EDGE ( 'NONE', *, *, #57928, .F. ) ;
#27402 = EDGE_CURVE ( 'NONE', #36482, #165694, #239326, .T. ) ;
#27403 = EDGE_LOOP ( 'NONE', ( #121604, #251272, #180042, #43087, #13009 ) ) ;
#27404 = AXIS2_PLACEMENT_3D ( 'NONE', #112088, #31291, #168235 ) ;
#27405 = CARTESIAN_POINT ( 'NONE',  ( -18.59999999999999787, 5.950000000011100632, -77.30570230503489881 ) ) ;
#27407 = EDGE_CURVE ( 'NONE', #256678, #11922, #156153, .T. ) ;
#27406 = CARTESIAN_POINT ( 'NONE',  ( 22.39999999999999503, 1.115600667400684642E-11, -21.85042919245520210 ) ) ;
#27408 = AXIS2_PLACEMENT_3D ( 'NONE', #55813, #16742, #23169 ) ;
#27409 = AXIS2_PLACEMENT_3D ( 'NONE', #135269, #15361, #115727 ) ;
#27410 = CIRCLE ( 'NONE', #43933, 0.1000000000000028644 ) ;
#27411 = ORIENTED_EDGE ( 'NONE', *, *, #24067, .F. ) ;
#27412 = ORIENTED_EDGE ( 'NONE', *, *, #126195, .T. ) ;
#27413 =( BOUNDED_SURFACE ( )  B_SPLINE_SURFACE ( 3, 2, ( 
 ( #159072, #143325, #160363 ),
 ( #118661, #61228, #142041 ),
 ( #161640, #221558, #196881 ),
 ( #239879, #177362, #83324 ),
 ( #119954, #138176, #18254 ),
 ( #3822, #241165, #121248 ) ),
 .UNSPECIFIED., .F., .F., .F. ) 
 B_SPLINE_SURFACE_WITH_KNOTS ( ( 4, 2, 4 ),
 ( 3, 3 ),
 ( 3.141592653589793116, 3.926990816987241395, 4.712388980384689674 ),
 ( 0.000000000000000000, 1.000000000000000000 ),
 .UNSPECIFIED. ) 
 GEOMETRIC_REPRESENTATION_ITEM ( )  RATIONAL_B_SPLINE_SURFACE ( (
 ( 1.000000000000000000, 0.9238795325112820755, 1.000000000000000000),
 ( 1.000000000000000000, 0.9240297172239489987, 1.000000000000000000),
 ( 1.000000000000000000, 0.9038128468044698272, 1.000000000000000000),
 ( 1.000000000000000000, 0.8282379607644166919, 1.000000000000000000),
 ( 1.000000000000000000, 0.7727932973495217350, 1.000000000000000000),
 ( 1.000000000000000000, 0.7071067811865475727, 1.000000000000000000) ) ) 
 REPRESENTATION_ITEM ( '' )  SURFACE ( )  );
#27414 = EDGE_CURVE ( 'NONE', #146352, #247780, #6259, .T. ) ;
#27415 = DIRECTION ( 'NONE',  ( 0.000000000000000000, 0.000000000000000000, 1.000000000000000000 ) ) ;
#27416 = ORIENTED_EDGE ( 'NONE', *, *, #117741, .F. ) ;
#27419 = EDGE_CURVE ( 'NONE', #147468, #247369, #185347, .T. ) ;
#27418 = EDGE_LOOP ( 'NONE', ( #165407, #91739, #105985, #172968 ) ) ;
#27417 = DIRECTION ( 'NONE',  ( -2.827886303505248766E-16, 0.8660254037844411501, 0.4999999999999956146 ) ) ;
#27420 = VERTEX_POINT ( 'NONE', #195661 ) ;
#27422 = ORIENTED_EDGE ( 'NONE', *, *, #44279, .F. ) ;
#27421 = VERTEX_POINT ( 'NONE', #93959 ) ;
#27423 = CARTESIAN_POINT ( 'NONE',  ( -18.43459694179558639, -9.494210124986880217, -107.1170052026610051 ) ) ;
#27424 = ORIENTED_EDGE ( 'NONE', *, *, #150607, .T. ) ;
#27425 = DIRECTION ( 'NONE',  ( -1.000000000000000000, -0.000000000000000000, -0.000000000000000000 ) ) ;
#27426 = DIRECTION ( 'NONE',  ( 0.000000000000000000, 0.000000000000000000, 1.000000000000000000 ) ) ;
#27427 = AXIS2_PLACEMENT_3D ( 'NONE', #157282, #80244, #141534 ) ;
#27428 = DIRECTION ( 'NONE',  ( 0.000000000000000000, -1.000000000000000000, -6.352154140967427193E-15 ) ) ;
#27429 =( GEOMETRIC_REPRESENTATION_CONTEXT ( 3 ) GLOBAL_UNCERTAINTY_ASSIGNED_CONTEXT ( ( #8685 ) ) GLOBAL_UNIT_ASSIGNED_CONTEXT ( ( #87038, #169206, #213418 ) ) REPRESENTATION_CONTEXT ( 'NONE', 'WORKASPACE' ) );
#27430 = EDGE_CURVE ( 'NONE', #79169, #19155, #126906, .T. ) ;
#27431 = CARTESIAN_POINT ( 'NONE',  ( -18.41809261886929150, 87.08727407717567814, -199.6327535754520852 ) ) ;
#27433 = ADVANCED_FACE ( 'NONE', ( #92677 ), #194379, .T. ) ;
#27432 = CIRCLE ( 'NONE', #39883, 0.09999999999998898659 ) ;
#27434 = ORIENTED_EDGE ( 'NONE', *, *, #34328, .T. ) ;
#27435 = ORIENTED_EDGE ( 'NONE', *, *, #215196, .F. ) ;
#27436 = CARTESIAN_POINT ( 'NONE',  ( -21.55000000000000071, 68.85000000001151932, -48.27310748452437394 ) ) ;
#27438 = ORIENTED_EDGE ( 'NONE', *, *, #223980, .T. ) ;
#27437 = CARTESIAN_POINT ( 'NONE',  ( -16.93826681692523195, 65.98857127972483738, -182.5776490171649868 ) ) ;
#27440 = DIRECTION ( 'NONE',  ( -1.000000000000000000, -0.000000000000000000, -0.000000000000000000 ) ) ;
#27439 = AXIS2_PLACEMENT_3D ( 'NONE', #66732, #48433, #246633 ) ;
#27442 = ORIENTED_EDGE ( 'NONE', *, *, #69375, .F. ) ;
#27441 = DIRECTION ( 'NONE',  ( 1.000000000000000000, 0.000000000000000000, 0.000000000000000000 ) ) ;
#27443 = ORIENTED_EDGE ( 'NONE', *, *, #133327, .T. ) ;
#27444 = DIRECTION ( 'NONE',  ( 0.000000000000000000, 0.000000000000000000, 1.000000000000000000 ) ) ;
#27445 = CIRCLE ( 'NONE', #156439, 0.09999999999999939493 ) ;
#27446 = AXIS2_PLACEMENT_3D ( 'NONE', #142429, #160750, #22511 ) ;
#27447 = VECTOR ( 'NONE', #146364, 1000.000000000000000 ) ;
#27448 = ORIENTED_EDGE ( 'NONE', *, *, #173474, .F. ) ;
#27449 = EDGE_CURVE ( 'NONE', #166959, #154073, #232221, .T. ) ;
#27450 = EDGE_LOOP ( 'NONE', ( #228195, #148069, #222139, #10069 ) ) ;
#27451 = CARTESIAN_POINT ( 'NONE',  ( -16.87036670365548474, 66.01058118071058800, -149.0435473672224020 ) ) ;
#27452 = EDGE_CURVE ( 'NONE', #219174, #200879, #133101, .T. ) ;
#27455 = ORIENTED_EDGE ( 'NONE', *, *, #160543, .F. ) ;
#27454 = VERTEX_POINT ( 'NONE', #193082 ) ;
#27453 = VECTOR ( 'NONE', #146351, 1000.000000000000000 ) ;
#27456 = ORIENTED_EDGE ( 'NONE', *, *, #188476, .F. ) ;
#27457 = CARTESIAN_POINT ( 'NONE',  ( -16.92989507731676824, 9.950000000011140600, -54.11749893061020344 ) ) ;
#27458 = VERTEX_POINT ( 'NONE', #95250 ) ;
#27459 = AXIS2_PLACEMENT_3D ( 'NONE', #108380, #72806, #245325 ) ;
#27460 = ORIENTED_EDGE ( 'NONE', *, *, #135985, .T. ) ;
#27461 = DIRECTION ( 'NONE',  ( 0.000000000000000000, 0.000000000000000000, -1.000000000000000000 ) ) ;
#27463 = ORIENTED_EDGE ( 'NONE', *, *, #110077, .F. ) ;
#27462 = DIRECTION ( 'NONE',  ( 0.000000000000000000, -6.467318590049456648E-15, 1.000000000000000000 ) ) ;
#27464 = CARTESIAN_POINT ( 'NONE',  ( 23.15000000000000213, -11.64999999999999147, -30.39999999999999858 ) ) ;
#27465 = CIRCLE ( 'NONE', #1880, 0.09999999999999799327 ) ;
#27466 = CIRCLE ( 'NONE', #10857, 0.09999999999999939493 ) ;
#27468 = CARTESIAN_POINT ( 'NONE',  ( 21.14999999999999858, 64.35000000001258513, -191.3731074845244393 ) ) ;
#27467 = CARTESIAN_POINT ( 'NONE',  ( -18.59999999999999787, 70.22659352830977753, -197.9852579278363578 ) ) ;
#27469 = ADVANCED_FACE ( 'NONE', ( #14459 ), #127318, .T. ) ;
#27470 = CARTESIAN_POINT ( 'NONE',  ( 18.49713797159830264, 85.44648232759176665, -196.4516493629133720 ) ) ;
#27471 = CARTESIAN_POINT ( 'NONE',  ( -23.25000000000000000, 1.115600667400684642E-11, -67.00000000000000000 ) ) ;
#27472 = EDGE_LOOP ( 'NONE', ( #146370, #115933, #79267, #220770 ) ) ;
#27473 = EDGE_CURVE ( 'NONE', #43445, #202942, #11230, .T. ) ;
#27474 = ORIENTED_EDGE ( 'NONE', *, *, #12227, .T. ) ;
#27475 = DIRECTION ( 'NONE',  ( 0.000000000000000000, -0.1350103645451945777, 0.9908441862701590219 ) ) ;
#27476 = CARTESIAN_POINT ( 'NONE',  ( -21.05000000000000071, 1.115600667400684642E-11, -189.1999999999999602 ) ) ;
#27478 = ADVANCED_FACE ( 'NONE', ( #191167 ), #170346, .T. ) ;
#27477 = EDGE_LOOP ( 'NONE', ( #95132, #244587, #150772, #49746 ) ) ;
#27479 = ADVANCED_FACE ( 'NONE', ( #89460 ), #51595, .F. ) ;
#27480 = DIRECTION ( 'NONE',  ( -1.000000000000000000, 1.207181226542539700E-16, -2.694675058168174199E-16 ) ) ;
#27481 = VERTEX_POINT ( 'NONE', #231562 ) ;
#27482 = VERTEX_POINT ( 'NONE', #69936 ) ;
#27483 = CARTESIAN_POINT ( 'NONE',  ( -20.95613430942426092, 64.25000000001263345, -196.6659448363049876 ) ) ;
#27484 = PLANE ( 'NONE',  #19655 ) ;
#27485 = ORIENTED_EDGE ( 'NONE', *, *, #30338, .T. ) ;
#27486 = DIRECTION ( 'NONE',  ( 0.000000000000000000, 0.9999631594459055250, 0.008583690987127922528 ) ) ;
#27487 = DIRECTION ( 'NONE',  ( 0.000000000000000000, 0.9654727137038715545, 0.2605042016806676242 ) ) ;
#27488 = EDGE_LOOP ( 'NONE', ( #7079, #70275, #88920, #135124 ) ) ;
#27489 = EDGE_CURVE ( 'NONE', #174398, #105079, #171615, .T. ) ;
#27490 = DIRECTION ( 'NONE',  ( 0.000000000000000000, -0.8814952561688476074, 0.4721928772777262417 ) ) ;
#27492 = LINE ( 'NONE', #224355, #24817 ) ;
#27491 = CYLINDRICAL_SURFACE ( 'NONE', #32255, 0.09999999999999609201 ) ;
#27493 = FACE_OUTER_BOUND ( 'NONE', #119415, .T. ) ;
#27494 = AXIS2_PLACEMENT_3D ( 'NONE', #40194, #218781, #235786 ) ;
#27495 = DIRECTION ( 'NONE',  ( 0.000000000000000000, -1.000000000000000000, 0.000000000000000000 ) ) ;
#27496 = DIRECTION ( 'NONE',  ( 0.000000000000000000, -0.9126074666063660468, -0.4088369013363524762 ) ) ;
#27497 = VECTOR ( 'NONE', #66820, 1000.000000000000000 ) ;
#27499 = ADVANCED_FACE ( 'NONE', ( #131162 ), #30814, .T. ) ;
#27498 = LINE ( 'NONE', #69172, #11953 ) ;
#27500 = CIRCLE ( 'NONE', #206514, 0.9750000000000036415 ) ;
#27501 = VECTOR ( 'NONE', #230037, 999.9999999999998863 ) ;
#27502 = VERTEX_POINT ( 'NONE', #227691 ) ;
#27503 = TOROIDAL_SURFACE ( 'NONE', #156666, 2.100000000000002309, 0.1000000000000000056 ) ;
#27505 = VERTEX_POINT ( 'NONE', #93321 ) ;
#27504 = VERTEX_POINT ( 'NONE', #112895 ) ;
#27506 = ORIENTED_EDGE ( 'NONE', *, *, #252656, .F. ) ;
#27508 = ADVANCED_FACE ( 'NONE', ( #172913 ), #252378, .T. ) ;
#27507 = CARTESIAN_POINT ( 'NONE',  ( -20.00857864376270001, 30.27561093622783517, -235.5248193094124645 ) ) ;
#27509 = DIRECTION ( 'NONE',  ( -1.000000000000000000, 1.875376730785737719E-16, 1.309568571767809260E-30 ) ) ;
#27510 = CIRCLE ( 'NONE', #198147, 0.09999999999999939493 ) ;
#27511 = DIRECTION ( 'NONE',  ( 0.000000000000000000, 0.000000000000000000, 1.000000000000000000 ) ) ;
#27512 = DIRECTION ( 'NONE',  ( 0.000000000000000000, -1.000000000000000000, 0.000000000000000000 ) ) ;
#27514 = ORIENTED_EDGE ( 'NONE', *, *, #195574, .T. ) ;
#27513 = TOROIDAL_SURFACE ( 'NONE', #168978, 0.2000000000000000111, 0.1000000000000000056 ) ;
#27515 = DIRECTION ( 'NONE',  ( 0.000000000000000000, -0.8660254037844411501, -0.4999999999999956146 ) ) ;
#27516 = DIRECTION ( 'NONE',  ( 0.000000000000000000, 1.000000000000000000, 7.272083257015735086E-15 ) ) ;
#27517 = DIRECTION ( 'NONE',  ( 0.000000000000000000, 1.000000000000000000, 0.000000000000000000 ) ) ;
#27518 = CARTESIAN_POINT ( 'NONE',  ( -18.50000000000000000, -1.162701749938009677, -8.099999999999999645 ) ) ;
#27519 = EDGE_LOOP ( 'NONE', ( #181750, #62776, #45661, #204647 ) ) ;
#27520 = DIRECTION ( 'NONE',  ( -1.000000000000000000, 0.000000000000000000, 0.000000000000000000 ) ) ;
#27521 = ORIENTED_EDGE ( 'NONE', *, *, #191749, .F. ) ;
#27522 = ORIENTED_EDGE ( 'NONE', *, *, #48838, .T. ) ;
#27523 = CARTESIAN_POINT ( 'NONE',  ( -18.34804628011471195, 64.52683809664951298, -93.77310748452438816 ) ) ;
#27524 = DIRECTION ( 'NONE',  ( 0.000000000000000000, -0.8814952561688430555, 0.4721928772777346239 ) ) ;
#27525 = AXIS2_PLACEMENT_3D ( 'NONE', #256637, #141876, #98871 ) ;
#27526 = CARTESIAN_POINT ( 'NONE',  ( -20.64999999999999858, -9.499999999988848032, -43.39396912265245021 ) ) ;
#27527 = DIRECTION ( 'NONE',  ( 0.000000000000000000, 0.000000000000000000, -1.000000000000000000 ) ) ;
#27528 = DIRECTION ( 'NONE',  ( -1.000000000000000000, -2.952720810173289112E-16, 0.000000000000000000 ) ) ;
#27529 = CARTESIAN_POINT ( 'NONE',  ( -21.05000000000000071, 6.299230910092280311, 0.09843750000031994962 ) ) ;
#27530 = EDGE_LOOP ( 'NONE', ( #119336, #179787, #255377 ) ) ;
#27531 = CARTESIAN_POINT ( 'NONE',  ( 23.24999999999999645, 1.148907358139439339E-11, -201.0000000000015064 ) ) ;
#27532 = DIRECTION ( 'NONE',  ( 0.000000000000000000, 0.000000000000000000, -1.000000000000000000 ) ) ;
#27534 = CARTESIAN_POINT ( 'NONE',  ( 23.24999999999999289, 64.25000000001227818, -157.8731074845244393 ) ) ;
#27533 = CARTESIAN_POINT ( 'NONE',  ( -18.59999999999999787, 63.24832102809784118, -245.4188802514362635 ) ) ;
#27535 = DIRECTION ( 'NONE',  ( -0.000000000000000000, -0.000000000000000000, 1.000000000000000000 ) ) ;
#27536 = DIRECTION ( 'NONE',  ( 0.000000000000000000, -1.000000000000000000, 0.000000000000000000 ) ) ;
#27537 = DIRECTION ( 'NONE',  ( 3.469446951953635015E-14, -0.000000000000000000, 1.000000000000000000 ) ) ;
#27538 = CARTESIAN_POINT ( 'NONE',  ( -21.05000000000000071, 1.115600667400684642E-11, -33.50000000000000000 ) ) ;
#27539 = AXIS2_PLACEMENT_3D ( 'NONE', #45120, #80363, #135544 ) ;
#27542 = ORIENTED_EDGE ( 'NONE', *, *, #237786, .F. ) ;
#27541 = TOROIDAL_SURFACE ( 'NONE', #173290, 1.900000000000002576, 0.1000000000000000056 ) ;
#27540 = CYLINDRICAL_SURFACE ( 'NONE', #194477, 0.09999999999999939493 ) ;
#27543 = CIRCLE ( 'NONE', #173292, 0.1000000000000000888 ) ;
#27544 = VECTOR ( 'NONE', #254183, 1000.000000000000114 ) ;
#27545 = EDGE_CURVE ( 'NONE', #67174, #59001, #215000, .T. ) ;
#27546 = CARTESIAN_POINT ( 'NONE',  ( 21.95218792049437795, 7.201507561257818324, -100.4009715602001194 ) ) ;
#27547 = EDGE_CURVE ( 'NONE', #218378, #11577, #248546, .T. ) ;
#27548 = EDGE_CURVE ( 'NONE', #201392, #101974, #226850, .T. ) ;
#27549 = CYLINDRICAL_SURFACE ( 'NONE', #237930, 0.09999999999999939493 ) ;
#27550 = VECTOR ( 'NONE', #64053, 1000.000000000000000 ) ;
#27551 = CARTESIAN_POINT ( 'NONE',  ( 14.11444803880197085, 9.457431528860068326, -148.9999169378996555 ) ) ;
#27552 = VECTOR ( 'NONE', #217646, 999.9999999999998863 ) ;
#27553 = ORIENTED_EDGE ( 'NONE', *, *, #154312, .F. ) ;
#27554 = CARTESIAN_POINT ( 'NONE',  ( -20.64999999999999858, -8.663551401858001100, -191.4758988819326646 ) ) ;
#27555 = CARTESIAN_POINT ( 'NONE',  ( -21.04999999999999716, -0.08574093702224511171, -94.08617371118702977 ) ) ;
#27556 = DIRECTION ( 'NONE',  ( 0.000000000000000000, 1.000000000000000000, 6.982962677686266711E-15 ) ) ;
#27557 = AXIS2_PLACEMENT_3D ( 'NONE', #125727, #245683, #26656 ) ;
#27558 = VERTEX_POINT ( 'NONE', #88155 ) ;
#27559 = CARTESIAN_POINT ( 'NONE',  ( -17.11825945287482753, 66.05000000001159322, -56.87310748452439668 ) ) ;
#27561 = ORIENTED_EDGE ( 'NONE', *, *, #72035, .F. ) ;
#27560 = DIRECTION ( 'NONE',  ( 1.000000000000000000, 0.000000000000000000, 0.000000000000000000 ) ) ;
#27563 = DIRECTION ( 'NONE',  ( -0.000000000000000000, 6.982962677686266711E-15, -1.000000000000000000 ) ) ;
#27562 = DIRECTION ( 'NONE',  ( 0.000000000000000000, 0.000000000000000000, -1.000000000000000000 ) ) ;
#27564 = EDGE_CURVE ( 'NONE', #11990, #219131, #235226, .T. ) ;
#27565 = DIRECTION ( 'NONE',  ( 0.000000000000000000, -1.000000000000000000, 5.551115123125768187E-14 ) ) ;
#27566 = VERTEX_POINT ( 'NONE', #52907 ) ;
#27567 = DIRECTION ( 'NONE',  ( 1.000000000000000000, -0.000000000000000000, -0.000000000000000000 ) ) ;
#27568 = CARTESIAN_POINT ( 'NONE',  ( 0.000000000000000000, 0.000000000000000000, 0.000000000000000000 ) ) ;
#27569 = CARTESIAN_POINT ( 'NONE',  ( -20.89878130938411616, 65.67252876774509218, -63.94570419949945261 ) ) ;
#27570 = CARTESIAN_POINT ( 'NONE',  ( -37.88850191057539973, -10.74999999999999289, -15.00000000000000000 ) ) ;
#27571 = CARTESIAN_POINT ( 'NONE',  ( 22.50000000000000000, 76.00000000001213607, -136.5231074845242745 ) ) ;
#27572 = ORIENTED_EDGE ( 'NONE', *, *, #24924, .F. ) ;
#27573 = CARTESIAN_POINT ( 'NONE',  ( -21.05000000000000071, 36.65892442174935439, -249.5511627012433848 ) ) ;
#27574 = DIRECTION ( 'NONE',  ( 1.020425574104004196E-15, 6.982962677686266711E-15, -1.000000000000000000 ) ) ;
#27575 = AXIS2_PLACEMENT_3D ( 'NONE', #68138, #171136, #130668 ) ;
#27576 = DIRECTION ( 'NONE',  ( 1.000000000000000000, 7.049440681616512959E-16, -1.911869773728117674E-16 ) ) ;
#27577 = DIRECTION ( 'NONE',  ( 0.000000000000000000, 0.000000000000000000, 1.000000000000000000 ) ) ;
#27578 = EDGE_CURVE ( 'NONE', #63488, #92976, #68637, .T. ) ;
#27579 = VERTEX_POINT ( 'NONE', #72499 ) ;
#27580 = ADVANCED_FACE ( 'NONE', ( #148159 ), #128607, .T. ) ;
#27581 = VERTEX_POINT ( 'NONE', #209414 ) ;
#27582 = CARTESIAN_POINT ( 'NONE',  ( 21.04116576186320486, 65.37533692126069695, -124.1945257158966029 ) ) ;
#27583 = DIRECTION ( 'NONE',  ( 1.000000000000000000, -0.000000000000000000, -0.000000000000000000 ) ) ;
#27584 = PLANE ( 'NONE',  #81770 ) ;
#27585 = CARTESIAN_POINT ( 'NONE',  ( 21.05000000000000071, 10.48459288120560551, -141.4567135705834460 ) ) ;
#27586 = CARTESIAN_POINT ( 'NONE',  ( -20.94999999999999929, 78.57896856393121254, -232.7977304333149675 ) ) ;
#27587 = EDGE_CURVE ( 'NONE', #171571, #43357, #71216, .T. ) ;
#27590 = DIRECTION ( 'NONE',  ( 0.000000000000000000, -1.000000000000000000, 0.000000000000000000 ) ) ;
#27589 = AXIS2_PLACEMENT_3D ( 'NONE', #220619, #121548, #199792 ) ;
#27588 = CARTESIAN_POINT ( 'NONE',  ( 18.39999999999997371, 11.75000000001113953, -176.7499999999999716 ) ) ;
#27591 = CARTESIAN_POINT ( 'NONE',  ( 21.05000000000000071, 4.136903274969363942, -245.4596299165286268 ) ) ;
#27592 = DIRECTION ( 'NONE',  ( -0.000000000000000000, -6.982962677686266711E-15, 1.000000000000000000 ) ) ;
#27593 = CARTESIAN_POINT ( 'NONE',  ( -21.05000000000000071, 1.681127862299736098, -208.7190549363676269 ) ) ;
#27594 = CARTESIAN_POINT ( 'NONE',  ( -21.14999999999999858, -0.09999999999999939493, 6.249999999999998224 ) ) ;
#27596 = ORIENTED_EDGE ( 'NONE', *, *, #248128, .F. ) ;
#27595 = CARTESIAN_POINT ( 'NONE',  ( 21.14999999999999858, 11.65000000001116298, -79.25000000000004263 ) ) ;
#27597 = DIRECTION ( 'NONE',  ( 0.000000000000000000, 0.000000000000000000, 1.000000000000000000 ) ) ;
#27598 = DIRECTION ( 'NONE',  ( -1.000000000000000000, 0.000000000000000000, 0.000000000000000000 ) ) ;
#27600 = DIRECTION ( 'NONE',  ( -0.000000000000000000, 6.982962677686266711E-15, -1.000000000000000000 ) ) ;
#27599 = DIRECTION ( 'NONE',  ( 0.000000000000000000, 0.9770955615653315052, 0.2128009952263603954 ) ) ;
#27601 = ORIENTED_EDGE ( 'NONE', *, *, #69175, .F. ) ;
#27602 = DIRECTION ( 'NONE',  ( 0.000000000000000000, 0.8660254037844377084, 0.5000000000000015543 ) ) ;
#27603 = CARTESIAN_POINT ( 'NONE',  ( 18.49999999999998934, 6.450000000000001066, -10.01702717044001822 ) ) ;
#27604 = DIRECTION ( 'NONE',  ( 1.000000000000000000, 0.000000000000000000, 0.000000000000000000 ) ) ;
#27605 = CARTESIAN_POINT ( 'NONE',  ( 22.10000000000000497, 6.223900101154157483, 12.09999999999999964 ) ) ;
#27606 = EDGE_LOOP ( 'NONE', ( #99406, #4538, #146482, #82487 ) ) ;
#27607 = EDGE_LOOP ( 'NONE', ( #216799, #158695, #100994, #182952, #132149, #101807 ) ) ;
#27608 = EDGE_CURVE ( 'NONE', #80096, #157474, #222929, .T. ) ;
#27609 = B_SPLINE_CURVE_WITH_KNOTS ( 'NONE', 3,
 ( #42514, #184593, #85458, #24264, #202872, #105014, #103747, #125896 ),
 .UNSPECIFIED., .F., .F.,
 ( 4, 2, 2, 4 ),
 ( 0.000000000000000000, 6.534141206311939467E-05, 0.0001306828241262387893, 0.0002613656482524399569 ),
 .UNSPECIFIED. ) ;
#27610 = CARTESIAN_POINT ( 'NONE',  ( -20.64999999999999858, 7.250000000011155521, -112.7500000000000284 ) ) ;
#27611 = ORIENTED_EDGE ( 'NONE', *, *, #136357, .F. ) ;
#27612 = DIRECTION ( 'NONE',  ( 0.000000000000000000, -7.056502275159894776E-15, 1.000000000000000000 ) ) ;
#27613 = VERTEX_POINT ( 'NONE', #137568 ) ;
#27614 = CARTESIAN_POINT ( 'NONE',  ( 21.05000000000000071, 11.65000000001116298, -126.9851942293460922 ) ) ;
#27615 = AXIS2_PLACEMENT_3D ( 'NONE', #111673, #66127, #145651 ) ;
#27616 = CARTESIAN_POINT ( 'NONE',  ( -18.79999999999999716, -8.250000000000005329, -7.800000000000000711 ) ) ;
#27617 = ADVANCED_FACE ( 'NONE', ( #76311 ), #157183, .T. ) ;
#27618 = LINE ( 'NONE', #204918, #30642 ) ;
#27620 = ORIENTED_EDGE ( 'NONE', *, *, #17880, .T. ) ;
#27619 = AXIS2_PLACEMENT_3D ( 'NONE', #220367, #121297, #177408 ) ;
#27621 = VECTOR ( 'NONE', #173281, 1000.000000000000000 ) ;
#27622 = ADVANCED_FACE ( 'NONE', ( #35940 ), #256182, .F. ) ;
#27624 = EDGE_CURVE ( 'NONE', #222419, #64966, #164682, .T. ) ;
#27623 = DIRECTION ( 'NONE',  ( 0.000000000000000000, 0.000000000000000000, 1.000000000000000000 ) ) ;
#27625 = AXIS2_PLACEMENT_3D ( 'NONE', #62700, #206056, #160538 ) ;
#27626 = CARTESIAN_POINT ( 'NONE',  ( -18.55121869061588669, 68.09900309800710261, -224.1499508721967686 ) ) ;
#27627 = FACE_OUTER_BOUND ( 'NONE', #79774, .T. ) ;
#27628 = CARTESIAN_POINT ( 'NONE',  ( -21.14999999999999858, 11.65000000001115588, -100.6000000000000369 ) ) ;
#27629 = PLANE ( 'NONE',  #62341 ) ;
#27630 = CARTESIAN_POINT ( 'NONE',  ( 21.04999999999908411, 11.16248219967772215, -211.0118371899025078 ) ) ;
#27631 = ORIENTED_EDGE ( 'NONE', *, *, #126451, .F. ) ;
#27633 = CYLINDRICAL_SURFACE ( 'NONE', #190890, 0.09999999999999939493 ) ;
#27632 = CARTESIAN_POINT ( 'NONE',  ( -16.97683809663753252, 66.05000000001207638, -123.2515827158544397 ) ) ;
#27634 = ORIENTED_EDGE ( 'NONE', *, *, #182122, .T. ) ;
#27636 = ORIENTED_EDGE ( 'NONE', *, *, #89843, .T. ) ;
#27635 = DIRECTION ( 'NONE',  ( 0.000000000000000000, 0.2128009952263604232, -0.9770955615653316162 ) ) ;
#27637 = EDGE_CURVE ( 'NONE', #139796, #161077, #172916, .T. ) ;
#27638 = CIRCLE ( 'NONE', #156804, 0.1000000000000032391 ) ;
#27639 = ORIENTED_EDGE ( 'NONE', *, *, #196171, .T. ) ;
#27640 = DIRECTION ( 'NONE',  ( -1.073024830501117725E-15, 0.000000000000000000, 1.000000000000000000 ) ) ;
#27641 = EDGE_CURVE ( 'NONE', #198456, #168941, #135441, .T. ) ;
#27642 = DIRECTION ( 'NONE',  ( 1.000000000000000000, -0.000000000000000000, -0.000000000000000000 ) ) ;
#27643 = VECTOR ( 'NONE', #49043, 1000.000000000000000 ) ;
#27644 = DIRECTION ( 'NONE',  ( 0.000000000000000000, -7.086529944415886769E-15, 1.000000000000000000 ) ) ;
#27645 = CARTESIAN_POINT ( 'NONE',  ( -20.94999999999999929, -11.39257802169451317, -164.4260504201680817 ) ) ;
#27646 = EDGE_LOOP ( 'NONE', ( #200927, #230556, #131223, #121887 ) ) ;
#27647 = LINE ( 'NONE', #151424, #97304 ) ;
#27649 = ADVANCED_FACE ( 'NONE', ( #257474 ), #99983, .T. ) ;
#27648 = FACE_OUTER_BOUND ( 'NONE', #116905, .T. ) ;
#27650 = EDGE_LOOP ( 'NONE', ( #246902, #198179, #197361, #222431 ) ) ;
#27651 = LINE ( 'NONE', #147558, #35710 ) ;
#27652 = ADVANCED_FACE ( 'NONE', ( #73794 ), #75081, .F. ) ;
#27653 = VECTOR ( 'NONE', #18412, 999.9999999999998863 ) ;
#27654 = VERTEX_POINT ( 'NONE', #253667 ) ;
#27655 = PLANE ( 'NONE',  #14552 ) ;
#27656 = EDGE_CURVE ( 'NONE', #79888, #42512, #160435, .T. ) ;
#27657 = EDGE_CURVE ( 'NONE', #22313, #53558, #196275, .T. ) ;
#27658 = ORIENTED_EDGE ( 'NONE', *, *, #245555, .F. ) ;
#27659 = CARTESIAN_POINT ( 'NONE',  ( -17.29158576265543346, 65.63525233399431613, -147.9403492397322566 ) ) ;
#27660 = EDGE_LOOP ( 'NONE', ( #57433, #72036, #117493, #74443 ) ) ;
#27661 = CARTESIAN_POINT ( 'NONE',  ( 18.59999999999999076, 7.788796164756791818, -245.4641525896719543 ) ) ;
#27662 = ADVANCED_FACE ( 'NONE', ( #254904 ), #118913, .T. ) ;
#27663 = DIRECTION ( 'NONE',  ( 0.000000000000000000, 0.000000000000000000, -1.000000000000000000 ) ) ;
#27665 = CARTESIAN_POINT ( 'NONE',  ( -20.64999999999999858, 7.250000000011155521, -179.8499999999999943 ) ) ;
#27664 =( REPRESENTATION_RELATIONSHIP ('NONE','NONE', #36900, #88607 ) REPRESENTATION_RELATIONSHIP_WITH_TRANSFORMATION ( #173204 )SHAPE_REPRESENTATION_RELATIONSHIP( ) );
#27666 = CARTESIAN_POINT ( 'NONE',  ( -18.59999999999999787, -1.851617760468904805, -45.10318971960366241 ) ) ;
#27667 = EDGE_CURVE ( 'NONE', #207366, #2694, #44921, .T. ) ;
#27668 = CIRCLE ( 'NONE', #11050, 11.80000000000000782 ) ;
#27669 = ADVANCED_FACE ( 'NONE', ( #162309 ), #43637, .F. ) ;
#27670 = CIRCLE ( 'NONE', #69336, 0.9000000000000014655 ) ;
#27671 = VECTOR ( 'NONE', #50516, 1000.000000000000000 ) ;
#27672 = AXIS2_PLACEMENT_3D ( 'NONE', #172682, #73565, #14865 ) ;
#27673 = ADVANCED_FACE ( 'NONE', ( #80142 ), #139721, .F. ) ;
#27674 = CYLINDRICAL_SURFACE ( 'NONE', #48891, 4.049999999999997158 ) ;
#27675 = LINE ( 'NONE', #186722, #109907 ) ;
#27676 = CARTESIAN_POINT ( 'NONE',  ( 20.89878130938411616, 10.32747123227773045, -72.57740328502492844 ) ) ;
#27677 = ORIENTED_EDGE ( 'NONE', *, *, #73671, .F. ) ;
#27679 = CARTESIAN_POINT ( 'NONE',  ( -5.900000000000003020, -11.75000000000000000, 9.900000000000002132 ) ) ;
#27678 = DIRECTION ( 'NONE',  ( 1.836970198721029934E-16, -1.000000000000000000, -0.000000000000000000 ) ) ;
#27680 = AXIS2_PLACEMENT_3D ( 'NONE', #35455, #229763, #51092 ) ;
#27681 = ORIENTED_EDGE ( 'NONE', *, *, #156495, .F. ) ;
#27682 = CARTESIAN_POINT ( 'NONE',  ( -18.59999999999999787, 77.73625713160926409, -91.45445515550680682 ) ) ;
#27683 = LINE ( 'NONE', #169760, #185902 ) ;
#27684 = DIRECTION ( 'NONE',  ( -1.000000000000000000, -0.000000000000000000, -0.000000000000000000 ) ) ;
#27686 = ORIENTED_EDGE ( 'NONE', *, *, #145628, .T. ) ;
#27685 = DIRECTION ( 'NONE',  ( 0.000000000000000000, 6.982962677686266711E-15, -1.000000000000000000 ) ) ;
#27688 = VERTEX_POINT ( 'NONE', #3195 ) ;
#27687 = CARTESIAN_POINT ( 'NONE',  ( 18.79999999999999716, -1.410778198689825347, -7.973296578895943121 ) ) ;
#27689 = EDGE_CURVE ( 'NONE', #49789, #9341, #184415, .T. ) ;
#27691 = CARTESIAN_POINT ( 'NONE',  ( -18.59999999999999787, 68.92903212821327941, -132.7765432626560766 ) ) ;
#27690 = VECTOR ( 'NONE', #244559, 1000.000000000000000 ) ;
#27692 = CARTESIAN_POINT ( 'NONE',  ( 19.88284271247461987, 64.30857864377489364, -145.2731074845244450 ) ) ;
#27693 = CIRCLE ( 'NONE', #81766, 0.1000000000000012546 ) ;
#27695 = EDGE_LOOP ( 'NONE', ( #208267, #173950, #25281, #252559 ) ) ;
#27694 = DIRECTION ( 'NONE',  ( 0.7071067811865463515, 0.7071067811865487940, 7.587431340288849180E-16 ) ) ;
#27696 = TOROIDAL_SURFACE ( 'NONE', #31783, 0.2000000000000000111, 0.1000000000000000056 ) ;
#27697 = CARTESIAN_POINT ( 'NONE',  ( -23.25000000000000000, 1.999999999999998224, -20.27537807723789953 ) ) ;
#27698 = DIRECTION ( 'NONE',  ( -3.265361837132813093E-16, -0.4088369013363283844, 0.9126074666063769270 ) ) ;
#27699 = ORIENTED_EDGE ( 'NONE', *, *, #127928, .T. ) ;
#27700 = CARTESIAN_POINT ( 'NONE',  ( 22.39999999999999858, 7.790779598384538929, -167.3999999999999773 ) ) ;
#27701 = ORIENTED_EDGE ( 'NONE', *, *, #237427, .T. ) ;
#27702 = AXIS2_PLACEMENT_3D ( 'NONE', #223661, #26794, #65890 ) ;
#27703 = DIRECTION ( 'NONE',  ( -1.000000000000000000, -0.000000000000000000, -0.000000000000000000 ) ) ;
#27704 = CYLINDRICAL_SURFACE ( 'NONE', #193235, 11.75000000000001066 ) ;
#27705 = ORIENTED_EDGE ( 'NONE', *, *, #86441, .F. ) ;
#27706 = DIRECTION ( 'NONE',  ( 0.000000000000000000, -0.9126074666063769270, -0.4088369013363280513 ) ) ;
#27707 = CARTESIAN_POINT ( 'NONE',  ( 22.10000000000000497, 6.223900101154156594, 12.09999999999999964 ) ) ;
#27708 = EDGE_CURVE ( 'NONE', #15679, #99499, #122997, .T. ) ;
#27709 = ORIENTED_EDGE ( 'NONE', *, *, #254894, .F. ) ;
#27710 = AXIS2_PLACEMENT_3D ( 'NONE', #164767, #107346, #169947 ) ;
#27712 = EDGE_CURVE ( 'NONE', #95067, #22968, #93753, .T. ) ;
#27711 = LINE ( 'NONE', #9381, #239474 ) ;
#27713 = AXIS2_PLACEMENT_3D ( 'NONE', #96543, #176132, #97819 ) ;
#27714 = CIRCLE ( 'NONE', #173492, 0.09999999999999939493 ) ;
#27715 = ORIENTED_EDGE ( 'NONE', *, *, #133541, .F. ) ;
#27716 = ORIENTED_EDGE ( 'NONE', *, *, #230025, .F. ) ;
#27717 = CARTESIAN_POINT ( 'NONE',  ( -21.04999999999965610, 61.13727535989644224, -234.2557234744361381 ) ) ;
#27718 = ORIENTED_EDGE ( 'NONE', *, *, #88445, .T. ) ;
#27719 = CYLINDRICAL_SURFACE ( 'NONE', #217079, 0.1000000000000057648 ) ;
#27720 = ORIENTED_EDGE ( 'NONE', *, *, #46548, .F. ) ;
#27722 = ORIENTED_EDGE ( 'NONE', *, *, #27334, .T. ) ;
#27721 = CARTESIAN_POINT ( 'NONE',  ( 21.14999999999999858, 6.550000000011156231, -179.8499999999999943 ) ) ;
#27723 = DIRECTION ( 'NONE',  ( -0.000000000000000000, 0.9126074666063771490, 0.4088369013363281623 ) ) ;
#27724 = VERTEX_POINT ( 'NONE', #106150 ) ;
#27725 = DIRECTION ( 'NONE',  ( 0.000000000000000000, -0.9126074666063765939, -0.4088369013363289950 ) ) ;
#27726 = EDGE_LOOP ( 'NONE', ( #69366, #121983, #66609, #178975 ) ) ;
#27729 = ORIENTED_EDGE ( 'NONE', *, *, #227876, .F. ) ;
#27728 = VERTEX_POINT ( 'NONE', #60605 ) ;
#27727 = DIRECTION ( 'NONE',  ( 1.000000000000000000, 0.000000000000000000, -0.000000000000000000 ) ) ;
#27730 = FACE_OUTER_BOUND ( 'NONE', #55761, .T. ) ;
#27731 = CIRCLE ( 'NONE', #244343, 11.70000000000000462 ) ;
#27732 = EDGE_CURVE ( 'NONE', #7443, #210483, #243789, .T. ) ;
#27733 = CARTESIAN_POINT ( 'NONE',  ( -18.50000000000000000, 6.846123162363745074, -104.2377262668499043 ) ) ;
#27734 = VECTOR ( 'NONE', #235943, 1000.000000000000000 ) ;
#27735 = CIRCLE ( 'NONE', #6845, 0.09999999999998898659 ) ;
#27736 = EDGE_LOOP ( 'NONE', ( #136155, #214590, #116737, #44758, #255640, #2099, #104867 ) ) ;
#27737 = VECTOR ( 'NONE', #167797, 1000.000000000000000 ) ;
#27738 = EDGE_LOOP ( 'NONE', ( #198966, #54479, #162243, #203953, #41886, #92477, #143610, #111856, #252632, #23414, #107548, #161082 ) ) ;
#27739 = CARTESIAN_POINT ( 'NONE',  ( -21.05000000000000071, 69.58633726514349860, -203.4375146211625065 ) ) ;
#27740 = CARTESIAN_POINT ( 'NONE',  ( -21.05000000000000071, -1.261786168553869603, -175.5864989635454378 ) ) ;
#27742 = ORIENTED_EDGE ( 'NONE', *, *, #256767, .T. ) ;
#27741 = DIRECTION ( 'NONE',  ( 0.000000000000000000, 1.000000000000000000, 0.000000000000000000 ) ) ;
#27743 = EDGE_LOOP ( 'NONE', ( #45441, #134007 ) ) ;
#27744 = DIRECTION ( 'NONE',  ( -1.000000000000000000, -0.000000000000000000, 0.000000000000000000 ) ) ;
#27745 = CARTESIAN_POINT ( 'NONE',  ( 18.49999999999999289, 65.58283456529555622, -111.6731074851050494 ) ) ;
#27746 = EDGE_LOOP ( 'NONE', ( #107474, #52917, #82773, #107776 ) ) ;
#27747 = PLANE ( 'NONE',  #144684 ) ;
#27748 = DIRECTION ( 'NONE',  ( -0.000000000000000000, 0.6922311945860613047, 0.7216758089626910122 ) ) ;
#27749 = ORIENTED_EDGE ( 'NONE', *, *, #120353, .F. ) ;
#27750 = CARTESIAN_POINT ( 'NONE',  ( 20.04142135623731136, 54.35086488289006468, -228.7501953506800589 ) ) ;
#27751 = CIRCLE ( 'NONE', #173522, 0.5000000000000004441 ) ;
#27753 = ORIENTED_EDGE ( 'NONE', *, *, #15485, .T. ) ;
#27752 = ORIENTED_EDGE ( 'NONE', *, *, #131464, .T. ) ;
#27754 = ORIENTED_EDGE ( 'NONE', *, *, #22877, .F. ) ;
#27755 = CARTESIAN_POINT ( 'NONE',  ( -21.05000000000000426, -0.09999999998884341601, -127.5229329788753176 ) ) ;
#27756 = ORIENTED_EDGE ( 'NONE', *, *, #23308, .F. ) ;
#27757 = CARTESIAN_POINT ( 'NONE',  ( -23.15000000000000213, 69.25640205380744874, -247.7135141964517402 ) ) ;
#27758 = ORIENTED_EDGE ( 'NONE', *, *, #247855, .F. ) ;
#27759 = CARTESIAN_POINT ( 'NONE',  ( -20.54999999999999716, 68.85000000001183196, -86.27310748452435973 ) ) ;
#27760 = PLANE ( 'NONE',  #2376 ) ;
#27761 = ADVANCED_FACE ( 'NONE', ( #85292 ), #193722, .F. ) ;
#27762 = ORIENTED_EDGE ( 'NONE', *, *, #7434, .F. ) ;
#27763 = EDGE_CURVE ( 'NONE', #103956, #170251, #140137, .T. ) ;
#27764 = ORIENTED_EDGE ( 'NONE', *, *, #9405, .F. ) ;
#27765 = VECTOR ( 'NONE', #3829, 999.9999999999998863 ) ;
#27766 = ORIENTED_EDGE ( 'NONE', *, *, #187125, .T. ) ;
#27767 = CIRCLE ( 'NONE', #131783, 0.09999999999999939493 ) ;
#27768 = AXIS2_PLACEMENT_3D ( 'NONE', #211835, #98250, #73627 ) ;
#27769 = EDGE_CURVE ( 'NONE', #125280, #53558, #210474, .T. ) ;
#27770 = CYLINDRICAL_SURFACE ( 'NONE', #43122, 0.09999999999998898659 ) ;
#27771 = ORIENTED_EDGE ( 'NONE', *, *, #253489, .T. ) ;
#27772 = DIRECTION ( 'NONE',  ( 1.000000000000000000, 0.000000000000000000, 0.000000000000000000 ) ) ;
#27775 = EDGE_CURVE ( 'NONE', #5506, #219593, #168819, .T. ) ;
#27774 = ORIENTED_EDGE ( 'NONE', *, *, #15092, .F. ) ;
#27773 = CARTESIAN_POINT ( 'NONE',  ( -22.39999999999999858, 68.20922040163897293, -170.0231074845243882 ) ) ;
#27776 = CARTESIAN_POINT ( 'NONE',  ( 19.88284271247461987, 64.30857864377520627, -178.7731074845244450 ) ) ;
#27777 = CARTESIAN_POINT ( 'NONE',  ( -22.47071067811865319, 10.68684811775433374, -226.8807012965928038 ) ) ;
#27778 = DIRECTION ( 'NONE',  ( 0.000000000000000000, 0.000000000000000000, 1.000000000000000000 ) ) ;
#27779 = DIRECTION ( 'NONE',  ( -4.408576920032446739E-17, 0.9371753822965314118, -0.3488585713686133682 ) ) ;
#27780 = CARTESIAN_POINT ( 'NONE',  ( -20.64999999999999858, 1.115600667400684642E-11, -167.4999999999999716 ) ) ;
#27782 = DIRECTION ( 'NONE',  ( -1.000000000000000000, 1.836970198721029934E-16, 1.282749433769087582E-30 ) ) ;
#27781 = CARTESIAN_POINT ( 'NONE',  ( -23.25000000000000000, 2.000000000011154189, -154.8753780772379116 ) ) ;
#27783 = LINE ( 'NONE', #44754, #232378 ) ;
#27784 = CARTESIAN_POINT ( 'NONE',  ( 22.50927854361892955, 76.10085807354020915, -181.7726746105512348 ) ) ;
#27785 = ADVANCED_FACE ( 'NONE', ( #63177 ), #131354, .T. ) ;
#27786 = LINE ( 'NONE', #249383, #68062 ) ;
#27787 = AXIS2_PLACEMENT_3D ( 'NONE', #107373, #232491, #49970 ) ;
#27788 = ORIENTED_EDGE ( 'NONE', *, *, #72898, .T. ) ;
#27789 = AXIS2_PLACEMENT_3D ( 'NONE', #231336, #136036, #52664 ) ;
#27790 = AXIS2_PLACEMENT_3D ( 'NONE', #186064, #226441, #244730 ) ;
#27792 = ORIENTED_EDGE ( 'NONE', *, *, #138511, .F. ) ;
#27791 = CIRCLE ( 'NONE', #65737, 0.09999999999998898659 ) ;
#27794 = ORIENTED_EDGE ( 'NONE', *, *, #69215, .T. ) ;
#27793 = CARTESIAN_POINT ( 'NONE',  ( -20.94999999999999929, 44.29184115892635987, -259.0069060397277667 ) ) ;
#27795 = CIRCLE ( 'NONE', #98434, 0.1000000000000054040 ) ;
#27796 = ORIENTED_EDGE ( 'NONE', *, *, #14360, .T. ) ;
#27798 = ADVANCED_FACE ( 'NONE', ( #4487 ), #240548, .F. ) ;
#27797 = LINE ( 'NONE', #146397, #91083 ) ;
#27799 = CARTESIAN_POINT ( 'NONE',  ( 20.12518398540832365, 9.975088720679844201, -141.9966682524667760 ) ) ;
#27800 = AXIS2_PLACEMENT_3D ( 'NONE', #167500, #87907, #84029 ) ;
#27801 = TOROIDAL_SURFACE ( 'NONE', #123448, 0.2000000000000000111, 0.1000000000000000056 ) ;
#27803 = DIRECTION ( 'NONE',  ( 0.000000000000000000, 6.982962677686266711E-15, -1.000000000000000000 ) ) ;
#27802 = CARTESIAN_POINT ( 'NONE',  ( 19.97071067811864609, 64.27928932189385591, -178.7731074845244450 ) ) ;
#27804 = ORIENTED_EDGE ( 'NONE', *, *, #222690, .F. ) ;
#27805 = CARTESIAN_POINT ( 'NONE',  ( 18.48536876927986583, -9.463527249856113599, -40.54861826508263789 ) ) ;
#27806 = LINE ( 'NONE', #105995, #236927 ) ;
#27807 = ORIENTED_EDGE ( 'NONE', *, *, #119560, .F. ) ;
#27809 = DIRECTION ( 'NONE',  ( 0.000000000000000000, 0.000000000000000000, 1.000000000000000000 ) ) ;
#27808 = VECTOR ( 'NONE', #105968, 1000.000000000000000 ) ;
#27810 = CARTESIAN_POINT ( 'NONE',  ( -16.85312841634287651, 9.913606177331363511, -180.3971731332925970 ) ) ;
#27811 = CARTESIAN_POINT ( 'NONE',  ( 20.94999999999999929, 76.00000000001267608, -203.5231074845243597 ) ) ;
#27812 = CARTESIAN_POINT ( 'NONE',  ( 21.05000000000000071, 65.37127968600724159, -61.85819391543678591 ) ) ;
#27813 = CIRCLE ( 'NONE', #240176, 4.900000000000004796 ) ;
#27814 = LINE ( 'NONE', #229829, #99681 ) ;
#27816 = ORIENTED_EDGE ( 'NONE', *, *, #116831, .F. ) ;
#27815 = DIRECTION ( 'NONE',  ( 1.000000000000000000, 0.000000000000000000, 0.000000000000000000 ) ) ;
#27817 = FACE_OUTER_BOUND ( 'NONE', #113040, .T. ) ;
#27818 = DIRECTION ( 'NONE',  ( 0.000000000000000000, -0.2965989261549410450, -0.9550021345545443019 ) ) ;
#27819 = FACE_OUTER_BOUND ( 'NONE', #237072, .T. ) ;
#27820 = CARTESIAN_POINT ( 'NONE',  ( -18.59999999999999787, 7.021664781911246322, -104.2335654018973372 ) ) ;
#27821 = ORIENTED_EDGE ( 'NONE', *, *, #128235, .T. ) ;
#27822 = LINE ( 'NONE', #201280, #94952 ) ;
#27823 = DIRECTION ( 'NONE',  ( -2.915501640297153790E-16, 1.000000000000000000, 0.000000000000000000 ) ) ;
#27825 = DIRECTION ( 'NONE',  ( 1.000000000000000000, 0.000000000000000000, 0.000000000000000000 ) ) ;
#27824 = CARTESIAN_POINT ( 'NONE',  ( 20.95512820512820440, 65.37615131630045084, -162.3581939154368285 ) ) ;
#27826 = CARTESIAN_POINT ( 'NONE',  ( 18.59999999999999787, -1.736705739456431807, -212.5174225876236846 ) ) ;
#27827 = LINE ( 'NONE', #162191, #249129 ) ;
#27828 = AXIS2_PLACEMENT_3D ( 'NONE', #22945, #102417, #185840 ) ;
#27829 = DIRECTION ( 'NONE',  ( 0.000000000000000000, 0.000000000000000000, -1.000000000000000000 ) ) ;
#27830 = CARTESIAN_POINT ( 'NONE',  ( 18.79999999999999716, 4.611773100472912112, 22.11686199900910665 ) ) ;
#27831 = CARTESIAN_POINT ( 'NONE',  ( 18.49999999999999645, 19.02280865327213277, -233.3540837620168986 ) ) ;
#27832 = CARTESIAN_POINT ( 'NONE',  ( -16.80939487329394666, 9.950000000011138823, -87.85000000000093223 ) ) ;
#27833 = EDGE_LOOP ( 'NONE', ( #48482, #143697, #230816, #233926 ) ) ;
#27834 = EDGE_CURVE ( 'NONE', #4561, #199335, #2162, .T. ) ;
#27835 = ORIENTED_EDGE ( 'NONE', *, *, #155743, .T. ) ;
#27836 = ORIENTED_EDGE ( 'NONE', *, *, #224172, .T. ) ;
#27837 = CARTESIAN_POINT ( 'NONE',  ( 20.44999100639871514, 65.56028929680009298, -95.26403175855385541 ) ) ;
#27838 = PLANE ( 'NONE',  #94404 ) ;
#27839 = ORIENTED_EDGE ( 'NONE', *, *, #234520, .F. ) ;
#27840 = EDGE_CURVE ( 'NONE', #74814, #201537, #142710, .T. ) ;
#27841 = AXIS2_PLACEMENT_3D ( 'NONE', #50111, #147943, #248320 ) ;
#27842 = AXIS2_PLACEMENT_3D ( 'NONE', #104937, #241909, #2005 ) ;
#27843 = ORIENTED_EDGE ( 'NONE', *, *, #61571, .T. ) ;
#27844 = EDGE_CURVE ( 'NONE', #136330, #116019, #197983, .T. ) ;
#27846 = EDGE_CURVE ( 'NONE', #160646, #166855, #152239, .T. ) ;
#27845 = AXIS2_PLACEMENT_3D ( 'NONE', #38076, #97999, #134563 ) ;
#27847 = AXIS2_PLACEMENT_3D ( 'NONE', #162077, #159506, #43394 ) ;
#27848 = ORIENTED_EDGE ( 'NONE', *, *, #148829, .F. ) ;
#27849 = FACE_OUTER_BOUND ( 'NONE', #100418, .T. ) ;
#27850 = VERTEX_POINT ( 'NONE', #132154 ) ;
#27851 = CIRCLE ( 'NONE', #86237, 0.1000000000000028644 ) ;
#27852 = CARTESIAN_POINT ( 'NONE',  ( 18.49999999999999645, 18.37021030142088662, -237.6367305148568221 ) ) ;
#27853 = DIRECTION ( 'NONE',  ( -0.8660254037843878594, 0.000000000000000000, 0.5000000000000880407 ) ) ;
#27854 = DIRECTION ( 'NONE',  ( -1.000000000000000000, -0.000000000000000000, -0.000000000000000000 ) ) ;
#27855 = DIRECTION ( 'NONE',  ( 0.000000000000000000, -1.000000000000000000, 0.000000000000000000 ) ) ;
#27856 = CARTESIAN_POINT ( 'NONE',  ( 18.59999999999999432, 5.699452464332755319, -121.4577260434301991 ) ) ;
#27857 = DIRECTION ( 'NONE',  ( -1.000000000000000000, -0.000000000000000000, -0.000000000000000000 ) ) ;
#27858 = ORIENTED_EDGE ( 'NONE', *, *, #205053, .T. ) ;
#27860 = DIRECTION ( 'NONE',  ( -0.000000000000000000, 0.000000000000000000, 1.000000000000000000 ) ) ;
#27859 = DIRECTION ( 'NONE',  ( 0.000000000000000000, -6.982962677686266711E-15, 1.000000000000000000 ) ) ;
#27861 = EDGE_CURVE ( 'NONE', #12448, #241925, #231332, .T. ) ;
#27862 = CARTESIAN_POINT ( 'NONE',  ( 21.05000000000000071, -11.48912529306489994, -197.8999999999999773 ) ) ;
#27863 = VECTOR ( 'NONE', #207728, 1000.000000000000114 ) ;
#27864 = ORIENTED_EDGE ( 'NONE', *, *, #7300, .F. ) ;
#27865 = DIRECTION ( 'NONE',  ( -1.646408749285562691E-14, 1.000000000000000000, 0.000000000000000000 ) ) ;
#27866 = CARTESIAN_POINT ( 'NONE',  ( -15.06774609480955363, 9.417651958852159666, -115.8587873924405045 ) ) ;
#27868 = EDGE_CURVE ( 'NONE', #156671, #241011, #27162, .T. ) ;
#27867 = DIRECTION ( 'NONE',  ( 0.000000000000000000, -1.000000000000000000, 0.000000000000000000 ) ) ;
#27870 = ORIENTED_EDGE ( 'NONE', *, *, #72921, .F. ) ;
#27869 = VECTOR ( 'NONE', #242297, 1000.000000000000000 ) ;
#27871 = CARTESIAN_POINT ( 'NONE',  ( -22.39999999999999858, 0.1000000000111554016, -126.2092204016266379 ) ) ;
#27872 = CARTESIAN_POINT ( 'NONE',  ( -16.83233564386400971, 66.06977820342729046, -82.29858682104901391 ) ) ;
#27873 = ORIENTED_EDGE ( 'NONE', *, *, #90242, .T. ) ;
#27874 = B_SPLINE_CURVE_WITH_KNOTS ( 'NONE', 3,
 ( #256306, #17745, #236803, #244182, #141253, #136395 ),
 .UNSPECIFIED., .F., .F.,
 ( 4, 2, 4 ),
 ( 0.000000000000000000, 0.0001569047307838634909, 0.0003138094615677269818 ),
 .UNSPECIFIED. ) ;
#27875 = LINE ( 'NONE', #31728, #117785 ) ;
#27876 = CARTESIAN_POINT ( 'NONE',  ( -20.54999999999999716, 74.00000000001151079, -49.24772940728643533 ) ) ;
#27877 = EDGE_CURVE ( 'NONE', #189461, #88741, #256184, .T. ) ;
#27878 = CARTESIAN_POINT ( 'NONE',  ( 22.50000000000000000, 0.1000000000111554016, -155.7499999999999716 ) ) ;
#27879 = DIRECTION ( 'NONE',  ( 1.000000000000000000, 0.000000000000000000, 0.000000000000000000 ) ) ;
#27880 = ADVANCED_FACE ( 'NONE', ( #226087 ), #127021, .T. ) ;
#27881 = ORIENTED_EDGE ( 'NONE', *, *, #88848, .F. ) ;
#27882 = ADVANCED_FACE ( 'NONE', ( #30508 ), #188274, .F. ) ;
#27883 = EDGE_LOOP ( 'NONE', ( #111430, #37201, #14139, #178986 ) ) ;
#27884 = DIRECTION ( 'NONE',  ( 0.000000000000000000, 0.000000000000000000, -1.000000000000000000 ) ) ;
#27885 = CARTESIAN_POINT ( 'NONE',  ( -21.05000000000000071, 0.4810385098657082859, -209.0827657365571213 ) ) ;
#27886 = LINE ( 'NONE', #183085, #224401 ) ;
#27887 = DIRECTION ( 'NONE',  ( 0.000000000000000000, -0.4721928772777351790, -0.8814952561688427224 ) ) ;
#27888 = AXIS2_PLACEMENT_3D ( 'NONE', #146167, #223135, #9227 ) ;
#27889 = AXIS2_PLACEMENT_3D ( 'NONE', #248133, #106029, #185593 ) ;
#27890 = CARTESIAN_POINT ( 'NONE',  ( 23.14999999999999147, 7.128833340093095217, -233.7327013124392749 ) ) ;
#27891 = VECTOR ( 'NONE', #146590, 1000.000000000000227 ) ;
#27892 = AXIS2_PLACEMENT_3D ( 'NONE', #37126, #4074, #81026 ) ;
#27893 = DIRECTION ( 'NONE',  ( 1.000000000000000000, 0.000000000000000000, 0.000000000000000000 ) ) ;
#27894 = ORIENTED_EDGE ( 'NONE', *, *, #213724, .F. ) ;
#27895 = CARTESIAN_POINT ( 'NONE',  ( -20.94403535211772294, 65.69367753730655579, -97.51892380663478832 ) ) ;
#27897 = ORIENTED_EDGE ( 'NONE', *, *, #74526, .F. ) ;
#27896 = DIRECTION ( 'NONE',  ( 0.000000000000000000, -1.000000000000000000, -6.982962677686265922E-15 ) ) ;
#27898 = DIRECTION ( 'NONE',  ( 1.000000000000000000, 0.000000000000000000, 0.000000000000000000 ) ) ;
#27899 = DIRECTION ( 'NONE',  ( -3.265361837132812107E-16, 0.4721928772777345684, 0.8814952561688429444 ) ) ;
#27900 = DIRECTION ( 'NONE',  ( 1.000000000000000000, 0.000000000000000000, 0.000000000000000000 ) ) ;
#27902 = ORIENTED_EDGE ( 'NONE', *, *, #87220, .F. ) ;
#27901 = DIRECTION ( 'NONE',  ( -1.000000000000000000, -2.885090398161910739E-16, -6.283419270304611573E-17 ) ) ;
#27903 = DIRECTION ( 'NONE',  ( 0.000000000000000000, -0.2617529984165152257, -0.9651348961777124202 ) ) ;
#27904 = CARTESIAN_POINT ( 'NONE',  ( -18.55121869061588669, 65.67252876774583115, -164.4457041994994881 ) ) ;
#27905 = CARTESIAN_POINT ( 'NONE',  ( 21.13461538461538325, 10.61458296203669249, -79.35000000000005116 ) ) ;
#27906 = VERTEX_POINT ( 'NONE', #130865 ) ;
#27907 = CARTESIAN_POINT ( 'NONE',  ( 18.49351773456763226, -7.697694071498478507, -210.0302349457594175 ) ) ;
#27908 = CARTESIAN_POINT ( 'NONE',  ( -16.87401514999234209, 66.05000000001201954, -115.7430894919920377 ) ) ;
#27909 = CARTESIAN_POINT ( 'NONE',  ( -21.05000000000000071, 76.00000000001126921, -203.5231074845248997 ) ) ;
#27910 = EDGE_CURVE ( 'NONE', #209120, #255663, #67049, .T. ) ;
#27911 = VECTOR ( 'NONE', #201033, 1000.000000000000000 ) ;
#27912 = AXIS2_PLACEMENT_3D ( 'NONE', #137806, #245599, #146472 ) ;
#27913 = CARTESIAN_POINT ( 'NONE',  ( -20.94999999999999929, 1.115600667400684642E-11, -189.1999999999999602 ) ) ;
#27914 = ORIENTED_EDGE ( 'NONE', *, *, #233434, .T. ) ;
#27915 = DIRECTION ( 'NONE',  ( 0.000000000000000000, 6.982962677686267499E-15, -1.000000000000000000 ) ) ;
#27916 = ORIENTED_EDGE ( 'NONE', *, *, #150576, .F. ) ;
#27918 = FACE_OUTER_BOUND ( 'NONE', #215240, .T. ) ;
#27917 = AXIS2_PLACEMENT_3D ( 'NONE', #158501, #80180, #140170 ) ;
#27919 = DIRECTION ( 'NONE',  ( 0.000000000000000000, 0.000000000000000000, -1.000000000000000000 ) ) ;
#27920 = EDGE_CURVE ( 'NONE', #52329, #106008, #73137, .T. ) ;
#27921 = DIRECTION ( 'NONE',  ( -0.000000000000000000, 0.9126074666063771490, 0.4088369013363281623 ) ) ;
#27922 = DIRECTION ( 'NONE',  ( 0.000000000000000000, 0.000000000000000000, -1.000000000000000000 ) ) ;
#27923 = ORIENTED_EDGE ( 'NONE', *, *, #71583, .F. ) ;
#27924 = EDGE_CURVE ( 'NONE', #64517, #69800, #33102, .T. ) ;
#27925 = DIRECTION ( 'NONE',  ( -0.000000000000000000, 0.9579639084728132081, 0.2868887416116073230 ) ) ;
#27926 = CARTESIAN_POINT ( 'NONE',  ( 21.05000000000000071, -1.736257131586239844, -45.06865232901750318 ) ) ;
#27927 = EDGE_CURVE ( 'NONE', #186771, #10427, #114798, .T. ) ;
#27928 = B_SPLINE_CURVE_WITH_KNOTS ( 'NONE', 3,
 ( #15544, #113332, #14255, #252831, #254109, #148625, #109464 ),
 .UNSPECIFIED., .F., .F.,
 ( 4, 3, 4 ),
 ( 0.000000000000000000, 0.0007844235214594263332, 0.001767853679404340298 ),
 .UNSPECIFIED. ) ;
#27929 = CARTESIAN_POINT ( 'NONE',  ( -18.79999999999999716, -11.65000000000000036, 5.900000000000001243 ) ) ;
#27930 = CARTESIAN_POINT ( 'NONE',  ( 20.99999999999999645, 9.750000000011137757, -180.1499999999999773 ) ) ;
#27931 = CIRCLE ( 'NONE', #173698, 0.1000000000000028644 ) ;
#27932 = CARTESIAN_POINT ( 'NONE',  ( 20.94999999999999929, -11.64999999998883595, -100.5000000000000426 ) ) ;
#27933 = ORIENTED_EDGE ( 'NONE', *, *, #99306, .T. ) ;
#27935 = ORIENTED_EDGE ( 'NONE', *, *, #41117, .F. ) ;
#27934 = DIRECTION ( 'NONE',  ( 0.000000000000000000, 0.9126074666063813678, 0.4088369013363182813 ) ) ;
#27936 = EDGE_CURVE ( 'NONE', #201031, #229898, #235580, .T. ) ;
#27937 = ORIENTED_EDGE ( 'NONE', *, *, #39212, .T. ) ;
#27938 = DIRECTION ( 'NONE',  ( 1.186688945009009831E-16, -1.000000000000000000, 0.000000000000000000 ) ) ;
#27939 = EDGE_CURVE ( 'NONE', #12767, #116556, #56499, .T. ) ;
#27940 = VERTEX_POINT ( 'NONE', #167459 ) ;
#27941 = CARTESIAN_POINT ( 'NONE',  ( 21.13507111622890022, 65.28231661301367694, -124.2739388981635926 ) ) ;
#27942 = DIRECTION ( 'NONE',  ( 0.000000000000000000, 0.000000000000000000, -1.000000000000000000 ) ) ;
#27943 = DIRECTION ( 'NONE',  ( 0.000000000000000000, 1.000000000000000000, 0.000000000000000000 ) ) ;
#27944 = ORIENTED_EDGE ( 'NONE', *, *, #204836, .F. ) ;
#27945 = CARTESIAN_POINT ( 'NONE',  ( -16.91247567987038636, 66.04091731634281359, -123.8943830259870253 ) ) ;
#27946 = DIRECTION ( 'NONE',  ( 0.000000000000000000, 0.000000000000000000, 1.000000000000000000 ) ) ;
#27947 = AXIS2_PLACEMENT_3D ( 'NONE', #199766, #238868, #137193 ) ;
#27948 = CARTESIAN_POINT ( 'NONE',  ( 21.30000000000002558, 76.00000000001162448, -65.47310748452431994 ) ) ;
#27949 = ORIENTED_EDGE ( 'NONE', *, *, #29199, .F. ) ;
#27950 = DIRECTION ( 'NONE',  ( 0.000000000000000000, 0.000000000000000000, 1.000000000000000000 ) ) ;
#27952 = ORIENTED_EDGE ( 'NONE', *, *, #205604, .T. ) ;
#27951 = DIRECTION ( 'NONE',  ( 0.000000000000000000, 0.000000000000000000, 1.000000000000000000 ) ) ;
#27953 = DIRECTION ( 'NONE',  ( 0.000000000000000000, 0.000000000000000000, 1.000000000000000000 ) ) ;
#27954 = DIRECTION ( 'NONE',  ( -0.9880948137434723000, 0.1538461538461483591, -0.000000000000000000 ) ) ;
#27955 = AXIS2_PLACEMENT_3D ( 'NONE', #63987, #237491, #217897 ) ;
#27956 = CIRCLE ( 'NONE', #32039, 0.09999999999999986677 ) ;
#27957 = ADVANCED_FACE ( 'NONE', ( #246955 ), #189575, .F. ) ;
#27958 = ADVANCED_FACE ( 'NONE', ( #150455 ), #243973, .F. ) ;
#27959 = ORIENTED_EDGE ( 'NONE', *, *, #144710, .T. ) ;
#27960 = CARTESIAN_POINT ( 'NONE',  ( 21.05000000000000071, 69.74218538953624602, -170.1208977758331855 ) ) ;
#27961 = CARTESIAN_POINT ( 'NONE',  ( -12.60206096961791999, 66.61031399435634626, -120.8502639781730181 ) ) ;
#27962 = DIRECTION ( 'NONE',  ( 0.000000000000000000, -0.9126074666063545004, -0.4088369013363783999 ) ) ;
#27964 = EDGE_LOOP ( 'NONE', ( #43749, #8695, #202720, #83736 ) ) ;
#27963 = AXIS2_PLACEMENT_3D ( 'NONE', #246457, #67816, #187785 ) ;
#27965 = CARTESIAN_POINT ( 'NONE',  ( -21.14999999999999858, -11.75000000000000000, 3.469446951953614189E-15 ) ) ;
#27966 = ADVANCED_FACE ( 'NONE', ( #69629 ), #229972, .F. ) ;
#27967 = AXIS2_PLACEMENT_3D ( 'NONE', #234350, #150979, #89698 ) ;
#27968 = SPHERICAL_SURFACE ( 'NONE', #139032, 0.1000000000000000056 ) ;
#27969 = ORIENTED_EDGE ( 'NONE', *, *, #9210, .T. ) ;
#27970 = ADVANCED_FACE ( 'NONE', ( #12231 ), #139891, .T. ) ;
#27971 = EDGE_CURVE ( 'NONE', #54334, #258000, #193915, .T. ) ;
#27972 = CIRCLE ( 'NONE', #231971, 0.4000000000000114575 ) ;
#27973 = AXIS2_PLACEMENT_3D ( 'NONE', #131276, #32204, #111719 ) ;
#27974 = ORIENTED_EDGE ( 'NONE', *, *, #91537, .T. ) ;
#27975 = DIRECTION ( 'NONE',  ( 0.000000000000000000, 0.000000000000000000, 1.000000000000000000 ) ) ;
#27976 = ADVANCED_FACE ( 'NONE', ( #93024 ), #134702, .F. ) ;
#27977 = AXIS2_PLACEMENT_3D ( 'NONE', #180087, #256988, #237485 ) ;
#27978 = VERTEX_POINT ( 'NONE', #17354 ) ;
#27979 = CARTESIAN_POINT ( 'NONE',  ( 18.55807992284871588, 10.32898536000685930, -39.08266832227643306 ) ) ;
#27980 = CARTESIAN_POINT ( 'NONE',  ( -16.87683809663752399, 66.13411015068015786, -183.2905342915938149 ) ) ;
#27982 = ORIENTED_EDGE ( 'NONE', *, *, #187071, .T. ) ;
#27981 = DIRECTION ( 'NONE',  ( 0.000000000000000000, -0.8814952561688476074, 0.4721928772777262417 ) ) ;
#27983 = CARTESIAN_POINT ( 'NONE',  ( 23.50000000000005684, 78.05591623545335267, -49.16694968567509250 ) ) ;
#27985 = CIRCLE ( 'NONE', #165321, 0.1000000000000028644 ) ;
#27984 = DIRECTION ( 'NONE',  ( 0.000000000000000000, 1.000000000000000000, 0.000000000000000000 ) ) ;
#27986 = FACE_OUTER_BOUND ( 'NONE', #183626, .T. ) ;
#27987 = CARTESIAN_POINT ( 'NONE',  ( 21.13614978966381841, 76.00000000001169553, -76.02221218635807531 ) ) ;
#27988 = EDGE_CURVE ( 'NONE', #104152, #163525, #172618, .T. ) ;
#27989 = FACE_OUTER_BOUND ( 'NONE', #217340, .T. ) ;
#27990 = FACE_OUTER_BOUND ( 'NONE', #70536, .T. ) ;
#27992 = ORIENTED_EDGE ( 'NONE', *, *, #145875, .T. ) ;
#27991 = CARTESIAN_POINT ( 'NONE',  ( -22.46246831459151494, 75.97808783307259262, -114.6729720457342694 ) ) ;
#27993 = DIRECTION ( 'NONE',  ( -0.000000000000000000, 1.000000000000000000, 0.000000000000000000 ) ) ;
#27994 = ORIENTED_EDGE ( 'NONE', *, *, #80269, .F. ) ;
#27995 = AXIS2_PLACEMENT_3D ( 'NONE', #202233, #26174, #204779 ) ;
#27996 = CIRCLE ( 'NONE', #82101, 0.09999999999999939493 ) ;
#27997 = CARTESIAN_POINT ( 'NONE',  ( -20.85000000000000142, -1.851617760457748618, -179.1031897196036766 ) ) ;
#27998 = CARTESIAN_POINT ( 'NONE',  ( -20.85000000000000142, 1.115600667400684642E-11, -134.0000000000000284 ) ) ;
#27999 = DIRECTION ( 'NONE',  ( -1.000000000000000000, 3.265361837132813093E-16, 2.280189983783949500E-30 ) ) ;
#28000 = FACE_OUTER_BOUND ( 'NONE', #160809, .T. ) ;
#28001 = VERTEX_POINT ( 'NONE', #38209 ) ;
#28002 = LINE ( 'NONE', #107497, #206484 ) ;
#28003 = DIRECTION ( 'NONE',  ( 1.000000000000000000, 0.000000000000000000, 0.000000000000000000 ) ) ;
#28004 = VECTOR ( 'NONE', #241659, 1000.000000000000000 ) ;
#28005 = ORIENTED_EDGE ( 'NONE', *, *, #27254, .F. ) ;
#28006 = CARTESIAN_POINT ( 'NONE',  ( 21.05000000000000071, 76.08559286337464300, -209.9367702193935372 ) ) ;
#28008 = CARTESIAN_POINT ( 'NONE',  ( -16.86132326855788577, 60.95208832852619452, -220.9947876425996753 ) ) ;
#28007 = CIRCLE ( 'NONE', #90502, 0.1000000000000055844 ) ;
#28009 = EDGE_LOOP ( 'NONE', ( #2671, #94756, #243071, #173360 ) ) ;
#28010 = EDGE_CURVE ( 'NONE', #168551, #37194, #56452, .T. ) ;
#28011 = DIRECTION ( 'NONE',  ( 1.000000000000000000, 0.000000000000000000, 0.000000000000000000 ) ) ;
#28012 = ORIENTED_EDGE ( 'NONE', *, *, #95875, .F. ) ;
#28013 = CARTESIAN_POINT ( 'NONE',  ( -12.93407622233968901, 9.417789466963363054, -48.85738454397688457 ) ) ;
#28014 = EDGE_LOOP ( 'NONE', ( #85192, #44487, #90079, #126315 ) ) ;
#28015 = CIRCLE ( 'NONE', #86228, 11.64999999999999325 ) ;
#28016 = DIRECTION ( 'NONE',  ( 0.000000000000000000, 0.000000000000000000, 1.000000000000000000 ) ) ;
#28017 = CIRCLE ( 'NONE', #119593, 0.2000000000000057288 ) ;
#28018 = CARTESIAN_POINT ( 'NONE',  ( -18.39999999999999858, 64.52683809664912928, -60.19716141771643692 ) ) ;
#28019 = CIRCLE ( 'NONE', #73810, 0.09999999999998898659 ) ;
#28020 = VECTOR ( 'NONE', #109241, 1000.000000000000000 ) ;
#28021 = ORIENTED_EDGE ( 'NONE', *, *, #175034, .T. ) ;
#28022 = EDGE_LOOP ( 'NONE', ( #241689, #221485, #47257, #52793 ) ) ;
#28023 = CARTESIAN_POINT ( 'NONE',  ( 18.59999999999999076, 11.65000000000000391, -24.75000000000000000 ) ) ;
#28025 = ORIENTED_EDGE ( 'NONE', *, *, #215549, .T. ) ;
#28024 = CARTESIAN_POINT ( 'NONE',  ( 12.93225390519045526, 9.417651958852164995, -48.85878739244044056 ) ) ;
#28026 = ADVANCED_FACE ( 'NONE', ( #59002 ), #18627, .T. ) ;
#28027 = CARTESIAN_POINT ( 'NONE',  ( 21.04999999999999716, 67.12872031401695949, -191.3731074845244109 ) ) ;
#28028 = VERTEX_POINT ( 'NONE', #13503 ) ;
#28029 = AXIS2_PLACEMENT_3D ( 'NONE', #255380, #41552, #76795 ) ;
#28030 =( BOUNDED_SURFACE ( )  B_SPLINE_SURFACE ( 3, 2, ( 
 ( #249522, #52578, #33078 ),
 ( #173875, #53880, #74764 ),
 ( #55123, #154311, #168742 ),
 ( #70901, #134672, #209094 ),
 ( #248228, #69603, #149146 ),
 ( #229942, #228680, #91719 ),
 ( #30478, #112577, #252071 ),
 ( #51271, #250784, #31779 ),
 ( #111287, #171311, #151725 ),
 ( #231252, #192126, #13474 ) ),
 .UNSPECIFIED., .F., .F., .F. ) 
 B_SPLINE_SURFACE_WITH_KNOTS ( ( 4, 2, 2, 2, 4 ),
 ( 3, 3 ),
 ( 0.002161241639767788603, 0.002579950749617449836, 0.002789305304542280452, 0.002893982582004695978, 0.002998659859467111069 ),
 ( 0.000000000000000000, 1.000000000000000000 ),
 .UNSPECIFIED. ) 
 GEOMETRIC_REPRESENTATION_ITEM ( )  RATIONAL_B_SPLINE_SURFACE ( (
 ( 1.000000000000000000, 0.7071067811864800712, 1.000000000000000000),
 ( 1.000000000000000000, 0.7632447400664645887, 1.000000000000000000),
 ( 1.000000000000000000, 0.8158073005108372744, 1.000000000000000000),
 ( 1.000000000000000000, 0.8906973462396270413, 1.000000000000000000),
 ( 1.000000000000000000, 0.9149408947800815595, 1.000000000000000000),
 ( 1.000000000000000000, 0.9493368785275272392, 1.000000000000000000),
 ( 1.000000000000000000, 0.9605194247156589871, 1.000000000000000000),
 ( 1.000000000000000000, 0.9803630264781161285, 1.000000000000000000),
 ( 1.000000000000000000, 0.9900844824271106681, 1.000000000000000000),
 ( 1.000000000000000000, 0.9894588281429282928, 1.000000000000000000) ) ) 
 REPRESENTATION_ITEM ( '' )  SURFACE ( )  );
#28031 = EDGE_LOOP ( 'NONE', ( #76784, #193384, #229541, #174619 ) ) ;
#28032 = DIRECTION ( 'NONE',  ( -1.000000000000000000, -0.000000000000000000, -0.000000000000000000 ) ) ;
#28033 = DIRECTION ( 'NONE',  ( 1.000000000000000000, 0.000000000000000000, 0.000000000000000000 ) ) ;
#28034 = DIRECTION ( 'NONE',  ( 1.000000000000000000, 0.000000000000000000, 0.000000000000000000 ) ) ;
#28035 = DIRECTION ( 'NONE',  ( 1.000000000000000000, 0.000000000000000000, 0.000000000000000000 ) ) ;
#28036 = VECTOR ( 'NONE', #186522, 1000.000000000000000 ) ;
#28037 = LINE ( 'NONE', #150531, #56436 ) ;
#28038 = B_SPLINE_CURVE_WITH_KNOTS ( 'NONE', 3,
 ( #82886, #162482, #63345, #68504, #166350, #189734, #107618, #227565, #205424, #72370, #89326, #48924, #208028, #26835, #28115, #91903, #131034, #125889, #191040 ),
 .UNSPECIFIED., .F., .F.,
 ( 4, 3, 3, 3, 3, 3, 4 ),
 ( 0.000000000000000000, 2.646747978908405501E-05, 5.271166642128941309E-05, 9.008788829884216409E-05, 0.0001426648776561083808, 0.0001897378458659868894, 0.0001917382627806458214 ),
 .UNSPECIFIED. ) ;
#28039 = LINE ( 'NONE', #204063, #92126 ) ;
#28040 = AXIS2_PLACEMENT_3D ( 'NONE', #66044, #243398, #123462 ) ;
#28041 = VERTEX_POINT ( 'NONE', #135984 ) ;
#28042 = DIRECTION ( 'NONE',  ( 0.000000000000000000, 0.6728971962616412394, 0.7397360091703134577 ) ) ;
#28043 = DIRECTION ( 'NONE',  ( -0.000000000000000000, -6.982962677686266711E-15, 1.000000000000000000 ) ) ;
#28044 = DIRECTION ( 'NONE',  ( 0.000000000000000000, 0.8700118002898393765, -0.4930308989875104575 ) ) ;
#28045 = ORIENTED_EDGE ( 'NONE', *, *, #171486, .T. ) ;
#28046 = CARTESIAN_POINT ( 'NONE',  ( 18.59117750673696179, 10.33248238083634796, -106.0948465439131922 ) ) ;
#28047 = ORIENTED_EDGE ( 'NONE', *, *, #214186, .T. ) ;
#28048 = DIRECTION ( 'NONE',  ( 0.000000000000000000, -7.056502275159890832E-15, 1.000000000000000000 ) ) ;
#28050 = ORIENTED_EDGE ( 'NONE', *, *, #13632, .F. ) ;
#28049 = CIRCLE ( 'NONE', #182147, 4.300000000000025580 ) ;
#28051 = DIRECTION ( 'NONE',  ( 1.000000000000000000, 0.000000000000000000, 0.000000000000000000 ) ) ;
#28052 = CARTESIAN_POINT ( 'NONE',  ( -20.94999999999999929, 72.02722222756958104, -225.1832529173024398 ) ) ;
#28053 = ORIENTED_EDGE ( 'NONE', *, *, #147768, .F. ) ;
#28054 = ORIENTED_EDGE ( 'NONE', *, *, #114725, .F. ) ;
#28056 = VERTEX_POINT ( 'NONE', #57738 ) ;
#28055 = CARTESIAN_POINT ( 'NONE',  ( -21.05000000000000071, 44.15969672213208952, -258.9565289832007693 ) ) ;
#28057 = DIRECTION ( 'NONE',  ( 0.000000000000000000, -1.000000000000000000, -0.000000000000000000 ) ) ;
#28058 = ORIENTED_EDGE ( 'NONE', *, *, #50746, .T. ) ;
#28059 = CARTESIAN_POINT ( 'NONE',  ( 18.39999999999999858, -7.667348966301519297, -236.4704904124130280 ) ) ;
#28060 = CARTESIAN_POINT ( 'NONE',  ( -23.25000000000000000, 76.00000000001213607, -136.5231074845242745 ) ) ;
#28061 = ORIENTED_EDGE ( 'NONE', *, *, #183596, .T. ) ;
#28062 = DIRECTION ( 'NONE',  ( 0.000000000000000000, -0.2128009952263601734, 0.9770955615653316162 ) ) ;
#28063 = EDGE_CURVE ( 'NONE', #171236, #232431, #81440, .T. ) ;
#28064 = CARTESIAN_POINT ( 'NONE',  ( -20.94999999999999929, -1.249999999988843369, -108.5000000000000426 ) ) ;
#28065 = AXIS2_PLACEMENT_3D ( 'NONE', #139430, #136883, #80742 ) ;
#28066 = AXIS2_PLACEMENT_3D ( 'NONE', #186263, #217971, #67587 ) ;
#28067 = CIRCLE ( 'NONE', #23800, 0.9000000000000014655 ) ;
#28068 = AXIS2_PLACEMENT_3D ( 'NONE', #106706, #147126, #109275 ) ;
#28069 = ORIENTED_EDGE ( 'NONE', *, *, #130369, .F. ) ;
#28070 = DIRECTION ( 'NONE',  ( 0.000000000000000000, -0.8814952561688437216, 0.4721928772777334582 ) ) ;
#28071 = EDGE_CURVE ( 'NONE', #182938, #20946, #102280, .T. ) ;
#28072 = DIRECTION ( 'NONE',  ( -3.265361837132813093E-16, 1.000000000000000000, 0.000000000000000000 ) ) ;
#28073 = ADVANCED_FACE ( 'NONE', ( #257179 ), #73314, .T. ) ;
#28074 = LINE ( 'NONE', #68463, #34392 ) ;
#28076 = VERTEX_POINT ( 'NONE', #255898 ) ;
#28075 = DIRECTION ( 'NONE',  ( 1.301042606982683418E-14, 0.7049548389604990417, -0.7092521942343054109 ) ) ;
#28077 = DIRECTION ( 'NONE',  ( 1.000000000000000000, 0.000000000000000000, 0.000000000000000000 ) ) ;
#28078 = LINE ( 'NONE', #106274, #252428 ) ;
#28079 = DIRECTION ( 'NONE',  ( -0.7071067811865475727, -0.7071067811865475727, 0.000000000000000000 ) ) ;
#28082 = DIRECTION ( 'NONE',  ( 1.000000000000000000, 0.000000000000000000, 0.000000000000000000 ) ) ;
#28081 = AXIS2_PLACEMENT_3D ( 'NONE', #125454, #204961, #165877 ) ;
#28080 = DIRECTION ( 'NONE',  ( 1.000000000000000000, 0.000000000000000000, 0.000000000000000000 ) ) ;
#28083 = CARTESIAN_POINT ( 'NONE',  ( 20.95512820512820085, 10.62384868372303615, -108.1649135690876449 ) ) ;
#28084 = DIRECTION ( 'NONE',  ( -1.000000000000000000, 8.034189347746079853E-16, -2.566115377699053192E-16 ) ) ;
#28085 = CIRCLE ( 'NONE', #173865, 0.1000000000000072498 ) ;
#28086 = EDGE_CURVE ( 'NONE', #64377, #76616, #153045, .T. ) ;
#28087 = DIRECTION ( 'NONE',  ( -1.000000000000000000, 0.000000000000000000, 0.000000000000000000 ) ) ;
#28088 = CARTESIAN_POINT ( 'NONE',  ( 20.94999999999999929, 1.115600667400684642E-11, -67.00000000000004263 ) ) ;
#28089 = ORIENTED_EDGE ( 'NONE', *, *, #180395, .T. ) ;
#28090 = VECTOR ( 'NONE', #214303, 1000.000000000000000 ) ;
#28091 = ORIENTED_EDGE ( 'NONE', *, *, #185825, .F. ) ;
#28092 = ORIENTED_EDGE ( 'NONE', *, *, #31759, .F. ) ;
#28093 = ADVANCED_FACE ( 'NONE', ( #158185 ), #94300, .F. ) ;
#28094 =( BOUNDED_SURFACE ( )  B_SPLINE_SURFACE ( 3, 2, ( 
 ( #78143, #25577, #136842 ),
 ( #216378, #37773, #237238 ),
 ( #58574, #116020, #138112 ),
 ( #195564, #59852, #142917 ),
 ( #43850, #24304, #84189 ),
 ( #204187, #105053, #184633 ) ),
 .UNSPECIFIED., .F., .F., .F. ) 
 B_SPLINE_SURFACE_WITH_KNOTS ( ( 4, 2, 4 ),
 ( 3, 3 ),
 ( 1.570796326794895448, 2.356194490192343505, 3.141592653589791784 ),
 ( 0.000000000000000000, 1.000000000000000000 ),
 .UNSPECIFIED. ) 
 GEOMETRIC_REPRESENTATION_ITEM ( )  RATIONAL_B_SPLINE_SURFACE ( (
 ( 1.000000000000000000, 0.7071067811865475727, 1.000000000000000000),
 ( 1.000000000000000000, 0.6611148371778921007, 1.000000000000000000),
 ( 1.000000000000000000, 0.6092287576696249207, 1.000000000000000000),
 ( 1.000000000000000000, 0.5278258667057440512, 1.000000000000000000),
 ( 1.000000000000000000, 0.4993418825334574596, 1.000000000000000000),
 ( 1.000000000000000000, 0.4999999999999960587, 1.000000000000000000) ) ) 
 REPRESENTATION_ITEM ( '' )  SURFACE ( )  );
#28095 = CARTESIAN_POINT ( 'NONE',  ( -20.94999999999999929, 64.35000000001220144, -143.3069731475025321 ) ) ;
#28096 = ORIENTED_EDGE ( 'NONE', *, *, #179557, .T. ) ;
#28097 = CARTESIAN_POINT ( 'NONE',  ( 20.94999999999999929, 70.97296516614450468, -234.1788952109995137 ) ) ;
#28098 = SPHERICAL_SURFACE ( 'NONE', #149748, 0.1000000000000000056 ) ;
#28100 = ORIENTED_EDGE ( 'NONE', *, *, #109601, .T. ) ;
#28099 = CIRCLE ( 'NONE', #94701, 0.1000000000000028644 ) ;
#28101 = DIRECTION ( 'NONE',  ( 0.000000000000000000, -0.2128009952263264781, 0.9770955615653388326 ) ) ;
#28102 = VERTEX_POINT ( 'NONE', #215536 ) ;
#28103 = EDGE_LOOP ( 'NONE', ( #188056, #115608, #156701, #63572 ) ) ;
#28104 = CARTESIAN_POINT ( 'NONE',  ( 21.05000000000000071, -11.48912529306490349, -137.1000000000000227 ) ) ;
#28105 = ORIENTED_EDGE ( 'NONE', *, *, #190891, .T. ) ;
#28106 = CARTESIAN_POINT ( 'NONE',  ( 21.22070241538126467, 0.09891903054618129965, -94.03005372713040799 ) ) ;
#28108 = ORIENTED_EDGE ( 'NONE', *, *, #253820, .F. ) ;
#28107 = CARTESIAN_POINT ( 'NONE',  ( -17.11825945287481332, 65.95000000001181206, -82.17310748452439384 ) ) ;
#28109 = LINE ( 'NONE', #85447, #70514 ) ;
#28111 = CARTESIAN_POINT ( 'NONE',  ( -16.88593481969334320, 9.950560090095466492, -121.3518722569445316 ) ) ;
#28110 = AXIS2_PLACEMENT_3D ( 'NONE', #85538, #188528, #110267 ) ;
#28114 = ADVANCED_FACE ( 'NONE', ( #176440 ), #19108, .T. ) ;
#28113 = ORIENTED_EDGE ( 'NONE', *, *, #127301, .T. ) ;
#28112 = DIRECTION ( 'NONE',  ( 0.000000000000000000, 0.000000000000000000, 1.000000000000000000 ) ) ;
#28115 = CARTESIAN_POINT ( 'NONE',  ( -18.50016250449483479, 10.29766095125286895, -72.47436639332757125 ) ) ;
#28116 = DIRECTION ( 'NONE',  ( 0.000000000000000000, 0.8814952561688476074, -0.4721928772777262417 ) ) ;
#28118 = AXIS2_PLACEMENT_3D ( 'NONE', #189553, #8347, #249526 ) ;
#28117 = B_SPLINE_CURVE_WITH_KNOTS ( 'NONE', 3,
 ( #211920, #231481, #95785, #56639, #132363, #33307 ),
 .UNSPECIFIED., .F., .F.,
 ( 4, 2, 4 ),
 ( 0.000000000000000000, 0.0001569047307838633283, 0.0003138094615677266565 ),
 .UNSPECIFIED. ) ;
#28120 = CARTESIAN_POINT ( 'NONE',  ( 21.05000000000000071, 8.776282889879928106, -179.6762151410682975 ) ) ;
#28119 = CARTESIAN_POINT ( 'NONE',  ( 21.14999999999999503, 11.65000000001116298, -134.0000000000000284 ) ) ;
#28121 = DIRECTION ( 'NONE',  ( 0.000000000000000000, -0.1350103645451904977, 0.9908441862701596881 ) ) ;
#28122 = CIRCLE ( 'NONE', #48759, 0.2000000000000057288 ) ;
#28123 = CIRCLE ( 'NONE', #182227, 0.1000000000000028644 ) ;
#28124 = DIRECTION ( 'NONE',  ( 1.000000000000000000, 0.000000000000000000, 0.000000000000000000 ) ) ;
#28125 = LINE ( 'NONE', #64651, #63647 ) ;
#28126 = ORIENTED_EDGE ( 'NONE', *, *, #209683, .T. ) ;
#28127 = ORIENTED_EDGE ( 'NONE', *, *, #71457, .T. ) ;
#28128 =( BOUNDED_CURVE ( )  B_SPLINE_CURVE ( 3, ( #256003, #99522, #77402, #257287 ),
 .UNSPECIFIED., .F., .F. ) 
 B_SPLINE_CURVE_WITH_KNOTS ( ( 4, 4 ),
 ( 0.3000847527772385614, 0.5517402753107881752 ),
 .UNSPECIFIED. ) 
 CURVE ( )  GEOMETRIC_REPRESENTATION_ITEM ( )  RATIONAL_B_SPLINE_CURVE ( ( 1.000000000000000000, 0.9947294176030464508, 0.9947294176030464508, 1.000000000000000000 ) ) 
 REPRESENTATION_ITEM ( '' )  );
#28129 = ORIENTED_EDGE ( 'NONE', *, *, #5215, .F. ) ;
#28130 = PRODUCT_DEFINITION_FORMATION_WITH_SPECIFIED_SOURCE ( 'ANY', '', #162165, .NOT_KNOWN. ) ;
#28131 = EDGE_CURVE ( 'NONE', #59001, #158817, #233832, .T. ) ;
#28132 = DIRECTION ( 'NONE',  ( -0.000000000000000000, 0.3427706569149635007, -0.9394191166662961834 ) ) ;
#28133 = VECTOR ( 'NONE', #107915, 1000.000000000000000 ) ;
#28134 = ORIENTED_EDGE ( 'NONE', *, *, #214888, .T. ) ;
#28135 = CARTESIAN_POINT ( 'NONE',  ( 18.52928932188133970, 15.28939250479744949, -222.8979625946709007 ) ) ;
#28136 = ORIENTED_EDGE ( 'NONE', *, *, #113859, .T. ) ;
#28138 = DIRECTION ( 'NONE',  ( 1.000000000000000000, -0.000000000000000000, -0.000000000000000000 ) ) ;
#28137 = CIRCLE ( 'NONE', #44862, 0.1000000000000028644 ) ;
#28139 = EDGE_CURVE ( 'NONE', #25796, #249301, #252324, .T. ) ;
#28140 = ORIENTED_EDGE ( 'NONE', *, *, #26945, .T. ) ;
#28141 = CARTESIAN_POINT ( 'NONE',  ( -18.59999999999999787, 77.83585931145600512, -158.5186683157258187 ) ) ;
#28142 = EDGE_CURVE ( 'NONE', #215216, #191947, #77306, .T. ) ;
#28143 = AXIS2_PLACEMENT_3D ( 'NONE', #199475, #20843, #80766 ) ;
#28144 = EDGE_LOOP ( 'NONE', ( #220064, #55554 ) ) ;
#28145 = EDGE_LOOP ( 'NONE', ( #205571, #191458, #243880, #58234 ) ) ;
#28146 = CIRCLE ( 'NONE', #236405, 0.1000000000000028644 ) ;
#28147 = EDGE_LOOP ( 'NONE', ( #77113, #65151, #100248, #129152 ) ) ;
#28149 = DIRECTION ( 'NONE',  ( 1.000000000000000000, 0.000000000000000000, 0.000000000000000000 ) ) ;
#28148 = AXIS2_PLACEMENT_3D ( 'NONE', #93800, #212491, #114657 ) ;
#28150 = CARTESIAN_POINT ( 'NONE',  ( 20.09999999999999787, 30.11188998467138944, -234.9833440560338147 ) ) ;
#28151 = PLANE ( 'NONE',  #5134 ) ;
#28152 = CIRCLE ( 'NONE', #224319, 0.09999999999999939493 ) ;
#28153 = DIRECTION ( 'NONE',  ( -0.000000000000000000, 0.9126074666063770380, 0.4088369013363281068 ) ) ;
#28154 = DIRECTION ( 'NONE',  ( 1.000000000000000000, 0.000000000000000000, 0.000000000000000000 ) ) ;
#28155 = AXIS2_PLACEMENT_3D ( 'NONE', #15808, #152753, #95312 ) ;
#28156 = CARTESIAN_POINT ( 'NONE',  ( 20.85000000000000142, 7.021664781911246322, -70.83356540189728889 ) ) ;
#28157 = ADVANCED_FACE ( 'NONE', ( #156885 ), #116452, .T. ) ;
#28159 = CYLINDRICAL_SURFACE ( 'NONE', #66034, 0.09999999999999939493 ) ;
#28158 = CARTESIAN_POINT ( 'NONE',  ( 21.05000000000000071, -11.29603075032412640, -130.9521008403361861 ) ) ;
#28160 = CARTESIAN_POINT ( 'NONE',  ( -20.93284271247462058, 11.75000000001115019, -160.4851942293460354 ) ) ;
#28162 = ORIENTED_EDGE ( 'NONE', *, *, #53819, .T. ) ;
#28161 = DIRECTION ( 'NONE',  ( 0.000000000000000000, -6.982962677686266711E-15, 1.000000000000000000 ) ) ;
#28164 = CARTESIAN_POINT ( 'NONE',  ( 23.14999999999999503, 69.55000000001186322, -90.67310748452435121 ) ) ;
#28163 = CARTESIAN_POINT ( 'NONE',  ( 20.53930447207976684, 8.977148687535432714, -75.44250714157833215 ) ) ;
#28165 = AXIS2_PLACEMENT_3D ( 'NONE', #71621, #246393, #169464 ) ;
#28166 = DIRECTION ( 'NONE',  ( 0.000000000000000000, 0.000000000000000000, -1.000000000000000000 ) ) ;
#28167 = ORIENTED_EDGE ( 'NONE', *, *, #100327, .T. ) ;
#28168 = DIRECTION ( 'NONE',  ( 1.000000000000000000, 0.000000000000000000, 0.000000000000000000 ) ) ;
#28169 = FACE_OUTER_BOUND ( 'NONE', #26326, .T. ) ;
#28171 = EDGE_CURVE ( 'NONE', #35900, #224021, #148115, .T. ) ;
#28170 = DIRECTION ( 'NONE',  ( -3.265361837132813093E-16, -1.000000000000000000, -7.086529944415894657E-15 ) ) ;
#28173 = ADVANCED_FACE ( 'NONE', ( #122872 ), #110697, .T. ) ;
#28172 = ORIENTED_EDGE ( 'NONE', *, *, #148815, .T. ) ;
#28174 = CARTESIAN_POINT ( 'NONE',  ( 23.15000000000000213, -9.499999999988844479, -57.10603087734755690 ) ) ;
#28175 = VECTOR ( 'NONE', #251630, 1000.000000000000000 ) ;
#28176 = DIRECTION ( 'NONE',  ( -4.701977403289178058E-30, 1.734723475976807094E-14, -1.000000000000000000 ) ) ;
#28177 = AXIS2_PLACEMENT_3D ( 'NONE', #110942, #13139, #50940 ) ;
#28179 = ORIENTED_EDGE ( 'NONE', *, *, #162458, .F. ) ;
#28178 = CIRCLE ( 'NONE', #65739, 11.75000000000001066 ) ;
#28180 = ORIENTED_EDGE ( 'NONE', *, *, #241854, .T. ) ;
#28181 = ADVANCED_FACE ( 'NONE', ( #22500 ), #119026, .F. ) ;
#28182 = CARTESIAN_POINT ( 'NONE',  ( -16.92507428761700083, 51.56100593717672353, -231.9723882365938152 ) ) ;
#28183 = VERTEX_POINT ( 'NONE', #1616 ) ;
#28184 = CARTESIAN_POINT ( 'NONE',  ( 21.30000000000002558, 1.115650265596050101E-11, -62.95000000000004547 ) ) ;
#28185 = PLANE ( 'NONE',  #240527 ) ;
#28187 = EDGE_CURVE ( 'NONE', #75576, #16270, #231511, .T. ) ;
#28186 = CARTESIAN_POINT ( 'NONE',  ( -20.94999675878240808, 10.29307482169071264, -206.4586421466939896 ) ) ;
#28188 = VERTEX_POINT ( 'NONE', #143699 ) ;
#28189 = EDGE_CURVE ( 'NONE', #110538, #183134, #177373, .T. ) ;
#28190 = DIRECTION ( 'NONE',  ( 1.000000000000000000, -0.000000000000000000, -0.000000000000000000 ) ) ;
#28191 = CIRCLE ( 'NONE', #157366, 0.09999999999999939493 ) ;
#28192 = FACE_OUTER_BOUND ( 'NONE', #234320, .T. ) ;
#28193 = CIRCLE ( 'NONE', #144667, 0.1000000000000028644 ) ;
#28194 = DIRECTION ( 'NONE',  ( 0.000000000000000000, 0.000000000000000000, 1.000000000000000000 ) ) ;
#28195 = DIRECTION ( 'NONE',  ( 1.000000000000000000, 3.265361837132813093E-16, -0.000000000000000000 ) ) ;
#28196 = AXIS2_PLACEMENT_3D ( 'NONE', #171279, #132103, #209069 ) ;
#28197 = ORIENTED_EDGE ( 'NONE', *, *, #248824, .T. ) ;
#28198 = CARTESIAN_POINT ( 'NONE',  ( 20.87600722750343252, 10.33112638555853913, -39.09012289269746532 ) ) ;
#28199 = AXIS2_PLACEMENT_3D ( 'NONE', #72333, #35780, #133570 ) ;
#28201 = VERTEX_POINT ( 'NONE', #182862 ) ;
#28200 = DIRECTION ( 'NONE',  ( 1.000000000000000000, 0.000000000000000000, 0.000000000000000000 ) ) ;
#28203 = EDGE_CURVE ( 'NONE', #222619, #231078, #52414, .T. ) ;
#28202 = CYLINDRICAL_SURFACE ( 'NONE', #153688, 0.09999999999999939493 ) ;
#28204 = CARTESIAN_POINT ( 'NONE',  ( 20.94999999999999574, 87.75000000001210765, -133.4231074845242233 ) ) ;
#28205 = CYLINDRICAL_SURFACE ( 'NONE', #68022, 0.5000000000000004441 ) ;
#28206 = EDGE_CURVE ( 'NONE', #174560, #231683, #111470, .T. ) ;
#28207 = DIRECTION ( 'NONE',  ( 1.000000000000000000, -1.875376730785737719E-16, -1.309568571767809260E-30 ) ) ;
#28208 = CARTESIAN_POINT ( 'NONE',  ( 21.09787244211743840, 8.775370707337266651, -12.23925338431755883 ) ) ;
#28209 = DIRECTION ( 'NONE',  ( 0.7071067811865474617, 0.7071067811865474617, 2.044391222244499837E-16 ) ) ;
#28210 = CARTESIAN_POINT ( 'NONE',  ( -20.64999999999999858, 7.250000000011155521, -112.8500000000000369 ) ) ;
#28211 = VERTEX_POINT ( 'NONE', #81146 ) ;
#28212 = CARTESIAN_POINT ( 'NONE',  ( -20.94999999999999929, -11.48912529306489994, -197.9999999999999432 ) ) ;
#28213 = DIRECTION ( 'NONE',  ( 0.000000000000000000, 0.7397890806274222131, 0.6728388485993012091 ) ) ;
#28214 = CIRCLE ( 'NONE', #161466, 0.1000000000000000472 ) ;
#28215 = AXIS2_PLACEMENT_3D ( 'NONE', #256396, #77810, #157406 ) ;
#28216 = CARTESIAN_POINT ( 'NONE',  ( -16.87036670365548474, 51.72098459467785858, -231.8575261499355236 ) ) ;
#28217 = EDGE_CURVE ( 'NONE', #59337, #138337, #27543, .T. ) ;
#28218 = TOROIDAL_SURFACE ( 'NONE', #120367, 0.2000000000000000111, 0.1000000000000000056 ) ;
#28219 = CARTESIAN_POINT ( 'NONE',  ( -18.40000000000000213, 64.25000000001188027, -90.37310748452439668 ) ) ;
#28220 = CYLINDRICAL_SURFACE ( 'NONE', #49057, 0.09999999999999990841 ) ;
#28221 = CIRCLE ( 'NONE', #20012, 0.09999999999999939493 ) ;
#28222 = ORIENTED_EDGE ( 'NONE', *, *, #100002, .F. ) ;
#28223 = ORIENTED_EDGE ( 'NONE', *, *, #145268, .F. ) ;
#28224 = DIRECTION ( 'NONE',  ( 0.000000000000000000, 0.000000000000000000, -1.000000000000000000 ) ) ;
#28225 = CARTESIAN_POINT ( 'NONE',  ( 21.07094088545367327, 0.09889370256337753906, -127.6798327780828686 ) ) ;
#28226 = CYLINDRICAL_SURFACE ( 'NONE', #91635, 0.09999999999998898659 ) ;
#28227 = DIRECTION ( 'NONE',  ( -0.000000000000000000, 0.9770955615653313941, 0.2128009952263603954 ) ) ;
#28228 = CARTESIAN_POINT ( 'NONE',  ( 22.14074124539698829, 7.390077851043746371, 0.09905289584407064862 ) ) ;
#28229 = AXIS2_PLACEMENT_3D ( 'NONE', #60597, #176725, #140129 ) ;
#28230 = EDGE_CURVE ( 'NONE', #38064, #238512, #240255, .T. ) ;
#28231 = DIRECTION ( 'NONE',  ( 1.000000000000000000, 0.000000000000000000, 0.000000000000000000 ) ) ;
#28232 = CARTESIAN_POINT ( 'NONE',  ( -21.05000000000000071, 17.11694853917243364, -224.3781540347815735 ) ) ;
#28233 = ADVANCED_FACE ( 'NONE', ( #144971 ), #92106, .T. ) ;
#28234 = AXIS2_PLACEMENT_3D ( 'NONE', #50982, #134378, #249225 ) ;
#28235 = VERTEX_POINT ( 'NONE', #210116 ) ;
#28236 = DIRECTION ( 'NONE',  ( 1.000000000000000000, 0.000000000000000000, 0.000000000000000000 ) ) ;
#28237 = EDGE_CURVE ( 'NONE', #172986, #14872, #173105, .T. ) ;
#28238 = ORIENTED_EDGE ( 'NONE', *, *, #191972, .F. ) ;
#28239 = CARTESIAN_POINT ( 'NONE',  ( 23.40000000000005542, 82.72707916847673459, -26.51159310135756897 ) ) ;
#28240 = DIRECTION ( 'NONE',  ( 1.000000000000000000, 0.000000000000000000, 0.000000000000000000 ) ) ;
#28241 = LINE ( 'NONE', #128596, #37034 ) ;
#28242 = CARTESIAN_POINT ( 'NONE',  ( 20.94999999999999929, 60.85896401437205583, -225.4389122456526025 ) ) ;
#28244 = EDGE_CURVE ( 'NONE', #123059, #95323, #27651, .T. ) ;
#28243 = CARTESIAN_POINT ( 'NONE',  ( -20.85000000000000142, 11.75000000001115197, -194.2161343370218560 ) ) ;
#28245 = CARTESIAN_POINT ( 'NONE',  ( -18.49999999999997868, -9.321008403361298988, -7.235938249077866757 ) ) ;
#28246 = CARTESIAN_POINT ( 'NONE',  ( -23.15000000000000213, 61.64632609160243248, -246.5149037406836214 ) ) ;
#28247 = ORIENTED_EDGE ( 'NONE', *, *, #155904, .F. ) ;
#28248 = CARTESIAN_POINT ( 'NONE',  ( 21.07094088545368393, 0.09889370256337753906, -94.17983277808291120 ) ) ;
#28249 = CARTESIAN_POINT ( 'NONE',  ( -23.15000000000000213, 0.000000000000000000, -33.50000000000000000 ) ) ;
#28250 = ADVANCED_FACE ( 'NONE', ( #224522 ), #127265, .T. ) ;
#28251 = CARTESIAN_POINT ( 'NONE',  ( -21.05000000000000071, 1.115600667400684642E-11, -67.00000000000004263 ) ) ;
#28252 = DIRECTION ( 'NONE',  ( 0.000000000000000000, -1.000000000000000000, 0.000000000000000000 ) ) ;
#28253 = TOROIDAL_SURFACE ( 'NONE', #15786, 11.90000000000000391, 0.1000000000000000056 ) ;
#28254 = CIRCLE ( 'NONE', #15788, 0.1000000000000028644 ) ;
#28255 = AXIS2_PLACEMENT_3D ( 'NONE', #214801, #115711, #209681 ) ;
#28256 = DIRECTION ( 'NONE',  ( -0.000000000000000000, -1.000000000000000000, -6.982962677686266711E-15 ) ) ;
#28257 = DIRECTION ( 'NONE',  ( 0.000000000000000000, -0.9770955615653316162, -0.2128009952263604232 ) ) ;
#28258 = ADVANCED_FACE ( 'NONE', ( #167158 ), #11923, .T. ) ;
#28260 = EDGE_CURVE ( 'NONE', #242599, #6865, #66745, .T. ) ;
#28259 = EDGE_CURVE ( 'NONE', #222610, #158360, #28947, .T. ) ;
#28261 = ORIENTED_EDGE ( 'NONE', *, *, #91991, .F. ) ;
#28262 = DIRECTION ( 'NONE',  ( 1.000000000000000000, 0.000000000000000000, 0.000000000000000000 ) ) ;
#28263 = DIRECTION ( 'NONE',  ( 0.000000000000000000, 2.851451713636794872E-13, 1.000000000000000000 ) ) ;
#28264 = VERTEX_POINT ( 'NONE', #130554 ) ;
#28265 = ORIENTED_EDGE ( 'NONE', *, *, #147450, .F. ) ;
#28266 = CARTESIAN_POINT ( 'NONE',  ( -16.87683809663752399, 29.49590395944699139, -234.5399335999045718 ) ) ;
#28267 = DIRECTION ( 'NONE',  ( 1.000000000000000000, 6.938893903907222067E-15, 0.000000000000000000 ) ) ;
#28268 = DIRECTION ( 'NONE',  ( 1.000000000000000000, -0.000000000000000000, -0.000000000000000000 ) ) ;
#28269 = ORIENTED_EDGE ( 'NONE', *, *, #14661, .F. ) ;
#28270 = VECTOR ( 'NONE', #237080, 1000.000000000000000 ) ;
#28271 = DIRECTION ( 'NONE',  ( 0.000000000000000000, 0.9908441862701791170, -0.1350103645450472789 ) ) ;
#28272 = CARTESIAN_POINT ( 'NONE',  ( -20.94999999999999929, 1.115600667400684642E-11, -200.9999999999999432 ) ) ;
#28273 = AXIS2_PLACEMENT_3D ( 'NONE', #17336, #57718, #156867 ) ;
#28274 = ORIENTED_EDGE ( 'NONE', *, *, #191069, .T. ) ;
#28275 = ADVANCED_FACE ( 'NONE', ( #207546 ), #90128, .T. ) ;
#28276 = EDGE_CURVE ( 'NONE', #151298, #43053, #120729, .T. ) ;
#28277 = AXIS2_PLACEMENT_3D ( 'NONE', #226900, #39634, #225591 ) ;
#28278 = LINE ( 'NONE', #222565, #185444 ) ;
#28279 = ADVANCED_FACE ( 'NONE', ( #190557 ), #87562, .F. ) ;
#28280 = ORIENTED_EDGE ( 'NONE', *, *, #153326, .F. ) ;
#28281 = CARTESIAN_POINT ( 'NONE',  ( 20.94999999999999574, 70.47363787294415260, -228.3418745167492432 ) ) ;
#28282 = DIRECTION ( 'NONE',  ( 0.000000000000000000, 0.2617529984165152257, 0.9651348961777124202 ) ) ;
#28283 = EDGE_CURVE ( 'NONE', #255303, #113692, #181457, .T. ) ;
#28284 = DIRECTION ( 'NONE',  ( 0.000000000000000000, 1.000000000000000000, 0.000000000000000000 ) ) ;
#28285 = DIRECTION ( 'NONE',  ( 1.000000000000000000, 0.000000000000000000, -0.000000000000000000 ) ) ;
#28286 = DIRECTION ( 'NONE',  ( 0.000000000000000000, 0.9856811345164803173, 0.1686199900910455851 ) ) ;
#28287 = CARTESIAN_POINT ( 'NONE',  ( -18.59999999999999787, 51.63105570370733233, -253.2535652827696424 ) ) ;
#28288 = EDGE_CURVE ( 'NONE', #71547, #224195, #206559, .T. ) ;
#28289 = DIRECTION ( 'NONE',  ( -1.000000000000000000, -7.304098846218105085E-16, -4.217023435051676515E-16 ) ) ;
#28290 = CARTESIAN_POINT ( 'NONE',  ( -21.64999999999999858, 7.250000000011148416, -188.7499999999999716 ) ) ;
#28291 = CARTESIAN_POINT ( 'NONE',  ( -18.59999999999999787, 43.35377423437995503, -245.1717807829448930 ) ) ;
#28293 = ORIENTED_EDGE ( 'NONE', *, *, #142597, .T. ) ;
#28292 = LINE ( 'NONE', #8694, #73519 ) ;
#28294 = ORIENTED_EDGE ( 'NONE', *, *, #163309, .F. ) ;
#28296 = CARTESIAN_POINT ( 'NONE',  ( -20.64999999999999858, 1.115600667400684642E-11, -67.00000000000004263 ) ) ;
#28295 = DIRECTION ( 'NONE',  ( 0.000000000000000000, -0.000000000000000000, -1.000000000000000000 ) ) ;
#28298 = ORIENTED_EDGE ( 'NONE', *, *, #139158, .F. ) ;
#28297 = DIRECTION ( 'NONE',  ( 1.000000000000000000, -0.000000000000000000, -0.000000000000000000 ) ) ;
#28299 = AXIS2_PLACEMENT_3D ( 'NONE', #79710, #75878, #39351 ) ;
#28300 = ORIENTED_EDGE ( 'NONE', *, *, #122048, .T. ) ;
#28301 = DIRECTION ( 'NONE',  ( 1.000000000000000000, 0.000000000000000000, 0.000000000000000000 ) ) ;
#28303 = CARTESIAN_POINT ( 'NONE',  ( 18.59999999999999787, -1.249999999988843369, -74.80048075441507649 ) ) ;
#28302 = AXIS2_PLACEMENT_3D ( 'NONE', #228485, #188064, #49827 ) ;
#28304 = DIRECTION ( 'NONE',  ( 0.000000000000000000, 0.000000000000000000, -1.000000000000000000 ) ) ;
#28305 = CARTESIAN_POINT ( 'NONE',  ( -20.94403535211772294, 10.30632246271647467, -173.0041836778896140 ) ) ;
#28306 = EDGE_CURVE ( 'NONE', #128012, #79795, #177423, .T. ) ;
#28307 = EDGE_CURVE ( 'NONE', #158135, #124226, #116148, .T. ) ;
#28308 = DIRECTION ( 'NONE',  ( -0.000000000000000000, -1.000000000000000000, -1.734723475976807292E-15 ) ) ;
#28310 = CIRCLE ( 'NONE', #90614, 0.3999999999999975797 ) ;
#28309 = DIRECTION ( 'NONE',  ( 0.000000000000000000, -0.2128009952263403282, 0.9770955615653358350 ) ) ;
#28311 = EDGE_CURVE ( 'NONE', #232107, #181313, #152616, .T. ) ;
#28312 = EDGE_LOOP ( 'NONE', ( #115394, #123553, #75543, #164624 ) ) ;
#28313 = ORIENTED_EDGE ( 'NONE', *, *, #185110, .F. ) ;
#28314 = LINE ( 'NONE', #30878, #177243 ) ;
#28315 = CIRCLE ( 'NONE', #61606, 0.1000000000000028644 ) ;
#28316 = CIRCLE ( 'NONE', #144787, 0.1000000000000028644 ) ;
#28317 = ORIENTED_EDGE ( 'NONE', *, *, #137570, .F. ) ;
#28318 = CARTESIAN_POINT ( 'NONE',  ( 20.12500000000000000, 66.25000000001232081, -161.9113362024101548 ) ) ;
#28319 = ORIENTED_EDGE ( 'NONE', *, *, #155869, .F. ) ;
#28321 = CARTESIAN_POINT ( 'NONE',  ( -16.81931177881023132, 9.936996059515063706, -154.7732178786172597 ) ) ;
#28320 = AXIS2_PLACEMENT_3D ( 'NONE', #146883, #46508, #246014 ) ;
#28322 = AXIS2_PLACEMENT_3D ( 'NONE', #9472, #185548, #125568 ) ;
#28323 = CARTESIAN_POINT ( 'NONE',  ( 21.05000000000000071, 1.162701749949165642, -141.9000000000000341 ) ) ;
#28324 = ADVANCED_FACE ( 'NONE', ( #156582 ), #196943, .F. ) ;
#28325 = VECTOR ( 'NONE', #166090, 1000.000000000000000 ) ;
#28326 = CARTESIAN_POINT ( 'NONE',  ( 20.94999999999999574, -11.41227409413852989, -137.0000000000000000 ) ) ;
#28327 = FACE_OUTER_BOUND ( 'NONE', #252103, .T. ) ;
#28328 = EDGE_LOOP ( 'NONE', ( #164592, #208017, #75831, #10279 ) ) ;
#28329 = CARTESIAN_POINT ( 'NONE',  ( -20.94999999999999929, 87.39257802171759693, -106.0970570643561501 ) ) ;
#28330 = ORIENTED_EDGE ( 'NONE', *, *, #201735, .T. ) ;
#28331 = DIRECTION ( 'NONE',  ( 0.000000000000000000, 0.000000000000000000, 1.000000000000000000 ) ) ;
#28332 = DIRECTION ( 'NONE',  ( -1.000000000000000000, 0.000000000000000000, 0.000000000000000000 ) ) ;
#28333 = CARTESIAN_POINT ( 'NONE',  ( 20.95429402530545815, 8.876194151113343977, -109.0230866979378703 ) ) ;
#28334 = CARTESIAN_POINT ( 'NONE',  ( -21.14999999999999858, 11.75000000001115552, -100.6000000000000369 ) ) ;
#28335 = VERTEX_POINT ( 'NONE', #15783 ) ;
#28336 = CARTESIAN_POINT ( 'NONE',  ( 21.05000000000000071, 11.60000000001116227, -194.0717967697244717 ) ) ;
#28337 = CIRCLE ( 'NONE', #215720, 0.09999999999999939493 ) ;
#28338 = ORIENTED_EDGE ( 'NONE', *, *, #39739, .T. ) ;
#28341 = ORIENTED_EDGE ( 'NONE', *, *, #34418, .T. ) ;
#28340 = CARTESIAN_POINT ( 'NONE',  ( 18.49999999999998934, 46.33035574435032800, -243.0552603638194284 ) ) ;
#28339 = CARTESIAN_POINT ( 'NONE',  ( -21.05000000000000071, 1.736257131608553550, -112.0686523290175245 ) ) ;
#28342 = ADVANCED_FACE ( 'NONE', ( #18315 ), #191853, .T. ) ;
#28343 = PLANE ( 'NONE',  #214509 ) ;
#28344 = CIRCLE ( 'NONE', #144812, 0.09999999999999799327 ) ;
#28345 = EDGE_LOOP ( 'NONE', ( #200354, #23836, #212849, #113937 ) ) ;
#28346 = AXIS2_PLACEMENT_3D ( 'NONE', #58509, #138052, #234599 ) ;
#28347 = DIRECTION ( 'NONE',  ( 1.000000000000000000, 0.000000000000000000, 0.000000000000000000 ) ) ;
#28348 = ORIENTED_EDGE ( 'NONE', *, *, #47014, .T. ) ;
#28349 = AXIS2_PLACEMENT_3D ( 'NONE', #61705, #158277, #196083 ) ;
#28350 = AXIS2_PLACEMENT_3D ( 'NONE', #195416, #235788, #58413 ) ;
#28351 = DIRECTION ( 'NONE',  ( 1.000000000000000000, 0.000000000000000000, 0.000000000000000000 ) ) ;
#28352 = AXIS2_PLACEMENT_3D ( 'NONE', #39885, #119402, #198924 ) ;
#28353 = DIRECTION ( 'NONE',  ( 0.000000000000000000, 0.8814952561688429444, -0.4721928772777345684 ) ) ;
#28354 = DIRECTION ( 'NONE',  ( 0.000000000000000000, 0.000000000000000000, -1.000000000000000000 ) ) ;
#28355 = DIRECTION ( 'NONE',  ( 0.000000000000000000, -0.4088369013363281068, 0.9126074666063770380 ) ) ;
#28356 = ORIENTED_EDGE ( 'NONE', *, *, #2647, .T. ) ;
#28357 = CYLINDRICAL_SURFACE ( 'NONE', #65037, 0.09999999999999939493 ) ;
#28358 = DIRECTION ( 'NONE',  ( 0.000000000000000000, 0.2741185865636956431, 0.9616958981405304696 ) ) ;
#28359 = CARTESIAN_POINT ( 'NONE',  ( 18.50000324121758055, 10.29307482169091692, -139.4586421466940180 ) ) ;
#28360 = VECTOR ( 'NONE', #57901, 1000.000000000000000 ) ;
#28361 = ORIENTED_EDGE ( 'NONE', *, *, #179370, .F. ) ;
#28362 = CARTESIAN_POINT ( 'NONE',  ( -21.95218792049438861, 0.09902843979991576839, 7.201507561246681455 ) ) ;
#28364 = ORIENTED_EDGE ( 'NONE', *, *, #78214, .F. ) ;
#28363 = AXIS2_PLACEMENT_3D ( 'NONE', #138587, #60362, #218137 ) ;
#28366 = VECTOR ( 'NONE', #49966, 1000.000000000000000 ) ;
#28365 = CARTESIAN_POINT ( 'NONE',  ( 23.14999999999999858, 76.00000000001237765, -170.0231074845243597 ) ) ;
#28367 = CLOSED_SHELL ( 'NONE', ( #85171, #225757, #59979, #8922, #34384, #222781, #6156, #137693, #195828, #18317, #84682, #213387, #171641, #41237, #183770, #8917, #216929, #84126, #168912, #51494, #160944, #152412, #47626, #257186, #179686, #3854, #175599, #193667, #144443, #81661, #77805, #165092, #116227, #31666, #184112, #214809, #54397, #94849, #196901, #109992, #50992, #63126, #146222, #219546, #169203, #75931, #102043, #157875, #213294, #240558, #183087, #9018, #255474, #221547, #224614, #75302, #116199, #27171, #44988, #55305, #133034, #214441, #102277, #168699, #159117, #220203, #210398, #1977, #171647, #25033, #154998, #54040, #24850, #31155, #109078, #12811, #15811, #181680, #185735, #121269, #159621, #182142, #2418, #35257, #100985, #233115, #164739, #253595, #203935, #220931, #123739, #10854, #63401, #17005, #51531, #50339, #66110, #122471, #175383, #239572, #121617, #244577, #158532, #82793, #121821, #240233, #110129, #183215, #223834, #86482, #182936, #31418, #31411, #76185, #6681, #130737, #13093, #225335, #109278, #178425, #108022, #162659, #49702, #96649, #229052, #223039, #246495, #82029, #143550, #145153, #202137, #123291, #207509, #102686, #171851, #253261, #125573, #74196, #85892, #98172, #69377, #236654, #185969, #190896, #182141, #228432, #134655, #235158, #34281, #125898, #5216, #77095, #83088, #245672, #47811, #77654, #12181, #246563, #4371, #225245, #220250, #39657, #49961, #202641, #203403, #10819, #79791, #172060, #100357, #191165, #86587, #240946, #220113, #154448, #210091, #47044, #196504, #112966, #170838, #72213, #78599, #41570, #142069, #249602, #232410, #173362, #257361, #185408, #24364, #84092, #44197, #105341, #105476, #142076, #8556, #215184, #32577, #145400, #162259, #100659, #208562, #209185, #4899, #95014, #250461, #95260, #12518, #205175, #43817, #172504, #88482, #161769, #74084, #14923, #96605, #157399, #27478, #218660, #189764, #149446, #37840, #23614, #130038, #4571, #200769, #155136, #241572, #110554, #64131, #225406, #190092, #234216, #205349, #206864, #229907, #95641, #200467, #112534, #93040, #49781, #20833, #257398, #238716, #202712, #100991, #100254, #63927, #191122, #54318, #17565, #257959, #207612, #145321, #9418, #233566, #231438, #106509, #88117, #124055, #93026, #19288, #79676, #98525, #159101, #15162, #55240, #74898, #81624, #217755, #230039, #184786, #217662, #134425, #105511, #177310, #156260, #41653, #32038, #134362, #43498, #65067, #20215, #214086, #106351, #237908, #47587, #102880, #134589, #73387, #9999, #82982, #165125, #120669, #36065, #246394, #142336, #72053, #106686, #243944, #78494, #188990, #143585, #226024, #23689, #211939, #26826, #12526, #254531, #156914, #4702, #28258, #106500, #157021, #117347, #232228, #174774, #254716, #145968, #208622, #47388, #258006, #167517, #121834, #87209, #251149, #36758, #91124, #193167, #242603, #210077, #164005, #164882, #158984, #147560, #104498, #28275, #56099, #96470, #73428, #18335, #187543, #132911, #209008, #21863, #78850, #120069, #173107, #100662, #116646, #238936, #93928, #52052, #18172, #26410, #117466, #245965, #234237, #227814, #8022, #142848, #28233, #182796, #154479, #242499, #119414, #51539, #100755, #7491, #22021, #20424, #112613, #46427, #7784, #124078, #15175, #59371, #89768, #77496, #41987, #194498, #112865, #180714, #212189, #181003, #124821, #219493, #88107, #252214, #119373, #94043, #232176, #136902, #228979, #87720, #105853, #194846, #246188, #32008, #57879, #186883, #175989, #44690, #171259, #221969, #75550, #43712, #132953, #1050, #85849, #211648, #242643, #29112, #238384, #253994, #178404, #83210, #93598, #228356, #41433, #122977, #162229, #34258, #100867, #80921, #107262, #98022, #256714, #165254, #87603, #164617, #155716, #54466, #81074, #2818, #42858, #114785, #188534, #145166, #256366, #27976, #100801, #157815, #249517, #202158, #83326, #236504, #109908, #16968, #69911, #106646, #142434, #107155, #121959, #18545, #115936, #166552, #96166, #161586, #214381, #44269, #255606, #36897, #72892, #45282, #22234, #72147, #232686, #119679, #231871, #244469, #167961, #186139, #245176, #69738, #243941, #161852, #211673, #30540 ) ) ;
#28368 = CARTESIAN_POINT ( 'NONE',  ( -16.87036670365549895, 9.989418819312803066, -146.5204398826979855 ) ) ;
#28370 = EDGE_LOOP ( 'NONE', ( #20998, #98900, #188652, #222905 ) ) ;
#28369 = CARTESIAN_POINT ( 'NONE',  ( -16.85697194749148409, 44.41252758811717882, -235.2202446609966842 ) ) ;
#28371 = DIRECTION ( 'NONE',  ( 0.000000000000000000, 0.000000000000000000, 1.000000000000000000 ) ) ;
#28372 = DIRECTION ( 'NONE',  ( -1.000000000000000000, -0.000000000000000000, -0.000000000000000000 ) ) ;
#28373 = AXIS2_PLACEMENT_3D ( 'NONE', #217312, #196477, #98627 ) ;
#28374 = EDGE_CURVE ( 'NONE', #37339, #188850, #13195, .T. ) ;
#28375 = CARTESIAN_POINT ( 'NONE',  ( -20.85000000000000142, -1.835859311432481045, -179.0044391687985410 ) ) ;
#28376 = CIRCLE ( 'NONE', #136459, 4.000000000000003553 ) ;
#28377 = ORIENTED_EDGE ( 'NONE', *, *, #249733, .F. ) ;
#28378 = DIRECTION ( 'NONE',  ( 1.000000000000000000, 0.000000000000000000, 0.000000000000000000 ) ) ;
#28379 = CARTESIAN_POINT ( 'NONE',  ( 18.46921299892756352, 85.50937817783609773, -163.0365287751538972 ) ) ;
#28380 = CIRCLE ( 'NONE', #90872, 0.09999999999998898659 ) ;
#28381 = VERTEX_POINT ( 'NONE', #233529 ) ;
#28382 = CARTESIAN_POINT ( 'NONE',  ( -16.94062896051973865, 9.992719105111833144, -146.6025165421188206 ) ) ;
#28383 = VERTEX_POINT ( 'NONE', #92705 ) ;
#28384 = AXIS2_PLACEMENT_3D ( 'NONE', #182985, #164697, #4315 ) ;
#28385 = FACE_OUTER_BOUND ( 'NONE', #235835, .T. ) ;
#28387 = ORIENTED_EDGE ( 'NONE', *, *, #167127, .T. ) ;
#28386 = CARTESIAN_POINT ( 'NONE',  ( -21.05000000000000071, 76.00000000001213607, -136.5231074845242745 ) ) ;
#28388 = EDGE_CURVE ( 'NONE', #253291, #198296, #23431, .T. ) ;
#28389 = AXIS2_PLACEMENT_3D ( 'NONE', #87001, #144405, #44055 ) ;
#28390 = EDGE_CURVE ( 'NONE', #118038, #151518, #94305, .T. ) ;
#28393 = ORIENTED_EDGE ( 'NONE', *, *, #147841, .F. ) ;
#28392 = ORIENTED_EDGE ( 'NONE', *, *, #117314, .F. ) ;
#28391 = DIRECTION ( 'NONE',  ( -0.000000000000000000, -0.000000000000000000, -1.000000000000000000 ) ) ;
#28394 = FACE_OUTER_BOUND ( 'NONE', #16629, .T. ) ;
#28395 = TOROIDAL_SURFACE ( 'NONE', #215602, 0.6000000000000017542, 0.1000000000000000056 ) ;
#28396 = DIRECTION ( 'NONE',  ( -1.000000000000000000, -0.000000000000000000, -0.000000000000000000 ) ) ;
#28397 = AXIS2_PLACEMENT_3D ( 'NONE', #14392, #92596, #30100 ) ;
#28399 = CARTESIAN_POINT ( 'NONE',  ( -15.15564720441980562, 66.58929125296442919, -51.45389907868027990 ) ) ;
#28398 = DIRECTION ( 'NONE',  ( 0.000000000000000000, -8.673617379883786823E-14, 1.000000000000000000 ) ) ;
#28400 = CARTESIAN_POINT ( 'NONE',  ( -18.59999999999999787, 77.26178616857765746, -195.4366085209788935 ) ) ;
#28401 = DIRECTION ( 'NONE',  ( 0.000000000000000000, 6.982962677686266711E-15, -1.000000000000000000 ) ) ;
#28402 = ADVANCED_FACE ( 'NONE', ( #134388 ), #173597, .F. ) ;
#28403 = DIRECTION ( 'NONE',  ( 0.000000000000000000, 0.8814952561688437216, -0.4721928772777334582 ) ) ;
#28404 = AXIS2_PLACEMENT_3D ( 'NONE', #217550, #162753, #18082 ) ;
#28405 = LINE ( 'NONE', #188715, #254829 ) ;
#28406 = ORIENTED_EDGE ( 'NONE', *, *, #59246, .T. ) ;
#28407 = ORIENTED_EDGE ( 'NONE', *, *, #223415, .T. ) ;
#28408 = ADVANCED_FACE ( 'NONE', ( #172309, #213952 ), #35352, .T. ) ;
#28409 = CARTESIAN_POINT ( 'NONE',  ( -21.05000000000000071, 64.25000000001175238, -76.53791325517833855 ) ) ;
#28412 = ORIENTED_EDGE ( 'NONE', *, *, #2855, .T. ) ;
#28411 = EDGE_CURVE ( 'NONE', #48521, #223292, #123357, .T. ) ;
#28410 = CARTESIAN_POINT ( 'NONE',  ( -23.25000000000000000, 4.150000000011156764, -155.1500000000000057 ) ) ;
#28413 = ORIENTED_EDGE ( 'NONE', *, *, #256561, .T. ) ;
#28414 = DIRECTION ( 'NONE',  ( 0.000000000000000000, 1.000000000000000000, 0.000000000000000000 ) ) ;
#28415 = VERTEX_POINT ( 'NONE', #36631 ) ;
#28416 = DIRECTION ( 'NONE',  ( 0.000000000000000000, 0.000000000000000000, -1.000000000000000000 ) ) ;
#28417 = EDGE_CURVE ( 'NONE', #54485, #208784, #185882, .T. ) ;
#28418 = AXIS2_PLACEMENT_3D ( 'NONE', #42998, #57396, #37878 ) ;
#28419 = ORIENTED_EDGE ( 'NONE', *, *, #195233, .F. ) ;
#28420 = ADVANCED_FACE ( 'NONE', ( #155295 ), #215236, .T. ) ;
#28421 = FACE_OUTER_BOUND ( 'NONE', #16522, .T. ) ;
#28422 = DIRECTION ( 'NONE',  ( 0.000000000000000000, 7.056502275159890832E-15, -1.000000000000000000 ) ) ;
#28423 = CIRCLE ( 'NONE', #183175, 11.64999999999999325 ) ;
#28425 = VERTEX_POINT ( 'NONE', #211389 ) ;
#28424 = ORIENTED_EDGE ( 'NONE', *, *, #63427, .T. ) ;
#28426 = VERTEX_POINT ( 'NONE', #56137 ) ;
#28427 = CARTESIAN_POINT ( 'NONE',  ( -20.94999999999999929, -1.851028230140860487, -11.65391326942249250 ) ) ;
#28428 = EDGE_LOOP ( 'NONE', ( #149983, #237374, #201953, #16005 ) ) ;
#28429 = EDGE_LOOP ( 'NONE', ( #69999, #114677, #1810, #83793 ) ) ;
#28430 = DIRECTION ( 'NONE',  ( -1.000000000000000000, 1.335000415235278971E-16, -2.979993593738921214E-16 ) ) ;
#28431 = CARTESIAN_POINT ( 'NONE',  ( -23.15000000000000213, 49.61306877027904250, -254.2671747026441551 ) ) ;
#28432 = FACE_OUTER_BOUND ( 'NONE', #134836, .T. ) ;
#28434 = VERTEX_POINT ( 'NONE', #232253 ) ;
#28433 = CARTESIAN_POINT ( 'NONE',  ( -20.94999999999999929, 7.070967871809997973, -104.2465642218683541 ) ) ;
#28435 = DIRECTION ( 'NONE',  ( -1.000000000000000000, 0.000000000000000000, 0.000000000000000000 ) ) ;
#28436 = DIRECTION ( 'NONE',  ( 0.000000000000000000, 0.9126074666063660468, 0.4088369013363524762 ) ) ;
#28438 = ORIENTED_EDGE ( 'NONE', *, *, #213625, .T. ) ;
#28437 = DIRECTION ( 'NONE',  ( -1.000000000000000000, -0.000000000000000000, -0.000000000000000000 ) ) ;
#28439 = VERTEX_POINT ( 'NONE', #53596 ) ;
#28440 = DIRECTION ( 'NONE',  ( 0.000000000000000000, -0.6728971962616783209, -0.7397360091702797069 ) ) ;
#28442 = EDGE_CURVE ( 'NONE', #36614, #216103, #206734, .T. ) ;
#28441 = EDGE_LOOP ( 'NONE', ( #17417, #39199, #171847, #255 ) ) ;
#28443 = CARTESIAN_POINT ( 'NONE',  ( 18.49999999999999289, 8.980461154494401299, -187.0187154576991304 ) ) ;
#28444 = CARTESIAN_POINT ( 'NONE',  ( 16.27683809663750125, 9.350000000011137402, -109.7500000000000426 ) ) ;
#28445 = ORIENTED_EDGE ( 'NONE', *, *, #113747, .T. ) ;
#28446 = AXIS2_PLACEMENT_3D ( 'NONE', #34294, #113792, #155527 ) ;
#28449 = DIRECTION ( 'NONE',  ( 1.000000000000000000, 0.000000000000000000, 0.000000000000000000 ) ) ;
#28448 = TOROIDAL_SURFACE ( 'NONE', #232442, 12.97499999999999787, 0.1000000000000000056 ) ;
#28447 = CARTESIAN_POINT ( 'NONE',  ( -22.39999999999999503, 76.00000000001273293, -211.3138870828977645 ) ) ;
#28450 = AXIS2_PLACEMENT_3D ( 'NONE', #97069, #176671, #235332 ) ;
#28451 = CYLINDRICAL_SURFACE ( 'NONE', #39050, 0.5000000000000004441 ) ;
#28452 = DIRECTION ( 'NONE',  ( 1.000000000000000000, 0.000000000000000000, 0.000000000000000000 ) ) ;
#28453 = CARTESIAN_POINT ( 'NONE',  ( -20.85000000000000142, 70.22659352830977753, -197.9852579278363578 ) ) ;
#28454 = ORIENTED_EDGE ( 'NONE', *, *, #242764, .F. ) ;
#28455 = VERTEX_POINT ( 'NONE', #24767 ) ;
#28456 = EDGE_CURVE ( 'NONE', #245309, #157060, #177559, .T. ) ;
#28457 = CARTESIAN_POINT ( 'NONE',  ( 20.94999999999999929, -8.999999999988842703, -57.10603087734755690 ) ) ;
#28458 = DIRECTION ( 'NONE',  ( 0.000000000000000000, -1.000000000000000000, -6.982962677686265922E-15 ) ) ;
#28459 = VERTEX_POINT ( 'NONE', #43024 ) ;
#28460 = ORIENTED_EDGE ( 'NONE', *, *, #124780, .F. ) ;
#28461 = CARTESIAN_POINT ( 'NONE',  ( -22.50000000000088463, 0.04536165659888222873, -55.34949116579123540 ) ) ;
#28462 = ORIENTED_EDGE ( 'NONE', *, *, #173952, .T. ) ;
#28463 =( LENGTH_UNIT ( ) NAMED_UNIT ( * ) SI_UNIT ( .MILLI., .METRE. ) );
#28464 = DIRECTION ( 'NONE',  ( 0.000000000000000000, -1.000000000000000000, -0.000000000000000000 ) ) ;
#28465 = CARTESIAN_POINT ( 'NONE',  ( 18.59999999999999076, 54.95667902235472013, -229.8578999281555753 ) ) ;
#28466 = VECTOR ( 'NONE', #52539, 1000.000000000000114 ) ;
#28467 = ORIENTED_EDGE ( 'NONE', *, *, #137886, .F. ) ;
#28468 = CIRCLE ( 'NONE', #249200, 0.09999999999999939493 ) ;
#28469 = CARTESIAN_POINT ( 'NONE',  ( -16.77779411440718249, 63.08607716446275049, -213.1412442136428922 ) ) ;
#28470 =( BOUNDED_CURVE ( )  B_SPLINE_CURVE ( 3, ( #69688, #194775, #149224, #153099 ),
 .UNSPECIFIED., .F., .T. ) 
 B_SPLINE_CURVE_WITH_KNOTS ( ( 4, 4 ),
 ( 3.141592653589791784, 4.712388980384688786 ),
 .UNSPECIFIED. ) 
 CURVE ( )  GEOMETRIC_REPRESENTATION_ITEM ( )  RATIONAL_B_SPLINE_CURVE ( ( 1.000000000000000000, 0.8047378541243649375, 0.8047378541243649375, 1.000000000000000000 ) ) 
 REPRESENTATION_ITEM ( '' )  );
#28471 = EDGE_CURVE ( 'NONE', #116664, #244409, #127444, .T. ) ;
#28472 = EDGE_LOOP ( 'NONE', ( #243184, #223803, #139535 ) ) ;
#28473 = CIRCLE ( 'NONE', #249203, 4.299999999999953637 ) ;
#28474 = ORIENTED_EDGE ( 'NONE', *, *, #147968, .T. ) ;
#28475 = ORIENTED_EDGE ( 'NONE', *, *, #110319, .F. ) ;
#28476 = DIRECTION ( 'NONE',  ( 1.000000000000000000, -0.000000000000000000, -0.000000000000000000 ) ) ;
#28477 = CARTESIAN_POINT ( 'NONE',  ( -23.15000000000000213, 70.88170441948386724, -234.2197789011331679 ) ) ;
#28478 = DIRECTION ( 'NONE',  ( -0.000000000000000000, 3.469446951953635015E-14, 1.000000000000000000 ) ) ;
#28479 = CARTESIAN_POINT ( 'NONE',  ( -23.25000000000000000, 5.950000000011167245, -123.6942976949652149 ) ) ;
#28480 = CARTESIAN_POINT ( 'NONE',  ( -16.86337532320260735, 9.979967204224358568, -20.94892446898280980 ) ) ;
#28481 = EDGE_CURVE ( 'NONE', #21796, #39612, #227399, .T. ) ;
#28483 = CARTESIAN_POINT ( 'NONE',  ( 21.05281448260627641, 8.776010158537628669, -12.17355791181142344 ) ) ;
#28482 = CYLINDRICAL_SURFACE ( 'NONE', #20500, 0.09999999999999939493 ) ;
#28485 = ORIENTED_EDGE ( 'NONE', *, *, #97652, .T. ) ;
#28484 = CARTESIAN_POINT ( 'NONE',  ( -23.15000000000000213, 67.23127455305841238, -235.8551265064783991 ) ) ;
#28486 = DIRECTION ( 'NONE',  ( 1.000000000000000000, -0.000000000000000000, -0.000000000000000000 ) ) ;
#28487 = ORIENTED_EDGE ( 'NONE', *, *, #95490, .F. ) ;
#28488 = CARTESIAN_POINT ( 'NONE',  ( 20.94999999999999929, -1.835341550213257733, -78.55515129256303908 ) ) ;
#28489 = ORIENTED_EDGE ( 'NONE', *, *, #204143, .T. ) ;
#28490 = ORIENTED_EDGE ( 'NONE', *, *, #10066, .F. ) ;
#28491 = DIRECTION ( 'NONE',  ( 0.000000000000000000, 0.9984213852963246261, 0.05616704890741601452 ) ) ;
#28492 = CARTESIAN_POINT ( 'NONE',  ( 23.14999999999999858, 71.00000000001223555, -148.9283735034374843 ) ) ;
#28494 = EDGE_CURVE ( 'NONE', #151867, #127058, #41755, .T. ) ;
#28493 = DIRECTION ( 'NONE',  ( 0.000000000000000000, -6.982962677686266711E-15, 1.000000000000000000 ) ) ;
#28495 = EDGE_CURVE ( 'NONE', #6502, #59214, #40173, .T. ) ;
#28496 = DIRECTION ( 'NONE',  ( 0.000000000000000000, 0.1350103645451876666, 0.9908441862701600211 ) ) ;
#28497 = AXIS2_PLACEMENT_3D ( 'NONE', #106666, #101515, #123698 ) ;
#28498 = ADVANCED_FACE ( 'NONE', ( #19613 ), #160794, .T. ) ;
#28499 = CIRCLE ( 'NONE', #228372, 12.87499999999999822 ) ;
#28500 = AXIS2_PLACEMENT_3D ( 'NONE', #239558, #256483, #36245 ) ;
#28501 = CARTESIAN_POINT ( 'NONE',  ( 23.15000000000000213, 84.59626168225477727, -78.97323500167453858 ) ) ;
#28502 = ORIENTED_EDGE ( 'NONE', *, *, #51340, .F. ) ;
#28503 = ORIENTED_EDGE ( 'NONE', *, *, #150151, .T. ) ;
#28504 = EDGE_CURVE ( 'NONE', #171429, #192475, #161701, .T. ) ;
#28505 = CARTESIAN_POINT ( 'NONE',  ( 18.59999999999999432, 77.29973367124252093, -79.49497796165491081 ) ) ;
#28506 = ORIENTED_EDGE ( 'NONE', *, *, #193578, .F. ) ;
#28507 = DIRECTION ( 'NONE',  ( 0.000000000000000000, 0.000000000000000000, 1.000000000000000000 ) ) ;
#28508 = DIRECTION ( 'NONE',  ( 0.000000000000000000, 0.9126074666063769270, 0.4088369013363280513 ) ) ;
#28509 = VERTEX_POINT ( 'NONE', #79549 ) ;
#28511 = CARTESIAN_POINT ( 'NONE',  ( 20.94999999999999574, 77.16270174995034381, -161.9231074845243370 ) ) ;
#28510 = TOROIDAL_SURFACE ( 'NONE', #49303, 2.100000000000002309, 0.1000000000000000056 ) ;
#28512 = CARTESIAN_POINT ( 'NONE',  ( 20.84999999999998721, 11.75000000001115552, -200.9999999999999432 ) ) ;
#28513 = DIRECTION ( 'NONE',  ( 1.000000000000000000, 0.000000000000000000, 0.000000000000000000 ) ) ;
#28514 = ORIENTED_EDGE ( 'NONE', *, *, #139148, .F. ) ;
#28515 = CARTESIAN_POINT ( 'NONE',  ( -22.59999999999999787, 64.25043287652275126, -136.6239658536230763 ) ) ;
#28516 = CARTESIAN_POINT ( 'NONE',  ( -20.94999999999999929, 11.60000000001115161, -140.9282032302755852 ) ) ;
#28517 = DIRECTION ( 'NONE',  ( 0.000000000000000000, -0.4088369013363281623, 0.9126074666063771490 ) ) ;
#28518 = DIRECTION ( 'NONE',  ( 0.000000000000000000, 6.982962677686266711E-15, -1.000000000000000000 ) ) ;
#28519 = DIRECTION ( 'NONE',  ( -3.265361837132813093E-16, -1.000000000000000000, -6.982962677686266711E-15 ) ) ;
#28520 = CIRCLE ( 'NONE', #149103, 7.899999999999990585 ) ;
#28521 = DIRECTION ( 'NONE',  ( 0.000000000000000000, 0.1335171055202867274, -0.9910465087640866200 ) ) ;
#28522 = AXIS2_PLACEMENT_3D ( 'NONE', #32975, #112479, #257058 ) ;
#28523 = CIRCLE ( 'NONE', #240858, 0.09999999999999939493 ) ;
#28524 = ADVANCED_FACE ( 'NONE', ( #83390 ), #106772, .T. ) ;
#28525 = ORIENTED_EDGE ( 'NONE', *, *, #223054, .F. ) ;
#28526 = CIRCLE ( 'NONE', #103281, 0.1000000000000028644 ) ;
#28527 = CARTESIAN_POINT ( 'NONE',  ( 20.27550659511088682, 66.78395627750374786, -190.8731074845244393 ) ) ;
#28528 = ORIENTED_EDGE ( 'NONE', *, *, #82816, .T. ) ;
#28529 = EDGE_CURVE ( 'NONE', #138960, #171330, #20969, .T. ) ;
#28530 = EDGE_CURVE ( 'NONE', #96628, #210104, #256566, .T. ) ;
#28531 = FACE_OUTER_BOUND ( 'NONE', #238433, .T. ) ;
#28532 = DIRECTION ( 'NONE',  ( -0.000000000000000000, -0.000000000000000000, -1.000000000000000000 ) ) ;
#28533 = CARTESIAN_POINT ( 'NONE',  ( -18.79999999999999716, 1.800000000000000044, -11.61130914238355771 ) ) ;
#28534 = CARTESIAN_POINT ( 'NONE',  ( 20.52683494730046476, 67.01946918171096002, -161.5178547619902076 ) ) ;
#28535 = VECTOR ( 'NONE', #219008, 1000.000000000000000 ) ;
#28536 = ORIENTED_EDGE ( 'NONE', *, *, #58658, .T. ) ;
#28537 = CARTESIAN_POINT ( 'NONE',  ( 23.15000000000000213, 87.75000000001186606, -90.77310748452423184 ) ) ;
#28538 = CARTESIAN_POINT ( 'NONE',  ( -20.85000000000000142, 7.021664781911246322, -171.1335654018973003 ) ) ;
#28539 = CARTESIAN_POINT ( 'NONE',  ( -18.50000000000000000, 74.36282728704119904, -57.94095411905231430 ) ) ;
#28540 = DIRECTION ( 'NONE',  ( 0.000000000000000000, 0.000000000000000000, -1.000000000000000000 ) ) ;
#28541 = VECTOR ( 'NONE', #81121, 1000.000000000000000 ) ;
#28542 = CIRCLE ( 'NONE', #111689, 0.1000000000000017680 ) ;
#28543 = LINE ( 'NONE', #244965, #140450 ) ;
#28544 = CIRCLE ( 'NONE', #203465, 0.09999999999999939493 ) ;
#28545 = VECTOR ( 'NONE', #22285, 1000.000000000000000 ) ;
#28547 = ORIENTED_EDGE ( 'NONE', *, *, #54054, .T. ) ;
#28546 = AXIS2_PLACEMENT_3D ( 'NONE', #182691, #166, #80983 ) ;
#28548 = ORIENTED_EDGE ( 'NONE', *, *, #221459, .F. ) ;
#28549 = DIRECTION ( 'NONE',  ( 1.000000000000000000, 0.000000000000000000, 0.000000000000000000 ) ) ;
#28551 = DIRECTION ( 'NONE',  ( 1.000000000000000000, 0.000000000000000000, 0.000000000000000000 ) ) ;
#28550 = VECTOR ( 'NONE', #68715, 1000.000000000000000 ) ;
#28552 = DIRECTION ( 'NONE',  ( -1.000000000000000000, 1.207181226542539700E-16, -2.694675058168174199E-16 ) ) ;
#28553 = CARTESIAN_POINT ( 'NONE',  ( 23.14999999999999858, 76.00000000001170974, -69.52310748452431710 ) ) ;
#28554 = DIRECTION ( 'NONE',  ( 0.000000000000000000, 0.9126074666064696306, 0.4088369013361213278 ) ) ;
#28555 = AXIS2_PLACEMENT_3D ( 'NONE', #185836, #26796, #159880 ) ;
#28556 = VERTEX_POINT ( 'NONE', #82109 ) ;
#28557 = DIRECTION ( 'NONE',  ( 0.000000000000000000, 0.2128009952263603954, -0.9770955615653315052 ) ) ;
#28558 = EDGE_CURVE ( 'NONE', #142940, #64487, #135802, .T. ) ;
#28559 = CARTESIAN_POINT ( 'NONE',  ( -21.05000000000000071, 76.00000000001210765, -132.2231074845243199 ) ) ;
#28560 = EDGE_LOOP ( 'NONE', ( #54850, #6094, #221918, #30572 ) ) ;
#28561 = DIRECTION ( 'NONE',  ( -1.000000000000000000, 0.000000000000000000, 0.000000000000000000 ) ) ;
#28562 = PRODUCT ( 'Snap Open Cable Crossbars 14', 'Snap Open Cable Crossbars 14', '', ( #228306 ) ) ;
#28563 = ADVANCED_FACE ( 'NONE', ( #138241 ), #217776, .T. ) ;
#28564 = CIRCLE ( 'NONE', #178380, 0.1000000000000089567 ) ;
#28565 = VECTOR ( 'NONE', #69248, 1000.000000000000000 ) ;
#28566 = ORIENTED_EDGE ( 'NONE', *, *, #84449, .F. ) ;
#28567 = ORIENTED_EDGE ( 'NONE', *, *, #162734, .F. ) ;
#28568 = ADVANCED_FACE ( 'NONE', ( #187681 ), #164260, .T. ) ;
#28569 = VERTEX_POINT ( 'NONE', #243782 ) ;
#28570 = DIRECTION ( 'NONE',  ( 0.000000000000000000, 0.000000000000000000, -1.000000000000000000 ) ) ;
#28571 = DIRECTION ( 'NONE',  ( 0.000000000000000000, -1.000000000000000000, -2.891205793294679805E-16 ) ) ;
#28572 = SPHERICAL_SURFACE ( 'NONE', #140887, 0.1000000000000000056 ) ;
#28573 = CARTESIAN_POINT ( 'NONE',  ( -21.14999999999999858, 69.45934304831071415, -103.0231074845243597 ) ) ;
#28575 = AXIS2_PLACEMENT_3D ( 'NONE', #124355, #25266, #205145 ) ;
#28574 = DIRECTION ( 'NONE',  ( 0.000000000000000000, 0.2128009952263605897, -0.9770955615653315052 ) ) ;
#28576 = EDGE_CURVE ( 'NONE', #210786, #252597, #165041, .T. ) ;
#28577 = DIRECTION ( 'NONE',  ( 0.000000000000000000, 0.000000000000000000, 1.000000000000000000 ) ) ;
#28578 = CARTESIAN_POINT ( 'NONE',  ( 23.24999999999999645, 79.90000000001244018, -170.0231074845243313 ) ) ;
#28579 = AXIS2_PLACEMENT_3D ( 'NONE', #38372, #132663, #257346 ) ;
#28581 = CYLINDRICAL_SURFACE ( 'NONE', #203648, 0.1999999999999987899 ) ;
#28580 = CARTESIAN_POINT ( 'NONE',  ( -20.64999999999999858, -9.399999999988846611, -90.60603087734760663 ) ) ;
#28582 = DIRECTION ( 'NONE',  ( 0.000000000000000000, 0.000000000000000000, -1.000000000000000000 ) ) ;
#28583 = ADVANCED_FACE ( 'NONE', ( #247633 ), #87253, .T. ) ;
#28584 = CIRCLE ( 'NONE', #32850, 0.2000000000000057288 ) ;
#28585 = DIRECTION ( 'NONE',  ( 0.000000000000000000, 0.8814952561688359500, -0.4721928772777478911 ) ) ;
#28586 = DIRECTION ( 'NONE',  ( 0.000000000000000000, 0.000000000000000000, 1.000000000000000000 ) ) ;
#28587 = DIRECTION ( 'NONE',  ( 0.000000000000000000, -0.8814952561688476074, 0.4721928772777262417 ) ) ;
#28588 = ORIENTED_EDGE ( 'NONE', *, *, #88215, .T. ) ;
#28589 = ORIENTED_EDGE ( 'NONE', *, *, #163974, .F. ) ;
#28590 = DIRECTION ( 'NONE',  ( 1.186688945009009831E-16, -1.000000000000000000, 0.000000000000000000 ) ) ;
#28591 = DIRECTION ( 'NONE',  ( 1.000000000000000000, 0.000000000000000000, 0.000000000000000000 ) ) ;
#28593 = CARTESIAN_POINT ( 'NONE',  ( -12.25000000000000178, 12.70026017068886404, -215.3766613508543628 ) ) ;
#28592 = CARTESIAN_POINT ( 'NONE',  ( -16.95709691156899268, 9.950000000011138823, -154.8399424374866271 ) ) ;
#28594 = CIRCLE ( 'NONE', #174327, 0.2000000000000057288 ) ;
#28595 = EDGE_CURVE ( 'NONE', #6953, #15908, #102461, .T. ) ;
#28596 = EDGE_CURVE ( 'NONE', #109657, #201957, #191846, .T. ) ;
#28597 = LINE ( 'NONE', #205884, #218527 ) ;
#28598 = DIRECTION ( 'NONE',  ( 1.000000000000000000, 0.000000000000000000, 0.000000000000000000 ) ) ;
#28599 = FACE_OUTER_BOUND ( 'NONE', #82476, .T. ) ;
#28600 = ORIENTED_EDGE ( 'NONE', *, *, #3999, .T. ) ;
#28601 = ORIENTED_EDGE ( 'NONE', *, *, #9375, .T. ) ;
#28602 = AXIS2_PLACEMENT_3D ( 'NONE', #57956, #140059, #180503 ) ;
#28603 = TOROIDAL_SURFACE ( 'NONE', #207627, 4.100000000000000533, 0.1000000000000000056 ) ;
#28604 = LINE ( 'NONE', #32433, #113799 ) ;
#28605 = CIRCLE ( 'NONE', #24474, 0.5999999999999934275 ) ;
#28606 = ORIENTED_EDGE ( 'NONE', *, *, #53815, .F. ) ;
#28607 = CARTESIAN_POINT ( 'NONE',  ( 21.14999999999999503, 11.75000000001115552, -100.5000000000000284 ) ) ;
#28608 = CIRCLE ( 'NONE', #61306, 0.09999999999999530098 ) ;
#28609 = EDGE_CURVE ( 'NONE', #120023, #84780, #52613, .T. ) ;
#28610 = EDGE_CURVE ( 'NONE', #29243, #170516, #44257, .T. ) ;
#28611 = CARTESIAN_POINT ( 'NONE',  ( -18.50000000000000000, 66.75000000001151079, -48.37310748452438247 ) ) ;
#28612 = ORIENTED_EDGE ( 'NONE', *, *, #99794, .F. ) ;
#28613 = ORIENTED_EDGE ( 'NONE', *, *, #193143, .F. ) ;
#28614 = DIRECTION ( 'NONE',  ( -1.000000000000000000, 0.000000000000000000, -0.000000000000000000 ) ) ;
#28615 = PLANE ( 'NONE',  #41163 ) ;
#28617 = DIRECTION ( 'NONE',  ( -1.000000000000000000, -2.952720810173289112E-16, 0.000000000000000000 ) ) ;
#28616 = CONICAL_SURFACE ( 'NONE', #211743, 4.299999999999966960, 0.7853981633974466137 ) ;
#28618 = CARTESIAN_POINT ( 'NONE',  ( 18.49713797159854778, -9.446482327567771620, -141.0714581216099077 ) ) ;
#28619 = DIRECTION ( 'NONE',  ( 1.000000000000000000, 0.000000000000000000, 0.000000000000000000 ) ) ;
#28620 = EDGE_CURVE ( 'NONE', #8351, #159233, #144664, .T. ) ;
#28621 = CARTESIAN_POINT ( 'NONE',  ( -20.94999999999999929, -1.849153571964891274, -78.60596661979704436 ) ) ;
#28622 = CARTESIAN_POINT ( 'NONE',  ( -17.01473183483382101, 9.950000000011138823, -79.75000000000005684 ) ) ;
#28623 = CARTESIAN_POINT ( 'NONE',  ( 21.14999999999999503, -11.74999999998883560, -155.7499999999999716 ) ) ;
#28626 = VERTEX_POINT ( 'NONE', #128979 ) ;
#28625 = EDGE_CURVE ( 'NONE', #223382, #247168, #77524, .T. ) ;
#28624 = DIRECTION ( 'NONE',  ( 1.000000000000000000, 0.000000000000000000, 0.000000000000000000 ) ) ;
#28627 = DIRECTION ( 'NONE',  ( 0.000000000000000000, -0.2128009952263603677, 0.9770955615653313941 ) ) ;
#28628 = ORIENTED_EDGE ( 'NONE', *, *, #204201, .F. ) ;
#28630 = ORIENTED_EDGE ( 'NONE', *, *, #176024, .T. ) ;
#28629 = FACE_OUTER_BOUND ( 'NONE', #107608, .T. ) ;
#28631 = ORIENTED_EDGE ( 'NONE', *, *, #214398, .T. ) ;
#28632 = DIRECTION ( 'NONE',  ( 0.000000000000000000, 1.000000000000000000, 0.000000000000000000 ) ) ;
#28633 = CARTESIAN_POINT ( 'NONE',  ( -18.37160782347004329, 11.47561641481354044, -143.2500000000000284 ) ) ;
#28634 = FACE_OUTER_BOUND ( 'NONE', #99177, .T. ) ;
#28635 = DIRECTION ( 'NONE',  ( 1.000000000000000000, 1.794895427898103559E-16, 3.909090864890002444E-17 ) ) ;
#28636 = CARTESIAN_POINT ( 'NONE',  ( 23.14999999999999503, 66.34920340998563404, -213.7018660128499334 ) ) ;
#28637 = EDGE_CURVE ( 'NONE', #43638, #36614, #46842, .T. ) ;
#28638 = CARTESIAN_POINT ( 'NONE',  ( -18.59999999999999787, 9.150000000011157653, -88.15000000000004832 ) ) ;
#28639 = DIRECTION ( 'NONE',  ( -1.000000000000000000, 0.000000000000000000, 0.000000000000000000 ) ) ;
#28640 = DIRECTION ( 'NONE',  ( 0.000000000000000000, -0.9964539953858966292, -0.08413937888696132461 ) ) ;
#28641 = DIRECTION ( 'NONE',  ( 1.000000000000000000, 0.000000000000000000, 0.000000000000000000 ) ) ;
#28642 = ADVANCED_FACE ( 'NONE', ( #125133 ), #225474, .F. ) ;
#28643 = AXIS2_PLACEMENT_3D ( 'NONE', #195645, #54809, #153979 ) ;
#28644 = ORIENTED_EDGE ( 'NONE', *, *, #45510, .T. ) ;
#28645 = EDGE_LOOP ( 'NONE', ( #181661, #238771, #168754, #249399, #256649 ) ) ;
#28646 = VECTOR ( 'NONE', #46309, 1000.000000000000000 ) ;
#28647 = CARTESIAN_POINT ( 'NONE',  ( -21.29999999999995808, 36.65892442174472876, -249.5511627012454596 ) ) ;
#28648 = CIRCLE ( 'NONE', #257653, 0.1000000000000075273 ) ;
#28649 = ORIENTED_EDGE ( 'NONE', *, *, #60456, .T. ) ;
#28650 = FACE_OUTER_BOUND ( 'NONE', #172609, .T. ) ;
#28651 = EDGE_LOOP ( 'NONE', ( #111008, #246381 ) ) ;
#28652 = CARTESIAN_POINT ( 'NONE',  ( -23.25000000000000000, 6.933893972137497030, -70.78564583437358237 ) ) ;
#28653 = TOROIDAL_SURFACE ( 'NONE', #182742, 0.2000000000000000111, 0.1000000000000000056 ) ;
#28654 = CARTESIAN_POINT ( 'NONE',  ( 19.75857864376269646, 11.65000000000000924, -24.75000000000000000 ) ) ;
#28655 = CARTESIAN_POINT ( 'NONE',  ( -5.999999999999938716, 64.75000000001119815, -22.02310748452479316 ) ) ;
#28656 = EDGE_CURVE ( 'NONE', #187924, #150841, #110888, .T. ) ;
#28657 = CARTESIAN_POINT ( 'NONE',  ( -21.05000000000000071, 1.316055977212913009, -230.7323992127457473 ) ) ;
#28658 = CARTESIAN_POINT ( 'NONE',  ( -22.39999999999999858, 1.115600667400684642E-11, -88.85042919245522341 ) ) ;
#28659 = ORIENTED_EDGE ( 'NONE', *, *, #184003, .F. ) ;
#28660 = DIRECTION ( 'NONE',  ( 0.000000000000000000, -6.982962677686266711E-15, 1.000000000000000000 ) ) ;
#28661 = CIRCLE ( 'NONE', #86843, 0.09999999999999983902 ) ;
#28662 = VECTOR ( 'NONE', #89989, 1000.000000000000000 ) ;
#28663 = DIRECTION ( 'NONE',  ( 0.000000000000000000, 0.2128009952263605897, -0.9770955615653315052 ) ) ;
#28664 = DIRECTION ( 'NONE',  ( -3.469446951953515108E-14, 0.000000000000000000, -1.000000000000000000 ) ) ;
#28665 = ORIENTED_EDGE ( 'NONE', *, *, #196288, .F. ) ;
#28667 = CARTESIAN_POINT ( 'NONE',  ( -20.54999999999999716, 1.925233644870967487, -188.2697564668738153 ) ) ;
#28666 = DIRECTION ( 'NONE',  ( -0.000000000000000000, -0.000000000000000000, 1.000000000000000000 ) ) ;
#28668 = ORIENTED_EDGE ( 'NONE', *, *, #246962, .T. ) ;
#28670 = EDGE_LOOP ( 'NONE', ( #43972, #253723, #118299, #238949 ) ) ;
#28669 = LINE ( 'NONE', #230680, #146284 ) ;
#28671 = VERTEX_POINT ( 'NONE', #88534 ) ;
#28672 = AXIS2_PLACEMENT_3D ( 'NONE', #43797, #244548, #106306 ) ;
#28673 = DIRECTION ( 'NONE',  ( -0.000000000000000000, 1.000000000000000000, 6.982962677686266711E-15 ) ) ;
#28674 = CARTESIAN_POINT ( 'NONE',  ( -22.50000000000000000, 11.75000000001115552, -134.0000000000000284 ) ) ;
#28675 = DIRECTION ( 'NONE',  ( 0.000000000000000000, -0.008583690987162452199, 0.9999631594459053030 ) ) ;
#28676 = ORIENTED_EDGE ( 'NONE', *, *, #133341, .F. ) ;
#28677 = CARTESIAN_POINT ( 'NONE',  ( 21.14999999999999858, 30.68987205111126926, -252.2252246220829193 ) ) ;
#28678 = CARTESIAN_POINT ( 'NONE',  ( -21.14999999999999858, 1.316055977212913009, -230.7323992127457473 ) ) ;
#28679 = CARTESIAN_POINT ( 'NONE',  ( -22.48660254037843487, 11.74999999999999822, 0.04999999999998229472 ) ) ;
#28681 = ORIENTED_EDGE ( 'NONE', *, *, #256036, .T. ) ;
#28680 = DIRECTION ( 'NONE',  ( 0.000000000000000000, 0.000000000000000000, 1.000000000000000000 ) ) ;
#28682 = EDGE_LOOP ( 'NONE', ( #118973, #195369, #200109, #248051 ) ) ;
#28683 = AXIS2_PLACEMENT_3D ( 'NONE', #243311, #242034, #63387 ) ;
#28684 = FACE_OUTER_BOUND ( 'NONE', #48234, .T. ) ;
#28685 = LINE ( 'NONE', #113303, #231133 ) ;
#28686 = VECTOR ( 'NONE', #118503, 1000.000000000000000 ) ;
#28687 = VECTOR ( 'NONE', #235693, 1000.000000000000000 ) ;
#28688 = CARTESIAN_POINT ( 'NONE',  ( 21.05000000000000071, 85.00000000001222134, -146.4170766071767389 ) ) ;
#28689 = ORIENTED_EDGE ( 'NONE', *, *, #138201, .T. ) ;
#28690 = DIRECTION ( 'NONE',  ( 1.000000000000000000, 0.000000000000000000, 0.000000000000000000 ) ) ;
#28691 = CARTESIAN_POINT ( 'NONE',  ( 18.58685178364169488, -9.406733083793085370, -141.1244204690877098 ) ) ;
#28692 = CIRCLE ( 'NONE', #124505, 2.000000000000001776 ) ;
#28693 = ORIENTED_EDGE ( 'NONE', *, *, #125140, .T. ) ;
#28694 = DIRECTION ( 'NONE',  ( 0.000000000000000000, 0.000000000000000000, 1.000000000000000000 ) ) ;
#28695 = EDGE_CURVE ( 'NONE', #85481, #87673, #156891, .T. ) ;
#28696 = VERTEX_POINT ( 'NONE', #188947 ) ;
#28697 = CIRCLE ( 'NONE', #49498, 0.1000000000000028644 ) ;
#28699 = AXIS2_PLACEMENT_3D ( 'NONE', #9205, #168334, #70505 ) ;
#28698 = CYLINDRICAL_SURFACE ( 'NONE', #68167, 0.1000000000000028644 ) ;
#28700 = DIRECTION ( 'NONE',  ( -0.5932847527679299127, 0.8049926720990051576, 6.366092712777055223E-16 ) ) ;
#28701 = VECTOR ( 'NONE', #67731, 1000.000000000000000 ) ;
#28702 = ORIENTED_EDGE ( 'NONE', *, *, #134047, .F. ) ;
#28703 = ORIENTED_EDGE ( 'NONE', *, *, #230771, .T. ) ;
#28704 = VECTOR ( 'NONE', #198170, 1000.000000000000000 ) ;
#28705 = DIRECTION ( 'NONE',  ( -1.000000000000000000, 0.000000000000000000, 0.000000000000000000 ) ) ;
#28706 = ORIENTED_EDGE ( 'NONE', *, *, #222517, .T. ) ;
#28708 = ORIENTED_EDGE ( 'NONE', *, *, #76646, .T. ) ;
#28707 = CARTESIAN_POINT ( 'NONE',  ( -22.50000000000094147, 0.1008583691097610646, -155.7504328765105583 ) ) ;
#28709 = EDGE_LOOP ( 'NONE', ( #212470, #49417, #71877, #67197 ) ) ;
#28710 = CIRCLE ( 'NONE', #195285, 0.5999999999999894307 ) ;
#28711 = CIRCLE ( 'NONE', #224474, 0.8750000000000007772 ) ;
#28712 = ADVANCED_FACE ( 'NONE', ( #185092 ), #135990, .F. ) ;
#28714 = ORIENTED_EDGE ( 'NONE', *, *, #85096, .F. ) ;
#28713 = ORIENTED_EDGE ( 'NONE', *, *, #193558, .T. ) ;
#28715 = CARTESIAN_POINT ( 'NONE',  ( -18.48179518609225624, -9.518325300483391871, -107.3897055767624522 ) ) ;
#28716 = ORIENTED_EDGE ( 'NONE', *, *, #48346, .T. ) ;
#28717 = DIRECTION ( 'NONE',  ( 0.000000000000000000, 0.4930308989874980785, 0.8700118002898462599 ) ) ;
#28718 = CARTESIAN_POINT ( 'NONE',  ( -21.05000000000000071, -1.236118717437885595, -194.8647072476926496 ) ) ;
#28719 = CARTESIAN_POINT ( 'NONE',  ( 21.04999999999999716, 67.12872031401698791, -194.9644784893834810 ) ) ;
#28720 = CIRCLE ( 'NONE', #174477, 0.2000000000000005107 ) ;
#28721 = CARTESIAN_POINT ( 'NONE',  ( -18.40000000000000213, 11.47316190337362762, -146.5500000000000114 ) ) ;
#28722 = AXIS2_PLACEMENT_3D ( 'NONE', #75970, #79789, #155541 ) ;
#28723 = AXIS2_PLACEMENT_3D ( 'NONE', #157714, #201930, #257994 ) ;
#28724 = ORIENTED_EDGE ( 'NONE', *, *, #30569, .T. ) ;
#28725 = MECHANICAL_DESIGN_GEOMETRIC_PRESENTATION_REPRESENTATION (  '', ( #137011 ), #132753 ) ;
#28726 = ORIENTED_EDGE ( 'NONE', *, *, #45600, .F. ) ;
#28727 = EDGE_CURVE ( 'NONE', #184131, #86042, #85956, .T. ) ;
#28728 = DIRECTION ( 'NONE',  ( -0.000000000000000000, 0.2128009952263603677, -0.9770955615653313941 ) ) ;
#28730 = ORIENTED_EDGE ( 'NONE', *, *, #42938, .F. ) ;
#28729 = ADVANCED_FACE ( 'NONE', ( #254940 ), #7000, .F. ) ;
#28731 = CARTESIAN_POINT ( 'NONE',  ( -16.78055652883087134, 9.946776916136505164, -180.1607918375923987 ) ) ;
#28733 = ORIENTED_EDGE ( 'NONE', *, *, #255859, .T. ) ;
#28732 = CARTESIAN_POINT ( 'NONE',  ( 20.94999999999999574, -11.41227409413852989, -36.50000000000000711 ) ) ;
#28734 = AXIS2_PLACEMENT_3D ( 'NONE', #166007, #206390, #188109 ) ;
#28735 = ORIENTED_EDGE ( 'NONE', *, *, #208449, .T. ) ;
#28736 = DIRECTION ( 'NONE',  ( 1.000000000000000000, 0.000000000000000000, 0.000000000000000000 ) ) ;
#28737 = EDGE_CURVE ( 'NONE', #124170, #246109, #118059, .T. ) ;
#28738 = ORIENTED_EDGE ( 'NONE', *, *, #207473, .T. ) ;
#28739 = ADVANCED_FACE ( 'NONE', ( #55482 ), #39839, .T. ) ;
#28740 = LINE ( 'NONE', #209911, #56222 ) ;
#28741 = DIRECTION ( 'NONE',  ( -1.000000000000000000, 0.000000000000000000, 0.000000000000000000 ) ) ;
#28742 = VECTOR ( 'NONE', #138929, 1000.000000000000000 ) ;
#28743 = AXIS2_PLACEMENT_3D ( 'NONE', #102887, #119947, #125057 ) ;
#28745 = ORIENTED_EDGE ( 'NONE', *, *, #210599, .F. ) ;
#28744 = EDGE_LOOP ( 'NONE', ( #173085, #208968, #240432, #4997 ) ) ;
#28747 = ORIENTED_EDGE ( 'NONE', *, *, #2408, .T. ) ;
#28746 = AXIS2_PLACEMENT_3D ( 'NONE', #87251, #207235, #250197 ) ;
#28748 = LINE ( 'NONE', #228190, #220018 ) ;
#28750 = ORIENTED_EDGE ( 'NONE', *, *, #165988, .F. ) ;
#28749 = ADVANCED_FACE ( 'NONE', ( #178058, #250200 ), #135033, .F. ) ;
#28751 = VERTEX_POINT ( 'NONE', #99757 ) ;
#28752 = DIRECTION ( 'NONE',  ( -0.000000000000000000, 1.000000000000000000, 8.717686153663073805E-15 ) ) ;
#28754 = EDGE_LOOP ( 'NONE', ( #6515, #77287, #186256, #150754 ) ) ;
#28753 = CARTESIAN_POINT ( 'NONE',  ( -21.05000000000000071, 76.00000000001126921, -203.5231074845248997 ) ) ;
#28755 = CARTESIAN_POINT ( 'NONE',  ( 21.14999999999999858, 6.650000000011155876, -112.8500000000000369 ) ) ;
#28757 = PLANE ( 'NONE',  #73538 ) ;
#28756 = CARTESIAN_POINT ( 'NONE',  ( 21.05000000000000071, 4.813084112160684214, -88.55848224347622022 ) ) ;
#28758 = CARTESIAN_POINT ( 'NONE',  ( -22.50000000000000000, 76.00000000001213607, -136.6231074845242972 ) ) ;
#28759 = DIRECTION ( 'NONE',  ( 0.000000000000000000, -7.056502275159890832E-15, 1.000000000000000000 ) ) ;
#28760 = VERTEX_POINT ( 'NONE', #138868 ) ;
#28761 = CIRCLE ( 'NONE', #236996, 0.09999999999998898659 ) ;
#28762 = TOROIDAL_SURFACE ( 'NONE', #70444, 1.900000000000002576, 0.1000000000000000056 ) ;
#28764 = EDGE_CURVE ( 'NONE', #167398, #246715, #48512, .T. ) ;
#28763 = VERTEX_POINT ( 'NONE', #37264 ) ;
#28765 = FACE_OUTER_BOUND ( 'NONE', #72607, .T. ) ;
#28766 = CIRCLE ( 'NONE', #224523, 0.09999999999999949207 ) ;
#28767 = EDGE_LOOP ( 'NONE', ( #231374, #213978, #82410, #227459 ) ) ;
#28768 = VECTOR ( 'NONE', #172786, 1000.000000000000227 ) ;
#28769 = FACE_OUTER_BOUND ( 'NONE', #154240, .T. ) ;
#28770 = ORIENTED_EDGE ( 'NONE', *, *, #180393, .T. ) ;
#28771 = VERTEX_POINT ( 'NONE', #214584 ) ;
#28772 = DIRECTION ( 'NONE',  ( -0.000000000000000000, 0.000000000000000000, 1.000000000000000000 ) ) ;
#28773 = LINE ( 'NONE', #106960, #28036 ) ;
#28774 = EDGE_LOOP ( 'NONE', ( #22829, #39623, #147403, #143624 ) ) ;
#28775 = DIRECTION ( 'NONE',  ( -1.000000000000000000, -0.000000000000000000, -0.000000000000000000 ) ) ;
#28776 = CARTESIAN_POINT ( 'NONE',  ( 21.10710606213542206, 8.776894023904366904, -112.7409965263994565 ) ) ;
#28777 = ORIENTED_EDGE ( 'NONE', *, *, #248678, .F. ) ;
#28778 = CARTESIAN_POINT ( 'NONE',  ( 21.05000000000000071, 39.26973050389061370, -236.6309188891183055 ) ) ;
#28779 = CARTESIAN_POINT ( 'NONE',  ( -20.85000000000000142, 7.021664781911246322, -70.83356540189728889 ) ) ;
#28781 = CARTESIAN_POINT ( 'NONE',  ( -18.50000000000000000, 1.637172712981535883, -45.08215336547201701 ) ) ;
#28780 = CARTESIAN_POINT ( 'NONE',  ( -23.25000000000000000, -1.851617760457748618, -78.60318971960367662 ) ) ;
#28782 = CARTESIAN_POINT ( 'NONE',  ( -20.85000000000000142, 10.33248238083634440, -72.59484654391314962 ) ) ;
#28784 = AXIS2_PLACEMENT_3D ( 'NONE', #216423, #217684, #58621 ) ;
#28783 = CARTESIAN_POINT ( 'NONE',  ( -21.05000000000000071, 87.75000000001216449, -139.6231074845242688 ) ) ;
#28785 = CIRCLE ( 'NONE', #203523, 0.1000000000000032391 ) ;
#28786 = CARTESIAN_POINT ( 'NONE',  ( -20.94999999999999929, 69.09936979046463534, -247.6075824278584889 ) ) ;
#28787 = AXIS2_PLACEMENT_3D ( 'NONE', #65530, #129366, #207639 ) ;
#28788 = VERTEX_POINT ( 'NONE', #115488 ) ;
#28789 = EDGE_CURVE ( 'NONE', #92927, #57247, #65268, .T. ) ;
#28791 = ORIENTED_EDGE ( 'NONE', *, *, #151485, .F. ) ;
#28790 = EDGE_LOOP ( 'NONE', ( #51492, #99945, #47170, #255793 ) ) ;
#28792 = ORIENTED_EDGE ( 'NONE', *, *, #256894, .T. ) ;
#28793 = EDGE_CURVE ( 'NONE', #37340, #4110, #219720, .T. ) ;
#28794 = DIRECTION ( 'NONE',  ( 0.000000000000000000, -0.9915357197604982575, 0.1298341882519033486 ) ) ;
#28795 = DIRECTION ( 'NONE',  ( -1.000000000000000000, -1.387778780781454006E-13, 2.775557561562908012E-13 ) ) ;
#28796 = ADVANCED_FACE ( 'NONE', ( #11606 ), #231891, .F. ) ;
#28797 = EDGE_CURVE ( 'NONE', #116304, #78944, #123532, .T. ) ;
#28799 = CARTESIAN_POINT ( 'NONE',  ( 20.94999999999999574, 62.00000000001264056, -198.0960149541419071 ) ) ;
#28798 = CARTESIAN_POINT ( 'NONE',  ( -18.59999999999999787, -1.835859311432481045, -212.5044391687984842 ) ) ;
#28800 = FACE_OUTER_BOUND ( 'NONE', #60067, .T. ) ;
#28801 = EDGE_LOOP ( 'NONE', ( #68185, #4849, #115317, #90305 ) ) ;
#28802 = DIRECTION ( 'NONE',  ( 0.000000000000000000, 0.000000000000000000, -1.000000000000000000 ) ) ;
#28803 = DIRECTION ( 'NONE',  ( 1.000000000000000000, -0.000000000000000000, 0.000000000000000000 ) ) ;
#28804 = CARTESIAN_POINT ( 'NONE',  ( -23.25000000000000000, 11.65000000001115588, -54.84999999999999432 ) ) ;
#28805 = EDGE_CURVE ( 'NONE', #166990, #241008, #19501, .T. ) ;
#28806 = DIRECTION ( 'NONE',  ( -0.000000000000000000, 6.982962677686266711E-15, -1.000000000000000000 ) ) ;
#28807 = VERTEX_POINT ( 'NONE', #136309 ) ;
#28808 = EDGE_CURVE ( 'NONE', #141200, #169154, #2713, .T. ) ;
#28810 = EDGE_CURVE ( 'NONE', #80843, #156398, #115167, .T. ) ;
#28809 = ADVANCED_FACE ( 'NONE', ( #97164 ), #77623, .T. ) ;
#28811 = DIRECTION ( 'NONE',  ( 0.7071067811865463515, 0.7071067811865487940, 4.937700262164540154E-15 ) ) ;
#28812 = DIRECTION ( 'NONE',  ( 0.000000000000000000, 0.000000000000000000, -1.000000000000000000 ) ) ;
#28813 = VERTEX_POINT ( 'NONE', #38532 ) ;
#28814 = VERTEX_POINT ( 'NONE', #158503 ) ;
#28815 = DIRECTION ( 'NONE',  ( 0.000000000000000000, 0.000000000000000000, -1.000000000000000000 ) ) ;
#28816 = LINE ( 'NONE', #225647, #189512 ) ;
#28817 = ADVANCED_FACE ( 'NONE', ( #237999 ), #59333, .F. ) ;
#28818 = DIRECTION ( 'NONE',  ( -0.000000000000000000, -6.982962677686266711E-15, 1.000000000000000000 ) ) ;
#28819 = DIRECTION ( 'NONE',  ( 0.000000000000000000, 0.000000000000000000, 1.000000000000000000 ) ) ;
#28820 = DIRECTION ( 'NONE',  ( 0.7071067811865487940, 0.6453109281988437251, 0.2890913453342125461 ) ) ;
#28821 = CARTESIAN_POINT ( 'NONE',  ( 21.05000000000000071, 1.115600667400684642E-11, -33.50000000000000000 ) ) ;
#28822 = ORIENTED_EDGE ( 'NONE', *, *, #123894, .T. ) ;
#28823 = CARTESIAN_POINT ( 'NONE',  ( -18.79999999999999716, 8.000000000000000000, -1.212568896937008089 ) ) ;
#28824 = EDGE_CURVE ( 'NONE', #234572, #94985, #145318, .T. ) ;
#28826 = DIRECTION ( 'NONE',  ( 0.000000000000000000, -0.9126074666063769270, -0.4088369013363280513 ) ) ;
#28825 = LINE ( 'NONE', #26223, #149473 ) ;
#28827 = DIRECTION ( 'NONE',  ( 1.000000000000000000, 0.000000000000000000, 0.000000000000000000 ) ) ;
#28828 = DIRECTION ( 'NONE',  ( 0.000000000000000000, -0.4721928772776973204, -0.8814952561688629284 ) ) ;
#28829 = AXIS2_PLACEMENT_3D ( 'NONE', #205555, #144284, #163890 ) ;
#28830 = AXIS2_PLACEMENT_3D ( 'NONE', #137122, #233662, #214088 ) ;
#28831 = CARTESIAN_POINT ( 'NONE',  ( -18.59999999999999787, 64.25000000001223555, -148.6731074845244507 ) ) ;
#28832 = CARTESIAN_POINT ( 'NONE',  ( 23.15000000000000213, 87.75000000001149658, -48.17310748452423752 ) ) ;
#28833 = EDGE_CURVE ( 'NONE', #215370, #127649, #226122, .T. ) ;
#28834 = VECTOR ( 'NONE', #200417, 1000.000000000000000 ) ;
#28836 = EDGE_CURVE ( 'NONE', #238735, #250167, #190189, .T. ) ;
#28835 = VECTOR ( 'NONE', #49597, 1000.000000000000000 ) ;
#28838 = EDGE_LOOP ( 'NONE', ( #30756, #65576, #254759, #190239 ) ) ;
#28837 = DIRECTION ( 'NONE',  ( 1.000000000000000000, -3.151514657663852580E-16, 8.547182517843351137E-17 ) ) ;
#28839 = ADVANCED_FACE ( 'NONE', ( #81468 ), #23619, .F. ) ;
#28840 = CIRCLE ( 'NONE', #178663, 7.900000000000003908 ) ;
#28841 = ADVANCED_FACE ( 'NONE', ( #67083 ), #224856, .F. ) ;
#28842 = EDGE_CURVE ( 'NONE', #78646, #204749, #125757, .T. ) ;
#28843 = AXIS2_PLACEMENT_3D ( 'NONE', #196713, #216272, #199299 ) ;
#28844 = CIRCLE ( 'NONE', #49633, 0.09999999999999939493 ) ;
#28846 = AXIS2_PLACEMENT_3D ( 'NONE', #88198, #203033, #107790 ) ;
#28845 = DIRECTION ( 'NONE',  ( -1.000000000000000000, 0.000000000000000000, -0.000000000000000000 ) ) ;
#28847 = CARTESIAN_POINT ( 'NONE',  ( -20.94999999999999929, 77.16270174994990327, -94.92310748452430857 ) ) ;
#28848 = ORIENTED_EDGE ( 'NONE', *, *, #169483, .T. ) ;
#28849 = AXIS2_PLACEMENT_3D ( 'NONE', #211560, #91605, #189429 ) ;
#28850 = CARTESIAN_POINT ( 'NONE',  ( 22.10000000000000142, -3.262756495241484158E-15, 32.89999999999999858 ) ) ;
#28851 = LINE ( 'NONE', #147458, #32690 ) ;
#28852 = CYLINDRICAL_SURFACE ( 'NONE', #15403, 0.1000000000000028644 ) ;
#28853 = EDGE_LOOP ( 'NONE', ( #85268, #107916, #129675, #157360, #229055, #128737, #247357, #41106, #18913, #37693, #82854, #132339, #62139, #128699, #165177, #131992, #13569, #88391 ) ) ;
#28854 = FACE_OUTER_BOUND ( 'NONE', #28645, .T. ) ;
#28856 = ORIENTED_EDGE ( 'NONE', *, *, #27133, .F. ) ;
#28855 = PLANE ( 'NONE',  #138417 ) ;
#28857 = PLANE ( 'NONE',  #21553 ) ;
#28858 =( BOUNDED_CURVE ( )  B_SPLINE_CURVE ( 3, ( #255211, #142995, #165157, #28243 ),
 .UNSPECIFIED., .F., .F. ) 
 B_SPLINE_CURVE_WITH_KNOTS ( ( 4, 4 ),
 ( 3.141592653589791784, 4.712388980384688786 ),
 .UNSPECIFIED. ) 
 CURVE ( )  GEOMETRIC_REPRESENTATION_ITEM ( )  RATIONAL_B_SPLINE_CURVE ( ( 1.000000000000000000, 0.8047378541243649375, 0.8047378541243649375, 1.000000000000000000 ) ) 
 REPRESENTATION_ITEM ( '' )  );
#28859 = CARTESIAN_POINT ( 'NONE',  ( -20.94999999999999929, 76.00000000001213607, -136.5231074845242745 ) ) ;
#28860 = VERTEX_POINT ( 'NONE', #101014 ) ;
#28861 = FACE_OUTER_BOUND ( 'NONE', #210231, .T. ) ;
#28862 = DIRECTION ( 'NONE',  ( 0.000000000000000000, 0.000000000000000000, 1.000000000000000000 ) ) ;
#28863 = CARTESIAN_POINT ( 'NONE',  ( -20.92356734117541706, 65.68026841930881687, -63.97257401318893955 ) ) ;
#28864 = CARTESIAN_POINT ( 'NONE',  ( -22.57320508075687115, 11.65000000000000036, -3.122502256758252770E-14 ) ) ;
#28865 = DIRECTION ( 'NONE',  ( 0.000000000000000000, 0.7092521942343286145, 0.7049548389604757270 ) ) ;
#28866 = ORIENTED_EDGE ( 'NONE', *, *, #49932, .T. ) ;
#28867 = DIRECTION ( 'NONE',  ( 0.000000000000000000, 0.000000000000000000, -1.000000000000000000 ) ) ;
#28868 = CYLINDRICAL_SURFACE ( 'NONE', #25717, 0.09999999999999939493 ) ;
#28869 = CIRCLE ( 'NONE', #103799, 0.09999999999999939493 ) ;
#28870 = B_SPLINE_CURVE_WITH_KNOTS ( 'NONE', 3,
 ( #191119, #228939, #91983, #131110, #11176, #171560, #209367 ),
 .UNSPECIFIED., .F., .F.,
 ( 4, 3, 4 ),
 ( 0.000000000000000000, 3.357501770815118507E-05, 5.199112466349255934E-05 ),
 .UNSPECIFIED. ) ;
#28871 = DIRECTION ( 'NONE',  ( -1.000000000000000000, 0.000000000000000000, 0.000000000000000000 ) ) ;
#28872 = EDGE_LOOP ( 'NONE', ( #44899, #120045, #167856, #246607 ) ) ;
#28873 = TOROIDAL_SURFACE ( 'NONE', #145331, 11.65000000000000036, 0.1000000000000000056 ) ;
#28874 = ORIENTED_EDGE ( 'NONE', *, *, #6892, .F. ) ;
#28875 = CARTESIAN_POINT ( 'NONE',  ( 21.05000000000000071, -11.29603075032412995, -70.04789915966391334 ) ) ;
#28876 = DIRECTION ( 'NONE',  ( 0.000000000000000000, -7.056502275159890832E-15, 1.000000000000000000 ) ) ;
#28877 = CARTESIAN_POINT ( 'NONE',  ( 18.59999999999998721, 56.14960075277857499, -134.2428044267230689 ) ) ;
#28878 = ADVANCED_FACE ( 'NONE', ( #144032 ), #1948, .T. ) ;
#28879 = FACE_BOUND ( 'NONE', #230763, .T. ) ;
#28880 = CARTESIAN_POINT ( 'NONE',  ( 20.95512828230152280, 8.876151312336450161, -146.2024302655031534 ) ) ;
#28882 = CARTESIAN_POINT ( 'NONE',  ( -22.59999999999999787, 31.76322370622491320, -238.8696546380523671 ) ) ;
#28881 = CARTESIAN_POINT ( 'NONE',  ( -23.25000000000000000, 67.23127455305841238, -235.8551265064783991 ) ) ;
#28884 = DIRECTION ( 'NONE',  ( -0.000000000000000000, 0.2128009952263604232, -0.9770955615653316162 ) ) ;
#28883 = CIRCLE ( 'NONE', #241235, 0.1000000000000028644 ) ;
#28885 = EDGE_CURVE ( 'NONE', #173825, #221150, #144342, .T. ) ;
#28886 = FACE_OUTER_BOUND ( 'NONE', #69089, .T. ) ;
#28887 = CARTESIAN_POINT ( 'NONE',  ( -21.05000000000000071, 5.900000000011162093, -90.28090023534366537 ) ) ;
#28888 = VECTOR ( 'NONE', #232795, 1000.000000000000000 ) ;
#28889 = CYLINDRICAL_SURFACE ( 'NONE', #77446, 1.749999999999998002 ) ;
#28891 = ORIENTED_EDGE ( 'NONE', *, *, #172474, .F. ) ;
#28890 = CYLINDRICAL_SURFACE ( 'NONE', #73961, 0.9000000000000014655 ) ;
#28892 = CARTESIAN_POINT ( 'NONE',  ( 21.08621493067296271, 69.65070570884071799, -170.0793023240005084 ) ) ;
#28893 = DIRECTION ( 'NONE',  ( -0.000000000000000000, -0.000000000000000000, -1.000000000000000000 ) ) ;
#28895 = CARTESIAN_POINT ( 'NONE',  ( -20.94999999999999929, 76.00000000001216449, -140.6231074845243256 ) ) ;
#28894 = CARTESIAN_POINT ( 'NONE',  ( 20.94999999999999929, -1.835341550213257733, -145.5551512925629822 ) ) ;
#28896 = EDGE_CURVE ( 'NONE', #91733, #143423, #181897, .T. ) ;
#28897 = EDGE_CURVE ( 'NONE', #234836, #191279, #141476, .T. ) ;
#28898 = EDGE_LOOP ( 'NONE', ( #10883, #69102, #185220, #136669 ) ) ;
#28899 = CARTESIAN_POINT ( 'NONE',  ( 20.94999999999999574, 74.25000000001186606, -91.35359592662267403 ) ) ;
#28900 = PLANE ( 'NONE',  #33151 ) ;
#28901 = CARTESIAN_POINT ( 'NONE',  ( 18.59999999999999787, -10.64999999999999325, 31.59999999999999787 ) ) ;
#28902 = CARTESIAN_POINT ( 'NONE',  ( 22.59999985501178799, 12.61921324905061326, -223.3442716046673127 ) ) ;
#28903 = ORIENTED_EDGE ( 'NONE', *, *, #158198, .F. ) ;
#28904 = AXIS2_PLACEMENT_3D ( 'NONE', #60186, #23671, #65327 ) ;
#28905 = CIRCLE ( 'NONE', #228768, 0.09999999999999939493 ) ;
#28906 = ORIENTED_EDGE ( 'NONE', *, *, #117634, .T. ) ;
#28907 = CARTESIAN_POINT ( 'NONE',  ( -21.45000000000000284, 44.77807522791015060, -237.4671205425215135 ) ) ;
#28908 = EDGE_LOOP ( 'NONE', ( #37303, #51139, #223001, #247615 ) ) ;
#28909 = DIRECTION ( 'NONE',  ( 0.000000000000000000, 0.2128009952263485993, -0.9770955615653341697 ) ) ;
#28910 = ORIENTED_EDGE ( 'NONE', *, *, #231577, .T. ) ;
#28911 = EDGE_CURVE ( 'NONE', #58001, #93827, #252696, .T. ) ;
#28912 = AXIS2_PLACEMENT_3D ( 'NONE', #88383, #123697, #183672 ) ;
#28913 = DIRECTION ( 'NONE',  ( 0.000000000000000000, 0.9876197685951252359, -0.1568667991644863424 ) ) ;
#28915 = EDGE_CURVE ( 'NONE', #223991, #180552, #42381, .T. ) ;
#28914 = VECTOR ( 'NONE', #211018, 999.9999999999998863 ) ;
#28916 = FACE_OUTER_BOUND ( 'NONE', #213179, .T. ) ;
#28917 = VECTOR ( 'NONE', #244871, 1000.000000000000227 ) ;
#28918 = CARTESIAN_POINT ( 'NONE',  ( 23.24999999999999645, 64.25000000001153921, -48.67310748452441516 ) ) ;
#28919 = ORIENTED_EDGE ( 'NONE', *, *, #155742, .F. ) ;
#28920 = DIRECTION ( 'NONE',  ( 1.000000000000000000, 0.000000000000000000, 0.000000000000000000 ) ) ;
#28921 = CARTESIAN_POINT ( 'NONE',  ( -18.50211644919735932, 68.02921119886117651, -224.2090419302654141 ) ) ;
#28922 = DIRECTION ( 'NONE',  ( 0.000000000000000000, -0.1332476588733448597, 0.9910827722268067408 ) ) ;
#28923 = CARTESIAN_POINT ( 'NONE',  ( -18.59999999999999787, 11.65000000001115232, -155.3500000000000227 ) ) ;
#28924 = EDGE_CURVE ( 'NONE', #84861, #42519, #221001, .T. ) ;
#28925 = CARTESIAN_POINT ( 'NONE',  ( -20.85000000000000142, 11.75000000001115197, -127.1583993101029790 ) ) ;
#28926 = DIRECTION ( 'NONE',  ( 1.000000000000000000, 3.265361837132813093E-16, -0.000000000000000000 ) ) ;
#28928 = EDGE_LOOP ( 'NONE', ( #162778, #76303, #48819, #236124 ) ) ;
#28927 = ADVANCED_FACE ( 'NONE', ( #3232 ), #82748, .F. ) ;
#28930 = CARTESIAN_POINT ( 'NONE',  ( -18.79999999999999716, 1.885425182446133885, -11.49641995933507843 ) ) ;
#28929 = DIRECTION ( 'NONE',  ( -1.000000000000000000, -5.551115123125816024E-13, 2.775557561562908012E-13 ) ) ;
#28931 = VERTEX_POINT ( 'NONE', #222267 ) ;
#28933 = ORIENTED_EDGE ( 'NONE', *, *, #132373, .T. ) ;
#28932 = CARTESIAN_POINT ( 'NONE',  ( -20.15000000000000568, 9.291421356248463326, -121.7500000000000426 ) ) ;
#28934 = VERTEX_POINT ( 'NONE', #123204 ) ;
#28935 = DIRECTION ( 'NONE',  ( 0.000000000000000000, 0.1335171055202821200, -0.9910465087640870641 ) ) ;
#28936 = CARTESIAN_POINT ( 'NONE',  ( 15.39170923737818342, 66.61047060254553287, -152.2059995716307128 ) ) ;
#28937 = DIRECTION ( 'NONE',  ( 1.000000000000000000, 0.000000000000000000, 0.000000000000000000 ) ) ;
#28938 = CARTESIAN_POINT ( 'NONE',  ( 21.05000000000000071, 65.43728505328409994, -129.0663053788799175 ) ) ;
#28939 = EDGE_LOOP ( 'NONE', ( #103357, #20358, #185600, #187539 ) ) ;
#28940 = LINE ( 'NONE', #211386, #93061 ) ;
#28941 = DIRECTION ( 'NONE',  ( 0.000000000000000000, 1.000000000000000000, 6.688090509790097607E-15 ) ) ;
#28942 = EDGE_CURVE ( 'NONE', #18391, #120146, #24126, .T. ) ;
#28943 = B_SPLINE_CURVE_WITH_KNOTS ( 'NONE', 3,
 ( #163451, #203849, #179188, #83862, #242974, #223402, #60475, #142578, #64354, #198715, #61776, #143869, #222105, #200011, #499, #80018 ),
 .UNSPECIFIED., .F., .F.,
 ( 4, 3, 3, 3, 3, 4 ),
 ( 0.000000000000000000, 1.810570668010542492E-05, 2.740575833570115904E-05, 4.256816319434871692E-05, 5.213463471023795320E-05, 6.641585710717593048E-05 ),
 .UNSPECIFIED. ) ;
#28944 = ORIENTED_EDGE ( 'NONE', *, *, #181862, .T. ) ;
#28945 = ADVANCED_FACE ( 'NONE', ( #104878 ), #204016, .T. ) ;
#28946 = AXIS2_PLACEMENT_3D ( 'NONE', #231960, #11623, #29912 ) ;
#28947 = LINE ( 'NONE', #48451, #48149 ) ;
#28948 = CIRCLE ( 'NONE', #241297, 0.9750000000000036415 ) ;
#28949 = CARTESIAN_POINT ( 'NONE',  ( -20.85000000000000142, 0.000000000000000000, -41.40000000000000568 ) ) ;
#28950 = ADVANCED_FACE ( 'NONE', ( #244427 ), #65794, .F. ) ;
#28951 = ORIENTED_EDGE ( 'NONE', *, *, #108045, .F. ) ;
#28952 = DIRECTION ( 'NONE',  ( -3.469446951953515108E-14, -1.000000000000000000, 0.000000000000000000 ) ) ;
#28953 = VECTOR ( 'NONE', #165742, 1000.000000000000000 ) ;
#28954 = ORIENTED_EDGE ( 'NONE', *, *, #12491, .F. ) ;
#28955 = CARTESIAN_POINT ( 'NONE',  ( -21.14999999999999858, 64.35000000001268461, -203.4231074845244507 ) ) ;
#28956 = ORIENTED_EDGE ( 'NONE', *, *, #205647, .T. ) ;
#28957 = CARTESIAN_POINT ( 'NONE',  ( -18.59999999999999787, 66.65000000001205649, -124.2731074845243597 ) ) ;
#28958 =( BOUNDED_CURVE ( )  B_SPLINE_CURVE ( 3, ( #139684, #91900, #99276, #60155 ),
 .UNSPECIFIED., .F., .F. ) 
 B_SPLINE_CURVE_WITH_KNOTS ( ( 4, 4 ),
 ( 3.141592653589719397, 4.712388980384693227 ),
 .UNSPECIFIED. ) 
 CURVE ( )  GEOMETRIC_REPRESENTATION_ITEM ( )  RATIONAL_B_SPLINE_CURVE ( ( 1.000000000000000000, 0.8047378541243468408, 0.8047378541243468408, 1.000000000000000000 ) ) 
 REPRESENTATION_ITEM ( '' )  );
#28959 = DIRECTION ( 'NONE',  ( 0.000000000000000000, 0.000000000000000000, -1.000000000000000000 ) ) ;
#28960 = CARTESIAN_POINT ( 'NONE',  ( 13.40000000000005898, 66.35000000001119247, -21.02310748452479316 ) ) ;
#28961 = ADVANCED_FACE ( 'NONE', ( #153085 ), #73534, .T. ) ;
#28962 = CARTESIAN_POINT ( 'NONE',  ( 23.24999999999999645, 1.115600667400684642E-11, -100.5000000000000426 ) ) ;
#28963 = CIRCLE ( 'NONE', #191245, 0.09999999999999108213 ) ;
#28964 = EDGE_CURVE ( 'NONE', #194795, #165593, #98463, .T. ) ;
#28965 = CARTESIAN_POINT ( 'NONE',  ( -23.25000000000000000, 7.128833340093095217, -233.7327013124392749 ) ) ;
#28966 = CARTESIAN_POINT ( 'NONE',  ( 19.58285714285715073, 65.61500148966047163, -95.39342281713442162 ) ) ;
#28967 = ORIENTED_EDGE ( 'NONE', *, *, #220656, .T. ) ;
#28969 = LINE ( 'NONE', #143719, #106160 ) ;
#28968 = AXIS2_PLACEMENT_3D ( 'NONE', #100719, #179051, #141177 ) ;
#28970 = ORIENTED_EDGE ( 'NONE', *, *, #64343, .T. ) ;
#28972 = CARTESIAN_POINT ( 'NONE',  ( 20.85000000000000142, 7.128833340094563376, -233.7327013124401276 ) ) ;
#28971 = CYLINDRICAL_SURFACE ( 'NONE', #111337, 0.1000000000000000472 ) ;
#28973 = ORIENTED_EDGE ( 'NONE', *, *, #79876, .T. ) ;
#28974 = CARTESIAN_POINT ( 'NONE',  ( -17.11825945287482753, 10.05000000001113847, -46.15000000000000568 ) ) ;
#28975 = CARTESIAN_POINT ( 'NONE',  ( 20.04999999999999716, 67.25000000001227818, -157.3731074845244109 ) ) ;
#28976 = CARTESIAN_POINT ( 'NONE',  ( -23.25000000000000000, 77.83585931145498193, -24.41866831572578533 ) ) ;
#28977 = ORIENTED_EDGE ( 'NONE', *, *, #49074, .F. ) ;
#28979 = ORIENTED_EDGE ( 'NONE', *, *, #192763, .T. ) ;
#28978 = CARTESIAN_POINT ( 'NONE',  ( 21.14999999999999503, 12.71802988599559647, -223.5105008658000258 ) ) ;
#28980 = CARTESIAN_POINT ( 'NONE',  ( 23.14999999999999858, 71.00000000001151079, -48.42837350343745584 ) ) ;
#28982 = CARTESIAN_POINT ( 'NONE',  ( 18.53691006697109600, 15.32283903239712330, -222.9441006232443669 ) ) ;
#28981 = CARTESIAN_POINT ( 'NONE',  ( -18.50000000000000000, 44.52640028187936849, -247.3006740988509193 ) ) ;
#28984 = ORIENTED_EDGE ( 'NONE', *, *, #59562, .F. ) ;
#28983 = CARTESIAN_POINT ( 'NONE',  ( -18.40000000000000213, 8.822561741677553471, -191.7499999999999716 ) ) ;
#28985 = VECTOR ( 'NONE', #3867, 1000.000000000000000 ) ;
#28986 = ORIENTED_EDGE ( 'NONE', *, *, #165647, .F. ) ;
#28987 = CARTESIAN_POINT ( 'NONE',  ( -20.94999999999999929, 64.30000000001219007, -143.2781056340430439 ) ) ;
#28988 = FACE_OUTER_BOUND ( 'NONE', #212380, .T. ) ;
#28989 = EDGE_LOOP ( 'NONE', ( #216052, #212467 ) ) ;
#28990 = VERTEX_POINT ( 'NONE', #206590 ) ;
#28991 = DIRECTION ( 'NONE',  ( 0.000000000000000000, -7.026728003956695223E-15, 1.000000000000000000 ) ) ;
#28992 = CARTESIAN_POINT ( 'NONE',  ( 19.97071067811865674, 34.39212750349580006, -235.0405048756463486 ) ) ;
#28993 = ORIENTED_EDGE ( 'NONE', *, *, #49354, .T. ) ;
#28994 = DIRECTION ( 'NONE',  ( 1.000000000000000000, 0.000000000000000000, 0.000000000000000000 ) ) ;
#28995 = AXIS2_PLACEMENT_3D ( 'NONE', #161005, #606, #239255 ) ;
#28996 = AXIS2_PLACEMENT_3D ( 'NONE', #49576, #129116, #110822 ) ;
#28997 = ORIENTED_EDGE ( 'NONE', *, *, #95303, .T. ) ;
#28998 = AXIS2_PLACEMENT_3D ( 'NONE', #17601, #56706, #22785 ) ;
#28999 = AXIS2_PLACEMENT_3D ( 'NONE', #170884, #226948, #250365 ) ;
#29000 = CARTESIAN_POINT ( 'NONE',  ( 21.14999999999999858, 6.390846877240206503, -199.6081416912452653 ) ) ;
#29001 = EDGE_LOOP ( 'NONE', ( #249948, #253133, #170357, #248624 ) ) ;
#29002 = ORIENTED_EDGE ( 'NONE', *, *, #117134, .F. ) ;
#29003 = DIRECTION ( 'NONE',  ( -0.000000000000000000, 0.000000000000000000, -1.000000000000000000 ) ) ;
#29004 = EDGE_LOOP ( 'NONE', ( #215813, #86730, #187208, #198955 ) ) ;
#29005 = CARTESIAN_POINT ( 'NONE',  ( -16.86132326855786090, 9.950000000011133494, -46.19863578466831910 ) ) ;
#29007 = ADVANCED_FACE ( 'NONE', ( #107487 ), #111349, .T. ) ;
#29006 = ORIENTED_EDGE ( 'NONE', *, *, #85586, .F. ) ;
#29009 = ORIENTED_EDGE ( 'NONE', *, *, #85843, .F. ) ;
#29008 = CARTESIAN_POINT ( 'NONE',  ( 18.59999999999999787, 7.128833340093095217, -233.7327013124392749 ) ) ;
#29010 = DIRECTION ( 'NONE',  ( 0.000000000000000000, 0.000000000000000000, 1.000000000000000000 ) ) ;
#29011 = ORIENTED_EDGE ( 'NONE', *, *, #164931, .T. ) ;
#29012 = EDGE_CURVE ( 'NONE', #144435, #235216, #98537, .T. ) ;
#29013 = CARTESIAN_POINT ( 'NONE',  ( 21.14999999999999858, 65.49889199258218753, -241.8691648588935266 ) ) ;
#29014 = AXIS2_PLACEMENT_3D ( 'NONE', #99843, #159876, #60731 ) ;
#29016 = ADVANCED_FACE ( 'NONE', ( #8403 ), #167491, .T. ) ;
#29015 = AXIS2_PLACEMENT_3D ( 'NONE', #110569, #130129, #233116 ) ;
#29017 = EDGE_LOOP ( 'NONE', ( #189642, #112689, #236184, #147629 ) ) ;
#29020 = ORIENTED_EDGE ( 'NONE', *, *, #5960, .T. ) ;
#29019 = EDGE_LOOP ( 'NONE', ( #246473, #107821, #226374, #208374 ) ) ;
#29018 = DIRECTION ( 'NONE',  ( -1.000000000000000000, -0.000000000000000000, -0.000000000000000000 ) ) ;
#29022 = CARTESIAN_POINT ( 'NONE',  ( 20.94999999999999929, 69.45000000001186891, -90.77310748452435973 ) ) ;
#29021 = AXIS2_PLACEMENT_3D ( 'NONE', #232905, #208197, #131200 ) ;
#29023 = LINE ( 'NONE', #52369, #143959 ) ;
#29024 = VERTEX_POINT ( 'NONE', #147916 ) ;
#29025 = AXIS2_PLACEMENT_3D ( 'NONE', #65972, #242035, #206768 ) ;
#29026 = ORIENTED_EDGE ( 'NONE', *, *, #225704, .F. ) ;
#29027 = EDGE_CURVE ( 'NONE', #53966, #171512, #69384, .T. ) ;
#29028 = DIRECTION ( 'NONE',  ( -1.000000000000000000, -0.000000000000000000, -0.000000000000000000 ) ) ;
#29029 = CARTESIAN_POINT ( 'NONE',  ( -18.69999999999999929, 1.350000000000000089, 16.60000000000000142 ) ) ;
#29031 = ORIENTED_EDGE ( 'NONE', *, *, #202066, .F. ) ;
#29030 = DIRECTION ( 'NONE',  ( 0.000000000000000000, -1.000000000000000000, 0.000000000000000000 ) ) ;
#29032 = DIRECTION ( 'NONE',  ( 0.000000000000000000, 0.000000000000000000, 1.000000000000000000 ) ) ;
#29033 = ORIENTED_EDGE ( 'NONE', *, *, #215428, .T. ) ;
#29034 = FACE_OUTER_BOUND ( 'NONE', #87645, .T. ) ;
#29035 = FACE_OUTER_BOUND ( 'NONE', #7927, .T. ) ;
#29036 = ORIENTED_EDGE ( 'NONE', *, *, #38810, .F. ) ;
#29037 = DIRECTION ( 'NONE',  ( 0.000000000000000000, 0.000000000000000000, -1.000000000000000000 ) ) ;
#29038 = FACE_BOUND ( 'NONE', #103028, .T. ) ;
#29039 = EDGE_LOOP ( 'NONE', ( #254555, #70789, #196064, #117543 ) ) ;
#29041 = ORIENTED_EDGE ( 'NONE', *, *, #198237, .T. ) ;
#29040 = CARTESIAN_POINT ( 'NONE',  ( -18.39999999999999858, -9.499999999988849808, -207.6001893912220169 ) ) ;
#29042 = CIRCLE ( 'NONE', #49838, 11.74999999999999822 ) ;
#29043 = CARTESIAN_POINT ( 'NONE',  ( 21.05000000000000071, 76.00000000001189449, -101.1231074845242972 ) ) ;
#29045 = ORIENTED_EDGE ( 'NONE', *, *, #204191, .F. ) ;
#29044 = VERTEX_POINT ( 'NONE', #227432 ) ;
#29046 = ORIENTED_EDGE ( 'NONE', *, *, #106565, .T. ) ;
#29047 = DIRECTION ( 'NONE',  ( -3.265361837132813093E-16, -1.000000000000000000, 7.445645354460596589E-46 ) ) ;
#29048 = EDGE_CURVE ( 'NONE', #105944, #213256, #244320, .T. ) ;
#29049 = ORIENTED_EDGE ( 'NONE', *, *, #184231, .F. ) ;
#29050 = EDGE_CURVE ( 'NONE', #218543, #115457, #102648, .T. ) ;
#29051 = DIRECTION ( 'NONE',  ( 1.000000000000000000, 0.000000000000000000, 0.000000000000000000 ) ) ;
#29052 = ORIENTED_EDGE ( 'NONE', *, *, #251102, .F. ) ;
#29053 = CARTESIAN_POINT ( 'NONE',  ( 23.15000000000000213, 82.09643798151613225, -215.4278993322501208 ) ) ;
#29054 = PLANE ( 'NONE',  #177410 ) ;
#29055 = ORIENTED_EDGE ( 'NONE', *, *, #232480, .T. ) ;
#29057 = ADVANCED_FACE ( 'NONE', ( #249585 ), #107145, .T. ) ;
#29056 = ORIENTED_EDGE ( 'NONE', *, *, #123062, .F. ) ;
#29059 = ORIENTED_EDGE ( 'NONE', *, *, #239166, .T. ) ;
#29058 = TOROIDAL_SURFACE ( 'NONE', #8180, 11.65000000000000036, 0.1000000000000000056 ) ;
#29060 = CARTESIAN_POINT ( 'NONE',  ( -23.15000000000000213, 1.115600667400684642E-11, -33.50000000000000000 ) ) ;
#29061 = VERTEX_POINT ( 'NONE', #188306 ) ;
#29062 = DIRECTION ( 'NONE',  ( 0.000000000000000000, 0.8660254037844411501, 0.4999999999999956701 ) ) ;
#29064 = VERTEX_POINT ( 'NONE', #150486 ) ;
#29063 = DIRECTION ( 'NONE',  ( -2.940209281316621509E-16, 1.000000000000000000, 2.352167425053297207E-15 ) ) ;
#29065 = CARTESIAN_POINT ( 'NONE',  ( -21.05000000000000071, 1.115600667400684642E-11, -55.19999999999999574 ) ) ;
#29066 = LINE ( 'NONE', #108565, #72586 ) ;
#29067 = AXIS2_PLACEMENT_3D ( 'NONE', #217655, #2468, #84538 ) ;
#29069 = TOROIDAL_SURFACE ( 'NONE', #83144, 11.65000000000000036, 0.1000000000000000056 ) ;
#29068 = DIRECTION ( 'NONE',  ( 1.000000000000000000, 0.000000000000000000, 0.000000000000000000 ) ) ;
#29070 = DIRECTION ( 'NONE',  ( 0.000000000000000000, 2.891205793294679805E-16, -1.000000000000000000 ) ) ;
#29072 = ADVANCED_FACE ( 'NONE', ( #130903 ), #144555, .T. ) ;
#29071 = DIRECTION ( 'NONE',  ( -1.000000000000000000, -0.000000000000000000, -0.000000000000000000 ) ) ;
#29074 = LINE ( 'NONE', #249378, #186930 ) ;
#29073 = FACE_OUTER_BOUND ( 'NONE', #35595, .T. ) ;
#29075 = CARTESIAN_POINT ( 'NONE',  ( 23.15000000000000213, -8.999999999988844479, -76.89396912265249284 ) ) ;
#29076 = CARTESIAN_POINT ( 'NONE',  ( 18.49999999999999645, 38.22609996598573190, -261.0782621420140117 ) ) ;
#29077 = CARTESIAN_POINT ( 'NONE',  ( 23.24999999999999645, 8.822561741677553471, -87.85000000000003695 ) ) ;
#29078 = EDGE_LOOP ( 'NONE', ( #236940, #88961, #231994, #147626 ) ) ;
#29079 = CIRCLE ( 'NONE', #149867, 0.1000000000000002554 ) ;
#29080 = CIRCLE ( 'NONE', #212219, 0.09999999999999693856 ) ;
#29081 = CIRCLE ( 'NONE', #158260, 0.1000000000000106498 ) ;
#29082 = AXIS2_PLACEMENT_3D ( 'NONE', #201582, #159920, #239445 ) ;
#29083 = TOROIDAL_SURFACE ( 'NONE', #116534, 14.20833333333334103, 0.1000000000000000056 ) ;
#29084 = EDGE_CURVE ( 'NONE', #128325, #31427, #145135, .T. ) ;
#29085 = ORIENTED_EDGE ( 'NONE', *, *, #110953, .T. ) ;
#29088 = ORIENTED_EDGE ( 'NONE', *, *, #80755, .F. ) ;
#29087 = EDGE_CURVE ( 'NONE', #48436, #216777, #95623, .T. ) ;
#29086 = CARTESIAN_POINT ( 'NONE',  ( -20.94999999999999929, 74.63912941281984104, -94.95010955743335046 ) ) ;
#29089 = EDGE_LOOP ( 'NONE', ( #133919, #132583, #96643, #11594, #54564 ) ) ;
#29090 = AXIS2_PLACEMENT_3D ( 'NONE', #41273, #16559, #136463 ) ;
#29091 = DIRECTION ( 'NONE',  ( 0.000000000000000000, 0.000000000000000000, -1.000000000000000000 ) ) ;
#29092 = CARTESIAN_POINT ( 'NONE',  ( 20.22516295850462598, 9.899364295461838381, -141.9100657120906135 ) ) ;
#29093 = EDGE_CURVE ( 'NONE', #253828, #145505, #165429, .T. ) ;
#29094 = EDGE_CURVE ( 'NONE', #97897, #17019, #253416, .T. ) ;
#29096 = DIRECTION ( 'NONE',  ( -1.000000000000000000, 0.000000000000000000, -0.000000000000000000 ) ) ;
#29095 = CARTESIAN_POINT ( 'NONE',  ( 23.24999999999999645, 5.000000000011153745, -112.9052660189131245 ) ) ;
#29097 = ORIENTED_EDGE ( 'NONE', *, *, #10243, .F. ) ;
#29098 = ORIENTED_EDGE ( 'NONE', *, *, #34408, .T. ) ;
#29099 =( NAMED_UNIT ( * ) SI_UNIT ( $, .STERADIAN. ) SOLID_ANGLE_UNIT ( ) );
#29100 = CARTESIAN_POINT ( 'NONE',  ( 18.39999999999999858, -9.519327731081279609, -40.47297637655933755 ) ) ;
#29101 = DIRECTION ( 'NONE',  ( 0.000000000000000000, 0.000000000000000000, 1.000000000000000000 ) ) ;
#29102 = ORIENTED_EDGE ( 'NONE', *, *, #51478, .T. ) ;
#29103 = EDGE_CURVE ( 'NONE', #216057, #2617, #140452, .T. ) ;
#29104 = FACE_OUTER_BOUND ( 'NONE', #50059, .T. ) ;
#29105 = CARTESIAN_POINT ( 'NONE',  ( -16.81453046979148880, 9.939102281452070642, -180.2117265236030050 ) ) ;
#29106 = EDGE_CURVE ( 'NONE', #231809, #177416, #115198, .T. ) ;
#29107 = FACE_OUTER_BOUND ( 'NONE', #213870, .T. ) ;
#29108 = DIRECTION ( 'NONE',  ( -1.000000000000000000, 0.000000000000000000, 0.000000000000000000 ) ) ;
#29109 = FACE_OUTER_BOUND ( 'NONE', #71549, .T. ) ;
#29111 = VERTEX_POINT ( 'NONE', #155646 ) ;
#29110 = CARTESIAN_POINT ( 'NONE',  ( 20.99999999999999645, 66.25000000001226397, -149.1731074845244223 ) ) ;
#29112 = ADVANCED_FACE ( 'NONE', ( #119059 ), #77912, .F. ) ;
#29113 = DIRECTION ( 'NONE',  ( 1.000000000000000000, 0.000000000000000000, 0.000000000000000000 ) ) ;
#29114 = CARTESIAN_POINT ( 'NONE',  ( 23.24999999999999289, 4.054946580507614584, -200.1168758698121053 ) ) ;
#29115 = DIRECTION ( 'NONE',  ( 1.000000000000000000, 0.000000000000000000, 0.000000000000000000 ) ) ;
#29116 = CYLINDRICAL_SURFACE ( 'NONE', #78983, 0.1999999999999987899 ) ;
#29117 = EDGE_LOOP ( 'NONE', ( #1824, #190933 ) ) ;
#29118 = CARTESIAN_POINT ( 'NONE',  ( -23.15000000000000213, 84.66355140188112216, -112.5472086025915388 ) ) ;
#29119 = AXIS2_PLACEMENT_3D ( 'NONE', #14851, #133486, #35703 ) ;
#29120 = DIRECTION ( 'NONE',  ( -1.186688945009009584E-16, 0.4721928772777345684, 0.8814952561688429444 ) ) ;
#29121 = EDGE_CURVE ( 'NONE', #47498, #252850, #233864, .T. ) ;
#29123 = DIRECTION ( 'NONE',  ( 1.000000000000000000, 0.000000000000000000, 0.000000000000000000 ) ) ;
#29122 = DIRECTION ( 'NONE',  ( -1.000000000000000000, -0.000000000000000000, 0.000000000000000000 ) ) ;
#29124 = DIRECTION ( 'NONE',  ( 1.000000000000000000, 0.000000000000000000, 0.000000000000000000 ) ) ;
#29125 = CIRCLE ( 'NONE', #8417, 0.1000000000000028644 ) ;
#29126 = CARTESIAN_POINT ( 'NONE',  ( -16.88705144915408596, 9.950000000011193890, -54.06902140528774936 ) ) ;
#29127 = CARTESIAN_POINT ( 'NONE',  ( 20.95000000000005258, 66.25000000001119815, -6.023107484524794941 ) ) ;
#29128 = FACE_OUTER_BOUND ( 'NONE', #196089, .T. ) ;
#29129 = DIRECTION ( 'NONE',  ( -0.7071067811865388020, 0.7071067811865561215, 0.000000000000000000 ) ) ;
#29130 = CARTESIAN_POINT ( 'NONE',  ( -23.15000000000000213, 1.115600667400684642E-11, -167.5000000000000284 ) ) ;
#29131 = EDGE_CURVE ( 'NONE', #249063, #113349, #65452, .T. ) ;
#29132 = EDGE_CURVE ( 'NONE', #211121, #138858, #219559, .T. ) ;
#29134 = ORIENTED_EDGE ( 'NONE', *, *, #221941, .T. ) ;
#29133 = AXIS2_PLACEMENT_3D ( 'NONE', #233419, #172190, #93880 ) ;
#29135 = ORIENTED_EDGE ( 'NONE', *, *, #13559, .F. ) ;
#29136 = ORIENTED_EDGE ( 'NONE', *, *, #241293, .T. ) ;
#29137 = EDGE_CURVE ( 'NONE', #235074, #162495, #223647, .T. ) ;
#29138 = CARTESIAN_POINT ( 'NONE',  ( 20.86036036209901923, 65.37895722344093485, -95.35675906601939289 ) ) ;
#29139 = DIRECTION ( 'NONE',  ( 0.000000000000000000, -0.9910827722268055195, 0.1332476588733540468 ) ) ;
#29140 = ORIENTED_EDGE ( 'NONE', *, *, #166302, .F. ) ;
#29141 = EDGE_CURVE ( 'NONE', #75516, #167339, #28067, .T. ) ;
#29142 = TOROIDAL_SURFACE ( 'NONE', #204045, 0.2000000000000000111, 0.1000000000000000056 ) ;
#29143 = EDGE_LOOP ( 'NONE', ( #121915, #90277, #38265, #95311, #150795, #143227, #131386, #172057, #113780, #11726, #190775, #134159, #35143, #62986, #86744, #242107, #121146, #16323 ) ) ;
#29144 = ADVANCED_FACE ( 'NONE', ( #257221 ), #175223, .T. ) ;
#29145 = ORIENTED_EDGE ( 'NONE', *, *, #87534, .F. ) ;
#29146 = DIRECTION ( 'NONE',  ( 0.000000000000000000, 1.000000000000000000, 6.982962677686266711E-15 ) ) ;
#29147 = AXIS2_PLACEMENT_3D ( 'NONE', #9787, #151897, #54047 ) ;
#29148 = VERTEX_POINT ( 'NONE', #194761 ) ;
#29149 = FACE_OUTER_BOUND ( 'NONE', #203469, .T. ) ;
#29150 = CARTESIAN_POINT ( 'NONE',  ( 18.59999999999999432, 14.72981487416292623, -236.4853282537515895 ) ) ;
#29151 = DIRECTION ( 'NONE',  ( 1.000000000000000000, 2.952720810173289112E-16, -0.000000000000000000 ) ) ;
#29152 = CARTESIAN_POINT ( 'NONE',  ( -16.97048361161166952, 29.77341243951207872, -234.5751436903205160 ) ) ;
#29153 = FACE_OUTER_BOUND ( 'NONE', #74772, .T. ) ;
#29155 = ORIENTED_EDGE ( 'NONE', *, *, #182694, .T. ) ;
#29154 = FACE_OUTER_BOUND ( 'NONE', #115684, .T. ) ;
#29157 = CARTESIAN_POINT ( 'NONE',  ( -21.64999999999999858, 68.65000000001205649, -124.1731074845243512 ) ) ;
#29156 = FACE_OUTER_BOUND ( 'NONE', #54619, .T. ) ;
#29158 = EDGE_CURVE ( 'NONE', #86618, #84696, #128008, .T. ) ;
#29159 = FACE_OUTER_BOUND ( 'NONE', #119028, .T. ) ;
#29160 = ORIENTED_EDGE ( 'NONE', *, *, #208296, .F. ) ;
#29161 = DIRECTION ( 'NONE',  ( 0.000000000000000000, -6.352154140967427193E-15, 1.000000000000000000 ) ) ;
#29162 = DIRECTION ( 'NONE',  ( 0.000000000000000000, 0.000000000000000000, -1.000000000000000000 ) ) ;
#29163 = LINE ( 'NONE', #249464, #45775 ) ;
#29164 = EDGE_LOOP ( 'NONE', ( #19876, #179780, #232334, #178753 ) ) ;
#29165 = CARTESIAN_POINT ( 'NONE',  ( -21.13614978966381841, 6.499104701844946597, -33.49999999999999289 ) ) ;
#29166 = AXIS2_PLACEMENT_3D ( 'NONE', #184748, #246024, #183483 ) ;
#29167 = AXIS2_PLACEMENT_3D ( 'NONE', #240282, #57761, #116475 ) ;
#29168 = CARTESIAN_POINT ( 'NONE',  ( -16.82055514392348172, 66.05000000001182059, -82.19990555906684904 ) ) ;
#29169 = VERTEX_POINT ( 'NONE', #35693 ) ;
#29170 = PLANE ( 'NONE',  #253563 ) ;
#29171 = LINE ( 'NONE', #111231, #132268 ) ;
#29172 = CARTESIAN_POINT ( 'NONE',  ( -21.55000000000000426, 7.750000000011155521, -179.8499999999999943 ) ) ;
#29173 = ORIENTED_EDGE ( 'NONE', *, *, #169248, .F. ) ;
#29174 = ORIENTED_EDGE ( 'NONE', *, *, #11859, .F. ) ;
#29175 = DIRECTION ( 'NONE',  ( 0.000000000000000000, 0.000000000000000000, -1.000000000000000000 ) ) ;
#29176 = CARTESIAN_POINT ( 'NONE',  ( 18.59999999999999432, 1.162701749949165642, -175.5999999999999659 ) ) ;
#29177 = AXIS2_PLACEMENT_3D ( 'NONE', #151740, #147869, #52597 ) ;
#29178 = EDGE_CURVE ( 'NONE', #55862, #102889, #202818, .T. ) ;
#29179 = CARTESIAN_POINT ( 'NONE',  ( -20.00857864376270001, 11.56851667937982775, -211.1200010790121553 ) ) ;
#29181 = DIRECTION ( 'NONE',  ( -0.000000000000000000, -0.000000000000000000, -1.000000000000000000 ) ) ;
#29180 = VECTOR ( 'NONE', #239129, 1000.000000000000000 ) ;
#29182 = AXIS2_PLACEMENT_3D ( 'NONE', #19092, #238132, #122055 ) ;
#29184 = VECTOR ( 'NONE', #175667, 1000.000000000000000 ) ;
#29183 = CARTESIAN_POINT ( 'NONE',  ( 20.94999999999999929, 1.115649653272650466E-11, -63.00000000000000000 ) ) ;
#29185 = DIRECTION ( 'NONE',  ( 0.000000000000000000, 0.9126074666063771490, 0.4088369013363278293 ) ) ;
#29186 = ADVANCED_FACE ( 'NONE', ( #16124 ), #157051, .F. ) ;
#29187 = DIRECTION ( 'NONE',  ( 0.000000000000000000, 1.000000000000000000, 0.000000000000000000 ) ) ;
#29188 = CARTESIAN_POINT ( 'NONE',  ( 18.60000000000000497, 76.00000000001237765, -170.0231074845243597 ) ) ;
#29189 = ORIENTED_EDGE ( 'NONE', *, *, #166328, .F. ) ;
#29190 = CARTESIAN_POINT ( 'NONE',  ( -23.25000000000000000, 64.25000000001277556, -215.2731074845244450 ) ) ;
#29192 = ORIENTED_EDGE ( 'NONE', *, *, #47897, .T. ) ;
#29191 = CARTESIAN_POINT ( 'NONE',  ( -22.39999999999999858, -0.09999999998884338825, -155.8504291924551808 ) ) ;
#29193 = CIRCLE ( 'NONE', #158362, 0.09999999999999939493 ) ;
#29194 = CARTESIAN_POINT ( 'NONE',  ( 20.94999999999999929, 76.00000000001195133, -103.0231074845243171 ) ) ;
#29195 = LINE ( 'NONE', #151699, #128123 ) ;
#29196 = DIRECTION ( 'NONE',  ( 1.000000000000000000, 0.000000000000000000, 0.000000000000000000 ) ) ;
#29197 = CARTESIAN_POINT ( 'NONE',  ( 21.05000000000000071, 70.62751970751253339, -223.3325012285725109 ) ) ;
#29198 = EDGE_CURVE ( 'NONE', #88017, #178217, #98729, .T. ) ;
#29199 = EDGE_CURVE ( 'NONE', #83997, #16604, #19677, .T. ) ;
#29200 = CARTESIAN_POINT ( 'NONE',  ( -23.15000000000000213, 82.09643798151613225, -215.4278993322501208 ) ) ;
#29202 = VERTEX_POINT ( 'NONE', #65484 ) ;
#29201 = DIRECTION ( 'NONE',  ( -1.000000000000000000, 0.000000000000000000, 0.000000000000000000 ) ) ;
#29204 = CARTESIAN_POINT ( 'NONE',  ( -23.25000000000000000, 5.082284216461512198E-16, 4.149999999999999467 ) ) ;
#29203 =( REPRESENTATION_RELATIONSHIP ('NONE','NONE', #36900, #206680 ) REPRESENTATION_RELATIONSHIP_WITH_TRANSFORMATION ( #42937 )SHAPE_REPRESENTATION_RELATIONSHIP( ) );
#29205 = DIRECTION ( 'NONE',  ( -3.265361837132813093E-16, -0.9651348961777157509, 0.2617529984165031243 ) ) ;
#29206 = CARTESIAN_POINT ( 'NONE',  ( -23.25000000000000000, -11.48912529306489994, -197.8999999999999773 ) ) ;
#29207 = FACE_OUTER_BOUND ( 'NONE', #186459, .T. ) ;
#29208 = EDGE_LOOP ( 'NONE', ( #112153, #111300, #139923, #74856 ) ) ;
#29209 = DIRECTION ( 'NONE',  ( 0.000000000000000000, 0.2617529984165031243, 0.9651348961777157509 ) ) ;
#29211 = VERTEX_POINT ( 'NONE', #100725 ) ;
#29210 = CIRCLE ( 'NONE', #41652, 0.09999999999999939493 ) ;
#29212 = DIRECTION ( 'NONE',  ( 0.000000000000000000, 1.000000000000000000, -6.308085367188393199E-16 ) ) ;
#29213 = AXIS2_PLACEMENT_3D ( 'NONE', #107489, #223566, #187057 ) ;
#29214 = DIRECTION ( 'NONE',  ( 1.296989514748957922E-15, -0.9887567792719341719, 0.1495327102803664099 ) ) ;
#29215 = ORIENTED_EDGE ( 'NONE', *, *, #101182, .T. ) ;
#29216 = DIRECTION ( 'NONE',  ( 0.000000000000000000, 0.000000000000000000, -1.000000000000000000 ) ) ;
#29217 = ORIENTED_EDGE ( 'NONE', *, *, #129528, .F. ) ;
#29218 = DIRECTION ( 'NONE',  ( 0.000000000000000000, -0.9915357197604804940, 0.1298341882520397950 ) ) ;
#29219 = CARTESIAN_POINT ( 'NONE',  ( 20.94999999999999929, 11.41170713998153019, -246.6906184681487275 ) ) ;
#29220 = DIRECTION ( 'NONE',  ( 0.7071067811865463515, -0.7071067811865487940, -5.696443396193425170E-15 ) ) ;
#29221 = ORIENTED_EDGE ( 'NONE', *, *, #187309, .T. ) ;
#29222 = FACE_OUTER_BOUND ( 'NONE', #187232, .T. ) ;
#29223 = CARTESIAN_POINT ( 'NONE',  ( 18.59999999999999076, 70.05000000001267324, -193.2174051794895320 ) ) ;
#29224 = CARTESIAN_POINT ( 'NONE',  ( 15.31784899511109721, 9.396630376317714806, -17.90705739281830589 ) ) ;
#29226 = CARTESIAN_POINT ( 'NONE',  ( 20.99142135623731065, 11.60000000001116049, -160.5717967697245285 ) ) ;
#29225 = CIRCLE ( 'NONE', #33318, 1.900000000000004574 ) ;
#29227 = ADVANCED_FACE ( 'NONE', ( #5490 ), #102847, .F. ) ;
#29228 = CARTESIAN_POINT ( 'NONE',  ( -18.59999999999999787, 7.021664781911246322, -70.73356540189729458 ) ) ;
#29229 = ORIENTED_EDGE ( 'NONE', *, *, #202946, .F. ) ;
#29231 = ORIENTED_EDGE ( 'NONE', *, *, #122087, .F. ) ;
#29230 = FACE_OUTER_BOUND ( 'NONE', #125951, .T. ) ;
#29232 = VERTEX_POINT ( 'NONE', #1649 ) ;
#29233 = LINE ( 'NONE', #7047, #65435 ) ;
#29234 = ORIENTED_EDGE ( 'NONE', *, *, #87920, .T. ) ;
#29235 = CARTESIAN_POINT ( 'NONE',  ( 21.05000000000000071, 61.15208969432440966, -234.1845329146948131 ) ) ;
#29236 = DIRECTION ( 'NONE',  ( 0.000000000000000000, 0.000000000000000000, 1.000000000000000000 ) ) ;
#29237 = DIRECTION ( 'NONE',  ( 0.000000000000000000, -1.000000000000000000, 0.000000000000000000 ) ) ;
#29238 = AXIS2_PLACEMENT_3D ( 'NONE', #190098, #170586, #28496 ) ;
#29239 = VERTEX_POINT ( 'NONE', #81182 ) ;
#29240 = CARTESIAN_POINT ( 'NONE',  ( -16.92132318717937522, 66.03392997600613512, -123.9007008541722996 ) ) ;
#29241 = CARTESIAN_POINT ( 'NONE',  ( -20.64999999999999858, 70.76939748184450707, -215.3970883796142743 ) ) ;
#29242 = ADVANCED_FACE ( 'NONE', ( #221965 ), #239003, .F. ) ;
#29243 = VERTEX_POINT ( 'NONE', #220716 ) ;
#29244 = CARTESIAN_POINT ( 'NONE',  ( -20.94999999999999929, 70.15000000001221281, -146.6556047088023149 ) ) ;
#29246 = ORIENTED_EDGE ( 'NONE', *, *, #48453, .F. ) ;
#29245 = DIRECTION ( 'NONE',  ( 1.000000000000000000, 0.000000000000000000, 0.000000000000000000 ) ) ;
#29248 = EDGE_CURVE ( 'NONE', #74091, #67839, #194476, .T. ) ;
#29247 = DIRECTION ( 'NONE',  ( 0.000000000000000000, 0.000000000000000000, -1.000000000000000000 ) ) ;
#29249 = CARTESIAN_POINT ( 'NONE',  ( -18.40000000000000213, 5.649999999999983480, -12.65000000000000213 ) ) ;
#29250 = TOROIDAL_SURFACE ( 'NONE', #41693, 12.97499999999999787, 0.1000000000000000056 ) ;
#29251 = CIRCLE ( 'NONE', #203982, 0.09999999999999939493 ) ;
#29252 = ORIENTED_EDGE ( 'NONE', *, *, #139782, .T. ) ;
#29253 = LINE ( 'NONE', #110023, #131230 ) ;
#29255 = ADVANCED_FACE ( 'NONE', ( #203724 ), #119635, .T. ) ;
#29254 = DIRECTION ( 'NONE',  ( 0.000000000000000000, -0.000000000000000000, 1.000000000000000000 ) ) ;
#29256 = CARTESIAN_POINT ( 'NONE',  ( -18.59999999999999787, 7.783179459866048866, -245.3643104511423303 ) ) ;
#29257 = ORIENTED_EDGE ( 'NONE', *, *, #254355, .F. ) ;
#29258 = DIRECTION ( 'NONE',  ( 1.000000000000000000, 0.000000000000000000, 0.000000000000000000 ) ) ;
#29259 = AXIS2_PLACEMENT_3D ( 'NONE', #12148, #27867, #186935 ) ;
#29260 = EDGE_CURVE ( 'NONE', #54771, #75787, #202438, .T. ) ;
#29261 = FACE_OUTER_BOUND ( 'NONE', #86386, .T. ) ;
#29262 = AXIS2_PLACEMENT_3D ( 'NONE', #117937, #236593, #138750 ) ;
#29263 = EDGE_CURVE ( 'NONE', #91559, #15975, #248610, .T. ) ;
#29264 = VECTOR ( 'NONE', #10301, 1000.000000000000000 ) ;
#29265 = ORIENTED_EDGE ( 'NONE', *, *, #208296, .T. ) ;
#29266 = EDGE_CURVE ( 'NONE', #33770, #108576, #104587, .T. ) ;
#29267 = CIRCLE ( 'NONE', #245698, 4.049999999999998046 ) ;
#29268 = VECTOR ( 'NONE', #174856, 1000.000000000000000 ) ;
#29269 = AXIS2_PLACEMENT_3D ( 'NONE', #186584, #13087, #229558 ) ;
#29270 = ORIENTED_EDGE ( 'NONE', *, *, #21154, .F. ) ;
#29272 = CARTESIAN_POINT ( 'NONE',  ( 22.14074124539698829, 68.60992214896893415, -203.6221603803684843 ) ) ;
#29271 = AXIS2_PLACEMENT_3D ( 'NONE', #20089, #99581, #240415 ) ;
#29273 = AXIS2_PLACEMENT_3D ( 'NONE', #163162, #228268, #232125 ) ;
#29274 = VERTEX_POINT ( 'NONE', #219411 ) ;
#29275 = CARTESIAN_POINT ( 'NONE',  ( -20.85000000000000142, 76.00000000001244871, -170.0231074845243597 ) ) ;
#29277 = ADVANCED_FACE ( 'NONE', ( #83731 ), #110381, .F. ) ;
#29276 = FACE_OUTER_BOUND ( 'NONE', #230997, .T. ) ;
#29279 = ORIENTED_EDGE ( 'NONE', *, *, #251746, .F. ) ;
#29278 = DIRECTION ( 'NONE',  ( 1.000000000000000000, 0.000000000000000000, 0.000000000000000000 ) ) ;
#29280 = CARTESIAN_POINT ( 'NONE',  ( -22.39999999999999858, 11.38316329224760359, -198.5208684056144079 ) ) ;
#29281 = DIRECTION ( 'NONE',  ( -0.000000000000000000, -6.982962677686266711E-15, 1.000000000000000000 ) ) ;
#29282 = CARTESIAN_POINT ( 'NONE',  ( -20.64999999999999858, -8.999999999988846255, -42.89396912265245021 ) ) ;
#29283 = FACE_OUTER_BOUND ( 'NONE', #57984, .T. ) ;
#29284 = CARTESIAN_POINT ( 'NONE',  ( 18.59999999999999432, 70.47363787294415260, -228.3418745167492432 ) ) ;
#29285 = CARTESIAN_POINT ( 'NONE',  ( -16.95709691156492127, 9.950000000011140600, -79.66005756250774539 ) ) ;
#29286 = FACE_OUTER_BOUND ( 'NONE', #152595, .T. ) ;
#29288 = ORIENTED_EDGE ( 'NONE', *, *, #55209, .F. ) ;
#29287 = DIRECTION ( 'NONE',  ( 0.000000000000000000, -0.4088369013363280513, 0.9126074666063772600 ) ) ;
#29289 = FACE_OUTER_BOUND ( 'NONE', #235852, .T. ) ;
#29290 = DIRECTION ( 'NONE',  ( 0.000000000000000000, 6.982962677686266711E-15, -1.000000000000000000 ) ) ;
#29291 = DIRECTION ( 'NONE',  ( -0.000000000000000000, 1.000000000000000000, 6.982962677686266711E-15 ) ) ;
#29292 = FACE_OUTER_BOUND ( 'NONE', #72042, .T. ) ;
#29293 = DIRECTION ( 'NONE',  ( -0.000000000000000000, 0.8660254037844377084, 0.5000000000000016653 ) ) ;
#29294 = ORIENTED_EDGE ( 'NONE', *, *, #124729, .T. ) ;
#29295 = CIRCLE ( 'NONE', #150080, 12.77499999999999503 ) ;
#29296 = DIRECTION ( 'NONE',  ( -1.000000000000000000, 0.000000000000000000, -0.000000000000000000 ) ) ;
#29297 = FACE_OUTER_BOUND ( 'NONE', #80336, .T. ) ;
#29298 = VECTOR ( 'NONE', #224283, 1000.000000000000000 ) ;
#29299 = ORIENTED_EDGE ( 'NONE', *, *, #1505, .F. ) ;
#29301 = EDGE_CURVE ( 'NONE', #75757, #41308, #44621, .T. ) ;
#29300 = DIRECTION ( 'NONE',  ( 0.000000000000000000, 0.000000000000000000, 1.000000000000000000 ) ) ;
#29302 = CARTESIAN_POINT ( 'NONE',  ( -16.93255653858138388, 9.998451453988312920, -79.58164336798972727 ) ) ;
#29303 = EDGE_LOOP ( 'NONE', ( #174258, #138070, #138580, #55651 ) ) ;
#29304 = PLANE ( 'NONE',  #140154 ) ;
#29305 = EDGE_LOOP ( 'NONE', ( #59532, #30026, #52916, #141542 ) ) ;
#29307 = EDGE_CURVE ( 'NONE', #175937, #15261, #61356, .T. ) ;
#29306 = DIRECTION ( 'NONE',  ( 0.000000000000000000, -1.000000000000000000, 0.000000000000000000 ) ) ;
#29308 = ORIENTED_EDGE ( 'NONE', *, *, #24639, .F. ) ;
#29309 = AXIS2_PLACEMENT_3D ( 'NONE', #244351, #47430, #27919 ) ;
#29310 = CARTESIAN_POINT ( 'NONE',  ( 20.84999999999999432, 7.021664781911246322, -104.3335654018973315 ) ) ;
#29311 = VECTOR ( 'NONE', #223988, 1000.000000000000000 ) ;
#29312 = EDGE_CURVE ( 'NONE', #37324, #245081, #256938, .T. ) ;
#29313 = LINE ( 'NONE', #10991, #80722 ) ;
#29314 = EDGE_CURVE ( 'NONE', #8860, #60251, #227755, .T. ) ;
#29315 = EDGE_LOOP ( 'NONE', ( #186817, #82819, #218529, #56246 ) ) ;
#29316 = ORIENTED_EDGE ( 'NONE', *, *, #122709, .T. ) ;
#29317 = FACE_BOUND ( 'NONE', #148798, .T. ) ;
#29319 = ORIENTED_EDGE ( 'NONE', *, *, #129543, .T. ) ;
#29318 = CARTESIAN_POINT ( 'NONE',  ( -23.15000000000000213, 64.40000000001249703, -176.9513107147999449 ) ) ;
#29320 = CARTESIAN_POINT ( 'NONE',  ( -40.23850191057533010, 87.75000000001119815, -4.523107484524794053 ) ) ;
#29321 = AXIS2_PLACEMENT_3D ( 'NONE', #126872, #229816, #51152 ) ;
#29322 = VERTEX_POINT ( 'NONE', #227123 ) ;
#29323 = AXIS2_PLACEMENT_3D ( 'NONE', #243976, #6647, #185294 ) ;
#29324 = ORIENTED_EDGE ( 'NONE', *, *, #72082, .T. ) ;
#29325 = EDGE_CURVE ( 'NONE', #41514, #257159, #211202, .T. ) ;
#29326 = LINE ( 'NONE', #128390, #203341 ) ;
#29327 = CARTESIAN_POINT ( 'NONE',  ( -15.55912972643741199, 10.96704414822730733, -211.4556836530944111 ) ) ;
#29328 = FACE_OUTER_BOUND ( 'NONE', #130502, .T. ) ;
#29329 = EDGE_CURVE ( 'NONE', #113369, #159975, #168496, .T. ) ;
#29330 = CARTESIAN_POINT ( 'NONE',  ( -21.05000000000000071, 76.00000000001213607, -136.5231074845242745 ) ) ;
#29331 = CARTESIAN_POINT ( 'NONE',  ( -23.15000000000000213, 68.70534379447684614, -223.0647885566232560 ) ) ;
#29332 = LINE ( 'NONE', #130961, #131153 ) ;
#29333 = ORIENTED_EDGE ( 'NONE', *, *, #174875, .T. ) ;
#29334 = CARTESIAN_POINT ( 'NONE',  ( -21.70464131381649509, 60.38329692807814553, -233.9978952701749506 ) ) ;
#29335 = DIRECTION ( 'NONE',  ( 1.000000000000000000, 0.000000000000000000, 0.000000000000000000 ) ) ;
#29337 = DIRECTION ( 'NONE',  ( 0.000000000000000000, 0.000000000000000000, 1.000000000000000000 ) ) ;
#29336 = PRODUCT_DEFINITION ( 'UNKNOWN', '', #115392, #134062 ) ;
#29338 = CIRCLE ( 'NONE', #179168, 3.899999999999999023 ) ;
#29339 = CYLINDRICAL_SURFACE ( 'NONE', #72201, 0.1000000000000000472 ) ;
#29340 = CIRCLE ( 'NONE', #58495, 4.049999999999990941 ) ;
#29341 = ORIENTED_EDGE ( 'NONE', *, *, #237310, .F. ) ;
#29342 = DIRECTION ( 'NONE',  ( 0.000000000000000000, 0.000000000000000000, 1.000000000000000000 ) ) ;
#29343 = ORIENTED_EDGE ( 'NONE', *, *, #219864, .T. ) ;
#29344 = CARTESIAN_POINT ( 'NONE',  ( -18.49346865148328334, -7.697768582032982643, -210.0301188723689449 ) ) ;
#29345 = ORIENTED_EDGE ( 'NONE', *, *, #29543, .T. ) ;
#29346 = CARTESIAN_POINT ( 'NONE',  ( -21.05000000000000071, 1.115600667400684642E-11, -167.4999999999999716 ) ) ;
#29347 = DIRECTION ( 'NONE',  ( 0.000000000000000000, -7.304098846218139203E-15, 1.000000000000000000 ) ) ;
#29348 = EDGE_CURVE ( 'NONE', #220835, #43053, #163629, .T. ) ;
#29349 = EDGE_LOOP ( 'NONE', ( #224367, #37568, #169751, #244990 ) ) ;
#29350 = EDGE_LOOP ( 'NONE', ( #230393, #111070, #191712, #20005 ) ) ;
#29352 = EDGE_LOOP ( 'NONE', ( #82610, #134913, #240621 ) ) ;
#29351 = DIRECTION ( 'NONE',  ( 0.000000000000000000, 0.000000000000000000, 1.000000000000000000 ) ) ;
#29353 = ADVANCED_FACE ( 'NONE', ( #30233 ), #245426, .T. ) ;
#29354 = DIRECTION ( 'NONE',  ( 0.000000000000000000, -0.2128009952263320570, 0.9770955615653377224 ) ) ;
#29355 = ORIENTED_EDGE ( 'NONE', *, *, #166904, .T. ) ;
#29356 = EDGE_CURVE ( 'NONE', #1798, #86120, #240426, .T. ) ;
#29357 = CARTESIAN_POINT ( 'NONE',  ( 23.15000000000000213, -9.500000000000000000, -23.60603087734755690 ) ) ;
#29358 = CARTESIAN_POINT ( 'NONE',  ( -18.50596464788227635, 65.69367753730635684, -64.01892380663478832 ) ) ;
#29359 = EDGE_LOOP ( 'NONE', ( #51269, #32616, #45795, #197967 ) ) ;
#29360 = AXIS2_PLACEMENT_3D ( 'NONE', #187971, #49732, #90123 ) ;
#29362 = VECTOR ( 'NONE', #176311, 1000.000000000000000 ) ;
#29361 = CARTESIAN_POINT ( 'NONE',  ( 20.94999999999999929, -8.999999999988844479, -110.3939691226524786 ) ) ;
#29363 = EDGE_CURVE ( 'NONE', #2598, #187000, #225818, .T. ) ;
#29365 = DIRECTION ( 'NONE',  ( 0.000000000000000000, 0.000000000000000000, -1.000000000000000000 ) ) ;
#29364 = CIRCLE ( 'NONE', #87568, 7.899999999999990585 ) ;
#29366 = ORIENTED_EDGE ( 'NONE', *, *, #258057, .T. ) ;
#29367 = AXIS2_PLACEMENT_3D ( 'NONE', #199122, #62187, #162583 ) ;
#29368 = CARTESIAN_POINT ( 'NONE',  ( 21.05000000000000071, -8.999999999988842703, -90.60603087734760663 ) ) ;
#29369 = DIRECTION ( 'NONE',  ( 0.000000000000000000, -0.1480365673253065117, 0.9889818879709274535 ) ) ;
#29370 = CARTESIAN_POINT ( 'NONE',  ( -18.59999999999999787, 11.65000000001115232, -122.2500000000000284 ) ) ;
#29372 = EDGE_LOOP ( 'NONE', ( #155404, #195529, #108678, #220039 ) ) ;
#29371 = CARTESIAN_POINT ( 'NONE',  ( -21.44999999999999929, 65.67360898266123570, -213.5186389139583980 ) ) ;
#29373 = CARTESIAN_POINT ( 'NONE',  ( 22.39999999999999503, 12.62988036037871176, -223.4632815780722410 ) ) ;
#29374 = AXIS2_PLACEMENT_3D ( 'NONE', #150071, #189182, #229593 ) ;
#29375 = CARTESIAN_POINT ( 'NONE',  ( 20.94999999999999574, -1.835341550213255957, -45.05515129256298223 ) ) ;
#29377 = EDGE_CURVE ( 'NONE', #135831, #160208, #90386, .T. ) ;
#29376 = FACE_OUTER_BOUND ( 'NONE', #169281, .T. ) ;
#29379 = CARTESIAN_POINT ( 'NONE',  ( -17.78241384943553172, 59.43689591760609403, -223.1219430936941990 ) ) ;
#29378 = CARTESIAN_POINT ( 'NONE',  ( 20.95512820512820440, 67.12384868372396340, -127.9644784893834100 ) ) ;
#29380 = CARTESIAN_POINT ( 'NONE',  ( 20.95595624212412744, 10.62389120310530544, -108.1296329141269297 ) ) ;
#29381 = DIRECTION ( 'NONE',  ( 0.000000000000000000, -6.853228547068871147E-15, 1.000000000000000000 ) ) ;
#29382 = DIRECTION ( 'NONE',  ( 0.000000000000000000, -0.9915357197604892647, 0.1298341882519715440 ) ) ;
#29383 = DIRECTION ( 'NONE',  ( -1.000000000000000000, -0.000000000000000000, -0.000000000000000000 ) ) ;
#29384 = ORIENTED_EDGE ( 'NONE', *, *, #118918, .F. ) ;
#29385 = ORIENTED_EDGE ( 'NONE', *, *, #26805, .T. ) ;
#29386 = EDGE_CURVE ( 'NONE', #255276, #43357, #87601, .T. ) ;
#29387 = EDGE_LOOP ( 'NONE', ( #183662, #67204, #175535, #137051 ) ) ;
#29388 = CARTESIAN_POINT ( 'NONE',  ( 20.94999999999999929, 0.000000000000000000, -33.50000000000000000 ) ) ;
#29389 = EDGE_CURVE ( 'NONE', #162352, #180226, #150182, .T. ) ;
#29390 = CARTESIAN_POINT ( 'NONE',  ( 20.95575313997065336, 65.38544669673750320, -162.4018167825796297 ) ) ;
#29391 = EDGE_LOOP ( 'NONE', ( #151145, #106236, #164933, #206851, #140465 ) ) ;
#29392 = DIRECTION ( 'NONE',  ( -1.000000000000000000, 0.000000000000000000, 0.000000000000000000 ) ) ;
#29393 = CARTESIAN_POINT ( 'NONE',  ( 20.88420186297724612, 10.33025634372637391, -206.5870929282638429 ) ) ;
#29394 = CIRCLE ( 'NONE', #41859, 11.75000000000001066 ) ;
#29395 = CARTESIAN_POINT ( 'NONE',  ( -21.05000000000000071, 14.00000000001115374, -128.5729074696175473 ) ) ;
#29396 = VERTEX_POINT ( 'NONE', #130592 ) ;
#29397 = ORIENTED_EDGE ( 'NONE', *, *, #135873, .T. ) ;
#29398 = EDGE_CURVE ( 'NONE', #235390, #158566, #108472, .T. ) ;
#29399 = CARTESIAN_POINT ( 'NONE',  ( -21.05000000000000071, 1.261786168565025568, -8.086498963545480478 ) ) ;
#29400 = FACE_OUTER_BOUND ( 'NONE', #110387, .T. ) ;
#29402 = ADVANCED_FACE ( 'NONE', ( #246687 ), #70662, .F. ) ;
#29401 = ORIENTED_EDGE ( 'NONE', *, *, #179289, .F. ) ;
#29403 = AXIS2_PLACEMENT_3D ( 'NONE', #106680, #166711, #11470 ) ;
#29404 = DIRECTION ( 'NONE',  ( 0.000000000000000000, 0.9908441862701782288, -0.1350103645450542456 ) ) ;
#29406 = EDGE_LOOP ( 'NONE', ( #26714, #104894 ) ) ;
#29405 = FACE_OUTER_BOUND ( 'NONE', #253061, .T. ) ;
#29407 = CARTESIAN_POINT ( 'NONE',  ( -22.19999999999999929, -11.75000000000000000, -15.00000000000000000 ) ) ;
#29408 = DIRECTION ( 'NONE',  ( 0.000000000000000000, 0.000000000000000000, 1.000000000000000000 ) ) ;
#29410 = ORIENTED_EDGE ( 'NONE', *, *, #147637, .F. ) ;
#29409 = DIRECTION ( 'NONE',  ( 0.000000000000000000, -1.000000000000000000, 0.000000000000000000 ) ) ;
#29411 = CARTESIAN_POINT ( 'NONE',  ( -20.85000000000000142, -1.135018845899022466, -175.2169768834323520 ) ) ;
#29412 = CARTESIAN_POINT ( 'NONE',  ( 20.85000000106584750, 64.25000000001219291, -143.3676028280509627 ) ) ;
#29413 = DIRECTION ( 'NONE',  ( 0.000000000000000000, 0.2617529984165022361, 0.9651348961777159730 ) ) ;
#29414 = LINE ( 'NONE', #9807, #173452 ) ;
#29415 = CARTESIAN_POINT ( 'NONE',  ( 21.06277459767431282, 8.872862438279383923, -179.7039991923569460 ) ) ;
#29416 = FACE_OUTER_BOUND ( 'NONE', #32294, .T. ) ;
#29417 = AXIS2_PLACEMENT_3D ( 'NONE', #7371, #222552, #160062 ) ;
#29418 = CARTESIAN_POINT ( 'NONE',  ( 18.59999999999996945, 7.021664781900089913, -37.33356540189728889 ) ) ;
#29419 = CARTESIAN_POINT ( 'NONE',  ( -22.94999999999999929, 7.900000000000000355, -1.300000000000000044 ) ) ;
#29420 = CARTESIAN_POINT ( 'NONE',  ( -16.87036670365548474, 9.989418819312801290, -188.4795601173020145 ) ) ;
#29422 = EDGE_CURVE ( 'NONE', #196986, #76430, #51027, .T. ) ;
#29421 = AXIS2_PLACEMENT_3D ( 'NONE', #141765, #144315, #23143 ) ;
#29423 = EDGE_LOOP ( 'NONE', ( #127578, #97029, #158222, #82014 ) ) ;
#29424 = EDGE_LOOP ( 'NONE', ( #125533, #59805, #38896, #44223 ) ) ;
#29425 = CARTESIAN_POINT ( 'NONE',  ( 18.39999999999999858, -9.682403433476396870, -40.15684337741279109 ) ) ;
#29426 = ORIENTED_EDGE ( 'NONE', *, *, #187529, .T. ) ;
#29428 = DIRECTION ( 'NONE',  ( 0.000000000000000000, -0.8814952561687088295, 0.4721928772779852013 ) ) ;
#29427 =( GEOMETRIC_REPRESENTATION_CONTEXT ( 3 ) GLOBAL_UNCERTAINTY_ASSIGNED_CONTEXT ( ( #47787 ) ) GLOBAL_UNIT_ASSIGNED_CONTEXT ( ( #23706, #79762, #159350 ) ) REPRESENTATION_CONTEXT ( 'NONE', 'WORKASPACE' ) );
#29429 = VERTEX_POINT ( 'NONE', #129319 ) ;
#29430 = EDGE_CURVE ( 'NONE', #185664, #81259, #208859, .T. ) ;
#29431 = CARTESIAN_POINT ( 'NONE',  ( -23.15000000000000213, 56.02567683926420727, -227.9999002286038774 ) ) ;
#29432 = LINE ( 'NONE', #232745, #235868 ) ;
#29433 = AXIS2_PLACEMENT_3D ( 'NONE', #139745, #116372, #78497 ) ;
#29434 = AXIS2_PLACEMENT_3D ( 'NONE', #141763, #98757, #122221 ) ;
#29435 = EDGE_CURVE ( 'NONE', #188768, #31301, #82171, .T. ) ;
#29436 = EDGE_LOOP ( 'NONE', ( #68717, #102527, #246254, #141794 ) ) ;
#29437 = CARTESIAN_POINT ( 'NONE',  ( -18.50000000000000000, 7.128833340094563376, -233.7327013124401276 ) ) ;
#29438 = EDGE_CURVE ( 'NONE', #70783, #175048, #115508, .T. ) ;
#29440 = ORIENTED_EDGE ( 'NONE', *, *, #94096, .F. ) ;
#29439 = AXIS2_PLACEMENT_3D ( 'NONE', #72778, #248825, #152308 ) ;
#29441 = ORIENTED_EDGE ( 'NONE', *, *, #14185, .T. ) ;
#29442 = TOROIDAL_SURFACE ( 'NONE', #204169, 7.791421356237316687, 0.1000000000000000056 ) ;
#29443 = AXIS2_PLACEMENT_3D ( 'NONE', #87144, #28518, #71472 ) ;
#29444 = ORIENTED_EDGE ( 'NONE', *, *, #28456, .F. ) ;
#29445 = CIRCLE ( 'NONE', #191939, 0.1000000000000028644 ) ;
#29446 = VECTOR ( 'NONE', #217650, 1000.000000000000000 ) ;
#29447 = CARTESIAN_POINT ( 'NONE',  ( -18.59999999999999787, 77.26327546522965406, -162.1212428177779543 ) ) ;
#29448 = DIRECTION ( 'NONE',  ( 1.000000000000000000, -0.000000000000000000, -0.000000000000000000 ) ) ;
#29449 = DIRECTION ( 'NONE',  ( 0.000000000000000000, -0.9126074666063622720, -0.4088369013363611360 ) ) ;
#29450 = DIRECTION ( 'NONE',  ( 0.000000000000000000, 0.000000000000000000, -1.000000000000000000 ) ) ;
#29452 = CYLINDRICAL_SURFACE ( 'NONE', #20264, 0.09999999999999939493 ) ;
#29451 = CYLINDRICAL_SURFACE ( 'NONE', #137347, 11.79999999999999716 ) ;
#29453 = CARTESIAN_POINT ( 'NONE',  ( 20.94999999999999574, -1.261786168553869603, -142.0864989635454947 ) ) ;
#29455 = ORIENTED_EDGE ( 'NONE', *, *, #161265, .F. ) ;
#29454 = LINE ( 'NONE', #89367, #235548 ) ;
#29456 = CARTESIAN_POINT ( 'NONE',  ( -23.25000000000000000, 76.00000000001267608, -203.5231074845243597 ) ) ;
#29457 = EDGE_CURVE ( 'NONE', #14729, #1615, #151474, .T. ) ;
#29458 = DIRECTION ( 'NONE',  ( 0.000000000000000000, 0.000000000000000000, -1.000000000000000000 ) ) ;
#29459 = EDGE_CURVE ( 'NONE', #69945, #75171, #256918, .T. ) ;
#29460 = ORIENTED_EDGE ( 'NONE', *, *, #109787, .F. ) ;
#29461 = CARTESIAN_POINT ( 'NONE',  ( 20.95556889135987788, 10.62194358774625336, -74.64239422185755757 ) ) ;
#29462 = CARTESIAN_POINT ( 'NONE',  ( 13.99999999999999822, 9.849999999999981881, -16.74999999999999645 ) ) ;
#29463 = CARTESIAN_POINT ( 'NONE',  ( -11.59999999999994458, 64.35000000001120668, -23.62310748452479103 ) ) ;
#29464 = EDGE_LOOP ( 'NONE', ( #210812, #218388, #42491, #59254 ) ) ;
#29465 = AXIS2_PLACEMENT_3D ( 'NONE', #93126, #111421, #230081 ) ;
#29466 = FACE_OUTER_BOUND ( 'NONE', #68722, .T. ) ;
#29467 = DIRECTION ( 'NONE',  ( 0.000000000000000000, 1.000000000000000000, 0.000000000000000000 ) ) ;
#29468 = DIRECTION ( 'NONE',  ( 1.000000000000000000, 0.000000000000000000, 0.000000000000000000 ) ) ;
#29469 = ORIENTED_EDGE ( 'NONE', *, *, #44, .T. ) ;
#29470 = EDGE_LOOP ( 'NONE', ( #160152, #221436, #160524, #98651 ) ) ;
#29471 = CARTESIAN_POINT ( 'NONE',  ( 21.14999999999999858, 11.65000000000000746, -12.15000000000000036 ) ) ;
#29472 = CARTESIAN_POINT ( 'NONE',  ( -18.50211644919735576, 10.30207779525982836, -172.9895520716782755 ) ) ;
#29473 = FACE_OUTER_BOUND ( 'NONE', #189984, .T. ) ;
#29474 = DIRECTION ( 'NONE',  ( -1.000000000000000000, 2.952720810173289112E-16, 2.061873921506763405E-30 ) ) ;
#29475 = ORIENTED_EDGE ( 'NONE', *, *, #164104, .F. ) ;
#29476 = AXIS2_PLACEMENT_3D ( 'NONE', #137040, #221687, #196994 ) ;
#29477 = CARTESIAN_POINT ( 'NONE',  ( 21.14999999999999858, 0.000000000000000000, 6.540656951701244282 ) ) ;
#29478 = CARTESIAN_POINT ( 'NONE',  ( -22.59066674512275696, 64.25000000001236344, -170.0536116081549380 ) ) ;
#29479 = CIRCLE ( 'NONE', #95877, 0.1000000000000013933 ) ;
#29480 = DIRECTION ( 'NONE',  ( 0.000000000000000000, 0.000000000000000000, -1.000000000000000000 ) ) ;
#29481 = CYLINDRICAL_SURFACE ( 'NONE', #215822, 0.1000000000000002554 ) ;
#29482 = B_SPLINE_CURVE_WITH_KNOTS ( 'NONE', 3,
 ( #173162, #171866, #253914, #36185, #75322, #31070, #154855 ),
 .UNSPECIFIED., .F., .F.,
 ( 4, 3, 4 ),
 ( 0.000000000000000000, 1.860045280646148997E-05, 5.251155757303900822E-05 ),
 .UNSPECIFIED. ) ;
#29483 = AXIS2_PLACEMENT_3D ( 'NONE', #119114, #239056, #175267 ) ;
#29484 = EDGE_CURVE ( 'NONE', #149704, #131288, #157165, .T. ) ;
#29485 = ORIENTED_EDGE ( 'NONE', *, *, #35409, .F. ) ;
#29486 = CARTESIAN_POINT ( 'NONE',  ( 23.24999999999999645, 19.44861527341281615, -230.3234391047226666 ) ) ;
#29487 = AXIS2_PLACEMENT_3D ( 'NONE', #208975, #256722, #18162 ) ;
#29489 = VERTEX_POINT ( 'NONE', #92745 ) ;
#29488 = DIRECTION ( 'NONE',  ( 0.000000000000000000, -0.9126074666063660468, -0.4088369013363524762 ) ) ;
#29490 = CARTESIAN_POINT ( 'NONE',  ( -22.39999999999999858, 68.20922040163897293, -170.1231074845244109 ) ) ;
#29491 = DIRECTION ( 'NONE',  ( 0.000000000000000000, -0.1495327102803180597, 0.9887567792719412774 ) ) ;
#29492 = CARTESIAN_POINT ( 'NONE',  ( -23.15000000000000213, 64.35000000001198828, -115.1731074845243796 ) ) ;
#29493 = CARTESIAN_POINT ( 'NONE',  ( 18.59999999999999432, 77.83585931145498193, -24.51866831572578320 ) ) ;
#29494 = FACE_OUTER_BOUND ( 'NONE', #166338, .T. ) ;
#29495 = DIRECTION ( 'NONE',  ( 0.000000000000000000, 0.9126074666063844765, 0.4088369013363114535 ) ) ;
#29496 = FACE_OUTER_BOUND ( 'NONE', #82063, .T. ) ;
#29497 = VERTEX_POINT ( 'NONE', #134429 ) ;
#29498 = CARTESIAN_POINT ( 'NONE',  ( -20.85000000000000142, 70.20041822846812352, -198.0817714174541493 ) ) ;
#29499 = CARTESIAN_POINT ( 'NONE',  ( -20.54999999999999716, 71.65000000001199965, -115.2731074845243171 ) ) ;
#29500 = CARTESIAN_POINT ( 'NONE',  ( 21.14999999999999503, 64.35000000001164722, -69.52310748452438816 ) ) ;
#29501 = CARTESIAN_POINT ( 'NONE',  ( -20.94999999999999929, -1.835859311432479268, -145.5044391687985694 ) ) ;
#29502 = EDGE_CURVE ( 'NONE', #150745, #20544, #147488, .T. ) ;
#29504 = CIRCLE ( 'NONE', #8626, 0.09999999999998898659 ) ;
#29503 = CYLINDRICAL_SURFACE ( 'NONE', #46782, 0.1000000000000055844 ) ;
#29506 = CARTESIAN_POINT ( 'NONE',  ( 12.93279065517211635, 9.417690691074255938, -185.6416006967645842 ) ) ;
#29505 = TOROIDAL_SURFACE ( 'NONE', #191993, 0.2000000000000000111, 0.1000000000000000056 ) ;
#29507 = ORIENTED_EDGE ( 'NONE', *, *, #51974, .T. ) ;
#29508 = ORIENTED_EDGE ( 'NONE', *, *, #55006, .F. ) ;
#29509 = CIRCLE ( 'NONE', #145989, 0.1000000000000028644 ) ;
#29510 = DIRECTION ( 'NONE',  ( -0.000000000000000000, 6.982962677686266711E-15, -1.000000000000000000 ) ) ;
#29511 = DIRECTION ( 'NONE',  ( -1.000000000000000000, -2.952720810173289112E-16, 0.000000000000000000 ) ) ;
#29512 = FACE_OUTER_BOUND ( 'NONE', #102977, .T. ) ;
#29513 = FACE_OUTER_BOUND ( 'NONE', #198370, .T. ) ;
#29514 = CARTESIAN_POINT ( 'NONE',  ( -20.64999999999999858, 62.24653955602229871, -247.9500786234238490 ) ) ;
#29515 = CARTESIAN_POINT ( 'NONE',  ( 21.14999999999999858, 64.35000000001228670, -157.8731074845244393 ) ) ;
#29516 = AXIS2_PLACEMENT_3D ( 'NONE', #184807, #20627, #24483 ) ;
#29517 = CYLINDRICAL_SURFACE ( 'NONE', #170473, 0.09999999999998898659 ) ;
#29518 = FACE_OUTER_BOUND ( 'NONE', #215336, .T. ) ;
#29519 = EDGE_LOOP ( 'NONE', ( #250829, #163724, #119639, #77360 ) ) ;
#29520 = CARTESIAN_POINT ( 'NONE',  ( -16.87036670365549895, 10.08494996326643189, -146.5500000000000114 ) ) ;
#29521 = EDGE_LOOP ( 'NONE', ( #165931, #72918, #122384, #209941 ) ) ;
#29522 = CARTESIAN_POINT ( 'NONE',  ( -21.55000000000000071, 63.37018259659601682, -222.0118260003222872 ) ) ;
#29523 = CARTESIAN_POINT ( 'NONE',  ( 21.05000000000000071, 10.60832956795391802, -7.591685013295530027 ) ) ;
#29524 = LINE ( 'NONE', #68624, #103430 ) ;
#29525 = CARTESIAN_POINT ( 'NONE',  ( -23.39999999999994529, 76.00000000001119815, -40.07310748452479032 ) ) ;
#29526 = FACE_OUTER_BOUND ( 'NONE', #75161, .T. ) ;
#29527 = CARTESIAN_POINT ( 'NONE',  ( -18.58693740092133240, -9.406432150253023039, -7.124816456501293693 ) ) ;
#29528 = CARTESIAN_POINT ( 'NONE',  ( 23.14999999999999858, 35.71453866719386383, -251.3141532135810792 ) ) ;
#29529 = ORIENTED_EDGE ( 'NONE', *, *, #134283, .F. ) ;
#29530 = CARTESIAN_POINT ( 'NONE',  ( -18.79999999999999716, 0.000000000000000000, 0.000000000000000000 ) ) ;
#29531 = VECTOR ( 'NONE', #245709, 1000.000000000000000 ) ;
#29532 = LINE ( 'NONE', #127316, #138089 ) ;
#29533 = CIRCLE ( 'NONE', #208589, 0.1000000000000001305 ) ;
#29535 = ADVANCED_FACE ( 'NONE', ( #113607 ), #226577, .T. ) ;
#29534 = CARTESIAN_POINT ( 'NONE',  ( 23.24999999999999289, 6.450000000011156587, -146.3500000000000227 ) ) ;
#29536 = CARTESIAN_POINT ( 'NONE',  ( -21.05000000000000071, -1.162701749938009677, -8.099999999999999645 ) ) ;
#29537 = AXIS2_PLACEMENT_3D ( 'NONE', #233742, #173815, #115067 ) ;
#29538 = CARTESIAN_POINT ( 'NONE',  ( -22.59066674512259709, 11.75000000001115552, -167.4694958763693364 ) ) ;
#29539 = AXIS2_PLACEMENT_3D ( 'NONE', #14752, #108685, #207816 ) ;
#29540 = ORIENTED_EDGE ( 'NONE', *, *, #96198, .F. ) ;
#29541 = DIRECTION ( 'NONE',  ( 0.000000000000000000, -0.4721928772777346794, -0.8814952561688431665 ) ) ;
#29543 = EDGE_CURVE ( 'NONE', #256947, #50959, #89215, .T. ) ;
#29542 = CARTESIAN_POINT ( 'NONE',  ( 20.04142135623730070, 64.35000000001251408, -178.8731074845244393 ) ) ;
#29544 = EDGE_LOOP ( 'NONE', ( #45075, #157520, #195825, #99268 ) ) ;
#29545 = ORIENTED_EDGE ( 'NONE', *, *, #223409, .T. ) ;
#29547 = EDGE_CURVE ( 'NONE', #30528, #138157, #159991, .T. ) ;
#29546 = FACE_OUTER_BOUND ( 'NONE', #231658, .T. ) ;
#29548 = DIRECTION ( 'NONE',  ( -1.000000000000000000, -0.000000000000000000, -0.000000000000000000 ) ) ;
#29549 = AXIS2_PLACEMENT_3D ( 'NONE', #142030, #44234, #221545 ) ;
#29550 = DIRECTION ( 'NONE',  ( -1.000000000000000000, 0.000000000000000000, 0.000000000000000000 ) ) ;
#29551 = EDGE_LOOP ( 'NONE', ( #231261, #16396, #245054, #41011 ) ) ;
#29552 = CARTESIAN_POINT ( 'NONE',  ( 20.84999999999999432, 68.97833521811179480, -99.18954208262705663 ) ) ;
#29553 = LINE ( 'NONE', #167775, #76687 ) ;
#29554 = ADVANCED_FACE ( 'NONE', ( #73233 ), #56182, .T. ) ;
#29555 = ORIENTED_EDGE ( 'NONE', *, *, #222072, .T. ) ;
#29556 = DIRECTION ( 'NONE',  ( 1.000000000000000000, 0.000000000000000000, -0.000000000000000000 ) ) ;
#29557 =( BOUNDED_SURFACE ( )  B_SPLINE_SURFACE ( 3, 2, ( 
 ( #204422, #44082, #25798 ),
 ( #6221, #4917, #128762 ),
 ( #83167, #225257, #123625 ),
 ( #126167, #8810, #247401 ),
 ( #147013, #162763, #7518 ),
 ( #87029, #207007, #28409 ) ),
 .UNSPECIFIED., .F., .F., .F. ) 
 B_SPLINE_SURFACE_WITH_KNOTS ( ( 4, 2, 4 ),
 ( 3, 3 ),
 ( 1.570796326794897668, 2.356194490192346169, 3.141592653589794448 ),
 ( 0.000000000000000000, 1.000000000000000000 ),
 .UNSPECIFIED. ) 
 GEOMETRIC_REPRESENTATION_ITEM ( )  RATIONAL_B_SPLINE_SURFACE ( (
 ( 1.000000000000000000, 0.7071067811865597852, 1.000000000000000000),
 ( 1.000000000000000000, 0.6611148371778731159, 1.000000000000000000),
 ( 1.000000000000000000, 0.6092287576696180373, 1.000000000000000000),
 ( 1.000000000000000000, 0.5278258667058124409, 1.000000000000000000),
 ( 1.000000000000000000, 0.4993418825333900690, 1.000000000000000000),
 ( 1.000000000000000000, 0.5000000000000154321, 1.000000000000000000) ) ) 
 REPRESENTATION_ITEM ( '' )  SURFACE ( )  );
#29558 = ORIENTED_EDGE ( 'NONE', *, *, #181276, .F. ) ;
#29559 = DIRECTION ( 'NONE',  ( 0.000000000000000000, 0.000000000000000000, 1.000000000000000000 ) ) ;
#29561 = EDGE_CURVE ( 'NONE', #215032, #132946, #164066, .T. ) ;
#29560 = CARTESIAN_POINT ( 'NONE',  ( -21.55000000000000071, 29.23678660621682113, -237.4641088729839282 ) ) ;
#29562 = TOROIDAL_SURFACE ( 'NONE', #8682, 0.2000000000000000111, 0.1000000000000000056 ) ;
#29564 = ORIENTED_EDGE ( 'NONE', *, *, #141912, .F. ) ;
#29563 = DIRECTION ( 'NONE',  ( -0.000000000000000000, -0.2617529984165028467, -0.9651348961777159730 ) ) ;
#29566 = CARTESIAN_POINT ( 'NONE',  ( 23.24999999999999645, 70.35000000001153353, -48.67310748452437252 ) ) ;
#29565 = UNCERTAINTY_MEASURE_WITH_UNIT (LENGTH_MEASURE( 1.000000000000000082E-05 ), #3045, 'distance_accuracy_value', 'NONE');
#29567 = DIRECTION ( 'NONE',  ( -1.000000000000000000, 0.000000000000000000, 0.000000000000000000 ) ) ;
#29568 = CARTESIAN_POINT ( 'NONE',  ( -16.88783316861828609, 66.05000000001230376, -157.2708434425446455 ) ) ;
#29569 = DIRECTION ( 'NONE',  ( 0.000000000000000000, 0.4031292884907143326, 0.9151430362303863975 ) ) ;
#29570 = CIRCLE ( 'NONE', #100250, 4.099999999999999645 ) ;
#29571 = DIRECTION ( 'NONE',  ( -0.000000000000000000, 1.000000000000000000, 6.982962677686266711E-15 ) ) ;
#29572 = FACE_BOUND ( 'NONE', #236359, .T. ) ;
#29574 = ORIENTED_EDGE ( 'NONE', *, *, #132722, .F. ) ;
#29573 = CARTESIAN_POINT ( 'NONE',  ( 20.94999999999999574, 87.39257802171759693, -99.94915790469229933 ) ) ;
#29575 = VERTEX_POINT ( 'NONE', #213999 ) ;
#29577 = DIRECTION ( 'NONE',  ( 0.000000000000000000, 6.982962677686266711E-15, -1.000000000000000000 ) ) ;
#29576 = DIRECTION ( 'NONE',  ( 1.000000000000000000, 0.000000000000000000, 0.000000000000000000 ) ) ;
#29579 = ORIENTED_EDGE ( 'NONE', *, *, #81450, .T. ) ;
#29578 = CARTESIAN_POINT ( 'NONE',  ( -23.49999999999994316, 87.60324567546805952, -37.87437456276921210 ) ) ;
#29580 = ADVANCED_BREP_SHAPE_REPRESENTATION ( '', ( #107142, #2425 ), #110949 ) ;
#29581 = ORIENTED_EDGE ( 'NONE', *, *, #7895, .T. ) ;
#29582 = CARTESIAN_POINT ( 'NONE',  ( -20.54999999999999716, 47.91013932883114990, -242.3192343197862044 ) ) ;
#29583 = CARTESIAN_POINT ( 'NONE',  ( 21.05000000000000071, 64.40000000001248281, -176.9513107147999449 ) ) ;
#29584 = DIRECTION ( 'NONE',  ( 0.000000000000000000, -0.2128009952263403282, 0.9770955615653358350 ) ) ;
#29585 = AXIS2_PLACEMENT_3D ( 'NONE', #238854, #139730, #120231 ) ;
#29586 = LINE ( 'NONE', #68686, #131633 ) ;
#29587 = CARTESIAN_POINT ( 'NONE',  ( -18.59999999999999787, 67.49222854868494892, -195.4187676019683693 ) ) ;
#29588 = DIRECTION ( 'NONE',  ( -1.000000000000000000, -3.265361837132813093E-16, 0.000000000000000000 ) ) ;
#29589 = DIRECTION ( 'NONE',  ( 1.000000000000000000, -0.000000000000000000, -0.000000000000000000 ) ) ;
#29590 = ORIENTED_EDGE ( 'NONE', *, *, #78932, .F. ) ;
#29591 = EDGE_LOOP ( 'NONE', ( #36885, #84732, #187892, #249763 ) ) ;
#29592 = FACE_OUTER_BOUND ( 'NONE', #248749, .T. ) ;
#29593 = CIRCLE ( 'NONE', #241937, 0.1000000000000000888 ) ;
#29594 = ORIENTED_EDGE ( 'NONE', *, *, #168617, .T. ) ;
#29596 = ORIENTED_EDGE ( 'NONE', *, *, #122142, .T. ) ;
#29595 = AXIS2_PLACEMENT_3D ( 'NONE', #78291, #58716, #22206 ) ;
#29597 = CARTESIAN_POINT ( 'NONE',  ( -23.25000000000000000, 76.00000000001195133, -103.0231074845243171 ) ) ;
#29598 = EDGE_CURVE ( 'NONE', #106745, #104724, #17099, .T. ) ;
#29599 = AXIS2_PLACEMENT_3D ( 'NONE', #62893, #104555, #6772 ) ;
#29600 = AXIS2_PLACEMENT_3D ( 'NONE', #65360, #144884, #70535 ) ;
#29601 = DIRECTION ( 'NONE',  ( -0.000000000000000000, 0.1350103645451807555, 0.9908441862701610203 ) ) ;
#29602 = CARTESIAN_POINT ( 'NONE',  ( 18.49999999999999289, 65.50857864377418593, -44.67310748452439384 ) ) ;
#29603 = CARTESIAN_POINT ( 'NONE',  ( -20.94999999999999929, 68.97833521811131163, -32.18954208262707795 ) ) ;
#29604 = ORIENTED_EDGE ( 'NONE', *, *, #64078, .T. ) ;
#29607 = EDGE_CURVE ( 'NONE', #148927, #67744, #22611, .T. ) ;
#29606 = AXIS2_PLACEMENT_3D ( 'NONE', #241851, #163613, #166212 ) ;
#29605 = DIRECTION ( 'NONE',  ( -1.000000000000000000, 7.304098846218135653E-16, 0.000000000000000000 ) ) ;
#29608 = ORIENTED_EDGE ( 'NONE', *, *, #42629, .F. ) ;
#29609 = LINE ( 'NONE', #167834, #250696 ) ;
#29610 = CARTESIAN_POINT ( 'NONE',  ( 21.05000000000000071, 1.115600667400684642E-11, -134.0000000000000284 ) ) ;
#29611 = EDGE_CURVE ( 'NONE', #124696, #20141, #254374, .T. ) ;
#29612 = ORIENTED_EDGE ( 'NONE', *, *, #121762, .F. ) ;
#29613 = CARTESIAN_POINT ( 'NONE',  ( -21.64999999999999858, 65.67360898266123570, -213.5186389139583980 ) ) ;
#29614 = ORIENTED_EDGE ( 'NONE', *, *, #240079, .F. ) ;
#29617 = ORIENTED_EDGE ( 'NONE', *, *, #74160, .F. ) ;
#29616 = CARTESIAN_POINT ( 'NONE',  ( 18.55807992284871233, 46.45729338110134421, -243.0823073233429170 ) ) ;
#29615 = CARTESIAN_POINT ( 'NONE',  ( -21.05000000000000071, 11.65000000001115588, -167.5999999999999659 ) ) ;
#29618 = CIRCLE ( 'NONE', #204552, 0.09999999999999939493 ) ;
#29619 = VECTOR ( 'NONE', #52310, 1000.000000000000000 ) ;
#29621 = VERTEX_POINT ( 'NONE', #96583 ) ;
#29620 = VECTOR ( 'NONE', #234046, 1000.000000000000114 ) ;
#29622 = AXIS2_PLACEMENT_3D ( 'NONE', #150655, #230185, #191090 ) ;
#29623 = AXIS2_PLACEMENT_3D ( 'NONE', #104932, #86662, #222319 ) ;
#29624 = DIRECTION ( 'NONE',  ( -0.000000000000000000, -0.000000000000000000, -1.000000000000000000 ) ) ;
#29625 = VERTEX_POINT ( 'NONE', #237411 ) ;
#29627 = ADVANCED_FACE ( 'NONE', ( #173640 ), #116196, .T. ) ;
#29626 = CARTESIAN_POINT ( 'NONE',  ( -21.05000000000000071, 76.00000000001237765, -170.0231074845243597 ) ) ;
#29628 = CARTESIAN_POINT ( 'NONE',  ( 21.14999999999999503, 87.75000000001276135, -215.2731074845242745 ) ) ;
#29629 =( BOUNDED_SURFACE ( )  B_SPLINE_SURFACE ( 3, 2, ( 
 ( #98867, #256635, #71977 ),
 ( #31590, #111092, #58467 ),
 ( #12015, #78046, #158905 ),
 ( #91535, #171117, #250593 ),
 ( #239707, #100156, #240988 ),
 ( #179739, #1057, #63625 ) ),
 .UNSPECIFIED., .F., .F., .F. ) 
 B_SPLINE_SURFACE_WITH_KNOTS ( ( 4, 2, 4 ),
 ( 3, 3 ),
 ( 6.719893378899590472E-05, 0.0002757154632485403294, 0.0004842319927080847406 ),
 ( 0.000000000000000000, 1.000000000000000000 ),
 .UNSPECIFIED. ) 
 GEOMETRIC_REPRESENTATION_ITEM ( )  RATIONAL_B_SPLINE_SURFACE ( (
 ( 1.000000000000000000, 0.7250110520819756932, 1.000000000000000000),
 ( 1.000000000000000000, 0.7277932058368190571, 1.000000000000000000),
 ( 1.000000000000000000, 0.7278452872605407631, 1.000000000000000000),
 ( 1.000000000000000000, 0.7221445671561397273, 1.000000000000000000),
 ( 1.000000000000000000, 0.7163662143770669344, 1.000000000000000000),
 ( 1.000000000000000000, 0.7071067811865475727, 1.000000000000000000) ) ) 
 REPRESENTATION_ITEM ( '' )  SURFACE ( )  );
#29630 = DIRECTION ( 'NONE',  ( -1.000000000000000000, -0.000000000000000000, -0.000000000000000000 ) ) ;
#29631 = ADVANCED_FACE ( 'NONE', ( #135725 ), #101664, .F. ) ;
#29632 = DIRECTION ( 'NONE',  ( 1.000000000000000000, 0.000000000000000000, 0.000000000000000000 ) ) ;
#29633 = AXIS2_PLACEMENT_3D ( 'NONE', #44089, #6228, #124919 ) ;
#29634 = ORIENTED_EDGE ( 'NONE', *, *, #181241, .T. ) ;
#29635 = DIRECTION ( 'NONE',  ( -0.000000000000000000, 1.000000000000000000, 0.000000000000000000 ) ) ;
#29636 = CARTESIAN_POINT ( 'NONE',  ( -23.15000000000000213, 11.75000000001115552, -155.3500000000000227 ) ) ;
#29637 = ORIENTED_EDGE ( 'NONE', *, *, #246368, .T. ) ;
#29638 = FACE_OUTER_BOUND ( 'NONE', #61369, .T. ) ;
#29639 = VERTEX_POINT ( 'NONE', #176173 ) ;
#29640 = DIRECTION ( 'NONE',  ( 0.000000000000000000, 7.116814260417676401E-15, -1.000000000000000000 ) ) ;
#29641 = ORIENTED_EDGE ( 'NONE', *, *, #172080, .F. ) ;
#29642 = EDGE_CURVE ( 'NONE', #99108, #111684, #234983, .T. ) ;
#29643 = DIRECTION ( 'NONE',  ( -0.000000000000000000, -2.891205793294679805E-16, 1.000000000000000000 ) ) ;
#29644 = CARTESIAN_POINT ( 'NONE',  ( 23.15000000000000213, -9.000000000000000000, -24.10603087734755690 ) ) ;
#29646 = VERTEX_POINT ( 'NONE', #161748 ) ;
#29645 = CARTESIAN_POINT ( 'NONE',  ( 18.59999999999999432, 77.16270174994961906, -61.42310748452431568 ) ) ;
#29647 = EDGE_CURVE ( 'NONE', #17339, #132836, #143435, .T. ) ;
#29648 = SPHERICAL_SURFACE ( 'NONE', #200307, 0.1000000000000000056 ) ;
#29649 = EDGE_CURVE ( 'NONE', #8352, #151091, #44355, .T. ) ;
#29650 = TOROIDAL_SURFACE ( 'NONE', #158825, 0.2000000000000000111, 0.1000000000000000056 ) ;
#29651 = CARTESIAN_POINT ( 'NONE',  ( -15.06720934482788010, 62.89055100415842503, -215.8809258249639242 ) ) ;
#29652 = CARTESIAN_POINT ( 'NONE',  ( -20.94999999999999929, 11.60000000001115161, -40.42820323027555673 ) ) ;
#29653 = ORIENTED_EDGE ( 'NONE', *, *, #98256, .F. ) ;
#29654 = CARTESIAN_POINT ( 'NONE',  ( 23.25000000000000000, 28.42524210734032408, -258.3567845160494585 ) ) ;
#29655 = CARTESIAN_POINT ( 'NONE',  ( 18.58685178364169488, 85.40673308381654749, -162.8986870154365363 ) ) ;
#29656 = VERTEX_POINT ( 'NONE', #19656 ) ;
#29657 = CARTESIAN_POINT ( 'NONE',  ( 20.00000000000000355, 5.454087299794355914, 16.60000000000000142 ) ) ;
#29658 = ORIENTED_EDGE ( 'NONE', *, *, #231644, .F. ) ;
#29659 =( BOUNDED_CURVE ( )  B_SPLINE_CURVE ( 3, ( #36048, #98522, #176849, #55555 ),
 .UNSPECIFIED., .F., .F. ) 
 B_SPLINE_CURVE_WITH_KNOTS ( ( 4, 4 ),
 ( 0.3000847527772393386, 0.5517402753107881752 ),
 .UNSPECIFIED. ) 
 CURVE ( )  GEOMETRIC_REPRESENTATION_ITEM ( )  RATIONAL_B_SPLINE_CURVE ( ( 1.000000000000000000, 0.9947294176030464508, 0.9947294176030464508, 1.000000000000000000 ) ) 
 REPRESENTATION_ITEM ( '' )  );
#29661 = CARTESIAN_POINT ( 'NONE',  ( -22.59999999999999787, 12.58798907299599179, -223.3278890275437050 ) ) ;
#29660 = TOROIDAL_SURFACE ( 'NONE', #121265, 12.77499999999999858, 0.1000000000000000056 ) ;
#29662 = CARTESIAN_POINT ( 'NONE',  ( 22.50000000000000000, 0.1000000000111554016, -159.7092204016265669 ) ) ;
#29663 = ADVANCED_FACE ( 'NONE', ( #99154 ), #100432, .T. ) ;
#29664 = EDGE_CURVE ( 'NONE', #235865, #207855, #224249, .T. ) ;
#29667 = ORIENTED_EDGE ( 'NONE', *, *, #229853, .F. ) ;
#29666 = ORIENTED_EDGE ( 'NONE', *, *, #18626, .F. ) ;
#29665 = FACE_OUTER_BOUND ( 'NONE', #149932, .T. ) ;
#29668 = CARTESIAN_POINT ( 'NONE',  ( 20.84999999999999432, 14.80545736607782814, -235.9842437978701639 ) ) ;
#29669 = DIRECTION ( 'NONE',  ( -1.000000000000000000, -0.000000000000000000, 0.000000000000000000 ) ) ;
#29671 = EDGE_CURVE ( 'NONE', #241513, #160000, #180820, .T. ) ;
#29670 = CARTESIAN_POINT ( 'NONE',  ( 22.10000000000000497, -11.75000000000000000, 32.89999999999999858 ) ) ;
#29673 = CARTESIAN_POINT ( 'NONE',  ( -13.77083647240106501, 66.54258906972138732, -51.02319157577811382 ) ) ;
#29672 = DIRECTION ( 'NONE',  ( 0.000000000000000000, 0.8814952561688476074, -0.4721928772777262417 ) ) ;
#29674 = CARTESIAN_POINT ( 'NONE',  ( 21.14999999999999503, 87.65000000001266756, -200.6231074845242688 ) ) ;
#29675 = DIRECTION ( 'NONE',  ( 1.000000000000000000, 0.000000000000000000, 0.000000000000000000 ) ) ;
#29676 = VECTOR ( 'NONE', #6301, 1000.000000000000000 ) ;
#29677 = DIRECTION ( 'NONE',  ( 1.000000000000000000, 1.836970198721029934E-16, 0.000000000000000000 ) ) ;
#29678 = AXIS2_PLACEMENT_3D ( 'NONE', #209273, #34518, #154481 ) ;
#29679 = FACE_OUTER_BOUND ( 'NONE', #80967, .T. ) ;
#29680 = EDGE_LOOP ( 'NONE', ( #203067, #17204, #83641, #127531, #254085, #3078, #167925, #246431, #183943, #52755 ) ) ;
#29681 = ORIENTED_EDGE ( 'NONE', *, *, #229858, .F. ) ;
#29682 = CARTESIAN_POINT ( 'NONE',  ( -18.39999999999999858, 38.03205796367813463, -261.1772988674111957 ) ) ;
#29684 = ORIENTED_EDGE ( 'NONE', *, *, #5136, .T. ) ;
#29683 = CARTESIAN_POINT ( 'NONE',  ( -21.05000000000000071, 1.835341550224411922, -11.55515129256298046 ) ) ;
#29685 = EDGE_LOOP ( 'NONE', ( #111827, #24273, #2019, #217885, #223715 ) ) ;
#29686 = CARTESIAN_POINT ( 'NONE',  ( -18.59999999999999787, 64.35000000001191722, -103.0231074845243882 ) ) ;
#29687 = EDGE_LOOP ( 'NONE', ( #222293, #3414, #164074, #3807 ) ) ;
#29688 = CARTESIAN_POINT ( 'NONE',  ( 21.06280952165534259, 43.45167128181677185, -234.8632948402907914 ) ) ;
#29689 = EDGE_CURVE ( 'NONE', #243619, #172429, #45633, .T. ) ;
#29690 = ORIENTED_EDGE ( 'NONE', *, *, #207197, .T. ) ;
#29691 = CIRCLE ( 'NONE', #108775, 1.749999999999999778 ) ;
#29692 = FACE_OUTER_BOUND ( 'NONE', #95361, .T. ) ;
#29694 = ADVANCED_FACE ( 'NONE', ( #203423 ), #193291, .T. ) ;
#29693 = CARTESIAN_POINT ( 'NONE',  ( 20.94999999999999574, -1.835341550213255957, -45.05515129256298223 ) ) ;
#29696 = ORIENTED_EDGE ( 'NONE', *, *, #257165, .T. ) ;
#29695 = ORIENTED_EDGE ( 'NONE', *, *, #74740, .T. ) ;
#29697 = ORIENTED_EDGE ( 'NONE', *, *, #214819, .F. ) ;
#29698 = CARTESIAN_POINT ( 'NONE',  ( -23.25000000000000000, 76.00000000001142553, -36.02310748452432421 ) ) ;
#29699 = ORIENTED_EDGE ( 'NONE', *, *, #24016, .T. ) ;
#29700 = ORIENTED_EDGE ( 'NONE', *, *, #77195, .F. ) ;
#29701 = EDGE_CURVE ( 'NONE', #52139, #20565, #191344, .T. ) ;
#29702 = CARTESIAN_POINT ( 'NONE',  ( -19.89999999999999858, 4.611773100472912112, 22.11686199900910665 ) ) ;
#29703 = DIRECTION ( 'NONE',  ( 0.000000000000000000, 0.000000000000000000, -1.000000000000000000 ) ) ;
#29704 = CARTESIAN_POINT ( 'NONE',  ( -14.22969084473441193, 9.456007326080463571, -185.9886334941467396 ) ) ;
#29707 = ADVANCED_FACE ( 'NONE', ( #140881 ), #160470, .F. ) ;
#29706 = VERTEX_POINT ( 'NONE', #178759 ) ;
#29705 = DIRECTION ( 'NONE',  ( 0.000000000000000000, 0.2128009952263601456, -0.9770955615653316162 ) ) ;
#29708 = CARTESIAN_POINT ( 'NONE',  ( -1.820710678118657944, 83.29276488265931278, -214.5670590782273166 ) ) ;
#29709 = CARTESIAN_POINT ( 'NONE',  ( 13.99999999999999822, 9.850000000011137402, -150.7500000000000284 ) ) ;
#29711 = ORIENTED_EDGE ( 'NONE', *, *, #26392, .T. ) ;
#29710 = DIRECTION ( 'NONE',  ( 0.000000000000000000, 0.000000000000000000, -1.000000000000000000 ) ) ;
#29712 = DIRECTION ( 'NONE',  ( -0.000000000000000000, -0.000000000000000000, -1.000000000000000000 ) ) ;
#29713 = ORIENTED_EDGE ( 'NONE', *, *, #157938, .F. ) ;
#29714 = EDGE_CURVE ( 'NONE', #241513, #50852, #239077, .T. ) ;
#29715 = DIRECTION ( 'NONE',  ( 0.000000000000000000, 0.000000000000000000, -1.000000000000000000 ) ) ;
#29716 = ORIENTED_EDGE ( 'NONE', *, *, #197497, .T. ) ;
#29717 = CARTESIAN_POINT ( 'NONE',  ( -20.94999999999999929, 18.71344899777637494, -226.7788045585494388 ) ) ;
#29718 = DIRECTION ( 'NONE',  ( 0.000000000000000000, 0.000000000000000000, 1.000000000000000000 ) ) ;
#29719 = CIRCLE ( 'NONE', #204637, 0.09999999999999939493 ) ;
#29720 = TOROIDAL_SURFACE ( 'NONE', #175456, 11.65000000000000036, 0.1000000000000000056 ) ;
#29721 = CIRCLE ( 'NONE', #113078, 0.09999999999999986677 ) ;
#29722 = ORIENTED_EDGE ( 'NONE', *, *, #256149, .T. ) ;
#29724 = FACE_OUTER_BOUND ( 'NONE', #252978, .T. ) ;
#29723 = CARTESIAN_POINT ( 'NONE',  ( -21.46681500597176395, 76.00000000001273293, -210.3806186439589396 ) ) ;
#29725 = CARTESIAN_POINT ( 'NONE',  ( 18.49999999999999645, 1.115600667400684642E-11, -200.9999999999999432 ) ) ;
#29726 = EDGE_CURVE ( 'NONE', #52869, #241355, #109871, .T. ) ;
#29727 = FACE_OUTER_BOUND ( 'NONE', #142125, .T. ) ;
#29728 = CARTESIAN_POINT ( 'NONE',  ( 23.40000000000005542, 74.16448838626247664, -47.52760213295649550 ) ) ;
#29729 = EDGE_CURVE ( 'NONE', #64566, #12012, #103013, .T. ) ;
#29730 = ORIENTED_EDGE ( 'NONE', *, *, #14339, .F. ) ;
#29731 = ORIENTED_EDGE ( 'NONE', *, *, #797, .T. ) ;
#29732 = CARTESIAN_POINT ( 'NONE',  ( -23.25000000000000000, -1.835859311432481045, -112.1044391687985780 ) ) ;
#29733 = DIRECTION ( 'NONE',  ( -0.7071067811865708874, 0.3338907855511046296, 0.6233112732207185536 ) ) ;
#29734 = ORIENTED_EDGE ( 'NONE', *, *, #243354, .F. ) ;
#29735 = CARTESIAN_POINT ( 'NONE',  ( -20.64999999999999858, 74.00000000001205080, -123.7984855617622060 ) ) ;
#29736 = ORIENTED_EDGE ( 'NONE', *, *, #160351, .T. ) ;
#29737 = EDGE_CURVE ( 'NONE', #109071, #191176, #181304, .T. ) ;
#29738 = DIRECTION ( 'NONE',  ( -0.000000000000000000, 0.2617529984165031243, 0.9651348961777157509 ) ) ;
#29739 = CARTESIAN_POINT ( 'NONE',  ( 20.97224591636399538, 60.18302304980271344, -221.2511297749800008 ) ) ;
#29740 = AXIS2_PLACEMENT_3D ( 'NONE', #74087, #151034, #93616 ) ;
#29741 = CARTESIAN_POINT ( 'NONE',  ( 20.94999999999999929, 76.00000000001173817, -73.52310748452431710 ) ) ;
#29742 = ORIENTED_EDGE ( 'NONE', *, *, #15944, .T. ) ;
#29743 = B_SPLINE_CURVE_WITH_KNOTS ( 'NONE', 3,
 ( #107657, #68545, #131073, #187223, #146758, #226301, #227602, #48967 ),
 .UNSPECIFIED., .F., .F.,
 ( 4, 2, 2, 4 ),
 ( 0.000000000000000000, 0.0002114466876442231736, 0.0003171700314663234441, 0.0004228933752884237417 ),
 .UNSPECIFIED. ) ;
#29744 = CARTESIAN_POINT ( 'NONE',  ( -16.77683809663752257, 66.05416425680844839, -190.8591584654202222 ) ) ;
#29745 = SURFACE_SIDE_STYLE ('',( #210914 ) ) ;
#29746 = EDGE_CURVE ( 'NONE', #184568, #91428, #122371, .T. ) ;
#29747 = ORIENTED_EDGE ( 'NONE', *, *, #95857, .F. ) ;
#29748 = VERTEX_POINT ( 'NONE', #63905 ) ;
#29749 = EDGE_LOOP ( 'NONE', ( #178144, #1013, #256263, #165819 ) ) ;
#29750 = EDGE_CURVE ( 'NONE', #101473, #145358, #67756, .T. ) ;
#29751 = CYLINDRICAL_SURFACE ( 'NONE', #224, 0.09999999999999939493 ) ;
#29752 = CARTESIAN_POINT ( 'NONE',  ( 22.39999999999999503, 64.25000000001215028, -136.5231074845243597 ) ) ;
#29753 = DIRECTION ( 'NONE',  ( 1.000000000000000000, 0.000000000000000000, 0.000000000000000000 ) ) ;
#29754 = CARTESIAN_POINT ( 'NONE',  ( 20.94999999999999929, -11.64999999999999147, -30.59999999999999432 ) ) ;
#29755 = DIRECTION ( 'NONE',  ( 0.000000000000000000, 6.982962677686266711E-15, -1.000000000000000000 ) ) ;
#29756 = CIRCLE ( 'NONE', #242092, 7.800000000000000711 ) ;
#29758 = FACE_OUTER_BOUND ( 'NONE', #57657, .T. ) ;
#29757 = CARTESIAN_POINT ( 'NONE',  ( 20.73486653747088937, 45.03492288895885309, -237.3066680331414489 ) ) ;
#29759 = EDGE_CURVE ( 'NONE', #254405, #9696, #246398, .T. ) ;
#29761 = VERTEX_POINT ( 'NONE', #170763 ) ;
#29760 = CARTESIAN_POINT ( 'NONE',  ( -21.05000000000000071, 61.16604239671104892, -234.3115055913011417 ) ) ;
#29762 = CARTESIAN_POINT ( 'NONE',  ( 18.52928932188133970, 10.27928932189250411, -91.75000000000005684 ) ) ;
#29763 = ORIENTED_EDGE ( 'NONE', *, *, #114474, .T. ) ;
#29764 = CARTESIAN_POINT ( 'NONE',  ( -20.64999999999999858, 1.940186915899004161, -188.1708807889466470 ) ) ;
#29765 = EDGE_CURVE ( 'NONE', #228509, #51680, #222278, .T. ) ;
#29766 = EDGE_LOOP ( 'NONE', ( #94971, #29736 ) ) ;
#29767 = ORIENTED_EDGE ( 'NONE', *, *, #202522, .F. ) ;
#29768 = CIRCLE ( 'NONE', #237825, 0.1000000000000001860 ) ;
#29769 = CARTESIAN_POINT ( 'NONE',  ( -16.94445028196808778, 9.992063609708889516, -46.10733017841845793 ) ) ;
#29770 = CARTESIAN_POINT ( 'NONE',  ( 20.94999999999999574, -11.41227409413852989, -136.9000000000000341 ) ) ;
#29771 = CARTESIAN_POINT ( 'NONE',  ( -21.59142135623730852, 7.850000000011158718, -112.8500000000000369 ) ) ;
#29772 = VECTOR ( 'NONE', #89532, 1000.000000000000227 ) ;
#29773 = CARTESIAN_POINT ( 'NONE',  ( -18.79999999999999716, 3.461118860469513336, 28.84309995045515507 ) ) ;
#29774 = AXIS2_PLACEMENT_3D ( 'NONE', #73705, #254821, #54103 ) ;
#29775 = ORIENTED_EDGE ( 'NONE', *, *, #199738, .F. ) ;
#29776 = EDGE_LOOP ( 'NONE', ( #152648, #252013, #29011, #94555, #77714, #248126 ) ) ;
#29777 = VECTOR ( 'NONE', #238544, 1000.000000000000000 ) ;
#29778 = CARTESIAN_POINT ( 'NONE',  ( -22.50000000000000000, 11.65000000001115588, -100.5000000000000284 ) ) ;
#29780 = EDGE_CURVE ( 'NONE', #112762, #88936, #143196, .T. ) ;
#29779 = VERTEX_POINT ( 'NONE', #190288 ) ;
#29781 = DIRECTION ( 'NONE',  ( 0.000000000000000000, 0.000000000000000000, 1.000000000000000000 ) ) ;
#29782 = CARTESIAN_POINT ( 'NONE',  ( 20.94999999999999929, -9.399999999988846611, -110.3939691226524786 ) ) ;
#29783 = ORIENTED_EDGE ( 'NONE', *, *, #104002, .F. ) ;
#29784 = DIRECTION ( 'NONE',  ( -0.000000000000000000, 1.000000000000000000, 6.982962677686266711E-15 ) ) ;
#29785 = DIRECTION ( 'NONE',  ( -1.000000000000000000, 1.614276770400120174E-15, 3.515722686956159758E-16 ) ) ;
#29786 = DIRECTION ( 'NONE',  ( -0.000000000000000000, 1.000000000000000000, 6.982962677686266711E-15 ) ) ;
#29787 = CARTESIAN_POINT ( 'NONE',  ( -20.64999999999999858, -8.999999999988846255, -177.3939691226524076 ) ) ;
#29788 = ORIENTED_EDGE ( 'NONE', *, *, #184364, .T. ) ;
#29789 = CARTESIAN_POINT ( 'NONE',  ( -20.64999999999999858, 71.65000000001207070, -124.1731074845243228 ) ) ;
#29791 = SPHERICAL_SURFACE ( 'NONE', #20871, 0.1000000000000000056 ) ;
#29790 = CIRCLE ( 'NONE', #246414, 0.5000000000000004441 ) ;
#29792 = LINE ( 'NONE', #191428, #62592 ) ;
#29794 = ADVANCED_FACE ( 'NONE', ( #26076 ), #147288, .F. ) ;
#29793 = DIRECTION ( 'NONE',  ( 0.000000000000000000, 0.000000000000000000, -1.000000000000000000 ) ) ;
#29795 = CARTESIAN_POINT ( 'NONE',  ( 20.85000000000000142, 28.60154115857409352, -258.4512230915049713 ) ) ;
#29796 = AXIS2_PLACEMENT_3D ( 'NONE', #48134, #202089, #83385 ) ;
#29797 = DIRECTION ( 'NONE',  ( 0.000000000000000000, -0.8814952561688476074, 0.4721928772777262417 ) ) ;
#29798 = AXIS2_PLACEMENT_3D ( 'NONE', #10344, #151134, #173306 ) ;
#29799 = ORIENTED_EDGE ( 'NONE', *, *, #71590, .T. ) ;
#29800 = AXIS2_PLACEMENT_3D ( 'NONE', #77544, #214507, #197509 ) ;
#29802 = EDGE_CURVE ( 'NONE', #135829, #175441, #243156, .T. ) ;
#29801 = CARTESIAN_POINT ( 'NONE',  ( 20.95512840106819752, 10.62384869377332031, -12.20247922079885328 ) ) ;
#29803 = ORIENTED_EDGE ( 'NONE', *, *, #76642, .F. ) ;
#29804 = AXIS2_PLACEMENT_3D ( 'NONE', #58404, #256580, #76701 ) ;
#29805 = CARTESIAN_POINT ( 'NONE',  ( -16.93658211146644987, 14.21365401117876814, -219.2987376607606507 ) ) ;
#29806 = CARTESIAN_POINT ( 'NONE',  ( 22.88900146558018989, 8.703904791123973084, -87.85000000000003695 ) ) ;
#29807 = LINE ( 'NONE', #53177, #50755 ) ;
#29808 = CARTESIAN_POINT ( 'NONE',  ( 20.58091095332318332, 66.98152984665858867, -161.6044573023666260 ) ) ;
#29809 = ORIENTED_EDGE ( 'NONE', *, *, #151432, .F. ) ;
#29810 = DIRECTION ( 'NONE',  ( -1.000000000000000000, -2.952720810173289112E-16, 0.000000000000000000 ) ) ;
#29811 = DIRECTION ( 'NONE',  ( 0.000000000000000000, 0.000000000000000000, -1.000000000000000000 ) ) ;
#29812 = CARTESIAN_POINT ( 'NONE',  ( -23.25000000000000000, 76.00000000001244871, -170.0231074845243597 ) ) ;
#29813 = EDGE_CURVE ( 'NONE', #71022, #37046, #17223, .T. ) ;
#29814 = AXIS2_PLACEMENT_3D ( 'NONE', #219036, #142067, #61261 ) ;
#29815 = VECTOR ( 'NONE', #96269, 1000.000000000000000 ) ;
#29816 = FACE_OUTER_BOUND ( 'NONE', #154389, .T. ) ;
#29817 = ORIENTED_EDGE ( 'NONE', *, *, #137989, .F. ) ;
#29818 = ORIENTED_EDGE ( 'NONE', *, *, #141008, .F. ) ;
#29819 = FACE_OUTER_BOUND ( 'NONE', #118142, .T. ) ;
#29820 = DIRECTION ( 'NONE',  ( 1.000000000000000000, 0.000000000000000000, 0.000000000000000000 ) ) ;
#29821 = CARTESIAN_POINT ( 'NONE',  ( 18.49999999999999289, 10.20857864377384239, -91.76715728752546397 ) ) ;
#29822 = PLANE ( 'NONE',  #70468 ) ;
#29823 = ORIENTED_EDGE ( 'NONE', *, *, #162173, .F. ) ;
#29824 = CARTESIAN_POINT ( 'NONE',  ( -21.05000000000000071, 1.115653327213047955E-11, -96.20000000000007390 ) ) ;
#29825 = CARTESIAN_POINT ( 'NONE',  ( 20.94999999999999929, 77.83534155023646406, -124.9679561919612922 ) ) ;
#29826 = ORIENTED_EDGE ( 'NONE', *, *, #203270, .F. ) ;
#29827 = CARTESIAN_POINT ( 'NONE',  ( 20.95512820512820440, 67.12384868372387814, -115.2731074845243597 ) ) ;
#29828 = ORIENTED_EDGE ( 'NONE', *, *, #189483, .T. ) ;
#29829 = ORIENTED_EDGE ( 'NONE', *, *, #220723, .F. ) ;
#29830 = ORIENTED_EDGE ( 'NONE', *, *, #227667, .F. ) ;
#29831 = DIRECTION ( 'NONE',  ( -0.000000000000000000, 0.000000000000000000, -1.000000000000000000 ) ) ;
#29832 = CARTESIAN_POINT ( 'NONE',  ( -20.64999999999999858, -9.400000000000002132, -23.60603087734756045 ) ) ;
#29833 = CARTESIAN_POINT ( 'NONE',  ( -21.14999999999999858, 10.21728496540352182, -227.9671432372868765 ) ) ;
#29834 = AXIS2_PLACEMENT_3D ( 'NONE', #163692, #204081, #86686 ) ;
#29835 = DIRECTION ( 'NONE',  ( 1.000000000000000000, -0.000000000000000000, -0.000000000000000000 ) ) ;
#29836 = DIRECTION ( 'NONE',  ( -1.000000000000000000, -0.000000000000000000, -0.000000000000000000 ) ) ;
#29837 = CARTESIAN_POINT ( 'NONE',  ( -20.54999999999999716, -8.663551401858004652, -110.0241011180673354 ) ) ;
#29838 = EDGE_CURVE ( 'NONE', #226886, #51917, #18312, .T. ) ;
#29840 = CYLINDRICAL_SURFACE ( 'NONE', #141282, 0.09999999999998898659 ) ;
#29839 = LINE ( 'NONE', #91066, #224279 ) ;
#29841 = CARTESIAN_POINT ( 'NONE',  ( 21.05000000000000071, -1.476031472317220317, -194.6925868278244991 ) ) ;
#29842 = DIRECTION ( 'NONE',  ( -5.603264701231745086E-32, 0.9126074666063769270, 0.4088369013363282733 ) ) ;
#29843 = DIRECTION ( 'NONE',  ( -4.448008912761043807E-16, 1.000000000000000000, -8.896017825522087613E-16 ) ) ;
#29844 = DIRECTION ( 'NONE',  ( 0.000000000000000000, 0.4721928772778128947, 0.8814952561688012000 ) ) ;
#29845 = ORIENTED_EDGE ( 'NONE', *, *, #29084, .T. ) ;
#29846 = ORIENTED_EDGE ( 'NONE', *, *, #113534, .T. ) ;
#29847 = CARTESIAN_POINT ( 'NONE',  ( -21.05315837397170142, 11.75000000001115019, -93.65835600089312152 ) ) ;
#29848 = DIRECTION ( 'NONE',  ( 0.000000000000000000, -0.1350103645451876666, -0.9908441862701600211 ) ) ;
#29850 = CARTESIAN_POINT ( 'NONE',  ( -23.15000000000000213, 11.75000000001115552, -45.75000000000000000 ) ) ;
#29849 = FACE_OUTER_BOUND ( 'NONE', #12497, .T. ) ;
#29851 = TOROIDAL_SURFACE ( 'NONE', #133859, 0.2000000000000000111, 0.1000000000000000056 ) ;
#29852 = CARTESIAN_POINT ( 'NONE',  ( 20.95325940946048249, 39.25995885369344762, -236.8548070915221047 ) ) ;
#29854 = ADVANCED_FACE ( 'NONE', ( #70357 ), #253556, .T. ) ;
#29853 = CARTESIAN_POINT ( 'NONE',  ( -20.64999999999999858, 1.115600667400684642E-11, -134.0000000000000000 ) ) ;
#29855 = DIRECTION ( 'NONE',  ( 1.000000000000000000, -3.265361837132813093E-16, -2.280189983783949500E-30 ) ) ;
#29856 = ORIENTED_EDGE ( 'NONE', *, *, #164913, .T. ) ;
#29857 = ORIENTED_EDGE ( 'NONE', *, *, #100672, .T. ) ;
#29858 = ADVANCED_FACE ( 'NONE', ( #6486 ), #228125, .F. ) ;
#29859 = DIRECTION ( 'NONE',  ( 0.000000000000000000, 0.2128009952263403282, -0.9770955615653358350 ) ) ;
#29860 = ORIENTED_EDGE ( 'NONE', *, *, #176621, .T. ) ;
#29861 = CARTESIAN_POINT ( 'NONE',  ( 22.39999999999999858, 1.115600667400684642E-11, -67.00000000000004263 ) ) ;
#29862 = VECTOR ( 'NONE', #163179, 1000.000000000000000 ) ;
#29863 = ADVANCED_FACE ( 'NONE', ( #7793 ), #207286, .F. ) ;
#29864 = CIRCLE ( 'NONE', #129777, 0.1000000000000028644 ) ;
#29865 = CARTESIAN_POINT ( 'NONE',  ( 21.97500000000000497, 66.25000000001158185, -57.27310748452438816 ) ) ;
#29866 = AXIS2_PLACEMENT_3D ( 'NONE', #67659, #108082, #175443 ) ;
#29867 = ADVANCED_FACE ( 'NONE', ( #148588 ), #54599, .T. ) ;
#29868 = EDGE_CURVE ( 'NONE', #57391, #45859, #105762, .T. ) ;
#29869 = VERTEX_POINT ( 'NONE', #214960 ) ;
#29870 = ORIENTED_EDGE ( 'NONE', *, *, #146724, .T. ) ;
#29871 = EDGE_CURVE ( 'NONE', #256969, #250524, #216230, .T. ) ;
#29872 = CARTESIAN_POINT ( 'NONE',  ( -20.64999999999999858, 85.00000000001261924, -193.6291383618718385 ) ) ;
#29873 = CARTESIAN_POINT ( 'NONE',  ( -20.94999999999999929, -11.41227409413852989, -137.0000000000000000 ) ) ;
#29874 = CARTESIAN_POINT ( 'NONE',  ( 21.30000000000002558, 76.00000000001213607, -136.5231074845242745 ) ) ;
#29875 = DIRECTION ( 'NONE',  ( 0.000000000000000000, -0.8496786552930076786, -0.5273008465188220306 ) ) ;
#29876 = DIRECTION ( 'NONE',  ( 0.000000000000000000, 0.2128009952263588411, -0.9770955615653318382 ) ) ;
#29877 = CARTESIAN_POINT ( 'NONE',  ( -20.94999999999999929, 74.83729825007388570, -95.12310748452432563 ) ) ;
#29878 = EDGE_CURVE ( 'NONE', #49525, #115218, #115868, .T. ) ;
#29879 = FACE_OUTER_BOUND ( 'NONE', #145956, .T. ) ;
#29880 = DIRECTION ( 'NONE',  ( 0.000000000000000000, -0.8660254037844383745, 0.5000000000000003331 ) ) ;
#29882 = ORIENTED_EDGE ( 'NONE', *, *, #231034, .T. ) ;
#29881 = CARTESIAN_POINT ( 'NONE',  ( 22.59999999999999787, 11.64957080755595520, -167.3999999999999773 ) ) ;
#29884 = CARTESIAN_POINT ( 'NONE',  ( 18.39999999999999503, 10.68101405709484197, -223.4922417449319028 ) ) ;
#29883 = CARTESIAN_POINT ( 'NONE',  ( -18.59999999999999787, 85.32100840337392356, -196.2871692354464130 ) ) ;
#29885 = EDGE_LOOP ( 'NONE', ( #130432, #58220, #54009, #221694 ) ) ;
#29887 = VERTEX_POINT ( 'NONE', #192848 ) ;
#29886 = LINE ( 'NONE', #125123, #160868 ) ;
#29888 = ORIENTED_EDGE ( 'NONE', *, *, #189380, .F. ) ;
#29889 = DIRECTION ( 'NONE',  ( 0.000000000000000000, 0.000000000000000000, -1.000000000000000000 ) ) ;
#29890 = CARTESIAN_POINT ( 'NONE',  ( -18.40000000000000213, 11.48667500176882328, -143.2500000000000284 ) ) ;
#29891 = CARTESIAN_POINT ( 'NONE',  ( 22.50000000000000000, 75.90000000001172964, -81.17267829206912211 ) ) ;
#29892 = DIRECTION ( 'NONE',  ( -1.000000000000000000, -1.836970198721029934E-16, -0.000000000000000000 ) ) ;
#29893 = CARTESIAN_POINT ( 'NONE',  ( -20.64999999999999858, 76.00000000001213607, -136.5231074845243313 ) ) ;
#29894 = DIRECTION ( 'NONE',  ( -1.000000000000000000, 0.000000000000000000, 0.000000000000000000 ) ) ;
#29896 = EDGE_CURVE ( 'NONE', #66806, #214983, #205740, .T. ) ;
#29895 = DIRECTION ( 'NONE',  ( 1.000000000000000000, 2.952720810173289112E-16, -0.000000000000000000 ) ) ;
#29897 = AXIS2_PLACEMENT_3D ( 'NONE', #98131, #96849, #196002 ) ;
#29898 = AXIS2_PLACEMENT_3D ( 'NONE', #166050, #147750, #146436 ) ;
#29900 = AXIS2_PLACEMENT_3D ( 'NONE', #128260, #207822, #227345 ) ;
#29899 = DIRECTION ( 'NONE',  ( 1.000000000000000000, 0.000000000000000000, 0.000000000000000000 ) ) ;
#29901 = ORIENTED_EDGE ( 'NONE', *, *, #88526, .T. ) ;
#29902 = ORIENTED_EDGE ( 'NONE', *, *, #38873, .T. ) ;
#29903 = DIRECTION ( 'NONE',  ( -1.000000000000000000, -0.000000000000000000, -0.000000000000000000 ) ) ;
#29904 = ORIENTED_EDGE ( 'NONE', *, *, #7528, .T. ) ;
#29905 = CARTESIAN_POINT ( 'NONE',  ( -20.94999999999999929, 0.2561057921033771945, -33.46510355832771211 ) ) ;
#29906 = VERTEX_POINT ( 'NONE', #251515 ) ;
#29907 = CARTESIAN_POINT ( 'NONE',  ( 23.24999999999999645, 68.08983204586466798, -237.7716021863518563 ) ) ;
#29908 = EDGE_CURVE ( 'NONE', #80974, #214401, #156310, .T. ) ;
#29909 = CARTESIAN_POINT ( 'NONE',  ( 19.81427058490548276, 11.66856398038106768, -24.75000000000000000 ) ) ;
#29910 = FACE_OUTER_BOUND ( 'NONE', #82322, .T. ) ;
#29911 = CARTESIAN_POINT ( 'NONE',  ( 20.94999999999999574, 14.00000000001115730, -172.9270925303825095 ) ) ;
#29912 = DIRECTION ( 'NONE',  ( 0.000000000000000000, -1.000000000000000000, 0.000000000000000000 ) ) ;
#29913 = EDGE_LOOP ( 'NONE', ( #202104, #66245, #251538, #171345 ) ) ;
#29914 = FACE_OUTER_BOUND ( 'NONE', #190567, .T. ) ;
#29915 = DIRECTION ( 'NONE',  ( 0.000000000000000000, 1.776356839400254803E-15, 1.000000000000000000 ) ) ;
#29916 = CYLINDRICAL_SURFACE ( 'NONE', #171440, 1.749999999999999778 ) ;
#29917 = DIRECTION ( 'NONE',  ( 0.000000000000000000, 0.7106264324241465813, -0.7035695228903323661 ) ) ;
#29919 = ADVANCED_FACE ( 'NONE', ( #33808 ), #153766, .F. ) ;
#29918 = CARTESIAN_POINT ( 'NONE',  ( 23.14999999999999858, -1.999999999988846699, -134.0000000000000284 ) ) ;
#29920 = VERTEX_POINT ( 'NONE', #16787 ) ;
#29922 = CARTESIAN_POINT ( 'NONE',  ( 20.94999999999999574, -1.349084418615859482, -175.4864989635454435 ) ) ;
#29921 = CARTESIAN_POINT ( 'NONE',  ( 21.14999999999999858, 60.91865828504416669, -234.1430899377568267 ) ) ;
#29923 = VERTEX_POINT ( 'NONE', #211120 ) ;
#29926 = VERTEX_POINT ( 'NONE', #194143 ) ;
#29925 = CARTESIAN_POINT ( 'NONE',  ( 20.95083306685154056, 67.08315735812212210, -161.5457826312660643 ) ) ;
#29924 = DIRECTION ( 'NONE',  ( -1.000000000000000000, 0.000000000000000000, -0.000000000000000000 ) ) ;
#29927 = ADVANCED_FACE ( 'NONE', ( #173326 ), #196669, .T. ) ;
#29928 = DIRECTION ( 'NONE',  ( 0.000000000000000000, 0.4999999999999956701, -0.8660254037844411501 ) ) ;
#29929 = DIRECTION ( 'NONE',  ( 0.000000000000000000, 1.000000000000000000, 0.000000000000000000 ) ) ;
#29930 = CARTESIAN_POINT ( 'NONE',  ( 22.50000000000000000, 64.05916333204672242, -247.1692862367248722 ) ) ;
#29931 = ORIENTED_EDGE ( 'NONE', *, *, #35996, .T. ) ;
#29932 = LINE ( 'NONE', #248968, #17829 ) ;
#29933 = AXIS2_PLACEMENT_3D ( 'NONE', #131936, #150238, #190653 ) ;
#29935 = ADVANCED_FACE ( 'NONE', ( #155019 ), #174617, .T. ) ;
#29934 = DIRECTION ( 'NONE',  ( 0.000000000000000000, 0.9126074666063769270, 0.4088369013363280513 ) ) ;
#29937 = CARTESIAN_POINT ( 'NONE',  ( 23.14999999999998437, 64.25000000001165290, -69.52310748452440237 ) ) ;
#29936 = CARTESIAN_POINT ( 'NONE',  ( -18.50000000000000000, 1.115600667400684642E-11, -67.00000000000000000 ) ) ;
#29939 = ORIENTED_EDGE ( 'NONE', *, *, #153006, .T. ) ;
#29938 = CARTESIAN_POINT ( 'NONE',  ( 18.50000000000000000, -9.499999999988842703, -73.60018939122204529 ) ) ;
#29940 = AXIS2_PLACEMENT_3D ( 'NONE', #246525, #67897, #125312 ) ;
#29941 = EDGE_CURVE ( 'NONE', #198941, #211904, #18500, .T. ) ;
#29942 = EDGE_CURVE ( 'NONE', #165206, #123641, #68572, .T. ) ;
#29943 = ORIENTED_EDGE ( 'NONE', *, *, #117843, .F. ) ;
#29944 = AXIS2_PLACEMENT_3D ( 'NONE', #168826, #170109, #147937 ) ;
#29945 = CARTESIAN_POINT ( 'NONE',  ( 21.05000000000000071, 69.35000000001262777, -193.6792853948412869 ) ) ;
#29946 = DIRECTION ( 'NONE',  ( 0.000000000000000000, 0.000000000000000000, -1.000000000000000000 ) ) ;
#29947 = CARTESIAN_POINT ( 'NONE',  ( 22.59999999999999787, 11.36146383068193444, -198.4232501820394816 ) ) ;
#29949 = EDGE_LOOP ( 'NONE', ( #137739, #36410, #63039, #78673 ) ) ;
#29948 = AXIS2_PLACEMENT_3D ( 'NONE', #142317, #202308, #198448 ) ;
#29950 = CARTESIAN_POINT ( 'NONE',  ( 18.49999999999999289, 6.846123162363745074, -171.2377262668498759 ) ) ;
#29951 = ADVANCED_FACE ( 'NONE', ( #97547 ), #152454, .F. ) ;
#29952 = AXIS2_PLACEMENT_3D ( 'NONE', #123431, #179571, #223797 ) ;
#29953 = DIRECTION ( 'NONE',  ( -1.000000000000000000, 0.000000000000000000, -0.000000000000000000 ) ) ;
#29954 = CARTESIAN_POINT ( 'NONE',  ( 18.39999999999999858, -9.519327731081283162, -140.9729763765593589 ) ) ;
#29955 = ORIENTED_EDGE ( 'NONE', *, *, #68430, .F. ) ;
#29956 = CARTESIAN_POINT ( 'NONE',  ( 20.94999999999999929, -8.999999999988842703, -191.6060308773475072 ) ) ;
#29957 = AXIS2_PLACEMENT_3D ( 'NONE', #173131, #169268, #251317 ) ;
#29958 = AXIS2_PLACEMENT_3D ( 'NONE', #85186, #228606, #207767 ) ;
#29959 = EDGE_LOOP ( 'NONE', ( #112820, #33566, #112019, #243181, #194787, #105028, #69831, #138111, #43145, #230486, #107683, #135926 ) ) ;
#29960 = AXIS2_PLACEMENT_3D ( 'NONE', #46527, #43978, #27015 ) ;
#29961 = DIRECTION ( 'NONE',  ( 1.000000000000000000, 0.000000000000000000, -0.000000000000000000 ) ) ;
#29962 = CYLINDRICAL_SURFACE ( 'NONE', #206341, 0.1000000000000028644 ) ;
#29963 = VECTOR ( 'NONE', #214620, 1000.000000000000000 ) ;
#29964 = EDGE_LOOP ( 'NONE', ( #122229, #11959, #86804, #141231 ) ) ;
#29965 = ORIENTED_EDGE ( 'NONE', *, *, #139310, .T. ) ;
#29966 = CIRCLE ( 'NONE', #59119, 11.80000000000000426 ) ;
#29967 = CARTESIAN_POINT ( 'NONE',  ( -20.85000000000000142, 78.48087866980282001, -232.8271061603568910 ) ) ;
#29968 = EDGE_LOOP ( 'NONE', ( #53964, #13965, #101412 ) ) ;
#29970 = ORIENTED_EDGE ( 'NONE', *, *, #158161, .T. ) ;
#29969 = CARTESIAN_POINT ( 'NONE',  ( 22.49999999999999289, 25.89494711235934687, -254.2627752153468350 ) ) ;
#29971 = EDGE_CURVE ( 'NONE', #245573, #69468, #135411, .T. ) ;
#29972 = EDGE_CURVE ( 'NONE', #206624, #57410, #12944, .T. ) ;
#29973 = AXIS2_PLACEMENT_3D ( 'NONE', #26373, #47185, #126747 ) ;
#29974 = ORIENTED_EDGE ( 'NONE', *, *, #224641, .T. ) ;
#29977 = ORIENTED_EDGE ( 'NONE', *, *, #152703, .F. ) ;
#29976 = ORIENTED_EDGE ( 'NONE', *, *, #32691, .F. ) ;
#29975 = DIRECTION ( 'NONE',  ( 1.000000000000000000, 0.000000000000000000, 0.000000000000000000 ) ) ;
#29979 = EDGE_CURVE ( 'NONE', #70573, #168873, #53325, .T. ) ;
#29978 = CARTESIAN_POINT ( 'NONE',  ( -18.40904629823846150, -9.499999999988851584, -107.1001895624817024 ) ) ;
#29980 = ORIENTED_EDGE ( 'NONE', *, *, #116315, .F. ) ;
#29981 = FACE_OUTER_BOUND ( 'NONE', #81194, .T. ) ;
#29982 = CARTESIAN_POINT ( 'NONE',  ( -21.05000000000000071, -1.489567864901279792, -194.6304332222954372 ) ) ;
#29983 = VECTOR ( 'NONE', #161029, 1000.000000000000000 ) ;
#29984 = AXIS2_PLACEMENT_3D ( 'NONE', #229284, #88447, #149761 ) ;
#29985 = DIRECTION ( 'NONE',  ( -1.000000000000000000, 0.000000000000000000, 0.000000000000000000 ) ) ;
#29986 =( BOUNDED_SURFACE ( )  B_SPLINE_SURFACE ( 3, 2, ( 
 ( #191178, #114181, #252390 ),
 ( #12540, #116750, #193729 ),
 ( #196286, #52918, #17641 ),
 ( #75091, #234123, #97143 ) ),
 .UNSPECIFIED., .F., .F., .T. ) 
 B_SPLINE_SURFACE_WITH_KNOTS ( ( 4, 4 ),
 ( 3, 3 ),
 ( 0.0006461284895274140927, 0.0007503702773985949665 ),
 ( 0.000000000000000000, 1.000000000000000000 ),
 .UNSPECIFIED. ) 
 GEOMETRIC_REPRESENTATION_ITEM ( )  RATIONAL_B_SPLINE_SURFACE ( (
 ( 1.000000000000000000, 0.7071067811865475727, 1.000000000000000000),
 ( 1.000000000000000000, 0.7076476444649274500, 1.000000000000000000),
 ( 1.000000000000000000, 0.7075727925191175327, 1.000000000000000000),
 ( 1.000000000000000000, 0.7071067811865558994, 1.000000000000000000) ) ) 
 REPRESENTATION_ITEM ( '' )  SURFACE ( )  );
#29987 = VECTOR ( 'NONE', #15080, 1000.000000000000000 ) ;
#29989 = CARTESIAN_POINT ( 'NONE',  ( 22.39999999999999858, 0.1000000000111554016, -25.70922040162662014 ) ) ;
#29988 = AXIS2_PLACEMENT_3D ( 'NONE', #209658, #12765, #53146 ) ;
#29990 = ORIENTED_EDGE ( 'NONE', *, *, #77044, .T. ) ;
#29991 = ORIENTED_EDGE ( 'NONE', *, *, #196405, .F. ) ;
#29992 = CARTESIAN_POINT ( 'NONE',  ( -21.55000000000000426, 7.708578643773852157, -121.7500000000000426 ) ) ;
#29994 = EDGE_LOOP ( 'NONE', ( #163652, #110192, #52928, #249685, #114836, #8278, #32152, #24584, #42163, #170412, #10672, #251547 ) ) ;
#29993 = CARTESIAN_POINT ( 'NONE',  ( 18.50000000000049383, 63.63806804479052914, -209.2187978148434979 ) ) ;
#29995 = DIRECTION ( 'NONE',  ( -1.000000000000000000, 0.000000000000000000, 0.000000000000000000 ) ) ;
#29997 = ORIENTED_EDGE ( 'NONE', *, *, #167330, .F. ) ;
#29996 = LINE ( 'NONE', #28732, #31679 ) ;
#29998 = ORIENTED_EDGE ( 'NONE', *, *, #54344, .T. ) ;
#29999 = CARTESIAN_POINT ( 'NONE',  ( 20.94999999999999574, 87.65000000001266756, -200.6231074845242688 ) ) ;
#30000 = ORIENTED_EDGE ( 'NONE', *, *, #96157, .F. ) ;
#30001 = SPHERICAL_SURFACE ( 'NONE', #156225, 0.1000000000000000056 ) ;
#30003 = ADVANCED_FACE ( 'NONE', ( #113295 ), #103971, .T. ) ;
#30002 = DIRECTION ( 'NONE',  ( 0.000000000000000000, -0.9770955615653316162, -0.2128009952263604232 ) ) ;
#30004 = VECTOR ( 'NONE', #236237, 1000.000000000000000 ) ;
#30006 = ORIENTED_EDGE ( 'NONE', *, *, #254181, .T. ) ;
#30005 = ORIENTED_EDGE ( 'NONE', *, *, #206902, .T. ) ;
#30007 = EDGE_LOOP ( 'NONE', ( #7584, #193070 ) ) ;
#30008 = CARTESIAN_POINT ( 'NONE',  ( 21.04999999999999716, 6.304455821958818262, -33.52103547654012772 ) ) ;
#30009 = ORIENTED_EDGE ( 'NONE', *, *, #174916, .F. ) ;
#30010 = ORIENTED_EDGE ( 'NONE', *, *, #245366, .T. ) ;
#30011 = DIRECTION ( 'NONE',  ( 0.000000000000000000, 0.000000000000000000, -1.000000000000000000 ) ) ;
#30014 = EDGE_CURVE ( 'NONE', #232094, #152894, #118444, .T. ) ;
#30013 = VERTEX_POINT ( 'NONE', #239666 ) ;
#30012 = DIRECTION ( 'NONE',  ( 0.000000000000000000, -0.9501938099239353175, 0.3116596277708039708 ) ) ;
#30015 = DIRECTION ( 'NONE',  ( 0.7071067811865493491, 0.7071067811865456854, 0.000000000000000000 ) ) ;
#30017 = DIRECTION ( 'NONE',  ( 0.000000000000000000, -1.000000000000000000, 0.000000000000000000 ) ) ;
#30016 = CARTESIAN_POINT ( 'NONE',  ( -20.64999999999999858, 24.07562609839690992, -252.7152152143214892 ) ) ;
#30018 = CARTESIAN_POINT ( 'NONE',  ( -21.45000000000000284, 7.708578643773852157, -112.7500000000000284 ) ) ;
#30019 = CARTESIAN_POINT ( 'NONE',  ( -12.60206096961792177, 62.27137470634865934, -218.2709398499965801 ) ) ;
#30020 = ORIENTED_EDGE ( 'NONE', *, *, #45576, .T. ) ;
#30021 = EDGE_CURVE ( 'NONE', #105632, #240452, #222221, .T. ) ;
#30022 = ORIENTED_EDGE ( 'NONE', *, *, #93786, .T. ) ;
#30023 = CARTESIAN_POINT ( 'NONE',  ( -21.05000000000000071, 74.25000000001259082, -191.8535959266227451 ) ) ;
#30024 = DIRECTION ( 'NONE',  ( 0.000000000000000000, 0.000000000000000000, 1.000000000000000000 ) ) ;
#30025 = EDGE_CURVE ( 'NONE', #249855, #19947, #122286, .T. ) ;
#30026 = ORIENTED_EDGE ( 'NONE', *, *, #141263, .F. ) ;
#30027 = EDGE_CURVE ( 'NONE', #150828, #24890, #143107, .T. ) ;
#30028 = VECTOR ( 'NONE', #172230, 1000.000000000000000 ) ;
#30029 = DIRECTION ( 'NONE',  ( 0.000000000000000000, 0.9126074666064236673, 0.4088369013362239679 ) ) ;
#30031 = EDGE_CURVE ( 'NONE', #249034, #206711, #243344, .T. ) ;
#30030 = EDGE_CURVE ( 'NONE', #179090, #213186, #143392, .T. ) ;
#30032 = VERTEX_POINT ( 'NONE', #220101 ) ;
#30033 = ORIENTED_EDGE ( 'NONE', *, *, #163048, .T. ) ;
#30034 = DIRECTION ( 'NONE',  ( 0.000000000000000000, 1.000000000000000000, 0.000000000000000000 ) ) ;
#30035 = DIRECTION ( 'NONE',  ( -0.000000000000000000, -0.000000000000000000, 1.000000000000000000 ) ) ;
#30036 = ORIENTED_EDGE ( 'NONE', *, *, #20276, .T. ) ;
#30037 = CARTESIAN_POINT ( 'NONE',  ( -18.50000000000000711, -9.419203418015495544, -174.7477858104286952 ) ) ;
#30038 = VERTEX_POINT ( 'NONE', #137971 ) ;
#30039 = CARTESIAN_POINT ( 'NONE',  ( 18.43630871534871218, -9.679800874791856913, -140.6606320679840394 ) ) ;
#30041 = DIRECTION ( 'NONE',  ( 0.000000000000000000, 0.9553114395362780620, -0.2956011730205483912 ) ) ;
#30040 =( BOUNDED_SURFACE ( )  B_SPLINE_SURFACE ( 3, 2, ( 
 ( #186024, #246005, #227703 ),
 ( #89474, #109040, #124778 ),
 ( #188582, #169069, #50337 ),
 ( #69950, #146871, #163900 ),
 ( #88172, #47773, #209429 ),
 ( #68654, #126035, #105151 ) ),
 .UNSPECIFIED., .F., .F., .F. ) 
 B_SPLINE_SURFACE_WITH_KNOTS ( ( 4, 2, 4 ),
 ( 3, 3 ),
 ( -1.776356839400250465E-15, 0.7853981633974468357, 1.570796326794895448 ),
 ( 0.000000000000000000, 1.000000000000000000 ),
 .UNSPECIFIED. ) 
 GEOMETRIC_REPRESENTATION_ITEM ( )  RATIONAL_B_SPLINE_SURFACE ( (
 ( 1.000000000000000000, 0.4999999999999704681, 1.000000000000000000),
 ( 1.000000000000000000, 0.4993418825335544931, 1.000000000000000000),
 ( 1.000000000000000000, 0.5278258667056193731, 1.000000000000000000),
 ( 1.000000000000000000, 0.6092287576697977824, 1.000000000000000000),
 ( 1.000000000000000000, 0.6611148371777476607, 1.000000000000000000),
 ( 1.000000000000000000, 0.7071067811865597852, 1.000000000000000000) ) ) 
 REPRESENTATION_ITEM ( '' )  SURFACE ( )  );
#30043 = DIRECTION ( 'NONE',  ( -1.000000000000000000, 0.000000000000000000, 0.000000000000000000 ) ) ;
#30042 = CARTESIAN_POINT ( 'NONE',  ( 21.14999999999999858, 1.316055977212909456, -230.7323992127457473 ) ) ;
#30044 = CARTESIAN_POINT ( 'NONE',  ( -16.87242674293849021, 9.950000000011138823, -87.85109024637240793 ) ) ;
#30045 = CARTESIAN_POINT ( 'NONE',  ( 22.94999999999999929, 0.000000000000000000, 0.000000000000000000 ) ) ;
#30046 = CARTESIAN_POINT ( 'NONE',  ( -21.64999999999999858, 7.349999999999998757, -21.25000000000000000 ) ) ;
#30047 = CARTESIAN_POINT ( 'NONE',  ( -23.15000000000000213, 82.09643798151613225, -215.4278993322501208 ) ) ;
#30048 = AXIS2_PLACEMENT_3D ( 'NONE', #177328, #118621, #256770 ) ;
#30049 = ORIENTED_EDGE ( 'NONE', *, *, #245581, .F. ) ;
#30050 = EDGE_CURVE ( 'NONE', #88021, #72890, #89398, .T. ) ;
#30051 = ADVANCED_FACE ( 'NONE', ( #44027 ), #161429, .T. ) ;
#30052 = CIRCLE ( 'NONE', #142439, 12.77500000000000924 ) ;
#30054 = ORIENTED_EDGE ( 'NONE', *, *, #100706, .F. ) ;
#30053 = ORIENTED_EDGE ( 'NONE', *, *, #100995, .F. ) ;
#30055 = EDGE_LOOP ( 'NONE', ( #16151, #95392, #12236, #116090, #214159, #48471, #226920, #139009, #37460, #5865, #166546, #247419, #36431, #103301, #97150, #28474, #106950, #198827, #177757, #45654, #38819, #117522, #9921, #194567, #222507, #229855, #53271 ) ) ;
#30056 = EDGE_CURVE ( 'NONE', #221551, #33482, #19331, .T. ) ;
#30057 = DIRECTION ( 'NONE',  ( 1.000000000000000000, 0.000000000000000000, 0.000000000000000000 ) ) ;
#30058 = DIRECTION ( 'NONE',  ( 0.000000000000000000, -0.9908441862701596881, -0.1350103645451904977 ) ) ;
#30060 = CARTESIAN_POINT ( 'NONE',  ( -20.85000000000000142, 62.46832465249013921, -225.2232495205141731 ) ) ;
#30059 = CARTESIAN_POINT ( 'NONE',  ( 23.14999999999999858, 55.49311008795314137, -234.6486875357297492 ) ) ;
#30061 = CARTESIAN_POINT ( 'NONE',  ( 18.59999999999999076, 19.02280865327213277, -233.3540837620168986 ) ) ;
#30062 = ORIENTED_EDGE ( 'NONE', *, *, #70594, .T. ) ;
#30063 = CARTESIAN_POINT ( 'NONE',  ( -22.49999999999999645, 11.74956712350054744, -100.3991416309013402 ) ) ;
#30064 = EDGE_CURVE ( 'NONE', #76792, #146896, #42739, .T. ) ;
#30065 = VERTEX_POINT ( 'NONE', #41482 ) ;
#30066 = CARTESIAN_POINT ( 'NONE',  ( -23.15000000000000213, 76.00000000001168132, -65.62310748452431142 ) ) ;
#30068 = VECTOR ( 'NONE', #54328, 1000.000000000000000 ) ;
#30067 = CARTESIAN_POINT ( 'NONE',  ( -20.94999999999999929, 72.02722222756959525, -225.1832529173024398 ) ) ;
#30069 = ADVANCED_FACE ( 'NONE', ( #238366 ), #59715, .F. ) ;
#30070 = CARTESIAN_POINT ( 'NONE',  ( -21.05000000000000071, 1.115653327213047955E-11, -62.70000000000008811 ) ) ;
#30072 = EDGE_LOOP ( 'NONE', ( #50689, #101298, #77671, #226157 ) ) ;
#30071 = B_SPLINE_CURVE_WITH_KNOTS ( 'NONE', 3,
 ( #41060, #198816, #218360, #39782 ),
 .UNSPECIFIED., .F., .F.,
 ( 4, 4 ),
 ( 0.000000000000000000, 7.713889350930119414E-05 ),
 .UNSPECIFIED. ) ;
#30073 = DIRECTION ( 'NONE',  ( 0.000000000000000000, -0.9126074666063660468, -0.4088369013363524762 ) ) ;
#30074 = CARTESIAN_POINT ( 'NONE',  ( 18.49999999999999645, 46.50671693017397246, -243.2369495081682942 ) ) ;
#30075 = ORIENTED_EDGE ( 'NONE', *, *, #146764, .F. ) ;
#30076 = VERTEX_POINT ( 'NONE', #119730 ) ;
#30077 = DIRECTION ( 'NONE',  ( 0.000000000000000000, 0.000000000000000000, -1.000000000000000000 ) ) ;
#30078 = CARTESIAN_POINT ( 'NONE',  ( 21.05000000000000071, 6.540656951701244282, -0.09999999999999939493 ) ) ;
#30079 = CARTESIAN_POINT ( 'NONE',  ( -20.85000000000000142, 74.93036000061670165, -233.6816308724374949 ) ) ;
#30080 = EDGE_CURVE ( 'NONE', #1569, #119358, #240949, .T. ) ;
#30081 = CARTESIAN_POINT ( 'NONE',  ( 20.89999999999999503, 1.212568896937007645, -8.000000000000000000 ) ) ;
#30082 = DIRECTION ( 'NONE',  ( 1.000000000000000000, 0.000000000000000000, 0.000000000000000000 ) ) ;
#30083 = PLANE ( 'NONE',  #50150 ) ;
#30084 = VERTEX_POINT ( 'NONE', #23206 ) ;
#30085 = DIRECTION ( 'NONE',  ( 0.000000000000000000, 0.000000000000000000, 1.000000000000000000 ) ) ;
#30088 = CARTESIAN_POINT ( 'NONE',  ( 23.14999999999999858, 1.115600667400684642E-11, -67.00000000000000000 ) ) ;
#30087 = CIRCLE ( 'NONE', #238328, 11.80000000000000426 ) ;
#30086 = CARTESIAN_POINT ( 'NONE',  ( -16.93415306273742260, 9.995622260023671046, -87.91005694236046963 ) ) ;
#30090 = CARTESIAN_POINT ( 'NONE',  ( 20.94999999999999929, -4.871452838297987142, -233.3782557782877518 ) ) ;
#30089 = AXIS2_PLACEMENT_3D ( 'NONE', #245646, #162272, #103543 ) ;
#30091 = VECTOR ( 'NONE', #17309, 1000.000000000000000 ) ;
#30093 = EDGE_CURVE ( 'NONE', #173330, #68843, #237948, .T. ) ;
#30092 = CARTESIAN_POINT ( 'NONE',  ( -18.42554971533677843, -9.497159669437746032, -7.039826913548645315 ) ) ;
#30094 = DIRECTION ( 'NONE',  ( 1.000000000000000000, 0.000000000000000000, 0.000000000000000000 ) ) ;
#30095 = DIRECTION ( 'NONE',  ( 2.840903330521631775E-16, -0.8700118002898321601, 0.4930308989875230585 ) ) ;
#30097 = ORIENTED_EDGE ( 'NONE', *, *, #169248, .T. ) ;
#30096 = CARTESIAN_POINT ( 'NONE',  ( -1.820710678118657944, -9.929289321870186313, -158.7500000000000284 ) ) ;
#30098 = EDGE_CURVE ( 'NONE', #85966, #224260, #181002, .T. ) ;
#30099 = VECTOR ( 'NONE', #99396, 1000.000000000000000 ) ;
#30100 = DIRECTION ( 'NONE',  ( 2.952720810173289112E-16, -1.000000000000000000, 0.000000000000000000 ) ) ;
#30101 = CARTESIAN_POINT ( 'NONE',  ( 18.59999999999998721, 19.85039924724470950, -69.28030305780140452 ) ) ;
#30102 = ORIENTED_EDGE ( 'NONE', *, *, #35523, .T. ) ;
#30103 = CIRCLE ( 'NONE', #184186, 0.09999999999999939493 ) ;
#30104 = DIRECTION ( 'NONE',  ( 1.000000000000000000, 0.000000000000000000, 0.000000000000000000 ) ) ;
#30105 = CARTESIAN_POINT ( 'NONE',  ( -21.05000000000000071, 0.09779029131994770863, -94.24218538952392521 ) ) ;
#30106 = DIRECTION ( 'NONE',  ( -1.000000000000000000, 0.000000000000000000, 0.000000000000000000 ) ) ;
#30107 = ORIENTED_EDGE ( 'NONE', *, *, #49437, .F. ) ;
#30108 = DIRECTION ( 'NONE',  ( 0.000000000000000000, 0.2128009952263403282, -0.9770955615653358350 ) ) ;
#30110 = VERTEX_POINT ( 'NONE', #126109 ) ;
#30109 = CARTESIAN_POINT ( 'NONE',  ( 21.70464131381650219, 68.90464198104452009, -170.0231074845243882 ) ) ;
#30111 = DIRECTION ( 'NONE',  ( -0.000000000000000000, 7.109473446599835262E-15, -1.000000000000000000 ) ) ;
#30112 = CIRCLE ( 'NONE', #79925, 0.09999999999999939493 ) ;
#30113 = CARTESIAN_POINT ( 'NONE',  ( 20.85000000000000142, 1.115600667400684642E-11, -167.5000000000000284 ) ) ;
#30114 = ORIENTED_EDGE ( 'NONE', *, *, #242400, .T. ) ;
#30115 = CARTESIAN_POINT ( 'NONE',  ( -16.85722902420150504, 66.05000000001261640, -190.7575600107546165 ) ) ;
#30116 = SHAPE_DEFINITION_REPRESENTATION ( #163737, #100031 ) ;
#30117 = CARTESIAN_POINT ( 'NONE',  ( 23.24999999999999289, 69.55000000001199112, -115.3731074845243398 ) ) ;
#30118 = DIRECTION ( 'NONE',  ( -1.000000000000000000, -0.000000000000000000, 0.000000000000000000 ) ) ;
#30120 = VECTOR ( 'NONE', #222964, 1000.000000000000000 ) ;
#30119 = DIRECTION ( 'NONE',  ( 0.000000000000000000, 0.7397890806274315390, 0.6728388485992909951 ) ) ;
#30121 = ORIENTED_EDGE ( 'NONE', *, *, #157124, .F. ) ;
#30122 = TOROIDAL_SURFACE ( 'NONE', #209153, 0.6000000000000006439, 0.1000000000000000056 ) ;
#30123 = DIRECTION ( 'NONE',  ( 0.000000000000000000, 0.000000000000000000, -1.000000000000000000 ) ) ;
#30124 = FACE_OUTER_BOUND ( 'NONE', #246390, .T. ) ;
#30125 = AXIS2_PLACEMENT_3D ( 'NONE', #126824, #167266, #129391 ) ;
#30126 = AXIS2_PLACEMENT_3D ( 'NONE', #200722, #2497, #97731 ) ;
#30127 = SPHERICAL_SURFACE ( 'NONE', #7863, 0.1000000000000000056 ) ;
#30128 = ORIENTED_EDGE ( 'NONE', *, *, #110219, .F. ) ;
#30129 = ORIENTED_EDGE ( 'NONE', *, *, #248744, .T. ) ;
#30131 = VECTOR ( 'NONE', #222438, 1000.000000000000000 ) ;
#30130 = CARTESIAN_POINT ( 'NONE',  ( 21.05000000000000071, 76.00000000001165290, -69.52310748452431710 ) ) ;
#30133 = VECTOR ( 'NONE', #43235, 1000.000000000000000 ) ;
#30132 = CARTESIAN_POINT ( 'NONE',  ( 18.39999999999999858, 85.50000000001185185, -96.42291809330220076 ) ) ;
#30134 = FACE_OUTER_BOUND ( 'NONE', #22811, .T. ) ;
#30135 = CARTESIAN_POINT ( 'NONE',  ( 21.06086055315971350, 8.774707514967413857, -146.2023221551539507 ) ) ;
#30136 = EDGE_CURVE ( 'NONE', #120786, #85465, #81013, .T. ) ;
#30138 = LINE ( 'NONE', #109638, #107772 ) ;
#30137 = CARTESIAN_POINT ( 'NONE',  ( 20.12500000000000000, 9.749999999999998224, -21.25000000000000000 ) ) ;
#30139 = AXIS2_PLACEMENT_3D ( 'NONE', #166222, #244434, #22852 ) ;
#30140 = AXIS2_PLACEMENT_3D ( 'NONE', #108266, #88664, #168279 ) ;
#30141 = CARTESIAN_POINT ( 'NONE',  ( -23.25000000000000000, 1.115600667400684642E-11, -134.0000000000000000 ) ) ;
#30143 = DIRECTION ( 'NONE',  ( -1.000000000000000000, 0.000000000000000000, -0.000000000000000000 ) ) ;
#30142 = AXIS2_PLACEMENT_3D ( 'NONE', #74988, #97041, #137478 ) ;
#30145 = VERTEX_POINT ( 'NONE', #88256 ) ;
#30144 = CARTESIAN_POINT ( 'NONE',  ( -16.88815647973233780, 12.41425476414399931, -211.2399925740093636 ) ) ;
#30146 = CARTESIAN_POINT ( 'NONE',  ( 21.08376601933332495, 69.65805272873672038, -170.0868834954544297 ) ) ;
#30147 = CARTESIAN_POINT ( 'NONE',  ( 20.94999999999999574, 87.75000000001162448, -66.62310748452424036 ) ) ;
#30149 = CARTESIAN_POINT ( 'NONE',  ( 23.14999999999999147, 1.115600667400684642E-11, -167.4999999999999716 ) ) ;
#30148 = CARTESIAN_POINT ( 'NONE',  ( -20.64999999999999858, 73.50000000001223555, -149.7477294072864709 ) ) ;
#30150 = AXIS2_PLACEMENT_3D ( 'NONE', #56683, #235344, #16334 ) ;
#30151 = ORIENTED_EDGE ( 'NONE', *, *, #52883, .F. ) ;
#30152 = CARTESIAN_POINT ( 'NONE',  ( -16.88328101497759448, 66.04964716579314654, -115.6719279695950888 ) ) ;
#30154 = ADVANCED_FACE ( 'NONE', ( #144377 ), #25749, .F. ) ;
#30153 = LINE ( 'NONE', #71848, #191363 ) ;
#30155 = CARTESIAN_POINT ( 'NONE',  ( 23.14999999999999858, 5.500000000011153745, -179.9052660189130677 ) ) ;
#30157 = CARTESIAN_POINT ( 'NONE',  ( 22.49999999999999645, 12.58798907299599534, -223.3278890275437050 ) ) ;
#30156 = AXIS2_PLACEMENT_3D ( 'NONE', #15259, #253835, #94772 ) ;
#30158 = ORIENTED_EDGE ( 'NONE', *, *, #256647, .T. ) ;
#30159 = ORIENTED_EDGE ( 'NONE', *, *, #20963, .F. ) ;
#30160 = ADVANCED_FACE ( 'NONE', ( #247351 ), #172665, .T. ) ;
#30161 = CARTESIAN_POINT ( 'NONE',  ( 21.04999999999999716, 6.304455821958816486, -100.5210354765401632 ) ) ;
#30162 = ORIENTED_EDGE ( 'NONE', *, *, #195277, .F. ) ;
#30163 = DIRECTION ( 'NONE',  ( -1.000000000000000000, -0.000000000000000000, -0.000000000000000000 ) ) ;
#30164 = CIRCLE ( 'NONE', #92675, 0.1999999999999987899 ) ;
#30165 = EDGE_LOOP ( 'NONE', ( #255883, #219928, #179320, #23474 ) ) ;
#30166 = VECTOR ( 'NONE', #14806, 1000.000000000000000 ) ;
#30167 = CARTESIAN_POINT ( 'NONE',  ( 20.94999999999999929, 76.00000000001246292, -171.9231074845243938 ) ) ;
#30168 = AXIS2_PLACEMENT_3D ( 'NONE', #88083, #29468, #45138 ) ;
#30169 = FACE_OUTER_BOUND ( 'NONE', #14457, .T. ) ;
#30170 = EDGE_CURVE ( 'NONE', #162722, #64408, #36839, .T. ) ;
#30172 = EDGE_CURVE ( 'NONE', #206647, #71756, #68727, .T. ) ;
#30171 = PLANE ( 'NONE',  #168040 ) ;
#30173 = ORIENTED_EDGE ( 'NONE', *, *, #205150, .T. ) ;
#30174 = ADVANCED_FACE ( 'NONE', ( #226487 ), #247628, .T. ) ;
#30175 = CARTESIAN_POINT ( 'NONE',  ( -17.11825945287481332, 14.23543104469003673, -219.1360829004572395 ) ) ;
#30176 = CARTESIAN_POINT ( 'NONE',  ( -18.50000972452446035, 68.00519115550238780, -224.2294631537215821 ) ) ;
#30177 = DIRECTION ( 'NONE',  ( 0.000000000000000000, -1.000000000000000000, -6.860497997771531562E-15 ) ) ;
#30178 = CYLINDRICAL_SURFACE ( 'NONE', #226827, 0.09999999999999939493 ) ;
#30179 = ADVANCED_FACE ( 'NONE', ( #49155 ), #184812, .F. ) ;
#30180 = CARTESIAN_POINT ( 'NONE',  ( 21.14999999999999858, 87.75000000001205080, -124.2731074845242176 ) ) ;
#30181 = ORIENTED_EDGE ( 'NONE', *, *, #49065, .T. ) ;
#30182 = CIRCLE ( 'NONE', #50975, 0.09999999999999158173 ) ;
#30184 = CARTESIAN_POINT ( 'NONE',  ( -21.14999999999999858, -0.1008583690875562017, -122.2504328765106294 ) ) ;
#30183 = CARTESIAN_POINT ( 'NONE',  ( 21.05000000000000071, 78.98983215084128062, -228.7927651294584450 ) ) ;
#30185 = ORIENTED_EDGE ( 'NONE', *, *, #210064, .F. ) ;
#30187 = ORIENTED_EDGE ( 'NONE', *, *, #214466, .F. ) ;
#30186 = PLANE ( 'NONE',  #89742 ) ;
#30188 = ORIENTED_EDGE ( 'NONE', *, *, #74783, .T. ) ;
#30189 = CARTESIAN_POINT ( 'NONE',  ( 20.85000000000000142, 76.00000000001142553, -36.02310748452432421 ) ) ;
#30190 = EDGE_CURVE ( 'NONE', #153040, #53024, #93497, .T. ) ;
#30191 = CARTESIAN_POINT ( 'NONE',  ( 18.55121869061587958, 10.32747123227773400, -72.57740328502492844 ) ) ;
#30192 = CARTESIAN_POINT ( 'NONE',  ( 18.52928932188133970, 65.72071067813041623, -78.37310748452439668 ) ) ;
#30193 = CARTESIAN_POINT ( 'NONE',  ( 21.05000000000000071, 65.31570632562440437, -128.9964335458868447 ) ) ;
#30194 = ORIENTED_EDGE ( 'NONE', *, *, #15154, .F. ) ;
#30195 = CARTESIAN_POINT ( 'NONE',  ( -20.85000000000000142, 7.675662554762638479, -241.7139905447625381 ) ) ;
#30196 = CARTESIAN_POINT ( 'NONE',  ( 23.15000000000000213, 87.48912529308852015, -173.0231074845243029 ) ) ;
#30197 = ORIENTED_EDGE ( 'NONE', *, *, #48637, .F. ) ;
#30199 = EDGE_CURVE ( 'NONE', #69221, #59204, #66155, .T. ) ;
#30198 = CARTESIAN_POINT ( 'NONE',  ( 18.52165635395202870, -9.481150711271050469, -174.5248375828624035 ) ) ;
#30200 = ORIENTED_EDGE ( 'NONE', *, *, #131741, .F. ) ;
#30201 = DIRECTION ( 'NONE',  ( 0.000000000000000000, 0.000000000000000000, -1.000000000000000000 ) ) ;
#30202 = VECTOR ( 'NONE', #9895, 1000.000000000000000 ) ;
#30203 = ORIENTED_EDGE ( 'NONE', *, *, #71757, .F. ) ;
#30204 = CARTESIAN_POINT ( 'NONE',  ( -20.07928932188135107, 9.220710678129810489, -179.8499999999999943 ) ) ;
#30205 = ORIENTED_EDGE ( 'NONE', *, *, #122331, .T. ) ;
#30206 = CARTESIAN_POINT ( 'NONE',  ( 23.40000000000004476, 77.16254490893143725, -44.02310748452479316 ) ) ;
#30207 = CARTESIAN_POINT ( 'NONE',  ( -23.15000000000000213, -8.596261682231830292, -91.04987248284976431 ) ) ;
#30208 = FACE_OUTER_BOUND ( 'NONE', #218990, .T. ) ;
#30209 = CARTESIAN_POINT ( 'NONE',  ( 20.94999999999999574, 76.00000000001237765, -170.0231074845243597 ) ) ;
#30210 = CIRCLE ( 'NONE', #63497, 4.049999999999998046 ) ;
#30211 = DIRECTION ( 'NONE',  ( -0.000000000000000000, 1.000000000000000000, 0.000000000000000000 ) ) ;
#30212 = CARTESIAN_POINT ( 'NONE',  ( 18.59999999999999432, 44.43513953521873106, -247.3415577889845736 ) ) ;
#30213 = ORIENTED_EDGE ( 'NONE', *, *, #31471, .F. ) ;
#30214 = CARTESIAN_POINT ( 'NONE',  ( 21.15000000000005187, 87.60324567546805952, -37.87437456276921210 ) ) ;
#30216 = ORIENTED_EDGE ( 'NONE', *, *, #162057, .T. ) ;
#30215 = VECTOR ( 'NONE', #179963, 1000.000000000000000 ) ;
#30218 = CARTESIAN_POINT ( 'NONE',  ( 21.05000000000000071, 67.22371710471938400, -90.87310748452436826 ) ) ;
#30217 = CARTESIAN_POINT ( 'NONE',  ( 18.39999999999999503, 5.650000000011139001, -180.1499999999999773 ) ) ;
#30219 = ADVANCED_FACE ( 'NONE', ( #109115 ), #118781, .T. ) ;
#30220 = ORIENTED_EDGE ( 'NONE', *, *, #203419, .T. ) ;
#30221 = CARTESIAN_POINT ( 'NONE',  ( -20.64999999999999858, 20.06933876993645782, -235.7297789824848451 ) ) ;
#30223 = FACE_OUTER_BOUND ( 'NONE', #145252, .T. ) ;
#30222 = AXIS2_PLACEMENT_3D ( 'NONE', #165387, #124978, #201946 ) ;
#30224 = DIRECTION ( 'NONE',  ( -0.000000000000000000, 0.1350103645451945777, -0.9908441862701590219 ) ) ;
#30225 = ORIENTED_EDGE ( 'NONE', *, *, #92323, .F. ) ;
#30227 = ORIENTED_EDGE ( 'NONE', *, *, #69954, .T. ) ;
#30226 = LINE ( 'NONE', #108466, #41405 ) ;
#30228 = EDGE_CURVE ( 'NONE', #167941, #141859, #156078, .T. ) ;
#30230 = EDGE_CURVE ( 'NONE', #195640, #73222, #6006, .T. ) ;
#30229 = CARTESIAN_POINT ( 'NONE',  ( -18.39999999999999858, 85.68240343348777799, -29.36626410711146562 ) ) ;
#30232 = CARTESIAN_POINT ( 'NONE',  ( 18.39999999999997371, 11.47316190337362940, -57.75000000000000711 ) ) ;
#30231 = CARTESIAN_POINT ( 'NONE',  ( -16.87683809663752399, 9.950000000011142376, -180.1499999999999773 ) ) ;
#30234 = ORIENTED_EDGE ( 'NONE', *, *, #51710, .T. ) ;
#30233 = FACE_OUTER_BOUND ( 'NONE', #129243, .T. ) ;
#30235 = AXIS2_PLACEMENT_3D ( 'NONE', #227531, #128443, #207999 ) ;
#30236 = ADVANCED_FACE ( 'NONE', ( #107845 ), #239257, .F. ) ;
#30237 = ADVANCED_FACE ( 'NONE', ( #13889 ), #15181, .F. ) ;
#30238 = VERTEX_POINT ( 'NONE', #72596 ) ;
#30239 = ADVANCED_FACE ( 'NONE', ( #132555 ), #135179, .T. ) ;
#30240 = EDGE_CURVE ( 'NONE', #169064, #43818, #255777, .T. ) ;
#30241 = CARTESIAN_POINT ( 'NONE',  ( 20.95512820512820440, 10.62384868372303615, -179.6499999999999773 ) ) ;
#30242 = CARTESIAN_POINT ( 'NONE',  ( 23.14999999999999503, 11.65000000001116298, -188.8499999999999659 ) ) ;
#30243 = ORIENTED_EDGE ( 'NONE', *, *, #82959, .F. ) ;
#30244 = DIRECTION ( 'NONE',  ( -3.469446951953515108E-14, 1.000000000000000000, 0.000000000000000000 ) ) ;
#30245 = ORIENTED_EDGE ( 'NONE', *, *, #217221, .T. ) ;
#30246 = EDGE_CURVE ( 'NONE', #124831, #228315, #213351, .T. ) ;
#30247 = VECTOR ( 'NONE', #92407, 1000.000000000000000 ) ;
#30248 = LINE ( 'NONE', #188030, #136595 ) ;
#30249 = CARTESIAN_POINT ( 'NONE',  ( -23.15000000000000213, 11.75000000001115552, -88.35000000000003695 ) ) ;
#30250 = VERTEX_POINT ( 'NONE', #94694 ) ;
#30251 = CARTESIAN_POINT ( 'NONE',  ( -23.15000000000000213, 11.65000000001115588, -79.25000000000004263 ) ) ;
#30252 = AXIS2_PLACEMENT_3D ( 'NONE', #90691, #169001, #227634 ) ;
#30253 = CIRCLE ( 'NONE', #130172, 0.1000000000000048767 ) ;
#30254 = VECTOR ( 'NONE', #237331, 1000.000000000000000 ) ;
#30255 = CIRCLE ( 'NONE', #101094, 0.09999999999999939493 ) ;
#30256 = ORIENTED_EDGE ( 'NONE', *, *, #70087, .T. ) ;
#30257 = DIRECTION ( 'NONE',  ( -1.000000000000000000, 0.000000000000000000, 0.000000000000000000 ) ) ;
#30258 = EDGE_CURVE ( 'NONE', #50587, #93986, #174296, .T. ) ;
#30259 = VERTEX_POINT ( 'NONE', #153446 ) ;
#30260 = ORIENTED_EDGE ( 'NONE', *, *, #102982, .F. ) ;
#30261 = CARTESIAN_POINT ( 'NONE',  ( -20.54999999999999716, 29.28400589394459530, -237.3759593473670293 ) ) ;
#30262 = ORIENTED_EDGE ( 'NONE', *, *, #182989, .F. ) ;
#30263 = CARTESIAN_POINT ( 'NONE',  ( 20.94999999999999929, 77.16270174995064224, -195.6231074845243540 ) ) ;
#30264 = ORIENTED_EDGE ( 'NONE', *, *, #100477, .F. ) ;
#30266 = ORIENTED_EDGE ( 'NONE', *, *, #226009, .F. ) ;
#30265 = DIRECTION ( 'NONE',  ( 0.000000000000000000, -0.5907332058517320572, 0.8068669527896995541 ) ) ;
#30267 = ADVANCED_FACE ( 'NONE', ( #136360 ), #31000, .T. ) ;
#30268 = EDGE_CURVE ( 'NONE', #56467, #177411, #111702, .T. ) ;
#30269 = ORIENTED_EDGE ( 'NONE', *, *, #233798, .F. ) ;
#30270 = CARTESIAN_POINT ( 'NONE',  ( 20.94999999999999929, 7.916168987336737572, -211.9720049928963874 ) ) ;
#30271 = ORIENTED_EDGE ( 'NONE', *, *, #43120, .T. ) ;
#30274 = ORIENTED_EDGE ( 'NONE', *, *, #110927, .F. ) ;
#30273 = ORIENTED_EDGE ( 'NONE', *, *, #24931, .F. ) ;
#30272 = CARTESIAN_POINT ( 'NONE',  ( 21.14999999999999858, 11.65000000001115943, -179.6499999999999773 ) ) ;
#30276 = DIRECTION ( 'NONE',  ( 1.000000000000000000, 0.000000000000000000, 0.000000000000000000 ) ) ;
#30275 = AXIS2_PLACEMENT_3D ( 'NONE', #238111, #116897, #140283 ) ;
#30277 = ORIENTED_EDGE ( 'NONE', *, *, #128764, .F. ) ;
#30278 = CIRCLE ( 'NONE', #192575, 0.1000000000000033362 ) ;
#30279 = ORIENTED_EDGE ( 'NONE', *, *, #73845, .T. ) ;
#30280 = AXIS2_PLACEMENT_3D ( 'NONE', #245813, #145411, #9756 ) ;
#30282 = ORIENTED_EDGE ( 'NONE', *, *, #107879, .T. ) ;
#30281 = FACE_OUTER_BOUND ( 'NONE', #20045, .T. ) ;
#30283 = CARTESIAN_POINT ( 'NONE',  ( -21.44999999999999929, 29.33122518167236237, -237.2878098217501588 ) ) ;
#30284 = ORIENTED_EDGE ( 'NONE', *, *, #232480, .F. ) ;
#30285 = CARTESIAN_POINT ( 'NONE',  ( -24.30000000000000071, -12.80000000000000249, 33.00000000000000000 ) ) ;
#30286 = CARTESIAN_POINT ( 'NONE',  ( 18.39999999999999858, -9.499999999988842703, -140.9146583429697159 ) ) ;
#30287 = CIRCLE ( 'NONE', #196857, 11.64999999999999325 ) ;
#30288 = ORIENTED_EDGE ( 'NONE', *, *, #157523, .T. ) ;
#30289 = DIRECTION ( 'NONE',  ( 0.000000000000000000, 0.1350103645451876666, 0.9908441862701600211 ) ) ;
#30290 = CARTESIAN_POINT ( 'NONE',  ( -21.44999999999999929, 11.48697431424113446, -220.1440440112397994 ) ) ;
#30291 = AXIS2_PLACEMENT_3D ( 'NONE', #252791, #33806, #233276 ) ;
#30293 = ORIENTED_EDGE ( 'NONE', *, *, #131848, .T. ) ;
#30292 = VECTOR ( 'NONE', #78080, 1000.000000000000000 ) ;
#30295 = EDGE_LOOP ( 'NONE', ( #148723, #207330, #213304 ) ) ;
#30294 = CARTESIAN_POINT ( 'NONE',  ( 19.94784844284934877, 54.41359201945252266, -228.7625389915575056 ) ) ;
#30296 = DIRECTION ( 'NONE',  ( 1.000000000000000000, 0.000000000000000000, 0.000000000000000000 ) ) ;
#30297 = AXIS2_PLACEMENT_3D ( 'NONE', #101251, #81699, #161300 ) ;
#30298 = AXIS2_PLACEMENT_3D ( 'NONE', #38882, #220069, #158837 ) ;
#30300 = ORIENTED_EDGE ( 'NONE', *, *, #3053, .T. ) ;
#30299 = ORIENTED_EDGE ( 'NONE', *, *, #233349, .F. ) ;
#30301 = EDGE_LOOP ( 'NONE', ( #178910, #77394, #52090, #40940 ) ) ;
#30302 = SPHERICAL_SURFACE ( 'NONE', #11770, 0.1000000000000000056 ) ;
#30303 = ORIENTED_EDGE ( 'NONE', *, *, #42357, .T. ) ;
#30304 = ORIENTED_EDGE ( 'NONE', *, *, #37990, .F. ) ;
#30305 = DIRECTION ( 'NONE',  ( -1.000000000000000000, 0.000000000000000000, 0.000000000000000000 ) ) ;
#30306 = EDGE_LOOP ( 'NONE', ( #193109, #35014, #136946, #100787 ) ) ;
#30307 = CARTESIAN_POINT ( 'NONE',  ( -13.39999999999994529, 64.25000000001119815, -23.72310748452479245 ) ) ;
#30308 = AXIS2_PLACEMENT_3D ( 'NONE', #202603, #63080, #60500 ) ;
#30309 = CARTESIAN_POINT ( 'NONE',  ( -23.25000000000000000, 76.00000000001136868, -28.12310748452432208 ) ) ;
#30311 = EDGE_LOOP ( 'NONE', ( #24319, #242860, #142210, #40788, #23680, #249184, #193562, #237266, #45732, #200686, #99771 ) ) ;
#30310 = VECTOR ( 'NONE', #20817, 1000.000000000000000 ) ;
#30312 = EDGE_CURVE ( 'NONE', #29779, #237818, #215912, .T. ) ;
#30313 = VERTEX_POINT ( 'NONE', #16475 ) ;
#30314 = AXIS2_PLACEMENT_3D ( 'NONE', #189659, #28044, #150538 ) ;
#30315 = CARTESIAN_POINT ( 'NONE',  ( -21.05000000000000071, 70.10000000001197407, -113.2422072491806944 ) ) ;
#30316 = ADVANCED_FACE ( 'NONE', ( #191268 ), #37316, .T. ) ;
#30317 = ORIENTED_EDGE ( 'NONE', *, *, #116711, .T. ) ;
#30318 = AXIS2_PLACEMENT_3D ( 'NONE', #84737, #122648, #178789 ) ;
#30319 = EDGE_CURVE ( 'NONE', #245391, #255725, #254990, .T. ) ;
#30320 = LINE ( 'NONE', #229784, #88701 ) ;
#30321 = ADVANCED_FACE ( 'NONE', ( #135094 ), #76406, .F. ) ;
#30322 = ORIENTED_EDGE ( 'NONE', *, *, #248128, .T. ) ;
#30323 = DIRECTION ( 'NONE',  ( 1.000000000000000000, 7.049440681616513945E-16, -1.911869773728117674E-16 ) ) ;
#30325 = ORIENTED_EDGE ( 'NONE', *, *, #156919, .T. ) ;
#30324 = CYLINDRICAL_SURFACE ( 'NONE', #221168, 7.899999999999990585 ) ;
#30326 = CYLINDRICAL_SURFACE ( 'NONE', #59440, 0.1000000000000028644 ) ;
#30327 = CARTESIAN_POINT ( 'NONE',  ( 18.49999999999999289, 16.67126802362266247, -222.8016931105129004 ) ) ;
#30328 = FACE_OUTER_BOUND ( 'NONE', #115944, .T. ) ;
#30329 = CARTESIAN_POINT ( 'NONE',  ( 23.25000000000000000, 85.60000000001231513, -160.1291383618718385 ) ) ;
#30330 = DIRECTION ( 'NONE',  ( 0.000000000000000000, -1.000000000000000000, 0.000000000000000000 ) ) ;
#30331 = LINE ( 'NONE', #105972, #157918 ) ;
#30332 = DIRECTION ( 'NONE',  ( 2.659396599871503635E-15, -0.6132151058540604716, 0.7899159663865477077 ) ) ;
#30333 = DIRECTION ( 'NONE',  ( 0.000000000000000000, -1.000000000000000000, -6.352154140967427193E-15 ) ) ;
#30334 = LINE ( 'NONE', #31637, #180673 ) ;
#30335 = AXIS2_PLACEMENT_3D ( 'NONE', #63901, #143431, #222959 ) ;
#30337 = ORIENTED_EDGE ( 'NONE', *, *, #8267, .T. ) ;
#30336 = VECTOR ( 'NONE', #199195, 1000.000000000000114 ) ;
#30338 = EDGE_CURVE ( 'NONE', #218378, #258034, #159905, .T. ) ;
#30339 = CIRCLE ( 'NONE', #138439, 0.1000000000000072220 ) ;
#30340 = ADVANCED_FACE ( 'NONE', ( #222316 ), #43715, .T. ) ;
#30341 = ORIENTED_EDGE ( 'NONE', *, *, #110912, .F. ) ;
#30343 = ORIENTED_EDGE ( 'NONE', *, *, #34532, .F. ) ;
#30342 = CARTESIAN_POINT ( 'NONE',  ( -18.40000000000000213, 11.75000000001113953, -113.1500000000000341 ) ) ;
#30344 = VERTEX_POINT ( 'NONE', #101063 ) ;
#30345 = FACE_BOUND ( 'NONE', #90075, .T. ) ;
#30346 =( BOUNDED_CURVE ( )  B_SPLINE_CURVE ( 3, ( #147694, #69458, #70751, #189389 ),
 .UNSPECIFIED., .F., .T. ) 
 B_SPLINE_CURVE_WITH_KNOTS ( ( 4, 4 ),
 ( 4.712388980384689674, 6.283185307179586232 ),
 .UNSPECIFIED. ) 
 CURVE ( )  GEOMETRIC_REPRESENTATION_ITEM ( )  RATIONAL_B_SPLINE_CURVE ( ( 1.000000000000000000, 0.8047378541243649375, 0.8047378541243649375, 1.000000000000000000 ) ) 
 REPRESENTATION_ITEM ( '' )  );
#30347 = DIRECTION ( 'NONE',  ( 0.000000000000000000, 1.000000000000000000, 6.982962677686266711E-15 ) ) ;
#30349 = CARTESIAN_POINT ( 'NONE',  ( 18.49999999999999645, -1.135018845910178431, -41.21697688343231647 ) ) ;
#30348 = DIRECTION ( 'NONE',  ( 1.000000000000000000, 0.000000000000000000, 0.000000000000000000 ) ) ;
#30350 = ORIENTED_EDGE ( 'NONE', *, *, #139916, .F. ) ;
#30351 = ORIENTED_EDGE ( 'NONE', *, *, #93247, .T. ) ;
#30352 =( NAMED_UNIT ( * ) SI_UNIT ( $, .STERADIAN. ) SOLID_ANGLE_UNIT ( ) );
#30353 = EDGE_CURVE ( 'NONE', #131951, #218226, #230898, .T. ) ;
#30354 = DIRECTION ( 'NONE',  ( -1.040834085586054343E-13, 0.9999176327611370985, 0.01283462868040226822 ) ) ;
#30355 = EDGE_CURVE ( 'NONE', #177267, #80905, #2083, .T. ) ;
#30356 = DIRECTION ( 'NONE',  ( 0.000000000000000000, 0.8814952561688437216, -0.4721928772777334582 ) ) ;
#30357 = AXIS2_PLACEMENT_3D ( 'NONE', #46358, #43816, #105019 ) ;
#30358 = EDGE_LOOP ( 'NONE', ( #103076, #100172, #84483, #32103 ) ) ;
#30359 = ORIENTED_EDGE ( 'NONE', *, *, #23116, .F. ) ;
#30360 = CARTESIAN_POINT ( 'NONE',  ( -16.80468759584937644, 9.942153675145295466, -180.1900188662016546 ) ) ;
#30361 = DIRECTION ( 'NONE',  ( -4.701977403289178058E-30, 1.734723475976807094E-14, -1.000000000000000000 ) ) ;
#30362 = CYLINDRICAL_SURFACE ( 'NONE', #88679, 0.1000000000000000472 ) ;
#30363 = AXIS2_PLACEMENT_3D ( 'NONE', #96495, #173544, #234747 ) ;
#30364 = CARTESIAN_POINT ( 'NONE',  ( -20.85000000000000142, 68.97833521811203639, -132.6895420826271277 ) ) ;
#30366 = ORIENTED_EDGE ( 'NONE', *, *, #237160, .T. ) ;
#30365 = DIRECTION ( 'NONE',  ( 0.000000000000000000, -6.982962677686266711E-15, 1.000000000000000000 ) ) ;
#30367 = DIRECTION ( 'NONE',  ( 0.000000000000000000, -0.8814952561688430555, 0.4721928772777346239 ) ) ;
#30368 = EDGE_CURVE ( 'NONE', #50227, #16840, #172850, .T. ) ;
#30369 = DIRECTION ( 'NONE',  ( 1.000000000000000000, 0.000000000000000000, 0.000000000000000000 ) ) ;
#30370 = CARTESIAN_POINT ( 'NONE',  ( -17.01825945287481545, 66.05000000001153637, -48.77310748452439526 ) ) ;
#30371 = CARTESIAN_POINT ( 'NONE',  ( 22.39999999999999503, 64.25000000001193712, -102.9231074845243938 ) ) ;
#30372 = ORIENTED_EDGE ( 'NONE', *, *, #81123, .T. ) ;
#30373 = CARTESIAN_POINT ( 'NONE',  ( 14.22916352759893854, 66.54258906972165732, -84.52319157577809960 ) ) ;
#30374 = EDGE_CURVE ( 'NONE', #235865, #81327, #247816, .T. ) ;
#30375 = DIRECTION ( 'NONE',  ( 0.000000000000000000, 0.8814952561688476074, -0.4721928772777262417 ) ) ;
#30377 = CARTESIAN_POINT ( 'NONE',  ( -18.59999999999999787, 13.63658454968486389, -219.6758818217417968 ) ) ;
#30376 = DIRECTION ( 'NONE',  ( 1.000000000000000000, 0.000000000000000000, 0.000000000000000000 ) ) ;
#30378 = DIRECTION ( 'NONE',  ( 0.000000000000000000, 0.000000000000000000, -1.000000000000000000 ) ) ;
#30379 = CARTESIAN_POINT ( 'NONE',  ( -16.84793658983419107, 9.950000000011138823, -54.26635332218975805 ) ) ;
#30381 = EDGE_CURVE ( 'NONE', #128197, #158817, #142787, .T. ) ;
#30380 = CARTESIAN_POINT ( 'NONE',  ( 20.94999999999999929, -1.135018845899022466, -175.2169768834323520 ) ) ;
#30382 = CARTESIAN_POINT ( 'NONE',  ( -18.50000000000000711, 11.65000000001115232, -141.0148057706539930 ) ) ;
#30383 = DIRECTION ( 'NONE',  ( 1.000000000000000000, -7.304098846218134667E-16, 0.000000000000000000 ) ) ;
#30384 = CARTESIAN_POINT ( 'NONE',  ( 22.50000000000000000, 75.90000000001170122, -77.31388708289770761 ) ) ;
#30385 = VERTEX_POINT ( 'NONE', #59386 ) ;
#30386 = CIRCLE ( 'NONE', #142763, 0.09999999999998898659 ) ;
#30387 = VERTEX_POINT ( 'NONE', #126785 ) ;
#30388 = ORIENTED_EDGE ( 'NONE', *, *, #204835, .T. ) ;
#30389 = CARTESIAN_POINT ( 'NONE',  ( 20.54374330479327426, 65.49498968578889446, -95.29742384963557811 ) ) ;
#30390 = DIRECTION ( 'NONE',  ( 0.000000000000000000, -1.000000000000000000, -8.717686153663073805E-15 ) ) ;
#30391 = ORIENTED_EDGE ( 'NONE', *, *, #153492, .T. ) ;
#30392 = EDGE_CURVE ( 'NONE', #181669, #206624, #218476, .T. ) ;
#30393 = ORIENTED_EDGE ( 'NONE', *, *, #226142, .F. ) ;
#30394 = EDGE_CURVE ( 'NONE', #106265, #161501, #89575, .T. ) ;
#30395 = CIRCLE ( 'NONE', #142773, 0.5000000000000004441 ) ;
#30396 = EDGE_LOOP ( 'NONE', ( #170779, #68535, #4602, #209987, #168653 ) ) ;
#30397 = LINE ( 'NONE', #32999, #121177 ) ;
#30398 = ORIENTED_EDGE ( 'NONE', *, *, #101447, .F. ) ;
#30399 = AXIS2_PLACEMENT_3D ( 'NONE', #182215, #243454, #161373 ) ;
#30400 = FACE_OUTER_BOUND ( 'NONE', #237720, .T. ) ;
#30401 = CARTESIAN_POINT ( 'NONE',  ( -23.15000000000000213, 7.575715430069919876, -235.7846019917273281 ) ) ;
#30402 = DIRECTION ( 'NONE',  ( 1.000000000000000000, -7.304098846218133681E-16, 0.000000000000000000 ) ) ;
#30403 = AXIS2_PLACEMENT_3D ( 'NONE', #43845, #4688, #20444 ) ;
#30404 = CYLINDRICAL_SURFACE ( 'NONE', #179100, 0.1000000000000004496 ) ;
#30405 = DIRECTION ( 'NONE',  ( 1.000000000000000000, -0.000000000000000000, -0.000000000000000000 ) ) ;
#30407 = ORIENTED_EDGE ( 'NONE', *, *, #64179, .T. ) ;
#30406 = CARTESIAN_POINT ( 'NONE',  ( 20.97462148592277487, 44.21428412855883749, -236.4418601092407926 ) ) ;
#30409 = LINE ( 'NONE', #10837, #79372 ) ;
#30408 = DIRECTION ( 'NONE',  ( -0.000000000000000000, -0.6132151058540604716, 0.7899159663865477077 ) ) ;
#30410 = CARTESIAN_POINT ( 'NONE',  ( 18.49999999999999289, 65.67426406872368716, -78.17310748452437963 ) ) ;
#30411 = ORIENTED_EDGE ( 'NONE', *, *, #71398, .F. ) ;
#30412 = CARTESIAN_POINT ( 'NONE',  ( 13.88302573338718560, 66.54258905524463330, -121.5230235107343333 ) ) ;
#30413 = CARTESIAN_POINT ( 'NONE',  ( -16.81744102076748959, 66.05000000001182059, -82.17310748452439384 ) ) ;
#30414 = CARTESIAN_POINT ( 'NONE',  ( 21.04999999999999361, 0.03486800302426068532, -60.72991413631088875 ) ) ;
#30415 = ORIENTED_EDGE ( 'NONE', *, *, #20241, .T. ) ;
#30416 = AXIS2_PLACEMENT_3D ( 'NONE', #182361, #222738, #44127 ) ;
#30417 =( NAMED_UNIT ( * ) SI_UNIT ( $, .STERADIAN. ) SOLID_ANGLE_UNIT ( ) );
#30419 = DIRECTION ( 'NONE',  ( 0.000000000000000000, 0.000000000000000000, -1.000000000000000000 ) ) ;
#30418 = AXIS2_PLACEMENT_3D ( 'NONE', #136368, #19020, #215920 ) ;
#30420 = DIRECTION ( 'NONE',  ( 0.000000000000000000, 0.000000000000000000, -1.000000000000000000 ) ) ;
#30421 = VERTEX_POINT ( 'NONE', #39892 ) ;
#30422 = DIRECTION ( 'NONE',  ( 0.000000000000000000, 0.000000000000000000, -1.000000000000000000 ) ) ;
#30423 = CARTESIAN_POINT ( 'NONE',  ( 23.15000000000000213, -11.74999999999999112, -30.39999999999999858 ) ) ;
#30424 = VECTOR ( 'NONE', #221152, 1000.000000000000000 ) ;
#30425 = CARTESIAN_POINT ( 'NONE',  ( 18.79999999999999716, 11.75000000000000000, 22.10000000000000142 ) ) ;
#30426 = DIRECTION ( 'NONE',  ( 0.000000000000000000, -0.8096735173027155286, 0.5868805631290314739 ) ) ;
#30427 = VERTEX_POINT ( 'NONE', #221055 ) ;
#30428 = ORIENTED_EDGE ( 'NONE', *, *, #6403, .T. ) ;
#30429 = CIRCLE ( 'NONE', #255212, 4.900000000000004796 ) ;
#30430 = AXIS2_PLACEMENT_3D ( 'NONE', #27300, #46803, #248887 ) ;
#30431 = CIRCLE ( 'NONE', #242799, 0.09999999999999939493 ) ;
#30432 = CARTESIAN_POINT ( 'NONE',  ( -17.11825945287481687, 65.95000000001255103, -182.6731074845244507 ) ) ;
#30433 = CARTESIAN_POINT ( 'NONE',  ( 23.24999999999999289, 64.35000000001267040, -203.5231074845244166 ) ) ;
#30434 = CARTESIAN_POINT ( 'NONE',  ( 20.85882249326303040, 65.66751761918722252, -164.4282609406112670 ) ) ;
#30435 = FACE_OUTER_BOUND ( 'NONE', #73997, .T. ) ;
#30436 = EDGE_CURVE ( 'NONE', #110098, #46741, #68750, .T. ) ;
#30438 = CARTESIAN_POINT ( 'NONE',  ( -21.05000000000000071, 77.16270174995034381, -162.0231074845243313 ) ) ;
#30437 = CYLINDRICAL_SURFACE ( 'NONE', #184229, 0.09999999999999982514 ) ;
#30439 = DIRECTION ( 'NONE',  ( -0.000000000000000000, 0.2617529984165031243, 0.9651348961777157509 ) ) ;
#30440 = CARTESIAN_POINT ( 'NONE',  ( -20.94999999999999929, 1.162701749949165642, -141.9000000000000341 ) ) ;
#30441 = CARTESIAN_POINT ( 'NONE',  ( 18.50000000000000000, -0.7490476236415681832, -242.2033265267442061 ) ) ;
#30442 = EDGE_LOOP ( 'NONE', ( #17162, #252191, #79292, #109650 ) ) ;
#30443 = CARTESIAN_POINT ( 'NONE',  ( -20.90851465518106167, 65.67467670974416194, -97.45317318268841689 ) ) ;
#30444 = B_SPLINE_CURVE_WITH_KNOTS ( 'NONE', 3,
 ( #87963, #243202, #67146, #247049, #47563, #204076, #85384, #68440, #227492, #108832, #9731, #50138, #74887, #31904, #153149, #12336, #55251, #133540, #253476, #52708, #231372, #150545, #113967, #154430, #72298, #190976 ),
 .UNSPECIFIED., .F., .F.,
 ( 4, 2, 2, 2, 2, 2, 2, 2, 2, 2, 2, 2, 4 ),
 ( 0.005476422646581350848, 0.006160811967703534037, 0.006845201288825718093, 0.007187395949386826167, 0.007529590609947933375, 0.007871785270509041449, 0.008213979931070149523, 0.008556174591631257598, 0.008898369252192365672, 0.009240563912753473746, 0.009582758573314580086, 0.01026714789443682226, 0.01095153721555906443 ),
 .UNSPECIFIED. ) ;
#30446 = ORIENTED_EDGE ( 'NONE', *, *, #246309, .F. ) ;
#30445 = DIRECTION ( 'NONE',  ( 0.000000000000000000, 0.000000000000000000, -1.000000000000000000 ) ) ;
#30447 = CARTESIAN_POINT ( 'NONE',  ( 20.99142135623731065, 16.98881331171930498, -224.4946931418895701 ) ) ;
#30448 = CYLINDRICAL_SURFACE ( 'NONE', #36577, 0.1000000000000028644 ) ;
#30449 = CARTESIAN_POINT ( 'NONE',  ( 23.14999999999999503, 53.24180694658302571, -234.8354225850497130 ) ) ;
#30450 =( BOUNDED_SURFACE ( )  B_SPLINE_SURFACE ( 3, 2, ( 
 ( #18886, #254871, #76287 ),
 ( #98382, #155863, #177984 ),
 ( #235362, #56698, #103547 ),
 ( #86540, #220929, #43600 ) ),
 .UNSPECIFIED., .F., .F., .T. ) 
 B_SPLINE_SURFACE_WITH_KNOTS ( ( 4, 4 ),
 ( 3, 3 ),
 ( -8.673617379884035472E-18, 0.001979672783031532438 ),
 ( 0.000000000000000000, 1.000000000000000000 ),
 .UNSPECIFIED. ) 
 GEOMETRIC_REPRESENTATION_ITEM ( )  RATIONAL_B_SPLINE_SURFACE ( (
 ( 1.000000000000000000, 0.7103081912007066512, 1.000000000000000000),
 ( 1.000000000000000000, 0.7104998333558129042, 1.000000000000000000),
 ( 1.000000000000000000, 0.7107238315756106983, 1.000000000000000000),
 ( 1.000000000000000000, 0.7110073749539022048, 1.000000000000000000) ) ) 
 REPRESENTATION_ITEM ( '' )  SURFACE ( )  );
#30451 = CARTESIAN_POINT ( 'NONE',  ( -18.79999999999999716, 6.783826713665066066, 9.593862367105556288 ) ) ;
#30452 = EDGE_CURVE ( 'NONE', #159714, #210115, #17712, .T. ) ;
#30453 = FACE_OUTER_BOUND ( 'NONE', #102125, .T. ) ;
#30455 = ORIENTED_EDGE ( 'NONE', *, *, #181212, .F. ) ;
#30454 = DIRECTION ( 'NONE',  ( 2.952720810173289112E-16, 0.4088369013363280513, -0.9126074666063769270 ) ) ;
#30456 = FACE_OUTER_BOUND ( 'NONE', #237170, .T. ) ;
#30457 = DIRECTION ( 'NONE',  ( 1.000000000000000000, -0.000000000000000000, 0.000000000000000000 ) ) ;
#30458 = FACE_OUTER_BOUND ( 'NONE', #61380, .T. ) ;
#30459 = ORIENTED_EDGE ( 'NONE', *, *, #256556, .T. ) ;
#30460 = DIRECTION ( 'NONE',  ( -0.000000000000000000, -0.8660254037844411501, -0.4999999999999956701 ) ) ;
#30461 = EDGE_CURVE ( 'NONE', #49384, #108024, #147424, .T. ) ;
#30463 = EDGE_CURVE ( 'NONE', #235258, #194903, #114541, .T. ) ;
#30462 = ORIENTED_EDGE ( 'NONE', *, *, #134829, .T. ) ;
#30464 = TOROIDAL_SURFACE ( 'NONE', #239111, 1.900000000000002576, 0.1000000000000000056 ) ;
#30465 = AXIS2_PLACEMENT_3D ( 'NONE', #158334, #102139, #139992 ) ;
#30466 = CARTESIAN_POINT ( 'NONE',  ( -17.11825945287482753, 66.05000000001189164, -90.27310748452437394 ) ) ;
#30467 = ORIENTED_EDGE ( 'NONE', *, *, #173041, .T. ) ;
#30468 = DIRECTION ( 'NONE',  ( 1.000000000000000000, 0.000000000000000000, 0.000000000000000000 ) ) ;
#30469 = ORIENTED_EDGE ( 'NONE', *, *, #101630, .F. ) ;
#30470 = DIRECTION ( 'NONE',  ( -1.000000000000000000, 0.000000000000000000, 0.000000000000000000 ) ) ;
#30471 = DIRECTION ( 'NONE',  ( 1.000000000000000000, 0.000000000000000000, -0.000000000000000000 ) ) ;
#30472 = AXIS2_PLACEMENT_3D ( 'NONE', #237780, #138640, #218187 ) ;
#30473 = EDGE_CURVE ( 'NONE', #224622, #146300, #113247, .T. ) ;
#30474 = AXIS2_PLACEMENT_3D ( 'NONE', #96663, #249372, #51127 ) ;
#30475 = FACE_OUTER_BOUND ( 'NONE', #233291, .T. ) ;
#30476 = ORIENTED_EDGE ( 'NONE', *, *, #49144, .F. ) ;
#30477 = VECTOR ( 'NONE', #80752, 1000.000000000000114 ) ;
#30478 = CARTESIAN_POINT ( 'NONE',  ( -16.87401514999235630, 9.949999999999983302, -12.71998200746783780 ) ) ;
#30480 = CIRCLE ( 'NONE', #255253, 0.1000000000000028644 ) ;
#30479 = CARTESIAN_POINT ( 'NONE',  ( -23.25000000000000000, 11.75000000001115552, -200.9999999999999432 ) ) ;
#30481 = FACE_OUTER_BOUND ( 'NONE', #91563, .T. ) ;
#30482 = AXIS2_PLACEMENT_3D ( 'NONE', #3014, #141266, #82537 ) ;
#30483 = AXIS2_PLACEMENT_3D ( 'NONE', #79357, #3678, #162780 ) ;
#30484 = CARTESIAN_POINT ( 'NONE',  ( 21.95218792049437795, 7.015487724139642722, -199.3707517748408122 ) ) ;
#30485 = CARTESIAN_POINT ( 'NONE',  ( -16.77180007708460963, 9.949999999999983302, -20.86438588104518388 ) ) ;
#30486 = CARTESIAN_POINT ( 'NONE',  ( 21.05000000000000071, 64.40000000001145963, -42.95131071479990936 ) ) ;
#30487 = ORIENTED_EDGE ( 'NONE', *, *, #249502, .T. ) ;
#30489 = EDGE_LOOP ( 'NONE', ( #150807, #154247, #252827, #21798 ) ) ;
#30488 = CARTESIAN_POINT ( 'NONE',  ( 20.93302460841142931, 10.31565961587945424, -106.0364194119178620 ) ) ;
#30490 = CIRCLE ( 'NONE', #205235, 12.87499999999999822 ) ;
#30491 = ORIENTED_EDGE ( 'NONE', *, *, #122796, .F. ) ;
#30492 = CARTESIAN_POINT ( 'NONE',  ( -18.50000000000000000, 66.85000000001200249, -115.3731074845243683 ) ) ;
#30493 = VERTEX_POINT ( 'NONE', #49815 ) ;
#30494 = EDGE_CURVE ( 'NONE', #226290, #131204, #231086, .T. ) ;
#30495 = CARTESIAN_POINT ( 'NONE',  ( -16.88560720703333473, 66.04943515626290207, -190.8749955636607183 ) ) ;
#30496 = LINE ( 'NONE', #87852, #230901 ) ;
#30497 = CARTESIAN_POINT ( 'NONE',  ( -22.50000000000094147, 75.90000000001182912, -81.17267829206915053 ) ) ;
#30498 = ORIENTED_EDGE ( 'NONE', *, *, #175367, .T. ) ;
#30499 = CARTESIAN_POINT ( 'NONE',  ( 23.24999999999999289, 69.55000000001179217, -81.87310748452435405 ) ) ;
#30500 = DIRECTION ( 'NONE',  ( -1.000000000000000000, -2.885090398161910739E-16, -6.283419270304611573E-17 ) ) ;
#30502 = DIRECTION ( 'NONE',  ( 1.000000000000000000, 0.000000000000000000, 0.000000000000000000 ) ) ;
#30501 = VECTOR ( 'NONE', #91645, 1000.000000000000114 ) ;
#30503 = ORIENTED_EDGE ( 'NONE', *, *, #143698, .F. ) ;
#30504 = CIRCLE ( 'NONE', #176250, 11.69999999999998863 ) ;
#30506 = ORIENTED_EDGE ( 'NONE', *, *, #234868, .T. ) ;
#30505 = CARTESIAN_POINT ( 'NONE',  ( -16.97683809663752186, 66.15000000001207070, -123.8731074845243683 ) ) ;
#30507 = DIRECTION ( 'NONE',  ( 1.734723475976817507E-14, 0.000000000000000000, -1.000000000000000000 ) ) ;
#30509 = EDGE_CURVE ( 'NONE', #235211, #182596, #6189, .T. ) ;
#30508 = FACE_OUTER_BOUND ( 'NONE', #227736, .T. ) ;
#30510 = AXIS2_PLACEMENT_3D ( 'NONE', #157961, #100474, #237449 ) ;
#30511 = CIRCLE ( 'NONE', #176256, 0.5000000000000004441 ) ;
#30512 = ORIENTED_EDGE ( 'NONE', *, *, #228926, .T. ) ;
#30513 = CIRCLE ( 'NONE', #5515, 0.09999999999999939493 ) ;
#30514 = VECTOR ( 'NONE', #71622, 1000.000000000000000 ) ;
#30515 = CARTESIAN_POINT ( 'NONE',  ( -17.01473183483379970, 9.950000000011140600, -87.75000000000005684 ) ) ;
#30516 = CARTESIAN_POINT ( 'NONE',  ( -12.93407622233968901, 66.58221053305987880, -121.1657229405475391 ) ) ;
#30517 = AXIS2_PLACEMENT_3D ( 'NONE', #149090, #169966, #129512 ) ;
#30518 = CARTESIAN_POINT ( 'NONE',  ( 18.59999999999999076, 11.75000000001115907, -192.3499999999999659 ) ) ;
#30519 = ORIENTED_EDGE ( 'NONE', *, *, #76646, .F. ) ;
#30520 = LINE ( 'NONE', #110028, #37793 ) ;
#30521 = CARTESIAN_POINT ( 'NONE',  ( -20.94999999999999929, 70.10000000001177511, -79.74220724918072278 ) ) ;
#30522 = DIRECTION ( 'NONE',  ( 0.000000000000000000, 0.8814952561688437216, -0.4721928772777334582 ) ) ;
#30523 = ORIENTED_EDGE ( 'NONE', *, *, #252746, .F. ) ;
#30524 = CIRCLE ( 'NONE', #205452, 0.1000000000000028644 ) ;
#30525 = AXIS2_PLACEMENT_3D ( 'NONE', #65792, #142742, #82745 ) ;
#30526 = CIRCLE ( 'NONE', #226105, 11.65000000000000036 ) ;
#30527 = CIRCLE ( 'NONE', #242696, 0.1000000000000002554 ) ;
#30528 = VERTEX_POINT ( 'NONE', #32869 ) ;
#30529 = CARTESIAN_POINT ( 'NONE',  ( 21.13461538461538680, 65.38541703798705385, -191.1731074845244223 ) ) ;
#30530 = EDGE_CURVE ( 'NONE', #33482, #44736, #43802, .T. ) ;
#30531 = EDGE_CURVE ( 'NONE', #20260, #64097, #118656, .T. ) ;
#30532 = ORIENTED_EDGE ( 'NONE', *, *, #194300, .T. ) ;
#30533 = DIRECTION ( 'NONE',  ( 1.000000000000000000, 0.000000000000000000, 0.000000000000000000 ) ) ;
#30534 = DIRECTION ( 'NONE',  ( 0.000000000000000000, 0.000000000000000000, -1.000000000000000000 ) ) ;
#30536 = ORIENTED_EDGE ( 'NONE', *, *, #127293, .F. ) ;
#30535 = CARTESIAN_POINT ( 'NONE',  ( 15.74999999999999645, 26.30888228346803714, -233.3999513616626587 ) ) ;
#30537 = LINE ( 'NONE', #245712, #74297 ) ;
#30538 = LINE ( 'NONE', #170076, #178232 ) ;
#30540 = ADVANCED_FACE ( 'NONE', ( #189337 ), #111073, .T. ) ;
#30539 = DIRECTION ( 'NONE',  ( 1.000000000000000000, 0.000000000000000000, 0.000000000000000000 ) ) ;
#30542 = ADVANCED_FACE ( 'NONE', ( #112373 ), #150221, .T. ) ;
#30541 = SPHERICAL_SURFACE ( 'NONE', #8920, 0.1000000000000000056 ) ;
#30543 = CARTESIAN_POINT ( 'NONE',  ( 18.49999999999999645, 77.16412189325305349, -95.10825939895268277 ) ) ;
#30544 = DIRECTION ( 'NONE',  ( 0.000000000000000000, 0.000000000000000000, 1.000000000000000000 ) ) ;
#30545 = CARTESIAN_POINT ( 'NONE',  ( 21.07971444708685738, 6.329792081637702239, -66.91217656368215216 ) ) ;
#30547 = ORIENTED_EDGE ( 'NONE', *, *, #64373, .T. ) ;
#30546 = DIRECTION ( 'NONE',  ( 0.000000000000000000, 0.000000000000000000, 1.000000000000000000 ) ) ;
#30548 = ADVANCED_FACE ( 'NONE', ( #191931 ), #210234, .F. ) ;
#30549 = EDGE_CURVE ( 'NONE', #157514, #69302, #190636, .T. ) ;
#30551 = ADVANCED_FACE ( 'NONE', ( #231048 ), #48529, .F. ) ;
#30550 = ADVANCED_FACE ( 'NONE', ( #12000 ), #206124, .T. ) ;
#30552 = DIRECTION ( 'NONE',  ( 1.000000000000000000, 0.000000000000000000, 0.000000000000000000 ) ) ;
#30553 = AXIS2_PLACEMENT_3D ( 'NONE', #69621, #228699, #55141 ) ;
#30554 = CARTESIAN_POINT ( 'NONE',  ( -23.25000000000000000, 26.42645436459467589, -241.9028176822583589 ) ) ;
#30555 = DIRECTION ( 'NONE',  ( 1.000000000000000000, 0.000000000000000000, 0.000000000000000000 ) ) ;
#30556 = DIRECTION ( 'NONE',  ( 0.000000000000000000, 0.000000000000000000, -1.000000000000000000 ) ) ;
#30557 = ORIENTED_EDGE ( 'NONE', *, *, #155034, .F. ) ;
#30558 = CARTESIAN_POINT ( 'NONE',  ( -22.59999999999999787, 64.25043287652226809, -69.62396585362311896 ) ) ;
#30559 = EDGE_CURVE ( 'NONE', #223911, #23864, #102035, .T. ) ;
#30560 = DIRECTION ( 'NONE',  ( 1.000000000000000000, 0.000000000000000000, 0.000000000000000000 ) ) ;
#30561 = DIRECTION ( 'NONE',  ( 0.000000000000000000, -0.9915357197604972583, 0.1298341882519109536 ) ) ;
#30562 = ORIENTED_EDGE ( 'NONE', *, *, #249441, .F. ) ;
#30563 = EDGE_CURVE ( 'NONE', #252182, #215011, #188054, .T. ) ;
#30565 = EDGE_CURVE ( 'NONE', #199454, #101237, #222661, .T. ) ;
#30564 = CIRCLE ( 'NONE', #180959, 0.1000000000000091788 ) ;
#30566 = CYLINDRICAL_SURFACE ( 'NONE', #10357, 7.900000000000007461 ) ;
#30567 = VECTOR ( 'NONE', #23757, 1000.000000000000000 ) ;
#30568 = DIRECTION ( 'NONE',  ( 0.000000000000000000, 0.000000000000000000, -1.000000000000000000 ) ) ;
#30569 = EDGE_CURVE ( 'NONE', #102134, #32374, #74565, .T. ) ;
#30570 = VERTEX_POINT ( 'NONE', #58777 ) ;
#30571 = CARTESIAN_POINT ( 'NONE',  ( -21.04999999999999716, 6.344723404101464403, -66.98528214347604148 ) ) ;
#30572 = ORIENTED_EDGE ( 'NONE', *, *, #221556, .F. ) ;
#30573 = CARTESIAN_POINT ( 'NONE',  ( -23.39999999999994529, 83.90000000001120384, -34.77310748452479316 ) ) ;
#30575 = ORIENTED_EDGE ( 'NONE', *, *, #218753, .F. ) ;
#30574 = CARTESIAN_POINT ( 'NONE',  ( -23.15000000000000213, 1.115600667400684642E-11, -100.5000000000000426 ) ) ;
#30576 = EDGE_CURVE ( 'NONE', #127119, #163489, #146926, .T. ) ;
#30577 = DIRECTION ( 'NONE',  ( -1.073024830501117725E-15, -6.982962677686266711E-15, 1.000000000000000000 ) ) ;
#30578 = ORIENTED_EDGE ( 'NONE', *, *, #129878, .F. ) ;
#30579 = DIRECTION ( 'NONE',  ( 0.000000000000000000, 0.000000000000000000, 1.000000000000000000 ) ) ;
#30581 = ORIENTED_EDGE ( 'NONE', *, *, #123043, .F. ) ;
#30580 = EDGE_CURVE ( 'NONE', #253024, #73463, #214483, .T. ) ;
#30582 = ORIENTED_EDGE ( 'NONE', *, *, #89279, .T. ) ;
#30584 = CARTESIAN_POINT ( 'NONE',  ( -20.94999999999999929, 5.021051876504146399E-16, -37.60000000000000142 ) ) ;
#30583 = CIRCLE ( 'NONE', #63883, 0.09999999999999939493 ) ;
#30586 = EDGE_LOOP ( 'NONE', ( #27286, #254296, #181780, #149024, #36427 ) ) ;
#30585 = DIRECTION ( 'NONE',  ( 0.000000000000000000, -1.000000000000000000, 2.771150684185008344E-14 ) ) ;
#30587 = CARTESIAN_POINT ( 'NONE',  ( 20.90851465518106167, 65.67467670974397720, -63.95317318268842399 ) ) ;
#30588 = EDGE_LOOP ( 'NONE', ( #82019, #168822, #124367, #46540, #144795 ) ) ;
#30589 = AXIS2_PLACEMENT_3D ( 'NONE', #176782, #35983, #94647 ) ;
#30590 = VECTOR ( 'NONE', #216251, 1000.000000000000000 ) ;
#30591 = ORIENTED_EDGE ( 'NONE', *, *, #197103, .T. ) ;
#30592 = SPHERICAL_SURFACE ( 'NONE', #20184, 0.1000000000000000056 ) ;
#30593 = CARTESIAN_POINT ( 'NONE',  ( -21.05000000000000071, 0.2561057921033771945, -66.96510355832775474 ) ) ;
#30594 = DIRECTION ( 'NONE',  ( 0.000000000000000000, -6.982962677686266711E-15, 1.000000000000000000 ) ) ;
#30595 = ORIENTED_EDGE ( 'NONE', *, *, #40751, .T. ) ;
#30596 = DIRECTION ( 'NONE',  ( -1.000000000000000000, -0.000000000000000000, 0.000000000000000000 ) ) ;
#30597 = CARTESIAN_POINT ( 'NONE',  ( -20.64999999999999858, 74.00000000001259082, -190.7984855617622770 ) ) ;
#30598 = DIRECTION ( 'NONE',  ( 0.000000000000000000, 0.000000000000000000, 1.000000000000000000 ) ) ;
#30599 = CIRCLE ( 'NONE', #230507, 11.80000000000000426 ) ;
#30600 = ORIENTED_EDGE ( 'NONE', *, *, #85777, .T. ) ;
#30601 = AXIS2_PLACEMENT_3D ( 'NONE', #122975, #21324, #39613 ) ;
#30602 = DIRECTION ( 'NONE',  ( 0.000000000000000000, -0.8660254037844384856, 0.5000000000000002220 ) ) ;
#30603 = CARTESIAN_POINT ( 'NONE',  ( 21.10000000000000142, 5.021051876504148371E-16, 4.100000000000000533 ) ) ;
#30604 = DIRECTION ( 'NONE',  ( 0.000000000000000000, -0.000000000000000000, -1.000000000000000000 ) ) ;
#30605 = AXIS2_PLACEMENT_3D ( 'NONE', #176430, #96832, #73487 ) ;
#30606 = CARTESIAN_POINT ( 'NONE',  ( 23.25000000000000000, 69.45000000001259366, -191.1731074845243938 ) ) ;
#30607 = ORIENTED_EDGE ( 'NONE', *, *, #208223, .T. ) ;
#30608 = CYLINDRICAL_SURFACE ( 'NONE', #126254, 0.09999999999999149847 ) ;
#30609 = VERTEX_POINT ( 'NONE', #135760 ) ;
#30610 = CARTESIAN_POINT ( 'NONE',  ( 21.05000000000000071, 7.216982865709976380, -233.7799206001670598 ) ) ;
#30611 = ORIENTED_EDGE ( 'NONE', *, *, #118475, .F. ) ;
#30612 = LINE ( 'NONE', #232664, #34752 ) ;
#30613 = CYLINDRICAL_SURFACE ( 'NONE', #193772, 2.000000000000001776 ) ;
#30615 = ORIENTED_EDGE ( 'NONE', *, *, #6834, .F. ) ;
#30614 = VECTOR ( 'NONE', #28132, 1000.000000000000227 ) ;
#30616 = ORIENTED_EDGE ( 'NONE', *, *, #248342, .T. ) ;
#30618 = VERTEX_POINT ( 'NONE', #101 ) ;
#30617 = DIRECTION ( 'NONE',  ( 0.7071067811865546782, -0.6824534298470523730, 0.1850873201761376874 ) ) ;
#30619 = DIRECTION ( 'NONE',  ( 0.000000000000000000, -0.1350103645451904977, -0.9908441862701596881 ) ) ;
#30620 = ORIENTED_EDGE ( 'NONE', *, *, #137104, .F. ) ;
#30621 = DIRECTION ( 'NONE',  ( 1.000000000000000000, 7.304098846218134667E-16, 5.100424963727256530E-30 ) ) ;
#30622 = AXIS2_PLACEMENT_3D ( 'NONE', #47089, #26277, #88783 ) ;
#30623 = CIRCLE ( 'NONE', #18129, 0.09999999999998898659 ) ;
#30624 = VECTOR ( 'NONE', #47771, 1000.000000000000000 ) ;
#30625 = CARTESIAN_POINT ( 'NONE',  ( -18.51697539158857353, 65.68434038414338261, -63.98668807260654745 ) ) ;
#30626 = AXIS2_PLACEMENT_3D ( 'NONE', #181802, #4433, #43580 ) ;
#30627 = ORIENTED_EDGE ( 'NONE', *, *, #240057, .F. ) ;
#30628 = EDGE_CURVE ( 'NONE', #207108, #46223, #78353, .T. ) ;
#30629 = CARTESIAN_POINT ( 'NONE',  ( 21.05000000000000071, 1.115600667400684642E-11, -200.9999999999999432 ) ) ;
#30630 = EDGE_CURVE ( 'NONE', #192232, #202799, #178794, .T. ) ;
#30631 = ORIENTED_EDGE ( 'NONE', *, *, #79395, .F. ) ;
#30632 = DIRECTION ( 'NONE',  ( 1.000000000000000000, 0.000000000000000000, 0.000000000000000000 ) ) ;
#30633 = EDGE_CURVE ( 'NONE', #230995, #77584, #218561, .T. ) ;
#30634 = CARTESIAN_POINT ( 'NONE',  ( -16.81744102076749314, 22.97806745954242302, -230.9350634111226270 ) ) ;
#30635 = EDGE_CURVE ( 'NONE', #159106, #163761, #106141, .T. ) ;
#30636 = CYLINDRICAL_SURFACE ( 'NONE', #180128, 0.09999999999999939493 ) ;
#30638 = ORIENTED_EDGE ( 'NONE', *, *, #167170, .T. ) ;
#30637 = CARTESIAN_POINT ( 'NONE',  ( -16.87683809663752399, 9.850000000011144508, -46.90236401819630885 ) ) ;
#30639 = DIRECTION ( 'NONE',  ( 0.000000000000000000, 0.9126074666063660468, 0.4088369013363524762 ) ) ;
#30640 = CARTESIAN_POINT ( 'NONE',  ( 21.05000000000000071, 67.22371710471912820, -61.03510676294002479 ) ) ;
#30641 = CARTESIAN_POINT ( 'NONE',  ( -21.14999999999999858, -0.09999999999999939493, 6.540656951701240729 ) ) ;
#30642 = VECTOR ( 'NONE', #83658, 1000.000000000000000 ) ;
#30644 = CARTESIAN_POINT ( 'NONE',  ( 18.39999999999999858, -9.499999999988842703, -107.5320693966997112 ) ) ;
#30643 = DIRECTION ( 'NONE',  ( 0.000000000000000000, -0.9770955615653316162, -0.2128009952263604232 ) ) ;
#30645 = CARTESIAN_POINT ( 'NONE',  ( 21.05000000000000071, 10.47338541492406172, -108.0786544642485580 ) ) ;
#30646 = FACE_OUTER_BOUND ( 'NONE', #252076, .T. ) ;
#30647 = VECTOR ( 'NONE', #199717, 1000.000000000000000 ) ;
#30648 = CARTESIAN_POINT ( 'NONE',  ( -21.52071067811865746, 68.22071067813014622, -48.37310748452437537 ) ) ;
#30649 = CARTESIAN_POINT ( 'NONE',  ( -21.05000000000000426, 75.98514436511895553, -176.3674665265674832 ) ) ;
#30650 = VERTEX_POINT ( 'NONE', #117498 ) ;
#30651 = ADVANCED_FACE ( 'NONE', ( #77077 ), #177507, .F. ) ;
#30652 = AXIS2_PLACEMENT_3D ( 'NONE', #190579, #9340, #229688 ) ;
#30653 = ORIENTED_EDGE ( 'NONE', *, *, #87062, .F. ) ;
#30654 = AXIS2_PLACEMENT_3D ( 'NONE', #197072, #121437, #19753 ) ;
#30655 = ORIENTED_EDGE ( 'NONE', *, *, #212941, .T. ) ;
#30656 = CARTESIAN_POINT ( 'NONE',  ( 21.00000000000000000, 66.25000000001199396, -115.3731074845243683 ) ) ;
#30657 = AXIS2_PLACEMENT_3D ( 'NONE', #19207, #236976, #139114 ) ;
#30658 = CYLINDRICAL_SURFACE ( 'NONE', #65310, 0.09999999999999939493 ) ;
#30659 = VERTEX_POINT ( 'NONE', #157954 ) ;
#30660 = AXIS2_PLACEMENT_3D ( 'NONE', #154413, #55234, #213051 ) ;
#30662 = VECTOR ( 'NONE', #46004, 1000.000000000000000 ) ;
#30661 = FILL_AREA_STYLE_COLOUR ( '', #135708 ) ;
#30663 = CARTESIAN_POINT ( 'NONE',  ( -23.15000000000000213, 1.910280373831774847, -20.86863214480106166 ) ) ;
#30664 = AXIS2_PLACEMENT_3D ( 'NONE', #78055, #160200, #100163 ) ;
#30665 = CARTESIAN_POINT ( 'NONE',  ( -20.94999999999999929, 11.60000000001115161, -73.92820323027559937 ) ) ;
#30666 = CIRCLE ( 'NONE', #84771, 0.09999999999999939493 ) ;
#30667 = PRODUCT ( 'Injection Molded Chain Links 9', 'Injection Molded Chain Links 9', '', ( #170944 ) ) ;
#30668 = EDGE_CURVE ( 'NONE', #62507, #138284, #36706, .T. ) ;
#30669 = DIRECTION ( 'NONE',  ( 0.000000000000000000, -7.116814260417668513E-15, 1.000000000000000000 ) ) ;
#30670 = ORIENTED_EDGE ( 'NONE', *, *, #189260, .T. ) ;
#30671 = ORIENTED_EDGE ( 'NONE', *, *, #115796, .F. ) ;
#30672 = CIRCLE ( 'NONE', #63970, 0.5000000000000005551 ) ;
#30673 = CARTESIAN_POINT ( 'NONE',  ( 18.59999999999999076, 14.49677803128281184, -219.5908849880255502 ) ) ;
#30674 = FACE_OUTER_BOUND ( 'NONE', #46260, .T. ) ;
#30675 = ORIENTED_EDGE ( 'NONE', *, *, #208631, .F. ) ;
#30676 = CARTESIAN_POINT ( 'NONE',  ( 20.94999999999999574, 7.128833340093095217, -233.7327013124392749 ) ) ;
#30678 = ORIENTED_EDGE ( 'NONE', *, *, #231145, .F. ) ;
#30677 = CARTESIAN_POINT ( 'NONE',  ( -23.15000000000000213, -3.642792592896924919, -226.5668142904084164 ) ) ;
#30679 = CYLINDRICAL_SURFACE ( 'NONE', #33473, 0.1000000000000013933 ) ;
#30680 = FACE_OUTER_BOUND ( 'NONE', #45109, .T. ) ;
#30681 = AXIS2_PLACEMENT_3D ( 'NONE', #159044, #24671, #201995 ) ;
#30682 = EDGE_CURVE ( 'NONE', #108130, #146336, #137058, .T. ) ;
#30684 = ORIENTED_EDGE ( 'NONE', *, *, #33724, .F. ) ;
#30683 = DIRECTION ( 'NONE',  ( -7.304098846217948299E-16, -1.000000000000000000, 0.000000000000000000 ) ) ;
#30685 = CARTESIAN_POINT ( 'NONE',  ( 22.50000000000000000, 64.35042919246734527, -136.6231074845243825 ) ) ;
#30686 = CARTESIAN_POINT ( 'NONE',  ( 20.94999999999999929, 64.35000000001218723, -143.3069731475025037 ) ) ;
#30687 = CARTESIAN_POINT ( 'NONE',  ( -18.59999999999999787, 9.350000000000001421, -21.35000000000000142 ) ) ;
#30688 = EDGE_CURVE ( 'NONE', #149398, #26287, #114931, .T. ) ;
#30689 = DIRECTION ( 'NONE',  ( 0.000000000000000000, 0.000000000000000000, -1.000000000000000000 ) ) ;
#30691 = DIRECTION ( 'NONE',  ( 0.000000000000000000, 0.4999999999999088507, 0.8660254037844913322 ) ) ;
#30690 = CARTESIAN_POINT ( 'NONE',  ( -20.94999999999999929, 11.60000000001115161, -174.4282032302755283 ) ) ;
#30692 = DIRECTION ( 'NONE',  ( -1.000000000000000000, 0.000000000000000000, 0.000000000000000000 ) ) ;
#30693 = CARTESIAN_POINT ( 'NONE',  ( -18.49372193242259144, 85.44248452337019728, -163.2583262244892808 ) ) ;
#30694 = DIRECTION ( 'NONE',  ( 0.000000000000000000, -0.9651348961777157509, 0.2617529984165031243 ) ) ;
#30695 = CARTESIAN_POINT ( 'NONE',  ( 22.39999999999999503, 11.75000000001115552, -100.5000000000000284 ) ) ;
#30696 = VECTOR ( 'NONE', #17746, 1000.000000000000000 ) ;
#30698 = ORIENTED_EDGE ( 'NONE', *, *, #220432, .T. ) ;
#30697 = CIRCLE ( 'NONE', #22321, 11.80000000000000249 ) ;
#30699 = EDGE_CURVE ( 'NONE', #58722, #11117, #122924, .T. ) ;
#30700 = FACE_OUTER_BOUND ( 'NONE', #232365, .T. ) ;
#30701 = CIRCLE ( 'NONE', #22323, 0.09999999999999939493 ) ;
#30702 = ORIENTED_EDGE ( 'NONE', *, *, #80194, .F. ) ;
#30703 = DIRECTION ( 'NONE',  ( 1.000000000000000000, 0.000000000000000000, 0.000000000000000000 ) ) ;
#30704 = EDGE_LOOP ( 'NONE', ( #65613, #54999, #195544, #31991 ) ) ;
#30705 = DIRECTION ( 'NONE',  ( 0.000000000000000000, -6.982962677686266711E-15, 1.000000000000000000 ) ) ;
#30706 = DIRECTION ( 'NONE',  ( 0.000000000000000000, 0.2617529984165030132, 0.9651348961777157509 ) ) ;
#30707 = EDGE_CURVE ( 'NONE', #154129, #29761, #131100, .T. ) ;
#30708 = EDGE_CURVE ( 'NONE', #255159, #226146, #34146, .T. ) ;
#30709 = ORIENTED_EDGE ( 'NONE', *, *, #56372, .T. ) ;
#30710 = EDGE_CURVE ( 'NONE', #143115, #16521, #93688, .T. ) ;
#30711 = CARTESIAN_POINT ( 'NONE',  ( -18.59999999999999787, 66.75000000001179501, -81.77310748452437394 ) ) ;
#30712 = CIRCLE ( 'NONE', #80147, 0.1999999999999987899 ) ;
#30713 = AXIS2_PLACEMENT_3D ( 'NONE', #200174, #183187, #123201 ) ;
#30714 = ORIENTED_EDGE ( 'NONE', *, *, #64305, .F. ) ;
#30715 = AXIS2_PLACEMENT_3D ( 'NONE', #135077, #157261, #137644 ) ;
#30717 = ORIENTED_EDGE ( 'NONE', *, *, #234814, .F. ) ;
#30716 = CIRCLE ( 'NONE', #93044, 0.09999999999999939493 ) ;
#30718 = ORIENTED_EDGE ( 'NONE', *, *, #145545, .F. ) ;
#30719 = CARTESIAN_POINT ( 'NONE',  ( 22.19999999999999929, -11.65000000000000036, 32.89999999999999858 ) ) ;
#30720 = LINE ( 'NONE', #35842, #228452 ) ;
#30721 = CARTESIAN_POINT ( 'NONE',  ( -18.40000000000000213, 56.47972699439914379, -234.4806356575134885 ) ) ;
#30722 = CARTESIAN_POINT ( 'NONE',  ( 12.30626653967340900, 26.71301589465422310, -233.6087318245599249 ) ) ;
#30723 = FACE_OUTER_BOUND ( 'NONE', #23041, .T. ) ;
#30724 = ADVANCED_FACE ( 'NONE', ( #256950 ), #17134, .T. ) ;
#30726 = DIRECTION ( 'NONE',  ( 1.000000000000000000, 0.000000000000000000, 0.000000000000000000 ) ) ;
#30725 = DIRECTION ( 'NONE',  ( -1.000000000000000000, 0.000000000000000000, 0.000000000000000000 ) ) ;
#30727 = CARTESIAN_POINT ( 'NONE',  ( 18.49999999999999645, 10.25000000263022670, -58.18717194963260653 ) ) ;
#30729 = VERTEX_POINT ( 'NONE', #198307 ) ;
#30728 = DIRECTION ( 'NONE',  ( 1.000000000000000000, -0.000000000000000000, -0.000000000000000000 ) ) ;
#30731 = DIRECTION ( 'NONE',  ( 0.000000000000000000, 6.982962677686266711E-15, -1.000000000000000000 ) ) ;
#30730 = CARTESIAN_POINT ( 'NONE',  ( 20.22894356738450838, 9.278498222849625776, -75.26852290624343311 ) ) ;
#30732 = CARTESIAN_POINT ( 'NONE',  ( -20.15000000000000568, 9.291421356248463326, -54.75000000000000000 ) ) ;
#30733 = ORIENTED_EDGE ( 'NONE', *, *, #171763, .F. ) ;
#30734 = DIRECTION ( 'NONE',  ( 0.000000000000000000, 0.9126074666063660468, 0.4088369013363524762 ) ) ;
#30735 = DIRECTION ( 'NONE',  ( 2.557131231893037478E-16, -0.1022405907414166287, -0.9947597004326451664 ) ) ;
#30736 = DIRECTION ( 'NONE',  ( 0.000000000000000000, 0.000000000000000000, -1.000000000000000000 ) ) ;
#30737 = ORIENTED_EDGE ( 'NONE', *, *, #48807, .T. ) ;
#30738 = CARTESIAN_POINT ( 'NONE',  ( -16.77683809663752257, 60.94702803318471496, -221.0293550571836647 ) ) ;
#30739 = CARTESIAN_POINT ( 'NONE',  ( -20.00857864376270001, 9.150000000011157653, -45.75000000000000000 ) ) ;
#30740 = CARTESIAN_POINT ( 'NONE',  ( 13.88302573338718560, 66.54258905524443435, -88.02302351073434750 ) ) ;
#30741 = ORIENTED_EDGE ( 'NONE', *, *, #237990, .F. ) ;
#30742 = EDGE_LOOP ( 'NONE', ( #190759, #113482, #77033, #228735 ) ) ;
#30743 = VECTOR ( 'NONE', #9323, 1000.000000000000000 ) ;
#30744 = LINE ( 'NONE', #188503, #190893 ) ;
#30745 = CARTESIAN_POINT ( 'NONE',  ( -20.85000000000000142, -1.149570369564537842, -208.8159124845019221 ) ) ;
#30746 = DIRECTION ( 'NONE',  ( -0.000000000000000000, 0.8660254037844502539, 0.4999999999999799050 ) ) ;
#30747 = CARTESIAN_POINT ( 'NONE',  ( 20.90000000000000213, 11.50977166988710820, -1.786320531569725478 ) ) ;
#30748 = VERTEX_POINT ( 'NONE', #19692 ) ;
#30749 = CARTESIAN_POINT ( 'NONE',  ( 23.14999999999999858, 70.50000000001260503, -191.1178414656113205 ) ) ;
#30750 = CARTESIAN_POINT ( 'NONE',  ( -23.25000000000000000, 42.98415524044399660, -233.9519173640447889 ) ) ;
#30751 = DIRECTION ( 'NONE',  ( -1.000000000000000000, 0.000000000000000000, 0.000000000000000000 ) ) ;
#30752 = CYLINDRICAL_SURFACE ( 'NONE', #236677, 11.80000000000000426 ) ;
#30753 = VECTOR ( 'NONE', #72241, 1000.000000000000000 ) ;
#30754 = EDGE_CURVE ( 'NONE', #102030, #124122, #127011, .T. ) ;
#30756 = ORIENTED_EDGE ( 'NONE', *, *, #22420, .T. ) ;
#30755 = CIRCLE ( 'NONE', #13990, 0.09999999999998898659 ) ;
#30757 = FACE_OUTER_BOUND ( 'NONE', #45458, .T. ) ;
#30758 = CIRCLE ( 'NONE', #243111, 0.09999999999999971412 ) ;
#30760 = ORIENTED_EDGE ( 'NONE', *, *, #78503, .T. ) ;
#30759 = FACE_OUTER_BOUND ( 'NONE', #205271, .T. ) ;
#30761 = FACE_OUTER_BOUND ( 'NONE', #111176, .T. ) ;
#30762 = CARTESIAN_POINT ( 'NONE',  ( -18.40000000000000213, 11.48667500176882328, -76.25000000000004263 ) ) ;
#30763 = EDGE_CURVE ( 'NONE', #180736, #44180, #38325, .T. ) ;
#30764 = CARTESIAN_POINT ( 'NONE',  ( -21.05000000000000071, 76.00000000001159606, -61.62310748452431852 ) ) ;
#30765 = EDGE_LOOP ( 'NONE', ( #69633, #158889, #161773, #184413 ) ) ;
#30766 = CYLINDRICAL_SURFACE ( 'NONE', #67283, 0.1000000000000106498 ) ;
#30767 = LINE ( 'NONE', #12482, #184234 ) ;
#30768 = CYLINDRICAL_SURFACE ( 'NONE', #2946, 0.1000000000000028644 ) ;
#30769 = ORIENTED_EDGE ( 'NONE', *, *, #65055, .T. ) ;
#30770 = CARTESIAN_POINT ( 'NONE',  ( 21.05000000000005400, 74.83745509109094485, -44.02310748452479316 ) ) ;
#30771 = LINE ( 'NONE', #29499, #248125 ) ;
#30773 = ADVANCED_FACE ( 'NONE', ( #139597 ), #218748, .F. ) ;
#30772 = CARTESIAN_POINT ( 'NONE',  ( -21.05000000000000071, 77.85102823015292017, -124.8691942151017855 ) ) ;
#30774 = EDGE_CURVE ( 'NONE', #239471, #253555, #243712, .T. ) ;
#30775 = DIRECTION ( 'NONE',  ( 0.000000000000000000, -0.2617529984165152257, -0.9651348961777124202 ) ) ;
#30776 = AXIS2_PLACEMENT_3D ( 'NONE', #163598, #144011, #220979 ) ;
#30777 = DIRECTION ( 'NONE',  ( 0.000000000000000000, 0.000000000000000000, -1.000000000000000000 ) ) ;
#30778 = AXIS2_PLACEMENT_3D ( 'NONE', #35386, #69350, #232287 ) ;
#30779 = CARTESIAN_POINT ( 'NONE',  ( 12.25000000000000000, 9.350000000011140955, -184.2499999999999716 ) ) ;
#30780 = ORIENTED_EDGE ( 'NONE', *, *, #18135, .T. ) ;
#30781 = ORIENTED_EDGE ( 'NONE', *, *, #212501, .T. ) ;
#30783 = LINE ( 'NONE', #17308, #238380 ) ;
#30782 = CIRCLE ( 'NONE', #201430, 0.4999999999999892308 ) ;
#30784 = DIRECTION ( 'NONE',  ( 1.000000000000000000, -3.151514657663852580E-16, 8.547182517843351137E-17 ) ) ;
#30785 = DIRECTION ( 'NONE',  ( 0.000000000000000000, 1.000000000000000000, 0.000000000000000000 ) ) ;
#30786 = EDGE_CURVE ( 'NONE', #126059, #67538, #81362, .T. ) ;
#30787 = DIRECTION ( 'NONE',  ( -1.000000000000000000, 1.836970198721029934E-16, 1.601412966608202925E-30 ) ) ;
#30788 = AXIS2_PLACEMENT_3D ( 'NONE', #798, #178215, #39994 ) ;
#30789 = VECTOR ( 'NONE', #32892, 1000.000000000000000 ) ;
#30790 = LINE ( 'NONE', #110293, #188106 ) ;
#30791 = CIRCLE ( 'NONE', #84893, 0.09999999999999939493 ) ;
#30792 = DIRECTION ( 'NONE',  ( 0.000000000000000000, 0.9126074666063774821, 0.4088369013363273297 ) ) ;
#30793 = DIRECTION ( 'NONE',  ( 0.000000000000000000, 0.000000000000000000, 1.000000000000000000 ) ) ;
#30794 = EDGE_LOOP ( 'NONE', ( #130918, #202320, #243620, #249465 ) ) ;
#30795 = DIRECTION ( 'NONE',  ( 1.000000000000000000, 0.000000000000000000, 0.000000000000000000 ) ) ;
#30796 = AXIS2_PLACEMENT_3D ( 'NONE', #162198, #244260, #44799 ) ;
#30797 = VERTEX_POINT ( 'NONE', #161781 ) ;
#30798 = ADVANCED_FACE ( 'NONE', ( #222997 ), #189729, .F. ) ;
#30799 = CARTESIAN_POINT ( 'NONE',  ( -18.50000000000000000, -9.399999999988850163, -140.9146583429697159 ) ) ;
#30800 = ADVANCED_FACE ( 'NONE', ( #243851 ), #2268, .T. ) ;
#30801 = CARTESIAN_POINT ( 'NONE',  ( -21.59142135623730852, 10.29829244934489552, -211.3966423728064115 ) ) ;
#30802 = DIRECTION ( 'NONE',  ( 1.000000000000000000, 0.000000000000000000, 0.000000000000000000 ) ) ;
#30804 = VECTOR ( 'NONE', #195740, 1000.000000000000000 ) ;
#30803 = DIRECTION ( 'NONE',  ( 0.000000000000000000, 0.000000000000000000, -1.000000000000000000 ) ) ;
#30805 = CARTESIAN_POINT ( 'NONE',  ( 21.05995757104869526, 22.02226065213599782, -231.7555846603365808 ) ) ;
#30806 = CARTESIAN_POINT ( 'NONE',  ( 18.39999999999999858, 85.68240343348806221, -62.86626410711144786 ) ) ;
#30807 = CIRCLE ( 'NONE', #234799, 11.70000000000001528 ) ;
#30808 = CARTESIAN_POINT ( 'NONE',  ( -20.94999999999999929, -1.360870587180885716, -75.07299792709100927 ) ) ;
#30809 = EDGE_LOOP ( 'NONE', ( #254340, #38309, #144350, #67569 ) ) ;
#30811 = CARTESIAN_POINT ( 'NONE',  ( -16.93262454970420094, 22.93468882618020999, -230.8528127703816040 ) ) ;
#30810 = AXIS2_PLACEMENT_3D ( 'NONE', #237303, #132106, #255517 ) ;
#30812 = CARTESIAN_POINT ( 'NONE',  ( -20.94999999999999929, -1.360870587180885716, -41.57299792709095954 ) ) ;
#30813 = CARTESIAN_POINT ( 'NONE',  ( -17.11825945287482753, 65.95000000001159890, -56.87310748452438958 ) ) ;
#30815 = EDGE_CURVE ( 'NONE', #255081, #138609, #227139, .T. ) ;
#30814 = CYLINDRICAL_SURFACE ( 'NONE', #81091, 0.1000000000000028644 ) ;
#30816 = CARTESIAN_POINT ( 'NONE',  ( -18.50000000000000000, 5.950000000011100632, -144.3057023050348846 ) ) ;
#30817 = ORIENTED_EDGE ( 'NONE', *, *, #66350, .F. ) ;
#30818 = CARTESIAN_POINT ( 'NONE',  ( -16.81095280782811230, 9.950000000011138823, -79.64999999999918145 ) ) ;
#30819 = DIRECTION ( 'NONE',  ( -1.000000000000000000, 2.775557561562908012E-13, 0.000000000000000000 ) ) ;
#30820 = EDGE_LOOP ( 'NONE', ( #190188, #14913, #51772, #27183, #242192 ) ) ;
#30821 = ORIENTED_EDGE ( 'NONE', *, *, #74480, .T. ) ;
#30822 = CARTESIAN_POINT ( 'NONE',  ( -23.15000000000000213, 69.09936979046463534, -247.6075824278584605 ) ) ;
#30823 = CARTESIAN_POINT ( 'NONE',  ( -20.94999999999999929, 33.04479387145709524, -247.6151719044046899 ) ) ;
#30824 = EDGE_CURVE ( 'NONE', #141418, #77408, #185457, .T. ) ;
#30825 = CIRCLE ( 'NONE', #176566, 0.09999999999999520384 ) ;
#30826 = ORIENTED_EDGE ( 'NONE', *, *, #227717, .F. ) ;
#30827 = DIRECTION ( 'NONE',  ( 0.000000000000000000, 0.000000000000000000, -1.000000000000000000 ) ) ;
#30828 = CARTESIAN_POINT ( 'NONE',  ( -23.15000000000000213, 76.00000000001260503, -190.7481074845243256 ) ) ;
#30829 = AXIS2_PLACEMENT_3D ( 'NONE', #94646, #218431, #116785 ) ;
#30831 = ORIENTED_EDGE ( 'NONE', *, *, #53744, .F. ) ;
#30830 = AXIS2_PLACEMENT_3D ( 'NONE', #245043, #70290, #48119 ) ;
#30833 = CARTESIAN_POINT ( 'NONE',  ( 20.94999999999999574, 77.25000000001209344, -128.5231074845242745 ) ) ;
#30832 = AXIS2_PLACEMENT_3D ( 'NONE', #111019, #34089, #70644 ) ;
#30834 = EDGE_CURVE ( 'NONE', #138239, #34950, #150101, .T. ) ;
#30835 = CIRCLE ( 'NONE', #176578, 0.09999999999999997780 ) ;
#30836 = ORIENTED_EDGE ( 'NONE', *, *, #132898, .T. ) ;
#30837 = CARTESIAN_POINT ( 'NONE',  ( 20.97224591636398827, 10.62515341617478271, -79.24992590466362685 ) ) ;
#30838 = CARTESIAN_POINT ( 'NONE',  ( 23.24999999999999645, 0.000000000000000000, -33.50000000000000000 ) ) ;
#30840 = ORIENTED_EDGE ( 'NONE', *, *, #60059, .F. ) ;
#30839 = DIRECTION ( 'NONE',  ( -1.000000000000000000, -0.000000000000000000, 0.000000000000000000 ) ) ;
#30841 = DIRECTION ( 'NONE',  ( 1.000000000000000000, 0.000000000000000000, 0.000000000000000000 ) ) ;
#30843 = CIRCLE ( 'NONE', #189045, 0.09999999999999939493 ) ;
#30842 = DIRECTION ( 'NONE',  ( -0.000000000000000000, 0.8660254037844383745, -0.5000000000000003331 ) ) ;
#30844 = EDGE_CURVE ( 'NONE', #239256, #46494, #6379, .T. ) ;
#30846 = ADVANCED_FACE ( 'NONE', ( #103043 ), #59611, .F. ) ;
#30845 = DIRECTION ( 'NONE',  ( -0.000000000000000000, 0.000000000000000000, -1.000000000000000000 ) ) ;
#30847 = DIRECTION ( 'NONE',  ( -1.000000000000000000, 0.000000000000000000, 0.000000000000000000 ) ) ;
#30848 = CARTESIAN_POINT ( 'NONE',  ( 23.40000000000005187, 87.60324567546805952, -37.87437456276921210 ) ) ;
#30849 = CIRCLE ( 'NONE', #160030, 0.1000000000000028644 ) ;
#30850 = DIRECTION ( 'NONE',  ( 0.000000000000000000, 0.000000000000000000, -1.000000000000000000 ) ) ;
#30851 = DIRECTION ( 'NONE',  ( 1.000000000000000000, 0.000000000000000000, 0.000000000000000000 ) ) ;
#30852 = AXIS2_PLACEMENT_3D ( 'NONE', #25967, #185026, #166785 ) ;
#30854 = EDGE_LOOP ( 'NONE', ( #170981, #63870, #44340, #16307, #147062, #202055, #221544, #75135, #249329, #215671, #210553, #213010, #19394, #155768, #62365, #241898, #120615, #70168, #204558, #238720, #213556, #76588, #50501, #110358, #172926, #109124, #107908 ) ) ;
#30853 = CARTESIAN_POINT ( 'NONE',  ( 21.05000000000000071, 76.00000000001195133, -103.0231074845243171 ) ) ;
#30855 = ORIENTED_EDGE ( 'NONE', *, *, #49569, .T. ) ;
#30857 = CARTESIAN_POINT ( 'NONE',  ( -18.39999999999999858, 58.59921997668411819, -223.8511959880075608 ) ) ;
#30856 = DIRECTION ( 'NONE',  ( 1.000000000000000000, 0.000000000000000000, 0.000000000000000000 ) ) ;
#30858 = CIRCLE ( 'NONE', #122425, 0.1000000000000054040 ) ;
#30860 = VERTEX_POINT ( 'NONE', #117055 ) ;
#30859 = DIRECTION ( 'NONE',  ( -0.000000000000000000, -0.8700118002898321601, 0.4930308989875230030 ) ) ;
#30861 = ORIENTED_EDGE ( 'NONE', *, *, #239238, .T. ) ;
#30862 = CARTESIAN_POINT ( 'NONE',  ( -22.00356870069710524, 0.7342531110970158537, -230.3072997392041259 ) ) ;
#30863 = DIRECTION ( 'NONE',  ( 1.000000000000000000, -0.000000000000000000, 0.000000000000000000 ) ) ;
#30864 = VECTOR ( 'NONE', #199272, 1000.000000000000000 ) ;
#30865 = ADVANCED_FACE ( 'NONE', ( #97454 ), #58332, .T. ) ;
#30866 = EDGE_CURVE ( 'NONE', #231172, #4043, #239569, .T. ) ;
#30867 = DIRECTION ( 'NONE',  ( 0.000000000000000000, 0.8814952561688437216, -0.4721928772777334582 ) ) ;
#30868 = FACE_OUTER_BOUND ( 'NONE', #126654, .T. ) ;
#30869 = FACE_OUTER_BOUND ( 'NONE', #187512, .T. ) ;
#30871 = EDGE_CURVE ( 'NONE', #18809, #134102, #179610, .T. ) ;
#30870 = TOROIDAL_SURFACE ( 'NONE', #251600, 4.149999999999999467, 0.1000000000000000056 ) ;
#30872 = CARTESIAN_POINT ( 'NONE',  ( -21.14999999999999858, 76.00000000001219291, -143.0637644362255401 ) ) ;
#30873 = LINE ( 'NONE', #7412, #93690 ) ;
#30874 = AXIS2_PLACEMENT_3D ( 'NONE', #144127, #145422, #46317 ) ;
#30876 = ORIENTED_EDGE ( 'NONE', *, *, #12814, .T. ) ;
#30875 = EDGE_CURVE ( 'NONE', #39669, #171236, #143747, .T. ) ;
#30877 = ORIENTED_EDGE ( 'NONE', *, *, #160740, .F. ) ;
#30878 = CARTESIAN_POINT ( 'NONE',  ( -21.55000000000000426, 68.25000000001230660, -157.6731074845243938 ) ) ;
#30879 = ORIENTED_EDGE ( 'NONE', *, *, #30025, .F. ) ;
#30880 = EDGE_CURVE ( 'NONE', #237399, #193788, #96184, .T. ) ;
#30881 = DIRECTION ( 'NONE',  ( 0.000000000000000000, -0.8814952561688431665, 0.4721928772777344574 ) ) ;
#30883 = EDGE_CURVE ( 'NONE', #197017, #16283, #18852, .T. ) ;
#30882 = VERTEX_POINT ( 'NONE', #237006 ) ;
#30885 = AXIS2_PLACEMENT_3D ( 'NONE', #254741, #76142, #155724 ) ;
#30884 = CARTESIAN_POINT ( 'NONE',  ( 18.59999999999999076, 65.79142135624930177, -115.1731074845243796 ) ) ;
#30886 = TOROIDAL_SURFACE ( 'NONE', #160058, 0.2000000000000000111, 0.1000000000000000056 ) ;
#30887 = AXIS2_PLACEMENT_3D ( 'NONE', #104813, #244350, #223500 ) ;
#30888 = CARTESIAN_POINT ( 'NONE',  ( 23.40000000000005187, 74.94272479589878344, -8.023107484524793165 ) ) ;
#30889 = EDGE_CURVE ( 'NONE', #43643, #214529, #136593, .T. ) ;
#30890 = CARTESIAN_POINT ( 'NONE',  ( 18.49999999999928946, 65.55993210786621717, -44.75598973563730709 ) ) ;
#30891 = ORIENTED_EDGE ( 'NONE', *, *, #228875, .F. ) ;
#30892 = CARTESIAN_POINT ( 'NONE',  ( 18.49999999999999645, 80.78317333349157536, -192.9003134612048882 ) ) ;
#30893 = ORIENTED_EDGE ( 'NONE', *, *, #209808, .T. ) ;
#30894 = ADVANCED_FACE ( 'NONE', ( #238268 ), #15401, .T. ) ;
#30895 = DIRECTION ( 'NONE',  ( 0.000000000000000000, -1.000000000000000000, -6.982962677686265922E-15 ) ) ;
#30896 = EDGE_CURVE ( 'NONE', #182032, #243821, #35653, .T. ) ;
#30897 = DIRECTION ( 'NONE',  ( 0.000000000000000000, 0.4088369013363281623, -0.9126074666063771490 ) ) ;
#30899 = ORIENTED_EDGE ( 'NONE', *, *, #53608, .F. ) ;
#30898 = ADVANCED_FACE ( 'NONE', ( #94906 ), #140448, .T. ) ;
#30900 = FACE_BOUND ( 'NONE', #4799, .T. ) ;
#30901 = EDGE_LOOP ( 'NONE', ( #11306, #210744, #252912 ) ) ;
#30904 = VERTEX_POINT ( 'NONE', #79188 ) ;
#30903 = CARTESIAN_POINT ( 'NONE',  ( 18.59117750673696179, 46.46967969402478360, -243.0849751855955674 ) ) ;
#30902 = DIRECTION ( 'NONE',  ( 0.000000000000000000, 1.776356839400303713E-15, 1.000000000000000000 ) ) ;
#30905 = AXIS2_PLACEMENT_3D ( 'NONE', #78619, #181604, #102017 ) ;
#30906 = CARTESIAN_POINT ( 'NONE',  ( 18.49999999999999289, 65.79142135624879018, -44.87310748452438958 ) ) ;
#30907 = VECTOR ( 'NONE', #171449, 1000.000000000000227 ) ;
#30908 = ORIENTED_EDGE ( 'NONE', *, *, #187841, .F. ) ;
#30909 = CARTESIAN_POINT ( 'NONE',  ( -23.15000000000000213, 2.000000000011154189, -121.3753780772379258 ) ) ;
#30910 = VERTEX_POINT ( 'NONE', #199155 ) ;
#30911 = CARTESIAN_POINT ( 'NONE',  ( -21.05000000000000071, 43.47002849391839874, -245.0086825852825143 ) ) ;
#30912 = EDGE_LOOP ( 'NONE', ( #97921, #154695, #41431, #238469 ) ) ;
#30913 = ADVANCED_FACE ( 'NONE', ( #75386 ), #31377, .T. ) ;
#30914 = DIRECTION ( 'NONE',  ( 0.000000000000000000, 6.982962677686266711E-15, -1.000000000000000000 ) ) ;
#30915 = DIRECTION ( 'NONE',  ( -1.000000000000000000, 1.836970198721029934E-16, 1.282749433769087582E-30 ) ) ;
#30916 = EDGE_CURVE ( 'NONE', #156660, #48836, #913, .T. ) ;
#30917 = DIRECTION ( 'NONE',  ( -4.801466763864314121E-15, 0.9876013379310922824, 0.1569827930593562515 ) ) ;
#30918 = FACE_OUTER_BOUND ( 'NONE', #202081, .T. ) ;
#30919 = VERTEX_POINT ( 'NONE', #36255 ) ;
#30920 = DIRECTION ( 'NONE',  ( 1.000000000000000000, -0.000000000000000000, -0.000000000000000000 ) ) ;
#30921 = CARTESIAN_POINT ( 'NONE',  ( 21.14999999999999858, -2.576749817950531707, -189.6385361693310756 ) ) ;
#30922 = CARTESIAN_POINT ( 'NONE',  ( 18.51697539158856998, 10.31565961587946312, -139.5364194119178478 ) ) ;
#30923 = ORIENTED_EDGE ( 'NONE', *, *, #72199, .F. ) ;
#30924 = CARTESIAN_POINT ( 'NONE',  ( 20.94999999999999574, 77.16270174995010223, -128.4231074845242802 ) ) ;
#30925 = VERTEX_POINT ( 'NONE', #80447 ) ;
#30926 = CARTESIAN_POINT ( 'NONE',  ( -23.15000000000000213, 76.00000000001190870, -103.0231074845243029 ) ) ;
#30927 = ORIENTED_EDGE ( 'NONE', *, *, #130588, .T. ) ;
#30928 = CIRCLE ( 'NONE', #176662, 12.87500000000000000 ) ;
#30929 = DIRECTION ( 'NONE',  ( 0.000000000000000000, -1.000000000000000000, -6.982962677686266711E-15 ) ) ;
#30930 = DIRECTION ( 'NONE',  ( -0.000000000000000000, 0.4701782451859590206, 0.8825714802517993229 ) ) ;
#30932 = EDGE_LOOP ( 'NONE', ( #258077, #162277, #255382, #144485 ) ) ;
#30931 = CARTESIAN_POINT ( 'NONE',  ( -20.94999999999999929, 0.6656436123793473270, -212.6810495496487476 ) ) ;
#30933 = LINE ( 'NONE', #10048, #175566 ) ;
#30934 = ORIENTED_EDGE ( 'NONE', *, *, #234197, .F. ) ;
#30935 = CARTESIAN_POINT ( 'NONE',  ( -20.85000000000000142, 36.22724532936083364, -235.9903003947922002 ) ) ;
#30936 = CARTESIAN_POINT ( 'NONE',  ( 21.05000000000000071, 67.22371710472015138, -194.9644784893834810 ) ) ;
#30937 = VERTEX_POINT ( 'NONE', #160053 ) ;
#30938 = EDGE_CURVE ( 'NONE', #173445, #244396, #233315, .T. ) ;
#30939 = FACE_OUTER_BOUND ( 'NONE', #212190, .T. ) ;
#30940 = DIRECTION ( 'NONE',  ( 0.000000000000000000, 0.000000000000000000, 1.000000000000000000 ) ) ;
#30941 = VERTEX_POINT ( 'NONE', #156206 ) ;
#30943 = CARTESIAN_POINT ( 'NONE',  ( -20.94999999999999929, 70.10000000001235776, -159.8040077198679683 ) ) ;
#30942 = AXIS2_PLACEMENT_3D ( 'NONE', #195752, #135738, #237424 ) ;
#30944 = EDGE_CURVE ( 'NONE', #207912, #5669, #89758, .T. ) ;
#30945 = CIRCLE ( 'NONE', #160112, 0.1000000000000028644 ) ;
#30946 = ORIENTED_EDGE ( 'NONE', *, *, #227545, .T. ) ;
#30947 = CIRCLE ( 'NONE', #10061, 11.74999999999999645 ) ;
#30948 = CIRCLE ( 'NONE', #64231, 0.09999999999999939493 ) ;
#30949 = LINE ( 'NONE', #32220, #137566 ) ;
#30950 = CARTESIAN_POINT ( 'NONE',  ( -18.42637059832564006, -9.496945461878546269, -73.60907730979984365 ) ) ;
#30953 = ORIENTED_EDGE ( 'NONE', *, *, #203339, .T. ) ;
#30952 = ORIENTED_EDGE ( 'NONE', *, *, #156228, .T. ) ;
#30951 = LINE ( 'NONE', #11358, #97277 ) ;
#30954 = CARTESIAN_POINT ( 'NONE',  ( -23.25000000000000000, 76.00000000001213607, -136.5231074845242745 ) ) ;
#30955 = FACE_OUTER_BOUND ( 'NONE', #52451, .T. ) ;
#30956 = CARTESIAN_POINT ( 'NONE',  ( -16.94132844910801694, 9.992436755180344576, -20.89620175598231455 ) ) ;
#30957 = AXIS2_PLACEMENT_3D ( 'NONE', #28960, #90141, #108448 ) ;
#30959 = CARTESIAN_POINT ( 'NONE',  ( -20.90000000000000213, 6.841561409100513025, 9.675512259591560138 ) ) ;
#30958 = CARTESIAN_POINT ( 'NONE',  ( 22.39999999999999503, 11.75000000001115552, -100.4000000000000483 ) ) ;
#30961 = EDGE_CURVE ( 'NONE', #111477, #23132, #123105, .T. ) ;
#30960 = CARTESIAN_POINT ( 'NONE',  ( -21.55000000000000426, 7.708578643773852157, -54.75000000000000000 ) ) ;
#30962 = DIRECTION ( 'NONE',  ( -1.000000000000000000, 0.000000000000000000, 0.000000000000000000 ) ) ;
#30963 = DIRECTION ( 'NONE',  ( 0.000000000000000000, -7.147358527629759053E-15, 1.000000000000000000 ) ) ;
#30964 = AXIS2_PLACEMENT_3D ( 'NONE', #46434, #45159, #225059 ) ;
#30965 = LINE ( 'NONE', #93456, #30068 ) ;
#30966 = AXIS2_PLACEMENT_3D ( 'NONE', #116207, #73244, #193172 ) ;
#30967 = ORIENTED_EDGE ( 'NONE', *, *, #191753, .T. ) ;
#30968 = ORIENTED_EDGE ( 'NONE', *, *, #211222, .T. ) ;
#30969 = DIRECTION ( 'NONE',  ( -2.827886303505248766E-16, -0.8660254037844377084, -0.5000000000000015543 ) ) ;
#30970 = AXIS2_PLACEMENT_3D ( 'NONE', #10579, #227039, #8013 ) ;
#30972 = ORIENTED_EDGE ( 'NONE', *, *, #2191, .F. ) ;
#30971 = CARTESIAN_POINT ( 'NONE',  ( -23.15000000000000213, -8.999999999988844479, -91.20603087734760095 ) ) ;
#30973 = ORIENTED_EDGE ( 'NONE', *, *, #218311, .T. ) ;
#30974 = CARTESIAN_POINT ( 'NONE',  ( 20.84999999999999432, 7.021664781911246322, -70.83356540189728889 ) ) ;
#30975 = ORIENTED_EDGE ( 'NONE', *, *, #61730, .F. ) ;
#30976 = CARTESIAN_POINT ( 'NONE',  ( 22.40000000000001279, 33.47376623175148325, -242.4412390690852703 ) ) ;
#30977 = VECTOR ( 'NONE', #151629, 1000.000000000000000 ) ;
#30978 = CIRCLE ( 'NONE', #218362, 0.1000000000000028644 ) ;
#30979 = VERTEX_POINT ( 'NONE', #243407 ) ;
#30980 = TOROIDAL_SURFACE ( 'NONE', #222459, 0.2000000000000000111, 0.1000000000000000056 ) ;
#30981 = CARTESIAN_POINT ( 'NONE',  ( 21.14999999999999858, 13.96869538424788715, -210.3925794786331949 ) ) ;
#30982 = DIRECTION ( 'NONE',  ( -1.000000000000000000, -0.000000000000000000, -0.000000000000000000 ) ) ;
#30983 = CIRCLE ( 'NONE', #226554, 1.900000000000012790 ) ;
#30985 = ORIENTED_EDGE ( 'NONE', *, *, #115469, .T. ) ;
#30984 = ORIENTED_EDGE ( 'NONE', *, *, #184685, .T. ) ;
#30986 = VERTEX_POINT ( 'NONE', #141738 ) ;
#30987 = ORIENTED_EDGE ( 'NONE', *, *, #139456, .T. ) ;
#30988 = ORIENTED_EDGE ( 'NONE', *, *, #225438, .F. ) ;
#30990 = CARTESIAN_POINT ( 'NONE',  ( -16.87665923198281348, 14.15900158805613884, -219.2550725561364118 ) ) ;
#30989 = AXIS2_PLACEMENT_3D ( 'NONE', #216234, #217511, #61014 ) ;
#30991 = DIRECTION ( 'NONE',  ( 1.000000000000000000, 0.000000000000000000, 0.000000000000000000 ) ) ;
#30992 = DIRECTION ( 'NONE',  ( 0.000000000000000000, -6.982962677686266711E-15, 1.000000000000000000 ) ) ;
#30994 = EDGE_LOOP ( 'NONE', ( #133895, #71460, #231115, #103685 ) ) ;
#30993 = DIRECTION ( 'NONE',  ( 0.000000000000000000, 0.000000000000000000, -1.000000000000000000 ) ) ;
#30995 = LINE ( 'NONE', #89633, #157330 ) ;
#30997 = ORIENTED_EDGE ( 'NONE', *, *, #132529, .F. ) ;
#30996 = CARTESIAN_POINT ( 'NONE',  ( 21.05000000000000071, 5.000000000011153745, -54.59473398108690390 ) ) ;
#30998 = CARTESIAN_POINT ( 'NONE',  ( 23.24999999999999645, 64.25000000001261924, -190.8731074845244393 ) ) ;
#30999 = ORIENTED_EDGE ( 'NONE', *, *, #84218, .F. ) ;
#31000 = TOROIDAL_SURFACE ( 'NONE', #164258, 11.65000000000000036, 0.1000000000000000056 ) ;
#31001 = CARTESIAN_POINT ( 'NONE',  ( -21.14999999999994174, 64.35000000001120668, -3.023107484524792277 ) ) ;
#31002 = ADVANCED_FACE ( 'NONE', ( #204271 ), #225108, .F. ) ;
#31003 = ORIENTED_EDGE ( 'NONE', *, *, #159207, .T. ) ;
#31004 = VECTOR ( 'NONE', #105126, 1000.000000000000000 ) ;
#31005 = CARTESIAN_POINT ( 'NONE',  ( -21.14999999999999858, 6.540656951712397138, -33.60000000000000142 ) ) ;
#31006 = CARTESIAN_POINT ( 'NONE',  ( -20.54999999999999716, 7.150000000011155876, -146.2500000000000284 ) ) ;
#31007 = ADVANCED_FACE ( 'NONE', ( #219994 ), #25655, .F. ) ;
#31008 = EDGE_LOOP ( 'NONE', ( #91186, #140275, #43018, #17405 ) ) ;
#31010 = CARTESIAN_POINT ( 'NONE',  ( -20.54999999999999716, -8.999999999988844479, -90.60603087734760663 ) ) ;
#31009 = CARTESIAN_POINT ( 'NONE',  ( -22.39999999999999858, 64.35000000001268461, -203.4231074845244507 ) ) ;
#31011 = DIRECTION ( 'NONE',  ( -1.000000000000000000, 0.000000000000000000, 0.000000000000000000 ) ) ;
#31012 = CARTESIAN_POINT ( 'NONE',  ( 20.94999999999999574, 46.54514716347711101, -243.1111603596801842 ) ) ;
#31013 = DIRECTION ( 'NONE',  ( -0.000000000000000000, 0.1350103645451876666, -0.9908441862701600211 ) ) ;
#31014 = ORIENTED_EDGE ( 'NONE', *, *, #146766, .T. ) ;
#31015 = EDGE_LOOP ( 'NONE', ( #186683, #148550, #155008, #251521 ) ) ;
#31016 = ADVANCED_FACE ( 'NONE', ( #205553 ), #43927, .T. ) ;
#31017 = DIRECTION ( 'NONE',  ( 1.000000000000000000, -0.000000000000000000, -0.000000000000000000 ) ) ;
#31018 = VERTEX_POINT ( 'NONE', #105137 ) ;
#31019 = CARTESIAN_POINT ( 'NONE',  ( -20.64999999999999858, 68.56901367119438362, -214.3038979092079046 ) ) ;
#31020 = ORIENTED_EDGE ( 'NONE', *, *, #46408, .F. ) ;
#31021 = CARTESIAN_POINT ( 'NONE',  ( 5.551115123125782702E-14, 67.65000000001118963, -3.023107484524792277 ) ) ;
#31022 = FACE_OUTER_BOUND ( 'NONE', #13964, .T. ) ;
#31023 = ADVANCED_FACE ( 'NONE', ( #85578, #2215, #143006 ), #46477, .F. ) ;
#31024 = DIRECTION ( 'NONE',  ( 1.000000000000000000, 0.000000000000000000, 0.000000000000000000 ) ) ;
#31025 = TOROIDAL_SURFACE ( 'NONE', #197567, 0.2000000000000000111, 0.1000000000000000056 ) ;
#31026 = CIRCLE ( 'NONE', #189220, 0.09999999999999939493 ) ;
#31027 = ORIENTED_EDGE ( 'NONE', *, *, #115834, .T. ) ;
#31028 = EDGE_CURVE ( 'NONE', #228990, #176585, #164614, .T. ) ;
#31029 = CARTESIAN_POINT ( 'NONE',  ( -2.995603634470891112E-16, 81.77808381374873647, -227.1078217596952697 ) ) ;
#31030 = CIRCLE ( 'NONE', #93337, 0.09999999999998898659 ) ;
#31031 = ORIENTED_EDGE ( 'NONE', *, *, #161379, .T. ) ;
#31032 = ORIENTED_EDGE ( 'NONE', *, *, #123051, .T. ) ;
#31033 = ORIENTED_EDGE ( 'NONE', *, *, #175307, .F. ) ;
#31034 = AXIS2_PLACEMENT_3D ( 'NONE', #87277, #228108, #131559 ) ;
#31035 = B_SPLINE_CURVE_WITH_KNOTS ( 'NONE', 3,
 ( #72862, #194080, #169404, #15438, #191522, #49415 ),
 .UNSPECIFIED., .F., .F.,
 ( 4, 2, 4 ),
 ( 0.000000000000000000, 0.0001568709654583518899, 0.0003137419309167037798 ),
 .UNSPECIFIED. ) ;
#31036 = CARTESIAN_POINT ( 'NONE',  ( 20.94999999999999929, 1.115600667400684642E-11, -113.3750000000000284 ) ) ;
#31037 = CARTESIAN_POINT ( 'NONE',  ( 13.22261339317536866, 66.56344716000714357, -54.34515201176409960 ) ) ;
#31038 = AXIS2_PLACEMENT_3D ( 'NONE', #114373, #190062, #11436 ) ;
#31039 = DIRECTION ( 'NONE',  ( 2.952720810173289112E-16, 1.000000000000000000, 6.982962677686266711E-15 ) ) ;
#31040 = DIRECTION ( 'NONE',  ( 0.000000000000000000, 0.000000000000000000, -1.000000000000000000 ) ) ;
#31041 = CARTESIAN_POINT ( 'NONE',  ( -16.86420534634261514, 9.970615445591718640, -20.91833654923738806 ) ) ;
#31042 = ADVANCED_FACE ( 'NONE', ( #6072 ), #165164, .T. ) ;
#31044 = CARTESIAN_POINT ( 'NONE',  ( 21.06600267594171783, 8.775166069199903163, -12.20426278237474094 ) ) ;
#31043 = CARTESIAN_POINT ( 'NONE',  ( -22.47007471830798764, 10.77449791745511476, -226.9269314985138237 ) ) ;
#31046 = VERTEX_POINT ( 'NONE', #84278 ) ;
#31045 = LINE ( 'NONE', #190085, #118879 ) ;
#31047 = LINE ( 'NONE', #147086, #83279 ) ;
#31048 = ORIENTED_EDGE ( 'NONE', *, *, #126834, .F. ) ;
#31049 = AXIS2_PLACEMENT_3D ( 'NONE', #193404, #153011, #33076 ) ;
#31050 = CARTESIAN_POINT ( 'NONE',  ( -16.86422026484317271, 22.92796883769972283, -230.8850307275119178 ) ) ;
#31051 = ORIENTED_EDGE ( 'NONE', *, *, #246762, .T. ) ;
#31052 = ORIENTED_EDGE ( 'NONE', *, *, #38327, .F. ) ;
#31053 = DIRECTION ( 'NONE',  ( -1.000000000000000000, 0.000000000000000000, 0.000000000000000000 ) ) ;
#31054 = AXIS2_PLACEMENT_3D ( 'NONE', #108893, #106307, #47619 ) ;
#31055 = DIRECTION ( 'NONE',  ( 0.000000000000000000, -0.9910827722268049644, 0.1332476588733589318 ) ) ;
#31056 = CARTESIAN_POINT ( 'NONE',  ( -21.15000000000000213, 76.00000000001273293, -210.0637644362255969 ) ) ;
#31057 = AXIS2_PLACEMENT_3D ( 'NONE', #57712, #19903, #99399 ) ;
#31058 = CIRCLE ( 'NONE', #10183, 0.1000000000000124678 ) ;
#31059 = FACE_OUTER_BOUND ( 'NONE', #217899, .T. ) ;
#31060 = ORIENTED_EDGE ( 'NONE', *, *, #101714, .F. ) ;
#31061 = ORIENTED_EDGE ( 'NONE', *, *, #156338, .T. ) ;
#31062 = DIRECTION ( 'NONE',  ( 0.000000000000000000, 1.000000000000000000, 0.000000000000000000 ) ) ;
#31063 = ORIENTED_EDGE ( 'NONE', *, *, #87418, .T. ) ;
#31064 = CARTESIAN_POINT ( 'NONE',  ( -16.77683809663752257, 9.949999999999983302, -20.85000000000000142 ) ) ;
#31065 = CARTESIAN_POINT ( 'NONE',  ( -16.77683809663752257, 9.950000000011138823, -54.35000000000000142 ) ) ;
#31066 = ORIENTED_EDGE ( 'NONE', *, *, #2804, .F. ) ;
#31067 = DIRECTION ( 'NONE',  ( -1.000000000000000000, 0.000000000000000000, 0.000000000000000000 ) ) ;
#31069 = CIRCLE ( 'NONE', #176787, 11.75000000000000000 ) ;
#31068 = DIRECTION ( 'NONE',  ( 0.000000000000000000, -0.9910465087640865089, 0.1335171055202867274 ) ) ;
#31070 = CARTESIAN_POINT ( 'NONE',  ( -22.50000000000000000, 64.35023708197972780, -69.61191746091132870 ) ) ;
#31071 = CARTESIAN_POINT ( 'NONE',  ( 20.94999999999999929, 68.48451787451661232, -224.2224406095231757 ) ) ;
#31072 = VERTEX_POINT ( 'NONE', #63478 ) ;
#31073 = PLANE ( 'NONE',  #220928 ) ;
#31074 = LINE ( 'NONE', #110566, #162507 ) ;
#31075 = CYLINDRICAL_SURFACE ( 'NONE', #125139, 0.09999999999999939493 ) ;
#31076 = DIRECTION ( 'NONE',  ( 1.000000000000000000, 1.541880601228652843E-16, 2.878400969107353907E-16 ) ) ;
#31077 = CIRCLE ( 'NONE', #6069, 0.1000000000000028644 ) ;
#31078 = CARTESIAN_POINT ( 'NONE',  ( 23.15000000000000213, -8.596261682231833845, -42.95012751715027832 ) ) ;
#31079 = DIRECTION ( 'NONE',  ( -1.000000000000000000, -0.000000000000000000, -0.000000000000000000 ) ) ;
#31080 = CIRCLE ( 'NONE', #214375, 11.74999999999999822 ) ;
#31081 = CIRCLE ( 'NONE', #47762, 0.09999999999998807065 ) ;
#31082 = EDGE_CURVE ( 'NONE', #110369, #148934, #221262, .T. ) ;
#31083 = ORIENTED_EDGE ( 'NONE', *, *, #226588, .F. ) ;
#31084 = AXIS2_PLACEMENT_3D ( 'NONE', #84942, #238930, #241496 ) ;
#31085 = CARTESIAN_POINT ( 'NONE',  ( -21.53752568617692020, 69.21319212550827160, -136.6220819458086737 ) ) ;
#31086 = ORIENTED_EDGE ( 'NONE', *, *, #233606, .T. ) ;
#31087 = FACE_OUTER_BOUND ( 'NONE', #117822, .T. ) ;
#31088 = EDGE_CURVE ( 'NONE', #32887, #72182, #90948, .T. ) ;
#31089 = DIRECTION ( 'NONE',  ( 0.000000000000000000, 0.9856811345164800953, 0.1686199900910462790 ) ) ;
#31090 = LINE ( 'NONE', #173180, #2315 ) ;
#31091 = DIRECTION ( 'NONE',  ( 1.000000000000000000, 0.000000000000000000, 0.000000000000000000 ) ) ;
#31092 = CARTESIAN_POINT ( 'NONE',  ( 20.51284917709620359, 65.68911337716701837, -162.3506342989327038 ) ) ;
#31093 = ORIENTED_EDGE ( 'NONE', *, *, #241636, .F. ) ;
#31094 = DIRECTION ( 'NONE',  ( 1.000000000000000000, 0.000000000000000000, 0.000000000000000000 ) ) ;
#31095 = DIRECTION ( 'NONE',  ( 0.000000000000000000, 1.000000000000000000, 6.938893903907222067E-15 ) ) ;
#31096 = EDGE_CURVE ( 'NONE', #177620, #70690, #122197, .T. ) ;
#31097 = ADVANCED_FACE ( 'NONE', ( #163888 ), #64639, .F. ) ;
#31098 = LINE ( 'NONE', #110588, #252187 ) ;
#31099 = FACE_OUTER_BOUND ( 'NONE', #714, .T. ) ;
#31100 = AXIS2_PLACEMENT_3D ( 'NONE', #124287, #163410, #123003 ) ;
#31101 = DIRECTION ( 'NONE',  ( 0.000000000000000000, 1.000000000000000000, 1.626303258728238113E-15 ) ) ;
#31102 = ORIENTED_EDGE ( 'NONE', *, *, #24643, .T. ) ;
#31103 = ORIENTED_EDGE ( 'NONE', *, *, #54517, .T. ) ;
#31104 = DIRECTION ( 'NONE',  ( 0.000000000000000000, -1.000000000000000000, -6.982962677686265922E-15 ) ) ;
#31105 = CARTESIAN_POINT ( 'NONE',  ( -21.10000000000000497, 6.342459739679071618, 12.00000000000000355 ) ) ;
#31106 = CARTESIAN_POINT ( 'NONE',  ( -18.58671080940900566, -9.406932858815460818, -107.6241544649047484 ) ) ;
#31107 = AXIS2_PLACEMENT_3D ( 'NONE', #184050, #240192, #164507 ) ;
#31108 =( BOUNDED_CURVE ( )  B_SPLINE_CURVE ( 3, ( #176525, #53988, #253461, #35741 ),
 .UNSPECIFIED., .F., .F. ) 
 B_SPLINE_CURVE_WITH_KNOTS ( ( 4, 4 ),
 ( 0.5235987755983901870, 1.570796326794896558 ),
 .UNSPECIFIED. ) 
 CURVE ( )  GEOMETRIC_REPRESENTATION_ITEM ( )  RATIONAL_B_SPLINE_CURVE ( ( 1.000000000000000000, 0.9106836025229743115, 0.9106836025229743115, 1.000000000000000000 ) ) 
 REPRESENTATION_ITEM ( '' )  );
#31109 = DIRECTION ( 'NONE',  ( 1.000000000000000000, 0.000000000000000000, 0.000000000000000000 ) ) ;
#31110 = EDGE_CURVE ( 'NONE', #121929, #243465, #101280, .T. ) ;
#31111 = EDGE_LOOP ( 'NONE', ( #177741, #256669, #117207, #251985 ) ) ;
#31112 = DIRECTION ( 'NONE',  ( 0.000000000000000000, 0.2128009952263604232, -0.9770955615653316162 ) ) ;
#31113 = ADVANCED_FACE ( 'NONE', ( #83019 ), #91398, .T. ) ;
#31114 = ITEM_DEFINED_TRANSFORMATION ( 'NONE', 'NONE', #2781,  #2425 ) ;
#31115 = DIRECTION ( 'NONE',  ( -0.000000000000000000, 0.7397360091702694929, 0.6728971962616898672 ) ) ;
#31116 = ORIENTED_EDGE ( 'NONE', *, *, #128327, .T. ) ;
#31117 = LINE ( 'NONE', #12822, #83818 ) ;
#31118 = AXIS2_PLACEMENT_3D ( 'NONE', #161074, #18969, #138888 ) ;
#31119 = AXIS2_PLACEMENT_3D ( 'NONE', #147910, #227425, #118396 ) ;
#31120 = ORIENTED_EDGE ( 'NONE', *, *, #129702, .T. ) ;
#31121 = ORIENTED_EDGE ( 'NONE', *, *, #194289, .F. ) ;
#31122 = ADVANCED_FACE ( 'NONE', ( #11881 ), #169691, .T. ) ;
#31123 = ORIENTED_EDGE ( 'NONE', *, *, #18768, .F. ) ;
#31124 = EDGE_CURVE ( 'NONE', #40380, #87179, #245338, .T. ) ;
#31125 = CARTESIAN_POINT ( 'NONE',  ( -16.92989507731676113, 9.950000000011138823, -154.6174989306102248 ) ) ;
#31126 = EDGE_CURVE ( 'NONE', #204362, #32814, #85448, .T. ) ;
#31127 = DIRECTION ( 'NONE',  ( 1.000000000000000000, -0.000000000000000000, -0.000000000000000000 ) ) ;
#31128 = DIRECTION ( 'NONE',  ( 0.000000000000000000, -2.664535259100396996E-15, 1.000000000000000000 ) ) ;
#31129 = DIRECTION ( 'NONE',  ( 0.000000000000000000, 0.000000000000000000, -1.000000000000000000 ) ) ;
#31130 = DIRECTION ( 'NONE',  ( 0.000000000000000000, -0.8814952561688428334, 0.4721928772777350680 ) ) ;
#31131 = CARTESIAN_POINT ( 'NONE',  ( -20.85000000000000142, 77.16412189325360771, -162.3082593989527425 ) ) ;
#31132 = DIRECTION ( 'NONE',  ( 0.000000000000000000, 0.000000000000000000, 1.000000000000000000 ) ) ;
#31134 = DIRECTION ( 'NONE',  ( 1.000000000000000000, 0.000000000000000000, 0.000000000000000000 ) ) ;
#31133 = DIRECTION ( 'NONE',  ( 0.000000000000000000, 0.4999999999999088507, -0.8660254037844913322 ) ) ;
#31135 = DIRECTION ( 'NONE',  ( 1.000000000000000000, 0.000000000000000000, 0.000000000000000000 ) ) ;
#31136 = DIRECTION ( 'NONE',  ( 0.000000000000000000, 0.000000000000000000, -1.000000000000000000 ) ) ;
#31137 = CARTESIAN_POINT ( 'NONE',  ( 22.50000000000000000, 0.1000000000111554016, -155.8504291924551808 ) ) ;
#31139 = DIRECTION ( 'NONE',  ( 1.000000000000000000, 8.674042436075353235E-17, 1.619280515896125144E-16 ) ) ;
#31138 = VECTOR ( 'NONE', #114597, 1000.000000000000000 ) ;
#31140 = ORIENTED_EDGE ( 'NONE', *, *, #113628, .F. ) ;
#31141 = AXIS2_PLACEMENT_3D ( 'NONE', #190563, #109704, #228396 ) ;
#31142 = EDGE_LOOP ( 'NONE', ( #219803, #246834, #149935, #193703 ) ) ;
#31143 = CARTESIAN_POINT ( 'NONE',  ( -18.33682934331515568, -9.511185591093616054, -40.40565476867323014 ) ) ;
#31144 = CARTESIAN_POINT ( 'NONE',  ( 23.14999999999999147, -4.149999999988843058, -33.50000000000000000 ) ) ;
#31146 = DIRECTION ( 'NONE',  ( 1.000000000000000000, -0.000000000000000000, -0.000000000000000000 ) ) ;
#31145 = AXIS2_PLACEMENT_3D ( 'NONE', #82938, #80375, #101208 ) ;
#31147 = CIRCLE ( 'NONE', #226912, 0.5000000000000069944 ) ;
#31148 = EDGE_CURVE ( 'NONE', #210729, #219970, #14800, .T. ) ;
#31150 = DIRECTION ( 'NONE',  ( 1.000000000000000000, 0.000000000000000000, 0.000000000000000000 ) ) ;
#31149 = PRESENTATION_LAYER_ASSIGNMENT (  '', '', ( #185229 ) ) ;
#31151 = CARTESIAN_POINT ( 'NONE',  ( -18.59999999999999787, 18.81339837015603322, -226.7756228984618190 ) ) ;
#31152 = CARTESIAN_POINT ( 'NONE',  ( 13.99999999999999822, 26.54497872210689735, -232.9592037335782209 ) ) ;
#31153 = ORIENTED_EDGE ( 'NONE', *, *, #224184, .T. ) ;
#31154 = EDGE_LOOP ( 'NONE', ( #195786, #188978, #137263, #234740 ) ) ;
#31155 = ADVANCED_FACE ( 'NONE', ( #129240 ), #229625, .T. ) ;
#31156 = DIRECTION ( 'NONE',  ( -1.000000000000000000, 0.000000000000000000, -0.000000000000000000 ) ) ;
#31157 = ORIENTED_EDGE ( 'NONE', *, *, #120083, .T. ) ;
#31158 = DIRECTION ( 'NONE',  ( 0.000000000000000000, 0.000000000000000000, -1.000000000000000000 ) ) ;
#31159 = AXIS2_PLACEMENT_3D ( 'NONE', #2089, #238135, #161188 ) ;
#31160 = AXIS2_PLACEMENT_3D ( 'NONE', #245800, #247065, #104958 ) ;
#31161 = AXIS2_PLACEMENT_3D ( 'NONE', #22144, #97770, #3843 ) ;
#31162 = ORIENTED_EDGE ( 'NONE', *, *, #232783, .F. ) ;
#31163 = CYLINDRICAL_SURFACE ( 'NONE', #210212, 0.09999999999999939493 ) ;
#31164 = ADVANCED_FACE ( 'NONE', ( #125393 ), #145408, .T. ) ;
#31165 = EDGE_LOOP ( 'NONE', ( #244128, #51541, #74122, #6582 ) ) ;
#31167 =( BOUNDED_SURFACE ( )  B_SPLINE_SURFACE ( 3, 2, ( 
 ( #97788, #177393, #241202 ),
 ( #1270, #80800, #122536 ),
 ( #256836, #102934, #160393 ),
 ( #202064, #23455, #255557 ) ),
 .UNSPECIFIED., .F., .F., .F. ) 
 B_SPLINE_SURFACE_WITH_KNOTS ( ( 4, 4 ),
 ( 3, 3 ),
 ( 4.712388980384689674, 5.765869716888531116 ),
 ( 0.000000000000000000, 1.000000000000000000 ),
 .UNSPECIFIED. ) 
 GEOMETRIC_REPRESENTATION_ITEM ( )  RATIONAL_B_SPLINE_SURFACE ( (
 ( 1.000000000000000000, 0.7071067811866457165, 1.000000000000000000),
 ( 1.000000000000000000, 0.7953136715912294541, 1.000000000000000000),
 ( 1.000000000000000000, 0.8646876308616092688, 1.000000000000000000),
 ( 1.000000000000000000, 0.8984936768950676500, 1.000000000000000000) ) ) 
 REPRESENTATION_ITEM ( '' )  SURFACE ( )  );
#31166 = CARTESIAN_POINT ( 'NONE',  ( 20.94999999999999929, 65.26666169030359299, -222.4689051838086300 ) ) ;
#31168 = LINE ( 'NONE', #71562, #149492 ) ;
#31170 = TOROIDAL_SURFACE ( 'NONE', #64456, 11.65000000000000036, 0.1000000000000000056 ) ;
#31169 = CARTESIAN_POINT ( 'NONE',  ( 18.59999999999999076, 11.65000000001115943, -58.35000000000000142 ) ) ;
#31171 = ADVANCED_FACE ( 'NONE', ( #26292 ), #189216, .F. ) ;
#31172 = AXIS2_PLACEMENT_3D ( 'NONE', #250176, #110656, #33739 ) ;
#31173 = FACE_OUTER_BOUND ( 'NONE', #87760, .T. ) ;
#31175 = VECTOR ( 'NONE', #115186, 1000.000000000000000 ) ;
#31174 = CARTESIAN_POINT ( 'NONE',  ( 20.95512820512820440, 10.49413282287806481, -207.4737445703522383 ) ) ;
#31176 = LINE ( 'NONE', #32452, #130081 ) ;
#31177 = DIRECTION ( 'NONE',  ( -1.000000000000000000, 0.000000000000000000, 0.000000000000000000 ) ) ;
#31178 = ADVANCED_FACE ( 'NONE', ( #167113 ), #148809, .T. ) ;
#31179 = ORIENTED_EDGE ( 'NONE', *, *, #62238, .T. ) ;
#31181 = CARTESIAN_POINT ( 'NONE',  ( -23.15000000000000213, 70.10000000001177511, -79.74220724918072278 ) ) ;
#31180 = DIRECTION ( 'NONE',  ( 0.000000000000000000, 0.000000000000000000, -1.000000000000000000 ) ) ;
#31182 = AXIS2_PLACEMENT_3D ( 'NONE', #251390, #151023, #88440 ) ;
#31183 = ORIENTED_EDGE ( 'NONE', *, *, #87606, .T. ) ;
#31185 = ORIENTED_EDGE ( 'NONE', *, *, #250928, .F. ) ;
#31184 = DIRECTION ( 'NONE',  ( 0.000000000000000000, 0.1350103645451974088, -0.9908441862701587999 ) ) ;
#31186 = EDGE_LOOP ( 'NONE', ( #131540, #15244, #11273, #93517 ) ) ;
#31187 = DIRECTION ( 'NONE',  ( 0.000000000000000000, -7.147358527629766941E-15, 1.000000000000000000 ) ) ;
#31188 = DIRECTION ( 'NONE',  ( -1.000000000000000000, -0.000000000000000000, -0.000000000000000000 ) ) ;
#31189 = EDGE_CURVE ( 'NONE', #209650, #102873, #80997, .T. ) ;
#31190 = CIRCLE ( 'NONE', #14596, 0.1000000000000028644 ) ;
#31191 = EDGE_CURVE ( 'NONE', #85747, #157859, #147654, .T. ) ;
#31192 = CIRCLE ( 'NONE', #85278, 0.5999999999999962030 ) ;
#31193 = CARTESIAN_POINT ( 'NONE',  ( 21.04386569057588119, 62.86478208612204810, -207.0655967136942479 ) ) ;
#31194 = CARTESIAN_POINT ( 'NONE',  ( -22.59999999999999787, 11.45898712536580177, -198.4011321578509808 ) ) ;
#31195 = AXIS2_PLACEMENT_3D ( 'NONE', #186781, #31576, #250575 ) ;
#31196 = CARTESIAN_POINT ( 'NONE',  ( -20.64999999999999858, 76.00000000001253397, -182.8981074845243597 ) ) ;
#31197 = CIRCLE ( 'NONE', #176920, 0.1000000000000024342 ) ;
#31198 = DIRECTION ( 'NONE',  ( -1.284434275755705296E-16, 0.7071067811865471286, -0.7071067811865479058 ) ) ;
#31199 = DIRECTION ( 'NONE',  ( 0.000000000000000000, -0.1298341882520124002, -0.9915357197604841577 ) ) ;
#31200 = CYLINDRICAL_SURFACE ( 'NONE', #126829, 0.09999999999998898659 ) ;
#31201 = ORIENTED_EDGE ( 'NONE', *, *, #61826, .F. ) ;
#31202 = ORIENTED_EDGE ( 'NONE', *, *, #236248, .T. ) ;
#31203 = DIRECTION ( 'NONE',  ( 1.000000000000000000, 0.000000000000000000, 0.000000000000000000 ) ) ;
#31204 = ADVANCED_FACE ( 'NONE', ( #90089 ), #181567, .F. ) ;
#31205 = ORIENTED_EDGE ( 'NONE', *, *, #121171, .T. ) ;
#31206 = DIRECTION ( 'NONE',  ( -0.000000000000000000, -0.000000000000000000, -1.000000000000000000 ) ) ;
#31208 = EDGE_CURVE ( 'NONE', #255306, #247138, #226752, .T. ) ;
#31207 = ORIENTED_EDGE ( 'NONE', *, *, #117733, .T. ) ;
#31209 = CARTESIAN_POINT ( 'NONE',  ( 22.49806830649814060, 11.64988965485023620, -33.42253568367449645 ) ) ;
#31210 =( BOUNDED_SURFACE ( )  B_SPLINE_SURFACE ( 3, 2, ( 
 ( #103288, #168475, #164582 ),
 ( #124176, #146280, #223241 ),
 ( #44629, #108450, #5464 ),
 ( #207564, #105852, #185419 ) ),
 .UNSPECIFIED., .F., .F., .F. ) 
 B_SPLINE_SURFACE_WITH_KNOTS ( ( 4, 4 ),
 ( 3, 3 ),
 ( 0.04058434257139457990, 0.04256401539001584966 ),
 ( 0.000000000000000000, 1.000000000000000000 ),
 .UNSPECIFIED. ) 
 GEOMETRIC_REPRESENTATION_ITEM ( )  RATIONAL_B_SPLINE_SURFACE ( (
 ( 1.000000000000000000, 0.7103081912008579746, 1.000000000000000000),
 ( 1.000000000000000000, 0.7104998333553130818, 1.000000000000000000),
 ( 1.000000000000000000, 0.7107238315756889691, 1.000000000000000000),
 ( 1.000000000000000000, 0.7110073749539658206, 1.000000000000000000) ) ) 
 REPRESENTATION_ITEM ( '' )  SURFACE ( )  );
#31211 = CARTESIAN_POINT ( 'NONE',  ( -20.64999999999999858, 24.12844930803500887, -253.0488546976795021 ) ) ;
#31212 = CARTESIAN_POINT ( 'NONE',  ( -22.47886152344871036, -2.442487176688612482, -189.6088675674811839 ) ) ;
#31213 = EDGE_CURVE ( 'NONE', #155399, #238367, #110955, .T. ) ;
#31214 = DIRECTION ( 'NONE',  ( -1.000000000000000000, 0.000000000000000000, 0.000000000000000000 ) ) ;
#31215 = ORIENTED_EDGE ( 'NONE', *, *, #88512, .F. ) ;
#31216 = CARTESIAN_POINT ( 'NONE',  ( -18.39999999999999858, 85.60000000001241460, -163.4229180933022576 ) ) ;
#31217 = AXIS2_PLACEMENT_3D ( 'NONE', #186375, #239929, #203362 ) ;
#31218 = CARTESIAN_POINT ( 'NONE',  ( 20.94999999999999929, 64.35000000001214460, -136.5231074845244166 ) ) ;
#31219 = EDGE_CURVE ( 'NONE', #166393, #233837, #115901, .T. ) ;
#31220 = AXIS2_PLACEMENT_3D ( 'NONE', #230683, #54591, #52011 ) ;
#31221 = DIRECTION ( 'NONE',  ( -0.7070776581709311559, 4.937903618720164857E-15, -0.7071359030027479786 ) ) ;
#31222 = FACE_OUTER_BOUND ( 'NONE', #7733, .T. ) ;
#31223 = AXIS2_PLACEMENT_3D ( 'NONE', #9669, #128348, #228740 ) ;
#31225 = ORIENTED_EDGE ( 'NONE', *, *, #152309, .F. ) ;
#31224 = EDGE_CURVE ( 'NONE', #225539, #232013, #14451, .T. ) ;
#31227 = FACE_OUTER_BOUND ( 'NONE', #247709, .T. ) ;
#31226 = CARTESIAN_POINT ( 'NONE',  ( -16.92209698673438822, 60.95522930754523117, -220.9832062338754781 ) ) ;
#31228 = ORIENTED_EDGE ( 'NONE', *, *, #239374, .T. ) ;
#31231 = ORIENTED_EDGE ( 'NONE', *, *, #79678, .F. ) ;
#31230 = CARTESIAN_POINT ( 'NONE',  ( 22.59999999999999076, 64.25012875563564307, -136.5885370755380563 ) ) ;
#31229 = DIRECTION ( 'NONE',  ( 0.000000000000000000, 1.000000000000000000, 8.717686153663073805E-15 ) ) ;
#31232 = FACE_OUTER_BOUND ( 'NONE', #162114, .T. ) ;
#31233 = CIRCLE ( 'NONE', #176957, 0.1000000000000028644 ) ;
#31234 = DIRECTION ( 'NONE',  ( 0.000000000000000000, 0.000000000000000000, 1.000000000000000000 ) ) ;
#31235 = ADVANCED_FACE ( 'NONE', ( #54813 ), #230924, .F. ) ;
#31236 = CARTESIAN_POINT ( 'NONE',  ( -18.42637059832564006, 85.49694546190156075, -96.41403017472441661 ) ) ;
#31237 = AXIS2_PLACEMENT_3D ( 'NONE', #183985, #144847, #88713 ) ;
#31238 = ORIENTED_EDGE ( 'NONE', *, *, #227726, .F. ) ;
#31239 = DIRECTION ( 'NONE',  ( 0.000000000000000000, -0.9126074666063660468, -0.4088369013363524762 ) ) ;
#31240 = LINE ( 'NONE', #229404, #15504 ) ;
#31242 = CARTESIAN_POINT ( 'NONE',  ( 13.40000000000000036, -8.250000000000005329, 19.04142135623731136 ) ) ;
#31241 = CARTESIAN_POINT ( 'NONE',  ( -23.25000000000000355, 58.31215475832291162, -223.8520309854405923 ) ) ;
#31243 = EDGE_CURVE ( 'NONE', #218543, #47449, #27465, .T. ) ;
#31245 = ORIENTED_EDGE ( 'NONE', *, *, #115905, .F. ) ;
#31244 = CARTESIAN_POINT ( 'NONE',  ( 21.05000000000000071, 11.75000000001116085, -93.65839931010300745 ) ) ;
#31246 = VECTOR ( 'NONE', #86431, 1000.000000000000000 ) ;
#31247 = EDGE_LOOP ( 'NONE', ( #167002, #187940, #2970, #121405 ) ) ;
#31248 = DIRECTION ( 'NONE',  ( 0.000000000000000000, 0.000000000000000000, -1.000000000000000000 ) ) ;
#31249 = DIRECTION ( 'NONE',  ( -0.4999999999999799050, -6.047423072554995242E-15, 0.8660254037844502539 ) ) ;
#31250 = CARTESIAN_POINT ( 'NONE',  ( 23.14999999999999858, 76.00000000001170974, -69.52310748452431710 ) ) ;
#31251 = ORIENTED_EDGE ( 'NONE', *, *, #137353, .T. ) ;
#31252 = DIRECTION ( 'NONE',  ( 1.000000000000000000, 3.265361837132813093E-16, -0.000000000000000000 ) ) ;
#31253 = DIRECTION ( 'NONE',  ( 3.469446951953635646E-14, -0.9126074666063771490, -0.4088369013363281623 ) ) ;
#31254 = CARTESIAN_POINT ( 'NONE',  ( -20.94999999999994600, 65.15000000001120384, -51.02310748452479316 ) ) ;
#31255 = TOROIDAL_SURFACE ( 'NONE', #72939, 0.2000000000000000111, 0.1000000000000000056 ) ;
#31256 = ORIENTED_EDGE ( 'NONE', *, *, #56199, .T. ) ;
#31257 = DIRECTION ( 'NONE',  ( 0.000000000000000000, 0.000000000000000000, -1.000000000000000000 ) ) ;
#31258 = DIRECTION ( 'NONE',  ( -0.000000000000000000, -0.9876197685951252359, -0.1568667991644863424 ) ) ;
#31259 = VERTEX_POINT ( 'NONE', #96500 ) ;
#31260 = FACE_OUTER_BOUND ( 'NONE', #31983, .T. ) ;
#31261 = CARTESIAN_POINT ( 'NONE',  ( -23.15000000000000213, -9.000000000000001776, -24.20603087734755832 ) ) ;
#31262 = AXIS2_PLACEMENT_3D ( 'NONE', #74616, #56277, #166326 ) ;
#31263 = ORIENTED_EDGE ( 'NONE', *, *, #255330, .F. ) ;
#31264 = CIRCLE ( 'NONE', #60252, 0.09999999999999939493 ) ;
#31265 = ORIENTED_EDGE ( 'NONE', *, *, #186678, .T. ) ;
#31266 = DIRECTION ( 'NONE',  ( 1.000000000000000000, 0.000000000000000000, 0.000000000000000000 ) ) ;
#31267 = ADVANCED_FACE ( 'NONE', ( #213901 ), #252251, .T. ) ;
#31268 = ORIENTED_EDGE ( 'NONE', *, *, #206744, .F. ) ;
#31270 = ORIENTED_EDGE ( 'NONE', *, *, #68139, .F. ) ;
#31269 = DIRECTION ( 'NONE',  ( -0.000000000000000000, 0.1350103645451859180, 0.9908441862701603542 ) ) ;
#31271 = VERTEX_POINT ( 'NONE', #131798 ) ;
#31274 = EDGE_LOOP ( 'NONE', ( #249689, #57341, #194975, #8672 ) ) ;
#31273 = ORIENTED_EDGE ( 'NONE', *, *, #3562, .F. ) ;
#31272 = CARTESIAN_POINT ( 'NONE',  ( -20.64999999999999858, 9.614325556249161409, -211.5456030694648746 ) ) ;
#31275 = DIRECTION ( 'NONE',  ( -1.000000000000000000, 0.000000000000000000, 0.000000000000000000 ) ) ;
#31276 = ORIENTED_EDGE ( 'NONE', *, *, #197415, .F. ) ;
#31277 = DIRECTION ( 'NONE',  ( 1.000000000000000000, 0.000000000000000000, 0.000000000000000000 ) ) ;
#31279 = ADVANCED_FACE ( 'NONE', ( #211344 ), #255542, .F. ) ;
#31278 = DIRECTION ( 'NONE',  ( -1.000000000000000000, 0.000000000000000000, 0.000000000000000000 ) ) ;
#31280 = VECTOR ( 'NONE', #221756, 1000.000000000000114 ) ;
#31281 = DIRECTION ( 'NONE',  ( 0.000000000000000000, 1.000000000000000000, 0.000000000000000000 ) ) ;
#31282 = DIRECTION ( 'NONE',  ( -1.000000000000000000, 0.000000000000000000, 0.000000000000000000 ) ) ;
#31283 = EDGE_LOOP ( 'NONE', ( #154774, #195519, #115257 ) ) ;
#31284 = ORIENTED_EDGE ( 'NONE', *, *, #12864, .F. ) ;
#31285 = ORIENTED_EDGE ( 'NONE', *, *, #84250, .T. ) ;
#31286 = CARTESIAN_POINT ( 'NONE',  ( 20.95512820512820795, 8.876151316299273120, -146.2001728591287701 ) ) ;
#31287 = VECTOR ( 'NONE', #60912, 1000.000000000000000 ) ;
#31289 = EDGE_LOOP ( 'NONE', ( #141431, #18415, #154100, #91178, #224190, #166767 ) ) ;
#31288 = LINE ( 'NONE', #96328, #24552 ) ;
#31290 = FACE_OUTER_BOUND ( 'NONE', #52720, .T. ) ;
#31292 = EDGE_LOOP ( 'NONE', ( #193123, #90992, #26434, #24466 ) ) ;
#31291 = DIRECTION ( 'NONE',  ( -1.000000000000000000, -0.000000000000000000, -0.000000000000000000 ) ) ;
#31293 = VERTEX_POINT ( 'NONE', #57377 ) ;
#31294 = CARTESIAN_POINT ( 'NONE',  ( 18.49999999999999289, 64.35000000001275566, -215.2731074845244450 ) ) ;
#31295 = VERTEX_POINT ( 'NONE', #34026 ) ;
#31296 = DIRECTION ( 'NONE',  ( -1.000000000000000000, 0.000000000000000000, 0.000000000000000000 ) ) ;
#31297 = DIRECTION ( 'NONE',  ( -3.469446951953635015E-14, 1.000000000000000000, 0.000000000000000000 ) ) ;
#31300 = ORIENTED_EDGE ( 'NONE', *, *, #82594, .T. ) ;
#31299 = VERTEX_POINT ( 'NONE', #136932 ) ;
#31298 = AXIS2_PLACEMENT_3D ( 'NONE', #232616, #210468, #16136 ) ;
#31301 = VERTEX_POINT ( 'NONE', #216462 ) ;
#31302 = CARTESIAN_POINT ( 'NONE',  ( 21.15000000000005542, 76.00000000001119815, -3.123107484524795474 ) ) ;
#31303 = ORIENTED_EDGE ( 'NONE', *, *, #237990, .T. ) ;
#31304 = ORIENTED_EDGE ( 'NONE', *, *, #192762, .F. ) ;
#31305 = DIRECTION ( 'NONE',  ( -0.000000000000000000, 0.9525900758537790836, -0.3042567129660269099 ) ) ;
#31307 = VERTEX_POINT ( 'NONE', #117376 ) ;
#31306 = DIRECTION ( 'NONE',  ( 0.000000000000000000, -0.9126074666063742624, -0.4088369013363343241 ) ) ;
#31308 = DIRECTION ( 'NONE',  ( -0.000000000000000000, 0.1298341882519668811, 0.9915357197604899309 ) ) ;
#31310 = CARTESIAN_POINT ( 'NONE',  ( 22.50000000000000000, 75.90000000001222702, -148.1726782920690937 ) ) ;
#31309 = CARTESIAN_POINT ( 'NONE',  ( -20.00857864376270001, 9.350000000011156942, -121.7500000000000426 ) ) ;
#31311 = CARTESIAN_POINT ( 'NONE',  ( -18.50000000000000000, 0.000000000000000000, -33.50000000000000000 ) ) ;
#31312 = CARTESIAN_POINT ( 'NONE',  ( -14.23072895065542909, 62.03428458984607374, -218.8918409208595222 ) ) ;
#31313 = VERTEX_POINT ( 'NONE', #196902 ) ;
#31314 = EDGE_CURVE ( 'NONE', #57244, #215487, #102389, .T. ) ;
#31315 = ORIENTED_EDGE ( 'NONE', *, *, #146602, .T. ) ;
#31316 = SPHERICAL_SURFACE ( 'NONE', #139233, 0.1000000000000000056 ) ;
#31317 = CARTESIAN_POINT ( 'NONE',  ( -20.94999999999999929, 72.02722222756959525, -225.1832529173024398 ) ) ;
#31318 = AXIS2_PLACEMENT_3D ( 'NONE', #114280, #197659, #231681 ) ;
#31319 = ORIENTED_EDGE ( 'NONE', *, *, #128961, .T. ) ;
#31320 = CIRCLE ( 'NONE', #177053, 0.5000000000000004441 ) ;
#31321 = VECTOR ( 'NONE', #7278, 1000.000000000000000 ) ;
#31322 = AXIS2_PLACEMENT_3D ( 'NONE', #65315, #27524, #183982 ) ;
#31323 = CARTESIAN_POINT ( 'NONE',  ( 21.13920837816993270, 44.24745038003037934, -236.5272538208875801 ) ) ;
#31324 = CARTESIAN_POINT ( 'NONE',  ( 20.27550659511089037, 9.216043722520002035, -146.6500000000000341 ) ) ;
#31325 = ORIENTED_EDGE ( 'NONE', *, *, #198005, .T. ) ;
#31326 = VERTEX_POINT ( 'NONE', #113523 ) ;
#31327 = COLOUR_RGB ( '', 0.66274510, 0.83137255, 0.94901961) ;
#31328 = EDGE_CURVE ( 'NONE', #120640, #84969, #69134, .T. ) ;
#31329 = CARTESIAN_POINT ( 'NONE',  ( 23.25000000000000000, 64.14229051353817113, -222.2212283990554624 ) ) ;
#31330 = VERTEX_POINT ( 'NONE', #139485 ) ;
#31331 = CARTESIAN_POINT ( 'NONE',  ( -18.39999999999999858, -9.499999999988849808, -174.5320693966996259 ) ) ;
#31332 = ORIENTED_EDGE ( 'NONE', *, *, #206914, .T. ) ;
#31333 = CARTESIAN_POINT ( 'NONE',  ( -21.05000000000000426, 6.477046381801003783, -100.6000000000000512 ) ) ;
#31334 = DIRECTION ( 'NONE',  ( 0.000000000000000000, 0.4088369013363281068, -0.9126074666063770380 ) ) ;
#31336 = CARTESIAN_POINT ( 'NONE',  ( -21.05000000000000071, 39.30548607490320734, -248.3655356873701123 ) ) ;
#31335 = DIRECTION ( 'NONE',  ( -0.000000000000000000, 1.000000000000000000, -0.000000000000000000 ) ) ;
#31337 = EDGE_CURVE ( 'NONE', #214000, #105911, #52341, .T. ) ;
#31338 = CARTESIAN_POINT ( 'NONE',  ( 19.99999999738043144, 11.75000000001115907, -91.68717194963230099 ) ) ;
#31339 = DIRECTION ( 'NONE',  ( 0.000000000000000000, 0.000000000000000000, -1.000000000000000000 ) ) ;
#31340 = CARTESIAN_POINT ( 'NONE',  ( -20.15000000000000568, 9.291421356248463326, -112.8500000000000369 ) ) ;
#31341 = DIRECTION ( 'NONE',  ( 1.000000000000000000, 0.000000000000000000, 0.000000000000000000 ) ) ;
#31342 = ADVANCED_FACE ( 'NONE', ( #119971 ), #114909, .T. ) ;
#31344 = ORIENTED_EDGE ( 'NONE', *, *, #234189, .F. ) ;
#31343 = DIRECTION ( 'NONE',  ( 0.000000000000000000, 0.000000000000000000, 1.000000000000000000 ) ) ;
#31345 = CIRCLE ( 'NONE', #164585, 0.09999999999999939493 ) ;
#31346 = CIRCLE ( 'NONE', #243689, 0.1000000000000028644 ) ;
#31348 = EDGE_LOOP ( 'NONE', ( #214771, #182410, #101520, #256633 ) ) ;
#31347 = ORIENTED_EDGE ( 'NONE', *, *, #45170, .T. ) ;
#31349 = EDGE_LOOP ( 'NONE', ( #176389, #216597, #154719, #251365 ) ) ;
#31350 = CIRCLE ( 'NONE', #22951, 0.1000000000000028783 ) ;
#31351 = DIRECTION ( 'NONE',  ( 0.000000000000000000, 0.000000000000000000, -1.000000000000000000 ) ) ;
#31352 = CARTESIAN_POINT ( 'NONE',  ( -20.64999999999999858, 6.268811756569107274, -220.3853799378769622 ) ) ;
#31353 = EDGE_CURVE ( 'NONE', #77226, #32098, #100347, .T. ) ;
#31355 = FACE_OUTER_BOUND ( 'NONE', #57405, .T. ) ;
#31354 = DIRECTION ( 'NONE',  ( 0.000000000000000000, -0.2606175937107792495, 0.9654421110809303652 ) ) ;
#31356 = DIRECTION ( 'NONE',  ( 0.000000000000000000, -0.9915357197604982575, 0.1298341882519033486 ) ) ;
#31357 = VERTEX_POINT ( 'NONE', #220335 ) ;
#31358 = AXIS2_PLACEMENT_3D ( 'NONE', #179019, #197257, #56447 ) ;
#31359 = DIRECTION ( 'NONE',  ( -1.000000000000000000, -0.000000000000000000, -0.000000000000000000 ) ) ;
#31360 = CIRCLE ( 'NONE', #243699, 0.5000000000000004441 ) ;
#31361 = AXIS2_PLACEMENT_3D ( 'NONE', #110130, #189674, #231380 ) ;
#31362 = ORIENTED_EDGE ( 'NONE', *, *, #187321, .T. ) ;
#31363 = DIRECTION ( 'NONE',  ( 0.000000000000000000, 6.982962677686266711E-15, -1.000000000000000000 ) ) ;
#31364 = CARTESIAN_POINT ( 'NONE',  ( 18.79999999999999361, -11.65000000000000036, 32.89999999999999858 ) ) ;
#31365 = ORIENTED_EDGE ( 'NONE', *, *, #253911, .F. ) ;
#31366 = DIRECTION ( 'NONE',  ( 0.000000000000000000, 0.000000000000000000, 1.000000000000000000 ) ) ;
#31367 = CIRCLE ( 'NONE', #64625, 0.2000000000000057288 ) ;
#31368 = CYLINDRICAL_SURFACE ( 'NONE', #188182, 0.09999999999999939493 ) ;
#31369 = VERTEX_POINT ( 'NONE', #23440 ) ;
#31370 = ORIENTED_EDGE ( 'NONE', *, *, #107579, .F. ) ;
#31371 = DIRECTION ( 'NONE',  ( 0.000000000000000000, 0.000000000000000000, -1.000000000000000000 ) ) ;
#31372 = CIRCLE ( 'NONE', #143744, 0.5000000000000008882 ) ;
#31373 = CYLINDRICAL_SURFACE ( 'NONE', #172972, 2.000000000000001776 ) ;
#31374 = PLANE ( 'NONE',  #52924 ) ;
#31375 = DIRECTION ( 'NONE',  ( 0.000000000000000000, 0.4088369013363280513, -0.9126074666063769270 ) ) ;
#31376 = LINE ( 'NONE', #67892, #56692 ) ;
#31377 = TOROIDAL_SURFACE ( 'NONE', #135555, 7.800000000000000711, 0.1000000000000000056 ) ;
#31378 = CARTESIAN_POINT ( 'NONE',  ( -21.07954640115341860, 6.329287696024277210, 0.06600770713963553804 ) ) ;
#31380 = EDGE_LOOP ( 'NONE', ( #80655, #43236, #168530, #247222 ) ) ;
#31379 = VECTOR ( 'NONE', #108782, 1000.000000000000114 ) ;
#31381 = DIRECTION ( 'NONE',  ( 0.000000000000000000, -1.000000000000000000, -6.982962677686265922E-15 ) ) ;
#31383 = EDGE_CURVE ( 'NONE', #25563, #63872, #19034, .T. ) ;
#31382 = CARTESIAN_POINT ( 'NONE',  ( -22.47071067811865674, 7.720074744509219045, -33.40090754529740025 ) ) ;
#31385 = DIRECTION ( 'NONE',  ( 1.000000000000000000, 0.000000000000000000, 0.000000000000000000 ) ) ;
#31384 = CARTESIAN_POINT ( 'NONE',  ( 23.14999999999999858, 72.10000000001190301, -103.0231074845243313 ) ) ;
#31386 = DIRECTION ( 'NONE',  ( 1.000000000000000000, 0.000000000000000000, 0.000000000000000000 ) ) ;
#31387 = CYLINDRICAL_SURFACE ( 'NONE', #29269, 0.1000000000000028644 ) ;
#31388 = DIRECTION ( 'NONE',  ( 0.000000000000000000, -3.552713678800376289E-15, 1.000000000000000000 ) ) ;
#31389 = CARTESIAN_POINT ( 'NONE',  ( 20.94999999999999929, 69.15387683765909799, -65.78538121767449809 ) ) ;
#31391 = ORIENTED_EDGE ( 'NONE', *, *, #181548, .T. ) ;
#31390 = DIRECTION ( 'NONE',  ( 0.000000000000000000, -1.000000000000000000, -6.982962677686266711E-15 ) ) ;
#31392 = EDGE_CURVE ( 'NONE', #188797, #127805, #140787, .T. ) ;
#31393 = EDGE_CURVE ( 'NONE', #11282, #133539, #198109, .T. ) ;
#31395 = VECTOR ( 'NONE', #2917, 1000.000000000000000 ) ;
#31394 = CARTESIAN_POINT ( 'NONE',  ( 21.14999999999999858, 76.00000000001260503, -191.3731074845243540 ) ) ;
#31396 = DIRECTION ( 'NONE',  ( 1.000000000000000000, 0.000000000000000000, 0.000000000000000000 ) ) ;
#31397 = ADVANCED_FACE ( 'NONE', ( #24723, #142059, #1254 ), #102920, .F. ) ;
#31398 = AXIS2_PLACEMENT_3D ( 'NONE', #234497, #117133, #55835 ) ;
#31399 = CYLINDRICAL_SURFACE ( 'NONE', #225351, 0.09999999999999693856 ) ;
#31400 = EDGE_LOOP ( 'NONE', ( #48508, #131940, #16758, #112596 ) ) ;
#31401 = LINE ( 'NONE', #230870, #114024 ) ;
#31402 = CARTESIAN_POINT ( 'NONE',  ( 21.05000000000000071, 1.115650877919449575E-11, -62.90000000000001279 ) ) ;
#31403 = CARTESIAN_POINT ( 'NONE',  ( -16.97683809663752186, 66.05000000001157900, -56.12074346632790878 ) ) ;
#31404 = AXIS2_PLACEMENT_3D ( 'NONE', #87623, #122931, #145038 ) ;
#31405 = AXIS2_PLACEMENT_3D ( 'NONE', #42894, #235942, #136846 ) ;
#31406 = ORIENTED_EDGE ( 'NONE', *, *, #235106, .T. ) ;
#31407 = DIRECTION ( 'NONE',  ( 0.000000000000000000, 0.2128009952263604510, -0.9770955615653315052 ) ) ;
#31409 = ORIENTED_EDGE ( 'NONE', *, *, #168829, .T. ) ;
#31408 = DIRECTION ( 'NONE',  ( 1.000000000000000000, 0.000000000000000000, 0.000000000000000000 ) ) ;
#31410 = CYLINDRICAL_SURFACE ( 'NONE', #109004, 0.1000000000000013933 ) ;
#31411 = ADVANCED_FACE ( 'NONE', ( #99061 ), #160380, .F. ) ;
#31412 = FACE_OUTER_BOUND ( 'NONE', #63767, .T. ) ;
#31413 = AXIS2_PLACEMENT_3D ( 'NONE', #146385, #241654, #63009 ) ;
#31414 = ORIENTED_EDGE ( 'NONE', *, *, #76410, .F. ) ;
#31415 = CARTESIAN_POINT ( 'NONE',  ( 21.05000000000000071, 76.00000000001126921, -203.5231074845248997 ) ) ;
#31416 = ADVANCED_FACE ( 'NONE', ( #198187 ), #219026, .T. ) ;
#31417 = CARTESIAN_POINT ( 'NONE',  ( -21.05000000000000071, 69.74218538953603286, -136.6208977758331287 ) ) ;
#31418 = ADVANCED_FACE ( 'NONE', ( #123799, #22147 ), #122522, .F. ) ;
#31419 = FACE_OUTER_BOUND ( 'NONE', #114338, .T. ) ;
#31420 = DIRECTION ( 'NONE',  ( 0.000000000000000000, 0.2617529984165152257, 0.9651348961777124202 ) ) ;
#31421 = AXIS2_PLACEMENT_3D ( 'NONE', #131427, #210974, #191444 ) ;
#31422 = VERTEX_POINT ( 'NONE', #202047 ) ;
#31423 = CARTESIAN_POINT ( 'NONE',  ( -21.05000000000000071, 1.115600667400684642E-11, -134.0000000000000000 ) ) ;
#31424 = CARTESIAN_POINT ( 'NONE',  ( -23.15000000000000213, 76.00000000001156764, -56.64810748452432421 ) ) ;
#31425 = EDGE_CURVE ( 'NONE', #5367, #52869, #137050, .T. ) ;
#31426 = DIRECTION ( 'NONE',  ( -1.020425574104004196E-15, 0.000000000000000000, -1.000000000000000000 ) ) ;
#31427 = VERTEX_POINT ( 'NONE', #183768 ) ;
#31428 = AXIS2_PLACEMENT_3D ( 'NONE', #188739, #33570, #113061 ) ;
#31429 = ORIENTED_EDGE ( 'NONE', *, *, #116822, .F. ) ;
#31430 = EDGE_CURVE ( 'NONE', #167819, #139486, #106492, .T. ) ;
#31431 = ADVANCED_FACE ( 'NONE', ( #203333 ), #40441, .F. ) ;
#31432 = LINE ( 'NONE', #91376, #221416 ) ;
#31433 = DIRECTION ( 'NONE',  ( 0.000000000000000000, -0.008583690987162452199, -0.9999631594459053030 ) ) ;
#31434 = LINE ( 'NONE', #62518, #81964 ) ;
#31435 = CARTESIAN_POINT ( 'NONE',  ( -23.15000000000000213, 11.75000000001115907, -127.1583993101029790 ) ) ;
#31437 = CARTESIAN_POINT ( 'NONE',  ( 22.49999999999999645, -2.392305309346458575, -189.5981695081429450 ) ) ;
#31436 = DIRECTION ( 'NONE',  ( -1.000000000000000000, -0.000000000000000000, -0.000000000000000000 ) ) ;
#31438 = DIRECTION ( 'NONE',  ( 0.000000000000000000, 0.8660254037844378194, 0.5000000000000016653 ) ) ;
#31439 = CARTESIAN_POINT ( 'NONE',  ( 21.05000000000000071, 85.40000000001262492, -193.6291383618718385 ) ) ;
#31440 = CARTESIAN_POINT ( 'NONE',  ( -20.65000000000000568, 65.69159657275406516, -213.8343546826533839 ) ) ;
#31441 = EDGE_LOOP ( 'NONE', ( #123018, #62527, #193804, #54241 ) ) ;
#31442 = AXIS2_PLACEMENT_3D ( 'NONE', #65281, #144801, #43162 ) ;
#31444 = ORIENTED_EDGE ( 'NONE', *, *, #135373, .F. ) ;
#31443 = DIRECTION ( 'NONE',  ( 0.000000000000000000, 0.000000000000000000, -1.000000000000000000 ) ) ;
#31445 = VECTOR ( 'NONE', #121897, 1000.000000000000000 ) ;
#31446 = CARTESIAN_POINT ( 'NONE',  ( 21.08035267497491105, 69.66829316022936780, -170.1057961093005417 ) ) ;
#31447 = LINE ( 'NONE', #113514, #116036 ) ;
#31449 = CARTESIAN_POINT ( 'NONE',  ( 20.94999999999999929, 65.70729864260954400, -30.56574559737246233 ) ) ;
#31448 = DIRECTION ( 'NONE',  ( 5.421010862427553724E-16, -0.4721928772777317374, -0.8814952561688446098 ) ) ;
#31450 = EDGE_CURVE ( 'NONE', #156427, #75842, #248181, .T. ) ;
#31451 = ORIENTED_EDGE ( 'NONE', *, *, #85489, .F. ) ;
#31452 = CARTESIAN_POINT ( 'NONE',  ( -16.88593481969334320, 66.04943990992768477, -115.6712352275798708 ) ) ;
#31454 = EDGE_CURVE ( 'NONE', #79646, #68928, #60712, .T. ) ;
#31453 = CARTESIAN_POINT ( 'NONE',  ( -20.94999999999999929, 87.48912529308852015, -173.1231074845242688 ) ) ;
#31455 = CARTESIAN_POINT ( 'NONE',  ( -21.05000000000000071, 69.45934304831071415, -102.9231074845243512 ) ) ;
#31456 = CARTESIAN_POINT ( 'NONE',  ( 22.50014994444026328, 12.60373254347212679, -223.3361492492176126 ) ) ;
#31457 = ORIENTED_EDGE ( 'NONE', *, *, #213084, .F. ) ;
#31458 = VERTEX_POINT ( 'NONE', #126355 ) ;
#31459 = ADVANCED_FACE ( 'NONE', ( #28599 ), #135739, .T. ) ;
#31460 = CARTESIAN_POINT ( 'NONE',  ( 23.14999999999999503, 11.65000000000000746, -26.48519422934606027 ) ) ;
#31461 = ORIENTED_EDGE ( 'NONE', *, *, #125284, .F. ) ;
#31462 = DIRECTION ( 'NONE',  ( 0.000000000000000000, -0.8660254037844343777, 0.5000000000000074385 ) ) ;
#31463 = DIRECTION ( 'NONE',  ( -1.000000000000000000, 0.000000000000000000, -0.000000000000000000 ) ) ;
#31464 = CARTESIAN_POINT ( 'NONE',  ( 21.05000000000000071, 8.776282648982402179, -142.4875923785201053 ) ) ;
#31465 = AXIS2_PLACEMENT_3D ( 'NONE', #134034, #96183, #175761 ) ;
#31466 = CARTESIAN_POINT ( 'NONE',  ( 21.00000000000000000, 6.239477252822119624, 11.95447128030241224 ) ) ;
#31467 = ORIENTED_EDGE ( 'NONE', *, *, #46531, .T. ) ;
#31468 = CARTESIAN_POINT ( 'NONE',  ( -23.25000000000000355, 14.17280543801757986, -210.8598471598932349 ) ) ;
#31469 = DIRECTION ( 'NONE',  ( -0.8660254037843529984, 0.4563037333032838316, 0.2044184506683135449 ) ) ;
#31470 = CARTESIAN_POINT ( 'NONE',  ( 19.97071067811865674, 11.72071067811866385, -24.70857864376269575 ) ) ;
#31471 = EDGE_CURVE ( 'NONE', #14418, #129536, #84615, .T. ) ;
#31472 = DIRECTION ( 'NONE',  ( 0.000000000000000000, -6.467318590049456648E-15, 1.000000000000000000 ) ) ;
#31473 = DIRECTION ( 'NONE',  ( -1.000000000000000000, 2.952720810173289112E-16, 2.061873921506763405E-30 ) ) ;
#31474 = CARTESIAN_POINT ( 'NONE',  ( 23.50000000000005684, 76.00000000001119815, -36.02310748452479316 ) ) ;
#31475 = CARTESIAN_POINT ( 'NONE',  ( -23.49999999999994316, 74.26359666348515987, -47.54092689884382850 ) ) ;
#31476 = EDGE_CURVE ( 'NONE', #156062, #91225, #187634, .T. ) ;
#31477 = VERTEX_POINT ( 'NONE', #209751 ) ;
#31479 = CARTESIAN_POINT ( 'NONE',  ( 20.04999999999999716, 8.750000000011173285, -180.1499999999999773 ) ) ;
#31478 = CARTESIAN_POINT ( 'NONE',  ( 13.99999999999999822, 62.10905854918434699, -217.1108499610991203 ) ) ;
#31480 = ORIENTED_EDGE ( 'NONE', *, *, #222878, .F. ) ;
#31482 = ORIENTED_EDGE ( 'NONE', *, *, #148751, .F. ) ;
#31481 = CYLINDRICAL_SURFACE ( 'NONE', #231587, 0.1000000000000028644 ) ;
#31483 = ORIENTED_EDGE ( 'NONE', *, *, #2486, .T. ) ;
#31484 = CIRCLE ( 'NONE', #64752, 0.1000000000000043771 ) ;
#31485 = CARTESIAN_POINT ( 'NONE',  ( -20.85000000000000142, 11.75000000001115197, -60.21613433702190576 ) ) ;
#31486 = CARTESIAN_POINT ( 'NONE',  ( 12.30626653967341788, 66.64320997496639620, -152.8182809759105112 ) ) ;
#31487 = CARTESIAN_POINT ( 'NONE',  ( 18.49999999999999289, 65.79142135624907439, -78.37310748452439668 ) ) ;
#31488 = CARTESIAN_POINT ( 'NONE',  ( 20.95429693346638800, 65.45669512011652103, -128.9622249462114496 ) ) ;
#31489 = EDGE_LOOP ( 'NONE', ( #11122, #167824, #195171, #134472, #74835 ) ) ;
#31490 = EDGE_CURVE ( 'NONE', #4950, #99917, #25984, .T. ) ;
#31491 = CARTESIAN_POINT ( 'NONE',  ( 21.05000000000000071, 69.52293297888793688, -203.4231074845244223 ) ) ;
#31492 = CARTESIAN_POINT ( 'NONE',  ( 21.14999999999999858, 1.115600667400684642E-11, -127.4593430482987912 ) ) ;
#31493 = EDGE_CURVE ( 'NONE', #102331, #56430, #248880, .T. ) ;
#31494 = ORIENTED_EDGE ( 'NONE', *, *, #18813, .T. ) ;
#31495 = CARTESIAN_POINT ( 'NONE',  ( -16.90128866880175806, 9.953795777214113016, -154.8626761833886576 ) ) ;
#31496 = EDGE_CURVE ( 'NONE', #88400, #205142, #85913, .T. ) ;
#31498 = CIRCLE ( 'NONE', #35586, 12.77500000000000036 ) ;
#31497 = CARTESIAN_POINT ( 'NONE',  ( -18.59999999999999787, 85.50000000001189449, -94.92310748452425173 ) ) ;
#31499 = ORIENTED_EDGE ( 'NONE', *, *, #49651, .F. ) ;
#31501 = DIRECTION ( 'NONE',  ( 0.000000000000000000, 0.000000000000000000, -1.000000000000000000 ) ) ;
#31500 = AXIS2_PLACEMENT_3D ( 'NONE', #86935, #88218, #109085 ) ;
#31502 = CIRCLE ( 'NONE', #18976, 4.099999999999992539 ) ;
#31503 = ADVANCED_FACE ( 'NONE', ( #8976 ), #130191, .F. ) ;
#31504 = ORIENTED_EDGE ( 'NONE', *, *, #15751, .T. ) ;
#31505 = CARTESIAN_POINT ( 'NONE',  ( 18.50000000000000000, -9.419209763398095347, -141.2477694627589244 ) ) ;
#31508 = EDGE_CURVE ( 'NONE', #174819, #151535, #50758, .T. ) ;
#31507 = EDGE_CURVE ( 'NONE', #256663, #97347, #110642, .T. ) ;
#31506 = ORIENTED_EDGE ( 'NONE', *, *, #160971, .T. ) ;
#31509 = LINE ( 'NONE', #34080, #42693 ) ;
#31510 = CARTESIAN_POINT ( 'NONE',  ( 20.85000000106584750, 64.25000000001175238, -76.36760282805070688 ) ) ;
#31511 = CARTESIAN_POINT ( 'NONE',  ( -23.25000000000000000, 6.982009704867601307, -137.6961521182563217 ) ) ;
#31512 = CARTESIAN_POINT ( 'NONE',  ( -21.05000000000000071, -1.162701749938009677, -8.000000000000000000 ) ) ;
#31513 = CARTESIAN_POINT ( 'NONE',  ( 21.05000000000000071, 67.32778804267617545, -235.8813018063200388 ) ) ;
#31514 = CARTESIAN_POINT ( 'NONE',  ( 22.39999999999999503, 76.00000000001200817, -110.8138870828976934 ) ) ;
#31515 = CARTESIAN_POINT ( 'NONE',  ( -20.64999999999999858, 71.65000000001187175, -90.77310748452434552 ) ) ;
#31517 = ORIENTED_EDGE ( 'NONE', *, *, #73263, .T. ) ;
#31516 = ADVANCED_FACE ( 'NONE', ( #5088 ), #229322, .T. ) ;
#31519 = EDGE_CURVE ( 'NONE', #48993, #185664, #70268, .T. ) ;
#31518 = DIRECTION ( 'NONE',  ( 1.000000000000000000, 0.000000000000000000, 0.000000000000000000 ) ) ;
#31520 = AXIS2_PLACEMENT_3D ( 'NONE', #54290, #90855, #133838 ) ;
#31521 = EDGE_LOOP ( 'NONE', ( #100059, #5867, #129879, #236300 ) ) ;
#31524 =( BOUNDED_SURFACE ( )  B_SPLINE_SURFACE ( 3, 2, ( 
 ( #38457, #234080, #213228 ),
 ( #172886, #252354, #214517 ),
 ( #76288, #37196, #235364 ),
 ( #112864, #55417, #72469 ) ),
 .UNSPECIFIED., .F., .F., .T. ) 
 B_SPLINE_SURFACE_WITH_KNOTS ( ( 4, 4 ),
 ( 3, 3 ),
 ( 3.658908243880901523, 4.712388980384689674 ),
 ( 0.000000000000000000, 1.000000000000000000 ),
 .UNSPECIFIED. ) 
 GEOMETRIC_REPRESENTATION_ITEM ( )  RATIONAL_B_SPLINE_SURFACE ( (
 ( 1.000000000000000000, 0.8984936768950559927, 1.000000000000000000),
 ( 1.000000000000000000, 0.8646876308615097928, 1.000000000000000000),
 ( 1.000000000000000000, 0.7953136715913377008, 1.000000000000000000),
 ( 1.000000000000000000, 0.7071067811864985009, 1.000000000000000000) ) ) 
 REPRESENTATION_ITEM ( '' )  SURFACE ( )  );
#31523 = CARTESIAN_POINT ( 'NONE',  ( -23.25000000000000000, 8.809961202382810441, -241.4517562488062481 ) ) ;
#31522 = CARTESIAN_POINT ( 'NONE',  ( -20.54999999999999716, -9.399999999988846611, -157.6060308773475924 ) ) ;
#31525 = COLOUR_RGB ( '', 0.31764706, 0.68627451, 0.89019608) ;
#31526 = ORIENTED_EDGE ( 'NONE', *, *, #238961, .T. ) ;
#31527 = CARTESIAN_POINT ( 'NONE',  ( 23.24999999999999645, 76.00000000001244871, -170.0231074845243597 ) ) ;
#31528 = CIRCLE ( 'NONE', #231409, 4.099999999999992539 ) ;
#31529 = FACE_OUTER_BOUND ( 'NONE', #217209, .T. ) ;
#31530 = DIRECTION ( 'NONE',  ( 0.000000000000000000, 0.2617529984165152257, 0.9651348961777124202 ) ) ;
#31531 = ADVANCED_FACE ( 'NONE', ( #144621 ), #65098, .T. ) ;
#31532 = DIRECTION ( 'NONE',  ( 0.000000000000000000, 0.000000000000000000, -1.000000000000000000 ) ) ;
#31533 = EDGE_LOOP ( 'NONE', ( #189331, #127851 ) ) ;
#31535 = VERTEX_POINT ( 'NONE', #45539 ) ;
#31534 = DIRECTION ( 'NONE',  ( -1.000000000000000000, 0.000000000000000000, 0.000000000000000000 ) ) ;
#31536 = AXIS2_PLACEMENT_3D ( 'NONE', #84966, #8047, #164552 ) ;
#31537 = EDGE_CURVE ( 'NONE', #167022, #109890, #14411, .T. ) ;
#31538 = TOROIDAL_SURFACE ( 'NONE', #152333, 11.65000000000000036, 0.1000000000000000056 ) ;
#31540 = CARTESIAN_POINT ( 'NONE',  ( 22.39999999999999503, 76.10085836911117951, -181.7726746080137445 ) ) ;
#31539 = DIRECTION ( 'NONE',  ( -1.000000000000000000, -0.000000000000000000, -0.000000000000000000 ) ) ;
#31541 = CIRCLE ( 'NONE', #27446, 0.09999999999998898659 ) ;
#31542 = VECTOR ( 'NONE', #120140, 1000.000000000000000 ) ;
#31543 = EDGE_CURVE ( 'NONE', #163251, #25250, #176895, .T. ) ;
#31545 = ORIENTED_EDGE ( 'NONE', *, *, #205034, .T. ) ;
#31544 = DIRECTION ( 'NONE',  ( 0.000000000000000000, 6.938893903907270030E-14, 1.000000000000000000 ) ) ;
#31546 = EDGE_LOOP ( 'NONE', ( #6875, #117031, #418 ) ) ;
#31547 = TOROIDAL_SURFACE ( 'NONE', #243878, 4.149999999999999467, 0.1000000000000000056 ) ;
#31548 = DIRECTION ( 'NONE',  ( 1.000000000000000000, -1.836970198721029934E-16, -1.282749433769087582E-30 ) ) ;
#31549 = ORIENTED_EDGE ( 'NONE', *, *, #96771, .T. ) ;
#31550 = FACE_OUTER_BOUND ( 'NONE', #68171, .T. ) ;
#31551 = EDGE_LOOP ( 'NONE', ( #171014, #1988, #188610, #169109 ) ) ;
#31552 = VECTOR ( 'NONE', #72139, 1000.000000000000114 ) ;
#31554 = EDGE_CURVE ( 'NONE', #181206, #208002, #235145, .T. ) ;
#31553 = CARTESIAN_POINT ( 'NONE',  ( -18.45140287520618116, -9.486077739518409047, -107.1405231266861620 ) ) ;
#31555 = CARTESIAN_POINT ( 'NONE',  ( 22.50000000000000000, 7.551210502620180343, -199.2530827308407027 ) ) ;
#31556 = AXIS2_PLACEMENT_3D ( 'NONE', #186657, #228343, #210068 ) ;
#31558 = ORIENTED_EDGE ( 'NONE', *, *, #190035, .T. ) ;
#31557 = VECTOR ( 'NONE', #57339, 1000.000000000000114 ) ;
#31559 = CARTESIAN_POINT ( 'NONE',  ( -20.85000000000000142, -0.3238857010591806307, -100.4575895893140256 ) ) ;
#31560 = EDGE_CURVE ( 'NONE', #173700, #154701, #51928, .T. ) ;
#31561 = ORIENTED_EDGE ( 'NONE', *, *, #193042, .F. ) ;
#31562 = DIRECTION ( 'NONE',  ( 0.000000000000000000, 0.000000000000000000, -1.000000000000000000 ) ) ;
#31563 = VERTEX_POINT ( 'NONE', #71545 ) ;
#31564 = ORIENTED_EDGE ( 'NONE', *, *, #94110, .T. ) ;
#31565 = CARTESIAN_POINT ( 'NONE',  ( 20.13684514580103269, 18.79075242197309947, -229.2072313918904456 ) ) ;
#31566 = ORIENTED_EDGE ( 'NONE', *, *, #25457, .F. ) ;
#31567 = EDGE_CURVE ( 'NONE', #79398, #98192, #174530, .T. ) ;
#31568 = EDGE_LOOP ( 'NONE', ( #35755, #188677, #31885 ) ) ;
#31570 = ORIENTED_EDGE ( 'NONE', *, *, #154558, .F. ) ;
#31569 = CARTESIAN_POINT ( 'NONE',  ( 22.59999999999999432, 25.98655542988603173, -254.2226763854395983 ) ) ;
#31571 = ORIENTED_EDGE ( 'NONE', *, *, #195381, .T. ) ;
#31572 = AXIS2_PLACEMENT_3D ( 'NONE', #177448, #196963, #237394 ) ;
#31573 = CARTESIAN_POINT ( 'NONE',  ( -21.14999999999999858, 1.115600667400684642E-11, -155.8504291924551808 ) ) ;
#31574 = EDGE_LOOP ( 'NONE', ( #167597, #3384, #152882, #226446 ) ) ;
#31575 = AXIS2_PLACEMENT_3D ( 'NONE', #131925, #211464, #210193 ) ;
#31578 = VERTEX_POINT ( 'NONE', #212333 ) ;
#31577 = EDGE_LOOP ( 'NONE', ( #10124, #54533, #177097, #236438 ) ) ;
#31576 = DIRECTION ( 'NONE',  ( -0.000000000000000000, 0.1350103645451904977, 0.9908441862701597991 ) ) ;
#31579 = CARTESIAN_POINT ( 'NONE',  ( -20.00857864376270001, 9.250000000011157297, -179.8499999999999943 ) ) ;
#31580 = ORIENTED_EDGE ( 'NONE', *, *, #200676, .T. ) ;
#31581 = EDGE_CURVE ( 'NONE', #144320, #234918, #160342, .T. ) ;
#31582 = CIRCLE ( 'NONE', #64854, 0.09999999999999939493 ) ;
#31583 = CARTESIAN_POINT ( 'NONE',  ( 23.15000000000000213, 86.45856254523212669, -209.4679346046102921 ) ) ;
#31584 = ORIENTED_EDGE ( 'NONE', *, *, #141221, .F. ) ;
#31585 = DIRECTION ( 'NONE',  ( 1.186688945009009831E-16, 0.4088369013363281068, -0.9126074666063770380 ) ) ;
#31587 = ORIENTED_EDGE ( 'NONE', *, *, #79568, .T. ) ;
#31586 = DIRECTION ( 'NONE',  ( -1.000000000000000000, 0.000000000000000000, -0.000000000000000000 ) ) ;
#31588 = CYLINDRICAL_SURFACE ( 'NONE', #92247, 0.5000000000000004441 ) ;
#31589 = ORIENTED_EDGE ( 'NONE', *, *, #145470, .F. ) ;
#31591 = VECTOR ( 'NONE', #156085, 1000.000000000000000 ) ;
#31590 = CARTESIAN_POINT ( 'NONE',  ( 21.05000000000000071, 65.27628318601222190, -95.42870824864037615 ) ) ;
#31592 = CARTESIAN_POINT ( 'NONE',  ( 23.24999999999999289, 80.15000000001268177, -203.5231074845243313 ) ) ;
#31593 = CIRCLE ( 'NONE', #85679, 0.09999999999998898659 ) ;
#31594 = EDGE_LOOP ( 'NONE', ( #128548, #95649, #132110, #51705 ) ) ;
#31595 = DIRECTION ( 'NONE',  ( -1.000000000000000000, 0.000000000000000000, -0.000000000000000000 ) ) ;
#31596 = DIRECTION ( 'NONE',  ( -1.000000000000000000, 0.000000000000000000, 0.000000000000000000 ) ) ;
#31597 = AXIS2_PLACEMENT_3D ( 'NONE', #75966, #91671, #252024 ) ;
#31598 = VERTEX_POINT ( 'NONE', #170673 ) ;
#31600 = ORIENTED_EDGE ( 'NONE', *, *, #13639, .F. ) ;
#31599 = LINE ( 'NONE', #108533, #84710 ) ;
#31601 = DIRECTION ( 'NONE',  ( -1.000000000000000000, -1.116774769942150098E-16, 0.000000000000000000 ) ) ;
#31603 = VERTEX_POINT ( 'NONE', #171945 ) ;
#31602 = ORIENTED_EDGE ( 'NONE', *, *, #165324, .F. ) ;
#31604 = ORIENTED_EDGE ( 'NONE', *, *, #113268, .T. ) ;
#31605 = DIRECTION ( 'NONE',  ( 0.000000000000000000, -0.8814952561688437216, 0.4721928772777334582 ) ) ;
#31606 = VERTEX_POINT ( 'NONE', #214873 ) ;
#31607 = ORIENTED_EDGE ( 'NONE', *, *, #34149, .F. ) ;
#31608 = DIRECTION ( 'NONE',  ( 0.000000000000000000, 0.000000000000000000, -1.000000000000000000 ) ) ;
#31609 = CIRCLE ( 'NONE', #64878, 0.1000000000000008937 ) ;
#31610 = VERTEX_POINT ( 'NONE', #57057 ) ;
#31611 = DIRECTION ( 'NONE',  ( 2.465190328815661345E-32, -0.8814952561688430555, 0.4721928772777344574 ) ) ;
#31612 = LINE ( 'NONE', #207664, #123209 ) ;
#31613 = ORIENTED_EDGE ( 'NONE', *, *, #248898, .T. ) ;
#31614 = EDGE_CURVE ( 'NONE', #168251, #47203, #96199, .T. ) ;
#31615 = ORIENTED_EDGE ( 'NONE', *, *, #154307, .F. ) ;
#31616 = DIRECTION ( 'NONE',  ( 0.000000000000000000, -0.7397360091702647189, -0.6728971962616949742 ) ) ;
#31617 = VERTEX_POINT ( 'NONE', #132797 ) ;
#31618 = CIRCLE ( 'NONE', #123353, 11.65000000000000036 ) ;
#31619 = AXIS2_PLACEMENT_3D ( 'NONE', #32297, #109225, #188769 ) ;
#31620 = CIRCLE ( 'NONE', #60792, 7.800000000000001599 ) ;
#31621 = FACE_OUTER_BOUND ( 'NONE', #250605, .T. ) ;
#31622 = ORIENTED_EDGE ( 'NONE', *, *, #150792, .F. ) ;
#31623 = EDGE_CURVE ( 'NONE', #98621, #251099, #214299, .T. ) ;
#31624 = DIRECTION ( 'NONE',  ( 1.000000000000000000, 0.000000000000000000, 0.000000000000000000 ) ) ;
#31626 = ORIENTED_EDGE ( 'NONE', *, *, #244847, .T. ) ;
#31625 = DIRECTION ( 'NONE',  ( 1.000000000000000000, 0.000000000000000000, 0.000000000000000000 ) ) ;
#31627 = CARTESIAN_POINT ( 'NONE',  ( 12.25000000000000000, 9.350000000011140955, -150.7500000000000284 ) ) ;
#31628 = DIRECTION ( 'NONE',  ( 0.000000000000000000, -4.440892098500570153E-15, 1.000000000000000000 ) ) ;
#31629 = CARTESIAN_POINT ( 'NONE',  ( 20.95265033839679347, 65.48774916754493347, -128.9573437284944077 ) ) ;
#31630 = CARTESIAN_POINT ( 'NONE',  ( -20.64999999999999858, 1.115600667400684642E-11, -46.47500000000000142 ) ) ;
#31631 = FACE_OUTER_BOUND ( 'NONE', #201524, .T. ) ;
#31632 = ADVANCED_FACE ( 'NONE', ( #131487 ), #93665, .T. ) ;
#31633 = CARTESIAN_POINT ( 'NONE',  ( 19.75857864376268935, 11.65000000001115943, -58.25000000000000000 ) ) ;
#31634 = CARTESIAN_POINT ( 'NONE',  ( 20.94999999999999929, 76.00000000001213607, -136.5231074845243313 ) ) ;
#31635 = LINE ( 'NONE', #250634, #170052 ) ;
#31636 = CARTESIAN_POINT ( 'NONE',  ( -20.85000000000000142, 46.01276039807270024, -256.6622985126337539 ) ) ;
#31637 = CARTESIAN_POINT ( 'NONE',  ( 21.72449340488910607, 20.13867536412185189, -229.0352267540020819 ) ) ;
#31638 = AXIS2_PLACEMENT_3D ( 'NONE', #197420, #80011, #117880 ) ;
#31639 = EDGE_CURVE ( 'NONE', #171197, #231120, #175773, .T. ) ;
#31640 = EDGE_LOOP ( 'NONE', ( #205707, #45684, #85234, #101435, #217644 ) ) ;
#31641 = EDGE_CURVE ( 'NONE', #20026, #78455, #181178, .T. ) ;
#31642 = VERTEX_POINT ( 'NONE', #173236 ) ;
#31643 = AXIS2_PLACEMENT_3D ( 'NONE', #58329, #239568, #123468 ) ;
#31644 = ORIENTED_EDGE ( 'NONE', *, *, #125080, .F. ) ;
#31645 = ADVANCED_FACE ( 'NONE', ( #113208 ), #235711, .F. ) ;
#31646 = VERTEX_POINT ( 'NONE', #91081 ) ;
#31647 = DIRECTION ( 'NONE',  ( -1.000000000000000000, 0.000000000000000000, 0.000000000000000000 ) ) ;
#31648 = CARTESIAN_POINT ( 'NONE',  ( -20.85000000000000142, 45.93315328338058379, -256.6017782078560003 ) ) ;
#31649 = ADVANCED_FACE ( 'NONE', ( #54515 ), #53242, .T. ) ;
#31651 = CARTESIAN_POINT ( 'NONE',  ( -20.54999999999999716, 74.00000000001205080, -123.2984855617622060 ) ) ;
#31650 = DIRECTION ( 'NONE',  ( -0.8191520442889914655, 0.5735764363510466035, 0.000000000000000000 ) ) ;
#31652 = ORIENTED_EDGE ( 'NONE', *, *, #46954, .F. ) ;
#31653 = ORIENTED_EDGE ( 'NONE', *, *, #74838, .T. ) ;
#31654 = CARTESIAN_POINT ( 'NONE',  ( 18.39999999999999858, -9.499999999988844479, -40.53206939669966857 ) ) ;
#31655 = EDGE_CURVE ( 'NONE', #225564, #139998, #222640, .T. ) ;
#31656 = CARTESIAN_POINT ( 'NONE',  ( 18.51697539158856642, 10.31565961587946134, -173.0364194119178478 ) ) ;
#31657 = LINE ( 'NONE', #53753, #62326 ) ;
#31658 = ORIENTED_EDGE ( 'NONE', *, *, #132024, .T. ) ;
#31659 = ORIENTED_EDGE ( 'NONE', *, *, #256937, .F. ) ;
#31660 = AXIS2_PLACEMENT_3D ( 'NONE', #242912, #104655, #142521 ) ;
#31661 = DIRECTION ( 'NONE',  ( -1.000000000000000000, 7.304098846218133681E-16, -4.217023435051677994E-16 ) ) ;
#31662 = DIRECTION ( 'NONE',  ( 1.000000000000000000, 0.000000000000000000, 0.000000000000000000 ) ) ;
#31663 = CARTESIAN_POINT ( 'NONE',  ( -18.46902351632712680, 78.23792127434718680, -231.6013883309054222 ) ) ;
#31665 = ORIENTED_EDGE ( 'NONE', *, *, #75390, .F. ) ;
#31664 = DIRECTION ( 'NONE',  ( 0.000000000000000000, 0.2128009952263602012, -0.9770955615653315052 ) ) ;
#31666 = ADVANCED_FACE ( 'NONE', ( #92356 ), #35446, .T. ) ;
#31667 = DIRECTION ( 'NONE',  ( 0.000000000000000000, 6.853228547068871147E-15, -1.000000000000000000 ) ) ;
#31668 = CARTESIAN_POINT ( 'NONE',  ( -23.15000000000000213, 0.000000000000000000, -33.50000000000000000 ) ) ;
#31669 = CARTESIAN_POINT ( 'NONE',  ( 20.94999999999999574, -11.74999999998883560, -136.9000000000000341 ) ) ;
#31670 = CARTESIAN_POINT ( 'NONE',  ( 18.45036689428371446, 85.49018414334094018, -96.01041165703843205 ) ) ;
#31671 = VERTEX_POINT ( 'NONE', #154935 ) ;
#31672 = CARTESIAN_POINT ( 'NONE',  ( -18.59999999999999787, 18.24178995542692050, -237.7003448530951459 ) ) ;
#31674 = EDGE_CURVE ( 'NONE', #144670, #23868, #126990, .T. ) ;
#31673 = CARTESIAN_POINT ( 'NONE',  ( -21.05000000000000071, 1.835341550224411922, -11.55515129256298046 ) ) ;
#31676 = CARTESIAN_POINT ( 'NONE',  ( -17.11825945287482753, 65.95000000001208207, -123.8731074845243683 ) ) ;
#31675 = CARTESIAN_POINT ( 'NONE',  ( -18.59999999999999787, 67.85909929089923764, -227.8797997985275856 ) ) ;
#31677 = CARTESIAN_POINT ( 'NONE',  ( -20.64999999999999858, 67.23127455305835554, -235.8551265064784559 ) ) ;
#31678 = CARTESIAN_POINT ( 'NONE',  ( -16.92280123533709713, 9.950000000011137047, -54.14936768591468308 ) ) ;
#31679 = VECTOR ( 'NONE', #190339, 1000.000000000000000 ) ;
#31680 = DIRECTION ( 'NONE',  ( -0.7071067811865475727, 0.7071067811865475727, 4.937700262164531476E-15 ) ) ;
#31681 = DIRECTION ( 'NONE',  ( 0.000000000000000000, 7.109473446599835262E-15, -1.000000000000000000 ) ) ;
#31682 = CARTESIAN_POINT ( 'NONE',  ( -23.25000000000000000, 0.000000000000000000, 0.000000000000000000 ) ) ;
#31683 = AXIS2_PLACEMENT_3D ( 'NONE', #248301, #227444, #110068 ) ;
#31684 = PLANE ( 'NONE',  #72660 ) ;
#31685 = AXIS2_PLACEMENT_3D ( 'NONE', #81689, #157456, #200400 ) ;
#31686 = ORIENTED_EDGE ( 'NONE', *, *, #16340, .F. ) ;
#31687 = VECTOR ( 'NONE', #7506, 999.9999999999998863 ) ;
#31688 = ORIENTED_EDGE ( 'NONE', *, *, #104620, .T. ) ;
#31690 = ORIENTED_EDGE ( 'NONE', *, *, #45837, .F. ) ;
#31689 = PRESENTATION_LAYER_ASSIGNMENT (  '', '', ( #239764 ) ) ;
#31691 = EDGE_CURVE ( 'NONE', #83686, #248838, #190196, .T. ) ;
#31692 = CARTESIAN_POINT ( 'NONE',  ( 21.00000000000000000, 9.750000000011153745, -112.7500000000000284 ) ) ;
#31693 = CARTESIAN_POINT ( 'NONE',  ( 20.99999999999997868, 7.128833340093095217, -233.7327013124392749 ) ) ;
#31694 = ORIENTED_EDGE ( 'NONE', *, *, #17871, .T. ) ;
#31695 = ORIENTED_EDGE ( 'NONE', *, *, #132319, .F. ) ;
#31696 = VERTEX_POINT ( 'NONE', #46180 ) ;
#31697 = CARTESIAN_POINT ( 'NONE',  ( -20.94999999999999929, 76.00000000001232081, -162.1231074845243540 ) ) ;
#31698 = VECTOR ( 'NONE', #26304, 1000.000000000000000 ) ;
#31699 = ORIENTED_EDGE ( 'NONE', *, *, #187916, .T. ) ;
#31700 = EDGE_CURVE ( 'NONE', #54936, #153680, #51947, .T. ) ;
#31701 = CARTESIAN_POINT ( 'NONE',  ( -21.44999999999999929, 53.03738849591485405, -234.3791188517465400 ) ) ;
#31702 = CIRCLE ( 'NONE', #223196, 0.1000000000000028644 ) ;
#31703 = CARTESIAN_POINT ( 'NONE',  ( -18.50000000000000000, 64.25000000001222134, -148.2731074845243882 ) ) ;
#31704 = DIRECTION ( 'NONE',  ( 0.000000000000000000, 0.1575844902526876978, 0.9875055080513731598 ) ) ;
#31705 = CYLINDRICAL_SURFACE ( 'NONE', #99915, 11.74999999999999112 ) ;
#31706 = DIRECTION ( 'NONE',  ( 0.000000000000000000, -1.000000000000000000, 0.000000000000000000 ) ) ;
#31709 = ORIENTED_EDGE ( 'NONE', *, *, #3338, .T. ) ;
#31708 = CARTESIAN_POINT ( 'NONE',  ( 21.30000000000002558, 68.29137419664525055, -231.9463301769586394 ) ) ;
#31707 = CIRCLE ( 'NONE', #219104, 0.1000000000000028644 ) ;
#31711 = DIRECTION ( 'NONE',  ( 1.000000000000000000, 0.000000000000000000, 0.000000000000000000 ) ) ;
#31710 = DIRECTION ( 'NONE',  ( -0.000000000000000000, -0.9651348961777157509, 0.2617529984165031243 ) ) ;
#31712 = CARTESIAN_POINT ( 'NONE',  ( -16.89268316805465986, 9.951721813253337601, -154.8557524785455541 ) ) ;
#31713 = ADVANCED_FACE ( 'NONE', ( #145273 ), #241664, .T. ) ;
#31714 = ORIENTED_EDGE ( 'NONE', *, *, #184789, .T. ) ;
#31715 = CARTESIAN_POINT ( 'NONE',  ( 15.74999999999999289, 66.65000000001207070, -120.0045385271217526 ) ) ;
#31716 = AXIS2_PLACEMENT_3D ( 'NONE', #208206, #187358, #247303 ) ;
#31717 = CARTESIAN_POINT ( 'NONE',  ( -21.37071067811865532, 8.070710678129811910, -54.75000000000000000 ) ) ;
#31718 = DIRECTION ( 'NONE',  ( -7.304098846218134667E-16, 1.000000000000000000, 6.982962677686267499E-15 ) ) ;
#31720 = ORIENTED_EDGE ( 'NONE', *, *, #100390, .T. ) ;
#31719 = AXIS2_PLACEMENT_3D ( 'NONE', #27464, #41871, #181383 ) ;
#31721 = EDGE_CURVE ( 'NONE', #172688, #105032, #97736, .T. ) ;
#31722 = CARTESIAN_POINT ( 'NONE',  ( -20.85000000000000142, 68.97833521811179480, -99.18954208262705663 ) ) ;
#31723 = EDGE_CURVE ( 'NONE', #42311, #77787, #85257, .T. ) ;
#31724 = CARTESIAN_POINT ( 'NONE',  ( 21.05000000000000071, 30.48950451747912993, -239.6099224343151946 ) ) ;
#31725 = ADVANCED_FACE ( 'NONE', ( #137883 ), #31170, .T. ) ;
#31726 = ORIENTED_EDGE ( 'NONE', *, *, #82426, .F. ) ;
#31727 = AXIS2_PLACEMENT_3D ( 'NONE', #72326, #129714, #207989 ) ;
#31728 = CARTESIAN_POINT ( 'NONE',  ( 18.54999999999999716, 8.750000000011182166, -76.25000000000004263 ) ) ;
#31729 = VECTOR ( 'NONE', #58942, 1000.000000000000000 ) ;
#31730 = EDGE_CURVE ( 'NONE', #184818, #159030, #164418, .T. ) ;
#31731 = DIRECTION ( 'NONE',  ( -1.000000000000000000, -1.646408749285562691E-14, 0.000000000000000000 ) ) ;
#31732 = FACE_OUTER_BOUND ( 'NONE', #167635, .T. ) ;
#31733 = VERTEX_POINT ( 'NONE', #5752 ) ;
#31734 = AXIS2_PLACEMENT_3D ( 'NONE', #10050, #89577, #187422 ) ;
#31735 = ORIENTED_EDGE ( 'NONE', *, *, #150494, .F. ) ;
#31736 = CARTESIAN_POINT ( 'NONE',  ( -21.04999999999994387, 76.00000000001119815, -36.02310748452479316 ) ) ;
#31737 = FACE_OUTER_BOUND ( 'NONE', #1358, .T. ) ;
#31738 = CARTESIAN_POINT ( 'NONE',  ( 20.94788355080264353, 65.69792220476374212, -164.5335554128461979 ) ) ;
#31739 = DIRECTION ( 'NONE',  ( 1.000000000000000000, 0.000000000000000000, 0.000000000000000000 ) ) ;
#31740 = CIRCLE ( 'NONE', #19821, 0.09999999999998715472 ) ;
#31742 = DIRECTION ( 'NONE',  ( 0.000000000000000000, 6.982962677686266711E-15, -1.000000000000000000 ) ) ;
#31741 = CARTESIAN_POINT ( 'NONE',  ( 21.15000000000005542, 76.00000000001119815, -3.123107484524795474 ) ) ;
#31743 = FACE_OUTER_BOUND ( 'NONE', #59184, .T. ) ;
#31744 = DIRECTION ( 'NONE',  ( 1.000000000000000000, 0.000000000000000000, 0.000000000000000000 ) ) ;
#31745 = CARTESIAN_POINT ( 'NONE',  ( -18.50000000000000000, 1.115600667400684642E-11, -134.0000000000000000 ) ) ;
#31746 = ORIENTED_EDGE ( 'NONE', *, *, #14166, .F. ) ;
#31747 = DIRECTION ( 'NONE',  ( -1.073024830501117725E-15, 6.982962677686266711E-15, -1.000000000000000000 ) ) ;
#31748 = EDGE_CURVE ( 'NONE', #230182, #21519, #18661, .T. ) ;
#31750 = EDGE_LOOP ( 'NONE', ( #136372, #240862, #62064, #221393 ) ) ;
#31749 = DIRECTION ( 'NONE',  ( 1.000000000000000000, 0.000000000000000000, 0.000000000000000000 ) ) ;
#31751 = CARTESIAN_POINT ( 'NONE',  ( 20.94999999999999929, -1.835341550224413698, -11.55515129256298046 ) ) ;
#31752 = DIRECTION ( 'NONE',  ( 0.000000000000000000, 0.9651348961777157509, -0.2617529984165031243 ) ) ;
#31753 = EDGE_CURVE ( 'NONE', #231369, #146114, #244377, .T. ) ;
#31754 = CARTESIAN_POINT ( 'NONE',  ( 20.99551997958312199, 11.75000000001053913, -194.1516591376895349 ) ) ;
#31756 = ORIENTED_EDGE ( 'NONE', *, *, #85209, .T. ) ;
#31755 = CARTESIAN_POINT ( 'NONE',  ( -15.75000000000000000, 62.53182050776837286, -217.4622410876595779 ) ) ;
#31757 = CARTESIAN_POINT ( 'NONE',  ( 22.39999999999999503, 0.09999999999999939493, 6.249999999999998224 ) ) ;
#31759 = EDGE_CURVE ( 'NONE', #75451, #52766, #98736, .T. ) ;
#31758 = DIRECTION ( 'NONE',  ( -0.7071067811865388020, 0.7071067811865561215, 0.000000000000000000 ) ) ;
#31760 = CARTESIAN_POINT ( 'NONE',  ( -20.94999999999999929, -1.162701749926853712, -41.50000000000000000 ) ) ;
#31761 = DIRECTION ( 'NONE',  ( -1.000000000000000000, -2.952720810173289112E-16, 0.000000000000000000 ) ) ;
#31762 = ORIENTED_EDGE ( 'NONE', *, *, #37549, .T. ) ;
#31763 = DIRECTION ( 'NONE',  ( -1.000000000000000000, 0.000000000000000000, 0.000000000000000000 ) ) ;
#31764 = CIRCLE ( 'NONE', #177504, 1.900000000000012790 ) ;
#31765 = VERTEX_POINT ( 'NONE', #93018 ) ;
#31766 = AXIS2_PLACEMENT_3D ( 'NONE', #42844, #201920, #59808 ) ;
#31767 = AXIS2_PLACEMENT_3D ( 'NONE', #87931, #228769, #110082 ) ;
#31768 = EDGE_CURVE ( 'NONE', #167923, #69945, #60341, .T. ) ;
#31769 = DIRECTION ( 'NONE',  ( 1.000000000000000000, 0.000000000000000000, 0.000000000000000000 ) ) ;
#31770 = VERTEX_POINT ( 'NONE', #250803 ) ;
#31771 = DIRECTION ( 'NONE',  ( 0.000000000000000000, 0.000000000000000000, 1.000000000000000000 ) ) ;
#31772 = VERTEX_POINT ( 'NONE', #149167 ) ;
#31773 = AXIS2_PLACEMENT_3D ( 'NONE', #200555, #103992, #46594 ) ;
#31774 = DIRECTION ( 'NONE',  ( 1.000000000000000000, 0.000000000000000000, 0.000000000000000000 ) ) ;
#31775 = FACE_OUTER_BOUND ( 'NONE', #175558, .T. ) ;
#31776 = DIRECTION ( 'NONE',  ( 1.000000000000000000, 0.000000000000000000, 0.000000000000000000 ) ) ;
#31777 = EDGE_LOOP ( 'NONE', ( #18284, #163471, #36846 ) ) ;
#31778 = AXIS2_PLACEMENT_3D ( 'NONE', #247122, #64644, #166351 ) ;
#31780 = AXIS2_PLACEMENT_3D ( 'NONE', #215772, #193669, #37176 ) ;
#31779 = CARTESIAN_POINT ( 'NONE',  ( -16.80621392010906945, 9.942202577507719852, -12.68959196541704060 ) ) ;
#31781 = EDGE_CURVE ( 'NONE', #132561, #144164, #81178, .T. ) ;
#31782 = CARTESIAN_POINT ( 'NONE',  ( 21.05000000000000071, 14.64166534854604507, -236.4381089660238331 ) ) ;
#31783 = AXIS2_PLACEMENT_3D ( 'NONE', #236313, #257112, #122811 ) ;
#31784 = CARTESIAN_POINT ( 'NONE',  ( -21.17356465864818560, 6.254644016943381679, -199.5365753680107161 ) ) ;
#31785 = CARTESIAN_POINT ( 'NONE',  ( 22.37643362114956247, 7.430040941609745708, -199.2804123294420720 ) ) ;
#31786 = CARTESIAN_POINT ( 'NONE',  ( -16.93301857435212199, 66.02369064527653109, -115.6373319133629423 ) ) ;
#31787 = ORIENTED_EDGE ( 'NONE', *, *, #27016, .T. ) ;
#31788 = DIRECTION ( 'NONE',  ( -1.000000000000000000, 0.000000000000000000, -0.000000000000000000 ) ) ;
#31789 = ORIENTED_EDGE ( 'NONE', *, *, #60657, .F. ) ;
#31791 = ORIENTED_EDGE ( 'NONE', *, *, #98055, .T. ) ;
#31790 = CARTESIAN_POINT ( 'NONE',  ( 20.84999999999998721, 10.33248238083634440, -106.0948465439131922 ) ) ;
#31792 = ORIENTED_EDGE ( 'NONE', *, *, #69145, .T. ) ;
#31793 = LINE ( 'NONE', #111301, #215456 ) ;
#31794 = EDGE_LOOP ( 'NONE', ( #234845, #21021, #37421, #161276 ) ) ;
#31795 = DIRECTION ( 'NONE',  ( 0.000000000000000000, -1.000000000000000000, 0.000000000000000000 ) ) ;
#31796 = DIRECTION ( 'NONE',  ( -1.000000000000000000, 0.000000000000000000, 0.000000000000000000 ) ) ;
#31797 = DIRECTION ( 'NONE',  ( 0.000000000000000000, 6.982962677686266711E-15, -1.000000000000000000 ) ) ;
#31799 = ORIENTED_EDGE ( 'NONE', *, *, #18710, .T. ) ;
#31798 = AXIS2_PLACEMENT_3D ( 'NONE', #15225, #230406, #235528 ) ;
#31800 = DIRECTION ( 'NONE',  ( -1.000000000000000000, 0.000000000000000000, -0.000000000000000000 ) ) ;
#31801 = CARTESIAN_POINT ( 'NONE',  ( -18.39999999999999858, -9.519327731081281385, -40.47297637655933045 ) ) ;
#31802 = ORIENTED_EDGE ( 'NONE', *, *, #187721, .T. ) ;
#31803 = EDGE_CURVE ( 'NONE', #40625, #88995, #89158, .T. ) ;
#31805 = ORIENTED_EDGE ( 'NONE', *, *, #163670, .T. ) ;
#31804 = CARTESIAN_POINT ( 'NONE',  ( 23.14999999999999503, 11.75000000001115552, -155.2500000000000284 ) ) ;
#31806 = LINE ( 'NONE', #69628, #194324 ) ;
#31807 = DIRECTION ( 'NONE',  ( 0.000000000000000000, 0.2617529984165152257, 0.9651348961777124202 ) ) ;
#31808 = EDGE_CURVE ( 'NONE', #152762, #76270, #118642, .T. ) ;
#31809 = AXIS2_PLACEMENT_3D ( 'NONE', #17050, #194412, #174878 ) ;
#31810 = VERTEX_POINT ( 'NONE', #227390 ) ;
#31811 = CARTESIAN_POINT ( 'NONE',  ( -20.54999999999999716, 7.533155231024652565, -235.5891828794142384 ) ) ;
#31813 = EDGE_CURVE ( 'NONE', #51771, #14172, #151961, .T. ) ;
#31812 = CARTESIAN_POINT ( 'NONE',  ( -12.25000000000000355, 66.65000000001207070, -120.0045385271217384 ) ) ;
#31814 = LINE ( 'NONE', #36952, #125725 ) ;
#31816 = EDGE_CURVE ( 'NONE', #11624, #33291, #101835, .T. ) ;
#31815 = ORIENTED_EDGE ( 'NONE', *, *, #160399, .T. ) ;
#31817 = CARTESIAN_POINT ( 'NONE',  ( -12.25000000000000178, 9.850000000011133849, -83.75000000000004263 ) ) ;
#31818 = CARTESIAN_POINT ( 'NONE',  ( -20.94999999999999929, 77.83534155023670564, -158.4679561919613491 ) ) ;
#31819 = DIRECTION ( 'NONE',  ( 0.000000000000000000, 1.000000000000000000, 0.000000000000000000 ) ) ;
#31820 = AXIS2_PLACEMENT_3D ( 'NONE', #66626, #144862, #202286 ) ;
#31821 = VECTOR ( 'NONE', #110873, 1000.000000000000000 ) ;
#31822 = EDGE_CURVE ( 'NONE', #153127, #49212, #22780, .T. ) ;
#31823 = EDGE_CURVE ( 'NONE', #173790, #239952, #190250, .T. ) ;
#31824 = ORIENTED_EDGE ( 'NONE', *, *, #209416, .F. ) ;
#31825 = CARTESIAN_POINT ( 'NONE',  ( 21.14999999999999858, 1.115600667400684642E-11, -93.95934304829877703 ) ) ;
#31826 = AXIS2_PLACEMENT_3D ( 'NONE', #219683, #137567, #58025 ) ;
#31827 = ORIENTED_EDGE ( 'NONE', *, *, #244084, .F. ) ;
#31828 = CARTESIAN_POINT ( 'NONE',  ( -22.10000000000000142, -11.65000000000000036, 32.89999999999999858 ) ) ;
#31829 = CYLINDRICAL_SURFACE ( 'NONE', #124996, 0.1000000000000028644 ) ;
#31831 = ORIENTED_EDGE ( 'NONE', *, *, #210993, .F. ) ;
#31830 = CARTESIAN_POINT ( 'NONE',  ( 19.58285714285715073, 10.38499851036257837, -141.6296846673899665 ) ) ;
#31832 = CARTESIAN_POINT ( 'NONE',  ( 21.05000000000000071, 85.00000000001207923, -126.6291383618717816 ) ) ;
#31833 = DIRECTION ( 'NONE',  ( 1.000000000000000000, 1.541880601228652843E-16, 2.878400969107353907E-16 ) ) ;
#31834 = FACE_OUTER_BOUND ( 'NONE', #69869, .T. ) ;
#31835 = CARTESIAN_POINT ( 'NONE',  ( -16.97683809663752186, 9.949999999999983302, -20.09763598180368405 ) ) ;
#31836 = CYLINDRICAL_SURFACE ( 'NONE', #72717, 0.09999999999999976963 ) ;
#31837 = CARTESIAN_POINT ( 'NONE',  ( -21.05000000000000071, -11.48912529306490349, -137.1000000000000227 ) ) ;
#31839 = EDGE_CURVE ( 'NONE', #240428, #33310, #185258, .T. ) ;
#31838 = CARTESIAN_POINT ( 'NONE',  ( 21.12757541349815682, 6.473380571262609351, -66.99483878419029281 ) ) ;
#31841 = ORIENTED_EDGE ( 'NONE', *, *, #132163, .T. ) ;
#31840 = DIRECTION ( 'NONE',  ( 0.7071067811865475727, 0.7071067811865475727, 4.937700262164531476E-15 ) ) ;
#31842 = EDGE_CURVE ( 'NONE', #224923, #15592, #72854, .T. ) ;
#31843 = CIRCLE ( 'NONE', #52644, 7.720710678118663850 ) ;
#31844 = CARTESIAN_POINT ( 'NONE',  ( -20.94999999999999929, -1.164121893230052995, -175.2148480855716173 ) ) ;
#31845 = CARTESIAN_POINT ( 'NONE',  ( -21.05000000000000071, 76.00000000001213607, -136.5231074845242745 ) ) ;
#31847 = ADVANCED_FACE ( 'NONE', ( #47452 ), #190873, .T. ) ;
#31846 = DIRECTION ( 'NONE',  ( 0.000000000000000000, -1.000000000000000000, -7.272083257015735086E-15 ) ) ;
#31848 = FACE_OUTER_BOUND ( 'NONE', #196067, .T. ) ;
#31849 = ORIENTED_EDGE ( 'NONE', *, *, #241026, .F. ) ;
#31850 = DIRECTION ( 'NONE',  ( 0.000000000000000000, -6.982962677686266711E-15, 1.000000000000000000 ) ) ;
#31851 = LINE ( 'NONE', #112650, #249094 ) ;
#31852 = TOROIDAL_SURFACE ( 'NONE', #52840, 11.65000000000000036, 0.1000000000000000056 ) ;
#31853 = EDGE_CURVE ( 'NONE', #200951, #121041, #107445, .T. ) ;
#31854 = ORIENTED_EDGE ( 'NONE', *, *, #175726, .F. ) ;
#31855 = CIRCLE ( 'NONE', #177616, 11.79999999999999005 ) ;
#31856 = VECTOR ( 'NONE', #91872, 1000.000000000000227 ) ;
#31857 = CYLINDRICAL_SURFACE ( 'NONE', #105981, 0.1000000000000028644 ) ;
#31858 = FACE_OUTER_BOUND ( 'NONE', #248081, .T. ) ;
#31859 = VERTEX_POINT ( 'NONE', #10932 ) ;
#31860 = DIRECTION ( 'NONE',  ( 0.000000000000000000, 0.000000000000000000, 1.000000000000000000 ) ) ;
#31861 = ORIENTED_EDGE ( 'NONE', *, *, #121046, .F. ) ;
#31862 = ADVANCED_FACE ( 'NONE', ( #8361 ), #167451, .F. ) ;
#31863 = LINE ( 'NONE', #12294, #204867 ) ;
#31865 = ORIENTED_EDGE ( 'NONE', *, *, #85173, .F. ) ;
#31864 = CARTESIAN_POINT ( 'NONE',  ( 18.60000000000000142, 85.48068669529106955, -129.5819923157664562 ) ) ;
#31866 = CARTESIAN_POINT ( 'NONE',  ( 23.14999999999999503, 69.35000000001228670, -157.7731074845243882 ) ) ;
#31867 = VERTEX_POINT ( 'NONE', #249544 ) ;
#31868 = CARTESIAN_POINT ( 'NONE',  ( -18.40000000000000213, 8.212522512469059066, -212.1579332307740344 ) ) ;
#31869 = ORIENTED_EDGE ( 'NONE', *, *, #179326, .F. ) ;
#31871 = EDGE_LOOP ( 'NONE', ( #149010, #149127, #9480, #240412 ) ) ;
#31870 = ORIENTED_EDGE ( 'NONE', *, *, #27236, .F. ) ;
#31872 = CARTESIAN_POINT ( 'NONE',  ( -23.25000000000000000, 11.75000000000000000, 11.75000000000000000 ) ) ;
#31874 = ORIENTED_EDGE ( 'NONE', *, *, #191260, .F. ) ;
#31873 = CARTESIAN_POINT ( 'NONE',  ( 15.74999999999999645, 9.350000000011133849, -50.01856895740262132 ) ) ;
#31875 = CARTESIAN_POINT ( 'NONE',  ( 20.94788355080264353, 65.69792220476300315, -64.03355541284614105 ) ) ;
#31877 = ORIENTED_EDGE ( 'NONE', *, *, #247308, .F. ) ;
#31876 = VECTOR ( 'NONE', #190808, 1000.000000000000000 ) ;
#31878 = CIRCLE ( 'NONE', #244212, 0.09999999999998898659 ) ;
#31879 = ORIENTED_EDGE ( 'NONE', *, *, #41676, .T. ) ;
#31880 = VECTOR ( 'NONE', #135356, 1000.000000000000000 ) ;
#31881 = DIRECTION ( 'NONE',  ( -0.000000000000000000, 0.4721928772777345684, 0.8814952561688429444 ) ) ;
#31882 = FACE_OUTER_BOUND ( 'NONE', #377, .T. ) ;
#31883 =( BOUNDED_CURVE ( )  B_SPLINE_CURVE ( 3, ( #221136, #3365, #46349, #146717 ),
 .UNSPECIFIED., .F., .F. ) 
 B_SPLINE_CURVE_WITH_KNOTS ( ( 4, 4 ),
 ( 0.3000847527772370071, 0.5497968875596834781 ),
 .UNSPECIFIED. ) 
 CURVE ( )  GEOMETRIC_REPRESENTATION_ITEM ( )  RATIONAL_B_SPLINE_CURVE ( ( 1.000000000000000000, 0.9948104011409417691, 0.9948104011409417691, 1.000000000000000000 ) ) 
 REPRESENTATION_ITEM ( '' )  );
#31884 = FACE_OUTER_BOUND ( 'NONE', #78038, .T. ) ;
#31885 = ORIENTED_EDGE ( 'NONE', *, *, #154632, .F. ) ;
#31886 = CIRCLE ( 'NONE', #148582, 0.09999999999998898659 ) ;
#31887 = CYLINDRICAL_SURFACE ( 'NONE', #16158, 1.500000000000001332 ) ;
#31888 = AXIS2_PLACEMENT_3D ( 'NONE', #133579, #35792, #193567 ) ;
#31889 = CARTESIAN_POINT ( 'NONE',  ( 21.08804281139606829, 65.37816569817040602, -57.17310751714594375 ) ) ;
#31890 = CARTESIAN_POINT ( 'NONE',  ( -21.05000000000000071, 1.115600667400684642E-11, -163.4000000000000341 ) ) ;
#31891 = ORIENTED_EDGE ( 'NONE', *, *, #239331, .T. ) ;
#31892 = DIRECTION ( 'NONE',  ( 0.000000000000000000, 2.891205793294679805E-16, -1.000000000000000000 ) ) ;
#31893 = DIRECTION ( 'NONE',  ( 0.000000000000000000, 0.8814952561688434995, -0.4721928772777337913 ) ) ;
#31894 = DIRECTION ( 'NONE',  ( 0.000000000000000000, -6.982962677686266711E-15, 1.000000000000000000 ) ) ;
#31895 = DIRECTION ( 'NONE',  ( 0.000000000000000000, 0.000000000000000000, -1.000000000000000000 ) ) ;
#31896 = ORIENTED_EDGE ( 'NONE', *, *, #108187, .T. ) ;
#31897 = CARTESIAN_POINT ( 'NONE',  ( -21.52071067811865746, 7.779289321892505882, -45.85000000000000142 ) ) ;
#31898 = ORIENTED_EDGE ( 'NONE', *, *, #90839, .F. ) ;
#31899 = CARTESIAN_POINT ( 'NONE',  ( -20.94999999999999929, 76.00000000001210765, -132.4231074845243370 ) ) ;
#31900 = EDGE_LOOP ( 'NONE', ( #41490, #179690, #102546, #199935 ) ) ;
#31901 = AXIS2_PLACEMENT_3D ( 'NONE', #197381, #236508, #57859 ) ;
#31902 = AXIS2_PLACEMENT_3D ( 'NONE', #88049, #167642, #244580 ) ;
#31903 = CIRCLE ( 'NONE', #235870, 0.1000000000000011990 ) ;
#31904 = CARTESIAN_POINT ( 'NONE',  ( -13.88555196119803803, 24.81692076904266386, -232.4788742220511608 ) ) ;
#31905 = FACE_OUTER_BOUND ( 'NONE', #33107, .T. ) ;
#31906 = ORIENTED_EDGE ( 'NONE', *, *, #72680, .F. ) ;
#31907 = ORIENTED_EDGE ( 'NONE', *, *, #78011, .T. ) ;
#31908 = DIRECTION ( 'NONE',  ( 0.000000000000000000, 0.9770955615653262871, 0.2128009952263842652 ) ) ;
#31909 = DIRECTION ( 'NONE',  ( 0.000000000000000000, -0.1686199900910528293, 0.9856811345164792071 ) ) ;
#31910 = ORIENTED_EDGE ( 'NONE', *, *, #26483, .F. ) ;
#31911 = CARTESIAN_POINT ( 'NONE',  ( -20.64999999999999858, 85.50000000001179501, -79.41707660717668205 ) ) ;
#31912 = DIRECTION ( 'NONE',  ( 1.000000000000000000, -0.000000000000000000, -0.000000000000000000 ) ) ;
#31913 = ORIENTED_EDGE ( 'NONE', *, *, #45168, .T. ) ;
#31914 = EDGE_CURVE ( 'NONE', #13227, #177719, #56047, .T. ) ;
#31915 = TOROIDAL_SURFACE ( 'NONE', #210965, 11.65000000000000036, 0.1000000000000000056 ) ;
#31916 = VERTEX_POINT ( 'NONE', #31801 ) ;
#31917 = DIRECTION ( 'NONE',  ( 0.7071359030027766224, -0.7070776581709024011, 0.000000000000000000 ) ) ;
#31919 = EDGE_CURVE ( 'NONE', #148888, #59550, #12225, .T. ) ;
#31918 = CARTESIAN_POINT ( 'NONE',  ( -20.64999999999999858, 67.23127455305835554, -235.8551265064784559 ) ) ;
#31920 = DIRECTION ( 'NONE',  ( 0.000000000000000000, -0.1568667991644714932, 0.9876197685951274563 ) ) ;
#31922 = VERTEX_POINT ( 'NONE', #171332 ) ;
#31921 = CARTESIAN_POINT ( 'NONE',  ( -21.14999999999994174, 74.83745509109094485, -43.92310748452479885 ) ) ;
#31923 = VECTOR ( 'NONE', #171693, 1000.000000000000000 ) ;
#31924 = DIRECTION ( 'NONE',  ( -1.000000000000000000, -2.952720810173289112E-16, 0.000000000000000000 ) ) ;
#31925 = EDGE_CURVE ( 'NONE', #140846, #220457, #177081, .T. ) ;
#31926 = DIRECTION ( 'NONE',  ( 1.000000000000000000, 0.000000000000000000, 0.000000000000000000 ) ) ;
#31927 = AXIS2_PLACEMENT_3D ( 'NONE', #180671, #103665, #222324 ) ;
#31928 = CARTESIAN_POINT ( 'NONE',  ( -20.94999999999999929, 74.83729825007408465, -128.5231074845243029 ) ) ;
#31930 = CARTESIAN_POINT ( 'NONE',  ( -20.94999999999999929, -11.64999999998884483, -197.9999999999999432 ) ) ;
#31929 = DIRECTION ( 'NONE',  ( -0.000000000000000000, 1.000000000000000000, 7.172728831056617961E-15 ) ) ;
#31932 = VECTOR ( 'NONE', #30367, 1000.000000000000000 ) ;
#31931 = CARTESIAN_POINT ( 'NONE',  ( 21.05000000000000071, 10.42338541492406989, -107.9920519238701218 ) ) ;
#31933 = CIRCLE ( 'NONE', #186027, 0.1000000000000072220 ) ;
#31934 = CARTESIAN_POINT ( 'NONE',  ( 18.50000000000000000, -9.419209763398095347, -107.7477694627589955 ) ) ;
#31935 = DIRECTION ( 'NONE',  ( 0.000000000000000000, 0.8814952561688430555, -0.4721928772777346239 ) ) ;
#31937 = ORIENTED_EDGE ( 'NONE', *, *, #10479, .F. ) ;
#31936 = VECTOR ( 'NONE', #219173, 1000.000000000000000 ) ;
#31938 = ORIENTED_EDGE ( 'NONE', *, *, #122329, .T. ) ;
#31939 = ADVANCED_FACE ( 'NONE', ( #14802 ), #185442, .T. ) ;
#31940 = EDGE_LOOP ( 'NONE', ( #239675, #65514, #249010, #403, #102660 ) ) ;
#31941 = EDGE_CURVE ( 'NONE', #190104, #29489, #73052, .T. ) ;
#31942 = DIRECTION ( 'NONE',  ( 1.000000000000000000, 0.000000000000000000, 0.000000000000000000 ) ) ;
#31943 = EDGE_CURVE ( 'NONE', #88270, #159975, #6362, .T. ) ;
#31944 = CIRCLE ( 'NONE', #77686, 0.09999999999999939493 ) ;
#31945 = CARTESIAN_POINT ( 'NONE',  ( 21.05000000000000071, 71.00000000001158185, -57.11784146561126363 ) ) ;
#31946 = ORIENTED_EDGE ( 'NONE', *, *, #45711, .T. ) ;
#31947 = VECTOR ( 'NONE', #78213, 1000.000000000000114 ) ;
#31948 = SURFACE_SIDE_STYLE ('',( #235249 ) ) ;
#31949 = CARTESIAN_POINT ( 'NONE',  ( -18.59999999999999787, 57.82359945636609666, -226.0354702357591350 ) ) ;
#31950 = CARTESIAN_POINT ( 'NONE',  ( -20.15000000000000568, 61.47027379766506527, -221.6001666287551188 ) ) ;
#31951 = DIRECTION ( 'NONE',  ( 0.000000000000000000, 0.000000000000000000, -1.000000000000000000 ) ) ;
#31952 = ORIENTED_EDGE ( 'NONE', *, *, #65647, .F. ) ;
#31953 = ORIENTED_EDGE ( 'NONE', *, *, #35767, .F. ) ;
#31954 = CARTESIAN_POINT ( 'NONE',  ( 21.05000000000000071, 60.06466898236885044, -221.3109722682306995 ) ) ;
#31955 = PLANE ( 'NONE',  #50953 ) ;
#31956 = ORIENTED_EDGE ( 'NONE', *, *, #167966, .F. ) ;
#31957 = EDGE_CURVE ( 'NONE', #204482, #96897, #14778, .T. ) ;
#31958 = CIRCLE ( 'NONE', #2700, 0.1000000000000028644 ) ;
#31959 = DIRECTION ( 'NONE',  ( 0.000000000000000000, 0.9915357197604862671, -0.1298341882519953583 ) ) ;
#31961 = ORIENTED_EDGE ( 'NONE', *, *, #173934, .F. ) ;
#31960 = CARTESIAN_POINT ( 'NONE',  ( 18.54999999999999716, 9.950000000011153034, -79.64999999999999147 ) ) ;
#31962 = PLANE ( 'NONE',  #120947 ) ;
#31964 = ORIENTED_EDGE ( 'NONE', *, *, #63763, .F. ) ;
#31963 = FACE_BOUND ( 'NONE', #91277, .T. ) ;
#31965 = FACE_OUTER_BOUND ( 'NONE', #123556, .T. ) ;
#31966 = CARTESIAN_POINT ( 'NONE',  ( 20.94999999999999929, 14.88773611405353314, -236.3451124650200370 ) ) ;
#31968 = EDGE_CURVE ( 'NONE', #148869, #212214, #189546, .T. ) ;
#31967 = FACE_OUTER_BOUND ( 'NONE', #124423, .T. ) ;
#31970 = CARTESIAN_POINT ( 'NONE',  ( 20.74897398619109268, 10.59569302167756888, -108.1793114562555473 ) ) ;
#31969 = CARTESIAN_POINT ( 'NONE',  ( 21.07928932188134397, 6.162520550847347955, -199.5566553493351307 ) ) ;
#31971 = DIRECTION ( 'NONE',  ( 0.000000000000000000, -6.982962677686266711E-15, 1.000000000000000000 ) ) ;
#31972 = DIRECTION ( 'NONE',  ( 1.000000000000000000, 0.000000000000000000, 0.000000000000000000 ) ) ;
#31973 = CIRCLE ( 'NONE', #240258, 0.1000000000000124678 ) ;
#31974 = CIRCLE ( 'NONE', #65267, 11.90000000000000746 ) ;
#31975 = CARTESIAN_POINT ( 'NONE',  ( -23.25000000000000000, 54.34471204062663219, -239.4366250215122420 ) ) ;
#31976 = AXIS2_PLACEMENT_3D ( 'NONE', #93058, #31840, #68373 ) ;
#31978 = CARTESIAN_POINT ( 'NONE',  ( -16.93388492042258875, 44.07359652990944454, -235.2844227631439367 ) ) ;
#31977 = VECTOR ( 'NONE', #217307, 1000.000000000000000 ) ;
#31979 = ORIENTED_EDGE ( 'NONE', *, *, #249299, .F. ) ;
#31980 = CARTESIAN_POINT ( 'NONE',  ( -17.80356949363855179, 10.87673139701218616, -77.28692697577338322 ) ) ;
#31981 = ORIENTED_EDGE ( 'NONE', *, *, #256129, .F. ) ;
#31982 = CARTESIAN_POINT ( 'NONE',  ( -20.00857864376270001, 13.44116543737180081, -219.7184420207870801 ) ) ;
#31983 = EDGE_LOOP ( 'NONE', ( #69653, #5032, #154763, #56078 ) ) ;
#31984 = DIRECTION ( 'NONE',  ( 0.000000000000000000, 0.9994937237965569876, 0.03181660087583042945 ) ) ;
#31985 = ORIENTED_EDGE ( 'NONE', *, *, #6766, .F. ) ;
#31986 = AXIS2_PLACEMENT_3D ( 'NONE', #76241, #112817, #251019 ) ;
#31987 = CARTESIAN_POINT ( 'NONE',  ( -20.54999999999999716, 85.50000000001261924, -193.6291383618718385 ) ) ;
#31988 = PRESENTATION_STYLE_ASSIGNMENT (( #145486 ) ) ;
#31989 = TOROIDAL_SURFACE ( 'NONE', #186092, 11.70000000000000107, 0.1000000000000000056 ) ;
#31990 = AXIS2_PLACEMENT_3D ( 'NONE', #121344, #41792, #84700 ) ;
#31991 = ORIENTED_EDGE ( 'NONE', *, *, #44106, .F. ) ;
#31992 = ORIENTED_EDGE ( 'NONE', *, *, #135606, .F. ) ;
#31993 = EDGE_CURVE ( 'NONE', #196290, #196513, #64614, .T. ) ;
#31994 = FACE_OUTER_BOUND ( 'NONE', #17205, .T. ) ;
#31995 = CARTESIAN_POINT ( 'NONE',  ( -16.81095280782811230, 66.05000000001157900, -56.87310748452526354 ) ) ;
#31996 = AXIS2_PLACEMENT_3D ( 'NONE', #248910, #149819, #10307 ) ;
#31997 = CARTESIAN_POINT ( 'NONE',  ( 21.13736287352038445, 8.046642376395153562, -87.85000000000003695 ) ) ;
#31998 = ADVANCED_FACE ( 'NONE', ( #235112 ), #164602, .T. ) ;
#31999 = LINE ( 'NONE', #1814, #74005 ) ;
#32000 = DIRECTION ( 'NONE',  ( 0.000000000000000000, -6.982962677686266711E-15, 1.000000000000000000 ) ) ;
#32002 = DIRECTION ( 'NONE',  ( 0.000000000000000000, -0.9915357197604853789, 0.1298341882520022694 ) ) ;
#32001 = CARTESIAN_POINT ( 'NONE',  ( -20.64999999999999858, -8.730841121484171907, -76.59807471898437825 ) ) ;
#32003 = CARTESIAN_POINT ( 'NONE',  ( 18.49999999999988276, 10.28015861706820466, -58.22457207120090317 ) ) ;
#32005 = ORIENTED_EDGE ( 'NONE', *, *, #202457, .F. ) ;
#32004 = DIRECTION ( 'NONE',  ( -1.000000000000000000, 0.000000000000000000, -0.000000000000000000 ) ) ;
#32007 = CARTESIAN_POINT ( 'NONE',  ( 21.98333005346336222, 1.115600667400684642E-11, -160.1259246709433057 ) ) ;
#32006 = CARTESIAN_POINT ( 'NONE',  ( 20.13684514580102913, 9.495855392761558988, -75.14303168568623903 ) ) ;
#32008 = ADVANCED_FACE ( 'NONE', ( #137273 ), #243698, .F. ) ;
#32009 = CARTESIAN_POINT ( 'NONE',  ( 18.59999999999999076, 1.250000000011167511, -175.4999999999999716 ) ) ;
#32010 = ADVANCED_FACE ( 'NONE', ( #138538 ), #195993, .T. ) ;
#32011 = EDGE_LOOP ( 'NONE', ( #179614, #108765, #81943, #150978 ) ) ;
#32012 = DIRECTION ( 'NONE',  ( 0.000000000000000000, -7.056502275159890832E-15, 1.000000000000000000 ) ) ;
#32013 = DIRECTION ( 'NONE',  ( -1.000000000000000000, 0.000000000000000000, 0.000000000000000000 ) ) ;
#32014 = DIRECTION ( 'NONE',  ( -1.000000000000000000, 0.000000000000000000, -0.000000000000000000 ) ) ;
#32015 = ORIENTED_EDGE ( 'NONE', *, *, #41549, .F. ) ;
#32016 = EDGE_CURVE ( 'NONE', #43683, #196513, #214459, .T. ) ;
#32017 = CARTESIAN_POINT ( 'NONE',  ( -23.25000000000000355, 70.35000000001261355, -190.8731074845244109 ) ) ;
#32018 = ADVANCED_FACE ( 'NONE', ( #158179 ), #98122, .T. ) ;
#32019 = AXIS2_PLACEMENT_3D ( 'NONE', #73643, #131013, #153189 ) ;
#32020 = DIRECTION ( 'NONE',  ( 1.000000000000000000, 0.000000000000000000, 0.000000000000000000 ) ) ;
#32021 = DIRECTION ( 'NONE',  ( 1.000000000000000000, 1.734723475976817507E-14, 0.000000000000000000 ) ) ;
#32023 = EDGE_CURVE ( 'NONE', #56882, #76756, #252069, .T. ) ;
#32022 = ADVANCED_FACE ( 'NONE', ( #119020 ), #198537, .T. ) ;
#32024 = ORIENTED_EDGE ( 'NONE', *, *, #83321, .T. ) ;
#32025 = ORIENTED_EDGE ( 'NONE', *, *, #22619, .T. ) ;
#32026 = CARTESIAN_POINT ( 'NONE',  ( 21.05000000000000071, -11.48912529306490349, -70.10000000000005116 ) ) ;
#32027 = DIRECTION ( 'NONE',  ( -0.000000000000000000, -0.9594490217226103734, -0.2818822000686205254 ) ) ;
#32028 = CARTESIAN_POINT ( 'NONE',  ( 17.23472005113828232, 65.69211804551153477, -158.5696843445931279 ) ) ;
#32029 = ORIENTED_EDGE ( 'NONE', *, *, #219462, .F. ) ;
#32030 = CIRCLE ( 'NONE', #165272, 0.09999999999999371891 ) ;
#32031 = CARTESIAN_POINT ( 'NONE',  ( 23.15000000000000213, 84.66355140188147743, -160.4990063664569959 ) ) ;
#32032 = EDGE_CURVE ( 'NONE', #223382, #239014, #39717, .T. ) ;
#32033 = DIRECTION ( 'NONE',  ( 0.000000000000000000, 7.086529944415894657E-15, -1.000000000000000000 ) ) ;
#32034 = CIRCLE ( 'NONE', #215168, 0.09999999999999939493 ) ;
#32035 = FACE_OUTER_BOUND ( 'NONE', #37043, .T. ) ;
#32036 = CARTESIAN_POINT ( 'NONE',  ( 21.14999999999999858, 47.74710514101221293, -244.5837943500090716 ) ) ;
#32037 = EDGE_CURVE ( 'NONE', #62010, #61601, #255893, .T. ) ;
#32038 = ADVANCED_FACE ( 'NONE', ( #34364 ), #193425, .F. ) ;
#32039 = AXIS2_PLACEMENT_3D ( 'NONE', #41579, #39001, #194236 ) ;
#32040 = ORIENTED_EDGE ( 'NONE', *, *, #74702, .F. ) ;
#32041 = DIRECTION ( 'NONE',  ( 0.000000000000000000, 0.000000000000000000, -1.000000000000000000 ) ) ;
#32042 =( GEOMETRIC_REPRESENTATION_CONTEXT ( 3 ) GLOBAL_UNCERTAINTY_ASSIGNED_CONTEXT ( ( #76659 ) ) GLOBAL_UNIT_ASSIGNED_CONTEXT ( ( #152956, #90365, #51213 ) ) REPRESENTATION_CONTEXT ( 'NONE', 'WORKASPACE' ) );
#32043 = EDGE_CURVE ( 'NONE', #201378, #42338, #22142, .T. ) ;
#32045 = ORIENTED_EDGE ( 'NONE', *, *, #87908, .T. ) ;
#32044 = DIRECTION ( 'NONE',  ( 1.186688945009010077E-16, 1.000000000000000000, 6.982962677686266711E-15 ) ) ;
#32046 = DIRECTION ( 'NONE',  ( 0.000000000000000000, 0.000000000000000000, 1.000000000000000000 ) ) ;
#32047 = FACE_OUTER_BOUND ( 'NONE', #139363, .T. ) ;
#32048 = DIRECTION ( 'NONE',  ( 0.000000000000000000, 0.000000000000000000, -1.000000000000000000 ) ) ;
#32049 = CIRCLE ( 'NONE', #48771, 0.2000000000000057288 ) ;
#32050 = CARTESIAN_POINT ( 'NONE',  ( 20.04142135623730070, 2.272311100394801109, -217.9150152700588592 ) ) ;
#32051 = ORIENTED_EDGE ( 'NONE', *, *, #149409, .T. ) ;
#32052 = CARTESIAN_POINT ( 'NONE',  ( 21.12400222705966968, 8.778511907077053422, -12.25000000000000000 ) ) ;
#32053 = EDGE_CURVE ( 'NONE', #100676, #92189, #122870, .T. ) ;
#32054 = DIRECTION ( 'NONE',  ( -1.000000000000000000, 0.000000000000000000, 0.000000000000000000 ) ) ;
#32055 = CARTESIAN_POINT ( 'NONE',  ( -18.59999999999999787, 74.65925378207906249, -213.7959699899455472 ) ) ;
#32056 = ORIENTED_EDGE ( 'NONE', *, *, #72374, .F. ) ;
#32057 = DIRECTION ( 'NONE',  ( 1.000000000000000000, 0.000000000000000000, 0.000000000000000000 ) ) ;
#32058 = DIRECTION ( 'NONE',  ( 1.000000000000000000, 0.000000000000000000, 0.000000000000000000 ) ) ;
#32059 = DIRECTION ( 'NONE',  ( 0.000000000000000000, -1.000000000000000000, 0.000000000000000000 ) ) ;
#32060 = CARTESIAN_POINT ( 'NONE',  ( 23.14999999999999858, 70.40000000001150227, -48.42837350343745584 ) ) ;
#32061 = CARTESIAN_POINT ( 'NONE',  ( 21.04999999999999716, 6.299230910098046365, -167.4015624999999829 ) ) ;
#32062 = CARTESIAN_POINT ( 'NONE',  ( 14.45963434102924694, 9.451541661396671401, -185.9538754988305698 ) ) ;
#32063 = AXIS2_PLACEMENT_3D ( 'NONE', #234218, #236783, #78972 ) ;
#32064 = ORIENTED_EDGE ( 'NONE', *, *, #175334, .T. ) ;
#32065 = ORIENTED_EDGE ( 'NONE', *, *, #114509, .F. ) ;
#32066 = AXIS2_PLACEMENT_3D ( 'NONE', #130736, #91613, #53769 ) ;
#32067 = CARTESIAN_POINT ( 'NONE',  ( -18.50000000000000000, -9.399999999988850163, -141.2972597596633193 ) ) ;
#32068 = DIRECTION ( 'NONE',  ( 0.000000000000000000, 0.000000000000000000, -1.000000000000000000 ) ) ;
#32069 = VECTOR ( 'NONE', #225806, 1000.000000000000000 ) ;
#32070 = DIRECTION ( 'NONE',  ( -0.000000000000000000, 1.000000000000000000, 6.352154140967427193E-15 ) ) ;
#32071 = CARTESIAN_POINT ( 'NONE',  ( -2.995603634470891112E-16, 85.04999629395501870, -215.0436355574738343 ) ) ;
#32072 = CIRCLE ( 'NONE', #223557, 0.09999999999999530098 ) ;
#32073 = AXIS2_PLACEMENT_3D ( 'NONE', #31648, #115002, #150295 ) ;
#32074 = DIRECTION ( 'NONE',  ( 0.000000000000000000, -1.000000000000000000, 6.308085367188393199E-16 ) ) ;
#32075 = CARTESIAN_POINT ( 'NONE',  ( -16.93772744219066340, 9.993541108763510650, -113.0980619719697273 ) ) ;
#32076 = CARTESIAN_POINT ( 'NONE',  ( -18.59999999999999787, 9.350000000011156942, -121.8500000000000369 ) ) ;
#32077 = AXIS2_PLACEMENT_3D ( 'NONE', #173732, #78416, #36776 ) ;
#32078 = CIRCLE ( 'NONE', #131831, 0.1000000000000033362 ) ;
#32079 = ORIENTED_EDGE ( 'NONE', *, *, #187682, .T. ) ;
#32080 = CARTESIAN_POINT ( 'NONE',  ( -18.59999999999999787, 1.261786168576181755, -108.5864989635455089 ) ) ;
#32081 = ORIENTED_EDGE ( 'NONE', *, *, #128666, .T. ) ;
#32082 = CARTESIAN_POINT ( 'NONE',  ( 20.95512820512820440, 65.37615131629992504, -81.77310748452438816 ) ) ;
#32083 = CYLINDRICAL_SURFACE ( 'NONE', #103929, 4.000000000000003553 ) ;
#32084 = CARTESIAN_POINT ( 'NONE',  ( 21.09706851349342216, 8.775842513484549912, -79.23556621639968967 ) ) ;
#32085 = CARTESIAN_POINT ( 'NONE',  ( 18.50000000000000000, 86.89640087696871262, -199.6396878666313341 ) ) ;
#32086 = CARTESIAN_POINT ( 'NONE',  ( 18.59999999999999432, 1.261786168576181755, -175.5864989635454378 ) ) ;
#32087 = DIRECTION ( 'NONE',  ( -0.000000000000000000, -0.000000000000000000, -1.000000000000000000 ) ) ;
#32088 = CARTESIAN_POINT ( 'NONE',  ( -18.50000000000000000, 74.98773774893902555, -233.8732236541320333 ) ) ;
#32089 = VERTEX_POINT ( 'NONE', #224518 ) ;
#32090 = CARTESIAN_POINT ( 'NONE',  ( -16.93772744219066340, 22.95284413564059278, -230.8721573634133222 ) ) ;
#32091 = ADVANCED_FACE ( 'NONE', ( #64172 ), #182858, .F. ) ;
#32092 = CARTESIAN_POINT ( 'NONE',  ( -23.15000000000000213, -1.109497582084245426, -218.6091262806550048 ) ) ;
#32093 = FACE_OUTER_BOUND ( 'NONE', #26295, .T. ) ;
#32094 = AXIS2_PLACEMENT_3D ( 'NONE', #150577, #148005, #112730 ) ;
#32095 = CARTESIAN_POINT ( 'NONE',  ( -16.87331047859651179, 66.05000000001230376, -157.3731074845244393 ) ) ;
#32096 = ADVANCED_FACE ( 'NONE', ( #143695 ), #160520, .F. ) ;
#32097 = CARTESIAN_POINT ( 'NONE',  ( -22.50000000000000000, 11.64957080755595520, -167.3999999999999773 ) ) ;
#32098 = VERTEX_POINT ( 'NONE', #125436 ) ;
#32099 = DIRECTION ( 'NONE',  ( 0.000000000000000000, 0.000000000000000000, 1.000000000000000000 ) ) ;
#32100 = EDGE_CURVE ( 'NONE', #52066, #33168, #141146, .T. ) ;
#32102 = ADVANCED_FACE ( 'NONE', ( #83685 ), #185398, .T. ) ;
#32101 = ORIENTED_EDGE ( 'NONE', *, *, #85862, .F. ) ;
#32103 = ORIENTED_EDGE ( 'NONE', *, *, #35005, .F. ) ;
#32104 = CARTESIAN_POINT ( 'NONE',  ( -20.94999999999999929, 77.04701199367727327, -199.6625678998140359 ) ) ;
#32105 = CARTESIAN_POINT ( 'NONE',  ( 18.50000000000000000, -9.419078080838369615, -174.3299253502083559 ) ) ;
#32106 = AXIS2_PLACEMENT_3D ( 'NONE', #1989, #46256, #142774 ) ;
#32107 = CIRCLE ( 'NONE', #3024, 11.70000000000001528 ) ;
#32108 = ORIENTED_EDGE ( 'NONE', *, *, #62958, .F. ) ;
#32110 = AXIS2_PLACEMENT_3D ( 'NONE', #30079, #249117, #170901 ) ;
#32109 = DIRECTION ( 'NONE',  ( 0.000000000000000000, 0.2617529984165152257, 0.9651348961777124202 ) ) ;
#32111 = LINE ( 'NONE', #73811, #168513 ) ;
#32112 = CIRCLE ( 'NONE', #227706, 0.1000000000000031558 ) ;
#32113 = EDGE_LOOP ( 'NONE', ( #170956, #45449, #51204, #34552, #228519 ) ) ;
#32114 = CIRCLE ( 'NONE', #244467, 11.64999999999999325 ) ;
#32115 = EDGE_CURVE ( 'NONE', #218493, #108252, #135341, .T. ) ;
#32116 = EDGE_CURVE ( 'NONE', #122268, #62135, #244077, .T. ) ;
#32117 = FACE_OUTER_BOUND ( 'NONE', #50529, .T. ) ;
#32118 = VERTEX_POINT ( 'NONE', #61600 ) ;
#32119 = CYLINDRICAL_SURFACE ( 'NONE', #172660, 0.5000000000000004441 ) ;
#32120 = CARTESIAN_POINT ( 'NONE',  ( -23.25000000000000000, 71.65000000001187175, -90.87310748452432563 ) ) ;
#32122 = ORIENTED_EDGE ( 'NONE', *, *, #91262, .F. ) ;
#32121 = FACE_OUTER_BOUND ( 'NONE', #83947, .T. ) ;
#32123 = CARTESIAN_POINT ( 'NONE',  ( 20.85000000000000142, 79.37986612816742138, -196.2658927859692142 ) ) ;
#32125 = FACE_OUTER_BOUND ( 'NONE', #14503, .T. ) ;
#32124 = UNCERTAINTY_MEASURE_WITH_UNIT (LENGTH_MEASURE( 1.000000000000000082E-05 ), #107297, 'distance_accuracy_value', 'NONE');
#32126 = CARTESIAN_POINT ( 'NONE',  ( -20.93302460841142931, 65.68434038414380893, -130.9866880726065972 ) ) ;
#32127 = AXIS2_PLACEMENT_3D ( 'NONE', #62412, #139351, #218895 ) ;
#32128 = LINE ( 'NONE', #111637, #251558 ) ;
#32129 = SPHERICAL_SURFACE ( 'NONE', #41882, 0.1000000000000000056 ) ;
#32130 = VECTOR ( 'NONE', #16677, 1000.000000000000000 ) ;
#32131 = DIRECTION ( 'NONE',  ( 0.000000000000000000, 0.000000000000000000, -1.000000000000000000 ) ) ;
#32132 = DIRECTION ( 'NONE',  ( 1.000000000000000000, 0.000000000000000000, 0.000000000000000000 ) ) ;
#32134 = ORIENTED_EDGE ( 'NONE', *, *, #133135, .F. ) ;
#32133 = EDGE_CURVE ( 'NONE', #121455, #172986, #44612, .T. ) ;
#32135 = ORIENTED_EDGE ( 'NONE', *, *, #185820, .T. ) ;
#32137 = LINE ( 'NONE', #152083, #206144 ) ;
#32136 = DIRECTION ( 'NONE',  ( 1.000000000000000000, 0.000000000000000000, 0.000000000000000000 ) ) ;
#32139 = VERTEX_POINT ( 'NONE', #219376 ) ;
#32138 = CARTESIAN_POINT ( 'NONE',  ( 20.04999999999999716, 8.750000000011173285, -188.3499999999999659 ) ) ;
#32140 = ORIENTED_EDGE ( 'NONE', *, *, #126671, .F. ) ;
#32141 = EDGE_CURVE ( 'NONE', #80942, #237795, #206289, .T. ) ;
#32142 = DIRECTION ( 'NONE',  ( -0.000000000000000000, 1.000000000000000000, -0.000000000000000000 ) ) ;
#32143 = DIRECTION ( 'NONE',  ( -0.000000000000000000, 0.1350103645451974088, -0.9908441862701587999 ) ) ;
#32144 = VECTOR ( 'NONE', #138818, 1000.000000000000114 ) ;
#32145 = LINE ( 'NONE', #251142, #21565 ) ;
#32146 = LINE ( 'NONE', #254951, #48602 ) ;
#32147 = CARTESIAN_POINT ( 'NONE',  ( -21.05000000000000071, 1.115600667400684642E-11, -167.5000000000000284 ) ) ;
#32149 = EDGE_CURVE ( 'NONE', #118177, #51736, #93852, .T. ) ;
#32148 = DIRECTION ( 'NONE',  ( 0.000000000000000000, -0.9770955615653313941, -0.2128009952263603677 ) ) ;
#32150 = EDGE_CURVE ( 'NONE', #115941, #198538, #241520, .T. ) ;
#32151 = FACE_OUTER_BOUND ( 'NONE', #89994, .T. ) ;
#32152 = ORIENTED_EDGE ( 'NONE', *, *, #3321, .F. ) ;
#32153 = ORIENTED_EDGE ( 'NONE', *, *, #73807, .T. ) ;
#32154 = DIRECTION ( 'NONE',  ( 0.000000000000000000, 1.224646799142015331E-16, 1.000000000000000000 ) ) ;
#32155 = EDGE_CURVE ( 'NONE', #9287, #96922, #142413, .T. ) ;
#32156 = VECTOR ( 'NONE', #27246, 1000.000000000000000 ) ;
#32157 = AXIS2_PLACEMENT_3D ( 'NONE', #256421, #101218, #97380 ) ;
#32158 = EDGE_LOOP ( 'NONE', ( #87706, #182677, #245665, #59628 ) ) ;
#32159 = AXIS2_PLACEMENT_3D ( 'NONE', #52642, #128353, #207903 ) ;
#32160 = DIRECTION ( 'NONE',  ( 0.000000000000000000, 0.000000000000000000, 1.000000000000000000 ) ) ;
#32161 = VERTEX_POINT ( 'NONE', #203679 ) ;
#32162 = DIRECTION ( 'NONE',  ( 1.000000000000000000, 0.000000000000000000, 0.000000000000000000 ) ) ;
#32163 = DIRECTION ( 'NONE',  ( 0.000000000000000000, 0.000000000000000000, -1.000000000000000000 ) ) ;
#32164 = DIRECTION ( 'NONE',  ( -1.000000000000000000, 0.000000000000000000, 0.000000000000000000 ) ) ;
#32165 = ORIENTED_EDGE ( 'NONE', *, *, #198863, .T. ) ;
#32166 = EDGE_CURVE ( 'NONE', #113736, #253910, #81346, .T. ) ;
#32167 = DIRECTION ( 'NONE',  ( -0.000000000000000000, -0.2128009952263603677, 0.9770955615653313941 ) ) ;
#32168 = ORIENTED_EDGE ( 'NONE', *, *, #133496, .T. ) ;
#32169 = CARTESIAN_POINT ( 'NONE',  ( -23.15000000000000213, 71.85000000001157616, -57.17310748452435121 ) ) ;
#32170 = CARTESIAN_POINT ( 'NONE',  ( 20.95263205890712399, 8.895740107905208305, -108.9895084069416527 ) ) ;
#32171 = ADVANCED_FACE ( 'NONE', ( #49735 ), #114705, .T. ) ;
#32172 = VECTOR ( 'NONE', #30211, 1000.000000000000000 ) ;
#32173 = ORIENTED_EDGE ( 'NONE', *, *, #82564, .F. ) ;
#32174 = VECTOR ( 'NONE', #192680, 1000.000000000000000 ) ;
#32176 = CARTESIAN_POINT ( 'NONE',  ( -20.94999999999999929, -11.48912529306489994, -63.89999999999999858 ) ) ;
#32175 = VECTOR ( 'NONE', #67749, 1000.000000000000000 ) ;
#32177 = ORIENTED_EDGE ( 'NONE', *, *, #139169, .T. ) ;
#32180 = EDGE_LOOP ( 'NONE', ( #189978, #55874, #171321, #197014 ) ) ;
#32179 = CARTESIAN_POINT ( 'NONE',  ( 23.15000000000000213, 88.41227409416160299, -106.0231074845242176 ) ) ;
#32178 = DIRECTION ( 'NONE',  ( 1.000000000000000000, 0.000000000000000000, 0.000000000000000000 ) ) ;
#32181 = CARTESIAN_POINT ( 'NONE',  ( -20.85000000000000142, 77.16412189325258453, -28.10825939895270764 ) ) ;
#32182 = ORIENTED_EDGE ( 'NONE', *, *, #211764, .T. ) ;
#32183 = AXIS2_PLACEMENT_3D ( 'NONE', #225145, #223866, #187345 ) ;
#32184 = EDGE_LOOP ( 'NONE', ( #151388, #243742, #29617, #134794 ) ) ;
#32185 = CARTESIAN_POINT ( 'NONE',  ( 21.05000000000000071, 0.000000000000000000, 0.000000000000000000 ) ) ;
#32186 = ORIENTED_EDGE ( 'NONE', *, *, #246647, .F. ) ;
#32187 = LINE ( 'NONE', #125183, #1719 ) ;
#32188 = DIRECTION ( 'NONE',  ( 0.000000000000000000, 6.982962677686266711E-15, -1.000000000000000000 ) ) ;
#32189 = FACE_OUTER_BOUND ( 'NONE', #174409, .T. ) ;
#32190 = PLANE ( 'NONE',  #214474 ) ;
#32191 = EDGE_LOOP ( 'NONE', ( #118612, #170034, #215307, #253962 ) ) ;
#32192 = CARTESIAN_POINT ( 'NONE',  ( -22.50000000000000000, 7.790779598373403836, 0.09999999999999939493 ) ) ;
#32193 = CARTESIAN_POINT ( 'NONE',  ( -20.94999999999999929, 74.63912941281955682, -61.45010955743337178 ) ) ;
#32194 = CARTESIAN_POINT ( 'NONE',  ( 21.11101077988997332, 6.423684734737197921, -33.48471473108569540 ) ) ;
#32195 = AXIS2_PLACEMENT_3D ( 'NONE', #104687, #66890, #147717 ) ;
#32196 = ORIENTED_EDGE ( 'NONE', *, *, #224251, .T. ) ;
#32197 = CARTESIAN_POINT ( 'NONE',  ( -20.64999999999999858, 76.00000000001246292, -171.9231074845243938 ) ) ;
#32198 = ORIENTED_EDGE ( 'NONE', *, *, #22865, .F. ) ;
#32199 = CARTESIAN_POINT ( 'NONE',  ( 18.39999999999999503, 5.650000000011139001, -180.1499999999999773 ) ) ;
#32200 = ORIENTED_EDGE ( 'NONE', *, *, #200216, .F. ) ;
#32201 = B_SPLINE_CURVE_WITH_KNOTS ( 'NONE', 3,
 ( #217506, #173325, #237097, #58427, #153765, #113294, #74211, #192847, #21902, #220099, #239663, #240948, #122285, #199260, #41481, #44024 ),
 .UNSPECIFIED., .F., .F.,
 ( 4, 3, 3, 3, 3, 4 ),
 ( 0.000000000000000000, 2.209075297431637548E-05, 5.594258369011413288E-05, 8.979524372343752631E-05, 0.0001236472815274714237, 0.0001574990747609671831 ),
 .UNSPECIFIED. ) ;
#32202 = DIRECTION ( 'NONE',  ( 0.000000000000000000, 0.9908441862701420355, 0.1350103645453197554 ) ) ;
#32203 = DIRECTION ( 'NONE',  ( 1.000000000000000000, 0.000000000000000000, 0.000000000000000000 ) ) ;
#32205 = ORIENTED_EDGE ( 'NONE', *, *, #202327, .F. ) ;
#32204 = DIRECTION ( 'NONE',  ( 1.836970198721029934E-16, -1.000000000000000000, -0.000000000000000000 ) ) ;
#32206 = CARTESIAN_POINT ( 'NONE',  ( 18.39999999999999503, 13.90230816252088530, -210.9187585823742666 ) ) ;
#32207 = ORIENTED_EDGE ( 'NONE', *, *, #93935, .F. ) ;
#32208 = AXIS2_PLACEMENT_3D ( 'NONE', #26920, #105102, #148126 ) ;
#32209 = CARTESIAN_POINT ( 'NONE',  ( -21.04386569057572487, 36.16263438457815482, -235.9556900804354314 ) ) ;
#32210 = CARTESIAN_POINT ( 'NONE',  ( -15.55912972643741199, 8.490870273573719373, -46.15000000000000568 ) ) ;
#32211 = ORIENTED_EDGE ( 'NONE', *, *, #53766, .T. ) ;
#32212 = CARTESIAN_POINT ( 'NONE',  ( -21.53752568622129004, 0.09897446127764164547, -127.2131921254514566 ) ) ;
#32213 = DIRECTION ( 'NONE',  ( 1.186688945009010077E-16, -1.000000000000000000, -0.000000000000000000 ) ) ;
#32214 = EDGE_LOOP ( 'NONE', ( #44184, #68320, #220279, #58988 ) ) ;
#32215 = CARTESIAN_POINT ( 'NONE',  ( -16.93230518875208546, 10.00075036143099894, -146.5757783481015508 ) ) ;
#32216 = CIRCLE ( 'NONE', #215349, 11.65000000000000036 ) ;
#32217 = AXIS2_PLACEMENT_3D ( 'NONE', #45088, #224980, #46354 ) ;
#32218 = EDGE_LOOP ( 'NONE', ( #4839, #237343, #4471, #251299, #46869, #177459 ) ) ;
#32219 = CARTESIAN_POINT ( 'NONE',  ( 20.85000000000000142, 42.15997144203495139, -239.2817429668763793 ) ) ;
#32220 = CARTESIAN_POINT ( 'NONE',  ( -18.50000000000000000, 102.4393534156124730, -51.38159887701667827 ) ) ;
#32222 = CARTESIAN_POINT ( 'NONE',  ( -18.50000000000000355, -9.419084502802135717, -73.82990780702543532 ) ) ;
#32221 = AXIS2_PLACEMENT_3D ( 'NONE', #29698, #188733, #143180 ) ;
#32223 = CIRCLE ( 'NONE', #132169, 0.1000000000000013933 ) ;
#32224 = EDGE_CURVE ( 'NONE', #92979, #71034, #127999, .T. ) ;
#32227 = ORIENTED_EDGE ( 'NONE', *, *, #133972, .T. ) ;
#32226 = ORIENTED_EDGE ( 'NONE', *, *, #38117, .F. ) ;
#32225 = DIRECTION ( 'NONE',  ( -1.000000000000000000, -0.000000000000000000, -0.000000000000000000 ) ) ;
#32228 = EDGE_CURVE ( 'NONE', #218074, #68733, #148015, .T. ) ;
#32229 = LINE ( 'NONE', #89593, #187035 ) ;
#32230 = ADVANCED_FACE ( 'NONE', ( #27648 ), #73866, .T. ) ;
#32231 = DIRECTION ( 'NONE',  ( 0.000000000000000000, 0.000000000000000000, -1.000000000000000000 ) ) ;
#32233 = DIRECTION ( 'NONE',  ( -1.000000000000000000, 0.000000000000000000, -0.000000000000000000 ) ) ;
#32232 = DIRECTION ( 'NONE',  ( 0.000000000000000000, 0.000000000000000000, 1.000000000000000000 ) ) ;
#32234 = CARTESIAN_POINT ( 'NONE',  ( 21.05000000000000071, 54.23099463892081928, -236.2002849323373255 ) ) ;
#32235 = SPHERICAL_SURFACE ( 'NONE', #102584, 0.1000000000000000056 ) ;
#32236 = AXIS2_PLACEMENT_3D ( 'NONE', #217711, #15714, #113496 ) ;
#32237 = FACE_OUTER_BOUND ( 'NONE', #23270, .T. ) ;
#32238 = DIRECTION ( 'NONE',  ( 0.000000000000000000, 0.2617529984165033463, 0.9651348961777157509 ) ) ;
#32239 = AXIS2_PLACEMENT_3D ( 'NONE', #223634, #239370, #179411 ) ;
#32240 = ORIENTED_EDGE ( 'NONE', *, *, #255063, .F. ) ;
#32241 = VERTEX_POINT ( 'NONE', #247927 ) ;
#32243 = CARTESIAN_POINT ( 'NONE',  ( -20.64999999999999858, 2.500000000011156409, -147.2246219227621111 ) ) ;
#32242 = VECTOR ( 'NONE', #199659, 1000.000000000000000 ) ;
#32244 = ORIENTED_EDGE ( 'NONE', *, *, #133673, .F. ) ;
#32245 = AXIS2_PLACEMENT_3D ( 'NONE', #213982, #35379, #216538 ) ;
#32246 = ORIENTED_EDGE ( 'NONE', *, *, #45943, .T. ) ;
#32247 = EDGE_CURVE ( 'NONE', #149328, #165926, #75271, .T. ) ;
#32248 = DIRECTION ( 'NONE',  ( 1.000000000000000000, 0.000000000000000000, 0.000000000000000000 ) ) ;
#32249 = VERTEX_POINT ( 'NONE', #112294 ) ;
#32250 = DIRECTION ( 'NONE',  ( 0.000000000000000000, -0.1298341882519953860, -0.9915357197604862671 ) ) ;
#32251 = CIRCLE ( 'NONE', #223748, 0.09999999999999939493 ) ;
#32252 = EDGE_LOOP ( 'NONE', ( #77552, #66453, #184306, #12634, #12682, #110240, #39806, #206284, #110789, #205045, #112973, #74274, #100981, #7567, #45989, #206010, #178838, #230447, #767, #166948, #45451, #173025, #254600 ) ) ;
#32253 = CARTESIAN_POINT ( 'NONE',  ( -16.87665923198281348, 66.05000000001224691, -149.1731074845244223 ) ) ;
#32254 = DIRECTION ( 'NONE',  ( 0.000000000000000000, 0.2128009952263485993, -0.9770955615653341697 ) ) ;
#32257 = ORIENTED_EDGE ( 'NONE', *, *, #27578, .T. ) ;
#32256 = ORIENTED_EDGE ( 'NONE', *, *, #89458, .F. ) ;
#32255 = AXIS2_PLACEMENT_3D ( 'NONE', #7902, #186529, #87403 ) ;
#32258 = ORIENTED_EDGE ( 'NONE', *, *, #3683, .T. ) ;
#32259 = AXIS2_PLACEMENT_3D ( 'NONE', #100634, #1556, #81089 ) ;
#32260 = AXIS2_PLACEMENT_3D ( 'NONE', #34260, #118598, #40366 ) ;
#32261 = ORIENTED_EDGE ( 'NONE', *, *, #42912, .T. ) ;
#32262 = EDGE_LOOP ( 'NONE', ( #187378, #115472, #187313, #6227, #192933 ) ) ;
#32263 = CARTESIAN_POINT ( 'NONE',  ( 19.92426406871192412, 64.25000000001176659, -78.17310748452437963 ) ) ;
#32264 = CARTESIAN_POINT ( 'NONE',  ( 21.05000000000000071, 43.37306621509043225, -234.7926750453023601 ) ) ;
#32265 = LINE ( 'NONE', #169220, #43869 ) ;
#32267 = ORIENTED_EDGE ( 'NONE', *, *, #172856, .T. ) ;
#32266 = CARTESIAN_POINT ( 'NONE',  ( -20.05000000000000426, 66.75000000001199396, -115.3731074845243683 ) ) ;
#32268 = ADVANCED_FACE ( 'NONE', ( #126708 ), #11921, .F. ) ;
#32269 = EDGE_CURVE ( 'NONE', #167954, #22444, #225783, .T. ) ;
#32270 = DIRECTION ( 'NONE',  ( -1.000000000000000000, -8.673617379884087537E-15, 0.000000000000000000 ) ) ;
#32271 = CARTESIAN_POINT ( 'NONE',  ( 22.00356870140516463, 7.254242362509886632, -167.4999999999999716 ) ) ;
#32273 = EDGE_LOOP ( 'NONE', ( #57288, #21739, #78278, #189043, #67139 ) ) ;
#32272 = DIRECTION ( 'NONE',  ( 1.000000000000000000, 0.000000000000000000, 0.000000000000000000 ) ) ;
#32274 = CARTESIAN_POINT ( 'NONE',  ( -23.25000000000000000, 41.46275801244657799, -260.2743004338703940 ) ) ;
#32275 = ORIENTED_EDGE ( 'NONE', *, *, #87984, .F. ) ;
#32276 = CARTESIAN_POINT ( 'NONE',  ( -22.39999999999999858, -1.560176095955062348, -193.3663837337744837 ) ) ;
#32277 = VERTEX_POINT ( 'NONE', #228387 ) ;
#32278 = VECTOR ( 'NONE', #86113, 1000.000000000000000 ) ;
#32279 = CARTESIAN_POINT ( 'NONE',  ( 23.30000000000000426, 3.332938107839120701, 33.00000000000000000 ) ) ;
#32280 = CARTESIAN_POINT ( 'NONE',  ( -16.85718274719385690, 30.29505757199756033, -234.8249179232091137 ) ) ;
#32281 = AXIS2_PLACEMENT_3D ( 'NONE', #94136, #113706, #193255 ) ;
#32282 = EDGE_CURVE ( 'NONE', #70740, #132220, #22958, .T. ) ;
#32283 = ORIENTED_EDGE ( 'NONE', *, *, #33837, .F. ) ;
#32285 = DIRECTION ( 'NONE',  ( 1.000000000000000000, 0.000000000000000000, 0.000000000000000000 ) ) ;
#32284 = FACE_OUTER_BOUND ( 'NONE', #91430, .T. ) ;
#32286 = CARTESIAN_POINT ( 'NONE',  ( -23.15000000000000213, 74.07476635515241981, -149.2533510176504876 ) ) ;
#32287 = LINE ( 'NONE', #251291, #59770 ) ;
#32288 = CARTESIAN_POINT ( 'NONE',  ( -21.05000000000000071, 64.35000000001214460, -136.4231074845243938 ) ) ;
#32289 = VERTEX_POINT ( 'NONE', #30196 ) ;
#32290 = ORIENTED_EDGE ( 'NONE', *, *, #31393, .T. ) ;
#32291 = AXIS2_PLACEMENT_3D ( 'NONE', #107890, #85721, #226529 ) ;
#32292 = CARTESIAN_POINT ( 'NONE',  ( -21.04999999999999716, 0.09843750001115456061, -127.7007690899131234 ) ) ;
#32293 = DIRECTION ( 'NONE',  ( -1.000000000000000000, 0.000000000000000000, 0.000000000000000000 ) ) ;
#32294 = EDGE_LOOP ( 'NONE', ( #97764, #44918, #251117, #64978 ) ) ;
#32295 = CARTESIAN_POINT ( 'NONE',  ( -21.45000000000000284, 12.05403912736948158, -220.1228874760914209 ) ) ;
#32296 = ORIENTED_EDGE ( 'NONE', *, *, #40549, .T. ) ;
#32297 = CARTESIAN_POINT ( 'NONE',  ( 21.15000000000005187, 64.35000000001120668, -51.02310748452479316 ) ) ;
#32298 = FACE_OUTER_BOUND ( 'NONE', #96395, .T. ) ;
#32299 = AXIS2_PLACEMENT_3D ( 'NONE', #1691, #102064, #81217 ) ;
#32300 = CARTESIAN_POINT ( 'NONE',  ( 22.45305468355010703, -0.1008583690885486023, -155.7504328765102457 ) ) ;
#32301 = VECTOR ( 'NONE', #92801, 1000.000000000000000 ) ;
#32302 = EDGE_CURVE ( 'NONE', #214263, #207792, #210557, .T. ) ;
#32303 = AXIS2_PLACEMENT_3D ( 'NONE', #97693, #212556, #74350 ) ;
#32304 = VECTOR ( 'NONE', #28153, 1000.000000000000114 ) ;
#32305 = ORIENTED_EDGE ( 'NONE', *, *, #116944, .F. ) ;
#32306 = CIRCLE ( 'NONE', #132231, 0.2000000000000057288 ) ;
#32307 = DIRECTION ( 'NONE',  ( -1.000000000000000000, -7.049440681616512959E-16, 1.911869773728122357E-16 ) ) ;
#32308 =( LENGTH_UNIT ( ) NAMED_UNIT ( * ) SI_UNIT ( .MILLI., .METRE. ) );
#32309 = ORIENTED_EDGE ( 'NONE', *, *, #14663, .F. ) ;
#32310 = VERTEX_POINT ( 'NONE', #131839 ) ;
#32311 = EDGE_LOOP ( 'NONE', ( #121270, #1949, #109539, #179872 ) ) ;
#32312 = ADVANCED_FACE ( 'NONE', ( #230969 ), #31538, .T. ) ;
#32313 = LINE ( 'NONE', #171833, #134054 ) ;
#32314 = CARTESIAN_POINT ( 'NONE',  ( 14.45204356427542081, 66.54933111084405084, -54.46756099431704712 ) ) ;
#32315 = CARTESIAN_POINT ( 'NONE',  ( -21.13498764882296044, 0.001656394742485926743, -127.5043818565260665 ) ) ;
#32316 = DIRECTION ( 'NONE',  ( -1.000000000000000000, -0.000000000000000000, -0.000000000000000000 ) ) ;
#32317 = CARTESIAN_POINT ( 'NONE',  ( -22.50000000000000000, 1.115600667400684642E-11, -134.0000000000000000 ) ) ;
#32319 = CARTESIAN_POINT ( 'NONE',  ( -23.15000000000000213, 74.07476635515169505, -48.75335101765046630 ) ) ;
#32318 = DIRECTION ( 'NONE',  ( -1.073024830501117923E-15, 0.9126074666063771490, 0.4088369013363281623 ) ) ;
#32321 = ORIENTED_EDGE ( 'NONE', *, *, #148904, .F. ) ;
#32320 = DIRECTION ( 'NONE',  ( 1.000000000000000000, -0.000000000000000000, -0.000000000000000000 ) ) ;
#32322 = DIRECTION ( 'NONE',  ( 0.000000000000000000, 0.000000000000000000, 1.000000000000000000 ) ) ;
#32323 = ORIENTED_EDGE ( 'NONE', *, *, #199209, .T. ) ;
#32324 = ADVANCED_FACE ( 'NONE', ( #47142, #206250 ), #107135, .T. ) ;
#32325 = CARTESIAN_POINT ( 'NONE',  ( -14.77738660682463667, 9.436552840015577814, -149.1779554727603454 ) ) ;
#32326 = EDGE_CURVE ( 'NONE', #236840, #166875, #163707, .T. ) ;
#32327 = ORIENTED_EDGE ( 'NONE', *, *, #6400, .T. ) ;
#32328 = VERTEX_POINT ( 'NONE', #217773 ) ;
#32329 = DIRECTION ( 'NONE',  ( 0.000000000000000000, 0.8660254037844281605, -0.5000000000000185407 ) ) ;
#32330 = AXIS2_PLACEMENT_3D ( 'NONE', #26648, #142702, #85282 ) ;
#32331 = DIRECTION ( 'NONE',  ( 0.000000000000000000, 6.505213034913742890E-15, -1.000000000000000000 ) ) ;
#32332 = FACE_OUTER_BOUND ( 'NONE', #115813, .T. ) ;
#32333 = CARTESIAN_POINT ( 'NONE',  ( -21.59142135623730852, 7.850000000011158718, -88.25000000000005684 ) ) ;
#32334 = VECTOR ( 'NONE', #323, 1000.000000000000000 ) ;
#32335 = EDGE_CURVE ( 'NONE', #227995, #149638, #73228, .T. ) ;
#32336 = CARTESIAN_POINT ( 'NONE',  ( 22.60000000000000142, 55.86495732666938352, -232.8769840133977880 ) ) ;
#32337 = ADVANCED_FACE ( 'NONE', ( #13191 ), #235486, .F. ) ;
#32338 = ORIENTED_EDGE ( 'NONE', *, *, #80584, .F. ) ;
#32339 = ORIENTED_EDGE ( 'NONE', *, *, #204639, .F. ) ;
#32340 = CARTESIAN_POINT ( 'NONE',  ( 23.24999999999999289, 66.49806749928671934, -213.5350143334560471 ) ) ;
#32341 = ORIENTED_EDGE ( 'NONE', *, *, #158330, .F. ) ;
#32342 = DIRECTION ( 'NONE',  ( 0.000000000000000000, 0.000000000000000000, -1.000000000000000000 ) ) ;
#32343 = CARTESIAN_POINT ( 'NONE',  ( 18.59999999999999076, 10.20857864376269575, -21.35000000000000142 ) ) ;
#32344 = VERTEX_POINT ( 'NONE', #96540 ) ;
#32345 = CARTESIAN_POINT ( 'NONE',  ( -20.94999999999999929, -11.48912529306490349, -170.4999999999999716 ) ) ;
#32347 = ADVANCED_FACE ( 'NONE', ( #133130 ), #214833, .F. ) ;
#32346 = CARTESIAN_POINT ( 'NONE',  ( -20.96077737575326694, 11.62390063401586282, -60.14079195710661452 ) ) ;
#32348 = DIRECTION ( 'NONE',  ( 0.000000000000000000, 0.000000000000000000, 1.000000000000000000 ) ) ;
#32349 = CARTESIAN_POINT ( 'NONE',  ( -18.59999999999999787, -10.64999999999999325, 33.00000000000000000 ) ) ;
#32350 = EDGE_LOOP ( 'NONE', ( #6730, #208573, #83221 ) ) ;
#32351 = DIRECTION ( 'NONE',  ( 0.000000000000000000, -1.000000000000000000, -6.982962677686266711E-15 ) ) ;
#32352 = DIRECTION ( 'NONE',  ( 2.952720810173289112E-16, 0.9651348961777191926, -0.2617529984164898571 ) ) ;
#32353 = FACE_OUTER_BOUND ( 'NONE', #129175, .T. ) ;
#32354 = CARTESIAN_POINT ( 'NONE',  ( -21.29999999999995808, 76.00000000001267608, -203.5231074845243597 ) ) ;
#32355 = ADVANCED_FACE ( 'NONE', ( #34066 ), #216509, .F. ) ;
#32356 = CARTESIAN_POINT ( 'NONE',  ( -21.00000000000000000, -1.720267447010333833E-15, 11.89999999999999858 ) ) ;
#32358 = CIRCLE ( 'NONE', #32157, 7.799999999999993605 ) ;
#32357 = CARTESIAN_POINT ( 'NONE',  ( -22.39999999999999858, 0.000000000000000000, 11.64957080754479968 ) ) ;
#32359 = ADVANCED_FACE ( 'NONE', ( #195696 ), #243871, .F. ) ;
#32360 = CIRCLE ( 'NONE', #52968, 0.09999999999998898659 ) ;
#32361 = ADVANCED_FACE ( 'NONE', ( #57420 ), #135674, .F. ) ;
#32362 = ORIENTED_EDGE ( 'NONE', *, *, #246313, .F. ) ;
#32363 = EDGE_CURVE ( 'NONE', #151810, #24271, #251787, .T. ) ;
#32364 = CARTESIAN_POINT ( 'NONE',  ( 21.04999999999999716, -0.03753606327451274732, -161.1677277260643564 ) ) ;
#32365 = ORIENTED_EDGE ( 'NONE', *, *, #237263, .F. ) ;
#32366 = DIRECTION ( 'NONE',  ( 0.000000000000000000, -6.982962677686266711E-15, 1.000000000000000000 ) ) ;
#32367 = CARTESIAN_POINT ( 'NONE',  ( 23.24999999999999289, 6.650000000011155876, -88.35000000000003695 ) ) ;
#32368 = CARTESIAN_POINT ( 'NONE',  ( -16.81453563122427752, 66.06089979457485128, -82.23484882387907646 ) ) ;
#32369 = EDGE_CURVE ( 'NONE', #75474, #196401, #135534, .T. ) ;
#32370 = CARTESIAN_POINT ( 'NONE',  ( 20.94999999999999929, 63.53162788017662166, -224.4728618886983043 ) ) ;
#32371 = DIRECTION ( 'NONE',  ( -2.915501640297152804E-16, -1.000000000000000000, -6.997203936713167125E-15 ) ) ;
#32372 = CARTESIAN_POINT ( 'NONE',  ( -20.64999999999999858, 84.66355140188167638, -179.5472086025916099 ) ) ;
#32373 = ADVANCED_FACE ( 'NONE', ( #173595 ), #198728, .T. ) ;
#32374 = VERTEX_POINT ( 'NONE', #17047 ) ;
#32375 = FACE_OUTER_BOUND ( 'NONE', #249669, .T. ) ;
#32376 = CARTESIAN_POINT ( 'NONE',  ( 21.14999999999999858, 67.21339244341194785, -124.2731074845243597 ) ) ;
#32378 = ADVANCED_FACE ( 'NONE', ( #236073 ), #136971, .F. ) ;
#32377 = CARTESIAN_POINT ( 'NONE',  ( -20.94999999999999929, 77.36087058720436005, -161.9501095574333931 ) ) ;
#32379 = DIRECTION ( 'NONE',  ( -1.000000000000000000, -0.000000000000000000, -0.000000000000000000 ) ) ;
#32380 = DIRECTION ( 'NONE',  ( -1.000000000000000000, -0.000000000000000000, 0.000000000000000000 ) ) ;
#32381 = CIRCLE ( 'NONE', #244703, 11.65000000000000746 ) ;
#32382 = ORIENTED_EDGE ( 'NONE', *, *, #89868, .F. ) ;
#32383 = ORIENTED_EDGE ( 'NONE', *, *, #181833, .T. ) ;
#32384 = DIRECTION ( 'NONE',  ( 1.000000000000000000, 1.186688945009010077E-16, 0.000000000000000000 ) ) ;
#32385 = DIRECTION ( 'NONE',  ( 0.000000000000000000, 0.000000000000000000, -1.000000000000000000 ) ) ;
#32386 = CARTESIAN_POINT ( 'NONE',  ( -21.05000000000000071, 75.74389420791943905, -69.55800392619661920 ) ) ;
#32387 = CYLINDRICAL_SURFACE ( 'NONE', #5517, 4.049999999999998046 ) ;
#32388 = CARTESIAN_POINT ( 'NONE',  ( -21.07016717456945898, 69.67905916191212157, -170.0231074845244450 ) ) ;
#32389 = EDGE_CURVE ( 'NONE', #121176, #227768, #52323, .T. ) ;
#32390 = ORIENTED_EDGE ( 'NONE', *, *, #158407, .T. ) ;
#32391 = DIRECTION ( 'NONE',  ( 1.000000000000000000, 0.000000000000000000, -0.000000000000000000 ) ) ;
#32392 = CONTEXT_DEPENDENT_SHAPE_REPRESENTATION ( #104145, #197407 ) ;
#32393 = DIRECTION ( 'NONE',  ( 1.000000000000000000, 0.000000000000000000, 0.000000000000000000 ) ) ;
#32394 = ORIENTED_EDGE ( 'NONE', *, *, #25635, .F. ) ;
#32395 = DIRECTION ( 'NONE',  ( 2.694716079187273439E-16, 1.000000000000000000, 6.467318590049456648E-15 ) ) ;
#32396 = CIRCLE ( 'NONE', #19906, 12.87499999999999822 ) ;
#32397 = AXIS2_PLACEMENT_3D ( 'NONE', #57817, #132240, #253458 ) ;
#32398 = ORIENTED_EDGE ( 'NONE', *, *, #86124, .T. ) ;
#32399 = EDGE_LOOP ( 'NONE', ( #243949, #194115, #252622 ) ) ;
#32400 = ORIENTED_EDGE ( 'NONE', *, *, #86158, .T. ) ;
#32401 = CARTESIAN_POINT ( 'NONE',  ( -16.81744102076748959, 9.950000000011138823, -154.8500000000000227 ) ) ;
#32402 = DIRECTION ( 'NONE',  ( -0.9880948137434723000, 0.1538461538461483591, -0.000000000000000000 ) ) ;
#32403 = AXIS2_PLACEMENT_3D ( 'NONE', #167408, #147832, #9583 ) ;
#32404 = DIRECTION ( 'NONE',  ( 0.000000000000000000, -0.2128009952263603677, 0.9770955615653313941 ) ) ;
#32405 = DIRECTION ( 'NONE',  ( 0.000000000000000000, 0.2128009952263601179, -0.9770955615653315052 ) ) ;
#32406 = CARTESIAN_POINT ( 'NONE',  ( -23.25000000000000000, 68.97833521811179480, -99.18954208262705663 ) ) ;
#32407 = LINE ( 'NONE', #230585, #20492 ) ;
#32408 = DIRECTION ( 'NONE',  ( 0.000000000000000000, 0.9998779222360096863, -0.01562500000001061998 ) ) ;
#32411 = DIRECTION ( 'NONE',  ( -0.000000000000000000, 1.000000000000000000, 6.982962677686267499E-15 ) ) ;
#32410 = VECTOR ( 'NONE', #112280, 1000.000000000000000 ) ;
#32409 = CARTESIAN_POINT ( 'NONE',  ( -23.15000000000000213, -11.48912529307605546, -30.39999999999999503 ) ) ;
#32412 = EDGE_CURVE ( 'NONE', #130620, #230224, #239941, .T. ) ;
#32413 = FACE_OUTER_BOUND ( 'NONE', #237501, .T. ) ;
#32414 = CARTESIAN_POINT ( 'NONE',  ( 21.05000000000000071, 21.98309897467605722, -231.7335930323676791 ) ) ;
#32415 = CARTESIAN_POINT ( 'NONE',  ( -21.14999999999999858, -0.09999999998884338825, -55.35042919245523763 ) ) ;
#32416 = DIRECTION ( 'NONE',  ( 1.000000000000000000, -0.000000000000000000, -0.000000000000000000 ) ) ;
#32417 = AXIS2_PLACEMENT_3D ( 'NONE', #163633, #3242, #200189 ) ;
#32418 = EDGE_LOOP ( 'NONE', ( #191249, #103411, #91368, #128069 ) ) ;
#32419 = CIRCLE ( 'NONE', #207368, 11.90000000000000746 ) ;
#32420 = EDGE_CURVE ( 'NONE', #155020, #30797, #158836, .T. ) ;
#32421 = CARTESIAN_POINT ( 'NONE',  ( -18.40000000000000213, -9.500000000000007105, -40.10018939122203818 ) ) ;
#32422 = AXIS2_PLACEMENT_3D ( 'NONE', #88186, #107779, #169081 ) ;
#32423 = DIRECTION ( 'NONE',  ( -1.000000000000000000, 0.000000000000000000, 0.000000000000000000 ) ) ;
#32424 = FACE_OUTER_BOUND ( 'NONE', #207726, .T. ) ;
#32425 = VECTOR ( 'NONE', #224662, 1000.000000000000000 ) ;
#32426 = DIRECTION ( 'NONE',  ( 0.000000000000000000, 0.000000000000000000, -1.000000000000000000 ) ) ;
#32427 = FACE_OUTER_BOUND ( 'NONE', #164096, .T. ) ;
#32428 = CIRCLE ( 'NONE', #73544, 0.1000000000000028644 ) ;
#32429 = DIRECTION ( 'NONE',  ( -1.000000000000000000, 0.000000000000000000, 0.000000000000000000 ) ) ;
#32430 = ADVANCED_FACE ( 'NONE', ( #5132 ), #200805, .F. ) ;
#32431 = ORIENTED_EDGE ( 'NONE', *, *, #136107, .F. ) ;
#32432 = ORIENTED_EDGE ( 'NONE', *, *, #67581, .T. ) ;
#32433 = CARTESIAN_POINT ( 'NONE',  ( -21.05000000000000071, 74.16465844978715438, -57.86795619196135476 ) ) ;
#32434 = VERTEX_POINT ( 'NONE', #161698 ) ;
#32436 = EDGE_CURVE ( 'NONE', #75618, #131400, #148191, .T. ) ;
#32435 = CARTESIAN_POINT ( 'NONE',  ( 18.49999999999999645, 2.859758780633683273, -208.6670499591424459 ) ) ;
#32437 = DIRECTION ( 'NONE',  ( 0.000000000000000000, 0.9908441862701596881, 0.1350103645451904977 ) ) ;
#32438 = AXIS2_PLACEMENT_3D ( 'NONE', #247565, #185023, #6383 ) ;
#32439 = AXIS2_PLACEMENT_3D ( 'NONE', #93125, #132259, #154433 ) ;
#32440 = AXIS2_PLACEMENT_3D ( 'NONE', #124258, #73289, #109800 ) ;
#32442 = ORIENTED_EDGE ( 'NONE', *, *, #107189, .T. ) ;
#32441 = AXIS2_PLACEMENT_3D ( 'NONE', #33793, #135398, #35074 ) ;
#32443 = CARTESIAN_POINT ( 'NONE',  ( 20.94999999999999929, 1.115600667400684642E-11, -67.00000000000000000 ) ) ;
#32444 = ORIENTED_EDGE ( 'NONE', *, *, #238961, .F. ) ;
#32445 = VECTOR ( 'NONE', #102358, 1000.000000000000000 ) ;
#32446 = DIRECTION ( 'NONE',  ( 0.000000000000000000, 1.000000000000000000, 7.116814260417668513E-15 ) ) ;
#32447 = DIRECTION ( 'NONE',  ( 0.000000000000000000, 0.000000000000000000, 1.000000000000000000 ) ) ;
#32448 = DIRECTION ( 'NONE',  ( 0.000000000000000000, 0.9177795674685970129, 0.3970902486049678326 ) ) ;
#32449 = CARTESIAN_POINT ( 'NONE',  ( -20.85000000000000142, 36.46860332481993794, -249.8166405164294588 ) ) ;
#32450 = DIRECTION ( 'NONE',  ( 1.000000000000000000, -0.000000000000000000, -0.000000000000000000 ) ) ;
#32451 = CARTESIAN_POINT ( 'NONE',  ( -21.07094088545368749, 0.09889370256337755294, -60.67983277808291120 ) ) ;
#32452 = CARTESIAN_POINT ( 'NONE',  ( 20.94999999999999929, 85.50000000001251976, -179.9170766071767389 ) ) ;
#32453 = CARTESIAN_POINT ( 'NONE',  ( -23.15000000000000213, 29.86062094194855376, -263.1160279713685100 ) ) ;
#32455 = VERTEX_POINT ( 'NONE', #220379 ) ;
#32454 = CARTESIAN_POINT ( 'NONE',  ( -18.49499033040907037, -9.438148771733517961, -40.69815322592344131 ) ) ;
#32457 = DIRECTION ( 'NONE',  ( -1.000000000000000000, -0.000000000000000000, 0.000000000000000000 ) ) ;
#32456 = DIRECTION ( 'NONE',  ( 1.000000000000000000, -2.952720810173289112E-16, -2.061873921506763405E-30 ) ) ;
#32458 = EDGE_LOOP ( 'NONE', ( #16279, #115975, #204056, #111535 ) ) ;
#32460 = ORIENTED_EDGE ( 'NONE', *, *, #40818, .T. ) ;
#32459 = CARTESIAN_POINT ( 'NONE',  ( -23.25000000000000355, 11.75000000001113953, -57.75000000000000000 ) ) ;
#32461 = AXIS2_PLACEMENT_3D ( 'NONE', #16885, #36463, #132981 ) ;
#32462 = EDGE_LOOP ( 'NONE', ( #44433, #48377, #118521, #70917 ) ) ;
#32463 = EDGE_CURVE ( 'NONE', #80661, #214176, #183804, .T. ) ;
#32464 = CARTESIAN_POINT ( 'NONE',  ( -20.54999999999999716, 7.250000000011155521, -54.65000000000000568 ) ) ;
#32465 = MECHANICAL_DESIGN_GEOMETRIC_PRESENTATION_REPRESENTATION (  '', ( #94955 ), #132379 ) ;
#32466 = CIRCLE ( 'NONE', #103140, 0.1000000000000029476 ) ;
#32467 = DIRECTION ( 'NONE',  ( -0.000000000000000000, 0.9126074666063771490, 0.4088369013363281623 ) ) ;
#32468 = CARTESIAN_POINT ( 'NONE',  ( 23.14999999999999858, 0.000000000000000000, -33.50000000000000000 ) ) ;
#32469 = DIRECTION ( 'NONE',  ( -1.000000000000000000, -0.000000000000000000, 0.000000000000000000 ) ) ;
#32470 = DIRECTION ( 'NONE',  ( 0.000000000000000000, -1.000000000000000000, 0.000000000000000000 ) ) ;
#32471 = DIRECTION ( 'NONE',  ( 1.000000000000000000, 0.000000000000000000, 0.000000000000000000 ) ) ;
#32473 = EDGE_CURVE ( 'NONE', #112914, #183016, #198090, .T. ) ;
#32472 = CARTESIAN_POINT ( 'NONE',  ( 23.14999999999999503, 64.35000000001176090, -76.53791325517833855 ) ) ;
#32474 = AXIS2_PLACEMENT_3D ( 'NONE', #2432, #199391, #40337 ) ;
#32475 = EDGE_CURVE ( 'NONE', #433, #68352, #177280, .T. ) ;
#32476 = AXIS2_PLACEMENT_3D ( 'NONE', #136807, #115986, #235904 ) ;
#32477 = FACE_OUTER_BOUND ( 'NONE', #226522, .T. ) ;
#32478 = ORIENTED_EDGE ( 'NONE', *, *, #178307, .T. ) ;
#32479 = ORIENTED_EDGE ( 'NONE', *, *, #247528, .F. ) ;
#32480 = CARTESIAN_POINT ( 'NONE',  ( -21.05000000000000071, 74.75000000001232081, -162.0231074845243597 ) ) ;
#32481 = AXIS2_PLACEMENT_3D ( 'NONE', #111559, #154567, #236621 ) ;
#32482 = ORIENTED_EDGE ( 'NONE', *, *, #213599, .F. ) ;
#32483 = DIRECTION ( 'NONE',  ( 0.000000000000000000, 0.9908441862701596881, 0.1350103645451904977 ) ) ;
#32484 = ORIENTED_EDGE ( 'NONE', *, *, #175385, .F. ) ;
#32485 = CARTESIAN_POINT ( 'NONE',  ( 18.44208962362730730, -9.552340496908351852, -40.34217305546407317 ) ) ;
#32486 = AXIS2_PLACEMENT_3D ( 'NONE', #150575, #214389, #172748 ) ;
#32487 = ADVANCED_FACE ( 'NONE', ( #139531 ), #182543, .F. ) ;
#32488 = DIRECTION ( 'NONE',  ( 1.000000000000000000, 0.000000000000000000, 0.000000000000000000 ) ) ;
#32489 = CARTESIAN_POINT ( 'NONE',  ( -22.50000000000000000, -2.381330705637465961, -189.5959759702857923 ) ) ;
#32490 = DIRECTION ( 'NONE',  ( 0.000000000000000000, 0.000000000000000000, -1.000000000000000000 ) ) ;
#32491 = EDGE_CURVE ( 'NONE', #127487, #233728, #247969, .T. ) ;
#32492 = CARTESIAN_POINT ( 'NONE',  ( 15.74999999999999645, 48.12247445990688988, -234.1702647910923361 ) ) ;
#32493 = EDGE_LOOP ( 'NONE', ( #61118, #76097, #128086 ) ) ;
#32494 = AXIS2_PLACEMENT_3D ( 'NONE', #26780, #123289, #185822 ) ;
#32495 = EDGE_CURVE ( 'NONE', #209093, #238512, #23484, .T. ) ;
#32496 = CARTESIAN_POINT ( 'NONE',  ( -18.48179518609192229, -9.518325300483091667, -207.8897055767644133 ) ) ;
#32497 = DIRECTION ( 'NONE',  ( -1.000000000000000000, 0.000000000000000000, 0.000000000000000000 ) ) ;
#32498 = CIRCLE ( 'NONE', #178229, 0.2000000000000057288 ) ;
#32500 = FACE_OUTER_BOUND ( 'NONE', #38791, .T. ) ;
#32499 = CIRCLE ( 'NONE', #178230, 11.80000000000000426 ) ;
#32501 = DIRECTION ( 'NONE',  ( 1.000000000000000000, 0.000000000000000000, 0.000000000000000000 ) ) ;
#32502 = EDGE_CURVE ( 'NONE', #240985, #256256, #108405, .T. ) ;
#32503 = CIRCLE ( 'NONE', #169882, 7.900000000000010125 ) ;
#32504 = CARTESIAN_POINT ( 'NONE',  ( 20.94999999999999929, 76.00000000001242029, -166.0231074845243597 ) ) ;
#32505 = ORIENTED_EDGE ( 'NONE', *, *, #181276, .T. ) ;
#32507 = CARTESIAN_POINT ( 'NONE',  ( -18.49999999999998934, 85.48068669529035901, -29.08199231576640642 ) ) ;
#32506 = CARTESIAN_POINT ( 'NONE',  ( -16.87242674293849731, 60.93907239080193250, -221.0427799704054621 ) ) ;
#32508 = EDGE_LOOP ( 'NONE', ( #229177, #61659, #83499 ) ) ;
#32511 = ORIENTED_EDGE ( 'NONE', *, *, #140296, .T. ) ;
#32510 = DIRECTION ( 'NONE',  ( -1.000000000000000000, 0.000000000000000000, -0.000000000000000000 ) ) ;
#32509 = FACE_OUTER_BOUND ( 'NONE', #69390, .T. ) ;
#32512 = AXIS2_PLACEMENT_3D ( 'NONE', #247098, #208009, #167603 ) ;
#32513 = CARTESIAN_POINT ( 'NONE',  ( 23.14999999999999858, 53.66153320161009788, -235.9075159595686841 ) ) ;
#32514 = CARTESIAN_POINT ( 'NONE',  ( -18.46907102845853288, 85.47372736477593946, -96.34707274578771319 ) ) ;
#32515 = ORIENTED_EDGE ( 'NONE', *, *, #194208, .T. ) ;
#32516 = CARTESIAN_POINT ( 'NONE',  ( 21.14999999999999858, 69.45934304831041572, -69.52310748452435973 ) ) ;
#32517 = EDGE_CURVE ( 'NONE', #89986, #228873, #224202, .T. ) ;
#32518 = CARTESIAN_POINT ( 'NONE',  ( -23.25000000000000355, 64.25000000001161027, -60.27310748452440947 ) ) ;
#32519 = DIRECTION ( 'NONE',  ( -1.000000000000000000, -0.000000000000000000, -0.000000000000000000 ) ) ;
#32521 = ORIENTED_EDGE ( 'NONE', *, *, #44968, .F. ) ;
#32520 = CARTESIAN_POINT ( 'NONE',  ( 18.50000000000000000, 29.81973725181491730, -263.0247672247078867 ) ) ;
#32522 = AXIS2_PLACEMENT_3D ( 'NONE', #225453, #108104, #143365 ) ;
#32523 = ORIENTED_EDGE ( 'NONE', *, *, #190891, .F. ) ;
#32524 = CARTESIAN_POINT ( 'NONE',  ( -17.27223548804520803, 10.34539739142213222, -111.8663938208072182 ) ) ;
#32525 = DIRECTION ( 'NONE',  ( -1.000000000000000000, 0.000000000000000000, 0.000000000000000000 ) ) ;
#32526 = CARTESIAN_POINT ( 'NONE',  ( -23.15000000000000213, 62.92003201576280702, -207.2439188921395896 ) ) ;
#32527 = AXIS2_PLACEMENT_3D ( 'NONE', #203367, #186381, #123835 ) ;
#32528 = DIRECTION ( 'NONE',  ( 0.000000000000000000, 0.8660254037844420383, -0.4999999999999943379 ) ) ;
#32529 = ORIENTED_EDGE ( 'NONE', *, *, #28244, .T. ) ;
#32530 = FACE_OUTER_BOUND ( 'NONE', #71294, .T. ) ;
#32531 = FACE_OUTER_BOUND ( 'NONE', #29470, .T. ) ;
#32532 = CARTESIAN_POINT ( 'NONE',  ( 20.94999999999999929, 87.65000000001246860, -173.0231074845243029 ) ) ;
#32533 = ORIENTED_EDGE ( 'NONE', *, *, #19645, .F. ) ;
#32534 = CYLINDRICAL_SURFACE ( 'NONE', #154553, 2.000000000000012879 ) ;
#32535 = CARTESIAN_POINT ( 'NONE',  ( 21.14999999999999503, 64.25000000001195133, -103.0231074845244024 ) ) ;
#32536 = ORIENTED_EDGE ( 'NONE', *, *, #221025, .T. ) ;
#32537 = AXIS2_PLACEMENT_3D ( 'NONE', #108387, #9277, #88790 ) ;
#32538 = CIRCLE ( 'NONE', #144908, 0.09999999999999939493 ) ;
#32539 = FACE_OUTER_BOUND ( 'NONE', #11232, .T. ) ;
#32540 = AXIS2_PLACEMENT_3D ( 'NONE', #34929, #114428, #174452 ) ;
#32541 = EDGE_CURVE ( 'NONE', #217845, #173295, #27445, .T. ) ;
#32542 = ORIENTED_EDGE ( 'NONE', *, *, #230813, .T. ) ;
#32543 = EDGE_LOOP ( 'NONE', ( #163790, #202314, #210711, #164596 ) ) ;
#32544 = CARTESIAN_POINT ( 'NONE',  ( 21.05000000000000071, 70.15000000001178648, -79.65560470880227228 ) ) ;
#32545 = ORIENTED_EDGE ( 'NONE', *, *, #79324, .T. ) ;
#32547 = EDGE_LOOP ( 'NONE', ( #28162, #67262 ) ) ;
#32546 = DIRECTION ( 'NONE',  ( -1.000000000000000000, 0.000000000000000000, 0.000000000000000000 ) ) ;
#32548 = ADVANCED_FACE ( 'NONE', ( #241229, #159136 ), #20909, .T. ) ;
#32549 = VERTEX_POINT ( 'NONE', #142103 ) ;
#32552 = VERTEX_POINT ( 'NONE', #62582 ) ;
#32551 = ORIENTED_EDGE ( 'NONE', *, *, #41269, .F. ) ;
#32550 = DIRECTION ( 'NONE',  ( 1.073024830501117725E-15, 0.000000000000000000, 1.000000000000000000 ) ) ;
#32553 = EDGE_CURVE ( 'NONE', #97608, #237457, #206467, .T. ) ;
#32554 = VECTOR ( 'NONE', #72134, 1000.000000000000000 ) ;
#32555 = EDGE_CURVE ( 'NONE', #132925, #2821, #43958, .T. ) ;
#32556 = CARTESIAN_POINT ( 'NONE',  ( 20.94999999999999929, 6.650000000011155876, -54.75000000000000000 ) ) ;
#32557 = CIRCLE ( 'NONE', #236516, 0.09999999999999939493 ) ;
#32558 = VERTEX_POINT ( 'NONE', #245060 ) ;
#32559 = DIRECTION ( 'NONE',  ( 1.000000000000000000, -0.000000000000000000, 0.000000000000000000 ) ) ;
#32560 = DIRECTION ( 'NONE',  ( 0.000000000000000000, -0.1350103645451807555, -0.9908441862701610203 ) ) ;
#32561 = DIRECTION ( 'NONE',  ( -3.265361837132813093E-16, -0.9651348961777155289, 0.2617529984165037904 ) ) ;
#32562 = DIRECTION ( 'NONE',  ( 1.000000000000000000, 0.000000000000000000, 0.000000000000000000 ) ) ;
#32563 = CIRCLE ( 'NONE', #44995, 0.2000000000000005107 ) ;
#32564 = DIRECTION ( 'NONE',  ( 0.000000000000000000, -0.9999176327611369874, 0.01283462868041987913 ) ) ;
#32565 = ORIENTED_EDGE ( 'NONE', *, *, #12507, .T. ) ;
#32566 = ORIENTED_EDGE ( 'NONE', *, *, #239328, .T. ) ;
#32567 = ORIENTED_EDGE ( 'NONE', *, *, #209381, .T. ) ;
#32568 = CARTESIAN_POINT ( 'NONE',  ( -23.15000000000000213, 4.150000000011156764, -122.2500000000000284 ) ) ;
#32570 = ORIENTED_EDGE ( 'NONE', *, *, #148095, .T. ) ;
#32569 = CARTESIAN_POINT ( 'NONE',  ( -16.93860193097148326, 66.00689223268328476, -182.6229691172175933 ) ) ;
#32571 = DIRECTION ( 'NONE',  ( 0.000000000000000000, 0.000000000000000000, 1.000000000000000000 ) ) ;
#32573 = ORIENTED_EDGE ( 'NONE', *, *, #65028, .F. ) ;
#32572 = DIRECTION ( 'NONE',  ( 0.000000000000000000, 0.000000000000000000, -1.000000000000000000 ) ) ;
#32574 = ADVANCED_FACE ( 'NONE', ( #89821 ), #239799, .T. ) ;
#32575 = ORIENTED_EDGE ( 'NONE', *, *, #97664, .F. ) ;
#32576 = CARTESIAN_POINT ( 'NONE',  ( -23.25000000000000000, -11.64999999998884483, -21.75000000000000355 ) ) ;
#32577 = ADVANCED_FACE ( 'NONE', ( #168140 ), #48245, .T. ) ;
#32579 = ORIENTED_EDGE ( 'NONE', *, *, #98097, .F. ) ;
#32578 = PRODUCT_DEFINITION ( 'UNKNOWN', '', #15469, #94935 ) ;
#32580 = CARTESIAN_POINT ( 'NONE',  ( -16.87401514999234919, 9.950000000011137047, -180.2199820074678769 ) ) ;
#32581 = FACE_OUTER_BOUND ( 'NONE', #257660, .T. ) ;
#32582 = AXIS2_PLACEMENT_3D ( 'NONE', #158686, #175664, #217319 ) ;
#32583 = CIRCLE ( 'NONE', #16007, 0.09999999999999939493 ) ;
#32585 = ORIENTED_EDGE ( 'NONE', *, *, #224730, .F. ) ;
#32584 = ORIENTED_EDGE ( 'NONE', *, *, #176332, .T. ) ;
#32586 = VERTEX_POINT ( 'NONE', #246348 ) ;
#32587 = SPHERICAL_SURFACE ( 'NONE', #244395, 0.1000000000000000056 ) ;
#32588 = ORIENTED_EDGE ( 'NONE', *, *, #208917, .T. ) ;
#32589 = VERTEX_POINT ( 'NONE', #105513 ) ;
#32590 = EDGE_CURVE ( 'NONE', #207953, #225579, #205930, .T. ) ;
#32591 = DIRECTION ( 'NONE',  ( 0.000000000000000000, 0.000000000000000000, -1.000000000000000000 ) ) ;
#32593 = ORIENTED_EDGE ( 'NONE', *, *, #251993, .T. ) ;
#32592 = DIRECTION ( 'NONE',  ( -1.000000000000000000, -1.836970198721029934E-16, 0.000000000000000000 ) ) ;
#32594 = ADVANCED_FACE ( 'NONE', ( #147239 ), #207234, .T. ) ;
#32595 = CARTESIAN_POINT ( 'NONE',  ( -18.59999999999999787, -9.499999999999998224, -12.15000000000000391 ) ) ;
#32596 = ADVANCED_FACE ( 'NONE', ( #70308 ), #190230, .T. ) ;
#32597 = CIRCLE ( 'NONE', #86689, 1.749999999999999778 ) ;
#32599 = CARTESIAN_POINT ( 'NONE',  ( 18.39999999999999858, -9.499999999988842703, -73.91465834296967330 ) ) ;
#32598 = CARTESIAN_POINT ( 'NONE',  ( 23.14999999999999858, 76.00000000001142553, -36.02310748452432421 ) ) ;
#32600 = DIRECTION ( 'NONE',  ( 0.000000000000000000, 1.000000000000000000, 7.116814260417668513E-15 ) ) ;
#32601 = DIRECTION ( 'NONE',  ( 1.000000000000000000, 0.000000000000000000, 0.000000000000000000 ) ) ;
#32602 = EDGE_LOOP ( 'NONE', ( #185301, #256011, #71061 ) ) ;
#32603 = ORIENTED_EDGE ( 'NONE', *, *, #153041, .T. ) ;
#32604 = CARTESIAN_POINT ( 'NONE',  ( 18.31325810956227684, 85.53638847601904160, -96.15466727821856807 ) ) ;
#32605 = DIRECTION ( 'NONE',  ( 1.000000000000000000, 0.000000000000000000, 0.000000000000000000 ) ) ;
#32606 = CARTESIAN_POINT ( 'NONE',  ( -18.38817693311004575, 64.51850848411172024, -45.27310748452440947 ) ) ;
#32607 = ORIENTED_EDGE ( 'NONE', *, *, #10552, .T. ) ;
#32608 = CIRCLE ( 'NONE', #11740, 0.09999999999998898659 ) ;
#32609 = AXIS2_PLACEMENT_3D ( 'NONE', #238835, #118904, #40677 ) ;
#32610 = CARTESIAN_POINT ( 'NONE',  ( -16.93521499325732549, 51.65267039475685351, -231.8822487893360176 ) ) ;
#32611 = CIRCLE ( 'NONE', #65880, 0.1000000000000043771 ) ;
#32612 = EDGE_LOOP ( 'NONE', ( #120994, #207395, #84500 ) ) ;
#32613 = VERTEX_POINT ( 'NONE', #247627 ) ;
#32614 = LINE ( 'NONE', #76828, #1038 ) ;
#32615 = CARTESIAN_POINT ( 'NONE',  ( 20.94999999999999574, -1.835341550213255957, -45.15515129256298366 ) ) ;
#32616 = ORIENTED_EDGE ( 'NONE', *, *, #134121, .F. ) ;
#32617 = DIRECTION ( 'NONE',  ( 0.000000000000000000, 1.000000000000000000, 0.000000000000000000 ) ) ;
#32619 = ORIENTED_EDGE ( 'NONE', *, *, #200063, .F. ) ;
#32618 = APPLICATION_CONTEXT ( 'automotive_design' ) ;
#32620 = CARTESIAN_POINT ( 'NONE',  ( 18.48197441911542072, -9.517954794695242526, -140.8902116422106872 ) ) ;
#32621 = CARTESIAN_POINT ( 'NONE',  ( 20.85000000000000142, 67.23127455305835554, -235.8551265064784559 ) ) ;
#32623 = DIRECTION ( 'NONE',  ( 0.000000000000000000, 0.000000000000000000, 1.000000000000000000 ) ) ;
#32622 = CARTESIAN_POINT ( 'NONE',  ( -18.39999999999999858, 11.47316190337362762, -109.8259460668080152 ) ) ;
#32624 = DIRECTION ( 'NONE',  ( -0.000000000000000000, -0.8700118002898321601, 0.4930308989875230030 ) ) ;
#32625 = DIRECTION ( 'NONE',  ( 0.000000000000000000, -6.982962677686266711E-15, 1.000000000000000000 ) ) ;
#32626 = ADVANCED_FACE ( 'NONE', ( #69014 ), #208522, .T. ) ;
#32627 = AXIS2_PLACEMENT_3D ( 'NONE', #112578, #105129, #113846 ) ;
#32629 = ORIENTED_EDGE ( 'NONE', *, *, #176643, .F. ) ;
#32628 = CARTESIAN_POINT ( 'NONE',  ( -23.25000000000000000, 76.10085836911075319, -114.7726746080137019 ) ) ;
#32632 = ORIENTED_EDGE ( 'NONE', *, *, #215464, .T. ) ;
#32631 = VERTEX_POINT ( 'NONE', #106818 ) ;
#32630 = CIRCLE ( 'NONE', #153435, 0.1000000000000011990 ) ;
#32633 = ORIENTED_EDGE ( 'NONE', *, *, #29561, .F. ) ;
#32634 =( GEOMETRIC_REPRESENTATION_CONTEXT ( 3 ) GLOBAL_UNCERTAINTY_ASSIGNED_CONTEXT ( ( #197955 ) ) GLOBAL_UNIT_ASSIGNED_CONTEXT ( ( #1399, #138334, #174974 ) ) REPRESENTATION_CONTEXT ( 'NONE', 'WORKASPACE' ) );
#32635 = CIRCLE ( 'NONE', #153630, 0.09999999999999939493 ) ;
#32636 = AXIS2_PLACEMENT_3D ( 'NONE', #56262, #177553, #159255 ) ;
#32637 = ADVANCED_FACE ( 'NONE', ( #130233 ), #23137, .T. ) ;
#32638 = CARTESIAN_POINT ( 'NONE',  ( -23.25000000000000000, 1.115600667400684642E-11, -134.0000000000000000 ) ) ;
#32639 =( BOUNDED_SURFACE ( )  B_SPLINE_SURFACE ( 3, 2, ( 
 ( #190921, #156926, #236428 ),
 ( #210465, #33145, #151791 ),
 ( #112641, #73542, #153091 ),
 ( #117768, #4226, #163329 ),
 ( #103324, #199896, #82462 ),
 ( #197298, #19977, #182898 ),
 ( #139882, #99464, #177771 ),
 ( #61650, #239008, #59044 ),
 ( #240297, #57777, #21271 ),
 ( #100732, #198583, #60355 ) ),
 .UNSPECIFIED., .F., .F., .F. ) 
 B_SPLINE_SURFACE_WITH_KNOTS ( ( 4, 2, 2, 2, 4 ),
 ( 3, 3 ),
 ( 0.0001836757140119223738, 0.0004000170051583624682, 0.0005081876507315825561, 0.0005622729735181925459, 0.0006163582963048025356 ),
 ( 0.000000000000000000, 1.000000000000000000 ),
 .UNSPECIFIED. ) 
 GEOMETRIC_REPRESENTATION_ITEM ( )  RATIONAL_B_SPLINE_SURFACE ( (
 ( 1.000000000000000000, 0.7071067811865475727, 1.000000000000000000),
 ( 1.000000000000000000, 0.6461995200020562713, 1.000000000000000000),
 ( 1.000000000000000000, 0.5776453529561037525, 1.000000000000000000),
 ( 1.000000000000000000, 0.4585233068345877516, 1.000000000000000000),
 ( 1.000000000000000000, 0.4154092989934964342, 1.000000000000000000),
 ( 1.000000000000000000, 0.3550093145838849051, 1.000000000000000000),
 ( 1.000000000000000000, 0.3354498651684990618, 1.000000000000000000),
 ( 1.000000000000000000, 0.3060347992256760019, 1.000000000000000000),
 ( 1.000000000000000000, 0.2963555829626124960, 1.000000000000000000),
 ( 1.000000000000000000, 0.2966190024560606542, 1.000000000000000000) ) ) 
 REPRESENTATION_ITEM ( '' )  SURFACE ( )  );
#32640 = DIRECTION ( 'NONE',  ( 0.000000000000000000, 0.8660254037844411501, 0.4999999999999956701 ) ) ;
#32641 = AXIS2_PLACEMENT_3D ( 'NONE', #33230, #127152, #107577 ) ;
#32643 = DIRECTION ( 'NONE',  ( 1.000000000000000000, 0.000000000000000000, -0.000000000000000000 ) ) ;
#32642 = FACE_OUTER_BOUND ( 'NONE', #121705, .T. ) ;
#32644 = DIRECTION ( 'NONE',  ( 0.000000000000000000, 0.4930308989875575865, 0.8700118002898125091 ) ) ;
#32645 = ORIENTED_EDGE ( 'NONE', *, *, #230502, .F. ) ;
#32646 = EDGE_CURVE ( 'NONE', #58739, #220374, #149831, .T. ) ;
#32647 = CARTESIAN_POINT ( 'NONE',  ( -20.64999999999999858, 76.00000000001215028, -138.4231074845243654 ) ) ;
#32648 = ORIENTED_EDGE ( 'NONE', *, *, #27000, .F. ) ;
#32649 = EDGE_LOOP ( 'NONE', ( #191886, #49503, #117546, #144557 ) ) ;
#32650 = LINE ( 'NONE', #194279, #108575 ) ;
#32651 = CARTESIAN_POINT ( 'NONE',  ( -22.39999999999999858, 1.115600667400684642E-11, -88.85042919245522341 ) ) ;
#32652 = EDGE_CURVE ( 'NONE', #190860, #118040, #6442, .T. ) ;
#32653 = DIRECTION ( 'NONE',  ( 0.000000000000000000, 0.000000000000000000, -1.000000000000000000 ) ) ;
#32654 = AXIS2_PLACEMENT_3D ( 'NONE', #30921, #186111, #227793 ) ;
#32655 = AXIS2_PLACEMENT_3D ( 'NONE', #164792, #86496, #241749 ) ;
#32656 = CARTESIAN_POINT ( 'NONE',  ( -23.15000000000000213, 1.115600667400684642E-11, -167.4999999999999716 ) ) ;
#32657 = EDGE_CURVE ( 'NONE', #147024, #187556, #48138, .T. ) ;
#32659 = CLOSED_SHELL ( 'NONE', ( #62020, #5838, #131662, #27433, #249797, #5445, #11819, #68124, #227541, #137983, #179382, #214191, #223780, #254883, #206002, #53684, #65490, #132113, #253059, #70634, #39872, #236641, #118568, #31279, #226539, #22775, #221626, #14149, #120296, #60730, #22917, #116489, #156775, #353, #190736, #140390, #217402, #33417, #81335, #123610, #165362, #100554, #158569, #1955, #26811, #215907, #48390, #36232, #130134, #107997, #142180, #135197, #144598 ) ) ;
#32658 = CARTESIAN_POINT ( 'NONE',  ( 22.40000000000020819, -0.1008583690885111045, -155.7504328765102457 ) ) ;
#32660 = EDGE_CURVE ( 'NONE', #167893, #69230, #102190, .T. ) ;
#32661 = ORIENTED_EDGE ( 'NONE', *, *, #215935, .F. ) ;
#32662 = ORIENTED_EDGE ( 'NONE', *, *, #134953, .T. ) ;
#32663 = CYLINDRICAL_SURFACE ( 'NONE', #74974, 0.1000000000000028644 ) ;
#32664 = CARTESIAN_POINT ( 'NONE',  ( -16.86445178670632217, 9.962211629127168067, -54.39077743811736099 ) ) ;
#32665 = DIRECTION ( 'NONE',  ( 0.7071067811865463515, -0.6824534298470387172, 0.1850873201762205933 ) ) ;
#32666 = DIRECTION ( 'NONE',  ( 1.000000000000000000, 0.000000000000000000, 0.000000000000000000 ) ) ;
#32667 = DIRECTION ( 'NONE',  ( 0.000000000000000000, 0.1618390714546045217, 0.9868171638914230437 ) ) ;
#32668 = DIRECTION ( 'NONE',  ( -0.7071067811865474617, -0.6909108974501236844, -0.1504730267678055788 ) ) ;
#32669 = EDGE_LOOP ( 'NONE', ( #255588, #20746, #15018, #45547, #38966, #204075, #152049, #35069, #46255, #144096, #150895, #127112, #83547, #232887, #79013, #84282 ) ) ;
#32670 = CARTESIAN_POINT ( 'NONE',  ( -18.59999999999999787, 9.350000000011156942, -112.8500000000000369 ) ) ;
#32671 = CARTESIAN_POINT ( 'NONE',  ( -21.53752568617666441, 6.786807874515170980, -33.40102553874074687 ) ) ;
#32672 = VECTOR ( 'NONE', #43840, 1000.000000000000000 ) ;
#32674 = DIRECTION ( 'NONE',  ( -1.000000000000000000, -1.652117596168391700E-15, -1.153667551319263085E-29 ) ) ;
#32673 = DIRECTION ( 'NONE',  ( 0.000000000000000000, 0.8814952561688430555, -0.4721928772777346239 ) ) ;
#32675 = CARTESIAN_POINT ( 'NONE',  ( -20.54999999999999716, 1.115600667400684642E-11, -134.0000000000000000 ) ) ;
#32676 = CARTESIAN_POINT ( 'NONE',  ( 18.59999999999999076, 10.49142135624846439, -158.8500000000000227 ) ) ;
#32677 = CARTESIAN_POINT ( 'NONE',  ( -18.50000000000000000, 9.350000000011156942, -45.85000000000000142 ) ) ;
#32679 = CARTESIAN_POINT ( 'NONE',  ( 20.88420186297724612, 10.33025634372637391, -139.5870929282639281 ) ) ;
#32678 = AXIS2_PLACEMENT_3D ( 'NONE', #47095, #126656, #184057 ) ;
#32681 = VERTEX_POINT ( 'NONE', #166845 ) ;
#32680 = CARTESIAN_POINT ( 'NONE',  ( 23.15000000000000213, -11.64999999998883595, -97.40000000000004832 ) ) ;
#32682 = EDGE_CURVE ( 'NONE', #93742, #374, #126676, .T. ) ;
#32683 = EDGE_CURVE ( 'NONE', #74935, #85530, #110603, .T. ) ;
#32684 = AXIS2_PLACEMENT_3D ( 'NONE', #26177, #206089, #87407 ) ;
#32685 = EDGE_CURVE ( 'NONE', #128006, #250275, #148397, .T. ) ;
#32686 = DIRECTION ( 'NONE',  ( 0.7071067811865487940, 4.851104656540973741E-15, -0.7071067811865463515 ) ) ;
#32687 = AXIS2_PLACEMENT_3D ( 'NONE', #6909, #129428, #86416 ) ;
#32688 = CARTESIAN_POINT ( 'NONE',  ( -22.50000000000000000, 64.25043287652256652, -103.1239658536230763 ) ) ;
#32689 = CIRCLE ( 'NONE', #11823, 0.09999999999999609201 ) ;
#32690 = VECTOR ( 'NONE', #9226, 1000.000000000000114 ) ;
#32691 = EDGE_CURVE ( 'NONE', #256568, #28814, #36301, .T. ) ;
#32692 = FACE_OUTER_BOUND ( 'NONE', #45627, .T. ) ;
#32693 = CIRCLE ( 'NONE', #178417, 0.09999999999999939493 ) ;
#32695 = EDGE_CURVE ( 'NONE', #167246, #138331, #123251, .T. ) ;
#32694 = CARTESIAN_POINT ( 'NONE',  ( 20.97239005616515328, 8.874843841361279573, -45.75015280215318825 ) ) ;
#32696 = DIRECTION ( 'NONE',  ( 1.000000000000000000, 0.000000000000000000, 0.000000000000000000 ) ) ;
#32697 = AXIS2_PLACEMENT_3D ( 'NONE', #121695, #129060, #148634 ) ;
#32698 = PLANE ( 'NONE',  #109754 ) ;
#32699 = LINE ( 'NONE', #131746, #211728 ) ;
#32700 = DIRECTION ( 'NONE',  ( 1.000000000000000000, 0.000000000000000000, 0.000000000000000000 ) ) ;
#32701 = ORIENTED_EDGE ( 'NONE', *, *, #31219, .F. ) ;
#32702 = DIRECTION ( 'NONE',  ( 0.000000000000000000, 0.000000000000000000, 1.000000000000000000 ) ) ;
#32704 = ORIENTED_EDGE ( 'NONE', *, *, #100716, .T. ) ;
#32703 = CARTESIAN_POINT ( 'NONE',  ( 18.59999999999999787, -10.80884033489985363, 5.900000000000001243 ) ) ;
#32705 = CARTESIAN_POINT ( 'NONE',  ( -17.04761207306819060, 44.10422576783453508, -235.2291619687160562 ) ) ;
#32706 = ADVANCED_FACE ( 'NONE', ( #211072 ), #169083, .T. ) ;
#32707 = DIRECTION ( 'NONE',  ( 0.000000000000000000, -0.1350103645451945777, 0.9908441862701590219 ) ) ;
#32708 = VERTEX_POINT ( 'NONE', #54555 ) ;
#32709 = DIRECTION ( 'NONE',  ( 1.875376730785737719E-16, -1.000000000000000000, 0.000000000000000000 ) ) ;
#32710 = EDGE_CURVE ( 'NONE', #26533, #41617, #76679, .T. ) ;
#32711 = AXIS2_PLACEMENT_3D ( 'NONE', #216166, #37560, #157536 ) ;
#32712 = APPLICATION_PROTOCOL_DEFINITION ( 'draft international standard', 'automotive_design', 1998, #195588 ) ;
#32713 = DIRECTION ( 'NONE',  ( 0.000000000000000000, -6.982962677686266711E-15, 1.000000000000000000 ) ) ;
#32714 = DIRECTION ( 'NONE',  ( -1.000000000000000000, 0.000000000000000000, 0.000000000000000000 ) ) ;
#32715 = EDGE_LOOP ( 'NONE', ( #214285, #238107, #240047, #201951 ) ) ;
#32716 = CYLINDRICAL_SURFACE ( 'NONE', #87930, 0.5000000000000004441 ) ;
#32717 = DIRECTION ( 'NONE',  ( 1.000000000000000000, 0.000000000000000000, 0.000000000000000000 ) ) ;
#32718 = DIRECTION ( 'NONE',  ( -1.000000000000000000, -0.000000000000000000, 0.000000000000000000 ) ) ;
#32719 = ORIENTED_EDGE ( 'NONE', *, *, #98257, .F. ) ;
#32720 = VERTEX_POINT ( 'NONE', #175811 ) ;
#32721 = DIRECTION ( 'NONE',  ( 0.000000000000000000, -1.000000000000000000, -6.982962677686266711E-15 ) ) ;
#32722 = DIRECTION ( 'NONE',  ( 0.000000000000000000, -0.4088369013363280513, 0.9126074666063769270 ) ) ;
#32723 = LINE ( 'NONE', #170960, #77503 ) ;
#32724 = CARTESIAN_POINT ( 'NONE',  ( 20.94999999999999574, 87.65000000001212754, -133.6231074845242119 ) ) ;
#32726 = DIRECTION ( 'NONE',  ( 1.000000000000000000, 0.000000000000000000, 0.000000000000000000 ) ) ;
#32725 = DIRECTION ( 'NONE',  ( 0.000000000000000000, 1.000000000000000000, 0.000000000000000000 ) ) ;
#32727 = TOROIDAL_SURFACE ( 'NONE', #149225, 4.149999999999999467, 0.1000000000000000056 ) ;
#32729 = CARTESIAN_POINT ( 'NONE',  ( 18.49999999999999289, 63.61019970229975229, -209.1253633388161006 ) ) ;
#32728 = VECTOR ( 'NONE', #81266, 1000.000000000000000 ) ;
#32730 = AXIS2_PLACEMENT_3D ( 'NONE', #115387, #159666, #20159 ) ;
#32731 = DIRECTION ( 'NONE',  ( 1.000000000000000000, 0.000000000000000000, 0.000000000000000000 ) ) ;
#32732 = ORIENTED_EDGE ( 'NONE', *, *, #22736, .T. ) ;
#32733 = EDGE_CURVE ( 'NONE', #76006, #173652, #53285, .T. ) ;
#32735 = VERTEX_POINT ( 'NONE', #136648 ) ;
#32734 = FACE_OUTER_BOUND ( 'NONE', #39998, .T. ) ;
#32736 = CARTESIAN_POINT ( 'NONE',  ( 21.13498764882293557, 69.50438185653851519, -170.0247638792557439 ) ) ;
#32737 = FACE_OUTER_BOUND ( 'NONE', #97242, .T. ) ;
#32738 = FACE_OUTER_BOUND ( 'NONE', #72940, .T. ) ;
#32739 =( BOUNDED_SURFACE ( )  B_SPLINE_SURFACE ( 3, 2, ( 
 ( #10875, #171278, #167399 ),
 ( #152985, #249492, #89115 ),
 ( #129537, #111256, #250753 ),
 ( #151698, #9573, #209068 ) ),
 .UNSPECIFIED., .F., .F., .F. ) 
 B_SPLINE_SURFACE_WITH_KNOTS ( ( 4, 4 ),
 ( 3, 3 ),
 ( 0.04058434257139476031, 0.04256401539001599538 ),
 ( 0.000000000000000000, 1.000000000000000000 ),
 .UNSPECIFIED. ) 
 GEOMETRIC_REPRESENTATION_ITEM ( )  RATIONAL_B_SPLINE_SURFACE ( (
 ( 1.000000000000000000, 0.7103081912007810361, 1.000000000000000000),
 ( 1.000000000000000000, 0.7104998333556836743, 1.000000000000000000),
 ( 1.000000000000000000, 0.7107238315753999780, 1.000000000000000000),
 ( 1.000000000000000000, 0.7110073749539779220, 1.000000000000000000) ) ) 
 REPRESENTATION_ITEM ( '' )  SURFACE ( )  );
#32740 = ORIENTED_EDGE ( 'NONE', *, *, #231012, .T. ) ;
#32741 = FACE_OUTER_BOUND ( 'NONE', #48059, .T. ) ;
#32742 = FACE_OUTER_BOUND ( 'NONE', #52029, .T. ) ;
#32743 = CARTESIAN_POINT ( 'NONE',  ( 22.49436431346199683, 11.64995094766461392, -133.9330964702777749 ) ) ;
#32744 = DIRECTION ( 'NONE',  ( -0.000000000000000000, 0.2128009952263604232, -0.9770955615653316162 ) ) ;
#32745 = EDGE_LOOP ( 'NONE', ( #163859, #77482, #121420, #176805 ) ) ;
#32746 = EDGE_LOOP ( 'NONE', ( #235895, #42147, #63179, #40969 ) ) ;
#32747 = CIRCLE ( 'NONE', #107709, 0.1000000000000028644 ) ;
#32749 = VECTOR ( 'NONE', #146243, 1000.000000000000000 ) ;
#32748 = DIRECTION ( 'NONE',  ( 0.000000000000000000, 0.9126074666063660468, 0.4088369013363524762 ) ) ;
#32750 = ORIENTED_EDGE ( 'NONE', *, *, #4381, .T. ) ;
#32751 = ADVANCED_FACE ( 'NONE', ( #216183 ), #117109, .F. ) ;
#32752 = DIRECTION ( 'NONE',  ( 0.000000000000000000, 1.000000000000000000, 7.272083257015735086E-15 ) ) ;
#32754 = DIRECTION ( 'NONE',  ( 0.000000000000000000, -0.8814952561688431665, 0.4721928772777346794 ) ) ;
#32753 = AXIS2_PLACEMENT_3D ( 'NONE', #205735, #67512, #45386 ) ;
#32755 = CARTESIAN_POINT ( 'NONE',  ( -21.08078803292166725, 65.49716426111221779, -241.9466111468314296 ) ) ;
#32756 = CARTESIAN_POINT ( 'NONE',  ( 21.00000000000000000, 9.749999999999998224, -12.25000000000000000 ) ) ;
#32757 = ORIENTED_EDGE ( 'NONE', *, *, #16754, .T. ) ;
#32758 = LINE ( 'NONE', #250470, #63953 ) ;
#32759 = B_SPLINE_CURVE_WITH_KNOTS ( 'NONE', 3,
 ( #30634, #245810, #47585, #247070, #51421, #170170, #206679, #141883, #11046, #90567, #249666, #71043, #150563 ),
 .UNSPECIFIED., .F., .F.,
 ( 4, 3, 3, 3, 4 ),
 ( 1.080553112431203744E-16, 1.946463881814594965E-05, 3.922356109943912858E-05, 4.215060953238345049E-05, 4.415117091092495043E-05 ),
 .UNSPECIFIED. ) ;
#32760 = CARTESIAN_POINT ( 'NONE',  ( 20.95512820512820440, 65.37615131629962661, -48.27310748452439526 ) ) ;
#32761 = FACE_OUTER_BOUND ( 'NONE', #151018, .T. ) ;
#32762 = CYLINDRICAL_SURFACE ( 'NONE', #4248, 0.1000000000000028644 ) ;
#32763 = DIRECTION ( 'NONE',  ( 1.000000000000000000, 0.000000000000000000, 0.000000000000000000 ) ) ;
#32764 = CARTESIAN_POINT ( 'NONE',  ( 20.94999999999999574, 44.25095746879271985, -258.9156452930671435 ) ) ;
#32765 = CARTESIAN_POINT ( 'NONE',  ( -20.64999999999999858, 1.925233644870967487, -54.26975646687386501 ) ) ;
#32766 = VECTOR ( 'NONE', #183362, 1000.000000000000000 ) ;
#32767 = VERTEX_POINT ( 'NONE', #72878 ) ;
#32769 = CARTESIAN_POINT ( 'NONE',  ( 18.59999999999999076, 74.16465844978765176, -124.9679561919613207 ) ) ;
#32768 = LINE ( 'NONE', #155279, #161725 ) ;
#32771 = ORIENTED_EDGE ( 'NONE', *, *, #25936, .F. ) ;
#32770 = AXIS2_PLACEMENT_3D ( 'NONE', #6538, #148641, #206034 ) ;
#32773 = ORIENTED_EDGE ( 'NONE', *, *, #16699, .T. ) ;
#32772 = DIRECTION ( 'NONE',  ( 1.000000000000000000, 0.000000000000000000, 0.000000000000000000 ) ) ;
#32774 = AXIS2_PLACEMENT_3D ( 'NONE', #214850, #16675, #96173 ) ;
#32775 = ORIENTED_EDGE ( 'NONE', *, *, #108959, .F. ) ;
#32776 = CARTESIAN_POINT ( 'NONE',  ( 23.24999999999999289, 42.98415524044398950, -233.9519173640447889 ) ) ;
#32777 = CARTESIAN_POINT ( 'NONE',  ( 15.74999999999999645, 66.65000000001228386, -153.2731074845244166 ) ) ;
#32778 = CYLINDRICAL_SURFACE ( 'NONE', #14227, 0.09999999999999881206 ) ;
#32779 = VERTEX_POINT ( 'NONE', #77957 ) ;
#32780 = CARTESIAN_POINT ( 'NONE',  ( 18.49999999999998934, 65.75000000001149658, -44.87310748452439668 ) ) ;
#32781 = VECTOR ( 'NONE', #7548, 1000.000000000000000 ) ;
#32782 = CARTESIAN_POINT ( 'NONE',  ( 18.49999999999999289, 10.41716543472752399, -158.8499999994178040 ) ) ;
#32783 = EDGE_LOOP ( 'NONE', ( #167539, #126184, #71852, #127015 ) ) ;
#32784 = CARTESIAN_POINT ( 'NONE',  ( 18.59999999999999076, 11.65000000001115943, -91.85000000000003695 ) ) ;
#32785 = EDGE_CURVE ( 'NONE', #70123, #167341, #89928, .T. ) ;
#32786 = DIRECTION ( 'NONE',  ( 0.000000000000000000, 0.000000000000000000, 1.000000000000000000 ) ) ;
#32787 = VECTOR ( 'NONE', #139576, 1000.000000000000000 ) ;
#32788 = ORIENTED_EDGE ( 'NONE', *, *, #143834, .F. ) ;
#32789 = AXIS2_PLACEMENT_3D ( 'NONE', #27533, #129166, #148735 ) ;
#32790 = LINE ( 'NONE', #210120, #72825 ) ;
#32791 = AXIS2_PLACEMENT_3D ( 'NONE', #143412, #77328, #123866 ) ;
#32792 = VERTEX_POINT ( 'NONE', #17989 ) ;
#32793 = CARTESIAN_POINT ( 'NONE',  ( 18.55121869061587958, 65.67252876774529113, -97.44570419949944551 ) ) ;
#32795 = ORIENTED_EDGE ( 'NONE', *, *, #161133, .F. ) ;
#32794 = AXIS2_PLACEMENT_3D ( 'NONE', #155234, #258097, #234734 ) ;
#32796 = DIRECTION ( 'NONE',  ( 0.000000000000000000, -0.000000000000000000, -1.000000000000000000 ) ) ;
#32797 = EDGE_CURVE ( 'NONE', #72750, #215500, #157556, .T. ) ;
#32798 = CARTESIAN_POINT ( 'NONE',  ( -20.54999999999999716, 23.68770167995059595, -252.8127582590406348 ) ) ;
#32799 = PLANE ( 'NONE',  #118425 ) ;
#32800 = ADVANCED_FACE ( 'NONE', ( #177105 ), #154973, .F. ) ;
#32801 = CARTESIAN_POINT ( 'NONE',  ( 18.49999999999999289, 10.20857864377385127, -58.15000000000000568 ) ) ;
#32802 = AXIS2_PLACEMENT_3D ( 'NONE', #44788, #124328, #142579 ) ;
#32803 = AXIS2_PLACEMENT_3D ( 'NONE', #233472, #73126, #116080 ) ;
#32804 = DIRECTION ( 'NONE',  ( -1.000000000000000000, 0.000000000000000000, 0.000000000000000000 ) ) ;
#32806 = EDGE_CURVE ( 'NONE', #170828, #148530, #23341, .T. ) ;
#32805 = AXIS2_PLACEMENT_3D ( 'NONE', #224180, #83366, #165518 ) ;
#32807 = CARTESIAN_POINT ( 'NONE',  ( 18.39999999999999858, -9.499999999988844479, -73.60018939122204529 ) ) ;
#32808 = CARTESIAN_POINT ( 'NONE',  ( 20.27550659511089037, 9.216043722508839409, -20.85000000000000142 ) ) ;
#32809 = EDGE_LOOP ( 'NONE', ( #144487, #36061, #251282, #100000 ) ) ;
#32810 = CARTESIAN_POINT ( 'NONE',  ( 23.14999999999999858, 73.90000000001141700, -36.02310748452433842 ) ) ;
#32811 = ORIENTED_EDGE ( 'NONE', *, *, #234867, .F. ) ;
#32814 = VERTEX_POINT ( 'NONE', #111984 ) ;
#32813 = DIRECTION ( 'NONE',  ( 0.000000000000000000, 0.000000000000000000, 1.000000000000000000 ) ) ;
#32812 = CARTESIAN_POINT ( 'NONE',  ( -23.25000000000000000, 11.65000000001115588, -59.98519422934604961 ) ) ;
#32815 = AXIS2_PLACEMENT_3D ( 'NONE', #164414, #226945, #45738 ) ;
#32816 = ORIENTED_EDGE ( 'NONE', *, *, #59149, .T. ) ;
#32817 = DIRECTION ( 'NONE',  ( 1.000000000000000000, 0.000000000000000000, 0.000000000000000000 ) ) ;
#32818 = COLOUR_RGB ( '', 0.09019608, 0.27058824, 0.51372549) ;
#32819 = AXIS2_PLACEMENT_3D ( 'NONE', #3717, #203204, #162820 ) ;
#32820 = DIRECTION ( 'NONE',  ( -0.000000000000000000, -0.1480365673253065117, 0.9889818879709273425 ) ) ;
#32821 = AXIS2_PLACEMENT_3D ( 'NONE', #15902, #135798, #116268 ) ;
#32822 = DIRECTION ( 'NONE',  ( 1.000000000000000000, 0.000000000000000000, 0.000000000000000000 ) ) ;
#32823 = DIRECTION ( 'NONE',  ( 1.000000000000000000, -0.000000000000000000, -0.000000000000000000 ) ) ;
#32824 = ORIENTED_EDGE ( 'NONE', *, *, #85206, .F. ) ;
#32826 = ORIENTED_EDGE ( 'NONE', *, *, #163044, .T. ) ;
#32825 = CARTESIAN_POINT ( 'NONE',  ( 20.95392731769792150, 67.11693852082386513, -195.0008795049531329 ) ) ;
#32827 = VECTOR ( 'NONE', #177854, 1000.000000000000000 ) ;
#32828 = EDGE_CURVE ( 'NONE', #176547, #115707, #239983, .T. ) ;
#32830 = CARTESIAN_POINT ( 'NONE',  ( 18.58143601961950608, 15.46352952504945932, -222.9623815432983918 ) ) ;
#32829 = CARTESIAN_POINT ( 'NONE',  ( -23.15000000000000213, 25.30967299857550401, -243.4716794062925374 ) ) ;
#32832 = ORIENTED_EDGE ( 'NONE', *, *, #151028, .T. ) ;
#32831 = DIRECTION ( 'NONE',  ( -1.000000000000000000, 0.000000000000000000, 0.000000000000000000 ) ) ;
#32833 = PRODUCT ( 'Injection Molded Chain Links 13', 'Injection Molded Chain Links 13', '', ( #95206 ) ) ;
#32834 = ORIENTED_EDGE ( 'NONE', *, *, #151707, .F. ) ;
#32835 = VECTOR ( 'NONE', #28043, 1000.000000000000000 ) ;
#32836 = VECTOR ( 'NONE', #178947, 1000.000000000000000 ) ;
#32837 = CARTESIAN_POINT ( 'NONE',  ( 20.95512820512820440, 12.01161663143393632, -206.2285874551107554 ) ) ;
#32838 = CARTESIAN_POINT ( 'NONE',  ( -18.50000000000000000, 11.65000000001115232, -179.7499999999999716 ) ) ;
#32839 = ORIENTED_EDGE ( 'NONE', *, *, #50521, .F. ) ;
#32840 = DIRECTION ( 'NONE',  ( -0.000000000000000000, 0.8096735173027124199, -0.5868805631290358038 ) ) ;
#32841 = EDGE_LOOP ( 'NONE', ( #13320, #71010, #35867, #99462 ) ) ;
#32842 = CARTESIAN_POINT ( 'NONE',  ( -16.77683809663752257, 52.34166666667894674, -153.2731074845245303 ) ) ;
#32843 = CARTESIAN_POINT ( 'NONE',  ( -20.64999999999999858, 1.115600667400684642E-11, -46.37500000000000000 ) ) ;
#32844 = ORIENTED_EDGE ( 'NONE', *, *, #168846, .F. ) ;
#32845 = DIRECTION ( 'NONE',  ( 0.000000000000000000, -0.2617529984165031243, -0.9651348961777157509 ) ) ;
#32846 = EDGE_CURVE ( 'NONE', #140173, #47344, #174568, .T. ) ;
#32847 = PRODUCT_DEFINITION_CONTEXT ( 'detailed design', #162437, 'design' ) ;
#32848 = AXIS2_PLACEMENT_3D ( 'NONE', #254813, #198741, #16287 ) ;
#32849 = TOROIDAL_SURFACE ( 'NONE', #132781, 0.6000000000000006439, 0.1000000000000000056 ) ;
#32850 = AXIS2_PLACEMENT_3D ( 'NONE', #256815, #78226, #237319 ) ;
#32851 = CARTESIAN_POINT ( 'NONE',  ( -17.78043020864320667, 10.85359211201684637, -123.6630491657202668 ) ) ;
#32852 = CIRCLE ( 'NONE', #70265, 0.1000000000000013933 ) ;
#32853 = EDGE_CURVE ( 'NONE', #75688, #144175, #33765, .T. ) ;
#32854 = ORIENTED_EDGE ( 'NONE', *, *, #36553, .T. ) ;
#32855 = ORIENTED_EDGE ( 'NONE', *, *, #46103, .F. ) ;
#32856 = CARTESIAN_POINT ( 'NONE',  ( 18.60000000000000142, -9.321008403350125704, -107.7359382490779325 ) ) ;
#32857 = ORIENTED_EDGE ( 'NONE', *, *, #251332, .T. ) ;
#32858 = FACE_OUTER_BOUND ( 'NONE', #98511, .T. ) ;
#32859 = EDGE_LOOP ( 'NONE', ( #80990, #192450, #231165, #120100, #23857, #125199, #253172 ) ) ;
#32861 = ORIENTED_EDGE ( 'NONE', *, *, #5340, .T. ) ;
#32860 = CARTESIAN_POINT ( 'NONE',  ( 21.07928932188134397, 75.90110485435759813, -109.3516241409176217 ) ) ;
#32862 = EDGE_CURVE ( 'NONE', #250321, #233023, #2629, .T. ) ;
#32863 = ORIENTED_EDGE ( 'NONE', *, *, #139800, .F. ) ;
#32864 = DIRECTION ( 'NONE',  ( 0.000000000000000000, 0.9999631594459055250, 0.008583690987131395445 ) ) ;
#32865 = AXIS2_PLACEMENT_3D ( 'NONE', #205171, #26576, #106063 ) ;
#32866 = AXIS2_PLACEMENT_3D ( 'NONE', #249782, #234058, #248499 ) ;
#32867 = ORIENTED_EDGE ( 'NONE', *, *, #230628, .F. ) ;
#32868 = B_SPLINE_CURVE_WITH_KNOTS ( 'NONE', 3,
 ( #223184, #161964, #139791, #241483, #44566, #142369 ),
 .UNSPECIFIED., .F., .F.,
 ( 4, 2, 4 ),
 ( 0.000000000000000000, 0.0001497467027049222718, 0.0002994934054098445436 ),
 .UNSPECIFIED. ) ;
#32871 = ORIENTED_EDGE ( 'NONE', *, *, #161975, .F. ) ;
#32870 = EDGE_LOOP ( 'NONE', ( #234709, #193177, #113873, #14314 ) ) ;
#32869 = CARTESIAN_POINT ( 'NONE',  ( 21.05000000000000071, 87.65000000001236913, -170.0231074845242745 ) ) ;
#32872 = EDGE_CURVE ( 'NONE', #206239, #114885, #19208, .T. ) ;
#32873 = CARTESIAN_POINT ( 'NONE',  ( -23.25000000000000000, 44.29184115892635987, -259.0069060397277667 ) ) ;
#32874 = ORIENTED_EDGE ( 'NONE', *, *, #22927, .F. ) ;
#32875 = CARTESIAN_POINT ( 'NONE',  ( 21.10710606213542206, 8.776894023904366904, -45.74099652639942093 ) ) ;
#32876 = ORIENTED_EDGE ( 'NONE', *, *, #137508, .F. ) ;
#32877 = CARTESIAN_POINT ( 'NONE',  ( -16.93234230245721861, 9.998107370558241058, -154.9176902816662675 ) ) ;
#32878 = EDGE_CURVE ( 'NONE', #95060, #14729, #254032, .T. ) ;
#32880 = ORIENTED_EDGE ( 'NONE', *, *, #144939, .F. ) ;
#32879 = CYLINDRICAL_SURFACE ( 'NONE', #153196, 0.09999999999999939493 ) ;
#32881 = DIRECTION ( 'NONE',  ( 0.000000000000000000, 0.2128009952263601456, -0.9770955615653316162 ) ) ;
#32882 = ORIENTED_EDGE ( 'NONE', *, *, #134713, .F. ) ;
#32883 = CARTESIAN_POINT ( 'NONE',  ( 20.94999999999999929, 76.00000000001168132, -65.42310748452432279 ) ) ;
#32884 = CARTESIAN_POINT ( 'NONE',  ( -22.94999999999999929, 5.488301202077012775, 16.40000000000000213 ) ) ;
#32885 = AXIS2_PLACEMENT_3D ( 'NONE', #233205, #36283, #51946 ) ;
#32887 = VERTEX_POINT ( 'NONE', #122241 ) ;
#32886 = EDGE_CURVE ( 'NONE', #83171, #20283, #194201, .T. ) ;
#32888 = EDGE_CURVE ( 'NONE', #110926, #257982, #162656, .T. ) ;
#32889 = CARTESIAN_POINT ( 'NONE',  ( 18.49999999999999645, 74.13328508995475374, -124.7704322382423072 ) ) ;
#32890 = CARTESIAN_POINT ( 'NONE',  ( 18.56579813702274961, 18.41141989892753372, -236.9935361838138022 ) ) ;
#32891 = ORIENTED_EDGE ( 'NONE', *, *, #92069, .F. ) ;
#32893 = VERTEX_POINT ( 'NONE', #139202 ) ;
#32892 = DIRECTION ( 'NONE',  ( -0.000000000000000000, -0.000000000000000000, -1.000000000000000000 ) ) ;
#32894 = CARTESIAN_POINT ( 'NONE',  ( 20.94999999999999929, 71.00000000001199396, -114.9283735034374274 ) ) ;
#32895 = EDGE_CURVE ( 'NONE', #156851, #155989, #85808, .T. ) ;
#32897 = ORIENTED_EDGE ( 'NONE', *, *, #63569, .T. ) ;
#32896 = VERTEX_POINT ( 'NONE', #42694 ) ;
#32898 = ORIENTED_EDGE ( 'NONE', *, *, #4857, .F. ) ;
#32899 = CARTESIAN_POINT ( 'NONE',  ( -16.94445028196807002, 9.992063609708893068, -54.39266982158155628 ) ) ;
#32900 = ORIENTED_EDGE ( 'NONE', *, *, #9740, .T. ) ;
#32901 = ORIENTED_EDGE ( 'NONE', *, *, #239815, .F. ) ;
#32902 = CARTESIAN_POINT ( 'NONE',  ( -18.40000000000000568, 30.96206749086277554, -233.4839438819913653 ) ) ;
#32903 = ORIENTED_EDGE ( 'NONE', *, *, #158209, .F. ) ;
#32904 = ADVANCED_FACE ( 'NONE', ( #221309 ), #160103, .T. ) ;
#32905 = CARTESIAN_POINT ( 'NONE',  ( 20.94999999999999574, -1.162701749926853712, -75.00000000000004263 ) ) ;
#32906 = EDGE_CURVE ( 'NONE', #179303, #143490, #35966, .T. ) ;
#32907 = DIRECTION ( 'NONE',  ( 1.000000000000000000, 0.000000000000000000, 0.000000000000000000 ) ) ;
#32908 = ORIENTED_EDGE ( 'NONE', *, *, #234361, .F. ) ;
#32909 = VERTEX_POINT ( 'NONE', #4823 ) ;
#32910 = VECTOR ( 'NONE', #6708, 1000.000000000000000 ) ;
#32911 = CARTESIAN_POINT ( 'NONE',  ( -15.55912972643740488, 8.490870273562565629, -20.85000000000000142 ) ) ;
#32912 = AXIS2_PLACEMENT_3D ( 'NONE', #15918, #234942, #35484 ) ;
#32913 = CIRCLE ( 'NONE', #99473, 11.65000000000000391 ) ;
#32914 = ORIENTED_EDGE ( 'NONE', *, *, #152628, .T. ) ;
#32915 = AXIS2_PLACEMENT_3D ( 'NONE', #62793, #24976, #100592 ) ;
#32916 = CARTESIAN_POINT ( 'NONE',  ( 23.04999999999999716, 8.822561741677553471, -76.25000000000004263 ) ) ;
#32917 = EDGE_LOOP ( 'NONE', ( #78405, #21904, #147763, #86234 ) ) ;
#32918 = EDGE_CURVE ( 'NONE', #189223, #201612, #127545, .T. ) ;
#32919 = ORIENTED_EDGE ( 'NONE', *, *, #200593, .T. ) ;
#32920 = EDGE_CURVE ( 'NONE', #121012, #111004, #43979, .T. ) ;
#32921 = DIRECTION ( 'NONE',  ( 1.000000000000000000, -0.000000000000000000, -0.000000000000000000 ) ) ;
#32923 = ORIENTED_EDGE ( 'NONE', *, *, #225315, .T. ) ;
#32922 = CARTESIAN_POINT ( 'NONE',  ( 18.49351773456780634, 85.44302569515740231, -162.8377819584964925 ) ) ;
#32924 = CARTESIAN_POINT ( 'NONE',  ( 23.14999999999999503, 21.06094381221970124, -233.8786389445302518 ) ) ;
#32925 = DIRECTION ( 'NONE',  ( 0.000000000000000000, 0.9126074666063771490, 0.4088369013363278848 ) ) ;
#32926 = CARTESIAN_POINT ( 'NONE',  ( 20.95378194480896639, 65.46508800846929432, -128.9580533363765369 ) ) ;
#32927 = CARTESIAN_POINT ( 'NONE',  ( 18.50000000000000711, 33.85801315034685643, -236.2828094960805174 ) ) ;
#32928 = CARTESIAN_POINT ( 'NONE',  ( -16.87331047859649757, 9.949999999999983302, -20.85000000000000142 ) ) ;
#32929 = CYLINDRICAL_SURFACE ( 'NONE', #114767, 0.5000000000000004441 ) ;
#32931 = LINE ( 'NONE', #54988, #170574 ) ;
#32930 = AXIS2_PLACEMENT_3D ( 'NONE', #77386, #235200, #76114 ) ;
#32933 = CARTESIAN_POINT ( 'NONE',  ( 22.14074124539698829, 10.53106080608756479, -227.1716106721344772 ) ) ;
#32932 = CIRCLE ( 'NONE', #45348, 0.1999999999999987899 ) ;
#32934 = CARTESIAN_POINT ( 'NONE',  ( 18.58725287972280071, 38.15563695641856157, -261.2056371150309246 ) ) ;
#32935 = ADVANCED_FACE ( 'NONE', ( #119681 ), #231594, .T. ) ;
#32936 = AXIS2_PLACEMENT_3D ( 'NONE', #58367, #76669, #80490 ) ;
#32937 = DIRECTION ( 'NONE',  ( 1.000000000000000000, 0.000000000000000000, 0.000000000000000000 ) ) ;
#32938 = ORIENTED_EDGE ( 'NONE', *, *, #134717, .F. ) ;
#32939 = VECTOR ( 'NONE', #99575, 1000.000000000000000 ) ;
#32941 = ORIENTED_EDGE ( 'NONE', *, *, #138707, .F. ) ;
#32940 = EDGE_LOOP ( 'NONE', ( #109812, #219955, #168064, #144695 ) ) ;
#32942 = ORIENTED_EDGE ( 'NONE', *, *, #92473, .F. ) ;
#32943 = DIRECTION ( 'NONE',  ( 1.000000000000000000, 0.000000000000000000, 0.000000000000000000 ) ) ;
#32944 = DIRECTION ( 'NONE',  ( -1.000000000000000000, 0.000000000000000000, 0.000000000000000000 ) ) ;
#32946 = DIRECTION ( 'NONE',  ( -3.265361837132813093E-16, 1.000000000000000000, 0.000000000000000000 ) ) ;
#32945 = CARTESIAN_POINT ( 'NONE',  ( -21.37071067811865532, 8.070710678129811910, -79.25000000000004263 ) ) ;
#32947 = EDGE_LOOP ( 'NONE', ( #118277, #236000, #159644, #30351 ) ) ;
#32948 = ORIENTED_EDGE ( 'NONE', *, *, #116767, .T. ) ;
#32949 = EDGE_CURVE ( 'NONE', #107789, #1569, #227473, .T. ) ;
#32950 = CARTESIAN_POINT ( 'NONE',  ( 18.42595409746875035, -9.499999812554021261, -40.49936235174737220 ) ) ;
#32951 = LINE ( 'NONE', #156742, #126407 ) ;
#32952 = EDGE_CURVE ( 'NONE', #230341, #93986, #218747, .T. ) ;
#32953 = DIRECTION ( 'NONE',  ( 0.000000000000000000, 1.000000000000000000, 6.982962677686266711E-15 ) ) ;
#32954 = VERTEX_POINT ( 'NONE', #102638 ) ;
#32955 = EDGE_LOOP ( 'NONE', ( #213981, #1304, #96230, #175713 ) ) ;
#32956 = VECTOR ( 'NONE', #209898, 1000.000000000000000 ) ;
#32957 = CIRCLE ( 'NONE', #66228, 14.30833333333333890 ) ;
#32958 = DIRECTION ( 'NONE',  ( 0.7071067811865463515, -0.7071067811865487940, 0.000000000000000000 ) ) ;
#32959 = CARTESIAN_POINT ( 'NONE',  ( -33.72168855820451938, 12.41403342719998903, -211.2428889513006425 ) ) ;
#32960 = ADVANCED_FACE ( 'NONE', ( #20586 ), #83062, .F. ) ;
#32961 = EDGE_CURVE ( 'NONE', #143803, #94061, #180001, .T. ) ;
#32962 = CARTESIAN_POINT ( 'NONE',  ( -18.58671080940899856, 78.17500251348390350, -231.4416493083392083 ) ) ;
#32964 = ORIENTED_EDGE ( 'NONE', *, *, #144379, .F. ) ;
#32963 = LINE ( 'NONE', #111175, #43856 ) ;
#32965 = TOROIDAL_SURFACE ( 'NONE', #245310, 11.90000000000000391, 0.1000000000000000056 ) ;
#32966 = LINE ( 'NONE', #188143, #148449 ) ;
#32967 = DIRECTION ( 'NONE',  ( 0.000000000000000000, -0.4856429311786307768, -0.8741572761215385956 ) ) ;
#32969 = EDGE_CURVE ( 'NONE', #211107, #158004, #178386, .T. ) ;
#32968 = CARTESIAN_POINT ( 'NONE',  ( -23.25000000000000000, 87.75000000001143974, -39.12310748452424747 ) ) ;
#32970 = DIRECTION ( 'NONE',  ( -1.000000000000000000, 0.000000000000000000, 0.000000000000000000 ) ) ;
#32971 = ORIENTED_EDGE ( 'NONE', *, *, #30668, .F. ) ;
#32972 = CARTESIAN_POINT ( 'NONE',  ( 12.68104795156995124, 66.60346600605790002, -85.11716770535107912 ) ) ;
#32973 = CARTESIAN_POINT ( 'NONE',  ( -23.25000000000000000, 14.06640494040441602, -210.3712993791105532 ) ) ;
#32974 = CARTESIAN_POINT ( 'NONE',  ( 22.39999999999999503, 76.10085836911075319, -114.7726746080137019 ) ) ;
#32976 = CARTESIAN_POINT ( 'NONE',  ( -23.25000000000000000, 1.910280373842930812, -54.36863214480106166 ) ) ;
#32975 = CARTESIAN_POINT ( 'NONE',  ( -18.59999999999999787, 64.35000000001234355, -163.0083017138704236 ) ) ;
#32977 = DIRECTION ( 'NONE',  ( 1.000000000000000000, 0.000000000000000000, 0.000000000000000000 ) ) ;
#32978 = DIRECTION ( 'NONE',  ( 1.000000000000000000, 0.000000000000000000, 0.000000000000000000 ) ) ;
#32979 = DIRECTION ( 'NONE',  ( 0.000000000000000000, 0.000000000000000000, -1.000000000000000000 ) ) ;
#32980 = AXIS2_PLACEMENT_3D ( 'NONE', #179229, #154543, #138749 ) ;
#32981 = CARTESIAN_POINT ( 'NONE',  ( 20.04142135623730070, 64.35000000001198828, -115.1731074845243796 ) ) ;
#32982 = DIRECTION ( 'NONE',  ( -0.000000000000000000, -0.000000000000000000, 1.000000000000000000 ) ) ;
#32983 = AXIS2_PLACEMENT_3D ( 'NONE', #108966, #188512, #89403 ) ;
#32984 = ORIENTED_EDGE ( 'NONE', *, *, #33638, .T. ) ;
#32985 = ADVANCED_FACE ( 'NONE', ( #158822 ), #101330, .F. ) ;
#32987 = EDGE_CURVE ( 'NONE', #245147, #158190, #23530, .T. ) ;
#32986 = AXIS2_PLACEMENT_3D ( 'NONE', #173224, #212315, #140115 ) ;
#32988 = ORIENTED_EDGE ( 'NONE', *, *, #55320, .F. ) ;
#32989 = ORIENTED_EDGE ( 'NONE', *, *, #68262, .T. ) ;
#32990 = DIRECTION ( 'NONE',  ( 0.000000000000000000, 0.000000000000000000, -1.000000000000000000 ) ) ;
#32991 = CARTESIAN_POINT ( 'NONE',  ( -20.85000000000000142, -1.835859311432481045, -78.60443916879853532 ) ) ;
#32992 = ORIENTED_EDGE ( 'NONE', *, *, #68707, .F. ) ;
#32993 = ADVANCED_FACE ( 'NONE', ( #81785 ), #240904, .F. ) ;
#32994 = DIRECTION ( 'NONE',  ( 1.000000000000000000, -1.186688945009009831E-16, -8.286604613020806758E-31 ) ) ;
#32995 = AXIS2_PLACEMENT_3D ( 'NONE', #34983, #91063, #250141 ) ;
#32996 = EDGE_LOOP ( 'NONE', ( #90338, #98333, #248315, #124029, #150007 ) ) ;
#32997 = ORIENTED_EDGE ( 'NONE', *, *, #32282, .F. ) ;
#32998 = EDGE_CURVE ( 'NONE', #164109, #120691, #139978, .T. ) ;
#32999 = CARTESIAN_POINT ( 'NONE',  ( 21.05000000000000071, -11.74999999998883560, -36.39999999999999858 ) ) ;
#33000 = EDGE_CURVE ( 'NONE', #148346, #102268, #235676, .T. ) ;
#33001 = ORIENTED_EDGE ( 'NONE', *, *, #173115, .F. ) ;
#33002 = LINE ( 'NONE', #9524, #121890 ) ;
#33003 = AXIS2_PLACEMENT_3D ( 'NONE', #231884, #71529, #187619 ) ;
#33004 = VECTOR ( 'NONE', #104082, 1000.000000000000000 ) ;
#33005 = CARTESIAN_POINT ( 'NONE',  ( 20.12500000000000000, 66.25000000001205080, -115.3731074845243683 ) ) ;
#33006 = CARTESIAN_POINT ( 'NONE',  ( 21.14999999999999858, 64.35000000001186038, -90.77310748452438816 ) ) ;
#33007 = COLOUR_RGB ( '', 0.09019608, 0.27058824, 0.51372549) ;
#33008 = EDGE_CURVE ( 'NONE', #144717, #72511, #152517, .T. ) ;
#33009 = CARTESIAN_POINT ( 'NONE',  ( -16.90138253750125941, 30.08429674386798069, -234.7416759015230241 ) ) ;
#33010 = CARTESIAN_POINT ( 'NONE',  ( -20.12071067811865888, 44.11897616243903286, -235.9958768108129448 ) ) ;
#33012 = ORIENTED_EDGE ( 'NONE', *, *, #115588, .F. ) ;
#33011 = CARTESIAN_POINT ( 'NONE',  ( -16.83558968593863270, 30.19548159561646372, -234.8012345828538514 ) ) ;
#33014 = LINE ( 'NONE', #112512, #108613 ) ;
#33013 = CARTESIAN_POINT ( 'NONE',  ( 20.94999999999999574, -11.48912529306490349, -36.60000000000000142 ) ) ;
#33015 = VECTOR ( 'NONE', #100525, 1000.000000000000000 ) ;
#33016 = CARTESIAN_POINT ( 'NONE',  ( -17.04295772865485148, 10.02489942525999567, -20.85000000000000142 ) ) ;
#33017 = ADVANCED_FACE ( 'NONE', ( #109077 ), #119165, .F. ) ;
#33018 = CARTESIAN_POINT ( 'NONE',  ( -21.14999999999994174, 67.85000000001119247, -3.123107484524795474 ) ) ;
#33019 = LINE ( 'NONE', #112515, #131416 ) ;
#33020 = DIRECTION ( 'NONE',  ( -0.000000000000000000, 1.000000000000000000, 0.000000000000000000 ) ) ;
#33021 = ORIENTED_EDGE ( 'NONE', *, *, #13202, .T. ) ;
#33022 = EDGE_CURVE ( 'NONE', #87151, #236886, #29586, .T. ) ;
#33023 = DIRECTION ( 'NONE',  ( 1.000000000000000000, 0.000000000000000000, 0.000000000000000000 ) ) ;
#33024 = FACE_OUTER_BOUND ( 'NONE', #183580, .T. ) ;
#33026 = ORIENTED_EDGE ( 'NONE', *, *, #6350, .T. ) ;
#33025 = VECTOR ( 'NONE', #203302, 1000.000000000000114 ) ;
#33027 = CARTESIAN_POINT ( 'NONE',  ( 23.14999999999998437, 0.000000000000000000, 0.000000000000000000 ) ) ;
#33028 = DIRECTION ( 'NONE',  ( 1.000000000000000000, 0.000000000000000000, 0.000000000000000000 ) ) ;
#33029 = DIRECTION ( 'NONE',  ( 0.000000000000000000, 1.000000000000000000, 0.000000000000000000 ) ) ;
#33030 = EDGE_CURVE ( 'NONE', #34147, #45256, #106671, .T. ) ;
#33031 = VERTEX_POINT ( 'NONE', #7407 ) ;
#33032 = ORIENTED_EDGE ( 'NONE', *, *, #228377, .T. ) ;
#33033 = AXIS2_PLACEMENT_3D ( 'NONE', #93585, #12790, #235648 ) ;
#33035 = ADVANCED_FACE ( 'NONE', ( #30868 ), #110364, .F. ) ;
#33034 = DIRECTION ( 'NONE',  ( 0.000000000000000000, 1.000000000000000000, 1.626303258728238113E-15 ) ) ;
#33036 = DIRECTION ( 'NONE',  ( 0.000000000000000000, 0.2128009952263604232, -0.9770955615653315052 ) ) ;
#33037 = DIRECTION ( 'NONE',  ( 0.000000000000000000, 0.2617529984165031243, 0.9651348961777157509 ) ) ;
#33038 = CARTESIAN_POINT ( 'NONE',  ( 18.59999999999998366, 67.85909929089923764, -227.8797997985275856 ) ) ;
#33039 = AXIS2_PLACEMENT_3D ( 'NONE', #204274, #41390, #240859 ) ;
#33041 = DIRECTION ( 'NONE',  ( 0.000000000000000000, 0.9126074666064696306, 0.4088369013361213278 ) ) ;
#33040 = CARTESIAN_POINT ( 'NONE',  ( -18.50000000000000000, 6.846123162363745074, -137.7377262668498759 ) ) ;
#33042 = DIRECTION ( 'NONE',  ( -1.000000000000000000, 0.000000000000000000, 0.000000000000000000 ) ) ;
#33043 = SPHERICAL_SURFACE ( 'NONE', #227249, 0.1000000000000000056 ) ;
#33044 = CARTESIAN_POINT ( 'NONE',  ( 21.05000000000000071, -11.64999999998883595, -131.1000000000000227 ) ) ;
#33045 = EDGE_LOOP ( 'NONE', ( #39842, #12903, #251442 ) ) ;
#33046 = DIRECTION ( 'NONE',  ( 1.000000000000000000, 0.000000000000000000, 0.000000000000000000 ) ) ;
#33047 = CIRCLE ( 'NONE', #212072, 0.09999999999999939493 ) ;
#33049 = ORIENTED_EDGE ( 'NONE', *, *, #109380, .F. ) ;
#33048 = CARTESIAN_POINT ( 'NONE',  ( -22.50000000000000000, 7.128833340093095217, -233.7327013124392749 ) ) ;
#33050 = LINE ( 'NONE', #248198, #39432 ) ;
#33051 = CARTESIAN_POINT ( 'NONE',  ( -20.64999999999999858, 76.00000000001126921, -203.5231074845248997 ) ) ;
#33053 = DIRECTION ( 'NONE',  ( 1.000000000000000000, 0.000000000000000000, 0.000000000000000000 ) ) ;
#33052 = LINE ( 'NONE', #49993, #449 ) ;
#33054 = ADVANCED_FACE ( 'NONE', ( #144331 ), #146907, .T. ) ;
#33055 = DIRECTION ( 'NONE',  ( 0.000000000000000000, 1.000000000000000000, 6.982962677686266711E-15 ) ) ;
#33057 = ORIENTED_EDGE ( 'NONE', *, *, #192819, .F. ) ;
#33056 = DIRECTION ( 'NONE',  ( 0.000000000000000000, 0.2128009952263601456, -0.9770955615653316162 ) ) ;
#33058 = CARTESIAN_POINT ( 'NONE',  ( -20.64999999999999858, 4.350000000011156054, -179.8499999999999943 ) ) ;
#33059 = CARTESIAN_POINT ( 'NONE',  ( -16.92989507731676113, 51.40668072027212787, -232.0415240324163335 ) ) ;
#33060 = PLANE ( 'NONE',  #146986 ) ;
#33061 = DIRECTION ( 'NONE',  ( -0.000000000000000000, 0.1298341882519735979, 0.9915357197604890427 ) ) ;
#33062 = EDGE_LOOP ( 'NONE', ( #77755, #120401, #161246, #254096 ) ) ;
#33063 = CARTESIAN_POINT ( 'NONE',  ( 18.39999999999999858, -7.792936614629562442, -209.8606550935952271 ) ) ;
#33065 = ORIENTED_EDGE ( 'NONE', *, *, #163812, .T. ) ;
#33064 = CIRCLE ( 'NONE', #74751, 0.09999999999999939493 ) ;
#33066 = CIRCLE ( 'NONE', #20555, 11.79999999999999361 ) ;
#33067 = DIRECTION ( 'NONE',  ( 0.000000000000000000, 0.4999999999999956701, -0.8660254037844411501 ) ) ;
#33068 = ORIENTED_EDGE ( 'NONE', *, *, #180184, .F. ) ;
#33069 = B_SPLINE_CURVE_WITH_KNOTS ( 'NONE', 3,
 ( #247478, #8873, #54410, #233077, #88379, #90968, #250049, #170571, #68863, #148386, #150953, #51822, #227920, #230491, #131378, #210922, #32315, #77809, #216041 ),
 .UNSPECIFIED., .F., .F.,
 ( 4, 3, 3, 3, 3, 3, 4 ),
 ( 0.000000000000000000, 1.655171619025768090E-05, 2.773500582848307641E-05, 5.941817267378768900E-05, 0.0001114174635873506033, 0.0001914169455916434233, 0.0002627181070750764539 ),
 .UNSPECIFIED. ) ;
#33070 = ADVANCED_FACE ( 'NONE', ( #11278 ), #19398, .T. ) ;
#33071 = CARTESIAN_POINT ( 'NONE',  ( 20.94999999999999929, 6.550000000011156231, -110.5170271704400591 ) ) ;
#33072 = VECTOR ( 'NONE', #95100, 1000.000000000000000 ) ;
#33073 = ORIENTED_EDGE ( 'NONE', *, *, #141803, .T. ) ;
#33074 = CARTESIAN_POINT ( 'NONE',  ( 20.00000000000000355, 1.249999999999999334, 16.60000000000000142 ) ) ;
#33075 = FACE_OUTER_BOUND ( 'NONE', #222777, .T. ) ;
#33076 = DIRECTION ( 'NONE',  ( 0.000000000000000000, -0.1332476588733448597, 0.9910827722268067408 ) ) ;
#33077 = ORIENTED_EDGE ( 'NONE', *, *, #2790, .T. ) ;
#33078 = CARTESIAN_POINT ( 'NONE',  ( -16.87683809663752399, 9.849999999999964118, -13.40236401819648115 ) ) ;
#33079 = CARTESIAN_POINT ( 'NONE',  ( 21.05000000000000071, -11.48912529306489994, -131.1000000000000227 ) ) ;
#33080 = DIRECTION ( 'NONE',  ( -1.000000000000000000, 0.000000000000000000, 0.000000000000000000 ) ) ;
#33082 = AXIS2_PLACEMENT_3D ( 'NONE', #235739, #57083, #146892 ) ;
#33081 = DIRECTION ( 'NONE',  ( 0.000000000000000000, -7.147358527629766941E-15, 1.000000000000000000 ) ) ;
#33083 = DIRECTION ( 'NONE',  ( 2.952720810173289112E-16, -1.000000000000000000, 0.000000000000000000 ) ) ;
#33084 = EDGE_LOOP ( 'NONE', ( #90185, #187812, #224196, #19368 ) ) ;
#33085 = CARTESIAN_POINT ( 'NONE',  ( -21.05000000000000071, 64.35000000001238618, -169.9231074845244507 ) ) ;
#33086 = VERTEX_POINT ( 'NONE', #149523 ) ;
#33088 = VERTEX_POINT ( 'NONE', #226440 ) ;
#33087 = CARTESIAN_POINT ( 'NONE',  ( 21.09706851349342216, 67.22415748653845924, -90.78754126812472691 ) ) ;
#33089 = ORIENTED_EDGE ( 'NONE', *, *, #185154, .F. ) ;
#33090 = CARTESIAN_POINT ( 'NONE',  ( 22.47071067811864964, 0.09909245471376176839, -59.27992525550201464 ) ) ;
#33091 = CARTESIAN_POINT ( 'NONE',  ( -16.88219499860498374, 66.04979357458500999, -190.8737977944171291 ) ) ;
#33092 = CARTESIAN_POINT ( 'NONE',  ( 23.24999999999999289, 11.75000000001116263, -88.75000000000004263 ) ) ;
#33093 = DIRECTION ( 'NONE',  ( 1.000000000000000000, -0.000000000000000000, -0.000000000000000000 ) ) ;
#33094 = ORIENTED_EDGE ( 'NONE', *, *, #216630, .F. ) ;
#33095 = CARTESIAN_POINT ( 'NONE',  ( -16.87304349924914604, 66.03825492205433534, -48.63404080947914565 ) ) ;
#33096 = CARTESIAN_POINT ( 'NONE',  ( 18.79999999999999716, 11.61130914238355771, 22.00000000000000355 ) ) ;
#33097 = ORIENTED_EDGE ( 'NONE', *, *, #54504, .T. ) ;
#33099 = ORIENTED_EDGE ( 'NONE', *, *, #218258, .F. ) ;
#33098 = CARTESIAN_POINT ( 'NONE',  ( -16.89318236219975944, 66.04846474213687202, -115.6679778524185309 ) ) ;
#33100 = EDGE_CURVE ( 'NONE', #237128, #160394, #130621, .T. ) ;
#33101 = DIRECTION ( 'NONE',  ( 1.000000000000000000, -0.000000000000000000, -0.000000000000000000 ) ) ;
#33102 = LINE ( 'NONE', #89164, #252146 ) ;
#33103 = AXIS2_PLACEMENT_3D ( 'NONE', #124747, #107737, #225094 ) ;
#33104 = AXIS2_PLACEMENT_3D ( 'NONE', #69162, #5278, #44454 ) ;
#33105 = CIRCLE ( 'NONE', #128734, 0.1000000000000027117 ) ;
#33106 = CIRCLE ( 'NONE', #178837, 0.2000000000000057288 ) ;
#33107 = EDGE_LOOP ( 'NONE', ( #140263, #184304, #30359, #170638 ) ) ;
#33108 = EDGE_LOOP ( 'NONE', ( #36034, #133092, #213330, #47975 ) ) ;
#33109 = CARTESIAN_POINT ( 'NONE',  ( 18.59999999999999076, 65.50857864377520912, -178.6731074845244223 ) ) ;
#33110 = VECTOR ( 'NONE', #58903, 1000.000000000000000 ) ;
#33111 = FACE_OUTER_BOUND ( 'NONE', #133507, .T. ) ;
#33112 = ORIENTED_EDGE ( 'NONE', *, *, #84347, .F. ) ;
#33113 = CARTESIAN_POINT ( 'NONE',  ( 15.74999999999999645, 26.54497872210689735, -232.9592037335782209 ) ) ;
#33114 = EDGE_CURVE ( 'NONE', #6554, #131901, #102748, .T. ) ;
#33115 = CARTESIAN_POINT ( 'NONE',  ( -18.59999999999999787, 11.66622623553636018, -211.0987209794895421 ) ) ;
#33116 = EDGE_CURVE ( 'NONE', #21197, #147150, #225158, .T. ) ;
#33117 = LINE ( 'NONE', #153065, #205210 ) ;
#33118 = CIRCLE ( 'NONE', #45542, 0.1000000000000054040 ) ;
#33119 = AXIS2_PLACEMENT_3D ( 'NONE', #2471, #119898, #136858 ) ;
#33120 = AXIS2_PLACEMENT_3D ( 'NONE', #196308, #17665, #179346 ) ;
#33121 = ADVANCED_FACE ( 'NONE', ( #234161 ), #253717, .T. ) ;
#33122 = VECTOR ( 'NONE', #232425, 1000.000000000000227 ) ;
#33123 = ORIENTED_EDGE ( 'NONE', *, *, #208992, .F. ) ;
#33124 = EDGE_CURVE ( 'NONE', #160229, #254598, #169465, .T. ) ;
#33125 = ORIENTED_EDGE ( 'NONE', *, *, #157365, .F. ) ;
#33126 = EDGE_CURVE ( 'NONE', #39669, #48866, #32146, .T. ) ;
#33127 = CARTESIAN_POINT ( 'NONE',  ( -20.99142135623731065, 11.60000000001115161, -60.07179676972450721 ) ) ;
#33128 = DIRECTION ( 'NONE',  ( -0.000000000000000000, -0.1350103645451807555, -0.9908441862701610203 ) ) ;
#33130 = ORIENTED_EDGE ( 'NONE', *, *, #54571, .T. ) ;
#33129 = CARTESIAN_POINT ( 'NONE',  ( 13.22261339317536866, 24.96400212477830749, -232.5813472152648558 ) ) ;
#33131 = DIRECTION ( 'NONE',  ( 0.000000000000000000, 6.982962677686266711E-15, -1.000000000000000000 ) ) ;
#33132 = CARTESIAN_POINT ( 'NONE',  ( 21.05563370358598263, 65.27576964416506655, -57.34001666856132573 ) ) ;
#33133 = EDGE_CURVE ( 'NONE', #28931, #214564, #40271, .T. ) ;
#33134 = DIRECTION ( 'NONE',  ( -1.000000000000000000, 0.000000000000000000, 0.000000000000000000 ) ) ;
#33135 = LINE ( 'NONE', #16118, #58775 ) ;
#33136 = CARTESIAN_POINT ( 'NONE',  ( 21.07954763557419042, 6.329290990048669130, -33.43412408138156167 ) ) ;
#33137 = CARTESIAN_POINT ( 'NONE',  ( -21.05000000000000071, 1.162701749949165642, -41.60000000000000142 ) ) ;
#33138 = LINE ( 'NONE', #130902, #28090 ) ;
#33140 = ORIENTED_EDGE ( 'NONE', *, *, #40598, .T. ) ;
#33139 = DIRECTION ( 'NONE',  ( 2.952720810173289112E-16, 1.000000000000000000, -6.088138035986627436E-46 ) ) ;
#33141 = EDGE_CURVE ( 'NONE', #229612, #67123, #215867, .T. ) ;
#33142 = AXIS2_PLACEMENT_3D ( 'NONE', #164231, #28614, #123816 ) ;
#33143 = CARTESIAN_POINT ( 'NONE',  ( -20.54999999999999716, 85.00000000001251976, -179.9170766071767389 ) ) ;
#33144 = DIRECTION ( 'NONE',  ( 0.000000000000000000, 1.000000000000000000, 7.116814260417668513E-15 ) ) ;
#33145 = CARTESIAN_POINT ( 'NONE',  ( -18.48179518609137517, 85.51832530050651826, -62.63340190776217753 ) ) ;
#33146 = LINE ( 'NONE', #253420, #197132 ) ;
#33147 = ORIENTED_EDGE ( 'NONE', *, *, #78505, .T. ) ;
#33148 = ADVANCED_FACE ( 'NONE', ( #136320 ), #173667, .T. ) ;
#33149 = FACE_OUTER_BOUND ( 'NONE', #143166, .T. ) ;
#33150 = VERTEX_POINT ( 'NONE', #92088 ) ;
#33151 = AXIS2_PLACEMENT_3D ( 'NONE', #147511, #227040, #207505 ) ;
#33152 = CARTESIAN_POINT ( 'NONE',  ( -12.25000000000000178, 26.30888228346803714, -233.3999513616626587 ) ) ;
#33153 = CIRCLE ( 'NONE', #4077, 4.150000000000001243 ) ;
#33154 = CARTESIAN_POINT ( 'NONE',  ( -22.47007471830798409, 59.77974727959313839, -233.8342073434303643 ) ) ;
#33155 = ADVANCED_FACE ( 'NONE', ( #90793 ), #76362, .T. ) ;
#33156 = ORIENTED_EDGE ( 'NONE', *, *, #233549, .T. ) ;
#33157 = CARTESIAN_POINT ( 'NONE',  ( 20.94999999999999929, 34.89593390941166007, -248.6067769466879156 ) ) ;
#33158 = EDGE_LOOP ( 'NONE', ( #179459, #255449, #231274, #3366, #193194 ) ) ;
#33159 = CARTESIAN_POINT ( 'NONE',  ( -20.94999999999999929, 1.162701749949165642, -175.5999999999999659 ) ) ;
#33161 = ORIENTED_EDGE ( 'NONE', *, *, #44961, .F. ) ;
#33160 = CARTESIAN_POINT ( 'NONE',  ( 22.47071067811864964, 75.90090754530959316, -144.2431822290223522 ) ) ;
#33162 = AXIS2_PLACEMENT_3D ( 'NONE', #225658, #9207, #146145 ) ;
#33163 = AXIS2_PLACEMENT_3D ( 'NONE', #149465, #32087, #111603 ) ;
#33164 = CARTESIAN_POINT ( 'NONE',  ( -16.87683809663752399, 54.76195096157850628, -56.87310748452446774 ) ) ;
#33165 = ORIENTED_EDGE ( 'NONE', *, *, #157157, .F. ) ;
#33166 = DIRECTION ( 'NONE',  ( 1.000000000000000000, -0.000000000000000000, 0.000000000000000000 ) ) ;
#33167 = ORIENTED_EDGE ( 'NONE', *, *, #69806, .F. ) ;
#33169 = ORIENTED_EDGE ( 'NONE', *, *, #19434, .T. ) ;
#33168 = VERTEX_POINT ( 'NONE', #252433 ) ;
#33170 = CYLINDRICAL_SURFACE ( 'NONE', #107097, 0.5000000000000004441 ) ;
#33172 = ORIENTED_EDGE ( 'NONE', *, *, #17032, .T. ) ;
#33171 = CARTESIAN_POINT ( 'NONE',  ( 15.74999999999999645, 9.350000000011139178, -50.25000000000000000 ) ) ;
#33173 = EDGE_CURVE ( 'NONE', #162955, #210786, #115245, .T. ) ;
#33174 = DIRECTION ( 'NONE',  ( 0.000000000000000000, -7.034366652768095332E-15, 1.000000000000000000 ) ) ;
#33175 = ORIENTED_EDGE ( 'NONE', *, *, #92358, .F. ) ;
#33176 = EDGE_CURVE ( 'NONE', #243985, #250992, #232914, .T. ) ;
#33177 = VECTOR ( 'NONE', #236579, 1000.000000000000000 ) ;
#33178 = CIRCLE ( 'NONE', #249625, 11.75000000000000000 ) ;
#33179 = VECTOR ( 'NONE', #238463, 1000.000000000000000 ) ;
#33180 = ORIENTED_EDGE ( 'NONE', *, *, #147342, .F. ) ;
#33182 = AXIS2_PLACEMENT_3D ( 'NONE', #116928, #196454, #37408 ) ;
#33181 = DIRECTION ( 'NONE',  ( 0.000000000000000000, 0.2128009952263601456, -0.9770955615653316162 ) ) ;
#33183 = DIRECTION ( 'NONE',  ( -1.000000000000000000, 0.000000000000000000, -0.000000000000000000 ) ) ;
#33184 = ADVANCED_FACE ( 'NONE', ( #72549 ), #230311, .F. ) ;
#33185 = CARTESIAN_POINT ( 'NONE',  ( -18.59999999999999787, 11.65000000001115232, -155.7499999999999716 ) ) ;
#33186 = ORIENTED_EDGE ( 'NONE', *, *, #169118, .F. ) ;
#33187 = CARTESIAN_POINT ( 'NONE',  ( 19.97071067811864609, 16.71907901384503603, -222.6889362516795927 ) ) ;
#33188 = CARTESIAN_POINT ( 'NONE',  ( -12.47155713865592119, 66.62433047358680938, -187.6553174751384745 ) ) ;
#33189 = DIRECTION ( 'NONE',  ( -1.000000000000000000, -0.000000000000000000, -0.000000000000000000 ) ) ;
#33191 = ORIENTED_EDGE ( 'NONE', *, *, #123735, .F. ) ;
#33190 = EDGE_CURVE ( 'NONE', #68442, #188971, #36161, .T. ) ;
#33193 = EDGE_CURVE ( 'NONE', #47449, #174034, #165141, .T. ) ;
#33192 = CARTESIAN_POINT ( 'NONE',  ( -20.00857864376270001, 9.150000000011157653, -79.35000000000005116 ) ) ;
#33194 = PLANE ( 'NONE',  #36207 ) ;
#33195 = SURFACE_SIDE_STYLE ('',( #233917 ) ) ;
#33196 = ORIENTED_EDGE ( 'NONE', *, *, #107991, .T. ) ;
#33197 = LINE ( 'NONE', #90544, #134611 ) ;
#33198 = ORIENTED_EDGE ( 'NONE', *, *, #178275, .F. ) ;
#33200 = AXIS2_PLACEMENT_3D ( 'NONE', #164396, #65285, #30043 ) ;
#33199 = CARTESIAN_POINT ( 'NONE',  ( 20.85000000000000142, 1.115600667400684642E-11, -100.5000000000000426 ) ) ;
#33201 = VERTEX_POINT ( 'NONE', #56781 ) ;
#33202 = CARTESIAN_POINT ( 'NONE',  ( -23.15000000000000213, 76.00000000001170974, -69.52310748452431710 ) ) ;
#33203 = DIRECTION ( 'NONE',  ( 1.000000000000000000, 0.000000000000000000, 0.000000000000000000 ) ) ;
#33204 = ADVANCED_FACE ( 'NONE', ( #162355 ), #176785, .F. ) ;
#33205 = VERTEX_POINT ( 'NONE', #217150 ) ;
#33206 = ORIENTED_EDGE ( 'NONE', *, *, #204395, .F. ) ;
#33207 = PLANE ( 'NONE',  #228233 ) ;
#33208 = CARTESIAN_POINT ( 'NONE',  ( -20.54999999999999716, -11.74999999998884448, -88.15000000000004832 ) ) ;
#33209 = EDGE_LOOP ( 'NONE', ( #133250, #3975, #176284, #176239 ) ) ;
#33210 = ORIENTED_EDGE ( 'NONE', *, *, #222456, .F. ) ;
#33211 = CYLINDRICAL_SURFACE ( 'NONE', #31361, 0.09999999999999939493 ) ;
#33212 = CARTESIAN_POINT ( 'NONE',  ( -18.50211644919735576, 65.69792220476300315, -64.03355541284614105 ) ) ;
#33213 = CIRCLE ( 'NONE', #49912, 0.09999999999999939493 ) ;
#33214 = ORIENTED_EDGE ( 'NONE', *, *, #179433, .F. ) ;
#33215 = AXIS2_PLACEMENT_3D ( 'NONE', #55982, #135526, #215080 ) ;
#33216 = ORIENTED_EDGE ( 'NONE', *, *, #248310, .F. ) ;
#33217 = VECTOR ( 'NONE', #79735, 1000.000000000000000 ) ;
#33218 = DIRECTION ( 'NONE',  ( -0.000000000000000000, 0.000000000000000000, -1.000000000000000000 ) ) ;
#33219 = DIRECTION ( 'NONE',  ( -2.915501640297152804E-16, -1.000000000000000000, -6.997203936713167125E-15 ) ) ;
#33220 = ADVANCED_FACE ( 'NONE', ( #137614 ), #221010, .F. ) ;
#33221 = EDGE_CURVE ( 'NONE', #6867, #150875, #123211, .T. ) ;
#33222 = CARTESIAN_POINT ( 'NONE',  ( -23.15000000000000213, 7.128833340093095217, -233.7327013124392749 ) ) ;
#33224 = VERTEX_POINT ( 'NONE', #222275 ) ;
#33223 = CARTESIAN_POINT ( 'NONE',  ( -23.25000000000000000, 1.115600667400684642E-11, -134.0000000000000284 ) ) ;
#33225 = PLANE ( 'NONE',  #57615 ) ;
#33226 = CIRCLE ( 'NONE', #12362, 11.70000000000000284 ) ;
#33227 = FACE_BOUND ( 'NONE', #250776, .T. ) ;
#33228 = FACE_OUTER_BOUND ( 'NONE', #9073, .T. ) ;
#33229 = AXIS2_PLACEMENT_3D ( 'NONE', #49209, #85731, #166632 ) ;
#33230 = CARTESIAN_POINT ( 'NONE',  ( -18.59999999999999787, 43.08613539620618837, -254.3146655184800409 ) ) ;
#33231 = CARTESIAN_POINT ( 'NONE',  ( -18.59999999999999787, 11.75000000001115197, -88.35000000000003695 ) ) ;
#33232 = CARTESIAN_POINT ( 'NONE',  ( -17.78043020864320667, 65.14640788800591054, -59.18615665024461947 ) ) ;
#33233 = EDGE_CURVE ( 'NONE', #60618, #161835, #123447, .T. ) ;
#33234 = DIRECTION ( 'NONE',  ( 0.000000000000000000, 0.000000000000000000, 1.000000000000000000 ) ) ;
#33235 = CARTESIAN_POINT ( 'NONE',  ( -21.04999999999999716, 75.90156250001244587, -176.3223383946112222 ) ) ;
#33236 = AXIS2_PLACEMENT_3D ( 'NONE', #233967, #239115, #60455 ) ;
#33237 = ORIENTED_EDGE ( 'NONE', *, *, #208854, .F. ) ;
#33238 = ORIENTED_EDGE ( 'NONE', *, *, #230464, .F. ) ;
#33239 = DIRECTION ( 'NONE',  ( 0.000000000000000000, 0.4721928772777346239, 0.8814952561688430555 ) ) ;
#33240 = DIRECTION ( 'NONE',  ( 1.000000000000000000, 0.000000000000000000, 0.000000000000000000 ) ) ;
#33241 = ORIENTED_EDGE ( 'NONE', *, *, #171438, .F. ) ;
#33243 = DIRECTION ( 'NONE',  ( 1.186688945009009584E-16, -0.4721928772777346239, -0.8814952561688430555 ) ) ;
#33242 = TOROIDAL_SURFACE ( 'NONE', #25051, 0.6000000000000015321, 0.1000000000000000056 ) ;
#33244 = AXIS2_PLACEMENT_3D ( 'NONE', #131879, #32823, #229702 ) ;
#33245 = EDGE_CURVE ( 'NONE', #137276, #116061, #200261, .T. ) ;
#33246 = CARTESIAN_POINT ( 'NONE',  ( -5.899999999999938183, 64.65000000001120384, -22.12310748452479103 ) ) ;
#33247 = ORIENTED_EDGE ( 'NONE', *, *, #8594, .F. ) ;
#33248 = ORIENTED_EDGE ( 'NONE', *, *, #21165, .T. ) ;
#33249 = DIRECTION ( 'NONE',  ( 1.000000000000000000, 0.000000000000000000, 0.000000000000000000 ) ) ;
#33250 = DIRECTION ( 'NONE',  ( 0.000000000000000000, 0.9229812358756199764, -0.3848449534832346086 ) ) ;
#33251 = ORIENTED_EDGE ( 'NONE', *, *, #179841, .F. ) ;
#33252 = EDGE_CURVE ( 'NONE', #257328, #111659, #11009, .T. ) ;
#33253 = CARTESIAN_POINT ( 'NONE',  ( 21.07928932188134397, 0.09889514566555242248, -94.17148334360672379 ) ) ;
#33255 = ORIENTED_EDGE ( 'NONE', *, *, #238373, .F. ) ;
#33254 = CARTESIAN_POINT ( 'NONE',  ( 17.74533788810829904, 10.81849979148195118, -90.18637732505249005 ) ) ;
#33256 = DIRECTION ( 'NONE',  ( -0.000000000000000000, 0.1335171055202901413, -0.9910465087640860649 ) ) ;
#33258 = ORIENTED_EDGE ( 'NONE', *, *, #223923, .T. ) ;
#33257 = CARTESIAN_POINT ( 'NONE',  ( -18.59999999999999787, 43.18640298906419162, -245.2812653309023574 ) ) ;
#33260 = EDGE_CURVE ( 'NONE', #155898, #10002, #17676, .T. ) ;
#33259 = DIRECTION ( 'NONE',  ( 1.073024830501117725E-15, -0.000000000000000000, -1.000000000000000000 ) ) ;
#33261 = DIRECTION ( 'NONE',  ( -0.7071067811865388020, 0.7071067811865561215, 0.000000000000000000 ) ) ;
#33262 = DIRECTION ( 'NONE',  ( -1.000000000000000000, 0.000000000000000000, 0.000000000000000000 ) ) ;
#33263 = CARTESIAN_POINT ( 'NONE',  ( 20.95000000000005258, 87.75000000001119815, -4.623107484524796362 ) ) ;
#33264 = CIRCLE ( 'NONE', #120552, 0.09999999999999971412 ) ;
#33267 = DIRECTION ( 'NONE',  ( -1.000000000000000000, 0.000000000000000000, 0.000000000000000000 ) ) ;
#33266 = AXIS2_PLACEMENT_3D ( 'NONE', #74946, #256059, #154492 ) ;
#33265 = CARTESIAN_POINT ( 'NONE',  ( -21.07928932188134041, 69.67148334361864670, -103.1220026301787414 ) ) ;
#33269 = EDGE_CURVE ( 'NONE', #200852, #101749, #177644, .T. ) ;
#33268 = LINE ( 'NONE', #214421, #241126 ) ;
#33270 = AXIS2_PLACEMENT_3D ( 'NONE', #256163, #20201, #42322 ) ;
#33271 = AXIS2_PLACEMENT_3D ( 'NONE', #172156, #249100, #93850 ) ;
#33272 = FACE_OUTER_BOUND ( 'NONE', #62016, .T. ) ;
#33273 = CARTESIAN_POINT ( 'NONE',  ( -18.46154800491006043, 85.48020627425442797, -163.3656566461428383 ) ) ;
#33274 = CARTESIAN_POINT ( 'NONE',  ( 21.07928932188134397, 1.596973512267586326, -230.6572452218016167 ) ) ;
#33275 = CARTESIAN_POINT ( 'NONE',  ( -16.87683809663752399, 23.65833333333332433, -16.75000000000000000 ) ) ;
#33276 = EDGE_LOOP ( 'NONE', ( #239988, #61031, #154126, #55367 ) ) ;
#33277 = ADVANCED_FACE ( 'NONE', ( #80193 ), #110972, .T. ) ;
#33278 = DIRECTION ( 'NONE',  ( 2.952720810173289112E-16, -1.000000000000000000, -0.000000000000000000 ) ) ;
#33279 = AXIS2_PLACEMENT_3D ( 'NONE', #217678, #15691, #14404 ) ;
#33281 = EDGE_CURVE ( 'NONE', #81327, #188797, #65176, .T. ) ;
#33280 = ADVANCED_FACE ( 'NONE', ( #43679 ), #121936, .F. ) ;
#33282 = ORIENTED_EDGE ( 'NONE', *, *, #204337, .F. ) ;
#33283 = DIRECTION ( 'NONE',  ( 0.000000000000000000, 0.9910827722268049644, -0.1332476588733589318 ) ) ;
#33284 = ORIENTED_EDGE ( 'NONE', *, *, #130906, .T. ) ;
#33285 = DIRECTION ( 'NONE',  ( 1.000000000000000000, 0.000000000000000000, 0.000000000000000000 ) ) ;
#33286 = DIRECTION ( 'NONE',  ( -0.7071067811865474617, 0.7071067811865474617, 4.937700262164531476E-15 ) ) ;
#33287 = AXIS2_PLACEMENT_3D ( 'NONE', #41331, #219938, #96124 ) ;
#33288 = ORIENTED_EDGE ( 'NONE', *, *, #6833, .T. ) ;
#33289 = VECTOR ( 'NONE', #24793, 1000.000000000000000 ) ;
#33290 = CARTESIAN_POINT ( 'NONE',  ( -21.05000000000000071, 30.91400355739106942, -252.1479406582309366 ) ) ;
#33291 = VERTEX_POINT ( 'NONE', #161066 ) ;
#33293 = EDGE_CURVE ( 'NONE', #7989, #14516, #61077, .T. ) ;
#33292 = VECTOR ( 'NONE', #71762, 1000.000000000000000 ) ;
#33294 = ADVANCED_FACE ( 'NONE', ( #98464 ), #44351, .T. ) ;
#33295 = VERTEX_POINT ( 'NONE', #77637 ) ;
#33296 = DIRECTION ( 'NONE',  ( -0.000000000000000000, -1.000000000000000000, -5.421010862427649374E-16 ) ) ;
#33297 = CARTESIAN_POINT ( 'NONE',  ( -23.25000000000000000, 1.115600667400684642E-11, -167.5000000000000284 ) ) ;
#33298 = DIRECTION ( 'NONE',  ( 1.000000000000000000, 0.000000000000000000, -0.000000000000000000 ) ) ;
#33299 = DIRECTION ( 'NONE',  ( 1.000000000000000000, 0.000000000000000000, 0.000000000000000000 ) ) ;
#33300 = CARTESIAN_POINT ( 'NONE',  ( 20.85000000000000142, 76.00000000001142553, -36.02310748452432421 ) ) ;
#33301 = ADVANCED_FACE ( 'NONE', ( #20271 ), #157232, .F. ) ;
#33303 = PRESENTATION_STYLE_ASSIGNMENT (( #238850 ) ) ;
#33302 = CARTESIAN_POINT ( 'NONE',  ( -18.69999999999999929, 1.410778198689828900, -7.973296578895943121 ) ) ;
#33304 = CARTESIAN_POINT ( 'NONE',  ( -15.06774609480955895, 9.417651958852161442, -82.35878739244051872 ) ) ;
#33306 = ORIENTED_EDGE ( 'NONE', *, *, #101379, .F. ) ;
#33305 = CARTESIAN_POINT ( 'NONE',  ( -20.85882249326303040, 10.33248238083634796, -139.5948465439131780 ) ) ;
#33308 = DIRECTION ( 'NONE',  ( -1.000000000000000000, 0.000000000000000000, -0.000000000000000000 ) ) ;
#33307 = CARTESIAN_POINT ( 'NONE',  ( 22.39999999999999503, 76.10085836911093793, -148.2726746080136877 ) ) ;
#33309 = FACE_OUTER_BOUND ( 'NONE', #17998, .T. ) ;
#33310 = VERTEX_POINT ( 'NONE', #99766 ) ;
#33311 = CARTESIAN_POINT ( 'NONE',  ( -18.45037301276657971, -9.490200447530781958, -174.5126741364145175 ) ) ;
#33312 = DIRECTION ( 'NONE',  ( 0.000000000000000000, 0.000000000000000000, -1.000000000000000000 ) ) ;
#33313 = DIRECTION ( 'NONE',  ( -0.000000000000000000, -0.7049548389605067023, 0.7092521942342977503 ) ) ;
#33314 = ORIENTED_EDGE ( 'NONE', *, *, #155967, .F. ) ;
#33315 = EDGE_CURVE ( 'NONE', #2973, #9452, #206830, .T. ) ;
#33316 = CARTESIAN_POINT ( 'NONE',  ( -16.79139129368507355, 60.94953642464052734, -221.0235123146207172 ) ) ;
#33317 = ADVANCED_FACE ( 'NONE', ( #48803 ), #24133, .T. ) ;
#33318 = AXIS2_PLACEMENT_3D ( 'NONE', #43955, #246013, #162632 ) ;
#33319 = CARTESIAN_POINT ( 'NONE',  ( -21.65000000000000213, 68.29142135624930177, -115.2731074845243455 ) ) ;
#33320 = CARTESIAN_POINT ( 'NONE',  ( -18.44362607810620602, 78.23832416459919159, -231.5274147598107959 ) ) ;
#33321 = ORIENTED_EDGE ( 'NONE', *, *, #137461, .T. ) ;
#33322 = ORIENTED_EDGE ( 'NONE', *, *, #57069, .T. ) ;
#33323 = CARTESIAN_POINT ( 'NONE',  ( 22.45380639572771742, 64.15556337341597271, -247.1958792975366066 ) ) ;
#33325 = CARTESIAN_POINT ( 'NONE',  ( -18.54148534481894472, 10.32532329027886320, -173.0699343018359855 ) ) ;
#33324 = CIRCLE ( 'NONE', #16735, 0.1000000000000055844 ) ;
#33326 = DIRECTION ( 'NONE',  ( -0.000000000000000000, -0.000000000000000000, -1.000000000000000000 ) ) ;
#33328 = EDGE_CURVE ( 'NONE', #66671, #146761, #94386, .T. ) ;
#33327 = CARTESIAN_POINT ( 'NONE',  ( -20.87600722750343252, 10.33112638556969465, -206.5901228926974227 ) ) ;
#33329 = ORIENTED_EDGE ( 'NONE', *, *, #23175, .T. ) ;
#33330 = CARTESIAN_POINT ( 'NONE',  ( 15.15590539855245744, 46.89406695649157797, -234.6540829047534942 ) ) ;
#33331 = DIRECTION ( 'NONE',  ( -0.000000000000000000, -6.982962677686266711E-15, 1.000000000000000000 ) ) ;
#33333 = EDGE_CURVE ( 'NONE', #144573, #49235, #256660, .T. ) ;
#33332 = DIRECTION ( 'NONE',  ( 1.000000000000000000, -3.265361837132813093E-16, -2.280189983783949500E-30 ) ) ;
#33334 = DIRECTION ( 'NONE',  ( -1.000000000000000000, 5.467925025959462129E-15, 3.427148797533442008E-14 ) ) ;
#33335 = EDGE_LOOP ( 'NONE', ( #163505, #131969, #96981, #150657 ) ) ;
#33337 = LINE ( 'NONE', #175403, #142635 ) ;
#33336 = AXIS2_PLACEMENT_3D ( 'NONE', #143370, #84639, #62563 ) ;
#33339 = ORIENTED_EDGE ( 'NONE', *, *, #147185, .F. ) ;
#33338 = CARTESIAN_POINT ( 'NONE',  ( -17.80356949363508079, 65.12326860301504894, -193.2361805087437006 ) ) ;
#33340 = DIRECTION ( 'NONE',  ( -3.265361837132813093E-16, -1.000000000000000000, 7.445645354460596589E-46 ) ) ;
#33341 = CARTESIAN_POINT ( 'NONE',  ( -20.00857864376270001, 66.85000000001254250, -182.2731074845244166 ) ) ;
#33342 = CARTESIAN_POINT ( 'NONE',  ( 23.14999999999999503, 61.47936603916258491, -212.1738987416902376 ) ) ;
#33343 = VECTOR ( 'NONE', #217024, 1000.000000000000000 ) ;
#33344 = CARTESIAN_POINT ( 'NONE',  ( 20.94999999999999929, 84.73084112150763758, -160.4250327655399531 ) ) ;
#33345 = EDGE_CURVE ( 'NONE', #42862, #25623, #8408, .T. ) ;
#33346 = DIRECTION ( 'NONE',  ( 1.000000000000000000, 0.000000000000000000, 0.000000000000000000 ) ) ;
#33348 = EDGE_LOOP ( 'NONE', ( #168859, #212454, #151844, #71290 ) ) ;
#33347 = DIRECTION ( 'NONE',  ( -1.000000000000000000, -0.000000000000000000, -0.000000000000000000 ) ) ;
#33349 = DIRECTION ( 'NONE',  ( 0.000000000000000000, -1.000000000000000000, 0.000000000000000000 ) ) ;
#33350 = CIRCLE ( 'NONE', #216648, 0.09999999999999939493 ) ;
#33351 = DIRECTION ( 'NONE',  ( 6.938893903907131190E-14, -0.8814952561688476074, 0.4721928772777262417 ) ) ;
#33352 = DIRECTION ( 'NONE',  ( 0.000000000000000000, 0.2128009952263485993, -0.9770955615653341697 ) ) ;
#33353 = CIRCLE ( 'NONE', #58232, 0.1000000000000021844 ) ;
#33354 = VERTEX_POINT ( 'NONE', #103619 ) ;
#33355 = CARTESIAN_POINT ( 'NONE',  ( 21.13461538461538325, 8.885417037985616773, -112.8500000000000369 ) ) ;
#33356 = DIRECTION ( 'NONE',  ( 0.000000000000000000, -0.9651348961777157509, 0.2617529984165031243 ) ) ;
#33357 = CARTESIAN_POINT ( 'NONE',  ( 19.75857864376268935, 11.75000000001115907, -58.35000000000000142 ) ) ;
#33358 = SPHERICAL_SURFACE ( 'NONE', #54474, 0.1000000000000000056 ) ;
#33359 = CARTESIAN_POINT ( 'NONE',  ( 21.05000000000000071, 6.477552182504824785, -167.5999999652990482 ) ) ;
#33360 = AXIS2_PLACEMENT_3D ( 'NONE', #213172, #136174, #158381 ) ;
#33361 = AXIS2_PLACEMENT_3D ( 'NONE', #213258, #13788, #136269 ) ;
#33363 = ORIENTED_EDGE ( 'NONE', *, *, #180403, .F. ) ;
#33362 = AXIS2_PLACEMENT_3D ( 'NONE', #220561, #64051, #83578 ) ;
#33364 = EDGE_LOOP ( 'NONE', ( #126087, #130292 ) ) ;
#33365 = AXIS2_PLACEMENT_3D ( 'NONE', #193587, #172779, #18782 ) ;
#33366 = VECTOR ( 'NONE', #60962, 1000.000000000000000 ) ;
#33367 = DIRECTION ( 'NONE',  ( 0.000000000000000000, 0.000000000000000000, 1.000000000000000000 ) ) ;
#33368 = LINE ( 'NONE', #56699, #137404 ) ;
#33369 = AXIS2_PLACEMENT_3D ( 'NONE', #76191, #197427, #215695 ) ;
#33370 = DIRECTION ( 'NONE',  ( 0.000000000000000000, 0.000000000000000000, -1.000000000000000000 ) ) ;
#33371 = CYLINDRICAL_SURFACE ( 'NONE', #26743, 0.5000000000000004441 ) ;
#33372 = FACE_OUTER_BOUND ( 'NONE', #66592, .T. ) ;
#33373 = DIRECTION ( 'NONE',  ( -1.000000000000000000, -0.000000000000000000, -0.000000000000000000 ) ) ;
#33374 = DIRECTION ( 'NONE',  ( 0.000000000000000000, 0.000000000000000000, -1.000000000000000000 ) ) ;
#33375 = DIRECTION ( 'NONE',  ( 0.000000000000000000, 0.000000000000000000, 1.000000000000000000 ) ) ;
#33376 = VERTEX_POINT ( 'NONE', #85336 ) ;
#33377 = CARTESIAN_POINT ( 'NONE',  ( -20.00857864376270001, 9.150000000011157653, -112.7500000000000284 ) ) ;
#33378 = ORIENTED_EDGE ( 'NONE', *, *, #104895, .T. ) ;
#33379 = DIRECTION ( 'NONE',  ( 0.000000000000000000, 0.000000000000000000, 1.000000000000000000 ) ) ;
#33380 = CARTESIAN_POINT ( 'NONE',  ( 21.05000000000000071, 10.72371681399907040, -7.594399235884193189 ) ) ;
#33382 = ORIENTED_EDGE ( 'NONE', *, *, #253642, .T. ) ;
#33381 = CARTESIAN_POINT ( 'NONE',  ( 21.04999999999908411, 8.776282895301829257, -79.15790900265254493 ) ) ;
#33383 = DIRECTION ( 'NONE',  ( 1.000000000000000000, 0.000000000000000000, 0.000000000000000000 ) ) ;
#33384 =( LENGTH_UNIT ( ) NAMED_UNIT ( * ) SI_UNIT ( .MILLI., .METRE. ) );
#33385 = CARTESIAN_POINT ( 'NONE',  ( 18.50000000000000355, 85.42107434499828855, -62.69863542509442311 ) ) ;
#33386 = CARTESIAN_POINT ( 'NONE',  ( 21.05000000000000071, 1.115600667400684642E-11, -33.50000000000000000 ) ) ;
#33388 = ORIENTED_EDGE ( 'NONE', *, *, #230937, .F. ) ;
#33387 = CIRCLE ( 'NONE', #241638, 0.09999999999999938105 ) ;
#33389 = CARTESIAN_POINT ( 'NONE',  ( -16.93302609847409457, 22.94403737378339869, -230.8638760910858707 ) ) ;
#33390 = CARTESIAN_POINT ( 'NONE',  ( 20.94999999999999574, 11.97453674493551645, -206.0596400812808611 ) ) ;
#33391 = ADVANCED_FACE ( 'NONE', ( #127065 ), #140165, .T. ) ;
#33392 = CIRCLE ( 'NONE', #195700, 0.1000000000000024342 ) ;
#33393 = DIRECTION ( 'NONE',  ( 1.000000000000000000, 0.000000000000000000, 0.000000000000000000 ) ) ;
#33394 = DIRECTION ( 'NONE',  ( -1.000000000000000000, -0.000000000000000000, -0.000000000000000000 ) ) ;
#33395 = CARTESIAN_POINT ( 'NONE',  ( 23.14999999999998437, 76.00000000001237765, -170.0231074845243597 ) ) ;
#33396 = VECTOR ( 'NONE', #69213, 1000.000000000000000 ) ;
#33397 = ORIENTED_EDGE ( 'NONE', *, *, #170133, .F. ) ;
#33398 = CARTESIAN_POINT ( 'NONE',  ( -22.45305610364635385, 76.10085836911093793, -148.2726746080136593 ) ) ;
#33399 = DIRECTION ( 'NONE',  ( 0.000000000000000000, -1.000000000000000000, -6.982962677686266711E-15 ) ) ;
#33400 = ORIENTED_EDGE ( 'NONE', *, *, #205370, .F. ) ;
#33401 = ORIENTED_EDGE ( 'NONE', *, *, #160748, .T. ) ;
#33402 = CARTESIAN_POINT ( 'NONE',  ( -21.05000000000000071, 72.06821323333463170, -225.0920403225231610 ) ) ;
#33403 = DIRECTION ( 'NONE',  ( 0.000000000000000000, 0.000000000000000000, 1.000000000000000000 ) ) ;
#33405 = EDGE_CURVE ( 'NONE', #98885, #109697, #31886, .T. ) ;
#33404 = VECTOR ( 'NONE', #231245, 1000.000000000000000 ) ;
#33406 = EDGE_CURVE ( 'NONE', #163151, #38982, #244220, .T. ) ;
#33407 = AXIS2_PLACEMENT_3D ( 'NONE', #88305, #242266, #68783 ) ;
#33408 = ORIENTED_EDGE ( 'NONE', *, *, #230075, .F. ) ;
#33409 = CARTESIAN_POINT ( 'NONE',  ( 20.12500000000000355, 39.64491763323097473, -236.9907406594410588 ) ) ;
#33410 = DIRECTION ( 'NONE',  ( 0.000000000000000000, 0.8814952561688438326, -0.4721928772777334582 ) ) ;
#33411 = ORIENTED_EDGE ( 'NONE', *, *, #27846, .F. ) ;
#33412 = CIRCLE ( 'NONE', #183225, 0.09999999999999892308 ) ;
#33413 = PRESENTATION_LAYER_ASSIGNMENT (  '', '', ( #145793 ) ) ;
#33414 = CARTESIAN_POINT ( 'NONE',  ( -21.05000000000000071, 11.75000000001115552, -126.9851942293460922 ) ) ;
#33415 = EDGE_CURVE ( 'NONE', #208514, #138090, #134013, .T. ) ;
#33416 = ORIENTED_EDGE ( 'NONE', *, *, #77916, .F. ) ;
#33417 = ADVANCED_FACE ( 'NONE', ( #128357 ), #166223, .F. ) ;
#33418 = CARTESIAN_POINT ( 'NONE',  ( 21.10257677756356998, 75.97504925044421498, -142.9214892270570658 ) ) ;
#33419 = CYLINDRICAL_SURFACE ( 'NONE', #100392, 0.1000000000000101225 ) ;
#33422 = ORIENTED_EDGE ( 'NONE', *, *, #144397, .T. ) ;
#33421 = DIRECTION ( 'NONE',  ( 1.000000000000000000, 0.000000000000000000, 0.000000000000000000 ) ) ;
#33420 =( BOUNDED_SURFACE ( )  B_SPLINE_SURFACE ( 3, 2, ( 
 ( #2676, #142199, #1385 ),
 ( #97902, #57508, #21001 ),
 ( #178803, #221710, #61379 ),
 ( #121398, #241316, #43106 ),
 ( #120108, #22272, #159219 ),
 ( #238734, #18400, #160510 ),
 ( #139605, #100475, #58787 ),
 ( #177517, #108, #156667 ),
 ( #138322, #236164, #137066 ),
 ( #216600, #79638, #122659 ) ),
 .UNSPECIFIED., .F., .F., .F. ) 
 B_SPLINE_SURFACE_WITH_KNOTS ( ( 4, 2, 2, 2, 4 ),
 ( 3, 3 ),
 ( 0.002161241639767251272, 0.002579950749615826135, 0.002789305304540113349, 0.002893982582002256956, 0.002998659859464400564 ),
 ( 0.000000000000000000, 1.000000000000000000 ),
 .UNSPECIFIED. ) 
 GEOMETRIC_REPRESENTATION_ITEM ( )  RATIONAL_B_SPLINE_SURFACE ( (
 ( 1.000000000000000000, 0.7071067811865655584, 1.000000000000000000),
 ( 1.000000000000000000, 0.7632447400662427661, 1.000000000000000000),
 ( 1.000000000000000000, 0.8158073005112935761, 1.000000000000000000),
 ( 1.000000000000000000, 0.8906973462394487395, 1.000000000000000000),
 ( 1.000000000000000000, 0.9149408947805062198, 1.000000000000000000),
 ( 1.000000000000000000, 0.9493368785273317290, 1.000000000000000000),
 ( 1.000000000000000000, 0.9605194247157643472, 1.000000000000000000),
 ( 1.000000000000000000, 0.9803630264780097692, 1.000000000000000000),
 ( 1.000000000000000000, 0.9900844824271883837, 1.000000000000000000),
 ( 1.000000000000000000, 0.9894588281429257393, 1.000000000000000000) ) ) 
 REPRESENTATION_ITEM ( '' )  SURFACE ( )  );
#33423 = DIRECTION ( 'NONE',  ( 1.000000000000000000, 0.000000000000000000, 0.000000000000000000 ) ) ;
#33424 = CARTESIAN_POINT ( 'NONE',  ( -21.44999999999999929, 7.349999999999998757, -12.34999999999999964 ) ) ;
#33425 = ADVANCED_FACE ( 'NONE', ( #9677 ), #152699, .F. ) ;
#33426 = DIRECTION ( 'NONE',  ( 0.000000000000000000, 0.000000000000000000, -1.000000000000000000 ) ) ;
#33427 = DIRECTION ( 'NONE',  ( 1.000000000000000000, 0.000000000000000000, 0.000000000000000000 ) ) ;
#33428 = DIRECTION ( 'NONE',  ( -0.000000000000000000, 1.000000000000000000, -0.000000000000000000 ) ) ;
#33429 = DIRECTION ( 'NONE',  ( 0.000000000000000000, 0.000000000000000000, 1.000000000000000000 ) ) ;
#33430 = DIRECTION ( 'NONE',  ( 0.000000000000000000, -1.000000000000000000, 0.000000000000000000 ) ) ;
#33432 = VERTEX_POINT ( 'NONE', #86621 ) ;
#33431 = DIRECTION ( 'NONE',  ( 0.000000000000000000, 0.000000000000000000, 1.000000000000000000 ) ) ;
#33433 = EDGE_LOOP ( 'NONE', ( #154399, #93332, #201403, #78768 ) ) ;
#33436 = CARTESIAN_POINT ( 'NONE',  ( -18.50000000000000000, 64.35000000001222986, -148.6731074845244507 ) ) ;
#33435 = DIRECTION ( 'NONE',  ( 0.000000000000000000, -0.8660254037844383745, 0.5000000000000003331 ) ) ;
#33434 = AXIS2_PLACEMENT_3D ( 'NONE', #36104, #214718, #215989 ) ;
#33437 = EDGE_CURVE ( 'NONE', #176509, #73651, #32072, .T. ) ;
#33438 = CIRCLE ( 'NONE', #120911, 12.87499999999999822 ) ;
#33440 = ORIENTED_EDGE ( 'NONE', *, *, #144736, .T. ) ;
#33439 = LINE ( 'NONE', #12574, #72584 ) ;
#33441 = ORIENTED_EDGE ( 'NONE', *, *, #22013, .F. ) ;
#33442 = DIRECTION ( 'NONE',  ( -1.000000000000000000, -0.000000000000000000, -0.000000000000000000 ) ) ;
#33443 = DIRECTION ( 'NONE',  ( -1.000000000000000000, 0.000000000000000000, 0.000000000000000000 ) ) ;
#33444 = ADVANCED_FACE ( 'NONE', ( #163630 ), #144039, .F. ) ;
#33445 =( BOUNDED_CURVE ( )  B_SPLINE_CURVE ( 3, ( #161457, #59742, #122317, #201845 ),
 .UNSPECIFIED., .F., .F. ) 
 B_SPLINE_CURVE_WITH_KNOTS ( ( 4, 4 ),
 ( 3.141592653589793116, 4.712388980384689674 ),
 .UNSPECIFIED. ) 
 CURVE ( )  GEOMETRIC_REPRESENTATION_ITEM ( )  RATIONAL_B_SPLINE_CURVE ( ( 1.000000000000000000, 0.8047378541243649375, 0.8047378541243649375, 1.000000000000000000 ) ) 
 REPRESENTATION_ITEM ( '' )  );
#33446 = DIRECTION ( 'NONE',  ( 1.000000000000000000, -0.000000000000000000, 0.000000000000000000 ) ) ;
#33447 = CARTESIAN_POINT ( 'NONE',  ( 20.01093837587850288, 11.75000000001116263, -58.25439743459698150 ) ) ;
#33448 = CARTESIAN_POINT ( 'NONE',  ( -18.50000972452446035, 67.49459761544872549, -195.5598716110968667 ) ) ;
#33449 = CARTESIAN_POINT ( 'NONE',  ( -23.25000000000000000, -11.64999999998884483, -63.89999999999999858 ) ) ;
#33450 = EDGE_CURVE ( 'NONE', #200975, #206663, #252790, .T. ) ;
#33451 = CARTESIAN_POINT ( 'NONE',  ( -20.94999999999999929, 1.250000000011155299, -41.50000000000000000 ) ) ;
#33452 = CIRCLE ( 'NONE', #179187, 0.09999999999999939493 ) ;
#33453 = ORIENTED_EDGE ( 'NONE', *, *, #113681, .T. ) ;
#33454 = ORIENTED_EDGE ( 'NONE', *, *, #40961, .T. ) ;
#33455 = AXIS2_PLACEMENT_3D ( 'NONE', #78454, #138411, #158056 ) ;
#33456 = FACE_OUTER_BOUND ( 'NONE', #70280, .T. ) ;
#33457 = CIRCLE ( 'NONE', #174943, 12.87499999999999822 ) ;
#33458 = AXIS2_PLACEMENT_3D ( 'NONE', #238177, #38720, #118247 ) ;
#33459 = ORIENTED_EDGE ( 'NONE', *, *, #87901, .T. ) ;
#33460 = PLANE ( 'NONE',  #213762 ) ;
#33461 = EDGE_LOOP ( 'NONE', ( #110578, #123195, #14201 ) ) ;
#33462 = DIRECTION ( 'NONE',  ( 0.000000000000000000, 0.1495327102803689356, -0.9887567792719336168 ) ) ;
#33463 =( BOUNDED_SURFACE ( )  B_SPLINE_SURFACE ( 3, 2, ( 
 ( #217529, #38927, #80574 ),
 ( #19354, #118469, #20653 ),
 ( #79301, #59730, #160174 ),
 ( #139270, #239686, #220122 ),
 ( #41501, #121050, #200551 ),
 ( #22017, #101491, #41593 ) ),
 .UNSPECIFIED., .F., .F., .F. ) 
 B_SPLINE_SURFACE_WITH_KNOTS ( ( 4, 2, 4 ),
 ( 3, 3 ),
 ( 1.570796326794897668, 2.356194490192346169, 3.141592653589794448 ),
 ( 0.000000000000000000, 1.000000000000000000 ),
 .UNSPECIFIED. ) 
 GEOMETRIC_REPRESENTATION_ITEM ( )  RATIONAL_B_SPLINE_SURFACE ( (
 ( 1.000000000000000000, 0.7071067811865597852, 1.000000000000000000),
 ( 1.000000000000000000, 0.6611148371781052635, 1.000000000000000000),
 ( 1.000000000000000000, 0.6092287576693442563, 1.000000000000000000),
 ( 1.000000000000000000, 0.5278258667060597986, 1.000000000000000000),
 ( 1.000000000000000000, 0.4993418825334668965, 1.000000000000000000),
 ( 1.000000000000000000, 0.5000000000000456302, 1.000000000000000000) ) ) 
 REPRESENTATION_ITEM ( '' )  SURFACE ( )  );
#33464 = VECTOR ( 'NONE', #256455, 1000.000000000000114 ) ;
#33465 = DIRECTION ( 'NONE',  ( 1.000000000000000000, 0.000000000000000000, -0.000000000000000000 ) ) ;
#33466 = FACE_OUTER_BOUND ( 'NONE', #35139, .T. ) ;
#33467 = VERTEX_POINT ( 'NONE', #106193 ) ;
#33468 = DIRECTION ( 'NONE',  ( 0.000000000000000000, 0.000000000000000000, 1.000000000000000000 ) ) ;
#33469 = ORIENTED_EDGE ( 'NONE', *, *, #213918, .T. ) ;
#33470 = CIRCLE ( 'NONE', #183272, 0.1999999999999987899 ) ;
#33471 = FACE_OUTER_BOUND ( 'NONE', #75577, .T. ) ;
#33473 = AXIS2_PLACEMENT_3D ( 'NONE', #110177, #26830, #188432 ) ;
#33472 = DIRECTION ( 'NONE',  ( -1.000000000000000000, 2.952720810173289112E-16, 2.061873921506763405E-30 ) ) ;
#33474 = EDGE_LOOP ( 'NONE', ( #102701, #232933, #84603, #6651 ) ) ;
#33475 = DIRECTION ( 'NONE',  ( 0.000000000000000000, -0.8660254037844377084, -0.5000000000000016653 ) ) ;
#33476 = B_SPLINE_CURVE_WITH_KNOTS ( 'NONE', 3,
 ( #96403, #155152, #256727, #20757, #59835, #79405, #233394, #158997, #175986, #218921, #238497, #139377, #117278, #114703, #55985, #213802, #199398, #179830, #153886, #37758, #54725, #194271, #255443, #15638, #95141, #174731 ),
 .UNSPECIFIED., .F., .F.,
 ( 4, 2, 2, 2, 2, 2, 2, 2, 2, 2, 2, 2, 4 ),
 ( 0.005476422646581360389, 0.006160811967703572201, 0.006845201288825784013, 0.007187395949386890352, 0.007529590609947995825, 0.007871785270509102164, 0.008213979931070208504, 0.008556174591631314844, 0.008898369252192419449, 0.009240563912753525788, 0.009582758573314632128, 0.01026714789443684134, 0.01095153721555904881 ),
 .UNSPECIFIED. ) ;
#33477 = EDGE_LOOP ( 'NONE', ( #189488, #188076, #10246, #4936 ) ) ;
#33480 = ORIENTED_EDGE ( 'NONE', *, *, #182872, .T. ) ;
#33479 = DIRECTION ( 'NONE',  ( 0.000000000000000000, 0.1332476588733636502, -0.9910827722268044093 ) ) ;
#33478 = CARTESIAN_POINT ( 'NONE',  ( 22.48970261584622676, 55.97295988302632708, -232.8591431001882484 ) ) ;
#33481 = CARTESIAN_POINT ( 'NONE',  ( -20.99551997958381833, 64.25000000001146816, -42.87144834683500960 ) ) ;
#33482 = VERTEX_POINT ( 'NONE', #147923 ) ;
#33483 = ADVANCED_FACE ( 'NONE', ( #185755 ), #111154, .T. ) ;
#33484 = EDGE_LOOP ( 'NONE', ( #33001, #44586, #110798, #206880 ) ) ;
#33485 = EDGE_CURVE ( 'NONE', #138899, #169470, #7102, .T. ) ;
#33486 = DIRECTION ( 'NONE',  ( 1.000000000000000000, 0.000000000000000000, 0.000000000000000000 ) ) ;
#33487 = ORIENTED_EDGE ( 'NONE', *, *, #17806, .F. ) ;
#33488 = ADVANCED_FACE ( 'NONE', ( #231320 ), #52646, .T. ) ;
#33489 = DIRECTION ( 'NONE',  ( 1.000000000000000000, 0.000000000000000000, 0.000000000000000000 ) ) ;
#33490 = ADVANCED_FACE ( 'NONE', ( #51338 ), #132200, .F. ) ;
#33491 = CARTESIAN_POINT ( 'NONE',  ( -22.50000000000000000, 11.64957080755595520, -33.40000000000000568 ) ) ;
#33492 = CARTESIAN_POINT ( 'NONE',  ( -23.25000000000000000, 69.01799029515598249, -166.3269553662681233 ) ) ;
#33493 = DIRECTION ( 'NONE',  ( -1.020425574104003999E-15, 0.2128009952263603677, -0.9770955615653313941 ) ) ;
#33495 = EDGE_LOOP ( 'NONE', ( #142533, #216917, #155545, #8295 ) ) ;
#33494 = ADVANCED_FACE ( 'NONE', ( #39230 ), #177462, .F. ) ;
#33496 = CARTESIAN_POINT ( 'NONE',  ( -20.94999999999999929, 62.98048128140160173, -207.0210305352945852 ) ) ;
#33497 = CARTESIAN_POINT ( 'NONE',  ( -21.04999999999994387, 74.63923853664559260, -43.99645795275012006 ) ) ;
#33498 = CARTESIAN_POINT ( 'NONE',  ( -13.77178122865955068, 66.54397173950437150, -155.0119094494586989 ) ) ;
#33499 = CIRCLE ( 'NONE', #183491, 0.1000000000000106498 ) ;
#33500 = EDGE_CURVE ( 'NONE', #210647, #220516, #256838, .T. ) ;
#33501 = ORIENTED_EDGE ( 'NONE', *, *, #168610, .F. ) ;
#33502 = CARTESIAN_POINT ( 'NONE',  ( -22.42357213249529124, 0.09908696400155765638, 7.672932386359936352 ) ) ;
#33504 = EDGE_CURVE ( 'NONE', #251232, #128048, #48788, .T. ) ;
#33503 = EDGE_LOOP ( 'NONE', ( #201096, #233425, #204017, #101452 ) ) ;
#33505 = DIRECTION ( 'NONE',  ( 0.000000000000000000, 0.2617529984164955192, 0.9651348961777178603 ) ) ;
#33506 = EDGE_LOOP ( 'NONE', ( #221197, #160908, #8110, #3475 ) ) ;
#33507 = DIRECTION ( 'NONE',  ( 1.000000000000000000, 0.000000000000000000, 0.000000000000000000 ) ) ;
#33508 = CYLINDRICAL_SURFACE ( 'NONE', #206066, 0.09999999999999939493 ) ;
#33509 = EDGE_CURVE ( 'NONE', #238381, #239916, #23884, .T. ) ;
#33510 = CIRCLE ( 'NONE', #8520, 0.1000000000000017958 ) ;
#33512 = VERTEX_POINT ( 'NONE', #79589 ) ;
#33511 = FACE_OUTER_BOUND ( 'NONE', #12034, .T. ) ;
#33513 = CARTESIAN_POINT ( 'NONE',  ( 18.52928932188133970, 63.76258513157054608, -209.3739165141045078 ) ) ;
#33514 = ORIENTED_EDGE ( 'NONE', *, *, #27407, .T. ) ;
#33515 = DIRECTION ( 'NONE',  ( -1.000000000000000000, 0.000000000000000000, 0.000000000000000000 ) ) ;
#33516 = EDGE_CURVE ( 'NONE', #173018, #31916, #137019, .T. ) ;
#33517 = DIRECTION ( 'NONE',  ( -0.7071067811865463515, 0.7071067811865487940, -0.000000000000000000 ) ) ;
#33518 = ORIENTED_EDGE ( 'NONE', *, *, #82243, .T. ) ;
#33519 = CARTESIAN_POINT ( 'NONE',  ( -21.46681500598102232, 1.115539681028482333E-11, -127.1424888405744724 ) ) ;
#33520 = CARTESIAN_POINT ( 'NONE',  ( -22.39999999999999858, -3.140208063160689012, -228.2318569537739847 ) ) ;
#33522 = ORIENTED_EDGE ( 'NONE', *, *, #234125, .F. ) ;
#33521 = EDGE_CURVE ( 'NONE', #27329, #16250, #216550, .T. ) ;
#33523 = CARTESIAN_POINT ( 'NONE',  ( 21.05000000000000426, 1.434708683019007225, -230.7796371565282527 ) ) ;
#33524 = AXIS2_PLACEMENT_3D ( 'NONE', #37537, #35002, #257796 ) ;
#33525 = VECTOR ( 'NONE', #180914, 1000.000000000000000 ) ;
#33526 = ORIENTED_EDGE ( 'NONE', *, *, #54896, .T. ) ;
#33527 = EDGE_CURVE ( 'NONE', #123690, #113902, #27985, .T. ) ;
#33528 = CARTESIAN_POINT ( 'NONE',  ( 12.25000000000000178, 9.350000000011140955, -117.3642676076161138 ) ) ;
#33529 = DIRECTION ( 'NONE',  ( 0.000000000000000000, -0.2128009952263612281, 0.9770955615653312831 ) ) ;
#33530 = STYLED_ITEM ( 'NONE', ( #199767 ), #193773 ) ;
#33531 = EDGE_CURVE ( 'NONE', #49507, #240745, #119551, .T. ) ;
#33532 = ADVANCED_FACE ( 'NONE', ( #37943, #129631 ), #255630, .T. ) ;
#33533 = VECTOR ( 'NONE', #193342, 1000.000000000000000 ) ;
#33534 = VECTOR ( 'NONE', #16714, 1000.000000000000000 ) ;
#33536 = VERTEX_POINT ( 'NONE', #209157 ) ;
#33535 = DIRECTION ( 'NONE',  ( 1.000000000000000000, 0.000000000000000000, 0.000000000000000000 ) ) ;
#33537 = CARTESIAN_POINT ( 'NONE',  ( 23.14999999999998437, 76.00000000001237765, -170.0231074845243597 ) ) ;
#33538 = CARTESIAN_POINT ( 'NONE',  ( 21.05000000000000071, 14.81796439977981272, -236.5325475414793743 ) ) ;
#33539 = CARTESIAN_POINT ( 'NONE',  ( -23.15000000000000213, -8.999999999988844479, -124.1060308773475924 ) ) ;
#33541 = CARTESIAN_POINT ( 'NONE',  ( -14.77538296656415717, 66.56333706821246210, -51.20007075222951443 ) ) ;
#33540 = DIRECTION ( 'NONE',  ( -1.000000000000000000, 0.000000000000000000, 0.000000000000000000 ) ) ;
#33542 = CYLINDRICAL_SURFACE ( 'NONE', #207637, 0.1000000000000106914 ) ;
#33543 = CARTESIAN_POINT ( 'NONE',  ( 20.84999999999998721, -11.74999999998884448, -67.00000000000000000 ) ) ;
#33544 = DIRECTION ( 'NONE',  ( 1.000000000000000000, 7.304098846218134667E-16, 5.100424963727256530E-30 ) ) ;
#33545 = VECTOR ( 'NONE', #63750, 1000.000000000000000 ) ;
#33546 = CARTESIAN_POINT ( 'NONE',  ( -13.39999999999994351, 64.35000000001120668, -18.42310748452479174 ) ) ;
#33547 = CIRCLE ( 'NONE', #145916, 0.1000000000000106914 ) ;
#33548 = AXIS2_PLACEMENT_3D ( 'NONE', #194298, #58588, #15666 ) ;
#33549 = ORIENTED_EDGE ( 'NONE', *, *, #193954, .T. ) ;
#33550 = VECTOR ( 'NONE', #16255, 1000.000000000000000 ) ;
#33552 = ORIENTED_EDGE ( 'NONE', *, *, #227696, .F. ) ;
#33551 = CIRCLE ( 'NONE', #158439, 11.70000000000000639 ) ;
#33553 = LINE ( 'NONE', #131312, #166683 ) ;
#33555 = EDGE_LOOP ( 'NONE', ( #2272, #233683, #44635, #34892, #150179, #120852, #193278, #174353, #4013, #136700, #90405 ) ) ;
#33554 = FACE_OUTER_BOUND ( 'NONE', #230728, .T. ) ;
#33556 = VERTEX_POINT ( 'NONE', #30554 ) ;
#33557 = LINE ( 'NONE', #10093, #201910 ) ;
#33558 = ORIENTED_EDGE ( 'NONE', *, *, #155932, .F. ) ;
#33559 = FACE_OUTER_BOUND ( 'NONE', #200078, .T. ) ;
#33560 = AXIS2_PLACEMENT_3D ( 'NONE', #5237, #207339, #245171 ) ;
#33561 = ORIENTED_EDGE ( 'NONE', *, *, #200124, .T. ) ;
#33562 = DIRECTION ( 'NONE',  ( 0.000000000000000000, 4.163336342344217877E-13, -1.000000000000000000 ) ) ;
#33564 = VERTEX_POINT ( 'NONE', #198269 ) ;
#33563 = ORIENTED_EDGE ( 'NONE', *, *, #122180, .F. ) ;
#33565 = ORIENTED_EDGE ( 'NONE', *, *, #191890, .F. ) ;
#33566 = ORIENTED_EDGE ( 'NONE', *, *, #201556, .T. ) ;
#33567 = EDGE_LOOP ( 'NONE', ( #173696, #74858, #157161, #66577 ) ) ;
#33568 = DIRECTION ( 'NONE',  ( 1.000000000000000000, 0.000000000000000000, 0.000000000000000000 ) ) ;
#33569 = DIRECTION ( 'NONE',  ( -1.000000000000000000, -0.000000000000000000, -0.000000000000000000 ) ) ;
#33570 = DIRECTION ( 'NONE',  ( -0.000000000000000000, -6.982962677686266711E-15, 1.000000000000000000 ) ) ;
#33572 = VERTEX_POINT ( 'NONE', #19650 ) ;
#33571 = CARTESIAN_POINT ( 'NONE',  ( -18.34374000495060386, 64.52683809664983983, -160.7731074845244450 ) ) ;
#33573 = CARTESIAN_POINT ( 'NONE',  ( -20.94999999999999929, 0.4879293624014888198, -209.1697915983179428 ) ) ;
#33574 = CARTESIAN_POINT ( 'NONE',  ( 21.53699400381851703, 6.787711793190427834, -167.4999999999999432 ) ) ;
#33576 = ORIENTED_EDGE ( 'NONE', *, *, #213842, .F. ) ;
#33575 = DIRECTION ( 'NONE',  ( 1.000000000000000000, 0.000000000000000000, 0.000000000000000000 ) ) ;
#33577 = LINE ( 'NONE', #202858, #170872 ) ;
#33578 = EDGE_LOOP ( 'NONE', ( #28113, #15067, #222911, #77711 ) ) ;
#33579 = DIRECTION ( 'NONE',  ( -0.000000000000000000, 0.8660254037844411501, 0.4999999999999956701 ) ) ;
#33580 = B_SPLINE_CURVE_WITH_KNOTS ( 'NONE', 3,
 ( #12934, #10354, #31230, #70346 ),
 .UNSPECIFIED., .F., .F.,
 ( 4, 4 ),
 ( 3.469446951953614189E-18, 0.0001058379652594603572 ),
 .UNSPECIFIED. ) ;
#33582 = ORIENTED_EDGE ( 'NONE', *, *, #111931, .T. ) ;
#33581 = CARTESIAN_POINT ( 'NONE',  ( -18.59999999999999787, 7.070967871809997973, -171.2465642218683115 ) ) ;
#33583 = CARTESIAN_POINT ( 'NONE',  ( -21.65000000000000213, 7.249999999999983125, -20.85000000000000142 ) ) ;
#33585 = ADVANCED_FACE ( 'NONE', ( #196977 ), #256914, .T. ) ;
#33584 = CARTESIAN_POINT ( 'NONE',  ( -16.87036670365548474, 30.33914847462231279, -234.8334748671511818 ) ) ;
#33586 = AXIS2_PLACEMENT_3D ( 'NONE', #204398, #103998, #25779 ) ;
#33587 = ORIENTED_EDGE ( 'NONE', *, *, #202985, .T. ) ;
#33589 = CARTESIAN_POINT ( 'NONE',  ( 20.94999999999999929, 87.48912529308852015, -173.1231074845242688 ) ) ;
#33588 = DIRECTION ( 'NONE',  ( 1.000000000000000000, 0.000000000000000000, 0.000000000000000000 ) ) ;
#33590 = EDGE_CURVE ( 'NONE', #38886, #99286, #189616, .T. ) ;
#33591 = CARTESIAN_POINT ( 'NONE',  ( 23.14999999999999858, 1.115600667400684642E-11, -100.5000000000000284 ) ) ;
#33592 = AXIS2_PLACEMENT_3D ( 'NONE', #166729, #220267, #161584 ) ;
#33593 = PLANE ( 'NONE',  #168187 ) ;
#33594 = CARTESIAN_POINT ( 'NONE',  ( 20.46382478191414833, 10.59862044130854031, -41.17781446934547063 ) ) ;
#33595 = ORIENTED_EDGE ( 'NONE', *, *, #37815, .F. ) ;
#33596 = ORIENTED_EDGE ( 'NONE', *, *, #118921, .F. ) ;
#33597 = EDGE_CURVE ( 'NONE', #63208, #224437, #182081, .T. ) ;
#33599 = AXIS2_PLACEMENT_3D ( 'NONE', #101508, #144507, #124974 ) ;
#33598 = CARTESIAN_POINT ( 'NONE',  ( 21.05000000000000071, 8.894723818377805458, -8.487084323149780118 ) ) ;
#33601 = EDGE_CURVE ( 'NONE', #249928, #254695, #144441, .T. ) ;
#33600 = LINE ( 'NONE', #54392, #152569 ) ;
#33602 = VERTEX_POINT ( 'NONE', #181301 ) ;
#33603 = DIRECTION ( 'NONE',  ( -0.000000000000000000, -0.1298341882519737922, -0.9915357197604890427 ) ) ;
#33604 = EDGE_LOOP ( 'NONE', ( #140236, #28100, #56123, #139503 ) ) ;
#33605 = SPHERICAL_SURFACE ( 'NONE', #252323, 0.1000000000000000056 ) ;
#33606 = CARTESIAN_POINT ( 'NONE',  ( 20.94999999999999574, 13.66123737402873495, -238.6633470470287648 ) ) ;
#33607 = CARTESIAN_POINT ( 'NONE',  ( 18.59999999999999076, 54.98105481382776816, -230.1569079895687366 ) ) ;
#33608 = VECTOR ( 'NONE', #54978, 1000.000000000000000 ) ;
#33609 = EDGE_LOOP ( 'NONE', ( #39952, #176135, #11143, #211476 ) ) ;
#33610 = DIRECTION ( 'NONE',  ( 1.000000000000000000, 0.000000000000000000, 0.000000000000000000 ) ) ;
#33611 = VECTOR ( 'NONE', #183681, 1000.000000000000000 ) ;
#33613 = VERTEX_POINT ( 'NONE', #103008 ) ;
#33612 = AXIS2_PLACEMENT_3D ( 'NONE', #71419, #248759, #12737 ) ;
#33614 = EDGE_LOOP ( 'NONE', ( #131629, #132624, #129988, #205289 ) ) ;
#33615 = EDGE_CURVE ( 'NONE', #60618, #102466, #182584, .T. ) ;
#33616 = EDGE_LOOP ( 'NONE', ( #74634, #93436, #257144, #114465, #219677 ) ) ;
#33617 = AXIS2_PLACEMENT_3D ( 'NONE', #231720, #73947, #93463 ) ;
#33618 = DIRECTION ( 'NONE',  ( 0.7070776581709139474, 0.7071359030027652981, 2.946958787807621248E-14 ) ) ;
#33619 = DIRECTION ( 'NONE',  ( -1.000000000000000000, 0.000000000000000000, 0.000000000000000000 ) ) ;
#33620 = FACE_OUTER_BOUND ( 'NONE', #232116, .T. ) ;
#33621 = LINE ( 'NONE', #149691, #165375 ) ;
#33622 = DIRECTION ( 'NONE',  ( 0.000000000000000000, 1.000000000000000000, 0.000000000000000000 ) ) ;
#33624 = CARTESIAN_POINT ( 'NONE',  ( 21.09706851349341861, 8.775842513473394391, -12.23556621639964703 ) ) ;
#33623 = CARTESIAN_POINT ( 'NONE',  ( -21.53699400380515527, 10.33394250185281926, -227.7493655664984828 ) ) ;
#33626 = ORIENTED_EDGE ( 'NONE', *, *, #219086, .F. ) ;
#33625 = CARTESIAN_POINT ( 'NONE',  ( 22.39999999999999503, 11.65000000001116298, -134.0000000000000284 ) ) ;
#33627 = CARTESIAN_POINT ( 'NONE',  ( -21.22070241538126112, 10.09669923035030692, -227.9827655035915654 ) ) ;
#33628 = ORIENTED_EDGE ( 'NONE', *, *, #38925, .F. ) ;
#33629 = CARTESIAN_POINT ( 'NONE',  ( 21.05000000000000071, 34.98408343502854478, -248.6539962344157004 ) ) ;
#33630 = ORIENTED_EDGE ( 'NONE', *, *, #35368, .F. ) ;
#33631 = ORIENTED_EDGE ( 'NONE', *, *, #233406, .F. ) ;
#33632 = DIRECTION ( 'NONE',  ( 0.000000000000000000, 0.000000000000000000, -1.000000000000000000 ) ) ;
#33633 = LINE ( 'NONE', #150966, #114295 ) ;
#33634 = CARTESIAN_POINT ( 'NONE',  ( -16.86578989773641979, 66.01519019875277650, -56.98777237114663308 ) ) ;
#33635 = ADVANCED_FACE ( 'NONE', ( #242532 ), #160465, .F. ) ;
#33636 = CARTESIAN_POINT ( 'NONE',  ( 20.95224633520496127, 8.900522166568386240, -75.49327644792130343 ) ) ;
#33637 = VECTOR ( 'NONE', #124848, 1000.000000000000000 ) ;
#33638 = EDGE_CURVE ( 'NONE', #136422, #181531, #211116, .T. ) ;
#33639 = DIRECTION ( 'NONE',  ( 0.000000000000000000, -4.336808689941893885E-15, 1.000000000000000000 ) ) ;
#33640 = ORIENTED_EDGE ( 'NONE', *, *, #170808, .F. ) ;
#33641 = ORIENTED_EDGE ( 'NONE', *, *, #241072, .T. ) ;
#33642 = DIRECTION ( 'NONE',  ( -1.000000000000000000, 0.000000000000000000, 0.000000000000000000 ) ) ;
#33643 = ORIENTED_EDGE ( 'NONE', *, *, #234632, .T. ) ;
#33644 = DIRECTION ( 'NONE',  ( -1.000000000000000000, 0.000000000000000000, 0.000000000000000000 ) ) ;
#33645 = DIRECTION ( 'NONE',  ( 1.000000000000000000, 0.000000000000000000, 0.000000000000000000 ) ) ;
#33646 = EDGE_LOOP ( 'NONE', ( #253217, #127986, #222732, #139321 ) ) ;
#33647 = CARTESIAN_POINT ( 'NONE',  ( 20.94999999999999929, 70.15000000001148805, -46.15560470880229360 ) ) ;
#33648 = CARTESIAN_POINT ( 'NONE',  ( -21.05315837350849506, 11.74999999738093059, -60.15835599785489052 ) ) ;
#33649 = CARTESIAN_POINT ( 'NONE',  ( -23.15000000000000213, 5.900000000000005684, -23.28090023534362629 ) ) ;
#33651 = ADVANCED_FACE ( 'NONE', ( #120055 ), #136248, .F. ) ;
#33650 = CARTESIAN_POINT ( 'NONE',  ( -20.64999999999999858, 7.250000000011155521, -179.7499999999999716 ) ) ;
#33652 = EDGE_LOOP ( 'NONE', ( #243868, #134091, #247997, #21405 ) ) ;
#33653 = ADVANCED_FACE ( 'NONE', ( #139564 ), #202916, .T. ) ;
#33654 = PLANE ( 'NONE',  #225195 ) ;
#33655 = CIRCLE ( 'NONE', #241698, 0.09999999999999761857 ) ;
#33656 = AXIS2_PLACEMENT_3D ( 'NONE', #178582, #79428, #41631 ) ;
#33657 = DIRECTION ( 'NONE',  ( -1.000000000000000000, -0.000000000000000000, -0.000000000000000000 ) ) ;
#33658 = AXIS2_PLACEMENT_3D ( 'NONE', #104756, #5661, #3101 ) ;
#33659 = ADVANCED_FACE ( 'NONE', ( #140877 ), #222961, .F. ) ;
#33660 = CARTESIAN_POINT ( 'NONE',  ( -20.64999999999999858, 68.56901367119438362, -214.3038979092079046 ) ) ;
#33661 = B_SPLINE_CURVE_WITH_KNOTS ( 'NONE', 3,
 ( #174518, #38806, #118346, #214859, #157495, #196575, #175760, #36253, #197858, #57039 ),
 .UNSPECIFIED., .F., .F.,
 ( 4, 2, 2, 2, 4 ),
 ( 0.000000000000000000, 0.0001584437871624776975, 0.0002376656807437485031, 0.0002772766275343839060, 0.0003168875743250193088 ),
 .UNSPECIFIED. ) ;
#33662 = ORIENTED_EDGE ( 'NONE', *, *, #181224, .F. ) ;
#33663 = AXIS2_PLACEMENT_3D ( 'NONE', #129824, #51543, #93266 ) ;
#33664 = CARTESIAN_POINT ( 'NONE',  ( -23.25000000000000000, 74.08971962618021223, -115.6544753397232626 ) ) ;
#33665 = ORIENTED_EDGE ( 'NONE', *, *, #2437, .F. ) ;
#33666 = CARTESIAN_POINT ( 'NONE',  ( 21.30000000000002558, 76.00000000001192291, -98.97310748452431994 ) ) ;
#33667 = EDGE_CURVE ( 'NONE', #239872, #128673, #123633, .T. ) ;
#33668 = CARTESIAN_POINT ( 'NONE',  ( -16.93433913041102912, 14.23186370317824156, -219.3265704725438638 ) ) ;
#33669 = CARTESIAN_POINT ( 'NONE',  ( 18.39999999999999858, 86.99291436658650412, -199.6658631664729739 ) ) ;
#33670 = DIRECTION ( 'NONE',  ( 0.000000000000000000, -0.3634403228828271271, 0.9316174814283092465 ) ) ;
#33671 = DIRECTION ( 'NONE',  ( 0.000000000000000000, 0.000000000000000000, 1.000000000000000000 ) ) ;
#33672 = CARTESIAN_POINT ( 'NONE',  ( 20.04142135623730070, 11.65000000001115943, -88.25000000000005684 ) ) ;
#33673 = AXIS2_PLACEMENT_3D ( 'NONE', #100607, #202315, #134922 ) ;
#33674 = ORIENTED_EDGE ( 'NONE', *, *, #37358, .F. ) ;
#33675 = CARTESIAN_POINT ( 'NONE',  ( 23.14999999999999858, 4.898587196589414801E-16, -29.50000000000000355 ) ) ;
#33676 = ADVANCED_FACE ( 'NONE', ( #165585 ), #90478, .F. ) ;
#33677 = CARTESIAN_POINT ( 'NONE',  ( -20.54999999999999716, -6.438379425586759908, -212.1495692908769684 ) ) ;
#33678 = DIRECTION ( 'NONE',  ( 1.734723475976817507E-14, 0.000000000000000000, -1.000000000000000000 ) ) ;
#33679 = DIRECTION ( 'NONE',  ( 0.7071067811865302533, -0.6909108974501196876, -0.1504730267679053324 ) ) ;
#33680 = ORIENTED_EDGE ( 'NONE', *, *, #85600, .T. ) ;
#33681 = ORIENTED_EDGE ( 'NONE', *, *, #135274, .F. ) ;
#33682 = CARTESIAN_POINT ( 'NONE',  ( 20.00000000000000355, 1.250000000000000000, 21.90000000000000213 ) ) ;
#33683 = CARTESIAN_POINT ( 'NONE',  ( 22.59999999999999432, 0.1000000000111554016, -155.8504291924551808 ) ) ;
#33684 = DIRECTION ( 'NONE',  ( -0.000000000000000000, -0.8700118002898321601, 0.4930308989875230030 ) ) ;
#33685 = SURFACE_SIDE_STYLE ('',( #153638 ) ) ;
#33686 = CARTESIAN_POINT ( 'NONE',  ( -22.50000000000000000, 0.09999999999999939493, 7.790779598373403836 ) ) ;
#33687 = CIRCLE ( 'NONE', #37756, 0.09999999999998802902 ) ;
#33688 = VERTEX_POINT ( 'NONE', #144704 ) ;
#33689 = DIRECTION ( 'NONE',  ( -3.265361837132813093E-16, -1.000000000000000000, 7.445645354460596589E-46 ) ) ;
#33690 = DIRECTION ( 'NONE',  ( -1.000000000000000000, 0.000000000000000000, 0.000000000000000000 ) ) ;
#33691 = AXIS2_PLACEMENT_3D ( 'NONE', #226338, #247202, #227637 ) ;
#33692 = ORIENTED_EDGE ( 'NONE', *, *, #90601, .F. ) ;
#33693 = CARTESIAN_POINT ( 'NONE',  ( 18.59999999999999432, 1.261786168576181755, -142.0864989635454947 ) ) ;
#33694 = CARTESIAN_POINT ( 'NONE',  ( 21.05000000000000071, 70.50000000001253397, -182.4283735034374843 ) ) ;
#33695 = AXIS2_PLACEMENT_3D ( 'NONE', #82446, #4211, #83720 ) ;
#33696 = ORIENTED_EDGE ( 'NONE', *, *, #191107, .F. ) ;
#33697 = DIRECTION ( 'NONE',  ( -1.000000000000000000, 0.000000000000000000, -0.000000000000000000 ) ) ;
#33698 = AXIS2_PLACEMENT_3D ( 'NONE', #28847, #249145, #193012 ) ;
#33699 = EDGE_LOOP ( 'NONE', ( #140606, #161783, #93399, #190021 ) ) ;
#33700 = CARTESIAN_POINT ( 'NONE',  ( 20.73486653747088937, 65.20902912466516455, -213.7034781834451280 ) ) ;
#33701 = DIRECTION ( 'NONE',  ( 1.000000000000000000, -0.000000000000000000, -0.000000000000000000 ) ) ;
#33702 = CARTESIAN_POINT ( 'NONE',  ( 21.06280952165527154, 10.62713230061232927, -112.7040538867790076 ) ) ;
#33703 = CARTESIAN_POINT ( 'NONE',  ( 18.59999999999999787, -10.74999999999999289, 33.00000000000000000 ) ) ;
#33704 = CARTESIAN_POINT ( 'NONE',  ( -20.64999999999999858, 21.30332930069722863, -233.2143729774842882 ) ) ;
#33705 = DIRECTION ( 'NONE',  ( 0.000000000000000000, 0.000000000000000000, 1.000000000000000000 ) ) ;
#33706 = CARTESIAN_POINT ( 'NONE',  ( -21.29999999999995808, 1.115600667400684642E-11, -33.50000000000000000 ) ) ;
#33708 = CARTESIAN_POINT ( 'NONE',  ( 23.04999999999999716, 10.58889512527366428, -208.1606840254082158 ) ) ;
#33707 = DIRECTION ( 'NONE',  ( 0.000000000000000000, 1.776356839400254803E-15, -1.000000000000000000 ) ) ;
#33709 = CARTESIAN_POINT ( 'NONE',  ( 20.09999999999999787, 66.25000000001233502, -160.7731074845244166 ) ) ;
#33710 = ADVANCED_FACE ( 'NONE', ( #125170 ), #65359, .T. ) ;
#33711 = DIRECTION ( 'NONE',  ( 1.000000000000000000, 0.000000000000000000, 0.000000000000000000 ) ) ;
#33712 = DIRECTION ( 'NONE',  ( 0.000000000000000000, 0.000000000000000000, 1.000000000000000000 ) ) ;
#33713 = AXIS2_PLACEMENT_3D ( 'NONE', #99104, #238645, #100385 ) ;
#33714 = EDGE_LOOP ( 'NONE', ( #77207, #232223, #201615, #93773 ) ) ;
#33715 = CARTESIAN_POINT ( 'NONE',  ( 21.15000000000005542, 77.36076146337680370, -43.99645795275012006 ) ) ;
#33716 = CIRCLE ( 'NONE', #233586, 0.09999999999999939493 ) ;
#33717 = CARTESIAN_POINT ( 'NONE',  ( 21.13461538461538680, 10.61458296203669427, -79.25000000000005684 ) ) ;
#33718 = DIRECTION ( 'NONE',  ( 0.000000000000000000, 1.000000000000000000, 0.000000000000000000 ) ) ;
#33719 = VECTOR ( 'NONE', #98133, 1000.000000000000000 ) ;
#33720 = AXIS2_PLACEMENT_3D ( 'NONE', #249157, #190478, #189168 ) ;
#33721 = DIRECTION ( 'NONE',  ( 0.000000000000000000, -7.124650136758317602E-15, 1.000000000000000000 ) ) ;
#33722 = LINE ( 'NONE', #91080, #116674 ) ;
#33724 = EDGE_CURVE ( 'NONE', #171424, #179646, #219467, .T. ) ;
#33723 = DIRECTION ( 'NONE',  ( 0.000000000000000000, -1.000000000000000000, 0.000000000000000000 ) ) ;
#33725 = CIRCLE ( 'NONE', #158592, 0.2000000000000005107 ) ;
#33726 = VECTOR ( 'NONE', #35967, 1000.000000000000000 ) ;
#33727 = VERTEX_POINT ( 'NONE', #26072 ) ;
#33728 = EDGE_CURVE ( 'NONE', #92979, #125420, #61267, .T. ) ;
#33729 = EDGE_CURVE ( 'NONE', #245148, #41808, #73767, .T. ) ;
#33730 = DIRECTION ( 'NONE',  ( 1.000000000000000000, 0.000000000000000000, 0.000000000000000000 ) ) ;
#33731 = ORIENTED_EDGE ( 'NONE', *, *, #166442, .F. ) ;
#33732 = CARTESIAN_POINT ( 'NONE',  ( 21.04999999999999716, 6.164532172064068227, -199.6789591974932421 ) ) ;
#33733 = DIRECTION ( 'NONE',  ( 0.000000000000000000, -0.9209589331071864615, 0.3896596508878908960 ) ) ;
#33734 = CIRCLE ( 'NONE', #50405, 7.800000000000001599 ) ;
#33735 = CIRCLE ( 'NONE', #212762, 0.09999999999998898659 ) ;
#33736 = VECTOR ( 'NONE', #193953, 1000.000000000000114 ) ;
#33737 = AXIS2_PLACEMENT_3D ( 'NONE', #111863, #209672, #11485 ) ;
#33738 = ORIENTED_EDGE ( 'NONE', *, *, #197806, .T. ) ;
#33739 = DIRECTION ( 'NONE',  ( 0.000000000000000000, 0.000000000000000000, -1.000000000000000000 ) ) ;
#33740 = EDGE_CURVE ( 'NONE', #72236, #36747, #185132, .T. ) ;
#33741 = ORIENTED_EDGE ( 'NONE', *, *, #27266, .F. ) ;
#33742 = DIRECTION ( 'NONE',  ( 0.000000000000000000, 0.000000000000000000, 1.000000000000000000 ) ) ;
#33743 = CARTESIAN_POINT ( 'NONE',  ( 21.06086055315979522, 67.22529248505583155, -124.3207853293703664 ) ) ;
#33744 = FACE_OUTER_BOUND ( 'NONE', #90965, .T. ) ;
#33745 = FACE_OUTER_BOUND ( 'NONE', #181305, .T. ) ;
#33746 = CARTESIAN_POINT ( 'NONE',  ( 18.59999999999999787, 72.06821323333463170, -225.0920403225231610 ) ) ;
#33747 = AXIS2_PLACEMENT_3D ( 'NONE', #248709, #32250, #34823 ) ;
#33748 = CARTESIAN_POINT ( 'NONE',  ( 20.12500000000000000, 10.82572568129133295, -207.2016591585088463 ) ) ;
#33749 = DIRECTION ( 'NONE',  ( 0.5000000000001141309, -6.047423072554455661E-15, 0.8660254037843729824 ) ) ;
#33750 = CARTESIAN_POINT ( 'NONE',  ( -18.50000000000000000, 7.021664781911246322, -204.8335654018972605 ) ) ;
#33752 = ORIENTED_EDGE ( 'NONE', *, *, #31219, .T. ) ;
#33751 = FACE_OUTER_BOUND ( 'NONE', #96376, .T. ) ;
#33754 = DIRECTION ( 'NONE',  ( 0.000000000000000000, -0.9651348961777379554, 0.2617529984164210233 ) ) ;
#33753 = CARTESIAN_POINT ( 'NONE',  ( -22.39999999999999858, 11.65000000001115588, -133.9000000000000057 ) ) ;
#33755 = ORIENTED_EDGE ( 'NONE', *, *, #192497, .T. ) ;
#33757 = ORIENTED_EDGE ( 'NONE', *, *, #192494, .T. ) ;
#33756 = CARTESIAN_POINT ( 'NONE',  ( 21.05000000000000071, -4.714262876194486473, -233.3440214805475819 ) ) ;
#33758 = ORIENTED_EDGE ( 'NONE', *, *, #198870, .T. ) ;
#33759 = CARTESIAN_POINT ( 'NONE',  ( -0.8999999999999437339, 67.75000000001118394, -10.02310748452479139 ) ) ;
#33760 = CARTESIAN_POINT ( 'NONE',  ( -18.59999999999999787, 74.25000000001205080, -124.8535959266226598 ) ) ;
#33761 = EDGE_CURVE ( 'NONE', #178394, #94509, #156968, .T. ) ;
#33763 = EDGE_CURVE ( 'NONE', #166897, #125226, #62625, .T. ) ;
#33762 = DIRECTION ( 'NONE',  ( 0.000000000000000000, 0.000000000000000000, 1.000000000000000000 ) ) ;
#33764 = DIRECTION ( 'NONE',  ( 0.000000000000000000, 0.000000000000000000, 1.000000000000000000 ) ) ;
#33765 = LINE ( 'NONE', #252745, #115071 ) ;
#33766 = CARTESIAN_POINT ( 'NONE',  ( 23.14999999999999858, 9.290509600414956992, -221.0404682250134840 ) ) ;
#33767 = AXIS2_PLACEMENT_3D ( 'NONE', #103987, #66174, #242230 ) ;
#33768 = EDGE_CURVE ( 'NONE', #53873, #140884, #163021, .T. ) ;
#33769 = CARTESIAN_POINT ( 'NONE',  ( -18.50000000000000000, 22.25400410509136151, -231.2278641261850680 ) ) ;
#33770 = VERTEX_POINT ( 'NONE', #170760 ) ;
#33771 = ORIENTED_EDGE ( 'NONE', *, *, #31753, .F. ) ;
#33772 = DIRECTION ( 'NONE',  ( -1.000000000000000000, -2.952720810173289112E-16, 0.000000000000000000 ) ) ;
#33773 = CIRCLE ( 'NONE', #196044, 0.1000000000000028644 ) ;
#33774 = ORIENTED_EDGE ( 'NONE', *, *, #165580, .F. ) ;
#33775 = DIRECTION ( 'NONE',  ( -1.000000000000000000, 0.000000000000000000, 0.000000000000000000 ) ) ;
#33776 = ORIENTED_EDGE ( 'NONE', *, *, #23556, .F. ) ;
#33777 = LINE ( 'NONE', #62275, #226534 ) ;
#33778 = AXIS2_PLACEMENT_3D ( 'NONE', #82924, #158680, #222436 ) ;
#33779 = DIRECTION ( 'NONE',  ( 0.000000000000000000, 0.000000000000000000, -1.000000000000000000 ) ) ;
#33780 = DIRECTION ( 'NONE',  ( -1.020425574104004394E-15, 0.9126074666063770380, 0.4088369013363281068 ) ) ;
#33781 = DIRECTION ( 'NONE',  ( 0.000000000000000000, -1.734723475976817507E-14, 1.000000000000000000 ) ) ;
#33782 = DIRECTION ( 'NONE',  ( 0.000000000000000000, -0.9908441862701605762, 0.1350103645451835310 ) ) ;
#33783 = VERTEX_POINT ( 'NONE', #187720 ) ;
#33784 = CARTESIAN_POINT ( 'NONE',  ( -18.43634282235129618, -9.679787199916868090, -207.6606518854537740 ) ) ;
#33785 = DIRECTION ( 'NONE',  ( 0.000000000000000000, 1.734723475976997999E-14, 1.000000000000000000 ) ) ;
#33786 = CARTESIAN_POINT ( 'NONE',  ( -18.59999999999999787, 76.00000000001190870, -103.0231074845243029 ) ) ;
#33787 = CARTESIAN_POINT ( 'NONE',  ( -20.94999999999999929, 7.128833340094563376, -233.7327013124401276 ) ) ;
#33788 = ORIENTED_EDGE ( 'NONE', *, *, #42579, .T. ) ;
#33791 = CYLINDRICAL_SURFACE ( 'NONE', #148234, 0.09999999999999939493 ) ;
#33790 = DIRECTION ( 'NONE',  ( 0.7071067811865474617, -0.7071067811865474617, -4.937700262164531476E-15 ) ) ;
#33789 = AXIS2_PLACEMENT_3D ( 'NONE', #175674, #253898, #72742 ) ;
#33792 = ORIENTED_EDGE ( 'NONE', *, *, #8998, .F. ) ;
#33795 = EDGE_LOOP ( 'NONE', ( #244366, #94069, #104533, #233535 ) ) ;
#33794 = CARTESIAN_POINT ( 'NONE',  ( 20.94999999999999929, -1.835859311432481045, -78.50443916879852679 ) ) ;
#33793 = CARTESIAN_POINT ( 'NONE',  ( -20.94999999999999929, 78.93126476241668854, -235.8702625865613243 ) ) ;
#33796 = CIRCLE ( 'NONE', #108755, 0.1000000000000106498 ) ;
#33797 = CARTESIAN_POINT ( 'NONE',  ( 18.49999999999999645, 74.36282728704222222, -191.9409541190523498 ) ) ;
#33798 = CIRCLE ( 'NONE', #246135, 0.9750000000000036415 ) ;
#33799 = EDGE_CURVE ( 'NONE', #3185, #163770, #152885, .T. ) ;
#33800 = CYLINDRICAL_SURFACE ( 'NONE', #54229, 0.09999999999998898659 ) ;
#33801 = ORIENTED_EDGE ( 'NONE', *, *, #3089, .F. ) ;
#33803 = EDGE_CURVE ( 'NONE', #41312, #17643, #31240, .T. ) ;
#33802 = DIRECTION ( 'NONE',  ( 0.000000000000000000, -1.000000000000000000, 0.000000000000000000 ) ) ;
#33804 = DIRECTION ( 'NONE',  ( 0.000000000000000000, 0.2617529984165083423, 0.9651348961777143076 ) ) ;
#33805 = EDGE_CURVE ( 'NONE', #204719, #194645, #52017, .T. ) ;
#33806 = DIRECTION ( 'NONE',  ( -1.000000000000000000, 0.000000000000000000, 0.000000000000000000 ) ) ;
#33807 = EDGE_CURVE ( 'NONE', #44944, #92704, #32251, .T. ) ;
#33809 = ORIENTED_EDGE ( 'NONE', *, *, #202714, .F. ) ;
#33808 = FACE_OUTER_BOUND ( 'NONE', #195247, .T. ) ;
#33810 = VECTOR ( 'NONE', #117788, 1000.000000000000000 ) ;
#33812 = ORIENTED_EDGE ( 'NONE', *, *, #200995, .T. ) ;
#33811 = EDGE_CURVE ( 'NONE', #126073, #143815, #190283, .T. ) ;
#33813 = SPHERICAL_SURFACE ( 'NONE', #245000, 0.1000000000000000056 ) ;
#33814 = DIRECTION ( 'NONE',  ( 0.000000000000000000, -0.4088369013363280513, 0.9126074666063769270 ) ) ;
#33815 = SPHERICAL_SURFACE ( 'NONE', #81240, 0.1000000000000000056 ) ;
#33816 = EDGE_CURVE ( 'NONE', #241398, #41988, #108174, .T. ) ;
#33817 = CYLINDRICAL_SURFACE ( 'NONE', #130162, 0.09999999999998898659 ) ;
#33820 = EDGE_CURVE ( 'NONE', #5530, #143771, #247673, .T. ) ;
#33819 = EDGE_CURVE ( 'NONE', #6556, #4734, #252981, .T. ) ;
#33818 = ORIENTED_EDGE ( 'NONE', *, *, #237325, .F. ) ;
#33821 = CARTESIAN_POINT ( 'NONE',  ( 11.60000000000006004, 67.75000000001118394, -21.02310748452479316 ) ) ;
#33822 = DIRECTION ( 'NONE',  ( 0.000000000000000000, 0.3427706569149635007, -0.9394191166662961834 ) ) ;
#33823 = FACE_OUTER_BOUND ( 'NONE', #174016, .T. ) ;
#33824 = ADVANCED_FACE ( 'NONE', ( #151154 ), #207283, .T. ) ;
#33825 = ORIENTED_EDGE ( 'NONE', *, *, #40825, .T. ) ;
#33826 = CARTESIAN_POINT ( 'NONE',  ( 20.22894356738840571, 60.44058279725945937, -225.4462117791892979 ) ) ;
#33827 = CARTESIAN_POINT ( 'NONE',  ( 21.05000000000000071, 5.850000000011105428, -144.1324972242779836 ) ) ;
#33828 = CIRCLE ( 'NONE', #87913, 0.5000000000000004441 ) ;
#33829 = ADVANCED_FACE ( 'NONE', ( #48180 ), #106863, .T. ) ;
#33830 = AXIS2_PLACEMENT_3D ( 'NONE', #34377, #70938, #112605 ) ;
#33831 = AXIS2_PLACEMENT_3D ( 'NONE', #248559, #84290, #28271 ) ;
#33832 = ORIENTED_EDGE ( 'NONE', *, *, #62428, .T. ) ;
#33833 = AXIS2_PLACEMENT_3D ( 'NONE', #204854, #132731, #243990 ) ;
#33834 = DIRECTION ( 'NONE',  ( 1.000000000000000000, 0.000000000000000000, 0.000000000000000000 ) ) ;
#33835 = CARTESIAN_POINT ( 'NONE',  ( 23.14999999999999858, 76.00000000001190870, -103.0231074845243029 ) ) ;
#33836 = ADVANCED_FACE ( 'NONE', ( #166890 ), #66470, .F. ) ;
#33837 = EDGE_CURVE ( 'NONE', #233025, #237894, #128094, .T. ) ;
#33838 = ORIENTED_EDGE ( 'NONE', *, *, #115932, .T. ) ;
#33839 = VERTEX_POINT ( 'NONE', #226821 ) ;
#33840 = ADVANCED_FACE ( 'NONE', ( #148581 ), #127737, .F. ) ;
#33841 = DIRECTION ( 'NONE',  ( 0.000000000000000000, 1.000000000000000000, 7.272083257015735086E-15 ) ) ;
#33842 = ORIENTED_EDGE ( 'NONE', *, *, #174455, .F. ) ;
#33844 = VERTEX_POINT ( 'NONE', #205977 ) ;
#33843 = DIRECTION ( 'NONE',  ( -0.000000000000000000, 1.000000000000000000, -0.000000000000000000 ) ) ;
#33845 = EDGE_CURVE ( 'NONE', #253894, #152504, #49473, .T. ) ;
#33846 = CIRCLE ( 'NONE', #154453, 0.09999999999999939493 ) ;
#33849 = ORIENTED_EDGE ( 'NONE', *, *, #99640, .F. ) ;
#33848 = ORIENTED_EDGE ( 'NONE', *, *, #170622, .F. ) ;
#33847 = CARTESIAN_POINT ( 'NONE',  ( -23.25000000000000000, -9.000000000000001776, -23.60603087734756045 ) ) ;
#33850 = ADVANCED_FACE ( 'NONE', ( #7789, #92432 ), #245106, .T. ) ;
#33851 = ORIENTED_EDGE ( 'NONE', *, *, #161028, .T. ) ;
#33852 = DIRECTION ( 'NONE',  ( 0.000000000000000000, -6.661338147750933721E-15, 1.000000000000000000 ) ) ;
#33853 = CARTESIAN_POINT ( 'NONE',  ( 21.05000000000000071, 10.72371710471867701, -112.6611902941274650 ) ) ;
#33854 = LINE ( 'NONE', #190329, #130615 ) ;
#33855 = CARTESIAN_POINT ( 'NONE',  ( 18.39999999999999503, 5.650000000011139001, -87.85000000000003695 ) ) ;
#33856 = DIRECTION ( 'NONE',  ( 0.000000000000000000, 0.8814952561688438326, -0.4721928772777330696 ) ) ;
#33857 = ORIENTED_EDGE ( 'NONE', *, *, #153492, .F. ) ;
#33858 = ORIENTED_EDGE ( 'NONE', *, *, #102321, .T. ) ;
#33859 = ORIENTED_EDGE ( 'NONE', *, *, #203904, .T. ) ;
#33860 = CARTESIAN_POINT ( 'NONE',  ( -40.23850191057533010, 87.75000000001122658, -30.02310748452481448 ) ) ;
#33862 = ORIENTED_EDGE ( 'NONE', *, *, #83477, .T. ) ;
#33861 = FACE_OUTER_BOUND ( 'NONE', #228291, .T. ) ;
#33863 = DIRECTION ( 'NONE',  ( -0.7071067811865474617, -0.7071067811865474617, -2.044391222244499837E-16 ) ) ;
#33864 = EDGE_LOOP ( 'NONE', ( #6150, #126818, #164840, #152487 ) ) ;
#33865 = EDGE_CURVE ( 'NONE', #4626, #87766, #107237, .T. ) ;
#33866 = CIRCLE ( 'NONE', #100428, 11.79999999999999538 ) ;
#33867 = ORIENTED_EDGE ( 'NONE', *, *, #194371, .T. ) ;
#33868 = CARTESIAN_POINT ( 'NONE',  ( -18.49513951962167724, -0.6503453050635661370, -242.3638832198185469 ) ) ;
#33869 = AXIS2_PLACEMENT_3D ( 'NONE', #217044, #197494, #141375 ) ;
#33870 = ORIENTED_EDGE ( 'NONE', *, *, #155725, .F. ) ;
#33872 = TOROIDAL_SURFACE ( 'NONE', #150539, 4.900000000000003020, 0.1000000000000000056 ) ;
#33871 = DIRECTION ( 'NONE',  ( 2.952720810173287633E-16, -0.9770955615653312831, -0.2128009952263610616 ) ) ;
#33873 = DIRECTION ( 'NONE',  ( -1.000000000000000000, -0.000000000000000000, 0.000000000000000000 ) ) ;
#33874 = B_SPLINE_CURVE_WITH_KNOTS ( 'NONE', 3,
 ( #49187, #10064, #89585, #248679, #90880, #50447, #132587, #149601, #154738, #114297, #135127, #214674, #189991, #253792, #72629, #230396, #36063, #229116, #232987, #51731, #93440, #193847, #15217, #249962, #94729, #231699, #170478, #173038, #33528, #152173 ),
 .UNSPECIFIED., .F., .F.,
 ( 4, 2, 2, 2, 2, 2, 2, 2, 2, 2, 2, 2, 2, 2, 4 ),
 ( 0.000000000000000000, 0.0003422764154113348617, 0.0006845528308226697233, 0.001026829246234006428, 0.001369105661645343350, 0.002053658492468013290, 0.002738211323290683664, 0.003080487738702016465, 0.003422764154113348400, 0.003765040569524680768, 0.004107316984936013569, 0.004449593400347345504, 0.004791869815758678305, 0.005134146231170010240, 0.005476422646581343041 ),
 .UNSPECIFIED. ) ;
#33876 = ORIENTED_EDGE ( 'NONE', *, *, #141858, .T. ) ;
#33875 = ORIENTED_EDGE ( 'NONE', *, *, #25936, .T. ) ;
#33877 = ORIENTED_EDGE ( 'NONE', *, *, #169884, .T. ) ;
#33879 = DIRECTION ( 'NONE',  ( -1.000000000000000000, -0.000000000000000000, -0.000000000000000000 ) ) ;
#33878 = CIRCLE ( 'NONE', #150370, 0.09999999999999939493 ) ;
#33880 = EDGE_LOOP ( 'NONE', ( #80884, #183811, #94453, #239212, #128418, #86979, #158219, #94411, #18718, #178150, #143311, #143260, #221612, #21509, #155570, #159359, #171116, #135735, #155681, #249851, #31938, #203133, #253153 ) ) ;
#33881 = VERTEX_POINT ( 'NONE', #38907 ) ;
#33882 = DIRECTION ( 'NONE',  ( -1.000000000000000000, -0.000000000000000000, 0.000000000000000000 ) ) ;
#33883 = AXIS2_PLACEMENT_3D ( 'NONE', #216412, #37806, #117320 ) ;
#33885 = EDGE_LOOP ( 'NONE', ( #190313, #80038, #7615, #186101 ) ) ;
#33884 = FACE_OUTER_BOUND ( 'NONE', #217868, .T. ) ;
#33886 = PLANE ( 'NONE',  #160873 ) ;
#33888 = CARTESIAN_POINT ( 'NONE',  ( 21.97500000000000497, 9.750000000011153745, -112.8500000000000369 ) ) ;
#33887 = DIRECTION ( 'NONE',  ( -1.000000000000000000, 0.000000000000000000, 0.000000000000000000 ) ) ;
#33889 = FACE_OUTER_BOUND ( 'NONE', #58647, .T. ) ;
#33890 = DIRECTION ( 'NONE',  ( 0.000000000000000000, 0.2617529984165034018, 0.9651348961777157509 ) ) ;
#33891 = CARTESIAN_POINT ( 'NONE',  ( 22.01447462590973814, 29.98943614194342189, -252.4304903617178297 ) ) ;
#33892 = ORIENTED_EDGE ( 'NONE', *, *, #251385, .T. ) ;
#33893 = CIRCLE ( 'NONE', #130074, 0.3999999999999926392 ) ;
#33894 = ORIENTED_EDGE ( 'NONE', *, *, #189924, .F. ) ;
#33895 = DIRECTION ( 'NONE',  ( 1.000000000000000000, 0.000000000000000000, 0.000000000000000000 ) ) ;
#33896 = LINE ( 'NONE', #113386, #143354 ) ;
#33898 = EDGE_CURVE ( 'NONE', #34950, #121961, #211298, .T. ) ;
#33897 = CARTESIAN_POINT ( 'NONE',  ( -18.34374000495059676, 64.52683809664901560, -45.27310748452439526 ) ) ;
#33900 = VERTEX_POINT ( 'NONE', #174614 ) ;
#33899 = VECTOR ( 'NONE', #82105, 1000.000000000000227 ) ;
#33901 = FACE_OUTER_BOUND ( 'NONE', #123526, .T. ) ;
#33902 = ADVANCED_FACE ( 'NONE', ( #117152 ), #255315, .F. ) ;
#33903 = CIRCLE ( 'NONE', #204701, 11.74999999999999645 ) ;
#33904 = CARTESIAN_POINT ( 'NONE',  ( 21.97500000000000497, 66.25000000001186606, -90.77310748452438816 ) ) ;
#33905 = DIRECTION ( 'NONE',  ( -1.000000000000000000, 0.000000000000000000, 0.000000000000000000 ) ) ;
#33906 = VERTEX_POINT ( 'NONE', #216227 ) ;
#33907 = ORIENTED_EDGE ( 'NONE', *, *, #37688, .T. ) ;
#33908 = AXIS2_PLACEMENT_3D ( 'NONE', #169858, #34186, #214070 ) ;
#33909 = ADVANCED_FACE ( 'NONE', ( #177147 ), #15697, .T. ) ;
#33910 = DIRECTION ( 'NONE',  ( 1.000000000000000000, 0.000000000000000000, -0.000000000000000000 ) ) ;
#33912 = ADVANCED_FACE ( 'NONE', ( #235798 ), #252789, .T. ) ;
#33911 = DIRECTION ( 'NONE',  ( -1.000000000000000000, 0.000000000000000000, 0.000000000000000000 ) ) ;
#33913 = ORIENTED_EDGE ( 'NONE', *, *, #143408, .F. ) ;
#33914 = CARTESIAN_POINT ( 'NONE',  ( -18.49499033040907037, -9.438148771733517961, -174.6981532259234200 ) ) ;
#33915 = VERTEX_POINT ( 'NONE', #113293 ) ;
#33916 = CARTESIAN_POINT ( 'NONE',  ( 18.36493879433272625, -9.500000806178645618, -140.9221486603523488 ) ) ;
#33917 = AXIS2_PLACEMENT_3D ( 'NONE', #81462, #181890, #138861 ) ;
#33919 = CARTESIAN_POINT ( 'NONE',  ( 18.59999999999999432, 44.52640028187936849, -247.3006740988509193 ) ) ;
#33918 = DIRECTION ( 'NONE',  ( -1.000000000000000000, 0.000000000000000000, 0.000000000000000000 ) ) ;
#33920 = CARTESIAN_POINT ( 'NONE',  ( -18.59999999999999787, 6.982009704867601307, -70.69615211825629331 ) ) ;
#33921 = DIRECTION ( 'NONE',  ( 1.000000000000000000, -0.000000000000000000, -0.000000000000000000 ) ) ;
#33922 = FACE_OUTER_BOUND ( 'NONE', #81662, .T. ) ;
#33924 = EDGE_LOOP ( 'NONE', ( #228874, #149607, #141171, #49926 ) ) ;
#33923 = DIRECTION ( 'NONE',  ( 1.000000000000000000, -0.000000000000000000, -0.000000000000000000 ) ) ;
#33925 = VECTOR ( 'NONE', #225444, 1000.000000000000227 ) ;
#33926 = STYLED_ITEM ( 'NONE', ( #85986 ), #24390 ) ;
#33927 = CIRCLE ( 'NONE', #17142, 0.09999999999999939493 ) ;
#33928 = AXIS2_PLACEMENT_3D ( 'NONE', #247572, #149783, #230591 ) ;
#33929 = ADVANCED_FACE ( 'NONE', ( #72920 ), #114583, .T. ) ;
#33931 = ORIENTED_EDGE ( 'NONE', *, *, #136023, .F. ) ;
#33930 = VERTEX_POINT ( 'NONE', #37629 ) ;
#33932 = ORIENTED_EDGE ( 'NONE', *, *, #126028, .T. ) ;
#33933 = AXIS2_PLACEMENT_3D ( 'NONE', #7409, #206908, #128667 ) ;
#33934 = DIRECTION ( 'NONE',  ( 0.000000000000000000, -1.000000000000000000, 0.000000000000000000 ) ) ;
#33935 = CARTESIAN_POINT ( 'NONE',  ( 22.40736611211992368, 0.000000000000000000, 11.64957080754479968 ) ) ;
#33936 = CARTESIAN_POINT ( 'NONE',  ( 20.94999999999999929, 85.00000000001179501, -78.91707660717668205 ) ) ;
#33938 = DIRECTION ( 'NONE',  ( 0.000000000000000000, 0.8660254037844377084, 0.5000000000000016653 ) ) ;
#33937 = CARTESIAN_POINT ( 'NONE',  ( -16.78493211734303614, 66.05416425680837733, -182.6870565036285257 ) ) ;
#33939 = VERTEX_POINT ( 'NONE', #152452 ) ;
#33940 = CARTESIAN_POINT ( 'NONE',  ( 23.14999999999999858, 78.10000000001171827, -69.52310748452430289 ) ) ;
#33941 = EDGE_LOOP ( 'NONE', ( #210489, #145709, #139073, #158829 ) ) ;
#33942 = EDGE_LOOP ( 'NONE', ( #188891, #34792, #94287, #26490 ) ) ;
#33943 = DIRECTION ( 'NONE',  ( -0.000000000000000000, -0.000000000000000000, 1.000000000000000000 ) ) ;
#33944 = DIRECTION ( 'NONE',  ( 0.000000000000000000, 0.000000000000000000, -1.000000000000000000 ) ) ;
#33945 = CARTESIAN_POINT ( 'NONE',  ( 22.47007471830798053, 76.00000000001274714, -211.2438181364508125 ) ) ;
#33946 = ADVANCED_FACE ( 'NONE', ( #212416 ), #157600, .T. ) ;
#33947 = DIRECTION ( 'NONE',  ( 1.000000000000000000, 0.000000000000000000, 0.000000000000000000 ) ) ;
#33948 = DIRECTION ( 'NONE',  ( -1.000000000000000000, 0.000000000000000000, 0.000000000000000000 ) ) ;
#33949 = ORIENTED_EDGE ( 'NONE', *, *, #12259, .T. ) ;
#33950 = ORIENTED_EDGE ( 'NONE', *, *, #66202, .F. ) ;
#33951 = CARTESIAN_POINT ( 'NONE',  ( 23.24999999999997513, 11.65000000001116298, -93.48519422934610645 ) ) ;
#33952 = CARTESIAN_POINT ( 'NONE',  ( 19.97071067811866385, 62.38675221621814870, -208.9400838588616693 ) ) ;
#33953 = DIRECTION ( 'NONE',  ( 0.000000000000000000, -7.056502275159890832E-15, 1.000000000000000000 ) ) ;
#33954 = CARTESIAN_POINT ( 'NONE',  ( 20.94999999999999929, 49.36776662947724503, -253.7196102226803021 ) ) ;
#33955 = DIRECTION ( 'NONE',  ( 0.000000000000000000, -1.000000000000000000, 0.000000000000000000 ) ) ;
#33957 = ADVANCED_FACE ( 'NONE', ( #231982 ), #182263, .T. ) ;
#33956 = DIRECTION ( 'NONE',  ( -1.073024830501117725E-15, 6.982962677686266711E-15, -1.000000000000000000 ) ) ;
#33958 = AXIS2_PLACEMENT_3D ( 'NONE', #162418, #106255, #101085 ) ;
#33959 = DIRECTION ( 'NONE',  ( 3.265361837132813093E-16, -1.000000000000000000, -0.000000000000000000 ) ) ;
#33961 = DIRECTION ( 'NONE',  ( 0.000000000000000000, 1.000000000000000000, 0.000000000000000000 ) ) ;
#33960 = DIRECTION ( 'NONE',  ( 0.000000000000000000, 1.000000000000000000, 6.982962677686266711E-15 ) ) ;
#33962 = PLANE ( 'NONE',  #141495 ) ;
#33963 = EDGE_CURVE ( 'NONE', #82676, #236070, #24059, .T. ) ;
#33964 = CARTESIAN_POINT ( 'NONE',  ( -14.00000000000000178, 13.18880795147152440, -215.2702608532411830 ) ) ;
#33965 = CARTESIAN_POINT ( 'NONE',  ( -20.12071067811865888, 11.73531732528137006, -211.0836736768127366 ) ) ;
#33966 = CARTESIAN_POINT ( 'NONE',  ( 20.92356734117541706, 10.31973158071402175, -139.5505334713354841 ) ) ;
#33968 = ORIENTED_EDGE ( 'NONE', *, *, #225089, .T. ) ;
#33967 = FACE_OUTER_BOUND ( 'NONE', #236206, .T. ) ;
#33969 = EDGE_CURVE ( 'NONE', #217985, #68121, #132874, .T. ) ;
#33970 = AXIS2_PLACEMENT_3D ( 'NONE', #82612, #117911, #100881 ) ;
#33971 = EDGE_CURVE ( 'NONE', #174834, #116521, #95007, .T. ) ;
#33972 = EDGE_CURVE ( 'NONE', #230960, #161116, #140543, .T. ) ;
#33973 = DIRECTION ( 'NONE',  ( 0.000000000000000000, -0.2128009952263604232, 0.9770955615653316162 ) ) ;
#33974 = CARTESIAN_POINT ( 'NONE',  ( 22.49436431346199683, 11.64995094766461392, -100.4330964702777749 ) ) ;
#33975 = ADVANCED_FACE ( 'NONE', ( #134123 ), #165516, .T. ) ;
#33976 = DIRECTION ( 'NONE',  ( 1.000000000000000000, 0.000000000000000000, 0.000000000000000000 ) ) ;
#33977 = DIRECTION ( 'NONE',  ( 0.000000000000000000, 0.8814952561688449428, -0.4721928772777310157 ) ) ;
#33978 = VECTOR ( 'NONE', #227248, 1000.000000000000000 ) ;
#33979 = CARTESIAN_POINT ( 'NONE',  ( 21.14999999999999503, -0.1008583690987122083, 11.74956712348939192 ) ) ;
#33980 = FACE_OUTER_BOUND ( 'NONE', #83384, .T. ) ;
#33982 = CARTESIAN_POINT ( 'NONE',  ( 21.04999999999998650, 69.35000000001205933, -124.2731074845243455 ) ) ;
#33981 = AXIS2_PLACEMENT_3D ( 'NONE', #116094, #75691, #56081 ) ;
#33983 = ORIENTED_EDGE ( 'NONE', *, *, #63256, .F. ) ;
#33984 = DIRECTION ( 'NONE',  ( 0.000000000000000000, -0.2617529984165152257, -0.9651348961777124202 ) ) ;
#33986 = ORIENTED_EDGE ( 'NONE', *, *, #82310, .F. ) ;
#33985 = LINE ( 'NONE', #73104, #184224 ) ;
#33987 = CYLINDRICAL_SURFACE ( 'NONE', #88135, 0.1000000000000026007 ) ;
#33988 = ADVANCED_FACE ( 'NONE', ( #35084 ), #75482, .F. ) ;
#33989 = CARTESIAN_POINT ( 'NONE',  ( -20.15000000000000568, 66.70857864377455826, -90.67310748452436542 ) ) ;
#33990 = EDGE_LOOP ( 'NONE', ( #46067, #14337, #73615, #87738 ) ) ;
#33991 = CARTESIAN_POINT ( 'NONE',  ( -20.94999999999999929, 13.59055429284667404, -238.6121134008722038 ) ) ;
#33992 = DIRECTION ( 'NONE',  ( -2.840903330521632269E-16, -0.8700118002898356018, 0.4930308989875170078 ) ) ;
#33993 = DIRECTION ( 'NONE',  ( 0.000000000000000000, 0.000000000000000000, -1.000000000000000000 ) ) ;
#33994 = AXIS2_PLACEMENT_3D ( 'NONE', #63793, #247563, #85888 ) ;
#33995 = ORIENTED_EDGE ( 'NONE', *, *, #8288, .T. ) ;
#33996 = FACE_OUTER_BOUND ( 'NONE', #23469, .T. ) ;
#33997 = DIRECTION ( 'NONE',  ( 0.000000000000000000, 0.8814952561688430555, -0.4721928772777346239 ) ) ;
#33998 = DIRECTION ( 'NONE',  ( 0.000000000000000000, 0.000000000000000000, 1.000000000000000000 ) ) ;
#33999 = EDGE_LOOP ( 'NONE', ( #78478, #174350, #90700, #118689 ) ) ;
#34000 = ORIENTED_EDGE ( 'NONE', *, *, #17355, .F. ) ;
#34001 = CARTESIAN_POINT ( 'NONE',  ( 23.14999999999999147, 0.000000000000000000, 0.000000000000000000 ) ) ;
#34002 = CARTESIAN_POINT ( 'NONE',  ( 20.84999999999998721, 10.33248238083634440, -173.0948465439131496 ) ) ;
#34003 = CARTESIAN_POINT ( 'NONE',  ( -20.94999999999999929, -1.835341550213255957, -45.05515129256298223 ) ) ;
#34005 = CARTESIAN_POINT ( 'NONE',  ( -20.05000000000000426, 66.75000000001253397, -182.3731074845244393 ) ) ;
#34004 = AXIS2_PLACEMENT_3D ( 'NONE', #49747, #90136, #129292 ) ;
#34006 = VECTOR ( 'NONE', #187275, 1000.000000000000114 ) ;
#34009 = CARTESIAN_POINT ( 'NONE',  ( 21.14999999999999858, 64.35000000001228670, -157.8731074845244393 ) ) ;
#34008 = VECTOR ( 'NONE', #202948, 1000.000000000000114 ) ;
#34007 = CARTESIAN_POINT ( 'NONE',  ( -20.54999999999999716, -8.730841121484173684, -110.0980747189843640 ) ) ;
#34010 = CARTESIAN_POINT ( 'NONE',  ( -20.94999999999999929, 77.16412189325286874, -61.80825939895269272 ) ) ;
#34011 = DIRECTION ( 'NONE',  ( -0.000000000000000000, 1.000000000000000000, -0.000000000000000000 ) ) ;
#34012 = FACE_OUTER_BOUND ( 'NONE', #15344, .T. ) ;
#34013 = CARTESIAN_POINT ( 'NONE',  ( -18.50000000000000355, 47.16152503674115337, -255.1462838189583806 ) ) ;
#34014 = ORIENTED_EDGE ( 'NONE', *, *, #22940, .T. ) ;
#34015 = EDGE_CURVE ( 'NONE', #70035, #238178, #153079, .T. ) ;
#34017 = ORIENTED_EDGE ( 'NONE', *, *, #153335, .T. ) ;
#34016 = CARTESIAN_POINT ( 'NONE',  ( 20.94999999999999574, -1.360870587192041681, -8.072997927090961312 ) ) ;
#34018 = CARTESIAN_POINT ( 'NONE',  ( -18.59999999999999787, 64.35000000001276987, -215.2731074845244450 ) ) ;
#34019 = DIRECTION ( 'NONE',  ( 1.000000000000000000, 0.000000000000000000, 0.000000000000000000 ) ) ;
#34021 = CARTESIAN_POINT ( 'NONE',  ( -18.40000000000000213, 43.42149616655404287, -233.9497663708821165 ) ) ;
#34020 = CARTESIAN_POINT ( 'NONE',  ( 21.12757541349815682, 69.52661942876019907, -69.52826870033410955 ) ) ;
#34022 = ORIENTED_EDGE ( 'NONE', *, *, #87534, .T. ) ;
#34023 = CARTESIAN_POINT ( 'NONE',  ( 20.94999999999999574, 18.52348994230296242, -223.9544021632493127 ) ) ;
#34024 = DIRECTION ( 'NONE',  ( -1.000000000000000000, -0.000000000000000000, 0.000000000000000000 ) ) ;
#34025 = CARTESIAN_POINT ( 'NONE',  ( -21.04999999999880345, 69.50298221357996908, -103.0085617939544562 ) ) ;
#34027 = EDGE_CURVE ( 'NONE', #81561, #184336, #139244, .T. ) ;
#34026 = CARTESIAN_POINT ( 'NONE',  ( 21.72449340488909897, 65.71604372252087956, -115.6731074845243796 ) ) ;
#34028 = ORIENTED_EDGE ( 'NONE', *, *, #85426, .F. ) ;
#34030 = ORIENTED_EDGE ( 'NONE', *, *, #222061, .T. ) ;
#34029 = AXIS2_PLACEMENT_3D ( 'NONE', #243704, #50619, #65065 ) ;
#34031 = ADVANCED_FACE ( 'NONE', ( #100117 ), #20630, .T. ) ;
#34032 = ADVANCED_FACE ( 'NONE', ( #24487 ), #79278, .F. ) ;
#34033 = DIRECTION ( 'NONE',  ( 0.000000000000000000, 0.2617529984165024026, 0.9651348961777158619 ) ) ;
#34034 = VERTEX_POINT ( 'NONE', #121027 ) ;
#34035 = DIRECTION ( 'NONE',  ( 0.000000000000000000, 0.000000000000000000, -1.000000000000000000 ) ) ;
#34036 = DIRECTION ( 'NONE',  ( 2.952720810173289112E-16, -1.000000000000000000, -0.000000000000000000 ) ) ;
#34037 = CARTESIAN_POINT ( 'NONE',  ( -21.08376601933334271, 65.50969838531518974, -241.9592675656176937 ) ) ;
#34038 = ORIENTED_EDGE ( 'NONE', *, *, #65832, .T. ) ;
#34039 = DIRECTION ( 'NONE',  ( -1.000000000000000000, 7.304098846218164250E-16, -4.217023435051628197E-16 ) ) ;
#34040 = ADVANCED_FACE ( 'NONE', ( #221353 ), #23203, .T. ) ;
#34041 = CIRCLE ( 'NONE', #13163, 11.75000000000000000 ) ;
#34042 = DIRECTION ( 'NONE',  ( 0.000000000000000000, 0.9651348961777157509, -0.2617529984165031243 ) ) ;
#34043 = CARTESIAN_POINT ( 'NONE',  ( 21.05000000000000426, -0.01681986837451829309, -27.19257478043459386 ) ) ;
#34044 = CARTESIAN_POINT ( 'NONE',  ( 21.05000000000000071, 1.115600667400684642E-11, -102.4000000000000483 ) ) ;
#34045 = FACE_OUTER_BOUND ( 'NONE', #115222, .T. ) ;
#34047 = CARTESIAN_POINT ( 'NONE',  ( 19.75857864376268935, 64.35000000001177511, -78.17310748452437963 ) ) ;
#34046 = LINE ( 'NONE', #251769, #108135 ) ;
#34049 = DIRECTION ( 'NONE',  ( -0.000000000000000000, -1.000000000000000000, -5.421010862427649374E-16 ) ) ;
#34048 = AXIS2_PLACEMENT_3D ( 'NONE', #185333, #6686, #86198 ) ;
#34050 = ORIENTED_EDGE ( 'NONE', *, *, #216960, .F. ) ;
#34052 = LINE ( 'NONE', #251775, #180841 ) ;
#34051 = CARTESIAN_POINT ( 'NONE',  ( 18.59999999999998366, 36.65892442174935439, -249.5511627012433848 ) ) ;
#34053 = ORIENTED_EDGE ( 'NONE', *, *, #86983, .T. ) ;
#34055 = EDGE_LOOP ( 'NONE', ( #185725, #255830, #227092, #8128 ) ) ;
#34054 = DIRECTION ( 'NONE',  ( 0.000000000000000000, 1.000000000000000000, -1.387778780781444413E-14 ) ) ;
#34056 = ORIENTED_EDGE ( 'NONE', *, *, #244234, .T. ) ;
#34057 = AXIS2_PLACEMENT_3D ( 'NONE', #5357, #150060, #84882 ) ;
#34058 = CARTESIAN_POINT ( 'NONE',  ( 13.43663047529820176, 66.55335465531702255, -151.6123010284242412 ) ) ;
#34059 = CARTESIAN_POINT ( 'NONE',  ( -20.94999999999999929, 76.00000000001149658, -47.82310748452432136 ) ) ;
#34060 = DIRECTION ( 'NONE',  ( -1.000000000000000000, -1.794895427898103559E-16, -3.909090864890002444E-17 ) ) ;
#34061 = AXIS2_PLACEMENT_3D ( 'NONE', #175727, #216097, #79146 ) ;
#34062 = VERTEX_POINT ( 'NONE', #161426 ) ;
#34063 = EDGE_CURVE ( 'NONE', #104591, #149704, #214836, .T. ) ;
#34064 = EDGE_CURVE ( 'NONE', #85452, #242283, #161427, .T. ) ;
#34065 = FACE_OUTER_BOUND ( 'NONE', #32649, .T. ) ;
#34066 = FACE_OUTER_BOUND ( 'NONE', #142176, .T. ) ;
#34067 = ORIENTED_EDGE ( 'NONE', *, *, #154904, .T. ) ;
#34068 = AXIS2_PLACEMENT_3D ( 'NONE', #96994, #98277, #17493 ) ;
#34069 = DIRECTION ( 'NONE',  ( 0.000000000000000000, -0.8149014228131966631, 0.5795995782408988051 ) ) ;
#34070 = CIRCLE ( 'NONE', #159141, 0.1000000000000106914 ) ;
#34071 = EDGE_CURVE ( 'NONE', #219189, #257964, #200528, .T. ) ;
#34072 = DIRECTION ( 'NONE',  ( 0.000000000000000000, -0.1495327102803283015, 0.9887567792719397231 ) ) ;
#34073 = CIRCLE ( 'NONE', #154675, 11.74999999999999645 ) ;
#34074 = VERTEX_POINT ( 'NONE', #182262 ) ;
#34075 = DIRECTION ( 'NONE',  ( -1.000000000000000000, -0.000000000000000000, -0.000000000000000000 ) ) ;
#34076 = CIRCLE ( 'NONE', #71647, 0.1000000000000035444 ) ;
#34077 = ORIENTED_EDGE ( 'NONE', *, *, #246609, .F. ) ;
#34078 = CARTESIAN_POINT ( 'NONE',  ( 18.44364597020195617, -9.490487317151101720, -141.0579778896838832 ) ) ;
#34079 = VERTEX_POINT ( 'NONE', #183543 ) ;
#34080 = CARTESIAN_POINT ( 'NONE',  ( -20.85000000000000142, 10.33248238083635151, -173.0948465439131780 ) ) ;
#34081 = CIRCLE ( 'NONE', #179799, 0.09999999999999939493 ) ;
#34082 = DIRECTION ( 'NONE',  ( -0.000000000000000000, -0.000000000000000000, 1.000000000000000000 ) ) ;
#34083 = CARTESIAN_POINT ( 'NONE',  ( 21.93642651522410603, 68.67283376068688483, -203.5231074845243882 ) ) ;
#34084 = AXIS2_PLACEMENT_3D ( 'NONE', #37608, #117132, #233253 ) ;
#34085 = CARTESIAN_POINT ( 'NONE',  ( 18.49999999999999289, 10.20857864377384239, -58.26715728752538581 ) ) ;
#34086 = ADVANCED_FACE ( 'NONE', ( #239662 ), #111344, .F. ) ;
#34087 = DIRECTION ( 'NONE',  ( -1.000000000000000000, 0.000000000000000000, 0.000000000000000000 ) ) ;
#34088 = CARTESIAN_POINT ( 'NONE',  ( -21.05000000000000071, -1.162701749926853712, -108.4000000000000341 ) ) ;
#34089 = DIRECTION ( 'NONE',  ( 1.000000000000000000, 0.000000000000000000, -0.000000000000000000 ) ) ;
#34090 = AXIS2_PLACEMENT_3D ( 'NONE', #241200, #99073, #116112 ) ;
#34091 = EDGE_LOOP ( 'NONE', ( #122930, #15331, #204713, #124877 ) ) ;
#34093 = CARTESIAN_POINT ( 'NONE',  ( 23.14999999999999858, 70.50000000001180922, -81.92837350343744163 ) ) ;
#34092 = CARTESIAN_POINT ( 'NONE',  ( 21.13461538461538680, 23.02743022372037274, -230.2075788195831478 ) ) ;
#34094 = EDGE_LOOP ( 'NONE', ( #189104, #45388, #173974, #184437 ) ) ;
#34097 = ORIENTED_EDGE ( 'NONE', *, *, #15219, .T. ) ;
#34096 = CARTESIAN_POINT ( 'NONE',  ( 20.94999999999999929, 6.650000000011155876, -45.65000000000000568 ) ) ;
#34095 = DIRECTION ( 'NONE',  ( 0.000000000000000000, -0.9770955615653320603, -0.2128009952263585081 ) ) ;
#34098 = CIRCLE ( 'NONE', #154889, 0.1999999999999987899 ) ;
#34099 = ORIENTED_EDGE ( 'NONE', *, *, #78032, .T. ) ;
#34100 = DIRECTION ( 'NONE',  ( -1.000000000000000000, 0.000000000000000000, 0.000000000000000000 ) ) ;
#34101 = CIRCLE ( 'NONE', #100661, 12.77500000000000391 ) ;
#34102 = CARTESIAN_POINT ( 'NONE',  ( -21.08479644141223019, 6.345038657731887355, 0.05855444256413715881 ) ) ;
#34103 = DIRECTION ( 'NONE',  ( 1.000000000000000000, 0.000000000000000000, -0.000000000000000000 ) ) ;
#34104 = EDGE_CURVE ( 'NONE', #206061, #212047, #69850, .T. ) ;
#34105 = CARTESIAN_POINT ( 'NONE',  ( 20.95566103547454517, 58.98089026282059422, -225.7100130536167342 ) ) ;
#34106 = EDGE_LOOP ( 'NONE', ( #160542, #166684, #136393, #80693 ) ) ;
#34108 = EDGE_LOOP ( 'NONE', ( #53454, #245602, #63984, #85470 ) ) ;
#34107 = CARTESIAN_POINT ( 'NONE',  ( 20.94999999999999929, 38.33376540847015690, -250.4483291680710693 ) ) ;
#34109 = EDGE_CURVE ( 'NONE', #122601, #76430, #215565, .T. ) ;
#34111 = CARTESIAN_POINT ( 'NONE',  ( 18.49999999999999289, 15.40600705476365029, -222.9910675435765199 ) ) ;
#34110 = CYLINDRICAL_SURFACE ( 'NONE', #34602, 0.1000000000000028644 ) ;
#34112 = ADVANCED_FACE ( 'NONE', ( #101374 ), #180976, .T. ) ;
#34114 = VERTEX_POINT ( 'NONE', #83106 ) ;
#34113 = CARTESIAN_POINT ( 'NONE',  ( -16.94389599337535657, 9.991197989767881538, -54.39235519820161358 ) ) ;
#34115 = ORIENTED_EDGE ( 'NONE', *, *, #53062, .T. ) ;
#34116 = AXIS2_PLACEMENT_3D ( 'NONE', #203540, #5300, #21079 ) ;
#34118 = ADVANCED_FACE ( 'NONE', ( #162700 ), #169141, .T. ) ;
#34117 = CARTESIAN_POINT ( 'NONE',  ( -20.90000000000000213, 11.49641995933507843, -1.885425182446133885 ) ) ;
#34119 = CARTESIAN_POINT ( 'NONE',  ( 21.05000000000000071, 67.12872031401624895, -94.46447848938342418 ) ) ;
#34121 = EDGE_CURVE ( 'NONE', #86058, #194468, #230351, .T. ) ;
#34120 = ORIENTED_EDGE ( 'NONE', *, *, #246368, .F. ) ;
#34122 = CARTESIAN_POINT ( 'NONE',  ( -18.39999999999999858, 85.40000000001246860, -181.7731074845243029 ) ) ;
#34123 = ORIENTED_EDGE ( 'NONE', *, *, #189256, .F. ) ;
#34124 = CARTESIAN_POINT ( 'NONE',  ( -18.36973785203556275, 11.47550320049537476, -158.2500000000000284 ) ) ;
#34125 = DIRECTION ( 'NONE',  ( 0.000000000000000000, -1.000000000000000000, 0.000000000000000000 ) ) ;
#34126 = ORIENTED_EDGE ( 'NONE', *, *, #165055, .F. ) ;
#34127 = DIRECTION ( 'NONE',  ( 2.342056488767300981E-15, 0.07893460099012014619, -0.9968797965484758050 ) ) ;
#34128 = EDGE_CURVE ( 'NONE', #240571, #78383, #7274, .T. ) ;
#34129 = CARTESIAN_POINT ( 'NONE',  ( -23.15000000000000213, -11.39257802169451139, -197.9260504201680249 ) ) ;
#34130 = EDGE_CURVE ( 'NONE', #5081, #236424, #136623, .T. ) ;
#34132 = ORIENTED_EDGE ( 'NONE', *, *, #98140, .T. ) ;
#34131 = AXIS2_PLACEMENT_3D ( 'NONE', #10551, #230893, #247864 ) ;
#34133 = ORIENTED_EDGE ( 'NONE', *, *, #68118, .T. ) ;
#34134 = CARTESIAN_POINT ( 'NONE',  ( -18.36527282682041928, -9.500000599987968641, -73.92214896449833361 ) ) ;
#34135 = EDGE_LOOP ( 'NONE', ( #33077, #191257, #50941, #172938 ) ) ;
#34136 = EDGE_CURVE ( 'NONE', #180612, #230787, #68725, .T. ) ;
#34137 = PLANE ( 'NONE',  #54601 ) ;
#34138 = ORIENTED_EDGE ( 'NONE', *, *, #184151, .T. ) ;
#34140 = ORIENTED_EDGE ( 'NONE', *, *, #168708, .F. ) ;
#34139 = DIRECTION ( 'NONE',  ( 1.836970198721029934E-16, 1.000000000000000000, 6.982962677686266711E-15 ) ) ;
#34142 = ADVANCED_FACE ( 'NONE', ( #86967 ), #107423, .T. ) ;
#34141 = VERTEX_POINT ( 'NONE', #7456 ) ;
#34143 = CARTESIAN_POINT ( 'NONE',  ( 21.05000000000000071, -11.48912529307605546, -30.39999999999999503 ) ) ;
#34145 = ORIENTED_EDGE ( 'NONE', *, *, #29141, .T. ) ;
#34144 = EDGE_CURVE ( 'NONE', #257702, #257588, #178180, .T. ) ;
#34148 = VERTEX_POINT ( 'NONE', #51691 ) ;
#34147 = VERTEX_POINT ( 'NONE', #47848 ) ;
#34146 = LINE ( 'NONE', #97893, #164440 ) ;
#34149 = EDGE_CURVE ( 'NONE', #6394, #94057, #27058, .T. ) ;
#34150 = AXIS2_PLACEMENT_3D ( 'NONE', #206146, #50890, #130453 ) ;
#34151 = ORIENTED_EDGE ( 'NONE', *, *, #201408, .T. ) ;
#34152 = VECTOR ( 'NONE', #190077, 1000.000000000000000 ) ;
#34153 = AXIS2_PLACEMENT_3D ( 'NONE', #115150, #95578, #175171 ) ;
#34154 = CARTESIAN_POINT ( 'NONE',  ( 21.14999999999999858, 8.786607556611267356, -45.75000000000000711 ) ) ;
#34155 = VERTEX_POINT ( 'NONE', #187397 ) ;
#34156 = CARTESIAN_POINT ( 'NONE',  ( -16.93353400591625757, 10.00461239618409515, -154.9326844702054586 ) ) ;
#34157 =( BOUNDED_SURFACE ( )  B_SPLINE_SURFACE ( 3, 2, ( 
 ( #238308, #101317, #201750 ),
 ( #220038, #257823, #23146 ),
 ( #60953, #38849, #163921 ),
 ( #41423, #59647, #183484 ),
 ( #139189, #21845, #141769 ),
 ( #119667, #161363, #42682 ),
 ( #242160, #84317, #218731 ),
 ( #180917, #118382, #62249 ) ),
 .UNSPECIFIED., .F., .F., .F. ) 
 B_SPLINE_SURFACE_WITH_KNOTS ( ( 4, 2, 2, 4 ),
 ( 3, 3 ),
 ( 0.0001723339234021445073, 0.0002782939632049937244, 0.0003842540030078429956, 0.0005961740826135415380 ),
 ( 0.000000000000000000, 1.000000000000000000 ),
 .UNSPECIFIED. ) 
 GEOMETRIC_REPRESENTATION_ITEM ( )  RATIONAL_B_SPLINE_SURFACE ( (
 ( 1.000000000000000000, 0.9504532311154628710, 1.000000000000000000),
 ( 1.000000000000000000, 0.9506023220710051458, 1.000000000000000000),
 ( 1.000000000000000000, 0.9395774818181180654, 1.000000000000000000),
 ( 1.000000000000000000, 0.9079328464647721253, 1.000000000000000000),
 ( 1.000000000000000000, 0.8875702416205415446, 1.000000000000000000),
 ( 1.000000000000000000, 0.8205919608040560531, 1.000000000000000000),
 ( 1.000000000000000000, 0.7666842783598126765, 1.000000000000000000),
 ( 1.000000000000000000, 0.7071067811864651942, 1.000000000000000000) ) ) 
 REPRESENTATION_ITEM ( '' )  SURFACE ( )  );
#34159 = EDGE_LOOP ( 'NONE', ( #48577, #24874 ) ) ;
#34158 = CARTESIAN_POINT ( 'NONE',  ( 20.94999999999999929, 4.850467289730776344, -54.96573259099832143 ) ) ;
#34160 = CARTESIAN_POINT ( 'NONE',  ( 18.49999999999999645, 77.13501884592258762, -162.3061306010920362 ) ) ;
#34161 = VERTEX_POINT ( 'NONE', #30911 ) ;
#34162 = EDGE_CURVE ( 'NONE', #131851, #191399, #11779, .T. ) ;
#34163 = ADVANCED_FACE ( 'NONE', ( #148254 ), #67432, .T. ) ;
#34164 = ORIENTED_EDGE ( 'NONE', *, *, #233295, .T. ) ;
#34165 = CARTESIAN_POINT ( 'NONE',  ( 18.41356215285962250, 85.50000000001165290, -62.49103808782466984 ) ) ;
#34166 = CARTESIAN_POINT ( 'NONE',  ( 18.49999999999999289, 18.34711819382569686, -236.8747682978092541 ) ) ;
#34167 = VECTOR ( 'NONE', #174507, 1000.000000000000227 ) ;
#34168 = VERTEX_POINT ( 'NONE', #110405 ) ;
#34169 = ORIENTED_EDGE ( 'NONE', *, *, #106532, .F. ) ;
#34170 = SPHERICAL_SURFACE ( 'NONE', #90155, 0.1000000000000000056 ) ;
#34172 = VERTEX_POINT ( 'NONE', #106538 ) ;
#34171 = ORIENTED_EDGE ( 'NONE', *, *, #103792, .F. ) ;
#34173 = VERTEX_POINT ( 'NONE', #189955 ) ;
#34174 = DIRECTION ( 'NONE',  ( 0.000000000000000000, 0.9893560106964510714, -0.1455152366551481502 ) ) ;
#34175 = ORIENTED_EDGE ( 'NONE', *, *, #138454, .T. ) ;
#34176 = VERTEX_POINT ( 'NONE', #184810 ) ;
#34177 = DIRECTION ( 'NONE',  ( -0.000000000000000000, 1.000000000000000000, 0.000000000000000000 ) ) ;
#34178 = ORIENTED_EDGE ( 'NONE', *, *, #170509, .T. ) ;
#34179 = DIRECTION ( 'NONE',  ( -0.000000000000000000, 0.1350103645451876666, 0.9908441862701600211 ) ) ;
#34180 = CARTESIAN_POINT ( 'NONE',  ( 20.99999999999999645, 9.750000000011137757, -42.75000000000000000 ) ) ;
#34181 = VERTEX_POINT ( 'NONE', #90835 ) ;
#34182 = CIRCLE ( 'NONE', #175815, 0.1000000000000000472 ) ;
#34183 = CIRCLE ( 'NONE', #134087, 0.5000000000000004441 ) ;
#34184 = ORIENTED_EDGE ( 'NONE', *, *, #77597, .T. ) ;
#34185 = AXIS2_PLACEMENT_3D ( 'NONE', #5706, #202645, #244335 ) ;
#34187 = EDGE_CURVE ( 'NONE', #139796, #146959, #236585, .T. ) ;
#34186 = DIRECTION ( 'NONE',  ( 0.000000000000000000, -0.1350103645451945777, 0.9908441862701591329 ) ) ;
#34188 = ORIENTED_EDGE ( 'NONE', *, *, #246657, .F. ) ;
#34189 = ADVANCED_FACE ( 'NONE', ( #246087 ), #7457, .F. ) ;
#34190 = DIRECTION ( 'NONE',  ( -1.000000000000000000, 0.000000000000000000, -0.000000000000000000 ) ) ;
#34191 = ORIENTED_EDGE ( 'NONE', *, *, #33000, .T. ) ;
#34192 = ORIENTED_EDGE ( 'NONE', *, *, #39591, .F. ) ;
#34193 = DIRECTION ( 'NONE',  ( 0.000000000000000000, -0.9126074666063767049, -0.4088369013363286619 ) ) ;
#34195 = ORIENTED_EDGE ( 'NONE', *, *, #59038, .T. ) ;
#34194 = CARTESIAN_POINT ( 'NONE',  ( 18.49713797159848738, 85.44648232759141138, -162.9516493629143952 ) ) ;
#34196 = DIRECTION ( 'NONE',  ( -1.000000000000000000, 0.000000000000000000, 0.000000000000000000 ) ) ;
#34197 = LINE ( 'NONE', #14623, #68657 ) ;
#34198 = CARTESIAN_POINT ( 'NONE',  ( 20.95539060131842746, 65.37613784235644232, -128.8693736708681854 ) ) ;
#34199 = CARTESIAN_POINT ( 'NONE',  ( 18.53691006697088284, 33.76830691225385550, -236.3156058738864544 ) ) ;
#34200 = VECTOR ( 'NONE', #131142, 1000.000000000000000 ) ;
#34201 = DIRECTION ( 'NONE',  ( -0.7071067811865475727, 0.7071067811865475727, 4.937700262164531476E-15 ) ) ;
#34202 = DIRECTION ( 'NONE',  ( -0.000000000000000000, -0.4721928772777346239, -0.8814952561688430555 ) ) ;
#34203 = CARTESIAN_POINT ( 'NONE',  ( -21.37071067811865532, 52.75222874190619393, -233.4979877221775837 ) ) ;
#34204 = CARTESIAN_POINT ( 'NONE',  ( 21.51976009735019346, 33.83367400564330296, -243.2446267297141844 ) ) ;
#34205 = CARTESIAN_POINT ( 'NONE',  ( -16.87683809663752044, 66.13508655273203374, -149.7988259332204279 ) ) ;
#34206 = CARTESIAN_POINT ( 'NONE',  ( -20.15000000000000568, 66.70857864377492774, -148.7731074845244166 ) ) ;
#34207 = FACE_OUTER_BOUND ( 'NONE', #70794, .T. ) ;
#34208 = EDGE_CURVE ( 'NONE', #55464, #28001, #165253, .T. ) ;
#34209 = ORIENTED_EDGE ( 'NONE', *, *, #184749, .T. ) ;
#34211 = ORIENTED_EDGE ( 'NONE', *, *, #42198, .T. ) ;
#34210 = ORIENTED_EDGE ( 'NONE', *, *, #179107, .F. ) ;
#34212 = EDGE_LOOP ( 'NONE', ( #135068, #39582, #131284, #95043 ) ) ;
#34213 = CARTESIAN_POINT ( 'NONE',  ( -18.59999999999999787, -11.75000000000000000, 6.100000000000001421 ) ) ;
#34214 = AXIS2_PLACEMENT_3D ( 'NONE', #10412, #52074, #132929 ) ;
#34215 = CARTESIAN_POINT ( 'NONE',  ( -18.50000000000000000, 11.64999999999999680, -0.1000000000000028644 ) ) ;
#34217 = DIRECTION ( 'NONE',  ( 1.020425574104004196E-15, -0.2617529984165031243, -0.9651348961777157509 ) ) ;
#34216 = CARTESIAN_POINT ( 'NONE',  ( 22.57320508075688537, 11.65000000001115588, -33.50000000000000000 ) ) ;
#34218 = ORIENTED_EDGE ( 'NONE', *, *, #188246, .F. ) ;
#34219 = ORIENTED_EDGE ( 'NONE', *, *, #71642, .F. ) ;
#34220 = AXIS2_PLACEMENT_3D ( 'NONE', #152288, #250082, #96119 ) ;
#34221 = DIRECTION ( 'NONE',  ( 1.000000000000000000, 0.000000000000000000, 0.000000000000000000 ) ) ;
#34222 = AXIS2_PLACEMENT_3D ( 'NONE', #165588, #160468, #142150 ) ;
#34223 = DIRECTION ( 'NONE',  ( -0.000000000000000000, -0.000000000000000000, -1.000000000000000000 ) ) ;
#34224 = CIRCLE ( 'NONE', #130022, 4.299999999999970512 ) ;
#34225 = AXIS2_PLACEMENT_3D ( 'NONE', #78389, #53700, #117528 ) ;
#34226 = DIRECTION ( 'NONE',  ( 1.000000000000000000, 0.000000000000000000, 0.000000000000000000 ) ) ;
#34227 = ORIENTED_EDGE ( 'NONE', *, *, #6135, .T. ) ;
#34228 = VERTEX_POINT ( 'NONE', #49152 ) ;
#34229 = DIRECTION ( 'NONE',  ( 1.000000000000000000, 0.000000000000000000, 0.000000000000000000 ) ) ;
#34230 = AXIS2_PLACEMENT_3D ( 'NONE', #202005, #3803, #156494 ) ;
#34231 = CARTESIAN_POINT ( 'NONE',  ( 23.24999999999999289, 6.650000000011155876, -54.65000000000000568 ) ) ;
#34232 = ORIENTED_EDGE ( 'NONE', *, *, #81714, .F. ) ;
#34233 = CARTESIAN_POINT ( 'NONE',  ( -18.59999999999999787, 8.809961202382808665, -241.4517562488062481 ) ) ;
#34235 = ORIENTED_EDGE ( 'NONE', *, *, #154194, .F. ) ;
#34234 = CARTESIAN_POINT ( 'NONE',  ( 18.39999999999999858, 77.26488334054521090, -241.9697969554615611 ) ) ;
#34236 = CARTESIAN_POINT ( 'NONE',  ( -20.64999999999999858, 84.73084112150739600, -126.9250327655398962 ) ) ;
#34237 = LINE ( 'NONE', #134564, #252164 ) ;
#34239 = CIRCLE ( 'NONE', #179970, 0.1000000000000028644 ) ;
#34238 = FACE_OUTER_BOUND ( 'NONE', #115216, .T. ) ;
#34240 = ORIENTED_EDGE ( 'NONE', *, *, #92151, .F. ) ;
#34241 = CARTESIAN_POINT ( 'NONE',  ( 15.57250062127604018, 66.62931007840923314, -85.49664235786335098 ) ) ;
#34242 = DIRECTION ( 'NONE',  ( 1.000000000000000000, -0.000000000000000000, -0.000000000000000000 ) ) ;
#34243 = PLANE ( 'NONE',  #123497 ) ;
#34244 = AXIS2_PLACEMENT_3D ( 'NONE', #120531, #57938, #80049 ) ;
#34246 = CARTESIAN_POINT ( 'NONE',  ( -21.05000000000000071, -1.851028230129704522, -112.1539132694225316 ) ) ;
#34245 = FACE_OUTER_BOUND ( 'NONE', #244607, .T. ) ;
#34247 = CARTESIAN_POINT ( 'NONE',  ( 20.94999999999999929, 71.00000000001253397, -182.0283735034374786 ) ) ;
#34248 = EDGE_CURVE ( 'NONE', #109505, #126, #128706, .T. ) ;
#34250 = DIRECTION ( 'NONE',  ( 0.000000000000000000, 0.000000000000000000, 1.000000000000000000 ) ) ;
#34249 = CIRCLE ( 'NONE', #100802, 0.1999999999999987899 ) ;
#34251 = CARTESIAN_POINT ( 'NONE',  ( -23.15000000000000213, 76.00000000001210765, -132.4731074845242915 ) ) ;
#34252 = CARTESIAN_POINT ( 'NONE',  ( 18.39999999999999858, -0.9152171842607033092, -242.2974985173726452 ) ) ;
#34253 = AXIS2_PLACEMENT_3D ( 'NONE', #130797, #231208, #52537 ) ;
#34254 = ORIENTED_EDGE ( 'NONE', *, *, #171103, .T. ) ;
#34256 =( BOUNDED_CURVE ( )  B_SPLINE_CURVE ( 3, ( #79982, #1742, #120461, #160855 ),
 .UNSPECIFIED., .F., .F. ) 
 B_SPLINE_CURVE_WITH_KNOTS ( ( 4, 4 ),
 ( 4.712388980384690562, 5.672655318024762749 ),
 .UNSPECIFIED. ) 
 CURVE ( )  GEOMETRIC_REPRESENTATION_ITEM ( )  RATIONAL_B_SPLINE_CURVE ( ( 1.000000000000000000, 0.9246222802177245237, 0.9246222802177245237, 1.000000000000000000 ) ) 
 REPRESENTATION_ITEM ( '' )  );
#34255 = AXIS2_PLACEMENT_3D ( 'NONE', #108980, #128560, #210660 ) ;
#34257 = ORIENTED_EDGE ( 'NONE', *, *, #182313, .F. ) ;
#34258 = ADVANCED_FACE ( 'NONE', ( #170440 ), #40820, .T. ) ;
#34259 = DIRECTION ( 'NONE',  ( 1.000000000000000000, 2.952720810173289112E-16, -0.000000000000000000 ) ) ;
#34260 = CARTESIAN_POINT ( 'NONE',  ( -21.05000000000000071, 67.23127455305835554, -235.8551265064784559 ) ) ;
#34261 = EDGE_LOOP ( 'NONE', ( #210170, #139281, #26530, #167511 ) ) ;
#34262 = AXIS2_PLACEMENT_3D ( 'NONE', #60543, #24021, #103514 ) ;
#34263 = ADVANCED_FACE ( 'NONE', ( #66152, #193806 ), #196358, .T. ) ;
#34264 = EDGE_LOOP ( 'NONE', ( #44604, #131622, #170745, #131993 ) ) ;
#34265 = SURFACE_SIDE_STYLE ('',( #151640 ) ) ;
#34266 = ADVANCED_FACE ( 'NONE', ( #175546, #210796 ), #36024, .F. ) ;
#34267 = ORIENTED_EDGE ( 'NONE', *, *, #69669, .T. ) ;
#34268 = CARTESIAN_POINT ( 'NONE',  ( 21.09107601085543848, 75.96069283529470795, -109.3869854598841300 ) ) ;
#34269 = AXIS2_PLACEMENT_3D ( 'NONE', #197836, #113177, #192721 ) ;
#34270 = ORIENTED_EDGE ( 'NONE', *, *, #29087, .T. ) ;
#34271 = AXIS2_PLACEMENT_3D ( 'NONE', #107449, #69626, #245681 ) ;
#34273 = FACE_OUTER_BOUND ( 'NONE', #177477, .T. ) ;
#34272 = VECTOR ( 'NONE', #65004, 1000.000000000000000 ) ;
#34274 = DIRECTION ( 'NONE',  ( 0.000000000000000000, 6.982962677686266711E-15, -1.000000000000000000 ) ) ;
#34275 = DIRECTION ( 'NONE',  ( -1.000000000000000000, -0.000000000000000000, -0.000000000000000000 ) ) ;
#34276 = CARTESIAN_POINT ( 'NONE',  ( 18.59999999999999787, -1.851028230129704522, -78.65391326942254580 ) ) ;
#34278 = ORIENTED_EDGE ( 'NONE', *, *, #40806, .T. ) ;
#34277 = CYLINDRICAL_SURFACE ( 'NONE', #175879, 0.5000000000000004441 ) ;
#34280 = CARTESIAN_POINT ( 'NONE',  ( -20.85000000000000142, 7.783179459866048866, -245.3643104511423019 ) ) ;
#34279 = DIRECTION ( 'NONE',  ( 0.000000000000000000, 0.9651348961777197477, -0.2617529984164879142 ) ) ;
#34281 = ADVANCED_FACE ( 'NONE', ( #116829 ), #154703, .F. ) ;
#34282 = CARTESIAN_POINT ( 'NONE',  ( 21.13461538461538325, 61.88829803306103372, -221.6099259868126694 ) ) ;
#34283 = CARTESIAN_POINT ( 'NONE',  ( 12.25000000000000000, 66.65000000001202807, -120.0015881126992241 ) ) ;
#34284 = DIRECTION ( 'NONE',  ( -1.000000000000000000, -0.000000000000000000, -0.000000000000000000 ) ) ;
#34285 = CARTESIAN_POINT ( 'NONE',  ( 18.49999999999999289, 11.75000000000000000, -24.85000000000000142 ) ) ;
#34286 = VERTEX_POINT ( 'NONE', #77678 ) ;
#34287 = CYLINDRICAL_SURFACE ( 'NONE', #250162, 0.09999999999999939493 ) ;
#34288 = VERTEX_POINT ( 'NONE', #94689 ) ;
#34289 = DIRECTION ( 'NONE',  ( -1.000000000000000000, -1.541880601228652843E-16, -2.878400969107353907E-16 ) ) ;
#34290 = CIRCLE ( 'NONE', #21795, 0.09999999999998898659 ) ;
#34292 = ORIENTED_EDGE ( 'NONE', *, *, #236806, .F. ) ;
#34291 = B_SPLINE_CURVE_WITH_KNOTS ( 'NONE', 3,
 ( #209994, #170911, #30092, #50880, #206135, #130439, #52178, #147440, #249130, #10511 ),
 .UNSPECIFIED., .F., .F.,
 ( 4, 2, 2, 2, 4 ),
 ( 0.000000000000000000, 3.990160268012752048E-05, 7.980320536025504096E-05, 0.0001596064107205164245, 0.0003192128214410408721 ),
 .UNSPECIFIED. ) ;
#34293 = DIRECTION ( 'NONE',  ( 1.000000000000000000, -0.000000000000000000, -0.000000000000000000 ) ) ;
#34294 = CARTESIAN_POINT ( 'NONE',  ( -18.59999999999999787, 77.83585931145600512, -158.5186683157258187 ) ) ;
#34295 = CARTESIAN_POINT ( 'NONE',  ( -18.50000000000000000, 11.65000000001115232, -112.6500000000000341 ) ) ;
#34296 = ORIENTED_EDGE ( 'NONE', *, *, #210020, .F. ) ;
#34297 = VERTEX_POINT ( 'NONE', #58110 ) ;
#34298 = CARTESIAN_POINT ( 'NONE',  ( 20.94999999999999574, -1.835341550213255957, -78.65515129256301918 ) ) ;
#34299 = FACE_OUTER_BOUND ( 'NONE', #216900, .T. ) ;
#34300 = CARTESIAN_POINT ( 'NONE',  ( 20.94999027547553894, 65.70673848567030007, -164.5638252334829588 ) ) ;
#34301 = CARTESIAN_POINT ( 'NONE',  ( -16.85718274719404164, 66.02385768539009803, -90.45976115234198289 ) ) ;
#34303 = CARTESIAN_POINT ( 'NONE',  ( 18.49999999999999289, 10.32573593129922607, -158.8499999999999943 ) ) ;
#34302 = DIRECTION ( 'NONE',  ( 0.000000000000000000, 0.7049548389604869403, -0.7092521942343174013 ) ) ;
#34304 = DIRECTION ( 'NONE',  ( 1.000000000000000000, 0.000000000000000000, 0.000000000000000000 ) ) ;
#34305 = FACE_OUTER_BOUND ( 'NONE', #136293, .T. ) ;
#34306 = FACE_OUTER_BOUND ( 'NONE', #114165, .T. ) ;
#34307 = ORIENTED_EDGE ( 'NONE', *, *, #34948, .F. ) ;
#34308 = CARTESIAN_POINT ( 'NONE',  ( 21.05000000000000071, 1.115600667400684642E-11, -167.5999999999999659 ) ) ;
#34309 = EDGE_CURVE ( 'NONE', #256568, #191326, #212095, .T. ) ;
#34310 = CIRCLE ( 'NONE', #180035, 0.1000000000000028644 ) ;
#34312 = VERTEX_POINT ( 'NONE', #157267 ) ;
#34311 = CARTESIAN_POINT ( 'NONE',  ( 20.95512820512820440, 14.90253654416821760, -219.5025151102366578 ) ) ;
#34313 = CARTESIAN_POINT ( 'NONE',  ( 20.95203847575071521, 65.49893946073862594, -195.9560361359008880 ) ) ;
#34314 = DIRECTION ( 'NONE',  ( -1.000000000000000000, 1.875376730785737719E-16, 1.309568571767809260E-30 ) ) ;
#34315 = DIRECTION ( 'NONE',  ( 1.000000000000000000, 0.000000000000000000, 0.000000000000000000 ) ) ;
#34317 = VERTEX_POINT ( 'NONE', #252471 ) ;
#34316 = CARTESIAN_POINT ( 'NONE',  ( 23.14999999999999503, 11.65000000001116298, -179.6499999999999773 ) ) ;
#34318 = LINE ( 'NONE', #78538, #71779 ) ;
#34319 = CARTESIAN_POINT ( 'NONE',  ( -20.64999999999999858, 2.000000000011154189, -121.2753780772379315 ) ) ;
#34320 = LINE ( 'NONE', #254594, #42774 ) ;
#34321 = CARTESIAN_POINT ( 'NONE',  ( -21.14999999999999858, 11.65000000001115588, -134.0000000000000284 ) ) ;
#34323 = EDGE_CURVE ( 'NONE', #193833, #155848, #44890, .T. ) ;
#34322 = CARTESIAN_POINT ( 'NONE',  ( 21.05000000000000071, 65.27628289530480288, -162.3581939154368285 ) ) ;
#34324 = ORIENTED_EDGE ( 'NONE', *, *, #38475, .T. ) ;
#34325 = DIRECTION ( 'NONE',  ( 0.000000000000000000, 0.2128009952263403282, -0.9770955615653358350 ) ) ;
#34326 = EDGE_LOOP ( 'NONE', ( #78261, #161775, #98611, #172075 ) ) ;
#34327 = EDGE_CURVE ( 'NONE', #45832, #252532, #24235, .T. ) ;
#34328 = EDGE_CURVE ( 'NONE', #224594, #217530, #207402, .T. ) ;
#34330 = CIRCLE ( 'NONE', #134236, 0.09999999999998898659 ) ;
#34329 = CARTESIAN_POINT ( 'NONE',  ( -17.01764560440456719, 66.05000000001189164, -90.27310748531118634 ) ) ;
#34331 = ORIENTED_EDGE ( 'NONE', *, *, #88099, .F. ) ;
#34332 = CARTESIAN_POINT ( 'NONE',  ( -16.92507428761701860, 9.950000000011138823, -154.7866025403784249 ) ) ;
#34333 = EDGE_LOOP ( 'NONE', ( #175858, #161721, #28986, #66460 ) ) ;
#34334 = TOROIDAL_SURFACE ( 'NONE', #225804, 0.2000000000000000111, 0.1000000000000000056 ) ;
#34335 = CARTESIAN_POINT ( 'NONE',  ( 21.05000000000000071, -0.09999999998884338825, -93.95934304829877703 ) ) ;
#34336 = CARTESIAN_POINT ( 'NONE',  ( 18.49999999999998934, 10.24999999999999822, -24.75000000000000000 ) ) ;
#34337 = AXIS2_PLACEMENT_3D ( 'NONE', #16898, #174728, #254191 ) ;
#34338 = EDGE_CURVE ( 'NONE', #242741, #65949, #115795, .T. ) ;
#34339 = ORIENTED_EDGE ( 'NONE', *, *, #119025, .F. ) ;
#34340 = EDGE_CURVE ( 'NONE', #17833, #36199, #72589, .T. ) ;
#34341 = EDGE_CURVE ( 'NONE', #177617, #26579, #190655, .T. ) ;
#34342 = CARTESIAN_POINT ( 'NONE',  ( -21.64999999999999858, 66.65000000001231228, -157.3731074845244393 ) ) ;
#34343 = DIRECTION ( 'NONE',  ( 0.000000000000000000, 0.9654727137038715545, -0.2605042016806676242 ) ) ;
#34344 = AXIS2_PLACEMENT_3D ( 'NONE', #191323, #12675, #92178 ) ;
#34345 = AXIS2_PLACEMENT_3D ( 'NONE', #74221, #11659, #32528 ) ;
#34346 = CARTESIAN_POINT ( 'NONE',  ( 22.32929514600007792, 7.383979495903388646, -199.2904498502753938 ) ) ;
#34347 = DIRECTION ( 'NONE',  ( 0.000000000000000000, 0.000000000000000000, -1.000000000000000000 ) ) ;
#34348 = ORIENTED_EDGE ( 'NONE', *, *, #161821, .T. ) ;
#34349 = CARTESIAN_POINT ( 'NONE',  ( -18.41809261886928439, 85.68240331476874871, -129.8662639344331637 ) ) ;
#34350 = ORIENTED_EDGE ( 'NONE', *, *, #243291, .T. ) ;
#34352 = VERTEX_POINT ( 'NONE', #155982 ) ;
#34351 = LINE ( 'NONE', #77286, #218918 ) ;
#34353 = EDGE_LOOP ( 'NONE', ( #256338, #18422, #192581, #185801, #253173, #107254 ) ) ;
#34354 = DIRECTION ( 'NONE',  ( 0.000000000000000000, 0.000000000000000000, -1.000000000000000000 ) ) ;
#34355 = DIRECTION ( 'NONE',  ( 0.000000000000000000, 0.2128009952263485993, -0.9770955615653341697 ) ) ;
#34356 = CARTESIAN_POINT ( 'NONE',  ( 21.05000000000000071, 1.360870587203197646, -75.07299792709100927 ) ) ;
#34357 = EDGE_CURVE ( 'NONE', #140623, #58126, #257214, .T. ) ;
#34358 = AXIS2_PLACEMENT_3D ( 'NONE', #96554, #133143, #174892 ) ;
#34359 = CARTESIAN_POINT ( 'NONE',  ( -22.39999999999999858, 76.10085836911045476, -81.27267460801371612 ) ) ;
#34360 = ORIENTED_EDGE ( 'NONE', *, *, #180033, .F. ) ;
#34361 = ADVANCED_FACE ( 'NONE', ( #235478 ), #206632, .F. ) ;
#34362 = EDGE_CURVE ( 'NONE', #123327, #39467, #215737, .T. ) ;
#34363 = DIRECTION ( 'NONE',  ( -0.7071067811865475727, -0.7071067811865475727, 0.000000000000000000 ) ) ;
#34364 = FACE_OUTER_BOUND ( 'NONE', #223106, .T. ) ;
#34365 = EDGE_LOOP ( 'NONE', ( #92202, #203183, #47895, #212596, #79781 ) ) ;
#34367 = ORIENTED_EDGE ( 'NONE', *, *, #84734, .F. ) ;
#34366 = CARTESIAN_POINT ( 'NONE',  ( -16.92973740335361299, 66.00749618554520737, -115.6170484493226525 ) ) ;
#34368 = AXIS2_PLACEMENT_3D ( 'NONE', #213962, #35364, #36641 ) ;
#34369 = VECTOR ( 'NONE', #203944, 1000.000000000000000 ) ;
#34370 = CARTESIAN_POINT ( 'NONE',  ( -21.55000000000000071, 68.75000000001230660, -157.6731074845243938 ) ) ;
#34371 = CARTESIAN_POINT ( 'NONE',  ( -21.14999999999999858, 1.658775325997247752, -230.6916041481598540 ) ) ;
#34372 = AXIS2_PLACEMENT_3D ( 'NONE', #31757, #205202, #10885 ) ;
#34373 = CARTESIAN_POINT ( 'NONE',  ( 20.85000000000000142, -1.835859311432481045, -145.5044391687985694 ) ) ;
#34374 = ORIENTED_EDGE ( 'NONE', *, *, #151870, .F. ) ;
#34375 = VERTEX_POINT ( 'NONE', #60683 ) ;
#34376 = DIRECTION ( 'NONE',  ( -1.836970198721029934E-16, -1.000000000000000000, -6.982962677686266711E-15 ) ) ;
#34377 = CARTESIAN_POINT ( 'NONE',  ( -20.54999999999999716, 76.00000000001237765, -170.0231074845243597 ) ) ;
#34378 = EDGE_LOOP ( 'NONE', ( #103584, #217825, #114339, #23561 ) ) ;
#34379 = FACE_OUTER_BOUND ( 'NONE', #104960, .T. ) ;
#34380 = EDGE_CURVE ( 'NONE', #3044, #129511, #94933, .T. ) ;
#34381 = ADVANCED_FACE ( 'NONE', ( #137650 ), #240624, .T. ) ;
#34382 = CARTESIAN_POINT ( 'NONE',  ( 21.00000000000000000, 9.750000000011153745, -188.7499999999999716 ) ) ;
#34383 = DIRECTION ( 'NONE',  ( 0.000000000000000000, 0.8660254037844482555, 0.4999999999999837907 ) ) ;
#34384 = ADVANCED_FACE ( 'NONE', ( #178107 ), #219837, .T. ) ;
#34385 = CIRCLE ( 'NONE', #88492, 0.09999999999999986677 ) ;
#34386 = AXIS2_PLACEMENT_3D ( 'NONE', #66568, #185226, #88660 ) ;
#34387 = ORIENTED_EDGE ( 'NONE', *, *, #181317, .T. ) ;
#34388 = DIRECTION ( 'NONE',  ( -4.801466763864314121E-15, 0.2605042016806606298, 0.9654727137038736640 ) ) ;
#34389 = EDGE_LOOP ( 'NONE', ( #41930, #36038, #136353, #36093 ) ) ;
#34390 = DIRECTION ( 'NONE',  ( 0.000000000000000000, -0.4721928772777346239, -0.8814952561688430555 ) ) ;
#34391 = DIRECTION ( 'NONE',  ( -1.000000000000000000, 0.000000000000000000, 0.000000000000000000 ) ) ;
#34392 = VECTOR ( 'NONE', #226201, 1000.000000000000000 ) ;
#34394 = ORIENTED_EDGE ( 'NONE', *, *, #66504, .F. ) ;
#34393 = CYLINDRICAL_SURFACE ( 'NONE', #208455, 0.5000000000000004441 ) ;
#34395 = CARTESIAN_POINT ( 'NONE',  ( 23.14999999999998437, 10.69888912757691202, -235.6450824654141059 ) ) ;
#34396 = CARTESIAN_POINT ( 'NONE',  ( 21.05000000000000071, 64.35000000001213039, -136.5231074845243597 ) ) ;
#34397 = DIRECTION ( 'NONE',  ( 1.000000000000000000, 0.000000000000000000, 0.000000000000000000 ) ) ;
#34398 = DIRECTION ( 'NONE',  ( 0.000000000000000000, -0.8068669527896844551, -0.5907332058517525963 ) ) ;
#34399 = DIRECTION ( 'NONE',  ( 0.000000000000000000, -2.602085213965497408E-13, 1.000000000000000000 ) ) ;
#34400 = VECTOR ( 'NONE', #107682, 1000.000000000000000 ) ;
#34401 = EDGE_CURVE ( 'NONE', #227485, #229941, #19959, .T. ) ;
#34402 = DIRECTION ( 'NONE',  ( 1.000000000000000000, 0.000000000000000000, 0.000000000000000000 ) ) ;
#34403 = DIRECTION ( 'NONE',  ( -1.000000000000000000, -0.000000000000000000, -0.000000000000000000 ) ) ;
#34405 = VERTEX_POINT ( 'NONE', #21594 ) ;
#34404 = CARTESIAN_POINT ( 'NONE',  ( -21.78635804494510708, 68.96433851485896582, -136.6221125500320284 ) ) ;
#34406 = AXIS2_PLACEMENT_3D ( 'NONE', #117154, #97546, #78007 ) ;
#34407 = AXIS2_PLACEMENT_3D ( 'NONE', #108858, #168882, #28072 ) ;
#34408 = EDGE_CURVE ( 'NONE', #128325, #53595, #15877, .T. ) ;
#34409 = AXIS2_PLACEMENT_3D ( 'NONE', #186499, #225585, #30011 ) ;
#34410 = AXIS2_PLACEMENT_3D ( 'NONE', #208133, #214218, #209389 ) ;
#34411 = B_SPLINE_CURVE_WITH_KNOTS ( 'NONE', 3,
 ( #102490, #219905, #184626, #162524, #21715, #41302, #36492, #182072 ),
 .UNSPECIFIED., .F., .F.,
 ( 4, 2, 2, 4 ),
 ( 0.000000000000000000, 6.534141206311692811E-05, 0.0001306828241262338562, 0.0002613656482524238022 ),
 .UNSPECIFIED. ) ;
#34412 = CIRCLE ( 'NONE', #230195, 12.87500000000000000 ) ;
#34414 = EDGE_CURVE ( 'NONE', #33930, #92153, #49153, .T. ) ;
#34413 = CARTESIAN_POINT ( 'NONE',  ( 20.99999999999999645, 9.749999999999982236, -20.84999999999999787 ) ) ;
#34415 = EDGE_CURVE ( 'NONE', #99410, #99179, #149144, .T. ) ;
#34416 = DIRECTION ( 'NONE',  ( -1.000000000000000000, 3.265361837132813093E-16, 2.280189983783949500E-30 ) ) ;
#34417 = CARTESIAN_POINT ( 'NONE',  ( 20.90000000000000213, -1.800000000000000044, -11.61130914238355771 ) ) ;
#34418 = EDGE_CURVE ( 'NONE', #94115, #173853, #158546, .T. ) ;
#34419 = VERTEX_POINT ( 'NONE', #218471 ) ;
#34420 = DIRECTION ( 'NONE',  ( -1.000000000000000000, 2.952720810173289112E-16, 2.061873921506763405E-30 ) ) ;
#34421 = AXIS2_PLACEMENT_3D ( 'NONE', #118931, #139738, #38109 ) ;
#34422 = FACE_OUTER_BOUND ( 'NONE', #177388, .T. ) ;
#34423 = LINE ( 'NONE', #134747, #244967 ) ;
#34424 = AXIS2_PLACEMENT_3D ( 'NONE', #195067, #659, #97174 ) ;
#34425 = AXIS2_PLACEMENT_3D ( 'NONE', #115976, #15612, #112134 ) ;
#34426 = ORIENTED_EDGE ( 'NONE', *, *, #33193, .T. ) ;
#34428 = EDGE_CURVE ( 'NONE', #111418, #155591, #222310, .T. ) ;
#34427 = DIRECTION ( 'NONE',  ( 1.000000000000000000, 1.541880601228652843E-16, 2.878400969107353907E-16 ) ) ;
#34429 = ADVANCED_FACE ( 'NONE', ( #1996 ), #217192, .F. ) ;
#34430 = AXIS2_PLACEMENT_3D ( 'NONE', #117184, #96309, #14251 ) ;
#34431 = CIRCLE ( 'NONE', #67533, 0.1000000000000000472 ) ;
#34432 = CARTESIAN_POINT ( 'NONE',  ( -16.93970660449832621, 10.01284139164672915, -79.55228173579450868 ) ) ;
#34433 = EDGE_LOOP ( 'NONE', ( #15143, #221995, #103743, #178720 ) ) ;
#34434 = CARTESIAN_POINT ( 'NONE',  ( -16.94107738177414291, 65.98576071487489969, -48.57310748452439952 ) ) ;
#34435 = ORIENTED_EDGE ( 'NONE', *, *, #191270, .F. ) ;
#34436 = EDGE_CURVE ( 'NONE', #2493, #178117, #99331, .T. ) ;
#34437 = VECTOR ( 'NONE', #52758, 1000.000000000000000 ) ;
#34439 = VERTEX_POINT ( 'NONE', #138916 ) ;
#34438 = CARTESIAN_POINT ( 'NONE',  ( 20.94999999999999574, -11.48912529306490349, -36.60000000000000142 ) ) ;
#34440 = CARTESIAN_POINT ( 'NONE',  ( -20.94999999999999929, -10.47749788991998088, -206.4278944321438587 ) ) ;
#34441 = ORIENTED_EDGE ( 'NONE', *, *, #256246, .F. ) ;
#34442 = FACE_OUTER_BOUND ( 'NONE', #115047, .T. ) ;
#34443 = ORIENTED_EDGE ( 'NONE', *, *, #84996, .F. ) ;
#34445 = ORIENTED_EDGE ( 'NONE', *, *, #235983, .F. ) ;
#34444 = ORIENTED_EDGE ( 'NONE', *, *, #33509, .F. ) ;
#34446 = CARTESIAN_POINT ( 'NONE',  ( -23.15000000000000213, 67.23127455305835554, -235.8551265064784559 ) ) ;
#34448 = ORIENTED_EDGE ( 'NONE', *, *, #154099, .T. ) ;
#34447 = DIRECTION ( 'NONE',  ( 1.000000000000000000, 0.000000000000000000, 0.000000000000000000 ) ) ;
#34449 = EDGE_CURVE ( 'NONE', #256108, #138529, #249098, .T. ) ;
#34450 = CARTESIAN_POINT ( 'NONE',  ( -20.64999999999999858, 85.50000000001222134, -146.4170766071767389 ) ) ;
#34452 = EDGE_LOOP ( 'NONE', ( #122387, #156066, #197439, #168174 ) ) ;
#34451 = TOROIDAL_SURFACE ( 'NONE', #9467, 0.2000000000000000111, 0.1000000000000000056 ) ;
#34453 = AXIS2_PLACEMENT_3D ( 'NONE', #7730, #218086, #87235 ) ;
#34454 = TOROIDAL_SURFACE ( 'NONE', #96743, 1.900000000000002576, 0.1000000000000000056 ) ;
#34455 = EDGE_CURVE ( 'NONE', #8771, #109129, #149261, .T. ) ;
#34456 = VERTEX_POINT ( 'NONE', #252054 ) ;
#34457 = CARTESIAN_POINT ( 'NONE',  ( -23.25000000000000000, 76.00000000001242029, -166.1231074845243825 ) ) ;
#34458 = DIRECTION ( 'NONE',  ( 0.000000000000000000, 0.000000000000000000, 1.000000000000000000 ) ) ;
#34460 = EDGE_CURVE ( 'NONE', #18158, #205787, #170018, .T. ) ;
#34459 = LINE ( 'NONE', #17424, #236532 ) ;
#34461 = ORIENTED_EDGE ( 'NONE', *, *, #100688, .T. ) ;
#34462 = LINE ( 'NONE', #133525, #3643 ) ;
#34463 = CARTESIAN_POINT ( 'NONE',  ( -18.52186455168988743, -9.481018481431364719, -74.02501647791453365 ) ) ;
#34464 = EDGE_CURVE ( 'NONE', #161528, #92616, #9301, .T. ) ;
#34465 = LINE ( 'NONE', #53989, #68815 ) ;
#34466 = ORIENTED_EDGE ( 'NONE', *, *, #113330, .F. ) ;
#34467 = FACE_OUTER_BOUND ( 'NONE', #166365, .T. ) ;
#34468 = CARTESIAN_POINT ( 'NONE',  ( -18.59999999999999787, 38.30077178631846380, -261.1858881914067751 ) ) ;
#34469 = ORIENTED_EDGE ( 'NONE', *, *, #145216, .T. ) ;
#34470 = CIRCLE ( 'NONE', #51153, 0.1000000000000028644 ) ;
#34471 = VERTEX_POINT ( 'NONE', #137240 ) ;
#34472 = DIRECTION ( 'NONE',  ( 1.000000000000000000, 2.986185139342071370E-16, -6.665775143889693760E-16 ) ) ;
#34473 = ORIENTED_EDGE ( 'NONE', *, *, #134741, .T. ) ;
#34474 = LINE ( 'NONE', #91847, #217860 ) ;
#34475 = EDGE_LOOP ( 'NONE', ( #190714, #9316, #175642, #62577 ) ) ;
#34476 = AXIS2_PLACEMENT_3D ( 'NONE', #48395, #152675, #11874 ) ;
#34477 = VERTEX_POINT ( 'NONE', #155561 ) ;
#34478 = FACE_OUTER_BOUND ( 'NONE', #165635, .T. ) ;
#34479 = EDGE_CURVE ( 'NONE', #105902, #91470, #203287, .T. ) ;
#34480 = CARTESIAN_POINT ( 'NONE',  ( -23.25000000000000000, 7.882824859404637508, -245.3558965132535832 ) ) ;
#34481 = ORIENTED_EDGE ( 'NONE', *, *, #121575, .T. ) ;
#34482 = ORIENTED_EDGE ( 'NONE', *, *, #186650, .F. ) ;
#34483 = CARTESIAN_POINT ( 'NONE',  ( -21.05000000000000071, 1.115600667400684642E-11, -100.5000000000000284 ) ) ;
#34484 = CARTESIAN_POINT ( 'NONE',  ( -18.55121869061588669, 65.67252876774509218, -63.94570419949943840 ) ) ;
#34485 = VERTEX_POINT ( 'NONE', #172577 ) ;
#34486 = B_SPLINE_CURVE_WITH_KNOTS ( 'NONE', 3,
 ( #90903, #175596, #4306, #255046, #104666, #195174, #76468 ),
 .UNSPECIFIED., .F., .F.,
 ( 4, 3, 4 ),
 ( 0.000000000000000000, 3.882884552234317513E-05, 5.798605692158501627E-05 ),
 .UNSPECIFIED. ) ;
#34487 = EDGE_LOOP ( 'NONE', ( #101406, #141936, #4254, #50526 ) ) ;
#34488 = CARTESIAN_POINT ( 'NONE',  ( -18.50000000000000000, -9.500000000000005329, 11.75000000000000000 ) ) ;
#34489 = EDGE_CURVE ( 'NONE', #127497, #145638, #90838, .T. ) ;
#34490 = CARTESIAN_POINT ( 'NONE',  ( 21.00000000000000000, 66.25000000001229239, -157.7731074845244166 ) ) ;
#34491 = CARTESIAN_POINT ( 'NONE',  ( -16.88560720703333473, 9.950564843760847822, -46.14811192086371960 ) ) ;
#34493 = ORIENTED_EDGE ( 'NONE', *, *, #60524, .F. ) ;
#34492 = CARTESIAN_POINT ( 'NONE',  ( 21.14999999999999503, -10.86374996222470379, -206.3339888224507206 ) ) ;
#34494 = CARTESIAN_POINT ( 'NONE',  ( 23.25000000000000000, -11.74999999998883560, -55.25000000000004974 ) ) ;
#34495 = CARTESIAN_POINT ( 'NONE',  ( -22.59999999999999787, -2.381330705637465961, -189.5959759702857923 ) ) ;
#34497 = CARTESIAN_POINT ( 'NONE',  ( 21.00000000000000000, -0.04453801223857078301, -0.3305886640091971196 ) ) ;
#34496 = CARTESIAN_POINT ( 'NONE',  ( 18.59999999999999076, 1.250000000011167511, -41.50000000000000000 ) ) ;
#34498 = CARTESIAN_POINT ( 'NONE',  ( -23.15000000000000213, 85.00000000001207923, -126.6291383618717816 ) ) ;
#34499 = DIRECTION ( 'NONE',  ( 1.000000000000000000, -7.304098846218134667E-16, -4.217023435051625732E-16 ) ) ;
#34500 = B_SPLINE_CURVE_WITH_KNOTS ( 'NONE', 3,
 ( #67021, #146532, #31784, #69605, #129570, #153019, #214242, #212955, #149147, #210399 ),
 .UNSPECIFIED., .F., .F.,
 ( 4, 3, 3, 4 ),
 ( 0.000000000000000000, 0.0002000000000008569359, 0.001000000000082977483, 0.001967863649483338889 ),
 .UNSPECIFIED. ) ;
#34501 = CIRCLE ( 'NONE', #1131, 0.1000000000000028644 ) ;
#34502 = DIRECTION ( 'NONE',  ( 1.000000000000000000, 0.000000000000000000, 0.000000000000000000 ) ) ;
#34503 = EDGE_CURVE ( 'NONE', #128659, #64025, #113824, .T. ) ;
#34504 = CYLINDRICAL_SURFACE ( 'NONE', #17714, 0.09999999999998898659 ) ;
#34505 = CIRCLE ( 'NONE', #142780, 0.1000000000000046685 ) ;
#34506 = VERTEX_POINT ( 'NONE', #173858 ) ;
#34507 = VECTOR ( 'NONE', #243308, 1000.000000000000000 ) ;
#34509 = ORIENTED_EDGE ( 'NONE', *, *, #154940, .T. ) ;
#34508 = CARTESIAN_POINT ( 'NONE',  ( -18.40000000000000213, 64.25000000001202238, -115.6731074845243938 ) ) ;
#34510 = DIRECTION ( 'NONE',  ( 0.000000000000000000, 0.2128009952263603677, -0.9770955615653313941 ) ) ;
#34511 = DIRECTION ( 'NONE',  ( -1.000000000000000000, 0.000000000000000000, 0.000000000000000000 ) ) ;
#34512 = B_SPLINE_CURVE_WITH_KNOTS ( 'NONE', 3,
 ( #149108, #126958, #48693, #147817, #106078, #124399, #27895, #205191, #228649, #184349, #146496, #30443, #245625, #108679, #90390, #129533, #109953, #107384, #85223 ),
 .UNSPECIFIED., .F., .F.,
 ( 4, 3, 3, 3, 3, 3, 4 ),
 ( -2.000416914659873068E-06, 0.000000000000000000, 4.714008503744566487E-05, 9.979203887777271477E-05, 0.0001372215519229485938, 0.0001635031576220933387, 0.0001900083748504131887 ),
 .UNSPECIFIED. ) ;
#34513 = ORIENTED_EDGE ( 'NONE', *, *, #144169, .T. ) ;
#34514 = CIRCLE ( 'NONE', #13644, 0.09999999999998898659 ) ;
#34515 = DIRECTION ( 'NONE',  ( -1.000000000000000000, 0.000000000000000000, 0.000000000000000000 ) ) ;
#34516 = CARTESIAN_POINT ( 'NONE',  ( 21.05000000000000071, 0.6656436123793473270, -212.6810495496487476 ) ) ;
#34517 = ORIENTED_EDGE ( 'NONE', *, *, #252271, .T. ) ;
#34518 = DIRECTION ( 'NONE',  ( -1.000000000000000000, -7.125593699324843413E-30, 1.020425574104004196E-15 ) ) ;
#34519 = DIRECTION ( 'NONE',  ( 0.000000000000000000, 1.000000000000000000, 8.717686153663073805E-15 ) ) ;
#34520 = TOROIDAL_SURFACE ( 'NONE', #138534, 7.800000000000000711, 0.1000000000000000056 ) ;
#34521 = CARTESIAN_POINT ( 'NONE',  ( -21.08479644141223375, 10.07329993697807069, -228.1119308447289598 ) ) ;
#34523 = ORIENTED_EDGE ( 'NONE', *, *, #56466, .F. ) ;
#34522 = DIRECTION ( 'NONE',  ( -1.000000000000000000, -0.000000000000000000, -0.000000000000000000 ) ) ;
#34524 = CARTESIAN_POINT ( 'NONE',  ( -21.05000000000000071, -11.29603075032412463, -63.95210084033612929 ) ) ;
#34526 = ORIENTED_EDGE ( 'NONE', *, *, #237213, .F. ) ;
#34525 = DIRECTION ( 'NONE',  ( -1.000000000000000000, 0.000000000000000000, 0.000000000000000000 ) ) ;
#34527 = AXIS2_PLACEMENT_3D ( 'NONE', #145531, #47709, #225055 ) ;
#34528 = CARTESIAN_POINT ( 'NONE',  ( -17.01825945287482966, 65.95000000001208207, -123.8731074845243683 ) ) ;
#34530 = DIRECTION ( 'NONE',  ( -1.000000000000000000, -2.952720810173289112E-16, 0.000000000000000000 ) ) ;
#34529 = VECTOR ( 'NONE', #248612, 999.9999999999998863 ) ;
#34532 = EDGE_CURVE ( 'NONE', #115992, #241817, #17315, .T. ) ;
#34531 = AXIS2_PLACEMENT_3D ( 'NONE', #84938, #22463, #45850 ) ;
#34533 = DIRECTION ( 'NONE',  ( 0.000000000000000000, 0.000000000000000000, 1.000000000000000000 ) ) ;
#34534 = FACE_OUTER_BOUND ( 'NONE', #98229, .T. ) ;
#34535 = VECTOR ( 'NONE', #129825, 1000.000000000000114 ) ;
#34537 = DIRECTION ( 'NONE',  ( 2.840903330521631775E-16, -0.8454177738465993297, -0.5341055959866553016 ) ) ;
#34536 = CARTESIAN_POINT ( 'NONE',  ( 18.41356215285961895, 8.841736820195405855, -245.4273993276876524 ) ) ;
#34538 = DIRECTION ( 'NONE',  ( 1.000000000000000000, 0.000000000000000000, 0.000000000000000000 ) ) ;
#34539 = SPHERICAL_SURFACE ( 'NONE', #37245, 0.1000000000000000056 ) ;
#34540 = CARTESIAN_POINT ( 'NONE',  ( 20.94999999999999929, 36.65892442174935439, -249.5511627012433848 ) ) ;
#34541 = CARTESIAN_POINT ( 'NONE',  ( -21.55000000000000426, 7.708578643773852157, -179.8499999999999943 ) ) ;
#34542 = DIRECTION ( 'NONE',  ( 0.000000000000000000, 0.2617529984164915779, 0.9651348961777189706 ) ) ;
#34543 = VERTEX_POINT ( 'NONE', #134648 ) ;
#34544 = FACE_OUTER_BOUND ( 'NONE', #15025, .T. ) ;
#34545 = ORIENTED_EDGE ( 'NONE', *, *, #175702, .F. ) ;
#34546 = ORIENTED_EDGE ( 'NONE', *, *, #90347, .T. ) ;
#34547 = EDGE_CURVE ( 'NONE', #93865, #41107, #154293, .T. ) ;
#34548 = FACE_OUTER_BOUND ( 'NONE', #177826, .T. ) ;
#34549 = DIRECTION ( 'NONE',  ( 0.000000000000000000, 0.000000000000000000, 1.000000000000000000 ) ) ;
#34550 = ORIENTED_EDGE ( 'NONE', *, *, #56733, .T. ) ;
#34551 = EDGE_CURVE ( 'NONE', #134482, #24049, #61824, .T. ) ;
#34552 = ORIENTED_EDGE ( 'NONE', *, *, #37696, .F. ) ;
#34553 = CARTESIAN_POINT ( 'NONE',  ( -21.05000000000000071, 30.93406981821913604, -252.0810274548579457 ) ) ;
#34554 = AXIS2_PLACEMENT_3D ( 'NONE', #142567, #103434, #220830 ) ;
#34555 = EDGE_CURVE ( 'NONE', #160408, #46245, #233330, .T. ) ;
#34556 = ORIENTED_EDGE ( 'NONE', *, *, #140979, .T. ) ;
#34557 = ORIENTED_EDGE ( 'NONE', *, *, #117332, .T. ) ;
#34558 = CARTESIAN_POINT ( 'NONE',  ( -20.94999999999999929, -11.48912529306490349, -137.1000000000000227 ) ) ;
#34559 = CARTESIAN_POINT ( 'NONE',  ( -18.59999999999999787, 1.162701749949165642, -108.6000000000000227 ) ) ;
#34560 = DIRECTION ( 'NONE',  ( 0.000000000000000000, 0.000000000000000000, -1.000000000000000000 ) ) ;
#34561 = CARTESIAN_POINT ( 'NONE',  ( 15.52844286134407703, 9.375669526425774336, -15.86779000938593676 ) ) ;
#34562 = AXIS2_PLACEMENT_3D ( 'NONE', #165267, #126124, #205665 ) ;
#34563 = AXIS2_PLACEMENT_3D ( 'NONE', #87695, #185534, #85105 ) ;
#34565 =( NAMED_UNIT ( * ) SI_UNIT ( $, .STERADIAN. ) SOLID_ANGLE_UNIT ( ) );
#34564 = DIRECTION ( 'NONE',  ( 0.000000000000000000, 0.9908441862701420355, 0.1350103645453197554 ) ) ;
#34566 = CARTESIAN_POINT ( 'NONE',  ( -12.29659703204451660, 9.355888454513703323, -83.28864289677802901 ) ) ;
#34568 = ORIENTED_EDGE ( 'NONE', *, *, #84295, .F. ) ;
#34567 = DIRECTION ( 'NONE',  ( -1.020425574104004196E-15, -0.000000000000000000, -1.000000000000000000 ) ) ;
#34570 = FACE_OUTER_BOUND ( 'NONE', #200914, .T. ) ;
#34569 = CYLINDRICAL_SURFACE ( 'NONE', #30142, 0.09999999999999939493 ) ;
#34571 = EDGE_CURVE ( 'NONE', #72649, #6502, #95139, .T. ) ;
#34572 = FACE_BOUND ( 'NONE', #236036, .T. ) ;
#34573 = ORIENTED_EDGE ( 'NONE', *, *, #146510, .T. ) ;
#34574 = CARTESIAN_POINT ( 'NONE',  ( 21.05000000000000071, 8.776282895303632259, -146.1500000000000341 ) ) ;
#34575 = CARTESIAN_POINT ( 'NONE',  ( 20.84999999999999432, 68.97833521811131163, -32.18954208262707795 ) ) ;
#34576 = ORIENTED_EDGE ( 'NONE', *, *, #229330, .T. ) ;
#34578 = EDGE_CURVE ( 'NONE', #54998, #211151, #195114, .T. ) ;
#34577 = VECTOR ( 'NONE', #115540, 1000.000000000000000 ) ;
#34580 = CARTESIAN_POINT ( 'NONE',  ( -5.999999999999938716, 64.35000000001120668, -22.02310748452479316 ) ) ;
#34579 = VECTOR ( 'NONE', #74903, 1000.000000000000000 ) ;
#34581 = DIRECTION ( 'NONE',  ( 0.000000000000000000, -0.9908441862701600211, -0.1350103645451876666 ) ) ;
#34582 = CARTESIAN_POINT ( 'NONE',  ( 14.11444803880196552, 66.54256847116293727, -88.02319054662473263 ) ) ;
#34583 = VERTEX_POINT ( 'NONE', #203635 ) ;
#34584 = ORIENTED_EDGE ( 'NONE', *, *, #157293, .F. ) ;
#34585 = AXIS2_PLACEMENT_3D ( 'NONE', #30888, #110382, #10006 ) ;
#34586 = FACE_OUTER_BOUND ( 'NONE', #180677, .T. ) ;
#34587 = CARTESIAN_POINT ( 'NONE',  ( -17.73285935862574902, 65.14201819622893197, -159.7816692942933230 ) ) ;
#34588 = CARTESIAN_POINT ( 'NONE',  ( 21.05000000000000071, 10.72371710471867701, -41.16491356908760935 ) ) ;
#34589 = DIRECTION ( 'NONE',  ( -0.000000000000000000, 0.9876197685951241256, 0.1568667991644932258 ) ) ;
#34590 = ORIENTED_EDGE ( 'NONE', *, *, #185387, .F. ) ;
#34591 = AXIS2_PLACEMENT_3D ( 'NONE', #54095, #236574, #57934 ) ;
#34592 = EDGE_CURVE ( 'NONE', #401, #203779, #221887, .T. ) ;
#34594 = AXIS2_PLACEMENT_3D ( 'NONE', #79467, #39098, #78185 ) ;
#34593 = LINE ( 'NONE', #210641, #29620 ) ;
#34595 = CARTESIAN_POINT ( 'NONE',  ( -22.50000000000000000, 64.35042919246758686, -170.1231074845244393 ) ) ;
#34596 = CARTESIAN_POINT ( 'NONE',  ( 21.78635804494511419, 0.09900506551883611617, -126.9643385148468440 ) ) ;
#34597 = AXIS2_PLACEMENT_3D ( 'NONE', #107538, #228796, #147964 ) ;
#34598 = FACE_OUTER_BOUND ( 'NONE', #209020, .T. ) ;
#34599 = B_SPLINE_CURVE_WITH_KNOTS ( 'NONE', 3,
 ( #1126, #80666, #201927, #42850, #122391, #23315, #102789 ),
 .UNSPECIFIED., .F., .F.,
 ( 4, 3, 4 ),
 ( 0.000000000000000000, 0.0009834301579440011751, 0.001767853679402673663 ),
 .UNSPECIFIED. ) ;
#34600 = AXIS2_PLACEMENT_3D ( 'NONE', #131604, #33843, #53355 ) ;
#34601 = VECTOR ( 'NONE', #211664, 1000.000000000000000 ) ;
#34602 = AXIS2_PLACEMENT_3D ( 'NONE', #57464, #52324, #91480 ) ;
#34603 = EDGE_CURVE ( 'NONE', #2617, #252276, #124116, .T. ) ;
#34605 = ORIENTED_EDGE ( 'NONE', *, *, #217815, .T. ) ;
#34604 = CARTESIAN_POINT ( 'NONE',  ( 18.49999999999999645, -1.164121893230052995, -175.4148480855716059 ) ) ;
#34606 = PLANE ( 'NONE',  #76805 ) ;
#34607 = DIRECTION ( 'NONE',  ( 0.000000000000000000, 6.982962677686267499E-15, -1.000000000000000000 ) ) ;
#34608 = FACE_OUTER_BOUND ( 'NONE', #170563, .T. ) ;
#34609 = LINE ( 'NONE', #35892, #184525 ) ;
#34610 = CYLINDRICAL_SURFACE ( 'NONE', #133627, 0.1000000000000028644 ) ;
#34612 = ORIENTED_EDGE ( 'NONE', *, *, #85058, .F. ) ;
#34611 = CARTESIAN_POINT ( 'NONE',  ( -20.64999999999999858, 11.48697431424113446, -220.1440440112397994 ) ) ;
#34613 = LINE ( 'NONE', #55398, #67457 ) ;
#34614 = CARTESIAN_POINT ( 'NONE',  ( 23.15000000000000213, -11.38316329222462464, -203.4791315943886048 ) ) ;
#34615 = DIRECTION ( 'NONE',  ( 0.000000000000000000, -0.9908441862701791170, 0.1350103645450472789 ) ) ;
#34616 = ADVANCED_FACE ( 'NONE', ( #242747 ), #144925, .F. ) ;
#34617 = VERTEX_POINT ( 'NONE', #42015 ) ;
#34618 = CARTESIAN_POINT ( 'NONE',  ( 23.14999999999999147, 1.115600667400684642E-11, -33.50000000000000000 ) ) ;
#34619 = CYLINDRICAL_SURFACE ( 'NONE', #185951, 0.09999999999999939493 ) ;
#34620 = CARTESIAN_POINT ( 'NONE',  ( 20.00000000000000355, 1.350000000000000089, 21.90000000000000213 ) ) ;
#34621 = CARTESIAN_POINT ( 'NONE',  ( 23.14999999999999503, 11.75000000001116263, -21.75000000000000355 ) ) ;
#34622 = EDGE_CURVE ( 'NONE', #226312, #74036, #157729, .T. ) ;
#34623 = DIRECTION ( 'NONE',  ( 1.000000000000000000, 0.000000000000000000, 0.000000000000000000 ) ) ;
#34624 = VECTOR ( 'NONE', #213993, 1000.000000000000000 ) ;
#34625 = CIRCLE ( 'NONE', #222013, 4.300000000000025580 ) ;
#34626 = EDGE_CURVE ( 'NONE', #216194, #184441, #139793, .T. ) ;
#34627 = DIRECTION ( 'NONE',  ( -1.000000000000000000, 2.952720810173289112E-16, 2.061873921506763405E-30 ) ) ;
#34628 = CIRCLE ( 'NONE', #242888, 0.1000000000000028644 ) ;
#34629 = VECTOR ( 'NONE', #235834, 1000.000000000000000 ) ;
#34630 = ORIENTED_EDGE ( 'NONE', *, *, #252508, .F. ) ;
#34631 = VERTEX_POINT ( 'NONE', #104504 ) ;
#34632 = FACE_OUTER_BOUND ( 'NONE', #70770, .T. ) ;
#34633 = CARTESIAN_POINT ( 'NONE',  ( -22.39999999999999858, 11.75000000000000000, -3.469446951953614189E-15 ) ) ;
#34634 = EDGE_CURVE ( 'NONE', #110389, #178700, #183425, .T. ) ;
#34635 = CARTESIAN_POINT ( 'NONE',  ( 18.39999999999999858, -0.7490476236415681832, -242.2033265267442061 ) ) ;
#34636 = DIRECTION ( 'NONE',  ( 1.000000000000000000, -0.000000000000000000, -0.000000000000000000 ) ) ;
#34637 = FACE_OUTER_BOUND ( 'NONE', #134484, .T. ) ;
#34638 = EDGE_CURVE ( 'NONE', #34148, #157381, #249274, .T. ) ;
#34640 = ADVANCED_FACE ( 'NONE', ( #61564 ), #291, .T. ) ;
#34639 = FACE_OUTER_BOUND ( 'NONE', #136829, .T. ) ;
#34641 = CARTESIAN_POINT ( 'NONE',  ( -16.94107738177415712, 10.01423928514777728, -113.0500000000000398 ) ) ;
#34642 = LINE ( 'NONE', #213242, #256804 ) ;
#34643 = EDGE_LOOP ( 'NONE', ( #217292, #207456, #205201, #253407, #201040 ) ) ;
#34644 = CARTESIAN_POINT ( 'NONE',  ( -20.94999999999999929, -1.835341550213257733, -45.05515129256298223 ) ) ;
#34645 = EDGE_CURVE ( 'NONE', #37547, #147319, #70229, .T. ) ;
#34646 = VECTOR ( 'NONE', #217093, 1000.000000000000000 ) ;
#34647 = ORIENTED_EDGE ( 'NONE', *, *, #99840, .T. ) ;
#34648 = CARTESIAN_POINT ( 'NONE',  ( -16.93388492042257809, 9.988541822527057690, -154.9005451231862196 ) ) ;
#34649 = FACE_OUTER_BOUND ( 'NONE', #73185, .T. ) ;
#34650 = DIRECTION ( 'NONE',  ( -1.073024830501117725E-15, -0.000000000000000000, -1.000000000000000000 ) ) ;
#34652 = ORIENTED_EDGE ( 'NONE', *, *, #149586, .T. ) ;
#34651 = DIRECTION ( 'NONE',  ( 0.000000000000000000, 0.000000000000000000, -1.000000000000000000 ) ) ;
#34653 = EDGE_CURVE ( 'NONE', #24049, #188383, #228433, .T. ) ;
#34654 = CARTESIAN_POINT ( 'NONE',  ( -16.87331047859651179, 66.05000000001207638, -123.8731074845243683 ) ) ;
#34655 = CARTESIAN_POINT ( 'NONE',  ( 21.08832698747859169, 22.05205433789857850, -231.7715725143952170 ) ) ;
#34656 = CARTESIAN_POINT ( 'NONE',  ( 18.49362639424906263, 85.44260436789974733, -62.75866655101247460 ) ) ;
#34657 = EDGE_LOOP ( 'NONE', ( #243766, #79910, #70178, #76798 ) ) ;
#34658 = LINE ( 'NONE', #195013, #241605 ) ;
#34659 = DIRECTION ( 'NONE',  ( 1.000000000000000000, 0.000000000000000000, 0.000000000000000000 ) ) ;
#34660 = CARTESIAN_POINT ( 'NONE',  ( 23.15000000000000213, 88.41227409416141825, -72.52310748452423184 ) ) ;
#34661 = CARTESIAN_POINT ( 'NONE',  ( -18.41799967126743454, 85.50000000001233502, -162.9910376712692539 ) ) ;
#34662 = VECTOR ( 'NONE', #190252, 1000.000000000000000 ) ;
#34663 = CARTESIAN_POINT ( 'NONE',  ( 18.59999999999998366, 7.021664781911246322, -104.3335654018973315 ) ) ;
#34664 = AXIS2_PLACEMENT_3D ( 'NONE', #256827, #118684, #15746 ) ;
#34665 = EDGE_LOOP ( 'NONE', ( #111568, #233409, #5719, #131872 ) ) ;
#34666 = DIRECTION ( 'NONE',  ( 0.000000000000000000, -6.547589603894048205E-15, 1.000000000000000000 ) ) ;
#34667 = CARTESIAN_POINT ( 'NONE',  ( -16.83199030136657726, 66.06935196689842371, -90.25070646186692613 ) ) ;
#34668 = ORIENTED_EDGE ( 'NONE', *, *, #258052, .F. ) ;
#34669 = DIRECTION ( 'NONE',  ( 0.000000000000000000, 0.000000000000000000, 1.000000000000000000 ) ) ;
#34670 = ADVANCED_FACE ( 'NONE', ( #82846 ), #99208, .T. ) ;
#34671 = EDGE_CURVE ( 'NONE', #108576, #154572, #190384, .T. ) ;
#34672 = FACE_OUTER_BOUND ( 'NONE', #101608, .T. ) ;
#34673 = DIRECTION ( 'NONE',  ( 0.000000000000000000, -0.4999999999999689138, 0.8660254037844565822 ) ) ;
#34674 = ORIENTED_EDGE ( 'NONE', *, *, #199622, .T. ) ;
#34675 = LINE ( 'NONE', #52923, #38086 ) ;
#34676 = CARTESIAN_POINT ( 'NONE',  ( 21.05000000000000071, 8.926614585098253229, -41.97168301922312850 ) ) ;
#34677 = EDGE_CURVE ( 'NONE', #17591, #229996, #240882, .T. ) ;
#34678 = CIRCLE ( 'NONE', #22207, 0.1999999999999985401 ) ;
#34679 = ORIENTED_EDGE ( 'NONE', *, *, #53523, .T. ) ;
#34680 = CIRCLE ( 'NONE', #247028, 0.6000000000000015321 ) ;
#34681 = AXIS2_PLACEMENT_3D ( 'NONE', #1033, #79300, #257902 ) ;
#34682 = ORIENTED_EDGE ( 'NONE', *, *, #210966, .F. ) ;
#34683 = FACE_OUTER_BOUND ( 'NONE', #117405, .T. ) ;
#34684 = FACE_OUTER_BOUND ( 'NONE', #214055, .T. ) ;
#34686 = ORIENTED_EDGE ( 'NONE', *, *, #173175, .F. ) ;
#34685 = DIRECTION ( 'NONE',  ( 0.000000000000000000, 0.1298341882520022694, 0.9915357197604852679 ) ) ;
#34687 = CARTESIAN_POINT ( 'NONE',  ( 18.69999999999999929, 1.149999999999999911, 16.60000000000000142 ) ) ;
#34688 = UNCERTAINTY_MEASURE_WITH_UNIT (LENGTH_MEASURE( 1.000000000000000082E-05 ), #476, 'distance_accuracy_value', 'NONE');
#34689 = CARTESIAN_POINT ( 'NONE',  ( 21.15000000000005542, 87.50449464844290048, -34.18759587077607165 ) ) ;
#34690 = CARTESIAN_POINT ( 'NONE',  ( 21.05000000000000071, 47.74710514101221293, -244.5837943500090716 ) ) ;
#34691 = FACE_OUTER_BOUND ( 'NONE', #149359, .T. ) ;
#34692 = CIRCLE ( 'NONE', #180424, 0.1000000000000063199 ) ;
#34693 = EDGE_CURVE ( 'NONE', #193316, #14866, #45238, .T. ) ;
#34694 = DIRECTION ( 'NONE',  ( 1.000000000000000000, -7.304098846218134667E-16, -5.100424963727256530E-30 ) ) ;
#34696 = DIRECTION ( 'NONE',  ( 0.000000000000000000, -6.982962677686266711E-15, 1.000000000000000000 ) ) ;
#34695 = VECTOR ( 'NONE', #26758, 1000.000000000000000 ) ;
#34698 = ORIENTED_EDGE ( 'NONE', *, *, #17075, .F. ) ;
#34697 = DIRECTION ( 'NONE',  ( 0.000000000000000000, 0.000000000000000000, 1.000000000000000000 ) ) ;
#34699 = EDGE_LOOP ( 'NONE', ( #69110, #148040, #121039, #132937 ) ) ;
#34702 = CARTESIAN_POINT ( 'NONE',  ( 22.88900146558018989, 8.703904791112817563, -20.84999999999999432 ) ) ;
#34701 = CARTESIAN_POINT ( 'NONE',  ( -21.44999999999999929, 29.23678660621682113, -237.4641088729839282 ) ) ;
#34700 = AXIS2_PLACEMENT_3D ( 'NONE', #106135, #185702, #219672 ) ;
#34704 = ORIENTED_EDGE ( 'NONE', *, *, #231874, .T. ) ;
#34703 = CARTESIAN_POINT ( 'NONE',  ( -23.15000000000000213, 67.23127455305835554, -235.8551265064784559 ) ) ;
#34705 = EDGE_CURVE ( 'NONE', #248947, #111286, #11961, .T. ) ;
#34706 = ORIENTED_EDGE ( 'NONE', *, *, #108050, .F. ) ;
#34707 = CARTESIAN_POINT ( 'NONE',  ( -16.78270389226384651, 66.05262738339554573, -182.6819004476129464 ) ) ;
#34708 = LINE ( 'NONE', #235434, #22213 ) ;
#34709 = FACE_OUTER_BOUND ( 'NONE', #90007, .T. ) ;
#34710 = VECTOR ( 'NONE', #36133, 1000.000000000000000 ) ;
#34711 = DIRECTION ( 'NONE',  ( 0.000000000000000000, 0.000000000000000000, -1.000000000000000000 ) ) ;
#34712 = ADVANCED_FACE ( 'NONE', ( #181998 ), #145419, .T. ) ;
#34713 = DIRECTION ( 'NONE',  ( -1.000000000000000000, 5.945622153099073960E-16, -5.981866248895712861E-16 ) ) ;
#34714 = PLANE ( 'NONE',  #136205 ) ;
#34715 = AXIS2_PLACEMENT_3D ( 'NONE', #104783, #106075, #228647 ) ;
#34716 = EDGE_CURVE ( 'NONE', #128122, #21732, #222362, .T. ) ;
#34717 = AXIS2_PLACEMENT_3D ( 'NONE', #94664, #174257, #38554 ) ;
#34718 = AXIS2_PLACEMENT_3D ( 'NONE', #108093, #88489, #148502 ) ;
#34720 = VECTOR ( 'NONE', #202640, 1000.000000000000000 ) ;
#34719 = CARTESIAN_POINT ( 'NONE',  ( 18.79999999999999716, 1.885425182446133885, -11.49641995933507843 ) ) ;
#34721 = ORIENTED_EDGE ( 'NONE', *, *, #171769, .T. ) ;
#34722 = ORIENTED_EDGE ( 'NONE', *, *, #111768, .F. ) ;
#34723 = EDGE_CURVE ( 'NONE', #93175, #109, #161151, .T. ) ;
#34724 = FACE_OUTER_BOUND ( 'NONE', #253832, .T. ) ;
#34725 = ORIENTED_EDGE ( 'NONE', *, *, #200976, .T. ) ;
#34726 = CARTESIAN_POINT ( 'NONE',  ( 20.94999999999999574, 79.26035508877829727, -236.0091442494974956 ) ) ;
#34727 = VERTEX_POINT ( 'NONE', #62056 ) ;
#34728 = EDGE_CURVE ( 'NONE', #79572, #103016, #5898, .T. ) ;
#34730 = EDGE_CURVE ( 'NONE', #46490, #88642, #106277, .T. ) ;
#34729 = EDGE_CURVE ( 'NONE', #96922, #203545, #221101, .T. ) ;
#34731 = CARTESIAN_POINT ( 'NONE',  ( -16.94275863009466576, 9.989496048673542461, -79.60830261795892682 ) ) ;
#34732 = ORIENTED_EDGE ( 'NONE', *, *, #154185, .T. ) ;
#34733 = CARTESIAN_POINT ( 'NONE',  ( -20.94999999999999929, 1.115600667400684642E-11, -55.20000000000000284 ) ) ;
#34734 = ORIENTED_EDGE ( 'NONE', *, *, #243629, .T. ) ;
#34735 = LINE ( 'NONE', #51673, #142155 ) ;
#34736 = ORIENTED_EDGE ( 'NONE', *, *, #209710, .F. ) ;
#34737 = DIRECTION ( 'NONE',  ( -1.000000000000000000, 0.000000000000000000, -0.000000000000000000 ) ) ;
#34738 = CIRCLE ( 'NONE', #184540, 0.09999999999999939493 ) ;
#34739 = ORIENTED_EDGE ( 'NONE', *, *, #131679, .F. ) ;
#34740 = CIRCLE ( 'NONE', #155567, 11.75000000000000000 ) ;
#34741 = DIRECTION ( 'NONE',  ( 0.000000000000000000, 1.000000000000000000, 6.982962677686266711E-15 ) ) ;
#34742 = EDGE_LOOP ( 'NONE', ( #143964, #144133, #93515, #119356 ) ) ;
#34745 = VERTEX_POINT ( 'NONE', #205382 ) ;
#34744 = FACE_OUTER_BOUND ( 'NONE', #214921, .T. ) ;
#34743 = FACE_OUTER_BOUND ( 'NONE', #7127, .T. ) ;
#34746 = AXIS2_PLACEMENT_3D ( 'NONE', #203659, #122852, #5426 ) ;
#34747 = EDGE_CURVE ( 'NONE', #197418, #109819, #132552, .T. ) ;
#34748 = CARTESIAN_POINT ( 'NONE',  ( -20.94999999999999929, 64.25000000001146816, -42.80697314750249660 ) ) ;
#34749 = EDGE_CURVE ( 'NONE', #234902, #224848, #111699, .T. ) ;
#34750 = EDGE_LOOP ( 'NONE', ( #251954, #173884, #228157, #99097 ) ) ;
#34751 = ORIENTED_EDGE ( 'NONE', *, *, #94673, .F. ) ;
#34752 = VECTOR ( 'NONE', #211807, 1000.000000000000000 ) ;
#34753 = EDGE_CURVE ( 'NONE', #236113, #184466, #186740, .T. ) ;
#34754 = VECTOR ( 'NONE', #11754, 1000.000000000000000 ) ;
#34755 = CARTESIAN_POINT ( 'NONE',  ( 21.07094088545369104, 0.09889370255222153239, 6.320167221917142975 ) ) ;
#34756 = ORIENTED_EDGE ( 'NONE', *, *, #58447, .T. ) ;
#34757 = DIRECTION ( 'NONE',  ( -0.000000000000000000, 0.000000000000000000, 1.000000000000000000 ) ) ;
#34758 = LINE ( 'NONE', #217195, #47006 ) ;
#34760 = ADVANCED_FACE ( 'NONE', ( #123307 ), #63310, .T. ) ;
#34759 = CARTESIAN_POINT ( 'NONE',  ( -22.47071067811865319, 68.27992525551387359, -103.1221999392269737 ) ) ;
#34761 = DIRECTION ( 'NONE',  ( 1.000000000000000000, 0.000000000000000000, 0.000000000000000000 ) ) ;
#34762 = AXIS2_PLACEMENT_3D ( 'NONE', #235675, #32391, #230565 ) ;
#34763 = CARTESIAN_POINT ( 'NONE',  ( -16.87036670365549895, 66.01058118071040326, -124.0026676018264169 ) ) ;
#34764 = EDGE_CURVE ( 'NONE', #28860, #179923, #4618, .T. ) ;
#34765 = AXIS2_PLACEMENT_3D ( 'NONE', #218167, #181650, #142494 ) ;
#34766 = ORIENTED_EDGE ( 'NONE', *, *, #20855, .F. ) ;
#34767 = AXIS2_PLACEMENT_3D ( 'NONE', #231392, #252210, #211827 ) ;
#34768 = CIRCLE ( 'NONE', #184750, 3.999999999999996447 ) ;
#34769 = CYLINDRICAL_SURFACE ( 'NONE', #190139, 0.09999999999999939493 ) ;
#34770 = DIRECTION ( 'NONE',  ( 6.938893903907991995E-14, 0.000000000000000000, -1.000000000000000000 ) ) ;
#34771 = CARTESIAN_POINT ( 'NONE',  ( 18.59117750673696534, 10.33248238083634796, -139.5948465439131780 ) ) ;
#34772 = ORIENTED_EDGE ( 'NONE', *, *, #82864, .T. ) ;
#34773 = DIRECTION ( 'NONE',  ( -1.000000000000000000, 0.000000000000000000, 0.000000000000000000 ) ) ;
#34774 = EDGE_LOOP ( 'NONE', ( #103044, #177176, #191614, #76452, #139880, #41186 ) ) ;
#34775 = DIRECTION ( 'NONE',  ( -1.000000000000000000, 0.000000000000000000, 0.000000000000000000 ) ) ;
#34777 = VERTEX_POINT ( 'NONE', #60737 ) ;
#34776 = TOROIDAL_SURFACE ( 'NONE', #172172, 0.2000000000000000111, 0.1000000000000000056 ) ;
#34778 = CARTESIAN_POINT ( 'NONE',  ( -17.11825945287482753, 65.95000000001188312, -90.37310748452438247 ) ) ;
#34779 = CARTESIAN_POINT ( 'NONE',  ( 18.59999999999999076, 77.83585931145498193, -24.41866831572578533 ) ) ;
#34781 = ORIENTED_EDGE ( 'NONE', *, *, #138256, .F. ) ;
#34780 = CARTESIAN_POINT ( 'NONE',  ( -18.59999999999999787, -1.263275465206102233, -175.4018646667464338 ) ) ;
#34782 = ADVANCED_FACE ( 'NONE', ( #219822 ), #41226, .T. ) ;
#34783 = ORIENTED_EDGE ( 'NONE', *, *, #45630, .F. ) ;
#34784 = AXIS2_PLACEMENT_3D ( 'NONE', #38103, #53797, #133344 ) ;
#34785 = DIRECTION ( 'NONE',  ( -0.000000000000000000, -0.000000000000000000, -1.000000000000000000 ) ) ;
#34786 = DIRECTION ( 'NONE',  ( 1.000000000000000000, 0.000000000000000000, 0.000000000000000000 ) ) ;
#34787 = ORIENTED_EDGE ( 'NONE', *, *, #81416, .F. ) ;
#34788 = ADVANCED_FACE ( 'NONE', ( #89295 ), #50167, .F. ) ;
#34789 = CIRCLE ( 'NONE', #188886, 1.500000000000001332 ) ;
#34790 = DIRECTION ( 'NONE',  ( 0.000000000000000000, 6.982962677686266711E-15, -1.000000000000000000 ) ) ;
#34791 = CARTESIAN_POINT ( 'NONE',  ( -23.25000000000000355, 64.25000000001233502, -160.7731074845244450 ) ) ;
#34792 = ORIENTED_EDGE ( 'NONE', *, *, #103249, .F. ) ;
#34793 = DIRECTION ( 'NONE',  ( 0.000000000000000000, -0.9908441862701605762, 0.1350103645451835310 ) ) ;
#34794 = AXIS2_PLACEMENT_3D ( 'NONE', #72630, #214675, #232989 ) ;
#34795 = ORIENTED_EDGE ( 'NONE', *, *, #185543, .F. ) ;
#34796 = CIRCLE ( 'NONE', #93032, 12.87499999999999822 ) ;
#34797 = TOROIDAL_SURFACE ( 'NONE', #151322, 0.9750000000000019762, 0.1000000000000000056 ) ;
#34798 = DIRECTION ( 'NONE',  ( 1.000000000000000000, 0.000000000000000000, -0.000000000000000000 ) ) ;
#34799 = DIRECTION ( 'NONE',  ( -0.7071067811865473507, -0.3338907855510733769, -0.6233112732207618523 ) ) ;
#34800 = EDGE_CURVE ( 'NONE', #198367, #149398, #51432, .T. ) ;
#34802 = ORIENTED_EDGE ( 'NONE', *, *, #121067, .T. ) ;
#34801 = LINE ( 'NONE', #232991, #234705 ) ;
#34803 = DIRECTION ( 'NONE',  ( 1.000000000000000000, -0.000000000000000000, -0.000000000000000000 ) ) ;
#34804 = CARTESIAN_POINT ( 'NONE',  ( -22.41119224318417125, 1.115600667400684642E-11, -155.8504291924551808 ) ) ;
#34805 = CARTESIAN_POINT ( 'NONE',  ( 18.59999999999999076, 6.650000000011155876, -88.15000000000004832 ) ) ;
#34807 = FACE_OUTER_BOUND ( 'NONE', #136749, .T. ) ;
#34806 = DIRECTION ( 'NONE',  ( -1.000000000000000000, 0.000000000000000000, 0.000000000000000000 ) ) ;
#34808 = PLANE ( 'NONE',  #186208 ) ;
#34809 = DIRECTION ( 'NONE',  ( 1.000000000000000000, 0.000000000000000000, 0.000000000000000000 ) ) ;
#34810 = AXIS2_PLACEMENT_3D ( 'NONE', #64858, #25745, #105226 ) ;
#34811 = CARTESIAN_POINT ( 'NONE',  ( 18.41416235934318379, 85.50000000001136868, -29.42291809330221497 ) ) ;
#34812 = TOROIDAL_SURFACE ( 'NONE', #242887, 0.6000000000000009770, 0.1000000000000000056 ) ;
#34813 = DIRECTION ( 'NONE',  ( -0.000000000000000000, 6.982962677686266711E-15, -1.000000000000000000 ) ) ;
#34814 = AXIS2_PLACEMENT_3D ( 'NONE', #92168, #231701, #33535 ) ;
#34815 = ORIENTED_EDGE ( 'NONE', *, *, #31941, .T. ) ;
#34816 = ORIENTED_EDGE ( 'NONE', *, *, #43261, .T. ) ;
#34817 = DIRECTION ( 'NONE',  ( 0.000000000000000000, 0.000000000000000000, -1.000000000000000000 ) ) ;
#34819 = ORIENTED_EDGE ( 'NONE', *, *, #123186, .F. ) ;
#34818 = DIRECTION ( 'NONE',  ( 0.000000000000000000, 0.8700118002898321601, -0.4930308989875230030 ) ) ;
#34820 = ORIENTED_EDGE ( 'NONE', *, *, #29979, .T. ) ;
#34821 = CARTESIAN_POINT ( 'NONE',  ( 21.05000000000000071, 5.500000000011153745, -54.59473398108690390 ) ) ;
#34822 = ORIENTED_EDGE ( 'NONE', *, *, #85730, .T. ) ;
#34823 = DIRECTION ( 'NONE',  ( 0.000000000000000000, 0.9915357197604982575, -0.1298341882519033486 ) ) ;
#34824 = ORIENTED_EDGE ( 'NONE', *, *, #69943, .F. ) ;
#34825 =( LENGTH_UNIT ( ) NAMED_UNIT ( * ) SI_UNIT ( .MILLI., .METRE. ) );
#34826 = DIRECTION ( 'NONE',  ( 0.000000000000000000, 1.000000000000000000, 6.982962677686266711E-15 ) ) ;
#34828 = VERTEX_POINT ( 'NONE', #168889 ) ;
#34827 = ORIENTED_EDGE ( 'NONE', *, *, #122966, .T. ) ;
#34829 = ORIENTED_EDGE ( 'NONE', *, *, #24163, .F. ) ;
#34830 = ORIENTED_EDGE ( 'NONE', *, *, #178780, .F. ) ;
#34831 = VERTEX_POINT ( 'NONE', #209249 ) ;
#34832 = CARTESIAN_POINT ( 'NONE',  ( 21.05000000000000071, 11.75000000000000711, -26.48519422934605316 ) ) ;
#34833 = DIRECTION ( 'NONE',  ( 0.000000000000000000, 0.9908441862701600211, 0.1350103645451876944 ) ) ;
#34834 = TOROIDAL_SURFACE ( 'NONE', #101391, 11.70000000000000107, 0.1000000000000000056 ) ;
#34835 = CARTESIAN_POINT ( 'NONE',  ( -16.86733706339143524, 30.26070006106851551, -234.8180300960572708 ) ) ;
#34837 = EDGE_LOOP ( 'NONE', ( #228465, #107901, #111217, #222328 ) ) ;
#34836 = DIRECTION ( 'NONE',  ( 1.000000000000000000, 0.000000000000000000, 0.000000000000000000 ) ) ;
#34838 = CARTESIAN_POINT ( 'NONE',  ( 20.94999999999999929, 6.650000000011155876, -77.01702717044007329 ) ) ;
#34839 = CARTESIAN_POINT ( 'NONE',  ( 21.05000000000000071, 11.77895973109482952, -206.1023438919106070 ) ) ;
#34841 = ORIENTED_EDGE ( 'NONE', *, *, #134740, .T. ) ;
#34840 = CARTESIAN_POINT ( 'NONE',  ( 20.95378194480896639, 10.53491199155394220, -141.5650541481478797 ) ) ;
#34842 = DIRECTION ( 'NONE',  ( 0.000000000000000000, 0.9876197685951252359, -0.1568667991644863424 ) ) ;
#34843 = ORIENTED_EDGE ( 'NONE', *, *, #122979, .T. ) ;
#34844 = CARTESIAN_POINT ( 'NONE',  ( -18.59999999999999787, 14.05000000001115623, -39.01369507076099552 ) ) ;
#34846 = VERTEX_POINT ( 'NONE', #149306 ) ;
#34845 = DIRECTION ( 'NONE',  ( 0.000000000000000000, 4.440892098500631684E-15, -1.000000000000000000 ) ) ;
#34847 = CARTESIAN_POINT ( 'NONE',  ( -18.40000000000000213, 11.74999999999998224, -12.65000000000000213 ) ) ;
#34848 = CARTESIAN_POINT ( 'NONE',  ( -16.89797118371633999, 9.976380722655555644, -113.0627066324413761 ) ) ;
#34849 = EDGE_CURVE ( 'NONE', #74203, #101747, #74331, .T. ) ;
#34850 = VERTEX_POINT ( 'NONE', #68470 ) ;
#34852 = CARTESIAN_POINT ( 'NONE',  ( -18.41418431465368144, -9.499999999989071853, -140.6001893912215053 ) ) ;
#34851 = CARTESIAN_POINT ( 'NONE',  ( 21.05000000000000071, 5.500000000011153745, -155.0947339810869323 ) ) ;
#34853 = VECTOR ( 'NONE', #194769, 1000.000000000000000 ) ;
#34854 = DIRECTION ( 'NONE',  ( -1.000000000000000000, -0.000000000000000000, -0.000000000000000000 ) ) ;
#34855 = AXIS2_PLACEMENT_3D ( 'NONE', #209758, #165507, #67670 ) ;
#34856 = DIRECTION ( 'NONE',  ( 0.000000000000000000, 1.000000000000000000, 6.982962677686266711E-15 ) ) ;
#34857 = DIRECTION ( 'NONE',  ( 0.000000000000000000, 0.000000000000000000, 1.000000000000000000 ) ) ;
#34858 = ORIENTED_EDGE ( 'NONE', *, *, #236285, .F. ) ;
#34860 = ORIENTED_EDGE ( 'NONE', *, *, #190774, .F. ) ;
#34859 = VECTOR ( 'NONE', #202261, 999.9999999999998863 ) ;
#34861 = B_SPLINE_CURVE_WITH_KNOTS ( 'NONE', 3,
 ( #115830, #157569, #194108, #158832, #37593, #137939, #154984, #76689, #234481, #156275 ),
 .UNSPECIFIED., .F., .F.,
 ( 4, 3, 3, 4 ),
 ( 0.000000000000000000, 3.394313611811197040E-05, 6.779740500699018625E-05, 0.0001049857339142625727 ),
 .UNSPECIFIED. ) ;
#34862 = CARTESIAN_POINT ( 'NONE',  ( 20.94999999999999929, 8.926614585087097709, -8.471683019223119615 ) ) ;
#34863 = DIRECTION ( 'NONE',  ( 0.000000000000000000, 0.000000000000000000, -1.000000000000000000 ) ) ;
#34864 = ORIENTED_EDGE ( 'NONE', *, *, #157193, .T. ) ;
#34865 = DIRECTION ( 'NONE',  ( 1.000000000000000000, -0.000000000000000000, -0.000000000000000000 ) ) ;
#34866 = ORIENTED_EDGE ( 'NONE', *, *, #4086, .T. ) ;
#34867 = EDGE_CURVE ( 'NONE', #96909, #19541, #207994, .T. ) ;
#34868 = CARTESIAN_POINT ( 'NONE',  ( -20.94999999999999929, 76.00000000001170974, -69.52310748452431710 ) ) ;
#34869 = DIRECTION ( 'NONE',  ( 0.000000000000000000, -0.9893560106964500722, 0.1455152366551550613 ) ) ;
#34870 = EDGE_CURVE ( 'NONE', #147215, #170466, #148003, .T. ) ;
#34871 = ORIENTED_EDGE ( 'NONE', *, *, #198640, .T. ) ;
#34872 = AXIS2_PLACEMENT_3D ( 'NONE', #238982, #236401, #95604 ) ;
#34873 = CARTESIAN_POINT ( 'NONE',  ( -16.83794237512072911, 66.07364077890511567, -190.7195653258254708 ) ) ;
#34874 =( NAMED_UNIT ( * ) PLANE_ANGLE_UNIT ( ) SI_UNIT ( $, .RADIAN. ) );
#34875 = EDGE_CURVE ( 'NONE', #133529, #75581, #192277, .T. ) ;
#34876 = VECTOR ( 'NONE', #79134, 1000.000000000000000 ) ;
#34877 = VERTEX_POINT ( 'NONE', #227525 ) ;
#34878 = ORIENTED_EDGE ( 'NONE', *, *, #240733, .F. ) ;
#34879 = CIRCLE ( 'NONE', #247220, 0.09999999999998898659 ) ;
#34880 = ORIENTED_EDGE ( 'NONE', *, *, #58526, .F. ) ;
#34881 = TOROIDAL_SURFACE ( 'NONE', #5779, 0.2000000000000000111, 0.1000000000000000056 ) ;
#34882 = EDGE_CURVE ( 'NONE', #245137, #40042, #191003, .T. ) ;
#34883 = DIRECTION ( 'NONE',  ( -0.000000000000000000, -1.000000000000000000, 6.308085367188393199E-16 ) ) ;
#34884 = CYLINDRICAL_SURFACE ( 'NONE', #115823, 0.1000000000000055844 ) ;
#34885 = CARTESIAN_POINT ( 'NONE',  ( -20.94999999999999929, 68.59681812508419796, -224.1344059333694361 ) ) ;
#34887 = EDGE_CURVE ( 'NONE', #101749, #4681, #187150, .T. ) ;
#34886 = DIRECTION ( 'NONE',  ( 1.000000000000000000, 0.000000000000000000, 0.000000000000000000 ) ) ;
#34888 = CARTESIAN_POINT ( 'NONE',  ( 12.33938619321247643, 66.63927620602599688, -119.2091802899176542 ) ) ;
#34890 = CARTESIAN_POINT ( 'NONE',  ( 23.24999999999999645, 8.822561741677553471, -113.1500000000000483 ) ) ;
#34889 = DIRECTION ( 'NONE',  ( 0.000000000000000000, 0.000000000000000000, 1.000000000000000000 ) ) ;
#34892 = ORIENTED_EDGE ( 'NONE', *, *, #93102, .T. ) ;
#34891 = CARTESIAN_POINT ( 'NONE',  ( -18.39999999999999858, 85.60000000001160458, -62.49103808782458458 ) ) ;
#34893 = DIRECTION ( 'NONE',  ( 0.000000000000000000, -0.9126074666063660468, -0.4088369013363524762 ) ) ;
#34894 = ORIENTED_EDGE ( 'NONE', *, *, #231933, .T. ) ;
#34895 = ADVANCED_FACE ( 'NONE', ( #12367 ), #8498, .T. ) ;
#34896 = DIRECTION ( 'NONE',  ( 0.000000000000000000, 0.000000000000000000, 1.000000000000000000 ) ) ;
#34897 = ORIENTED_EDGE ( 'NONE', *, *, #71221, .T. ) ;
#34898 = VERTEX_POINT ( 'NONE', #30644 ) ;
#34899 = DIRECTION ( 'NONE',  ( 0.000000000000000000, 0.9955484899852913294, -0.09425075112701486457 ) ) ;
#34901 = AXIS2_PLACEMENT_3D ( 'NONE', #70134, #47958, #68835 ) ;
#34900 = CARTESIAN_POINT ( 'NONE',  ( -16.93970660449832621, 10.01284139164672915, -46.05228173579446604 ) ) ;
#34902 = DIRECTION ( 'NONE',  ( 1.000000000000000000, 0.000000000000000000, 0.000000000000000000 ) ) ;
#34903 = AXIS2_PLACEMENT_3D ( 'NONE', #229761, #70719, #148963 ) ;
#34904 = CARTESIAN_POINT ( 'NONE',  ( 20.95346350065193519, 8.887177249185651107, -75.51173194703542890 ) ) ;
#34905 = AXIS2_PLACEMENT_3D ( 'NONE', #120329, #160731, #240247 ) ;
#34906 = ADVANCED_FACE ( 'NONE', ( #87996 ), #228832, .F. ) ;
#34907 = CARTESIAN_POINT ( 'NONE',  ( 20.88420186297724612, 18.41141989892752662, -236.9935361838138022 ) ) ;
#34908 = EDGE_LOOP ( 'NONE', ( #88123, #77536, #62699, #126128 ) ) ;
#34910 = ORIENTED_EDGE ( 'NONE', *, *, #114602, .F. ) ;
#34909 = EDGE_CURVE ( 'NONE', #59389, #5863, #135013, .T. ) ;
#34911 = CIRCLE ( 'NONE', #47314, 0.4000000000000114575 ) ;
#34912 = FACE_OUTER_BOUND ( 'NONE', #186959, .T. ) ;
#34913 = ORIENTED_EDGE ( 'NONE', *, *, #34753, .T. ) ;
#34914 = CARTESIAN_POINT ( 'NONE',  ( -23.15000000000000213, 1.910280373842930812, -54.36863214480106166 ) ) ;
#34915 = CARTESIAN_POINT ( 'NONE',  ( -20.85000000000000142, -11.74999999998884448, -131.1000000000000227 ) ) ;
#34916 = VERTEX_POINT ( 'NONE', #91873 ) ;
#34917 = ADVANCED_FACE ( 'NONE', ( #170180 ), #226916, .T. ) ;
#34918 = DIRECTION ( 'NONE',  ( 0.000000000000000000, -2.005774019098195320E-13, 1.000000000000000000 ) ) ;
#34919 = CARTESIAN_POINT ( 'NONE',  ( -23.25000000000000000, 87.75000000001216449, -139.6231074845242688 ) ) ;
#34920 = LINE ( 'NONE', #113136, #2997 ) ;
#34921 = DIRECTION ( 'NONE',  ( 0.000000000000000000, 0.000000000000000000, 1.000000000000000000 ) ) ;
#34922 = ORIENTED_EDGE ( 'NONE', *, *, #118590, .F. ) ;
#34923 = AXIS2_PLACEMENT_3D ( 'NONE', #254280, #130492, #193059 ) ;
#34924 = AXIS2_PLACEMENT_3D ( 'NONE', #7376, #204286, #166490 ) ;
#34925 = EDGE_CURVE ( 'NONE', #5814, #243331, #36919, .T. ) ;
#34926 = AXIS2_PLACEMENT_3D ( 'NONE', #1226, #58634, #258089 ) ;
#34927 = DIRECTION ( 'NONE',  ( 0.000000000000000000, 0.5859227990963362664, 0.8103668758649469339 ) ) ;
#34928 = DIRECTION ( 'NONE',  ( 0.000000000000000000, 0.000000000000000000, 1.000000000000000000 ) ) ;
#34929 = CARTESIAN_POINT ( 'NONE',  ( 20.94999999999999574, 1.835341550235567887, -78.55515129256303908 ) ) ;
#34930 = EDGE_LOOP ( 'NONE', ( #146529, #212852, #256796, #5516 ) ) ;
#34931 = EDGE_CURVE ( 'NONE', #89225, #248318, #257310, .T. ) ;
#34932 = DIRECTION ( 'NONE',  ( 0.000000000000000000, 1.000000000000000000, 6.982962677686266711E-15 ) ) ;
#34933 = VERTEX_POINT ( 'NONE', #252220 ) ;
#34934 = DIRECTION ( 'NONE',  ( 1.000000000000000000, 0.000000000000000000, 0.000000000000000000 ) ) ;
#34935 = CARTESIAN_POINT ( 'NONE',  ( 23.24999999999999289, 64.25000000001276135, -215.2731074845244450 ) ) ;
#34936 = DIRECTION ( 'NONE',  ( -0.000000000000000000, 0.1290532225515392817, 0.9916376685811522096 ) ) ;
#34937 = FACE_OUTER_BOUND ( 'NONE', #109719, .T. ) ;
#34938 = LINE ( 'NONE', #193994, #7220 ) ;
#34939 = ORIENTED_EDGE ( 'NONE', *, *, #86462, .T. ) ;
#34940 = CARTESIAN_POINT ( 'NONE',  ( -16.94107738177415712, 65.98576071487543970, -123.9731074845243626 ) ) ;
#34941 = AXIS2_PLACEMENT_3D ( 'NONE', #127331, #189873, #206866 ) ;
#34942 = CYLINDRICAL_SURFACE ( 'NONE', #181509, 0.09999999999999939493 ) ;
#34943 = CARTESIAN_POINT ( 'NONE',  ( -21.64999999999999858, 10.04999999999998295, -12.75000000000000178 ) ) ;
#34945 = CIRCLE ( 'NONE', #234816, 0.1000000000000002554 ) ;
#34944 = DIRECTION ( 'NONE',  ( 0.000000000000000000, 0.000000000000000000, -1.000000000000000000 ) ) ;
#34946 = VECTOR ( 'NONE', #36284, 1000.000000000000000 ) ;
#34947 = LINE ( 'NONE', #54464, #78275 ) ;
#34948 = EDGE_CURVE ( 'NONE', #132961, #93865, #22076, .T. ) ;
#34949 = EDGE_LOOP ( 'NONE', ( #139320, #252150, #45876, #104980 ) ) ;
#34950 = VERTEX_POINT ( 'NONE', #138667 ) ;
#34951 = DIRECTION ( 'NONE',  ( 1.000000000000000000, 0.000000000000000000, 0.000000000000000000 ) ) ;
#34952 = VECTOR ( 'NONE', #90149, 1000.000000000000000 ) ;
#34953 = CARTESIAN_POINT ( 'NONE',  ( 20.00000000000000355, 1.350000000000000089, 22.00000000000000355 ) ) ;
#34954 = CARTESIAN_POINT ( 'NONE',  ( 23.14999999999999858, 2.449293598294710852E-16, -31.50000000000000000 ) ) ;
#34955 = DIRECTION ( 'NONE',  ( 1.000000000000000000, 0.000000000000000000, 0.000000000000000000 ) ) ;
#34956 = VECTOR ( 'NONE', #201922, 999.9999999999998863 ) ;
#34957 = CARTESIAN_POINT ( 'NONE',  ( 21.05000000000000071, -8.999999999988842703, -191.1060308773475072 ) ) ;
#34959 = ADVANCED_FACE ( 'NONE', ( #35779 ), #115287, .F. ) ;
#34958 =( BOUNDED_SURFACE ( )  B_SPLINE_SURFACE ( 3, 2, ( 
 ( #139766, #138476, #219318 ),
 ( #39441, #40728, #155540 ),
 ( #96777, #81080, #216751 ),
 ( #195934, #160668, #134629 ) ),
 .UNSPECIFIED., .F., .F., .F. ) 
 B_SPLINE_SURFACE_WITH_KNOTS ( ( 4, 4 ),
 ( 3, 3 ),
 ( -1.908195823574487804E-17, 0.001979672783031562362 ),
 ( 0.000000000000000000, 1.000000000000000000 ),
 .UNSPECIFIED. ) 
 GEOMETRIC_REPRESENTATION_ITEM ( )  RATIONAL_B_SPLINE_SURFACE ( (
 ( 1.000000000000000000, 0.7103081912008383236, 1.000000000000000000),
 ( 1.000000000000000000, 0.7104998333558345536, 1.000000000000000000),
 ( 1.000000000000000000, 0.7107238315755375346, 1.000000000000000000),
 ( 1.000000000000000000, 0.7110073749539294052, 1.000000000000000000) ) ) 
 REPRESENTATION_ITEM ( '' )  SURFACE ( )  );
#34960 = VERTEX_POINT ( 'NONE', #158309 ) ;
#34961 = CARTESIAN_POINT ( 'NONE',  ( -23.25000000000000000, 76.00000000001237765, -170.0231074845243597 ) ) ;
#34962 = CARTESIAN_POINT ( 'NONE',  ( 18.39999999999999503, 5.650000000011139001, -113.1500000000000341 ) ) ;
#34963 = EDGE_CURVE ( 'NONE', #196712, #237038, #116192, .T. ) ;
#34964 = ORIENTED_EDGE ( 'NONE', *, *, #109336, .T. ) ;
#34965 = EDGE_CURVE ( 'NONE', #14771, #61206, #194855, .T. ) ;
#34966 = VECTOR ( 'NONE', #207173, 1000.000000000000227 ) ;
#34967 = AXIS2_PLACEMENT_3D ( 'NONE', #128148, #125564, #149006 ) ;
#34968 = CARTESIAN_POINT ( 'NONE',  ( 21.14999999999999858, 87.75000000001186606, -90.77310748452423184 ) ) ;
#34969 = EDGE_CURVE ( 'NONE', #225579, #133625, #95326, .T. ) ;
#34970 = EDGE_CURVE ( 'NONE', #225834, #47428, #119152, .T. ) ;
#34971 = TOROIDAL_SURFACE ( 'NONE', #214005, 0.2000000000000000111, 0.1000000000000000056 ) ;
#34972 = EDGE_LOOP ( 'NONE', ( #67721, #117200, #70153, #241024 ) ) ;
#34974 =( BOUNDED_SURFACE ( )  B_SPLINE_SURFACE ( 3, 2, ( 
 ( #49894, #66893, #72045 ),
 ( #52448, #132004, #186859 ),
 ( #248093, #147722, #208970 ),
 ( #90290, #9481, #10780 ),
 ( #168619, #27805, #189419 ),
 ( #206405, #249397, #169901 ),
 ( #211551, #32950, #108589 ),
 ( #31654, #130714, #29100 ) ),
 .UNSPECIFIED., .F., .F., .F. ) 
 B_SPLINE_SURFACE_WITH_KNOTS ( ( 4, 2, 2, 4 ),
 ( 3, 3 ),
 ( 0.0001704874539069835152, 0.0003809798300636603702, 0.0004862260181419988383, 0.0005914722062203372523 ),
 ( 0.000000000000000000, 1.000000000000000000 ),
 .UNSPECIFIED. ) 
 GEOMETRIC_REPRESENTATION_ITEM ( )  RATIONAL_B_SPLINE_SURFACE ( (
 ( 1.000000000000000000, 0.7071067811864942820, 1.000000000000000000),
 ( 1.000000000000000000, 0.7670648383578960727, 1.000000000000000000),
 ( 1.000000000000000000, 0.8204820770248829609, 1.000000000000000000),
 ( 1.000000000000000000, 0.8877218296115439999, 1.000000000000000000),
 ( 1.000000000000000000, 0.9080815932664635381, 1.000000000000000000),
 ( 1.000000000000000000, 0.9395541505862817777, 1.000000000000000000),
 ( 1.000000000000000000, 0.9506520335378265685, 1.000000000000000000),
 ( 1.000000000000000000, 0.9504532311154628710, 1.000000000000000000) ) ) 
 REPRESENTATION_ITEM ( '' )  SURFACE ( )  );
#34973 = DIRECTION ( 'NONE',  ( 0.000000000000000000, 0.000000000000000000, -1.000000000000000000 ) ) ;
#34975 = EDGE_CURVE ( 'NONE', #119689, #72236, #236974, .T. ) ;
#34976 = ORIENTED_EDGE ( 'NONE', *, *, #192204, .F. ) ;
#34977 = DIRECTION ( 'NONE',  ( 1.073024830501117725E-15, 6.982962677686266711E-15, -1.000000000000000000 ) ) ;
#34978 = DIRECTION ( 'NONE',  ( 0.000000000000000000, 0.000000000000000000, -1.000000000000000000 ) ) ;
#34979 = LINE ( 'NONE', #100006, #240837 ) ;
#34980 = CARTESIAN_POINT ( 'NONE',  ( 20.94999999999999929, 85.50000000001159606, -59.62913836187181715 ) ) ;
#34981 = DIRECTION ( 'NONE',  ( 0.000000000000000000, 6.938893903907222067E-15, -1.000000000000000000 ) ) ;
#34982 = CARTESIAN_POINT ( 'NONE',  ( 21.05000000000000071, 76.00000000001213607, -136.5231074845243313 ) ) ;
#34983 = CARTESIAN_POINT ( 'NONE',  ( -18.59999999999999787, 11.65000000001115232, -79.15000000000003411 ) ) ;
#34984 = LINE ( 'NONE', #98720, #247287 ) ;
#34986 = DIRECTION ( 'NONE',  ( -0.000000000000000000, -0.000000000000000000, 1.000000000000000000 ) ) ;
#34985 = CARTESIAN_POINT ( 'NONE',  ( 20.05000000000002913, 68.75000000001227818, -157.3731074845244109 ) ) ;
#34987 = CARTESIAN_POINT ( 'NONE',  ( -23.15000000000000213, -8.999999999988844479, -157.6060308773475924 ) ) ;
#34988 = CARTESIAN_POINT ( 'NONE',  ( 21.14999999999999858, 22.07612373182271881, -231.7717111801312342 ) ) ;
#34989 = CARTESIAN_POINT ( 'NONE',  ( -20.64999999999999858, 71.65000000001253966, -182.3731074845244109 ) ) ;
#34990 = CARTESIAN_POINT ( 'NONE',  ( -21.07928932188134041, 76.00000000001195133, -103.0231074845243171 ) ) ;
#34991 = ORIENTED_EDGE ( 'NONE', *, *, #249136, .T. ) ;
#34992 = CARTESIAN_POINT ( 'NONE',  ( -18.47130263965434338, -9.471155585964025292, -40.18340476547687956 ) ) ;
#34993 = VECTOR ( 'NONE', #159871, 1000.000000000000000 ) ;
#34994 = CARTESIAN_POINT ( 'NONE',  ( -21.64999999999999858, 52.99650480578122824, -234.2878581050858884 ) ) ;
#34995 = CARTESIAN_POINT ( 'NONE',  ( -20.64999999999999858, -8.663551401858004652, -76.52410111806734960 ) ) ;
#34996 =( BOUNDED_SURFACE ( )  B_SPLINE_SURFACE ( 3, 2, ( 
 ( #48783, #3220, #206579 ),
 ( #27980, #187044, #204005 ),
 ( #103598, #107476, #65782 ),
 ( #166207, #145304, #224846 ),
 ( #8393, #82737, #87885 ),
 ( #162336, #167479, #246980 ),
 ( #241845, #46210, #63193 ),
 ( #147903, #67072, #227419 ),
 ( #142733, #123193, #202718 ),
 ( #24115, #163607, #243131 ) ),
 .UNSPECIFIED., .F., .F., .F. ) 
 B_SPLINE_SURFACE_WITH_KNOTS ( ( 4, 2, 2, 2, 4 ),
 ( 3, 3 ),
 ( 0.002161241639767276426, 0.002579950749615843482, 0.002789305304540127227, 0.002893982582002269099, 0.002998659859464410972 ),
 ( 0.000000000000000000, 1.000000000000000000 ),
 .UNSPECIFIED. ) 
 GEOMETRIC_REPRESENTATION_ITEM ( )  RATIONAL_B_SPLINE_SURFACE ( (
 ( 1.000000000000000000, 0.7071067811865475727, 1.000000000000000000),
 ( 1.000000000000000000, 0.7632447400664224002, 1.000000000000000000),
 ( 1.000000000000000000, 0.8158073005110438869, 1.000000000000000000),
 ( 1.000000000000000000, 0.8906973462395797458, 1.000000000000000000),
 ( 1.000000000000000000, 0.9149408947802050163, 1.000000000000000000),
 ( 1.000000000000000000, 0.9493368785274935995, 1.000000000000000000),
 ( 1.000000000000000000, 0.9605194247157773368, 1.000000000000000000),
 ( 1.000000000000000000, 0.9803630264780145431, 1.000000000000000000),
 ( 1.000000000000000000, 0.9900844824271928246, 1.000000000000000000),
 ( 1.000000000000000000, 0.9894588281429246290, 1.000000000000000000) ) ) 
 REPRESENTATION_ITEM ( '' )  SURFACE ( )  );
#34997 = AXIS2_PLACEMENT_3D ( 'NONE', #207931, #189640, #166248 ) ;
#34998 = EDGE_CURVE ( 'NONE', #20565, #145748, #207771, .T. ) ;
#34999 = VECTOR ( 'NONE', #128577, 1000.000000000000000 ) ;
#35000 = ORIENTED_EDGE ( 'NONE', *, *, #116149, .T. ) ;
#35001 = DIRECTION ( 'NONE',  ( -1.000000000000000000, -0.000000000000000000, -0.000000000000000000 ) ) ;
#35002 = DIRECTION ( 'NONE',  ( -1.000000000000000000, -0.000000000000000000, -0.000000000000000000 ) ) ;
#35003 = DIRECTION ( 'NONE',  ( -1.000000000000000000, 0.000000000000000000, 0.000000000000000000 ) ) ;
#35004 = EDGE_CURVE ( 'NONE', #182432, #114575, #73628, .T. ) ;
#35005 = EDGE_CURVE ( 'NONE', #252143, #19078, #256026, .T. ) ;
#35006 = ORIENTED_EDGE ( 'NONE', *, *, #198245, .F. ) ;
#35007 = CARTESIAN_POINT ( 'NONE',  ( -20.85000000000000142, 68.87972903831409610, -65.86354444268503983 ) ) ;
#35008 = ORIENTED_EDGE ( 'NONE', *, *, #2188, .T. ) ;
#35009 = DIRECTION ( 'NONE',  ( 1.000000000000000000, 0.000000000000000000, 0.000000000000000000 ) ) ;
#35010 = CARTESIAN_POINT ( 'NONE',  ( -20.54999999999999716, -8.999999999988846255, -177.3939691226524076 ) ) ;
#35011 = CIRCLE ( 'NONE', #147399, 0.5000000000000007772 ) ;
#35012 = CIRCLE ( 'NONE', #85005, 7.899999999999995914 ) ;
#35013 = AXIS2_PLACEMENT_3D ( 'NONE', #133562, #18748, #35773 ) ;
#35014 = ORIENTED_EDGE ( 'NONE', *, *, #222466, .F. ) ;
#35015 = FACE_OUTER_BOUND ( 'NONE', #215373, .T. ) ;
#35016 = ORIENTED_EDGE ( 'NONE', *, *, #253795, .T. ) ;
#35017 = CARTESIAN_POINT ( 'NONE',  ( 21.05000005001280527, 67.12872030824186709, -124.3451598962785738 ) ) ;
#35019 = CARTESIAN_POINT ( 'NONE',  ( -20.00857864376270001, 9.250000000011157297, -188.7499999999999716 ) ) ;
#35018 = PRODUCT_DEFINITION_CONTEXT ( 'detailed design', #32618, 'design' ) ;
#35020 = DIRECTION ( 'NONE',  ( 0.000000000000000000, -6.982962677686266711E-15, 1.000000000000000000 ) ) ;
#35021 = CARTESIAN_POINT ( 'NONE',  ( 23.14999999999999503, 69.55000000001253113, -182.3731074845244109 ) ) ;
#35022 = PLANE ( 'NONE',  #199907 ) ;
#35023 = CARTESIAN_POINT ( 'NONE',  ( -20.64999999999999858, 68.85000000001254250, -182.3731074845244109 ) ) ;
#35024 = CARTESIAN_POINT ( 'NONE',  ( -21.05000000000000071, 68.22930980752001062, -227.7331931781284879 ) ) ;
#35026 = VERTEX_POINT ( 'NONE', #193556 ) ;
#35025 = DIRECTION ( 'NONE',  ( 0.000000000000000000, 0.000000000000000000, -1.000000000000000000 ) ) ;
#35027 = VERTEX_POINT ( 'NONE', #14925 ) ;
#35029 = DIRECTION ( 'NONE',  ( -1.000000000000000000, 0.000000000000000000, -0.000000000000000000 ) ) ;
#35028 = DIRECTION ( 'NONE',  ( 1.000000000000000000, 0.000000000000000000, 0.000000000000000000 ) ) ;
#35030 = EDGE_LOOP ( 'NONE', ( #83141, #62113, #103255, #195824 ) ) ;
#35032 = ORIENTED_EDGE ( 'NONE', *, *, #159760, .T. ) ;
#35031 = CARTESIAN_POINT ( 'NONE',  ( 23.14999999999999503, 6.550000000011156231, -88.25000000000005684 ) ) ;
#35033 = ORIENTED_EDGE ( 'NONE', *, *, #238614, .T. ) ;
#35034 = DIRECTION ( 'NONE',  ( 0.000000000000000000, 0.9126074666063660468, 0.4088369013363524762 ) ) ;
#35035 = CARTESIAN_POINT ( 'NONE',  ( 20.22894356738451194, 9.278498222849622223, -175.7685229062464600 ) ) ;
#35036 = VECTOR ( 'NONE', #232249, 1000.000000000000000 ) ;
#35037 = CARTESIAN_POINT ( 'NONE',  ( -20.07928932188135107, 52.19080555870878158, -232.4893728257138719 ) ) ;
#35038 = CARTESIAN_POINT ( 'NONE',  ( 18.46947024752524769, -9.509297157156085589, -6.986689448697918081 ) ) ;
#35039 = DIRECTION ( 'NONE',  ( 3.469446951953728416E-14, -0.9525900758537746427, 0.3042567129660413983 ) ) ;
#35040 = FACE_OUTER_BOUND ( 'NONE', #29519, .T. ) ;
#35041 = DIRECTION ( 'NONE',  ( 0.000000000000000000, 0.000000000000000000, 1.000000000000000000 ) ) ;
#35042 = EDGE_CURVE ( 'NONE', #80585, #216962, #245169, .T. ) ;
#35043 = CARTESIAN_POINT ( 'NONE',  ( 21.14999999999999503, 31.89597452117651244, -238.9192857152811484 ) ) ;
#35044 = ORIENTED_EDGE ( 'NONE', *, *, #105332, .T. ) ;
#35045 = ORIENTED_EDGE ( 'NONE', *, *, #151671, .T. ) ;
#35046 = ADVANCED_FACE ( 'NONE', ( #174028 ), #111908, .T. ) ;
#35047 = CARTESIAN_POINT ( 'NONE',  ( 21.70464131381650219, 6.932842828061961171, -199.4901007520778080 ) ) ;
#35048 = CIRCLE ( 'NONE', #214071, 12.87499999999999822 ) ;
#35049 = CIRCLE ( 'NONE', #226514, 0.09999999999998898659 ) ;
#35050 = ORIENTED_EDGE ( 'NONE', *, *, #50551, .F. ) ;
#35051 = DIRECTION ( 'NONE',  ( 1.000000000000000000, 0.000000000000000000, 0.000000000000000000 ) ) ;
#35052 = ORIENTED_EDGE ( 'NONE', *, *, #67735, .F. ) ;
#35053 = CARTESIAN_POINT ( 'NONE',  ( 18.44206774312970865, -9.491027357540085418, -40.12622750469819977 ) ) ;
#35054 = CIRCLE ( 'NONE', #164209, 0.09999999999999939493 ) ;
#35055 = AXIS2_PLACEMENT_3D ( 'NONE', #17813, #16563, #179493 ) ;
#35056 = EDGE_CURVE ( 'NONE', #129370, #146650, #196121, .T. ) ;
#35057 = EDGE_CURVE ( 'NONE', #64025, #138313, #38336, .T. ) ;
#35058 = CARTESIAN_POINT ( 'NONE',  ( -20.64999999999999858, -8.999999999988844479, -91.00603087734759811 ) ) ;
#35059 = DIRECTION ( 'NONE',  ( -1.000000000000000000, -0.000000000000000000, -0.000000000000000000 ) ) ;
#35060 = CARTESIAN_POINT ( 'NONE',  ( -21.17356465864818205, 6.422803126252873973, -33.40108875898613405 ) ) ;
#35061 = DIRECTION ( 'NONE',  ( 1.000000000000000000, 0.000000000000000000, 0.000000000000000000 ) ) ;
#35062 = VERTEX_POINT ( 'NONE', #236513 ) ;
#35063 = CARTESIAN_POINT ( 'NONE',  ( -18.39999999999999858, -9.499999999988851584, -207.6001893912219884 ) ) ;
#35064 = CARTESIAN_POINT ( 'NONE',  ( 21.00000000000000000, 66.25000000001186606, -90.67310748452437963 ) ) ;
#35065 = CARTESIAN_POINT ( 'NONE',  ( 20.94999999999999929, 9.307299318941717914, -220.9418877738490039 ) ) ;
#35067 = CIRCLE ( 'NONE', #222427, 11.79999999999999005 ) ;
#35066 = DIRECTION ( 'NONE',  ( 0.000000000000000000, 0.4721928772776973204, 0.8814952561688629284 ) ) ;
#35068 = CARTESIAN_POINT ( 'NONE',  ( -21.05000000000000071, 6.413759733821436271, -134.0856130608038939 ) ) ;
#35069 = ORIENTED_EDGE ( 'NONE', *, *, #685, .T. ) ;
#35071 = DIRECTION ( 'NONE',  ( 1.000000000000000000, 0.000000000000000000, 0.000000000000000000 ) ) ;
#35070 = DIRECTION ( 'NONE',  ( -0.000000000000000000, 0.2617529984165031243, 0.9651348961777157509 ) ) ;
#35073 = ORIENTED_EDGE ( 'NONE', *, *, #110832, .F. ) ;
#35072 = CIRCLE ( 'NONE', #189344, 0.1000000000000024342 ) ;
#35075 = ORIENTED_EDGE ( 'NONE', *, *, #65539, .F. ) ;
#35074 = DIRECTION ( 'NONE',  ( 0.000000000000000000, -0.9999991631930157387, 0.001293682058423061953 ) ) ;
#35076 = EDGE_CURVE ( 'NONE', #159793, #69974, #228611, .T. ) ;
#35077 = DIRECTION ( 'NONE',  ( -0.000000000000000000, 0.1350103645451649625, -0.9908441862701631297 ) ) ;
#35078 = ADVANCED_FACE ( 'NONE', ( #98251 ), #100815, .T. ) ;
#35079 = AXIS2_PLACEMENT_3D ( 'NONE', #238338, #218762, #217477 ) ;
#35080 = AXIS2_PLACEMENT_3D ( 'NONE', #62036, #198956, #217222 ) ;
#35081 = CARTESIAN_POINT ( 'NONE',  ( -22.50000000000000000, 64.35042919246686210, -69.62310748452439668 ) ) ;
#35082 = ORIENTED_EDGE ( 'NONE', *, *, #110628, .T. ) ;
#35083 = CYLINDRICAL_SURFACE ( 'NONE', #172210, 0.09999999999999971412 ) ;
#35084 = FACE_OUTER_BOUND ( 'NONE', #212036, .T. ) ;
#35085 = CARTESIAN_POINT ( 'NONE',  ( -17.04295772865479819, 10.02489942525997257, -12.65000000000000391 ) ) ;
#35087 = ORIENTED_EDGE ( 'NONE', *, *, #15082, .F. ) ;
#35086 = DIRECTION ( 'NONE',  ( 1.000000000000000000, 0.000000000000000000, 0.000000000000000000 ) ) ;
#35088 = AXIS2_PLACEMENT_3D ( 'NONE', #201417, #22815, #41095 ) ;
#35089 = ADVANCED_FACE ( 'NONE', ( #202531 ), #182984, .F. ) ;
#35090 = VECTOR ( 'NONE', #236068, 1000.000000000000000 ) ;
#35091 = ORIENTED_EDGE ( 'NONE', *, *, #134603, .T. ) ;
#35093 = ADVANCED_FACE ( 'NONE', ( #242933 ), #219512, .F. ) ;
#35092 = CYLINDRICAL_SURFACE ( 'NONE', #215759, 0.1000000000000006162 ) ;
#35094 = CARTESIAN_POINT ( 'NONE',  ( 23.40000000000005187, 87.50449464844290048, -34.18759587077607165 ) ) ;
#35095 = CARTESIAN_POINT ( 'NONE',  ( -23.15000000000000213, -11.64999999998884483, -197.9999999999999432 ) ) ;
#35096 = DIRECTION ( 'NONE',  ( 0.000000000000000000, 1.000000000000000000, 0.000000000000000000 ) ) ;
#35097 = EDGE_LOOP ( 'NONE', ( #238559, #201560, #187964, #154782 ) ) ;
#35098 = CARTESIAN_POINT ( 'NONE',  ( -16.97683809663752186, 22.93084817181464530, -231.0232129367395260 ) ) ;
#35099 = CIRCLE ( 'NONE', #118268, 0.8750000000000007772 ) ;
#35100 = DIRECTION ( 'NONE',  ( 0.000000000000000000, 0.000000000000000000, 1.000000000000000000 ) ) ;
#35101 = FACE_OUTER_BOUND ( 'NONE', #165577, .T. ) ;
#35102 = ORIENTED_EDGE ( 'NONE', *, *, #137459, .F. ) ;
#35103 = EDGE_CURVE ( 'NONE', #69221, #50036, #240382, .T. ) ;
#35104 = DIRECTION ( 'NONE',  ( -1.000000000000000000, 3.151514657663852580E-16, -8.547182517843351137E-17 ) ) ;
#35105 = AXIS2_PLACEMENT_3D ( 'NONE', #97861, #172349, #251830 ) ;
#35107 = AXIS2_PLACEMENT_3D ( 'NONE', #119620, #175751, #98713 ) ;
#35106 = DIRECTION ( 'NONE',  ( 1.073024830501117725E-15, -6.982962677686266711E-15, 1.000000000000000000 ) ) ;
#35108 = ORIENTED_EDGE ( 'NONE', *, *, #139230, .F. ) ;
#35109 = ADVANCED_FACE ( 'NONE', ( #21355 ), #55054, .T. ) ;
#35110 = LINE ( 'NONE', #1039, #176516 ) ;
#35111 = DIRECTION ( 'NONE',  ( -1.000000000000000000, 1.772924042024179204E-16, -4.808324575169891715E-17 ) ) ;
#35112 = CYLINDRICAL_SURFACE ( 'NONE', #127957, 0.1000000000000024342 ) ;
#35113 = VERTEX_POINT ( 'NONE', #22634 ) ;
#35114 = ORIENTED_EDGE ( 'NONE', *, *, #99913, .F. ) ;
#35115 = DIRECTION ( 'NONE',  ( -1.000000000000000000, -0.000000000000000000, -0.000000000000000000 ) ) ;
#35116 = ORIENTED_EDGE ( 'NONE', *, *, #5514, .T. ) ;
#35117 = ORIENTED_EDGE ( 'NONE', *, *, #32949, .F. ) ;
#35118 = EDGE_CURVE ( 'NONE', #254860, #18904, #12081, .T. ) ;
#35121 = VERTEX_POINT ( 'NONE', #179150 ) ;
#35120 = ORIENTED_EDGE ( 'NONE', *, *, #73351, .T. ) ;
#35119 = LINE ( 'NONE', #91209, #80356 ) ;
#35122 = EDGE_CURVE ( 'NONE', #233526, #19722, #124546, .T. ) ;
#35123 = AXIS2_PLACEMENT_3D ( 'NONE', #154015, #233517, #173579 ) ;
#35124 = CIRCLE ( 'NONE', #184927, 0.1999999999999987899 ) ;
#35125 = CARTESIAN_POINT ( 'NONE',  ( -23.25000000000000000, 67.55989888862310977, -211.9120700681549465 ) ) ;
#35126 = FACE_OUTER_BOUND ( 'NONE', #135006, .T. ) ;
#35127 = FACE_OUTER_BOUND ( 'NONE', #100594, .T. ) ;
#35128 = AXIS2_PLACEMENT_3D ( 'NONE', #184743, #246020, #170382 ) ;
#35129 = DIRECTION ( 'NONE',  ( 0.000000000000000000, 7.147358527629766941E-15, -1.000000000000000000 ) ) ;
#35130 = DIRECTION ( 'NONE',  ( 0.000000000000000000, -6.982962677686266711E-15, 1.000000000000000000 ) ) ;
#35131 = CARTESIAN_POINT ( 'NONE',  ( 18.49999999999999645, -1.362429037182155023, -141.8888812479212334 ) ) ;
#35132 = ORIENTED_EDGE ( 'NONE', *, *, #11079, .T. ) ;
#35133 = EDGE_LOOP ( 'NONE', ( #232350, #61830, #222119 ) ) ;
#35135 = ORIENTED_EDGE ( 'NONE', *, *, #157938, .T. ) ;
#35134 = TOROIDAL_SURFACE ( 'NONE', #147527, 0.2000000000000000111, 0.1000000000000000056 ) ;
#35136 = CARTESIAN_POINT ( 'NONE',  ( 20.97239005616515684, 8.874843841361279573, -146.2501528021531954 ) ) ;
#35137 = AXIS2_PLACEMENT_3D ( 'NONE', #199046, #38692, #154812 ) ;
#35139 = EDGE_LOOP ( 'NONE', ( #216889, #11883, #256656, #144417 ) ) ;
#35138 = DIRECTION ( 'NONE',  ( 0.000000000000000000, 1.000000000000000000, 0.000000000000000000 ) ) ;
#35140 = DIRECTION ( 'NONE',  ( 0.000000000000000000, 1.000000000000000000, 0.000000000000000000 ) ) ;
#35141 = VERTEX_POINT ( 'NONE', #222059 ) ;
#35142 = DIRECTION ( 'NONE',  ( -0.1538461538461493860, 0.9654630569144674324, 0.2102675597426261755 ) ) ;
#35143 = ORIENTED_EDGE ( 'NONE', *, *, #175416, .T. ) ;
#35144 = CARTESIAN_POINT ( 'NONE',  ( 23.24999999999999289, 29.04162040546706436, -238.0402253144129929 ) ) ;
#35145 = CIRCLE ( 'NONE', #180859, 0.1999999999999996503 ) ;
#35146 = AXIS2_PLACEMENT_3D ( 'NONE', #39488, #137257, #171610 ) ;
#35147 = ORIENTED_EDGE ( 'NONE', *, *, #47046, .F. ) ;
#35148 = VECTOR ( 'NONE', #76505, 1000.000000000000000 ) ;
#35149 = CARTESIAN_POINT ( 'NONE',  ( 20.05000000000002913, 65.69159657275403674, -213.8343546826533554 ) ) ;
#35150 = DIRECTION ( 'NONE',  ( 1.000000000000000000, -0.000000000000000000, -0.000000000000000000 ) ) ;
#35151 = AXIS2_PLACEMENT_3D ( 'NONE', #51711, #210815, #32202 ) ;
#35153 = ORIENTED_EDGE ( 'NONE', *, *, #50655, .F. ) ;
#35152 = ORIENTED_EDGE ( 'NONE', *, *, #124650, .F. ) ;
#35154 = ORIENTED_EDGE ( 'NONE', *, *, #162087, .F. ) ;
#35155 = CARTESIAN_POINT ( 'NONE',  ( -21.05000000000000071, 76.00000000001142553, -36.02310748452432421 ) ) ;
#35156 = ORIENTED_EDGE ( 'NONE', *, *, #163309, .T. ) ;
#35157 = ORIENTED_EDGE ( 'NONE', *, *, #57421, .T. ) ;
#35158 = DIRECTION ( 'NONE',  ( 0.000000000000000000, -7.487053152578127080E-15, 1.000000000000000000 ) ) ;
#35160 = ORIENTED_EDGE ( 'NONE', *, *, #57117, .T. ) ;
#35159 = CARTESIAN_POINT ( 'NONE',  ( 18.33683296300512922, -9.511149971121900748, -107.4057074127093756 ) ) ;
#35161 = DIRECTION ( 'NONE',  ( -1.000000000000000000, 0.000000000000000000, 0.000000000000000000 ) ) ;
#35162 = TOROIDAL_SURFACE ( 'NONE', #80894, 0.4000000000000003553, 0.1000000000000000056 ) ;
#35164 = DIRECTION ( 'NONE',  ( 0.000000000000000000, 0.8660254037844384856, -0.5000000000000003331 ) ) ;
#35163 = PLANE ( 'NONE',  #94748 ) ;
#35165 = PLANE ( 'NONE',  #157463 ) ;
#35166 = CARTESIAN_POINT ( 'NONE',  ( 18.45068634130097607, -9.486506073331600675, -74.06877843116815541 ) ) ;
#35167 = CARTESIAN_POINT ( 'NONE',  ( 21.40925344232282868, 30.54185590562371999, -252.1831082382518048 ) ) ;
#35168 = ORIENTED_EDGE ( 'NONE', *, *, #247167, .F. ) ;
#35169 = ORIENTED_EDGE ( 'NONE', *, *, #146283, .F. ) ;
#35170 = AXIS2_PLACEMENT_3D ( 'NONE', #163720, #43765, #123313 ) ;
#35171 = CARTESIAN_POINT ( 'NONE',  ( -16.87331047859651179, 66.05000000001261640, -190.8731074845244393 ) ) ;
#35172 = FACE_OUTER_BOUND ( 'NONE', #174743, .T. ) ;
#35173 = EDGE_CURVE ( 'NONE', #97978, #182621, #159563, .T. ) ;
#35174 = ORIENTED_EDGE ( 'NONE', *, *, #213206, .T. ) ;
#35175 = DIRECTION ( 'NONE',  ( 0.000000000000000000, -0.000000000000000000, -1.000000000000000000 ) ) ;
#35176 = AXIS2_PLACEMENT_3D ( 'NONE', #150561, #51419, #171442 ) ;
#35177 = AXIS2_PLACEMENT_3D ( 'NONE', #36705, #32864, #254406 ) ;
#35178 = CARTESIAN_POINT ( 'NONE',  ( -16.93353400591625757, 51.67199383424718206, -231.8628248725454455 ) ) ;
#35179 = CIRCLE ( 'NONE', #193377, 0.09999999999999939493 ) ;
#35180 = DIRECTION ( 'NONE',  ( 0.000000000000000000, 0.000000000000000000, -1.000000000000000000 ) ) ;
#35181 = ORIENTED_EDGE ( 'NONE', *, *, #186099, .F. ) ;
#35182 = ORIENTED_EDGE ( 'NONE', *, *, #73976, .T. ) ;
#35183 = DIRECTION ( 'NONE',  ( 0.000000000000000000, -0.9229812358756199764, 0.3848449534832346086 ) ) ;
#35184 = EDGE_CURVE ( 'NONE', #210177, #47156, #57876, .T. ) ;
#35185 = CARTESIAN_POINT ( 'NONE',  ( -16.79184697841823493, 66.05123833835365588, -123.8689652139218538 ) ) ;
#35186 = VERTEX_POINT ( 'NONE', #129415 ) ;
#35187 = CARTESIAN_POINT ( 'NONE',  ( 21.14999999999999503, 76.10085836911147794, -215.2726746080137445 ) ) ;
#35188 = ORIENTED_EDGE ( 'NONE', *, *, #160241, .F. ) ;
#35189 = FACE_OUTER_BOUND ( 'NONE', #110256, .T. ) ;
#35190 = CARTESIAN_POINT ( 'NONE',  ( -23.25000000000000000, 76.10085836911045476, -81.27267460801371612 ) ) ;
#35192 = DIRECTION ( 'NONE',  ( 1.000000000000000000, 0.000000000000000000, 0.000000000000000000 ) ) ;
#35191 = DIRECTION ( 'NONE',  ( 0.000000000000000000, 0.4999999999999689138, -0.8660254037844565822 ) ) ;
#35193 = EDGE_CURVE ( 'NONE', #20407, #254122, #211849, .T. ) ;
#35194 = CARTESIAN_POINT ( 'NONE',  ( 0.9000000000000547562, 67.75000000001118394, -12.62310748452478926 ) ) ;
#35195 = CARTESIAN_POINT ( 'NONE',  ( 21.06490991615909536, 65.27510865242474836, -90.81939613099125097 ) ) ;
#35196 = CARTESIAN_POINT ( 'NONE',  ( -18.50000000000000000, -9.399999999988850163, -140.8820418481727188 ) ) ;
#35197 = AXIS2_PLACEMENT_3D ( 'NONE', #217908, #97956, #232387 ) ;
#35199 = VERTEX_POINT ( 'NONE', #146387 ) ;
#35198 = ORIENTED_EDGE ( 'NONE', *, *, #68575, .F. ) ;
#35200 = ORIENTED_EDGE ( 'NONE', *, *, #255430, .F. ) ;
#35201 = EDGE_CURVE ( 'NONE', #52101, #5474, #147700, .T. ) ;
#35202 = PLANE ( 'NONE',  #125691 ) ;
#35203 = CARTESIAN_POINT ( 'NONE',  ( -16.81744102076749314, 60.93935776605891164, -221.0417277355860790 ) ) ;
#35204 = VECTOR ( 'NONE', #229270, 1000.000000000000000 ) ;
#35205 = EDGE_CURVE ( 'NONE', #165054, #4905, #30331, .T. ) ;
#35206 = CARTESIAN_POINT ( 'NONE',  ( -18.44362607810620958, -9.490496158073669974, -107.5579538668471571 ) ) ;
#35208 = DIRECTION ( 'NONE',  ( 0.000000000000000000, 0.7397360091702755991, -0.6728971962616832059 ) ) ;
#35207 = CARTESIAN_POINT ( 'NONE',  ( -18.50000000000000000, 64.25000000001222134, -148.2731074845243882 ) ) ;
#35209 = DIRECTION ( 'NONE',  ( 0.000000000000000000, 0.000000000000000000, 1.000000000000000000 ) ) ;
#35210 = ORIENTED_EDGE ( 'NONE', *, *, #21477, .T. ) ;
#35211 = CARTESIAN_POINT ( 'NONE',  ( 18.49999999999999645, 36.65892442174472876, -249.5511627012454596 ) ) ;
#35212 = ORIENTED_EDGE ( 'NONE', *, *, #41132, .T. ) ;
#35213 = ORIENTED_EDGE ( 'NONE', *, *, #216478, .T. ) ;
#35214 = FACE_OUTER_BOUND ( 'NONE', #252007, .T. ) ;
#35215 = DIRECTION ( 'NONE',  ( 1.734723475976817507E-14, 0.000000000000000000, -1.000000000000000000 ) ) ;
#35216 = CARTESIAN_POINT ( 'NONE',  ( -18.59999999999999787, -1.162701749926853712, -175.5999999999999659 ) ) ;
#35217 = DIRECTION ( 'NONE',  ( 0.000000000000000000, 0.000000000000000000, -1.000000000000000000 ) ) ;
#35218 = EDGE_LOOP ( 'NONE', ( #116706, #17477, #87316 ) ) ;
#35220 = ORIENTED_EDGE ( 'NONE', *, *, #211005, .T. ) ;
#35219 = EDGE_CURVE ( 'NONE', #56292, #16105, #90267, .T. ) ;
#35221 = CARTESIAN_POINT ( 'NONE',  ( -21.14999999999999858, 11.65000000001115232, -33.50000000000000000 ) ) ;
#35222 = DIRECTION ( 'NONE',  ( -1.000000000000000000, 0.000000000000000000, -0.000000000000000000 ) ) ;
#35223 = DIRECTION ( 'NONE',  ( -0.000000000000000000, 0.08413937888707637147, -0.9964539953858869703 ) ) ;
#35224 = DIRECTION ( 'NONE',  ( -0.000000000000000000, 0.8814952561688430555, -0.4721928772777346239 ) ) ;
#35225 = CARTESIAN_POINT ( 'NONE',  ( -16.94226253665225812, 9.950000000011138823, -188.0532654043842342 ) ) ;
#35226 = CARTESIAN_POINT ( 'NONE',  ( 20.94999999999999929, 76.00000000001215028, -138.4231074845243654 ) ) ;
#35227 = CARTESIAN_POINT ( 'NONE',  ( -20.85000000000000142, 76.00000000001244871, -170.0231074845243597 ) ) ;
#35229 = CARTESIAN_POINT ( 'NONE',  ( 18.59999999999999076, 28.90625159212240547, -238.0811555523021070 ) ) ;
#35228 = CARTESIAN_POINT ( 'NONE',  ( 21.05000000000000071, 77.25000000001209344, -128.6231074845242972 ) ) ;
#35230 = CYLINDRICAL_SURFACE ( 'NONE', #87322, 0.09999999999999976963 ) ;
#35231 = ADVANCED_FACE ( 'NONE', ( #246783 ), #107277, .F. ) ;
#35232 = CARTESIAN_POINT ( 'NONE',  ( 21.05000000000000426, 65.27628289530409234, -61.92869009291128179 ) ) ;
#35233 = CARTESIAN_POINT ( 'NONE',  ( -20.94999999999999929, -1.164121893230052995, -141.7148480855716457 ) ) ;
#35234 = DIRECTION ( 'NONE',  ( 0.000000000000000000, 0.2128009952263582305, -0.9770955615653319493 ) ) ;
#35235 = TOROIDAL_SURFACE ( 'NONE', #68513, 0.2000000000000000111, 0.1000000000000000056 ) ;
#35237 = ORIENTED_EDGE ( 'NONE', *, *, #158386, .F. ) ;
#35236 = CARTESIAN_POINT ( 'NONE',  ( -22.50000000000000000, 64.25000000001269029, -203.5231074845244166 ) ) ;
#35238 = AXIS2_PLACEMENT_3D ( 'NONE', #126715, #162016, #186707 ) ;
#35239 = AXIS2_PLACEMENT_3D ( 'NONE', #248790, #25896, #148403 ) ;
#35240 = CIRCLE ( 'NONE', #226726, 1.900000000000012790 ) ;
#35241 = CARTESIAN_POINT ( 'NONE',  ( 21.14999999999999858, 64.35000000001204512, -124.3731074845243825 ) ) ;
#35242 = ORIENTED_EDGE ( 'NONE', *, *, #141732, .F. ) ;
#35243 = FACE_OUTER_BOUND ( 'NONE', #27646, .T. ) ;
#35244 = EDGE_CURVE ( 'NONE', #184113, #112510, #174489, .T. ) ;
#35246 = CARTESIAN_POINT ( 'NONE',  ( -23.15000000000000213, 4.350000000011156054, -121.6500000000000341 ) ) ;
#35245 = AXIS2_PLACEMENT_3D ( 'NONE', #88550, #211089, #106838 ) ;
#35247 = CARTESIAN_POINT ( 'NONE',  ( 14.22916352759893321, 9.457410930301314522, -85.49991590874631697 ) ) ;
#35248 = DIRECTION ( 'NONE',  ( 1.000000000000000000, 0.000000000000000000, 0.000000000000000000 ) ) ;
#35249 = VECTOR ( 'NONE', #133907, 1000.000000000000114 ) ;
#35250 = DIRECTION ( 'NONE',  ( -1.000000000000000000, 0.000000000000000000, 0.000000000000000000 ) ) ;
#35251 = AXIS2_PLACEMENT_3D ( 'NONE', #250550, #15835, #253109 ) ;
#35252 = CARTESIAN_POINT ( 'NONE',  ( 18.49999999999999289, 10.20857864608310273, -24.70250686562995668 ) ) ;
#35253 = CARTESIAN_POINT ( 'NONE',  ( 13.99999999999999822, 66.15000000001155911, -52.77310748452440237 ) ) ;
#35254 = AXIS2_PLACEMENT_3D ( 'NONE', #60718, #7166, #144107 ) ;
#35255 = EDGE_CURVE ( 'NONE', #184383, #224941, #78725, .T. ) ;
#35257 = ADVANCED_FACE ( 'NONE', ( #229795 ), #171162, .T. ) ;
#35256 = VECTOR ( 'NONE', #134042, 1000.000000000000114 ) ;
#35258 = ORIENTED_EDGE ( 'NONE', *, *, #121036, .F. ) ;
#35259 = FACE_OUTER_BOUND ( 'NONE', #210571, .T. ) ;
#35261 = ORIENTED_EDGE ( 'NONE', *, *, #199743, .F. ) ;
#35260 = CARTESIAN_POINT ( 'NONE',  ( 23.15000000000000213, -11.64999999998883595, -130.9000000000000341 ) ) ;
#35262 = CARTESIAN_POINT ( 'NONE',  ( -23.15000000000000213, 2.000000000011154189, -154.7753780772379173 ) ) ;
#35263 = DIRECTION ( 'NONE',  ( 0.000000000000000000, -0.2617529984187939029, -0.9651348961770944701 ) ) ;
#35265 = EDGE_CURVE ( 'NONE', #55596, #250549, #224491, .T. ) ;
#35264 = CARTESIAN_POINT ( 'NONE',  ( -22.59999999999999787, 31.76322370622491320, -238.8696546380523671 ) ) ;
#35266 = EDGE_CURVE ( 'NONE', #199045, #164389, #20317, .T. ) ;
#35267 = ORIENTED_EDGE ( 'NONE', *, *, #25644, .F. ) ;
#35268 = CARTESIAN_POINT ( 'NONE',  ( -16.77431908686106965, 66.05419424549462803, -190.8589467021746486 ) ) ;
#35269 = AXIS2_PLACEMENT_3D ( 'NONE', #127013, #206550, #170041 ) ;
#35270 = VECTOR ( 'NONE', #70806, 1000.000000000000000 ) ;
#35271 = SHAPE_DEFINITION_REPRESENTATION ( #51454, #88607 ) ;
#35272 = AXIS2_PLACEMENT_3D ( 'NONE', #32443, #70281, #54531 ) ;
#35274 = AXIS2_PLACEMENT_3D ( 'NONE', #101001, #180596, #75104 ) ;
#35273 = DIRECTION ( 'NONE',  ( -1.000000000000000000, -0.000000000000000000, -0.000000000000000000 ) ) ;
#35275 = CARTESIAN_POINT ( 'NONE',  ( -23.15000000000000213, 4.350000000011156054, -188.8499999999999659 ) ) ;
#35276 = ADVANCED_FACE ( 'NONE', ( #9464 ), #166089, .T. ) ;
#35277 = ORIENTED_EDGE ( 'NONE', *, *, #248054, .F. ) ;
#35278 = LINE ( 'NONE', #233463, #233547 ) ;
#35279 = DIRECTION ( 'NONE',  ( -1.000000000000000000, 3.469446951953635015E-14, 0.000000000000000000 ) ) ;
#35280 = VECTOR ( 'NONE', #9363, 1000.000000000000000 ) ;
#35281 = EDGE_CURVE ( 'NONE', #25616, #75851, #168595, .T. ) ;
#35283 = EDGE_CURVE ( 'NONE', #86816, #64487, #29074, .T. ) ;
#35282 = EDGE_CURVE ( 'NONE', #77452, #113079, #232704, .T. ) ;
#35284 = CIRCLE ( 'NONE', #85083, 0.1000000000000028644 ) ;
#35285 = DIRECTION ( 'NONE',  ( 0.000000000000000000, -0.8814952561688437216, 0.4721928772777334582 ) ) ;
#35286 = ORIENTED_EDGE ( 'NONE', *, *, #4857, .T. ) ;
#35287 = ORIENTED_EDGE ( 'NONE', *, *, #241584, .T. ) ;
#35288 = AXIS2_PLACEMENT_3D ( 'NONE', #21903, #139246, #218797 ) ;
#35289 = VECTOR ( 'NONE', #219068, 1000.000000000000000 ) ;
#35290 = DIRECTION ( 'NONE',  ( 0.000000000000000000, 1.000000000000000000, 0.000000000000000000 ) ) ;
#35291 = CARTESIAN_POINT ( 'NONE',  ( 20.94999999999999929, 10.72371710471867701, -88.25000000000005684 ) ) ;
#35292 = ADVANCED_FACE ( 'NONE', ( #210253 ), #86402, .T. ) ;
#35293 = DIRECTION ( 'NONE',  ( -0.7071067811865475727, -0.7071067811865475727, 0.000000000000000000 ) ) ;
#35295 = DIRECTION ( 'NONE',  ( 1.000000000000000000, 0.000000000000000000, 0.000000000000000000 ) ) ;
#35294 = DIRECTION ( 'NONE',  ( -1.000000000000000000, 0.000000000000000000, -0.000000000000000000 ) ) ;
#35297 = ADVANCED_FACE ( 'NONE', ( #91576 ), #8199, .T. ) ;
#35296 = LINE ( 'NONE', #236013, #131010 ) ;
#35298 = CARTESIAN_POINT ( 'NONE',  ( 18.49999999999999289, 65.70729864260954400, -30.56574559737245877 ) ) ;
#35300 = EDGE_CURVE ( 'NONE', #157067, #221948, #141124, .T. ) ;
#35299 = DIRECTION ( 'NONE',  ( -0.000000000000000000, -1.000000000000000000, -7.272083257015735086E-15 ) ) ;
#35301 = ORIENTED_EDGE ( 'NONE', *, *, #100830, .T. ) ;
#35302 = VERTEX_POINT ( 'NONE', #131981 ) ;
#35303 = CARTESIAN_POINT ( 'NONE',  ( -21.05000000000000071, 77.25000000001209344, -128.5231074845242745 ) ) ;
#35304 = CARTESIAN_POINT ( 'NONE',  ( -16.87036670365547408, 66.01058118071060221, -149.0435473672224305 ) ) ;
#35306 = DIRECTION ( 'NONE',  ( 1.000000000000000000, 0.000000000000000000, 0.000000000000000000 ) ) ;
#35305 = CARTESIAN_POINT ( 'NONE',  ( 21.08621493067296271, 69.65070570883999324, -69.57930232400047998 ) ) ;
#35307 = ADVANCED_FACE ( 'NONE', ( #175016 ), #193252, .F. ) ;
#35308 = DIRECTION ( 'NONE',  ( 0.000000000000000000, -0.8741572761215280485, 0.4856429311786498171 ) ) ;
#35309 = CARTESIAN_POINT ( 'NONE',  ( -23.49999999999994316, 87.60324567546805952, -37.87437456276921210 ) ) ;
#35310 = CARTESIAN_POINT ( 'NONE',  ( -18.59999999999999787, 77.83534155023646406, -124.9679561919613064 ) ) ;
#35311 = ORIENTED_EDGE ( 'NONE', *, *, #27763, .F. ) ;
#35312 = ADVANCED_FACE ( 'NONE', ( #97964 ), #211527, .T. ) ;
#35313 = VERTEX_POINT ( 'NONE', #232393 ) ;
#35314 = TOROIDAL_SURFACE ( 'NONE', #214330, 12.77499999999999858, 0.1000000000000000056 ) ;
#35315 = AXIS2_PLACEMENT_3D ( 'NONE', #134116, #170752, #96272 ) ;
#35316 = CARTESIAN_POINT ( 'NONE',  ( -22.39999999999999858, 11.65000000001115588, -167.3999999999999773 ) ) ;
#35317 = ORIENTED_EDGE ( 'NONE', *, *, #138443, .T. ) ;
#35318 = LINE ( 'NONE', #198197, #72249 ) ;
#35319 = CIRCLE ( 'NONE', #181032, 0.09999999999999867328 ) ;
#35320 = DIRECTION ( 'NONE',  ( -0.000000000000000000, 0.2128009952263604232, -0.9770955615653316162 ) ) ;
#35321 = CARTESIAN_POINT ( 'NONE',  ( 21.04999999999999716, 8.871279686006802834, -142.5586289951409640 ) ) ;
#35322 = TOROIDAL_SURFACE ( 'NONE', #72722, 0.6000000000000006439, 0.1000000000000000056 ) ;
#35323 = ORIENTED_EDGE ( 'NONE', *, *, #254490, .T. ) ;
#35324 = DIRECTION ( 'NONE',  ( 1.000000000000000000, 0.000000000000000000, 0.000000000000000000 ) ) ;
#35325 = CARTESIAN_POINT ( 'NONE',  ( -21.05000000000000071, 55.11435547888748232, -226.8560373590520101 ) ) ;
#35327 = CIRCLE ( 'NONE', #81234, 4.000000000000000000 ) ;
#35326 = CARTESIAN_POINT ( 'NONE',  ( 18.59999999999999076, 65.79142135624880439, -48.17310748452439384 ) ) ;
#35328 = CARTESIAN_POINT ( 'NONE',  ( 23.15000000000000213, 85.60000000001220144, -146.4170766071767389 ) ) ;
#35329 = CARTESIAN_POINT ( 'NONE',  ( 22.01447462590973458, 75.90096299995266804, -143.7869076857541870 ) ) ;
#35331 = VECTOR ( 'NONE', #207526, 1000.000000000000000 ) ;
#35330 = DIRECTION ( 'NONE',  ( 1.000000000000000000, -0.000000000000000000, -0.000000000000000000 ) ) ;
#35333 = DIRECTION ( 'NONE',  ( 1.000000000000000000, 0.000000000000000000, 0.000000000000000000 ) ) ;
#35332 = CARTESIAN_POINT ( 'NONE',  ( 20.94999999999999574, 1.162701749949165642, -75.00000000000004263 ) ) ;
#35334 = VECTOR ( 'NONE', #64360, 1000.000000000000000 ) ;
#35335 = CARTESIAN_POINT ( 'NONE',  ( -16.84981964351528916, 66.08268176591339227, -149.3927090985447705 ) ) ;
#35336 = ORIENTED_EDGE ( 'NONE', *, *, #59183, .T. ) ;
#35338 = CARTESIAN_POINT ( 'NONE',  ( -23.25000000000000000, 0.000000000000000000, -33.50000000000000000 ) ) ;
#35337 = SPHERICAL_SURFACE ( 'NONE', #99313, 0.1000000000000000056 ) ;
#35339 = ORIENTED_EDGE ( 'NONE', *, *, #136519, .F. ) ;
#35341 = ORIENTED_EDGE ( 'NONE', *, *, #199125, .F. ) ;
#35340 = DIRECTION ( 'NONE',  ( 0.000000000000000000, 0.000000000000000000, 1.000000000000000000 ) ) ;
#35342 = ORIENTED_EDGE ( 'NONE', *, *, #220646, .T. ) ;
#35343 = CARTESIAN_POINT ( 'NONE',  ( -16.90202395485792408, 9.965944544561779139, -146.5969862787401325 ) ) ;
#35344 = FACE_OUTER_BOUND ( 'NONE', #1152, .T. ) ;
#35345 = DIRECTION ( 'NONE',  ( 0.000000000000000000, -6.982962677686266711E-15, 1.000000000000000000 ) ) ;
#35346 = LINE ( 'NONE', #196936, #25238 ) ;
#35347 = ORIENTED_EDGE ( 'NONE', *, *, #66719, .T. ) ;
#35348 = CARTESIAN_POINT ( 'NONE',  ( -18.34374000495060386, 40.40989152675300033, -235.2989281452919954 ) ) ;
#35350 = DIRECTION ( 'NONE',  ( -7.304098846218134667E-16, 1.000000000000000000, 6.982962677686266711E-15 ) ) ;
#35349 = CIRCLE ( 'NONE', #222723, 0.1000000000000028644 ) ;
#35351 = EDGE_LOOP ( 'NONE', ( #155979, #79098, #84801, #246178 ) ) ;
#35352 = PLANE ( 'NONE',  #148294 ) ;
#35353 = VECTOR ( 'NONE', #120466, 1000.000000000000000 ) ;
#35354 = EDGE_CURVE ( 'NONE', #136961, #51884, #152871, .T. ) ;
#35355 = CARTESIAN_POINT ( 'NONE',  ( -20.94999999999999929, 77.36242903720570041, -162.1342262366031548 ) ) ;
#35356 = EDGE_LOOP ( 'NONE', ( #5990, #210522, #148025, #184212 ) ) ;
#35357 = EDGE_LOOP ( 'NONE', ( #76984, #82794, #192357 ) ) ;
#35358 = EDGE_CURVE ( 'NONE', #5240, #176861, #216655, .T. ) ;
#35359 = DIRECTION ( 'NONE',  ( 0.000000000000000000, 1.000000000000000000, 0.000000000000000000 ) ) ;
#35360 = AXIS2_PLACEMENT_3D ( 'NONE', #257963, #241030, #179779 ) ;
#35361 = AXIS2_PLACEMENT_3D ( 'NONE', #13957, #251253, #190018 ) ;
#35362 = EDGE_LOOP ( 'NONE', ( #208361, #22241, #169891, #53061 ) ) ;
#35363 = AXIS2_PLACEMENT_3D ( 'NONE', #230260, #247250, #12531 ) ;
#35364 = DIRECTION ( 'NONE',  ( 1.000000000000000000, 0.000000000000000000, 0.000000000000000000 ) ) ;
#35365 = ORIENTED_EDGE ( 'NONE', *, *, #25604, .T. ) ;
#35366 = LINE ( 'NONE', #212689, #184332 ) ;
#35367 = B_SPLINE_CURVE_WITH_KNOTS ( 'NONE', 3,
 ( #135556, #113440, #230846, #92578, #212559, #13080, #35225, #136848, #156460, #192989 ),
 .UNSPECIFIED., .F., .F.,
 ( 4, 2, 2, 2, 4 ),
 ( 5.247129907028296623E-16, 9.930191194499898442E-05, 0.0001986038238894732421, 0.0003972076477784217846, 0.0007944152955563189237 ),
 .UNSPECIFIED. ) ;
#35368 = EDGE_CURVE ( 'NONE', #178487, #1827, #177573, .T. ) ;
#35369 = EDGE_CURVE ( 'NONE', #161400, #76954, #74622, .T. ) ;
#35370 = DIRECTION ( 'NONE',  ( 1.000000000000000000, -0.000000000000000000, -0.000000000000000000 ) ) ;
#35371 = CARTESIAN_POINT ( 'NONE',  ( 21.05000000000000071, 60.98263066423243117, -225.3662366191166200 ) ) ;
#35372 = FACE_OUTER_BOUND ( 'NONE', #182739, .T. ) ;
#35373 = CARTESIAN_POINT ( 'NONE',  ( -22.32929514600008503, 0.09907567812507747651, -25.92135243462349692 ) ) ;
#35374 = DIRECTION ( 'NONE',  ( -0.000000000000000000, 0.000000000000000000, 1.000000000000000000 ) ) ;
#35375 = DIRECTION ( 'NONE',  ( 1.000000000000000000, 0.000000000000000000, 0.000000000000000000 ) ) ;
#35376 = EDGE_LOOP ( 'NONE', ( #161953, #36494, #12651, #167338 ) ) ;
#35377 = DIRECTION ( 'NONE',  ( 1.000000000000000000, 0.000000000000000000, 0.000000000000000000 ) ) ;
#35378 = ORIENTED_EDGE ( 'NONE', *, *, #180100, .F. ) ;
#35381 = ORIENTED_EDGE ( 'NONE', *, *, #147076, .F. ) ;
#35380 = CARTESIAN_POINT ( 'NONE',  ( -21.05000000000000071, 4.639061695946145925, -222.3006832421257286 ) ) ;
#35379 = DIRECTION ( 'NONE',  ( 1.000000000000000000, 0.000000000000000000, 0.000000000000000000 ) ) ;
#35382 = ADVANCED_FACE ( 'NONE', ( #96672 ), #114987, .T. ) ;
#35383 = ORIENTED_EDGE ( 'NONE', *, *, #24174, .F. ) ;
#35384 = LINE ( 'NONE', #14525, #251553 ) ;
#35385 = ADVANCED_FACE ( 'NONE', ( #197081 ), #158017, .F. ) ;
#35386 = CARTESIAN_POINT ( 'NONE',  ( 18.59999999999999787, 76.00000000001213607, -136.5231074845242745 ) ) ;
#35387 = CARTESIAN_POINT ( 'NONE',  ( 21.05000000000000071, 76.10000000001166143, -69.52310748452431710 ) ) ;
#35388 = CARTESIAN_POINT ( 'NONE',  ( -18.38817693311004575, 64.51850848411244499, -145.7731074845244450 ) ) ;
#35389 = AXIS2_PLACEMENT_3D ( 'NONE', #169677, #189201, #66683 ) ;
#35390 = ORIENTED_EDGE ( 'NONE', *, *, #213108, .T. ) ;
#35392 = ORIENTED_EDGE ( 'NONE', *, *, #253422, .T. ) ;
#35391 = DIRECTION ( 'NONE',  ( 0.000000000000000000, -1.000000000000000000, -8.717686153663073805E-15 ) ) ;
#35393 = CARTESIAN_POINT ( 'NONE',  ( 20.95512820512820440, 10.62384868371188062, -7.664913569087605794 ) ) ;
#35395 = ORIENTED_EDGE ( 'NONE', *, *, #84663, .T. ) ;
#35394 = CARTESIAN_POINT ( 'NONE',  ( -16.94165728009537375, 9.987869755934930538, -54.39105500851019315 ) ) ;
#35396 = EDGE_CURVE ( 'NONE', #47883, #21693, #32931, .T. ) ;
#35397 = EDGE_LOOP ( 'NONE', ( #244513, #142949, #152800, #29355, #37732, #82866 ) ) ;
#35398 = ADVANCED_FACE ( 'NONE', ( #173734 ), #212817, .F. ) ;
#35399 = DIRECTION ( 'NONE',  ( 1.000000000000000000, -0.000000000000000000, -0.000000000000000000 ) ) ;
#35400 = AXIS2_PLACEMENT_3D ( 'NONE', #138948, #20348, #60715 ) ;
#35401 = TOROIDAL_SURFACE ( 'NONE', #160292, 0.2000000000000000111, 0.1000000000000000056 ) ;
#35402 = CARTESIAN_POINT ( 'NONE',  ( -21.56666275994540172, 65.41016251146584182, -242.5699255415354685 ) ) ;
#35403 = ORIENTED_EDGE ( 'NONE', *, *, #144346, .F. ) ;
#35404 = CYLINDRICAL_SURFACE ( 'NONE', #176699, 0.5000000000000004441 ) ;
#35405 = ORIENTED_EDGE ( 'NONE', *, *, #168326, .T. ) ;
#35406 = DIRECTION ( 'NONE',  ( 1.020425574104004394E-15, -0.9126074666063770380, -0.4088369013363281068 ) ) ;
#35407 = DIRECTION ( 'NONE',  ( 2.952720810173289112E-16, -1.000000000000000000, 0.000000000000000000 ) ) ;
#35408 = ORIENTED_EDGE ( 'NONE', *, *, #177498, .T. ) ;
#35409 = EDGE_CURVE ( 'NONE', #207337, #15628, #158095, .T. ) ;
#35410 = CARTESIAN_POINT ( 'NONE',  ( -17.11825945287482753, 60.96553306590055854, -220.9452142459683159 ) ) ;
#35411 = ADVANCED_FACE ( 'NONE', ( #214091 ), #176275, .F. ) ;
#35412 = CIRCLE ( 'NONE', #201981, 0.1000000000000002554 ) ;
#35413 = EDGE_CURVE ( 'NONE', #209692, #103352, #94134, .T. ) ;
#35414 = CARTESIAN_POINT ( 'NONE',  ( 20.94999999999999929, 5.000000000011153745, -188.9947339810868812 ) ) ;
#35415 = AXIS2_PLACEMENT_3D ( 'NONE', #10329, #29903, #151115 ) ;
#35416 = AXIS2_PLACEMENT_3D ( 'NONE', #76315, #196280, #60609 ) ;
#35417 = ORIENTED_EDGE ( 'NONE', *, *, #108225, .T. ) ;
#35418 = ORIENTED_EDGE ( 'NONE', *, *, #128526, .F. ) ;
#35419 = CARTESIAN_POINT ( 'NONE',  ( 20.74625933824019697, 18.86462450770046928, -229.9421460041290004 ) ) ;
#35420 = EDGE_LOOP ( 'NONE', ( #245849, #194838, #206574, #74006 ) ) ;
#35421 = ORIENTED_EDGE ( 'NONE', *, *, #22453, .T. ) ;
#35423 = ORIENTED_EDGE ( 'NONE', *, *, #140617, .F. ) ;
#35422 = FACE_OUTER_BOUND ( 'NONE', #115682, .T. ) ;
#35424 = EDGE_CURVE ( 'NONE', #56815, #74339, #178755, .T. ) ;
#35425 = ORIENTED_EDGE ( 'NONE', *, *, #36559, .F. ) ;
#35426 = DIRECTION ( 'NONE',  ( -0.000000000000000000, -0.1350103645451945777, 0.9908441862701590219 ) ) ;
#35427 = ORIENTED_EDGE ( 'NONE', *, *, #63896, .F. ) ;
#35430 = ORIENTED_EDGE ( 'NONE', *, *, #228409, .T. ) ;
#35429 = ORIENTED_EDGE ( 'NONE', *, *, #127975, .T. ) ;
#35428 = DIRECTION ( 'NONE',  ( 0.000000000000000000, 0.9594490217226103734, 0.2818822000686205254 ) ) ;
#35431 = EDGE_CURVE ( 'NONE', #12989, #225036, #215365, .T. ) ;
#35432 = ORIENTED_EDGE ( 'NONE', *, *, #90316, .F. ) ;
#35433 = DIRECTION ( 'NONE',  ( -1.000000000000000000, 0.000000000000000000, 0.000000000000000000 ) ) ;
#35434 = CIRCLE ( 'NONE', #151943, 0.09999999999999997780 ) ;
#35435 = AXIS2_PLACEMENT_3D ( 'NONE', #119801, #144445, #23274 ) ;
#35436 = DIRECTION ( 'NONE',  ( 1.000000000000000000, 0.000000000000000000, 0.000000000000000000 ) ) ;
#35437 = VECTOR ( 'NONE', #54811, 1000.000000000000000 ) ;
#35438 = VERTEX_POINT ( 'NONE', #195838 ) ;
#35439 = DIRECTION ( 'NONE',  ( -1.000000000000000000, 0.000000000000000000, 0.000000000000000000 ) ) ;
#35440 = EDGE_CURVE ( 'NONE', #22816, #72890, #124732, .T. ) ;
#35442 = ORIENTED_EDGE ( 'NONE', *, *, #79127, .F. ) ;
#35441 = CARTESIAN_POINT ( 'NONE',  ( -20.64999999999999858, 76.00000000001227818, -157.1481074845243882 ) ) ;
#35443 = DIRECTION ( 'NONE',  ( 0.000000000000000000, 1.000000000000000000, 0.000000000000000000 ) ) ;
#35444 = ORIENTED_EDGE ( 'NONE', *, *, #89907, .F. ) ;
#35445 = ORIENTED_EDGE ( 'NONE', *, *, #54578, .F. ) ;
#35446 = TOROIDAL_SURFACE ( 'NONE', #89376, 7.800000000000000711, 0.1000000000000000056 ) ;
#35447 = AXIS2_PLACEMENT_3D ( 'NONE', #39523, #201122, #143712 ) ;
#35448 = TOROIDAL_SURFACE ( 'NONE', #135344, 0.2000000000000000111, 0.1000000000000000056 ) ;
#35449 = DIRECTION ( 'NONE',  ( 1.000000000000000000, 0.000000000000000000, 0.000000000000000000 ) ) ;
#35450 = CARTESIAN_POINT ( 'NONE',  ( -20.85000000000000142, 64.25000000001220712, -143.3069731475025321 ) ) ;
#35451 = CIRCLE ( 'NONE', #176898, 2.099999999999990763 ) ;
#35452 = ORIENTED_EDGE ( 'NONE', *, *, #198268, .T. ) ;
#35453 = VERTEX_POINT ( 'NONE', #19761 ) ;
#35454 = DIRECTION ( 'NONE',  ( -1.000000000000000000, 0.000000000000000000, 0.000000000000000000 ) ) ;
#35455 = CARTESIAN_POINT ( 'NONE',  ( 20.85000000000000142, 45.93315328338058379, -256.6017782078560003 ) ) ;
#35458 = EDGE_LOOP ( 'NONE', ( #21759, #193279, #254171, #216148 ) ) ;
#35457 = ORIENTED_EDGE ( 'NONE', *, *, #174891, .F. ) ;
#35456 = VECTOR ( 'NONE', #176828, 1000.000000000000000 ) ;
#35459 = ORIENTED_EDGE ( 'NONE', *, *, #77674, .F. ) ;
#35460 = CARTESIAN_POINT ( 'NONE',  ( -20.54999999999999716, 76.00000000001143974, -37.92310748452432989 ) ) ;
#35461 = ORIENTED_EDGE ( 'NONE', *, *, #109691, .F. ) ;
#35462 = AXIS2_PLACEMENT_3D ( 'NONE', #136586, #38799, #2208 ) ;
#35463 = ORIENTED_EDGE ( 'NONE', *, *, #197, .T. ) ;
#35464 = SPHERICAL_SURFACE ( 'NONE', #138221, 0.1000000000000000056 ) ;
#35465 = ORIENTED_EDGE ( 'NONE', *, *, #179990, .F. ) ;
#35466 = CARTESIAN_POINT ( 'NONE',  ( -5.900000000000003020, -11.34999999999999964, 10.00000000000000178 ) ) ;
#35467 = AXIS2_PLACEMENT_3D ( 'NONE', #198929, #176827, #78958 ) ;
#35468 = VECTOR ( 'NONE', #203049, 1000.000000000000000 ) ;
#35469 = DIRECTION ( 'NONE',  ( -0.000000000000000000, 0.000000000000000000, -1.000000000000000000 ) ) ;
#35470 = ORIENTED_EDGE ( 'NONE', *, *, #70609, .F. ) ;
#35471 = ORIENTED_EDGE ( 'NONE', *, *, #151758, .T. ) ;
#35472 = FACE_OUTER_BOUND ( 'NONE', #241576, .T. ) ;
#35473 = EDGE_LOOP ( 'NONE', ( #107809, #116251, #153518 ) ) ;
#35474 = DIRECTION ( 'NONE',  ( 0.000000000000000000, 7.086529944415894657E-15, -1.000000000000000000 ) ) ;
#35475 = ORIENTED_EDGE ( 'NONE', *, *, #78991, .T. ) ;
#35476 = ORIENTED_EDGE ( 'NONE', *, *, #1312, .T. ) ;
#35477 = DIRECTION ( 'NONE',  ( 1.000000000000000000, 0.000000000000000000, 0.000000000000000000 ) ) ;
#35478 = EDGE_CURVE ( 'NONE', #88823, #254838, #124947, .T. ) ;
#35480 = ORIENTED_EDGE ( 'NONE', *, *, #105279, .T. ) ;
#35479 = DIRECTION ( 'NONE',  ( 0.000000000000000000, 0.000000000000000000, -1.000000000000000000 ) ) ;
#35481 = CARTESIAN_POINT ( 'NONE',  ( -21.44999999999999929, 68.65000000001180069, -81.77310748452435973 ) ) ;
#35482 = CARTESIAN_POINT ( 'NONE',  ( -18.59999999999999787, 38.29773864426884700, -236.0513742605307925 ) ) ;
#35483 = CARTESIAN_POINT ( 'NONE',  ( 20.95035502843362707, 65.52236167323562199, -128.9468077757879882 ) ) ;
#35484 = DIRECTION ( 'NONE',  ( -1.000000000000000000, 0.000000000000000000, 0.000000000000000000 ) ) ;
#35485 = CARTESIAN_POINT ( 'NONE',  ( 21.05000000000000071, 76.00000000001212186, -134.5231074845243313 ) ) ;
#35486 = LINE ( 'NONE', #215364, #164842 ) ;
#35487 = AXIS2_PLACEMENT_3D ( 'NONE', #35978, #115491, #118063 ) ;
#35488 = EDGE_CURVE ( 'NONE', #47548, #194507, #58838, .T. ) ;
#35489 = DIRECTION ( 'NONE',  ( 1.000000000000000000, 0.000000000000000000, 0.000000000000000000 ) ) ;
#35491 = EDGE_CURVE ( 'NONE', #47348, #74533, #99561, .T. ) ;
#35490 = FACE_OUTER_BOUND ( 'NONE', #33364, .T. ) ;
#35492 = CARTESIAN_POINT ( 'NONE',  ( -21.78635804494510708, 68.96433851485846844, -69.62211255003204258 ) ) ;
#35493 = DIRECTION ( 'NONE',  ( -1.000000000000000000, -0.000000000000000000, -0.000000000000000000 ) ) ;
#35494 = DIRECTION ( 'NONE',  ( 5.603264701231745086E-32, 7.172728831056619538E-15, -1.000000000000000000 ) ) ;
#35495 = AXIS2_PLACEMENT_3D ( 'NONE', #72900, #190260, #191561 ) ;
#35496 = B_SPLINE_CURVE_WITH_KNOTS ( 'NONE', 3,
 ( #24604, #207070, #28469, #107964, #83232, #162822, #8866, #88370, #167970, #51813 ),
 .UNSPECIFIED., .F., .F.,
 ( 4, 3, 3, 4 ),
 ( -2.000561356221172119E-06, 0.000000000000000000, 1.787822682429087714E-05, 4.206475347090508942E-05 ),
 .UNSPECIFIED. ) ;
#35497 = ORIENTED_EDGE ( 'NONE', *, *, #107833, .F. ) ;
#35498 = CIRCLE ( 'NONE', #118687, 0.1000000000000124678 ) ;
#35500 = VERTEX_POINT ( 'NONE', #224025 ) ;
#35499 = ORIENTED_EDGE ( 'NONE', *, *, #150943, .T. ) ;
#35501 = AXIS2_PLACEMENT_3D ( 'NONE', #199416, #140699, #122433 ) ;
#35502 = ORIENTED_EDGE ( 'NONE', *, *, #85243, .F. ) ;
#35503 = EDGE_CURVE ( 'NONE', #248708, #211242, #139663, .T. ) ;
#35504 = CARTESIAN_POINT ( 'NONE',  ( -18.50000000000000000, 7.120270961708746960, -70.65956304183933412 ) ) ;
#35505 = CARTESIAN_POINT ( 'NONE',  ( 20.96937028524355640, 10.62446937163783289, -141.4914261011695942 ) ) ;
#35507 = CARTESIAN_POINT ( 'NONE',  ( -22.39999999999999858, 25.97741635855165754, -254.4468634167653249 ) ) ;
#35506 = DIRECTION ( 'NONE',  ( 0.000000000000000000, 0.000000000000000000, -1.000000000000000000 ) ) ;
#35508 = VERTEX_POINT ( 'NONE', #87069 ) ;
#35510 = ORIENTED_EDGE ( 'NONE', *, *, #210323, .T. ) ;
#35509 = AXIS2_PLACEMENT_3D ( 'NONE', #36808, #41611, #81955 ) ;
#35511 = DIRECTION ( 'NONE',  ( 0.000000000000000000, 0.000000000000000000, -1.000000000000000000 ) ) ;
#35512 =( LENGTH_UNIT ( ) NAMED_UNIT ( * ) SI_UNIT ( .MILLI., .METRE. ) );
#35513 = CARTESIAN_POINT ( 'NONE',  ( 23.24999999999999289, 8.980461154494404852, -187.0187154576991304 ) ) ;
#35514 = CIRCLE ( 'NONE', #52023, 12.87499999999999112 ) ;
#35515 = DIRECTION ( 'NONE',  ( 0.000000000000000000, -1.000000000000000000, -6.982962677686266711E-15 ) ) ;
#35516 = DIRECTION ( 'NONE',  ( 1.000000000000000000, 0.000000000000000000, 0.000000000000000000 ) ) ;
#35517 = ORIENTED_EDGE ( 'NONE', *, *, #106028, .T. ) ;
#35518 = ORIENTED_EDGE ( 'NONE', *, *, #18917, .F. ) ;
#35519 = AXIS2_PLACEMENT_3D ( 'NONE', #15455, #144332, #2269 ) ;
#35520 = LINE ( 'NONE', #152897, #55028 ) ;
#35521 = CARTESIAN_POINT ( 'NONE',  ( 18.39999999999999858, 8.780520186313291120, -245.4165333277510115 ) ) ;
#35522 = ORIENTED_EDGE ( 'NONE', *, *, #191369, .F. ) ;
#35523 = EDGE_CURVE ( 'NONE', #215121, #150106, #82991, .T. ) ;
#35524 = CARTESIAN_POINT ( 'NONE',  ( 23.15000000000000213, -8.874060656858233642, -215.4698323230865640 ) ) ;
#35525 = DIRECTION ( 'NONE',  ( -0.000000000000000000, -0.000000000000000000, -1.000000000000000000 ) ) ;
#35526 = EDGE_CURVE ( 'NONE', #234655, #110369, #216292, .T. ) ;
#35527 = CIRCLE ( 'NONE', #118718, 0.09999999999999939493 ) ;
#35528 = CARTESIAN_POINT ( 'NONE',  ( -40.23850191057533010, 65.19115966511134275, -29.92310748452479174 ) ) ;
#35529 = CARTESIAN_POINT ( 'NONE',  ( 23.14999999999999858, 70.50000000001253397, -182.4283735034374843 ) ) ;
#35530 = VERTEX_POINT ( 'NONE', #107940 ) ;
#35531 = LINE ( 'NONE', #78456, #19579 ) ;
#35532 = CARTESIAN_POINT ( 'NONE',  ( -23.25000000000000000, 31.49702336731127872, -233.4564499823349877 ) ) ;
#35533 = LINE ( 'NONE', #150318, #131883 ) ;
#35535 = CARTESIAN_POINT ( 'NONE',  ( -23.25000000000000000, 36.65892442174935439, -249.5511627012433848 ) ) ;
#35534 = CARTESIAN_POINT ( 'NONE',  ( -16.80100426158790938, 66.05684947961590581, -123.8401617316903156 ) ) ;
#35536 = DIRECTION ( 'NONE',  ( -1.000000000000000000, -0.000000000000000000, 0.000000000000000000 ) ) ;
#35537 = EDGE_CURVE ( 'NONE', #25563, #76942, #160564, .T. ) ;
#35538 = DIRECTION ( 'NONE',  ( 1.000000000000000000, 0.000000000000000000, -0.000000000000000000 ) ) ;
#35539 = CARTESIAN_POINT ( 'NONE',  ( -21.64999999999999858, 10.05000000001113847, -113.1500000000000341 ) ) ;
#35540 = DIRECTION ( 'NONE',  ( 0.000000000000000000, 0.8700118002898393765, -0.4930308989875104575 ) ) ;
#35542 = EDGE_LOOP ( 'NONE', ( #155032, #65219, #202465, #63570, #225009 ) ) ;
#35541 = AXIS2_PLACEMENT_3D ( 'NONE', #184555, #22953, #45057 ) ;
#35543 = ORIENTED_EDGE ( 'NONE', *, *, #83493, .F. ) ;
#35544 = DIRECTION ( 'NONE',  ( 1.000000000000000000, 0.000000000000000000, 0.000000000000000000 ) ) ;
#35545 = ORIENTED_EDGE ( 'NONE', *, *, #65882, .F. ) ;
#35546 = DIRECTION ( 'NONE',  ( 0.000000000000000000, 0.2617529984165152257, 0.9651348961777124202 ) ) ;
#35548 = EDGE_CURVE ( 'NONE', #32792, #142560, #112090, .T. ) ;
#35547 = ORIENTED_EDGE ( 'NONE', *, *, #236977, .F. ) ;
#35549 = CARTESIAN_POINT ( 'NONE',  ( 21.10000000000000142, 6.223900101154157483, 12.00000000000000000 ) ) ;
#35550 = ORIENTED_EDGE ( 'NONE', *, *, #6986, .F. ) ;
#35551 = DIRECTION ( 'NONE',  ( 1.000000000000000000, 0.000000000000000000, 0.000000000000000000 ) ) ;
#35552 = CARTESIAN_POINT ( 'NONE',  ( 22.50000000000000000, 0.1000000000111554016, -88.75000000000004263 ) ) ;
#35553 = DIRECTION ( 'NONE',  ( 0.000000000000000000, -0.1298341882519953583, -0.9915357197604862671 ) ) ;
#35554 = EDGE_CURVE ( 'NONE', #162422, #254810, #220420, .T. ) ;
#35556 = ORIENTED_EDGE ( 'NONE', *, *, #62671, .F. ) ;
#35555 = CARTESIAN_POINT ( 'NONE',  ( -16.82055514392420648, 30.18270618454418752, -234.7943911448769256 ) ) ;
#35558 = CARTESIAN_POINT ( 'NONE',  ( 19.94784844284930969, 11.71308993304057999, -192.2021987172990407 ) ) ;
#35557 = DIRECTION ( 'NONE',  ( 1.000000000000000000, 0.000000000000000000, 0.000000000000000000 ) ) ;
#35559 = CARTESIAN_POINT ( 'NONE',  ( 19.75857864376268935, 64.35000000001147669, -44.77310748452440237 ) ) ;
#35560 = LINE ( 'NONE', #216728, #177374 ) ;
#35561 = CARTESIAN_POINT ( 'NONE',  ( -12.47155713865592297, 9.375669526436929857, -116.3677900093859989 ) ) ;
#35563 = EDGE_CURVE ( 'NONE', #107789, #3259, #41366, .T. ) ;
#35562 = CARTESIAN_POINT ( 'NONE',  ( -18.50000000000000355, 74.95904887477786360, -233.7774272632847783 ) ) ;
#35564 = ADVANCED_FACE ( 'NONE', ( #127509 ), #238797, .T. ) ;
#35565 = EDGE_LOOP ( 'NONE', ( #2952, #50676, #220488, #252924 ) ) ;
#35566 =( NAMED_UNIT ( * ) SI_UNIT ( $, .STERADIAN. ) SOLID_ANGLE_UNIT ( ) );
#35567 = DIRECTION ( 'NONE',  ( -1.000000000000000000, 0.000000000000000000, 0.000000000000000000 ) ) ;
#35568 = ORIENTED_EDGE ( 'NONE', *, *, #11070, .T. ) ;
#35569 = LINE ( 'NONE', #115078, #40390 ) ;
#35570 = EDGE_LOOP ( 'NONE', ( #200552, #8792, #232446, #183605, #130923, #63170 ) ) ;
#35571 = EDGE_CURVE ( 'NONE', #197037, #118795, #153820, .T. ) ;
#35572 = AXIS2_PLACEMENT_3D ( 'NONE', #28060, #142812, #185817 ) ;
#35574 = DIRECTION ( 'NONE',  ( 1.000000000000000000, 0.000000000000000000, 0.000000000000000000 ) ) ;
#35573 = AXIS2_PLACEMENT_3D ( 'NONE', #201989, #23380, #147136 ) ;
#35575 = EDGE_CURVE ( 'NONE', #224018, #8661, #27159, .T. ) ;
#35576 = LINE ( 'NONE', #236308, #240901 ) ;
#35577 = VERTEX_POINT ( 'NONE', #178856 ) ;
#35578 = EDGE_CURVE ( 'NONE', #160183, #175179, #145371, .T. ) ;
#35579 = VERTEX_POINT ( 'NONE', #64953 ) ;
#35580 = CARTESIAN_POINT ( 'NONE',  ( 23.14999999999999858, 1.115600667400684642E-11, -200.9999999999999432 ) ) ;
#35581 = CARTESIAN_POINT ( 'NONE',  ( 23.24999999999999289, 11.75000000001116263, -155.7499999999999716 ) ) ;
#35582 = EDGE_CURVE ( 'NONE', #233528, #195076, #79695, .T. ) ;
#35583 = CARTESIAN_POINT ( 'NONE',  ( -16.87998658237703964, 63.02981155563863069, -213.3338125889567038 ) ) ;
#35584 = DIRECTION ( 'NONE',  ( -0.000000000000000000, 0.1350103645451876666, 0.9908441862701600211 ) ) ;
#35587 = CARTESIAN_POINT ( 'NONE',  ( 20.94999999999999929, 87.48912529308779540, -72.62310748452422615 ) ) ;
#35586 = AXIS2_PLACEMENT_3D ( 'NONE', #50139, #11031, #185807 ) ;
#35585 = DIRECTION ( 'NONE',  ( -0.000000000000000000, 0.01283462868039629209, -0.9999176327611372095 ) ) ;
#35588 = CARTESIAN_POINT ( 'NONE',  ( -18.40000000000000213, 34.05335961020092839, -234.8258093264404636 ) ) ;
#35589 = AXIS2_PLACEMENT_3D ( 'NONE', #98786, #58385, #217471 ) ;
#35591 = EDGE_CURVE ( 'NONE', #64290, #63066, #212033, .T. ) ;
#35590 = CARTESIAN_POINT ( 'NONE',  ( 12.24999999999999467, 9.350000000011135626, -50.36426760761606403 ) ) ;
#35593 = EDGE_CURVE ( 'NONE', #193457, #254110, #62192, .T. ) ;
#35592 = CARTESIAN_POINT ( 'NONE',  ( -18.59999999999999787, -1.835859311443637010, -45.10443916879852821 ) ) ;
#35595 = EDGE_LOOP ( 'NONE', ( #24911, #27079, #5698, #56755 ) ) ;
#35594 = AXIS2_PLACEMENT_3D ( 'NONE', #48668, #146473, #243014 ) ;
#35596 = CARTESIAN_POINT ( 'NONE',  ( -16.87036670365548474, 9.989418819312801290, -188.4795601173020145 ) ) ;
#35597 = AXIS2_PLACEMENT_3D ( 'NONE', #224384, #147429, #207420 ) ;
#35599 = ORIENTED_EDGE ( 'NONE', *, *, #213269, .F. ) ;
#35598 = CARTESIAN_POINT ( 'NONE',  ( 21.05000000000000071, 0.000000000000000000, 0.000000000000000000 ) ) ;
#35600 = CARTESIAN_POINT ( 'NONE',  ( 22.50014994444007499, 11.74971973189203744, 0.08308015671907631461 ) ) ;
#35601 = CARTESIAN_POINT ( 'NONE',  ( 22.49231231312463208, 11.37015642645466507, -198.4612171126308624 ) ) ;
#35603 = CARTESIAN_POINT ( 'NONE',  ( -18.39999999999999858, -9.682403433465239573, -107.1568433774128408 ) ) ;
#35602 = DIRECTION ( 'NONE',  ( 1.000000000000000000, 0.000000000000000000, 0.000000000000000000 ) ) ;
#35604 =( GEOMETRIC_REPRESENTATION_CONTEXT ( 3 ) GLOBAL_UNCERTAINTY_ASSIGNED_CONTEXT ( ( #251122 ) ) GLOBAL_UNIT_ASSIGNED_CONTEXT ( ( #169260, #34874, #94809 ) ) REPRESENTATION_CONTEXT ( 'NONE', 'WORKASPACE' ) );
#35605 = EDGE_CURVE ( 'NONE', #159477, #245204, #47954, .T. ) ;
#35607 = VERTEX_POINT ( 'NONE', #92219 ) ;
#35606 = CARTESIAN_POINT ( 'NONE',  ( 21.00023020733438273, 69.60913075474442735, -136.5231074845243597 ) ) ;
#35609 = DIRECTION ( 'NONE',  ( 1.000000000000000000, -0.000000000000000000, -0.000000000000000000 ) ) ;
#35608 = DIRECTION ( 'NONE',  ( -0.000000000000000000, 0.9651348961777157509, -0.2617529984165028467 ) ) ;
#35610 = FACE_OUTER_BOUND ( 'NONE', #202536, .T. ) ;
#35611 = LINE ( 'NONE', #98079, #84610 ) ;
#35612 = CARTESIAN_POINT ( 'NONE',  ( -20.94999999999999929, 42.15997144203495139, -239.2817429668763793 ) ) ;
#35613 = CARTESIAN_POINT ( 'NONE',  ( 23.25000000000000000, 11.60058429089262333, -246.3380203656811887 ) ) ;
#35614 = ORIENTED_EDGE ( 'NONE', *, *, #49856, .T. ) ;
#35615 = CARTESIAN_POINT ( 'NONE',  ( 18.39999999999999858, -7.817436562502981801, -209.8389866834999111 ) ) ;
#35616 = EDGE_CURVE ( 'NONE', #219593, #172822, #74247, .T. ) ;
#35617 = ORIENTED_EDGE ( 'NONE', *, *, #229369, .T. ) ;
#35618 = EDGE_CURVE ( 'NONE', #96501, #214102, #95497, .T. ) ;
#35619 = EDGE_CURVE ( 'NONE', #17763, #154055, #248743, .T. ) ;
#35620 = CARTESIAN_POINT ( 'NONE',  ( -18.50000000000000000, -9.419084502813289461, -40.32990780702540690 ) ) ;
#35621 = ORIENTED_EDGE ( 'NONE', *, *, #253435, .F. ) ;
#35622 = DIRECTION ( 'NONE',  ( -1.000000000000000000, -0.000000000000000000, -0.000000000000000000 ) ) ;
#35623 = VECTOR ( 'NONE', #183555, 1000.000000000000000 ) ;
#35624 = ORIENTED_EDGE ( 'NONE', *, *, #191305, .T. ) ;
#35625 = FACE_OUTER_BOUND ( 'NONE', #237316, .T. ) ;
#35627 = CARTESIAN_POINT ( 'NONE',  ( 20.85000000000000142, 78.48087866980282001, -232.8271061603568910 ) ) ;
#35626 = VECTOR ( 'NONE', #62222, 1000.000000000000000 ) ;
#35628 = PLANE ( 'NONE',  #176763 ) ;
#35630 = ORIENTED_EDGE ( 'NONE', *, *, #56128, .T. ) ;
#35629 = AXIS2_PLACEMENT_3D ( 'NONE', #183135, #25356, #138815 ) ;
#35631 = EDGE_CURVE ( 'NONE', #88943, #120640, #228785, .T. ) ;
#35632 = AXIS2_PLACEMENT_3D ( 'NONE', #171022, #50989, #246643 ) ;
#35633 = VECTOR ( 'NONE', #34082, 1000.000000000000000 ) ;
#35635 = CARTESIAN_POINT ( 'NONE',  ( 20.94999999999999929, 71.14953271029291670, -182.0573748935260880 ) ) ;
#35634 = VECTOR ( 'NONE', #64285, 1000.000000000000000 ) ;
#35636 = LINE ( 'NONE', #96819, #45047 ) ;
#35637 = CARTESIAN_POINT ( 'NONE',  ( 21.30000000000002558, 76.00000000001234923, -165.9731074845243768 ) ) ;
#35638 = LINE ( 'NONE', #115140, #241240 ) ;
#35639 = DIRECTION ( 'NONE',  ( -1.000000000000000000, 0.000000000000000000, 0.000000000000000000 ) ) ;
#35640 = VERTEX_POINT ( 'NONE', #173101 ) ;
#35641 = CARTESIAN_POINT ( 'NONE',  ( 23.24999999999999289, 11.65000000001116298, -59.98519422934606382 ) ) ;
#35642 = ORIENTED_EDGE ( 'NONE', *, *, #109336, .F. ) ;
#35644 = ORIENTED_EDGE ( 'NONE', *, *, #161338, .F. ) ;
#35643 = CARTESIAN_POINT ( 'NONE',  ( 21.30000000000002558, 1.115600667400684642E-11, -96.45000000000003126 ) ) ;
#35645 = AXIS2_PLACEMENT_3D ( 'NONE', #40881, #220772, #64267 ) ;
#35646 = EDGE_LOOP ( 'NONE', ( #14580, #107300, #50922, #23268 ) ) ;
#35647 = CARTESIAN_POINT ( 'NONE',  ( 18.39999999999999858, 85.50000000001263345, -196.4910380878246201 ) ) ;
#35648 = CYLINDRICAL_SURFACE ( 'NONE', #67429, 12.87499999999999822 ) ;
#35649 = AXIS2_PLACEMENT_3D ( 'NONE', #25593, #122124, #23042 ) ;
#35650 = CARTESIAN_POINT ( 'NONE',  ( 21.05000000000000071, 74.83729825007408465, -128.4231074845243086 ) ) ;
#35651 = DIRECTION ( 'NONE',  ( -1.000000000000000000, 2.952720810173289112E-16, 2.061873921506763405E-30 ) ) ;
#35652 = ORIENTED_EDGE ( 'NONE', *, *, #19115, .F. ) ;
#35653 = CIRCLE ( 'NONE', #139636, 0.09999999999999917288 ) ;
#35654 = SPHERICAL_SURFACE ( 'NONE', #222220, 0.1000000000000000056 ) ;
#35655 = CARTESIAN_POINT ( 'NONE',  ( 19.99999999999998934, 51.28888318656201761, -230.2315015618842153 ) ) ;
#35656 = AXIS2_PLACEMENT_3D ( 'NONE', #114228, #154670, #135050 ) ;
#35657 = VERTEX_POINT ( 'NONE', #191361 ) ;
#35659 = ORIENTED_EDGE ( 'NONE', *, *, #123115, .T. ) ;
#35658 = CARTESIAN_POINT ( 'NONE',  ( -16.85718274719364373, 66.02385768539031119, -115.5864538167070066 ) ) ;
#35660 = DIRECTION ( 'NONE',  ( 2.694716079187272946E-16, -1.000000000000000000, 0.000000000000000000 ) ) ;
#35661 = CARTESIAN_POINT ( 'NONE',  ( -23.15000000000000213, 70.57516910782923958, -223.5255282078080654 ) ) ;
#35662 = EDGE_CURVE ( 'NONE', #83495, #182032, #3929, .T. ) ;
#35663 = DIRECTION ( 'NONE',  ( -1.000000000000000000, -0.000000000000000000, -0.000000000000000000 ) ) ;
#35664 = ADVANCED_FACE ( 'NONE', ( #193910 ), #37250, .T. ) ;
#35665 = ORIENTED_EDGE ( 'NONE', *, *, #179237, .F. ) ;
#35666 = CARTESIAN_POINT ( 'NONE',  ( -20.94999999999999929, 18.34743685832668803, -236.8753540304231535 ) ) ;
#35667 = ORIENTED_EDGE ( 'NONE', *, *, #174143, .F. ) ;
#35668 = DIRECTION ( 'NONE',  ( -0.000000000000000000, -0.000000000000000000, 1.000000000000000000 ) ) ;
#35669 = CARTESIAN_POINT ( 'NONE',  ( 20.94999999999999929, 64.35000000001249987, -176.8069731475025321 ) ) ;
#35670 = CARTESIAN_POINT ( 'NONE',  ( -23.25000000000000000, 77.14957036958807635, -162.2071950000224092 ) ) ;
#35671 = AXIS2_PLACEMENT_3D ( 'NONE', #4205, #47169, #244102 ) ;
#35672 = AXIS2_PLACEMENT_3D ( 'NONE', #158544, #136350, #218467 ) ;
#35673 = ADVANCED_FACE ( 'NONE', ( #29724 ), #12722, .T. ) ;
#35674 = CIRCLE ( 'NONE', #68985, 0.9750000000000036415 ) ;
#35675 = EDGE_LOOP ( 'NONE', ( #173577, #103307, #112416, #16467 ) ) ;
#35676 = DIRECTION ( 'NONE',  ( 1.000000000000000000, 0.000000000000000000, 0.000000000000000000 ) ) ;
#35677 = CIRCLE ( 'NONE', #23198, 12.87499999999999822 ) ;
#35678 = ORIENTED_EDGE ( 'NONE', *, *, #218113, .T. ) ;
#35679 = CARTESIAN_POINT ( 'NONE',  ( 18.59999999999999432, 77.63717271298267519, -158.4409541190523214 ) ) ;
#35680 = CARTESIAN_POINT ( 'NONE',  ( -20.54999999999999716, 4.350000000011156054, -112.8500000000000369 ) ) ;
#35683 = EDGE_LOOP ( 'NONE', ( #160800, #55527, #110988, #85239 ) ) ;
#35682 = FACE_OUTER_BOUND ( 'NONE', #176285, .T. ) ;
#35681 =( BOUNDED_CURVE ( )  B_SPLINE_CURVE ( 3, ( #14304, #233351, #129094, #152540 ),
 .UNSPECIFIED., .F., .F. ) 
 B_SPLINE_CURVE_WITH_KNOTS ( ( 4, 4 ),
 ( 4.712388980384689674, 6.283185307179586232 ),
 .UNSPECIFIED. ) 
 CURVE ( )  GEOMETRIC_REPRESENTATION_ITEM ( )  RATIONAL_B_SPLINE_CURVE ( ( 1.000000000000000000, 0.8047378541243649375, 0.8047378541243649375, 1.000000000000000000 ) ) 
 REPRESENTATION_ITEM ( '' )  );
#35684 = DIRECTION ( 'NONE',  ( 1.000000000000000000, 1.836970198721029934E-16, -0.000000000000000000 ) ) ;
#35685 = CARTESIAN_POINT ( 'NONE',  ( -23.25000000000000000, 0.000000000000000000, -33.50000000000000000 ) ) ;
#35686 = CARTESIAN_POINT ( 'NONE',  ( 19.58285714285715073, 39.37606100570253886, -236.9544388824136831 ) ) ;
#35688 = CYLINDRICAL_SURFACE ( 'NONE', #37982, 0.5000000000000004441 ) ;
#35687 = AXIS2_PLACEMENT_3D ( 'NONE', #90265, #30330, #173733 ) ;
#35689 = DIRECTION ( 'NONE',  ( -1.000000000000000000, -0.000000000000000000, -0.000000000000000000 ) ) ;
#35690 = CIRCLE ( 'NONE', #181426, 0.09999999999998898659 ) ;
#35691 = DIRECTION ( 'NONE',  ( -1.000000000000000000, -0.000000000000000000, -0.000000000000000000 ) ) ;
#35692 = CARTESIAN_POINT ( 'NONE',  ( -20.54999999999999716, 68.85000000001228670, -157.6731074845243938 ) ) ;
#35694 = ORIENTED_EDGE ( 'NONE', *, *, #48694, .F. ) ;
#35693 = CARTESIAN_POINT ( 'NONE',  ( -20.54999999999999716, 82.20113918088273408, -215.0418453737790401 ) ) ;
#35695 = VECTOR ( 'NONE', #23378, 1000.000000000000000 ) ;
#35696 = CIRCLE ( 'NONE', #248040, 0.5999999999999992006 ) ;
#35697 = DIRECTION ( 'NONE',  ( 0.000000000000000000, 0.000000000000000000, -1.000000000000000000 ) ) ;
#35698 = AXIS2_PLACEMENT_3D ( 'NONE', #225552, #229440, #50767 ) ;
#35699 = DIRECTION ( 'NONE',  ( 0.000000000000000000, 0.000000000000000000, -1.000000000000000000 ) ) ;
#35700 = CARTESIAN_POINT ( 'NONE',  ( -22.94999999999999929, 1.901609089591594692, -11.59510167572422112 ) ) ;
#35701 = VERTEX_POINT ( 'NONE', #152233 ) ;
#35702 = ADVANCED_FACE ( 'NONE', ( #231754 ), #209611, .T. ) ;
#35703 = DIRECTION ( 'NONE',  ( 0.000000000000000000, 0.000000000000000000, 1.000000000000000000 ) ) ;
#35704 = CARTESIAN_POINT ( 'NONE',  ( -21.55000000000000426, 29.50054346320101928, -236.9717244483098568 ) ) ;
#35705 = EDGE_CURVE ( 'NONE', #99016, #180036, #137192, .T. ) ;
#35706 = DIRECTION ( 'NONE',  ( 0.000000000000000000, 0.000000000000000000, -1.000000000000000000 ) ) ;
#35707 = ORIENTED_EDGE ( 'NONE', *, *, #35859, .T. ) ;
#35708 = AXIS2_PLACEMENT_3D ( 'NONE', #106965, #147390, #207380 ) ;
#35709 = DIRECTION ( 'NONE',  ( 0.000000000000000000, -0.4999999999999088507, 0.8660254037844913322 ) ) ;
#35710 = VECTOR ( 'NONE', #204944, 1000.000000000000000 ) ;
#35711 = DIRECTION ( 'NONE',  ( 0.000000000000000000, 6.982962677686266711E-15, -1.000000000000000000 ) ) ;
#35712 = ADVANCED_FACE ( 'NONE', ( #233047 ), #68830, .T. ) ;
#35713 = ORIENTED_EDGE ( 'NONE', *, *, #93472, .T. ) ;
#35714 = CARTESIAN_POINT ( 'NONE',  ( -17.80356949364257702, 65.12326860300646558, -46.31003446030745607 ) ) ;
#35715 = EDGE_LOOP ( 'NONE', ( #94497, #48979, #236396, #180970 ) ) ;
#35716 = FACE_OUTER_BOUND ( 'NONE', #32214, .T. ) ;
#35718 = ORIENTED_EDGE ( 'NONE', *, *, #77294, .F. ) ;
#35717 = CARTESIAN_POINT ( 'NONE',  ( 21.05000000000000071, 6.540656951712402467, -134.0000000000000284 ) ) ;
#35719 = EDGE_CURVE ( 'NONE', #226840, #225164, #104030, .T. ) ;
#35720 = ADVANCED_FACE ( 'NONE', ( #213454 ), #128801, .F. ) ;
#35721 = CARTESIAN_POINT ( 'NONE',  ( 18.59999999999999432, 44.55458850188623643, -247.3966190010231969 ) ) ;
#35722 = ORIENTED_EDGE ( 'NONE', *, *, #66590, .F. ) ;
#35723 = DIRECTION ( 'NONE',  ( 1.000000000000000000, 0.000000000000000000, 0.000000000000000000 ) ) ;
#35724 = EDGE_LOOP ( 'NONE', ( #85782, #196392, #117903, #176631 ) ) ;
#35726 = ORIENTED_EDGE ( 'NONE', *, *, #245544, .F. ) ;
#35725 = ORIENTED_EDGE ( 'NONE', *, *, #89291, .F. ) ;
#35727 = DIRECTION ( 'NONE',  ( -1.000000000000000000, 0.000000000000000000, 0.000000000000000000 ) ) ;
#35728 = EDGE_CURVE ( 'NONE', #207133, #136223, #154003, .T. ) ;
#35729 = ORIENTED_EDGE ( 'NONE', *, *, #245653, .T. ) ;
#35730 = DIRECTION ( 'NONE',  ( 0.000000000000000000, 0.1350103645451974088, -0.9908441862701587999 ) ) ;
#35731 = AXIS2_PLACEMENT_3D ( 'NONE', #95457, #57602, #175052 ) ;
#35732 = ORIENTED_EDGE ( 'NONE', *, *, #189787, .F. ) ;
#35733 = EDGE_LOOP ( 'NONE', ( #43743, #67980, #127891, #121743 ) ) ;
#35734 = B_SPLINE_CURVE_WITH_KNOTS ( 'NONE', 3,
 ( #213027, #111367, #150502, #173961, #69691, #13562, #190931, #113927, #230028, #29302, #130928, #53952, #133495, #108789, #12288, #231333, #34432, #52660, #89224 ),
 .UNSPECIFIED., .F., .F.,
 ( 4, 3, 3, 3, 3, 3, 4 ),
 ( 0.0001624081864585800018, 0.0001685232196531700956, 0.0001764526673566917288, 0.0001916878551483148813, 0.0002009890782182524550, 0.0002238845907555116882, 0.0002283406619926272728 ),
 .UNSPECIFIED. ) ;
#35735 = CARTESIAN_POINT ( 'NONE',  ( 23.15000000000000213, 87.48912529308749697, -39.02310748452423894 ) ) ;
#35736 = EDGE_CURVE ( 'NONE', #51036, #28439, #249811, .T. ) ;
#35737 = LINE ( 'NONE', #112682, #205398 ) ;
#35738 = DIRECTION ( 'NONE',  ( 0.000000000000000000, 0.000000000000000000, -1.000000000000000000 ) ) ;
#35739 = ORIENTED_EDGE ( 'NONE', *, *, #84262, .F. ) ;
#35740 = PLANE ( 'NONE',  #249377 ) ;
#35741 = CARTESIAN_POINT ( 'NONE',  ( -17.11825945287482753, 9.950000000011138823, -146.7500000000000284 ) ) ;
#35742 = DIRECTION ( 'NONE',  ( 0.000000000000000000, 0.000000000000000000, 1.000000000000000000 ) ) ;
#35743 = ORIENTED_EDGE ( 'NONE', *, *, #114055, .T. ) ;
#35744 = CARTESIAN_POINT ( 'NONE',  ( 20.94999999999999929, 38.42191493408704872, -250.4955484557988541 ) ) ;
#35745 = DIRECTION ( 'NONE',  ( 0.000000000000000000, 0.008583690987128220901, 0.9999631594459055250 ) ) ;
#35746 = LINE ( 'NONE', #76122, #207397 ) ;
#35747 = ORIENTED_EDGE ( 'NONE', *, *, #207477, .F. ) ;
#35748 = B_SPLINE_CURVE_WITH_KNOTS ( 'NONE', 3,
 ( #240116, #22366, #99287, #224383, #142283, #101851, #120199, #243951, #23661, #103143 ),
 .UNSPECIFIED., .F., .F.,
 ( 4, 3, 3, 4 ),
 ( 1.957469226477651626E-15, 8.145022132833432322E-06, 1.905645951092475529E-05, 2.061107371225855961E-05 ),
 .UNSPECIFIED. ) ;
#35749 = DIRECTION ( 'NONE',  ( 1.000000000000000000, 0.000000000000000000, 0.000000000000000000 ) ) ;
#35750 = ORIENTED_EDGE ( 'NONE', *, *, #199789, .T. ) ;
#35751 = ORIENTED_EDGE ( 'NONE', *, *, #34638, .T. ) ;
#35752 = AXIS2_PLACEMENT_3D ( 'NONE', #162575, #51239, #89104 ) ;
#35753 = DIRECTION ( 'NONE',  ( 0.000000000000000000, -0.7071067811865479058, -0.7071067811865472397 ) ) ;
#35754 = ORIENTED_EDGE ( 'NONE', *, *, #105723, .F. ) ;
#35755 = ORIENTED_EDGE ( 'NONE', *, *, #214977, .F. ) ;
#35756 = LINE ( 'NONE', #177835, #178169 ) ;
#35757 = CARTESIAN_POINT ( 'NONE',  ( -16.93344882324368683, 9.996588767299030565, -188.4130256948049009 ) ) ;
#35758 = ORIENTED_EDGE ( 'NONE', *, *, #10864, .F. ) ;
#35759 = VERTEX_POINT ( 'NONE', #140320 ) ;
#35760 = CARTESIAN_POINT ( 'NONE',  ( 23.14999999999999503, 6.650000000011155876, -155.1500000000000057 ) ) ;
#35761 = DIRECTION ( 'NONE',  ( 1.000000000000000000, 0.000000000000000000, 0.000000000000000000 ) ) ;
#35762 = ORIENTED_EDGE ( 'NONE', *, *, #212001, .F. ) ;
#35763 = AXIS2_PLACEMENT_3D ( 'NONE', #251573, #211170, #247725 ) ;
#35764 = ORIENTED_EDGE ( 'NONE', *, *, #223158, .T. ) ;
#35765 = VECTOR ( 'NONE', #43891, 1000.000000000000000 ) ;
#35766 = AXIS2_PLACEMENT_3D ( 'NONE', #89910, #131612, #130321 ) ;
#35767 = EDGE_CURVE ( 'NONE', #4740, #14640, #4104, .T. ) ;
#35768 = CARTESIAN_POINT ( 'NONE',  ( -18.59999999999999787, 9.250000000011157297, -121.7500000000000426 ) ) ;
#35769 =( BOUNDED_CURVE ( )  B_SPLINE_CURVE ( 3, ( #178703, #187334, #181255, #238641 ),
 .UNSPECIFIED., .F., .T. ) 
 B_SPLINE_CURVE_WITH_KNOTS ( ( 4, 4 ),
 ( 0.000000000000000000, 1.570796326794916320 ),
 .UNSPECIFIED. ) 
 CURVE ( )  GEOMETRIC_REPRESENTATION_ITEM ( )  RATIONAL_B_SPLINE_CURVE ( ( 1.000000000000000000, 0.8047378541243603856, 0.8047378541243603856, 1.000000000000000000 ) ) 
 REPRESENTATION_ITEM ( '' )  );
#35770 = CARTESIAN_POINT ( 'NONE',  ( -20.94999999999999929, 69.15387683765983695, -166.2853812176745691 ) ) ;
#35771 = EDGE_CURVE ( 'NONE', #63208, #180293, #45798, .T. ) ;
#35772 = DIRECTION ( 'NONE',  ( 0.000000000000000000, -0.8814952561688430555, 0.4721928772777346239 ) ) ;
#35773 = DIRECTION ( 'NONE',  ( 1.000000000000000000, 0.000000000000000000, 0.000000000000000000 ) ) ;
#35774 = DIRECTION ( 'NONE',  ( -0.000000000000000000, -0.000000000000000000, -1.000000000000000000 ) ) ;
#35775 = CARTESIAN_POINT ( 'NONE',  ( -22.48660254037843487, 11.65000000001115588, -66.95000000000005969 ) ) ;
#35776 = DIRECTION ( 'NONE',  ( 0.000000000000000000, 0.000000000000000000, 1.000000000000000000 ) ) ;
#35777 = ADVANCED_FACE ( 'NONE', ( #235576 ), #219869, .F. ) ;
#35779 = FACE_OUTER_BOUND ( 'NONE', #210970, .T. ) ;
#35778 = DIRECTION ( 'NONE',  ( 0.000000000000000000, 0.8741572761215393728, -0.4856429311786291669 ) ) ;
#35781 = EDGE_CURVE ( 'NONE', #110195, #151077, #119505, .T. ) ;
#35780 = DIRECTION ( 'NONE',  ( 0.000000000000000000, 0.03181660087582099256, -0.9994937237965573207 ) ) ;
#35782 = CARTESIAN_POINT ( 'NONE',  ( 23.14999999999999147, 71.85000000001268461, -203.5231074845243597 ) ) ;
#35783 = CARTESIAN_POINT ( 'NONE',  ( -21.07928932188134041, 1.115600667400684642E-11, -100.5000000000000284 ) ) ;
#35784 = DIRECTION ( 'NONE',  ( 0.000000000000000000, 6.982962677686266711E-15, -1.000000000000000000 ) ) ;
#35785 = AXIS2_PLACEMENT_3D ( 'NONE', #82813, #48858, #43728 ) ;
#35786 = ORIENTED_EDGE ( 'NONE', *, *, #62120, .F. ) ;
#35787 = AXIS2_PLACEMENT_3D ( 'NONE', #158839, #212388, #33781 ) ;
#35789 = ORIENTED_EDGE ( 'NONE', *, *, #3260, .T. ) ;
#35788 = DIRECTION ( 'NONE',  ( 1.000000000000000000, 0.000000000000000000, 0.000000000000000000 ) ) ;
#35790 = VECTOR ( 'NONE', #60289, 1000.000000000000000 ) ;
#35791 = EDGE_CURVE ( 'NONE', #116639, #190614, #41546, .T. ) ;
#35792 = DIRECTION ( 'NONE',  ( -4.408576920032447972E-17, -0.1350103645451946055, 0.9908441862701591329 ) ) ;
#35793 = EDGE_CURVE ( 'NONE', #137271, #196016, #112451, .T. ) ;
#35794 = FACE_OUTER_BOUND ( 'NONE', #62312, .T. ) ;
#35795 = ORIENTED_EDGE ( 'NONE', *, *, #242813, .T. ) ;
#35796 = PLANE ( 'NONE',  #108214 ) ;
#35797 = CARTESIAN_POINT ( 'NONE',  ( -16.91049119928363353, 9.950000000011138823, -54.38172039319083240 ) ) ;
#35798 = ORIENTED_EDGE ( 'NONE', *, *, #220336, .F. ) ;
#35800 = FACE_OUTER_BOUND ( 'NONE', #202502, .T. ) ;
#35799 = CIRCLE ( 'NONE', #181559, 0.09999999999998898659 ) ;
#35801 = CARTESIAN_POINT ( 'NONE',  ( -20.64999999999999858, 74.00000000001186606, -89.79848556176222019 ) ) ;
#35802 = CIRCLE ( 'NONE', #169101, 0.8750000000000007772 ) ;
#35803 = EDGE_CURVE ( 'NONE', #123690, #159228, #23850, .T. ) ;
#35804 = EDGE_CURVE ( 'NONE', #152778, #151773, #10153, .T. ) ;
#35805 = CARTESIAN_POINT ( 'NONE',  ( -20.54999999999999716, 70.62751970751253339, -223.3325012285725393 ) ) ;
#35807 = ORIENTED_EDGE ( 'NONE', *, *, #251507, .F. ) ;
#35806 = DIRECTION ( 'NONE',  ( -3.035766082959431348E-14, 0.9126074666063771490, 0.4088369013363281623 ) ) ;
#35808 = CARTESIAN_POINT ( 'NONE',  ( -20.64999999999999858, 7.250000000011155521, -188.7499999999999716 ) ) ;
#35809 = EDGE_CURVE ( 'NONE', #27566, #19033, #200315, .T. ) ;
#35810 = AXIS2_PLACEMENT_3D ( 'NONE', #222879, #238603, #44266 ) ;
#35811 = AXIS2_PLACEMENT_3D ( 'NONE', #67935, #30118, #48369 ) ;
#35812 = ORIENTED_EDGE ( 'NONE', *, *, #54698, .F. ) ;
#35813 = LINE ( 'NONE', #253538, #249984 ) ;
#35814 = CARTESIAN_POINT ( 'NONE',  ( 21.11701782572533048, 10.72160911600745692, -12.24503742951121055 ) ) ;
#35815 = LINE ( 'NONE', #176608, #61065 ) ;
#35816 = DIRECTION ( 'NONE',  ( -1.000000000000000000, 2.952720810173289112E-16, 2.061873921506763405E-30 ) ) ;
#35818 = CARTESIAN_POINT ( 'NONE',  ( -21.65000000000000213, 63.54522198573874192, -221.7484608313106378 ) ) ;
#35817 = CARTESIAN_POINT ( 'NONE',  ( 18.50000000000000000, 9.122720154857379526, -245.4644708025848558 ) ) ;
#35819 = DIRECTION ( 'NONE',  ( -1.000000000000000000, -0.000000000000000000, -0.000000000000000000 ) ) ;
#35820 = CARTESIAN_POINT ( 'NONE',  ( -21.14999999893415250, 64.25000000001233502, -163.1786121409978136 ) ) ;
#35821 = CARTESIAN_POINT ( 'NONE',  ( 21.05000000000000071, 76.00000000001216449, -140.5231074845243597 ) ) ;
#35822 = CARTESIAN_POINT ( 'NONE',  ( -23.25000000000000000, -0.9152171842607033092, -242.2974985173726452 ) ) ;
#35823 = ORIENTED_EDGE ( 'NONE', *, *, #114958, .F. ) ;
#35824 = DIRECTION ( 'NONE',  ( 0.000000000000000000, 1.000000000000000000, 0.000000000000000000 ) ) ;
#35825 = EDGE_LOOP ( 'NONE', ( #179931, #37151, #236753 ) ) ;
#35826 = ORIENTED_EDGE ( 'NONE', *, *, #135039, .T. ) ;
#35827 = CARTESIAN_POINT ( 'NONE',  ( -23.15000000000000213, 11.65000000000000036, -26.48519422934604961 ) ) ;
#35828 = DIRECTION ( 'NONE',  ( 0.000000000000000000, 0.3042567129660269654, 0.9525900758537791946 ) ) ;
#35829 = ORIENTED_EDGE ( 'NONE', *, *, #253576, .T. ) ;
#35830 = TOROIDAL_SURFACE ( 'NONE', #152565, 0.2000000000000000111, 0.1000000000000000056 ) ;
#35831 = VECTOR ( 'NONE', #220756, 1000.000000000000000 ) ;
#35833 = EDGE_CURVE ( 'NONE', #61020, #134077, #83172, .T. ) ;
#35832 = ORIENTED_EDGE ( 'NONE', *, *, #111558, .F. ) ;
#35834 = DIRECTION ( 'NONE',  ( 0.000000000000000000, 0.4721928772777551075, 0.8814952561688320642 ) ) ;
#35835 = SURFACE_STYLE_USAGE ( .BOTH. , #136162 ) ;
#35836 = VECTOR ( 'NONE', #222744, 1000.000000000000000 ) ;
#35837 = CIRCLE ( 'NONE', #44213, 2.100000000000002309 ) ;
#35838 = EDGE_LOOP ( 'NONE', ( #48241, #232953, #44014, #122025 ) ) ;
#35839 = VERTEX_POINT ( 'NONE', #96062 ) ;
#35840 = TOROIDAL_SURFACE ( 'NONE', #44219, 2.100000000000002309, 0.1000000000000000056 ) ;
#35841 = DIRECTION ( 'NONE',  ( 0.000000000000000000, 0.000000000000000000, -1.000000000000000000 ) ) ;
#35842 = CARTESIAN_POINT ( 'NONE',  ( 20.94999999999999929, 0.000000000000000000, -35.50000000000000711 ) ) ;
#35843 = CARTESIAN_POINT ( 'NONE',  ( -21.14999999999999858, -0.09999999998884338825, -21.85042919245520210 ) ) ;
#35844 = DIRECTION ( 'NONE',  ( 0.000000000000000000, -1.000000000000000000, 0.000000000000000000 ) ) ;
#35845 = FACE_OUTER_BOUND ( 'NONE', #100910, .T. ) ;
#35846 = EDGE_CURVE ( 'NONE', #143626, #57915, #39988, .T. ) ;
#35848 = CARTESIAN_POINT ( 'NONE',  ( -18.39999999999999858, 85.60000000001167564, -62.92291809330219365 ) ) ;
#35847 = CARTESIAN_POINT ( 'NONE',  ( -18.58735405345342784, 77.36886435760402492, -241.7961888098465408 ) ) ;
#35849 = DIRECTION ( 'NONE',  ( 1.000000000000000000, 0.000000000000000000, 0.000000000000000000 ) ) ;
#35851 = ORIENTED_EDGE ( 'NONE', *, *, #117340, .F. ) ;
#35850 = CARTESIAN_POINT ( 'NONE',  ( -20.94999999999999929, -1.835341550213257733, -145.5551512925629822 ) ) ;
#35853 = CARTESIAN_POINT ( 'NONE',  ( 23.24999999999997513, 56.06656052939784729, -228.0911609752645290 ) ) ;
#35852 = CARTESIAN_POINT ( 'NONE',  ( -18.59999999999999787, 64.25000000001173817, -81.27310748452440237 ) ) ;
#35854 = DIRECTION ( 'NONE',  ( 1.000000000000000000, 0.000000000000000000, -0.000000000000000000 ) ) ;
#35855 = AXIS2_PLACEMENT_3D ( 'NONE', #56280, #155442, #39330 ) ;
#35856 = ORIENTED_EDGE ( 'NONE', *, *, #62930, .F. ) ;
#35857 = DIRECTION ( 'NONE',  ( 0.000000000000000000, -0.9998779222360104635, -0.01562499999996343723 ) ) ;
#35859 = EDGE_CURVE ( 'NONE', #37415, #208398, #255095, .T. ) ;
#35858 = CARTESIAN_POINT ( 'NONE',  ( -20.85000000000000142, 77.83585931145546510, -91.51866831572576189 ) ) ;
#35860 = ORIENTED_EDGE ( 'NONE', *, *, #97773, .T. ) ;
#35861 = VECTOR ( 'NONE', #70858, 1000.000000000000000 ) ;
#35862 = DIRECTION ( 'NONE',  ( 1.000000000000000000, -2.952720810173289112E-16, -2.061873921506763405E-30 ) ) ;
#35863 = EDGE_CURVE ( 'NONE', #155813, #130245, #183178, .T. ) ;
#35864 = CARTESIAN_POINT ( 'NONE',  ( -18.59999999999999787, 74.16465844978787914, -158.4679561919613775 ) ) ;
#35865 = CARTESIAN_POINT ( 'NONE',  ( 15.70340296795548518, 66.64411154550927563, -86.73446458774637335 ) ) ;
#35866 = ORIENTED_EDGE ( 'NONE', *, *, #170997, .F. ) ;
#35867 = ORIENTED_EDGE ( 'NONE', *, *, #21925, .F. ) ;
#35868 = EDGE_CURVE ( 'NONE', #144086, #250305, #166455, .T. ) ;
#35870 = EDGE_CURVE ( 'NONE', #200814, #36945, #197740, .T. ) ;
#35869 = DIRECTION ( 'NONE',  ( 0.000000000000000000, 1.000000000000000000, 0.000000000000000000 ) ) ;
#35871 = CARTESIAN_POINT ( 'NONE',  ( -18.44204374631835464, -0.7347539659637959408, -242.2268351530478867 ) ) ;
#35872 = AXIS2_PLACEMENT_3D ( 'NONE', #67475, #226525, #167897 ) ;
#35873 = CARTESIAN_POINT ( 'NONE',  ( -21.07928932188134041, 6.328516656404449492, -100.4011048543456468 ) ) ;
#35874 = DIRECTION ( 'NONE',  ( 0.000000000000000000, -1.000000000000000000, 0.000000000000000000 ) ) ;
#35875 = VERTEX_POINT ( 'NONE', #239449 ) ;
#35876 = CARTESIAN_POINT ( 'NONE',  ( 21.05000000000000071, 45.77234354862702048, -239.5513518621457365 ) ) ;
#35877 = DIRECTION ( 'NONE',  ( 0.000000000000000000, 0.000000000000000000, -1.000000000000000000 ) ) ;
#35878 = DIRECTION ( 'NONE',  ( 1.000000000000000000, 0.000000000000000000, 0.000000000000000000 ) ) ;
#35879 = DIRECTION ( 'NONE',  ( -1.000000000000000000, -0.000000000000000000, -0.000000000000000000 ) ) ;
#35880 = AXIS2_PLACEMENT_3D ( 'NONE', #244593, #215099, #116017 ) ;
#35881 = VECTOR ( 'NONE', #184922, 1000.000000000000000 ) ;
#35882 = EDGE_CURVE ( 'NONE', #74336, #222562, #137356, .T. ) ;
#35883 = AXIS2_PLACEMENT_3D ( 'NONE', #93987, #236075, #57424 ) ;
#35884 = AXIS2_PLACEMENT_3D ( 'NONE', #114689, #149996, #31343 ) ;
#35886 = EDGE_CURVE ( 'NONE', #238714, #42318, #18333, .T. ) ;
#35885 = DIRECTION ( 'NONE',  ( -0.000000000000000000, 0.000000000000000000, 1.000000000000000000 ) ) ;
#35888 = ORIENTED_EDGE ( 'NONE', *, *, #76724, .F. ) ;
#35887 = CARTESIAN_POINT ( 'NONE',  ( -17.27223548802716380, 65.65460260865593511, -192.1567136637387705 ) ) ;
#35889 = DIRECTION ( 'NONE',  ( 0.000000000000000000, 0.000000000000000000, -1.000000000000000000 ) ) ;
#35890 = SPHERICAL_SURFACE ( 'NONE', #107827, 0.1000000000000000056 ) ;
#35891 = CARTESIAN_POINT ( 'NONE',  ( 18.39999999999999858, 77.26488334054519669, -241.9697969554615611 ) ) ;
#35892 = CARTESIAN_POINT ( 'NONE',  ( 20.94999999999999929, -8.663551401857999323, -57.47589888193269303 ) ) ;
#35893 = EDGE_CURVE ( 'NONE', #2024, #223475, #185876, .T. ) ;
#35894 = FACE_OUTER_BOUND ( 'NONE', #118634, .T. ) ;
#35896 = EDGE_LOOP ( 'NONE', ( #157198, #161187, #192107, #181373 ) ) ;
#35895 = FACE_OUTER_BOUND ( 'NONE', #117160, .T. ) ;
#35897 = CARTESIAN_POINT ( 'NONE',  ( 21.04999999999999716, 8.871279685995643760, -12.15000000000000036 ) ) ;
#35898 = DIRECTION ( 'NONE',  ( 0.000000000000000000, 0.2128009952263693050, -0.9770955615653296178 ) ) ;
#35899 = DIRECTION ( 'NONE',  ( 0.000000000000000000, 0.000000000000000000, 1.000000000000000000 ) ) ;
#35900 = VERTEX_POINT ( 'NONE', #46355 ) ;
#35901 = CARTESIAN_POINT ( 'NONE',  ( 20.94999999999999929, 69.34766280046808617, -247.6726305063181144 ) ) ;
#35902 = CARTESIAN_POINT ( 'NONE',  ( 22.47071067811865319, 59.75442326890421896, -233.9300113800879046 ) ) ;
#35903 = CARTESIAN_POINT ( 'NONE',  ( -20.65000000000000568, 68.75000000001261924, -190.8731074845244109 ) ) ;
#35904 = EDGE_CURVE ( 'NONE', #208784, #62371, #24980, .T. ) ;
#35905 = DIRECTION ( 'NONE',  ( 0.000000000000000000, 1.000000000000000000, 0.000000000000000000 ) ) ;
#35906 = VECTOR ( 'NONE', #99300, 1000.000000000000114 ) ;
#35907 = ADVANCED_FACE ( 'NONE', ( #146727 ), #165035, .F. ) ;
#35908 = AXIS2_PLACEMENT_3D ( 'NONE', #91317, #32667, #48326 ) ;
#35909 = CARTESIAN_POINT ( 'NONE',  ( -18.46093223321787846, 78.23581486479142200, -231.4991767757356058 ) ) ;
#35910 = CARTESIAN_POINT ( 'NONE',  ( 18.59999999999999787, 11.75000000000000000, 31.39999999999999858 ) ) ;
#35911 = ORIENTED_EDGE ( 'NONE', *, *, #141580, .T. ) ;
#35912 = ORIENTED_EDGE ( 'NONE', *, *, #108523, .F. ) ;
#35913 = EDGE_CURVE ( 'NONE', #85340, #3248, #116536, .T. ) ;
#35915 = DIRECTION ( 'NONE',  ( 1.000000000000000000, 0.000000000000000000, 0.000000000000000000 ) ) ;
#35914 = CIRCLE ( 'NONE', #190013, 0.2000000000000057288 ) ;
#35916 = CARTESIAN_POINT ( 'NONE',  ( -18.50000000000000000, 67.23127455305835554, -235.8551265064784559 ) ) ;
#35917 = FACE_OUTER_BOUND ( 'NONE', #100679, .T. ) ;
#35918 = CARTESIAN_POINT ( 'NONE',  ( -22.01447462590972748, 7.263800201241075172, -133.9009629999404751 ) ) ;
#35919 = EDGE_CURVE ( 'NONE', #122787, #28569, #27609, .T. ) ;
#35920 = DIRECTION ( 'NONE',  ( 0.7071067811865474617, -0.6824534298470372740, 0.1850873201762209819 ) ) ;
#35921 = FACE_OUTER_BOUND ( 'NONE', #149682, .T. ) ;
#35922 = CARTESIAN_POINT ( 'NONE',  ( -16.94062896051973865, 9.992719105111833144, -113.1025165421188348 ) ) ;
#35923 = DIRECTION ( 'NONE',  ( 0.000000000000000000, -0.9910465087640866200, 0.1335171055202861445 ) ) ;
#35924 = AXIS2_PLACEMENT_3D ( 'NONE', #34180, #113677, #109817 ) ;
#35925 = ORIENTED_EDGE ( 'NONE', *, *, #8072, .T. ) ;
#35926 = DIRECTION ( 'NONE',  ( -1.000000000000000000, 0.000000000000000000, -0.000000000000000000 ) ) ;
#35927 = VERTEX_POINT ( 'NONE', #182039 ) ;
#35928 = ORIENTED_EDGE ( 'NONE', *, *, #88736, .F. ) ;
#35929 = DIRECTION ( 'NONE',  ( 2.952720810173289112E-16, 1.000000000000000000, 6.938893903907229955E-15 ) ) ;
#35930 = DIRECTION ( 'NONE',  ( 1.000000000000000000, 0.000000000000000000, 0.000000000000000000 ) ) ;
#35931 = FACE_OUTER_BOUND ( 'NONE', #87602, .T. ) ;
#35933 = VERTEX_POINT ( 'NONE', #183321 ) ;
#35932 = SPHERICAL_SURFACE ( 'NONE', #16187, 0.1000000000000000056 ) ;
#35934 = DIRECTION ( 'NONE',  ( -1.000000000000000000, -0.000000000000000000, 0.000000000000000000 ) ) ;
#35935 = DIRECTION ( 'NONE',  ( 0.000000000000000000, -1.000000000000000000, -0.000000000000000000 ) ) ;
#35936 = EDGE_LOOP ( 'NONE', ( #33662, #73742, #57156, #112401 ) ) ;
#35937 = CARTESIAN_POINT ( 'NONE',  ( -21.37071067811865532, 67.92928932189357738, -148.7731074845244166 ) ) ;
#35938 = FACE_OUTER_BOUND ( 'NONE', #177327, .T. ) ;
#35939 = LINE ( 'NONE', #175457, #206576 ) ;
#35940 = FACE_OUTER_BOUND ( 'NONE', #171123, .T. ) ;
#35941 = CIRCLE ( 'NONE', #139951, 0.09999999999998898659 ) ;
#35942 = VECTOR ( 'NONE', #165123, 1000.000000000000227 ) ;
#35943 = AXIS2_PLACEMENT_3D ( 'NONE', #169184, #149614, #229129 ) ;
#35944 = B_SPLINE_CURVE_WITH_KNOTS ( 'NONE', 3,
 ( #125488, #246708, #68080, #224575, #128061, #182909, #26402, #245450, #244133, #207610 ),
 .UNSPECIFIED., .F., .F.,
 ( 4, 3, 3, 4 ),
 ( 0.000000000000000000, 1.004626015991446001E-05, 1.831183478183186726E-05, 2.062343583996000413E-05 ),
 .UNSPECIFIED. ) ;
#35945 = VERTEX_POINT ( 'NONE', #65939 ) ;
#35946 = DIRECTION ( 'NONE',  ( 1.000000000000000000, -2.952720810173289112E-16, -2.061873921506763405E-30 ) ) ;
#35947 = DIRECTION ( 'NONE',  ( 0.000000000000000000, 0.000000000000000000, 1.000000000000000000 ) ) ;
#35948 = ADVANCED_FACE ( 'NONE', ( #145460 ), #84156, .T. ) ;
#35949 = EDGE_LOOP ( 'NONE', ( #62616, #197133, #159284, #147548 ) ) ;
#35950 = DIRECTION ( 'NONE',  ( -1.000000000000000000, -2.952720810173289112E-16, 0.000000000000000000 ) ) ;
#35951 = ORIENTED_EDGE ( 'NONE', *, *, #141188, .F. ) ;
#35952 = CARTESIAN_POINT ( 'NONE',  ( 18.50000000000000355, -9.480686695267808162, -174.4411151687578752 ) ) ;
#35953 = CARTESIAN_POINT ( 'NONE',  ( 18.49999999999998934, 11.65000000001115943, -158.7500000000000284 ) ) ;
#35954 = EDGE_CURVE ( 'NONE', #143795, #242995, #5936, .T. ) ;
#35955 = ORIENTED_EDGE ( 'NONE', *, *, #183774, .T. ) ;
#35956 = AXIS2_PLACEMENT_3D ( 'NONE', #26583, #220894, #44844 ) ;
#35957 = CIRCLE ( 'NONE', #56574, 0.09999999999999939493 ) ;
#35958 = ORIENTED_EDGE ( 'NONE', *, *, #38179, .T. ) ;
#35959 = CIRCLE ( 'NONE', #131626, 0.5000000000000004441 ) ;
#35960 = FACE_OUTER_BOUND ( 'NONE', #206442, .T. ) ;
#35961 = DIRECTION ( 'NONE',  ( -1.000000000000000000, -0.000000000000000000, -0.000000000000000000 ) ) ;
#35963 = VERTEX_POINT ( 'NONE', #122065 ) ;
#35962 = DIRECTION ( 'NONE',  ( -1.000000000000000000, 0.000000000000000000, -0.000000000000000000 ) ) ;
#35964 = FACE_OUTER_BOUND ( 'NONE', #206554, .T. ) ;
#35966 = CIRCLE ( 'NONE', #206641, 0.09999999999999982514 ) ;
#35965 = FACE_OUTER_BOUND ( 'NONE', #95354, .T. ) ;
#35967 = DIRECTION ( 'NONE',  ( 1.000000000000000000, 0.000000000000000000, 0.000000000000000000 ) ) ;
#35968 = AXIS2_PLACEMENT_3D ( 'NONE', #134204, #239417, #114656 ) ;
#35969 = CARTESIAN_POINT ( 'NONE',  ( -18.41418431465368499, 85.50000000001189449, -62.92291809330281893 ) ) ;
#35970 = DIRECTION ( 'NONE',  ( 0.000000000000000000, 0.000000000000000000, -1.000000000000000000 ) ) ;
#35971 = CARTESIAN_POINT ( 'NONE',  ( -1.739115166359751801E-14, 64.35000000001205933, -124.2731074845243739 ) ) ;
#35972 = DIRECTION ( 'NONE',  ( 1.000000000000000000, 0.000000000000000000, 0.000000000000000000 ) ) ;
#35974 = EDGE_LOOP ( 'NONE', ( #150330, #42668, #244903, #20581 ) ) ;
#35973 = DIRECTION ( 'NONE',  ( 0.000000000000000000, 1.000000000000000000, 0.000000000000000000 ) ) ;
#35976 = VERTEX_POINT ( 'NONE', #25539 ) ;
#35975 = DIRECTION ( 'NONE',  ( 0.000000000000000000, -1.000000000000000000, -6.982962677686265922E-15 ) ) ;
#35978 = CARTESIAN_POINT ( 'NONE',  ( -20.64999999999999858, -8.730841121484170131, -191.4019252810156217 ) ) ;
#35977 = CARTESIAN_POINT ( 'NONE',  ( -20.94999999999999929, 62.98048128140160173, -207.0210305352945852 ) ) ;
#35980 = EDGE_LOOP ( 'NONE', ( #6630, #27379, #122585, #218785 ) ) ;
#35979 = FACE_OUTER_BOUND ( 'NONE', #17080, .T. ) ;
#35981 = ORIENTED_EDGE ( 'NONE', *, *, #83186, .T. ) ;
#35982 = CARTESIAN_POINT ( 'NONE',  ( -18.50000000000000000, 10.29270135741298375, -105.9573618871519898 ) ) ;
#35983 = DIRECTION ( 'NONE',  ( -0.000000000000000000, -0.1350103645451718737, 0.9908441862701622416 ) ) ;
#35984 = TOROIDAL_SURFACE ( 'NONE', #69308, 0.2000000000000000111, 0.1000000000000000056 ) ;
#35985 = AXIS2_PLACEMENT_3D ( 'NONE', #193607, #13676, #94490 ) ;
#35986 = AXIS2_PLACEMENT_3D ( 'NONE', #146841, #47744, #106425 ) ;
#35987 = DIRECTION ( 'NONE',  ( -1.000000000000000000, 2.952720810173289112E-16, 2.061873921506763405E-30 ) ) ;
#35988 = DIRECTION ( 'NONE',  ( -1.000000000000000000, -0.000000000000000000, -0.000000000000000000 ) ) ;
#35989 = FACE_OUTER_BOUND ( 'NONE', #206035, .T. ) ;
#35990 = AXIS2_PLACEMENT_3D ( 'NONE', #129979, #72618, #252499 ) ;
#35991 = FACE_OUTER_BOUND ( 'NONE', #118152, .T. ) ;
#35992 = DIRECTION ( 'NONE',  ( 0.000000000000000000, -0.1350103645451945777, 0.9908441862701591329 ) ) ;
#35993 = ORIENTED_EDGE ( 'NONE', *, *, #244867, .T. ) ;
#35994 = ORIENTED_EDGE ( 'NONE', *, *, #189081, .F. ) ;
#35995 = CARTESIAN_POINT ( 'NONE',  ( 21.09107601085606021, 30.83513164543635909, -252.1170788411612023 ) ) ;
#35996 = EDGE_CURVE ( 'NONE', #45065, #83518, #81694, .T. ) ;
#35997 = VECTOR ( 'NONE', #226211, 1000.000000000000114 ) ;
#35998 = EDGE_LOOP ( 'NONE', ( #186244, #34240, #204342, #32871 ) ) ;
#35999 = DIRECTION ( 'NONE',  ( 0.000000000000000000, 0.000000000000000000, 1.000000000000000000 ) ) ;
#36000 = CARTESIAN_POINT ( 'NONE',  ( 18.51024323315077069, 68.05374558910872906, -224.1882283518531835 ) ) ;
#36001 = CARTESIAN_POINT ( 'NONE',  ( -23.25000000000000000, 68.97833521811159585, -65.68954208262705663 ) ) ;
#36002 = CARTESIAN_POINT ( 'NONE',  ( -16.92925196614875816, 9.972331796421277872, -79.61674484771684490 ) ) ;
#36003 = ADVANCED_FACE ( 'NONE', ( #223707 ), #245860, .T. ) ;
#36004 = ORIENTED_EDGE ( 'NONE', *, *, #123280, .F. ) ;
#36005 = DIRECTION ( 'NONE',  ( -0.000000000000000000, 0.8660254037844377084, 0.5000000000000016653 ) ) ;
#36006 = ORIENTED_EDGE ( 'NONE', *, *, #248484, .F. ) ;
#36007 = CARTESIAN_POINT ( 'NONE',  ( 20.85000000000000142, 45.93315328338058379, -256.6017782078560003 ) ) ;
#36008 = EDGE_LOOP ( 'NONE', ( #88239, #140014, #60653, #116586 ) ) ;
#36009 = ADVANCED_FACE ( 'NONE', ( #67217 ), #161734, .T. ) ;
#36010 = VECTOR ( 'NONE', #169131, 1000.000000000000000 ) ;
#36011 = CARTESIAN_POINT ( 'NONE',  ( 18.59999999999999432, 85.48068669529034480, -29.08199231576640287 ) ) ;
#36012 = AXIS2_PLACEMENT_3D ( 'NONE', #141838, #201817, #73896 ) ;
#36013 = CARTESIAN_POINT ( 'NONE',  ( -20.00857864376270001, 66.85000000001186038, -90.77310748452437394 ) ) ;
#36014 = LINE ( 'NONE', #236747, #72205 ) ;
#36015 = CONICAL_SURFACE ( 'NONE', #86034, 4.299999999999970512, 0.7853981633974466137 ) ;
#36016 = VERTEX_POINT ( 'NONE', #48931 ) ;
#36017 = EDGE_CURVE ( 'NONE', #6205, #19640, #170759, .T. ) ;
#36019 = VERTEX_POINT ( 'NONE', #153210 ) ;
#36018 = CARTESIAN_POINT ( 'NONE',  ( -18.50000000000000000, 3.912899247233453615, -11.48182297301096888 ) ) ;
#36020 = DIRECTION ( 'NONE',  ( 0.000000000000000000, -0.4999999999999088507, 0.8660254037844913322 ) ) ;
#36021 = EDGE_LOOP ( 'NONE', ( #114652, #216989, #69435 ) ) ;
#36022 = VECTOR ( 'NONE', #10726, 1000.000000000000114 ) ;
#36023 = ORIENTED_EDGE ( 'NONE', *, *, #212981, .F. ) ;
#36024 = PLANE ( 'NONE',  #232349 ) ;
#36025 = ORIENTED_EDGE ( 'NONE', *, *, #212615, .T. ) ;
#36026 = CARTESIAN_POINT ( 'NONE',  ( -22.50000000000000000, 36.65892442174472876, -249.5511627012454596 ) ) ;
#36027 = ADVANCED_FACE ( 'NONE', ( #69808 ), #188447, .F. ) ;
#36028 = CARTESIAN_POINT ( 'NONE',  ( 22.43288208788031568, 64.17721423152049454, -247.0973294774646831 ) ) ;
#36029 = VECTOR ( 'NONE', #63349, 1000.000000000000000 ) ;
#36030 = CARTESIAN_POINT ( 'NONE',  ( -14.00000000000000178, 66.15000000001155911, -52.77310748452439526 ) ) ;
#36031 = DIRECTION ( 'NONE',  ( -0.000000000000000000, 1.000000000000000000, 6.982962677686266711E-15 ) ) ;
#36032 = AXIS2_PLACEMENT_3D ( 'NONE', #81378, #120568, #243053 ) ;
#36033 = AXIS2_PLACEMENT_3D ( 'NONE', #4121, #125365, #246581 ) ;
#36034 = ORIENTED_EDGE ( 'NONE', *, *, #49517, .T. ) ;
#36035 = CARTESIAN_POINT ( 'NONE',  ( -18.59999999999999787, 14.72981487416292623, -236.4853282537515895 ) ) ;
#36036 = FACE_OUTER_BOUND ( 'NONE', #235665, .T. ) ;
#36037 = LINE ( 'NONE', #75174, #92825 ) ;
#36038 = ORIENTED_EDGE ( 'NONE', *, *, #75773, .F. ) ;
#36039 = CARTESIAN_POINT ( 'NONE',  ( 20.86777300164945004, 68.11153784908182729, -224.1393723182492579 ) ) ;
#36040 = ORIENTED_EDGE ( 'NONE', *, *, #22221, .F. ) ;
#36041 = CARTESIAN_POINT ( 'NONE',  ( 18.39999999999999858, -9.519327731081283162, -73.97297637655937308 ) ) ;
#36042 = EDGE_LOOP ( 'NONE', ( #232531, #156046, #204730, #116255 ) ) ;
#36043 = CARTESIAN_POINT ( 'NONE',  ( -21.14999999999994174, 84.00000000001119815, -34.86056257560453986 ) ) ;
#36044 = PLANE ( 'NONE',  #31318 ) ;
#36045 = AXIS2_PLACEMENT_3D ( 'NONE', #171750, #13937, #132599 ) ;
#36047 = ORIENTED_EDGE ( 'NONE', *, *, #209446, .F. ) ;
#36046 = CARTESIAN_POINT ( 'NONE',  ( -23.25000000000000000, -1.164121893230052995, -108.4148480855716485 ) ) ;
#36048 = CARTESIAN_POINT ( 'NONE',  ( -16.87036670365548474, 9.989418819312801290, -121.4795601173020856 ) ) ;
#36049 = VERTEX_POINT ( 'NONE', #148047 ) ;
#36050 = EDGE_CURVE ( 'NONE', #97383, #247446, #233081, .T. ) ;
#36051 = DIRECTION ( 'NONE',  ( 0.000000000000000000, -0.000000000000000000, 1.000000000000000000 ) ) ;
#36052 = CARTESIAN_POINT ( 'NONE',  ( -16.87998658237741978, 9.950000000011073098, -113.3636395677385309 ) ) ;
#36053 = EDGE_LOOP ( 'NONE', ( #209141, #99369 ) ) ;
#36054 = CARTESIAN_POINT ( 'NONE',  ( -22.39999999999999503, 1.115541036281197940E-11, -126.2092204016266379 ) ) ;
#36055 = CARTESIAN_POINT ( 'NONE',  ( -22.50000000000094147, -3.092988775432980564, -228.1437074281571995 ) ) ;
#36056 = EDGE_LOOP ( 'NONE', ( #144054, #178883, #53229, #77289 ) ) ;
#36057 = DIRECTION ( 'NONE',  ( 0.000000000000000000, 0.2128009952263604232, -0.9770955615653315052 ) ) ;
#36058 = AXIS2_PLACEMENT_3D ( 'NONE', #186921, #8269, #70828 ) ;
#36059 = AXIS2_PLACEMENT_3D ( 'NONE', #148061, #33285, #188459 ) ;
#36060 = VECTOR ( 'NONE', #25405, 1000.000000000000000 ) ;
#36061 = ORIENTED_EDGE ( 'NONE', *, *, #218231, .F. ) ;
#36062 = ADVANCED_FACE ( 'NONE', ( #227571 ), #9810, .T. ) ;
#36063 = CARTESIAN_POINT ( 'NONE',  ( 13.43663047529820709, 9.446645344706402270, -118.9108064561002323 ) ) ;
#36064 = DIRECTION ( 'NONE',  ( 0.000000000000000000, -0.1350103645451904977, 0.9908441862701596881 ) ) ;
#36065 = ADVANCED_FACE ( 'NONE', ( #110186 ), #48700, .F. ) ;
#36067 = ORIENTED_EDGE ( 'NONE', *, *, #167222, .T. ) ;
#36066 = DIRECTION ( 'NONE',  ( 1.000000000000000000, -7.510212038922846022E-17, 1.676432719286211941E-16 ) ) ;
#36068 = DIRECTION ( 'NONE',  ( 0.000000000000000000, -0.2128009952263604232, 0.9770955615653316162 ) ) ;
#36069 = DIRECTION ( 'NONE',  ( 0.000000000000000000, 0.1575546449569757979, 0.9875102702516471709 ) ) ;
#36070 = CARTESIAN_POINT ( 'NONE',  ( -16.93262454970419384, 10.00202046793035748, -20.92707622623731467 ) ) ;
#36071 = AXIS2_PLACEMENT_3D ( 'NONE', #157093, #63096, #103499 ) ;
#36073 = DIRECTION ( 'NONE',  ( 0.000000000000000000, 1.776356839400250859E-15, -1.000000000000000000 ) ) ;
#36072 = CARTESIAN_POINT ( 'NONE',  ( 20.95392731769792150, 8.883061479199918509, -42.02222797957130496 ) ) ;
#36075 = EDGE_CURVE ( 'NONE', #86236, #188417, #187188, .T. ) ;
#36074 = CARTESIAN_POINT ( 'NONE',  ( 20.73486653747088226, 7.250000000011182166, -113.1500000000000483 ) ) ;
#36076 = CARTESIAN_POINT ( 'NONE',  ( 20.94999999999999574, 0.5876173420563349792, -209.1618981382189588 ) ) ;
#36077 = AXIS2_PLACEMENT_3D ( 'NONE', #20780, #199417, #122434 ) ;
#36078 = VECTOR ( 'NONE', #254366, 1000.000000000000000 ) ;
#36079 = DIRECTION ( 'NONE',  ( 0.000000000000000000, 0.9868171638914228216, 0.1618390714546044939 ) ) ;
#36080 = DIRECTION ( 'NONE',  ( 0.000000000000000000, 6.608470384673536035E-15, -1.000000000000000000 ) ) ;
#36081 = EDGE_LOOP ( 'NONE', ( #19278, #159204, #166593, #232669, #159177, #53910, #60021, #79419, #31483, #49830, #220427, #43774, #78830, #44910, #152805, #32816, #79049, #34721, #162293, #231337, #84163, #35405, #37486, #100398, #56643, #39271, #22005, #142092, #213429 ) ) ;
#36082 = ORIENTED_EDGE ( 'NONE', *, *, #142953, .F. ) ;
#36083 = CARTESIAN_POINT ( 'NONE',  ( 18.50000000000000000, 85.40000000001232650, -162.7258477248609836 ) ) ;
#36085 = ORIENTED_EDGE ( 'NONE', *, *, #137657, .T. ) ;
#36084 = CARTESIAN_POINT ( 'NONE',  ( 21.05000000000000071, 28.08470566095357057, -239.2860081655328770 ) ) ;
#36086 = VERTEX_POINT ( 'NONE', #35818 ) ;
#36087 = CARTESIAN_POINT ( 'NONE',  ( 20.94999999999999574, 74.25000000001156764, -57.85359592662268824 ) ) ;
#36088 = EDGE_CURVE ( 'NONE', #159861, #135978, #136144, .T. ) ;
#36089 = ORIENTED_EDGE ( 'NONE', *, *, #209169, .F. ) ;
#36090 = CARTESIAN_POINT ( 'NONE',  ( -20.94999999999999929, 13.71992543034163958, -238.5823796952984992 ) ) ;
#36091 = EDGE_CURVE ( 'NONE', #248144, #209151, #95669, .T. ) ;
#36092 = EDGE_CURVE ( 'NONE', #193487, #190676, #241445, .T. ) ;
#36093 = ORIENTED_EDGE ( 'NONE', *, *, #190682, .F. ) ;
#36094 =( NAMED_UNIT ( * ) PLANE_ANGLE_UNIT ( ) SI_UNIT ( $, .RADIAN. ) );
#36095 = LINE ( 'NONE', #17778, #36600 ) ;
#36097 = ORIENTED_EDGE ( 'NONE', *, *, #191264, .T. ) ;
#36096 = EDGE_LOOP ( 'NONE', ( #121320, #145298, #10187, #210488 ) ) ;
#36098 = ORIENTED_EDGE ( 'NONE', *, *, #56341, .T. ) ;
#36099 = ORIENTED_EDGE ( 'NONE', *, *, #215598, .F. ) ;
#36100 = ORIENTED_EDGE ( 'NONE', *, *, #141381, .T. ) ;
#36101 = EDGE_CURVE ( 'NONE', #59500, #248733, #245536, .T. ) ;
#36102 = CARTESIAN_POINT ( 'NONE',  ( -18.59999999999999787, 76.00000000001126921, -203.5231074845248997 ) ) ;
#36103 = CARTESIAN_POINT ( 'NONE',  ( -18.58671080940900211, -9.406932858826619892, -7.124154464904687956 ) ) ;
#36105 = VERTEX_POINT ( 'NONE', #155776 ) ;
#36104 = CARTESIAN_POINT ( 'NONE',  ( -21.14999999999999858, 64.25000000001269029, -203.4231074845244507 ) ) ;
#36106 = CARTESIAN_POINT ( 'NONE',  ( 20.97438252431638972, 40.74183068305447364, -237.9419367875085527 ) ) ;
#36107 = EDGE_CURVE ( 'NONE', #218506, #82377, #95747, .T. ) ;
#36108 = CARTESIAN_POINT ( 'NONE',  ( 13.54556439290363379, 12.43810346549959611, -213.7002393734605619 ) ) ;
#36110 = ORIENTED_EDGE ( 'NONE', *, *, #102974, .F. ) ;
#36109 = DIRECTION ( 'NONE',  ( 0.000000000000000000, 6.982962677686266711E-15, -1.000000000000000000 ) ) ;
#36111 = CARTESIAN_POINT ( 'NONE',  ( -20.64999999999999858, 74.00000000001259082, -190.2984855617622770 ) ) ;
#36113 = ADVANCED_FACE ( 'NONE', ( #18788 ), #37065, .T. ) ;
#36112 = ORIENTED_EDGE ( 'NONE', *, *, #161700, .F. ) ;
#36115 = TOROIDAL_SURFACE ( 'NONE', #181853, 11.89999999999999858, 0.1000000000000000056 ) ;
#36114 = DIRECTION ( 'NONE',  ( -1.000000000000000000, 0.000000000000000000, -0.000000000000000000 ) ) ;
#36117 = ORIENTED_EDGE ( 'NONE', *, *, #30394, .T. ) ;
#36116 = CARTESIAN_POINT ( 'NONE',  ( 21.56666275994539461, 1.115600667400684642E-11, -60.04263159310671938 ) ) ;
#36118 = DIRECTION ( 'NONE',  ( -1.000000000000000000, 0.000000000000000000, 0.000000000000000000 ) ) ;
#36119 = DIRECTION ( 'NONE',  ( 0.000000000000000000, 0.000000000000000000, -1.000000000000000000 ) ) ;
#36120 = CARTESIAN_POINT ( 'NONE',  ( 20.00000000000000355, 11.75000000001116263, -91.65000000000004832 ) ) ;
#36121 = AXIS2_PLACEMENT_3D ( 'NONE', #209398, #11211, #30793 ) ;
#36122 = ORIENTED_EDGE ( 'NONE', *, *, #48101, .T. ) ;
#36124 = CARTESIAN_POINT ( 'NONE',  ( -20.94999999999999929, 64.25000000001190870, -96.00830171387039513 ) ) ;
#36123 = CARTESIAN_POINT ( 'NONE',  ( -16.97092634996655036, 10.00088896635952018, -121.3698572337023478 ) ) ;
#36125 = DIRECTION ( 'NONE',  ( -1.000000000000000000, -7.304098846218135653E-16, 4.607487905232624742E-31 ) ) ;
#36126 = AXIS2_PLACEMENT_3D ( 'NONE', #255272, #233228, #19287 ) ;
#36127 = VECTOR ( 'NONE', #87995, 1000.000000000000000 ) ;
#36128 = CARTESIAN_POINT ( 'NONE',  ( -23.49999999999994316, 83.90000000001120384, -34.77310748452479316 ) ) ;
#36129 = FACE_OUTER_BOUND ( 'NONE', #163566, .T. ) ;
#36130 = ORIENTED_EDGE ( 'NONE', *, *, #34882, .F. ) ;
#36131 = EDGE_LOOP ( 'NONE', ( #205393, #224989, #169139, #130114 ) ) ;
#36132 = AXIS2_PLACEMENT_3D ( 'NONE', #41974, #255818, #198457 ) ;
#36133 = DIRECTION ( 'NONE',  ( -1.000000000000000000, -0.000000000000000000, -0.000000000000000000 ) ) ;
#36134 = DIRECTION ( 'NONE',  ( 0.000000000000000000, 0.8814952561688430555, -0.4721928772777346239 ) ) ;
#36136 = ORIENTED_EDGE ( 'NONE', *, *, #49027, .T. ) ;
#36135 = EDGE_CURVE ( 'NONE', #240452, #251749, #199374, .T. ) ;
#36137 = LINE ( 'NONE', #79065, #185129 ) ;
#36138 = EDGE_LOOP ( 'NONE', ( #107544, #233552, #222554, #137575 ) ) ;
#36139 = EDGE_CURVE ( 'NONE', #43027, #230716, #87478, .T. ) ;
#36140 = CARTESIAN_POINT ( 'NONE',  ( 23.14999999999999858, 0.000000000000000000, 0.000000000000000000 ) ) ;
#36141 = FACE_OUTER_BOUND ( 'NONE', #150933, .T. ) ;
#36143 = EDGE_CURVE ( 'NONE', #239004, #245309, #66066, .T. ) ;
#36142 = EDGE_LOOP ( 'NONE', ( #134491, #32585, #68253, #21995 ) ) ;
#36144 = CYLINDRICAL_SURFACE ( 'NONE', #177740, 11.75000000000000000 ) ;
#36145 = AXIS2_PLACEMENT_3D ( 'NONE', #188207, #126949, #168695 ) ;
#36146 = ORIENTED_EDGE ( 'NONE', *, *, #129599, .F. ) ;
#36147 = ORIENTED_EDGE ( 'NONE', *, *, #89091, .T. ) ;
#36148 = CIRCLE ( 'NONE', #185973, 0.1000000000000000472 ) ;
#36149 = ORIENTED_EDGE ( 'NONE', *, *, #75013, .T. ) ;
#36150 = DIRECTION ( 'NONE',  ( 0.000000000000000000, 0.2128009952263603399, -0.9770955615653315052 ) ) ;
#36151 = CARTESIAN_POINT ( 'NONE',  ( 11.60000000000006004, 64.25000000001119815, -23.72310748452479601 ) ) ;
#36152 = CARTESIAN_POINT ( 'NONE',  ( -16.94333152886236249, 66.00965798856108790, -56.91513901557880217 ) ) ;
#36153 = AXIS2_PLACEMENT_3D ( 'NONE', #246339, #67698, #147231 ) ;
#36154 = CARTESIAN_POINT ( 'NONE',  ( 21.05000000000000071, 45.93587830916155212, -239.9163948487882863 ) ) ;
#36156 = DIRECTION ( 'NONE',  ( 0.000000000000000000, 1.192622389734062135E-14, -1.000000000000000000 ) ) ;
#36155 = FACE_OUTER_BOUND ( 'NONE', #178887, .T. ) ;
#36158 = VERTEX_POINT ( 'NONE', #116617 ) ;
#36157 = FACE_OUTER_BOUND ( 'NONE', #50649, .T. ) ;
#36159 = CARTESIAN_POINT ( 'NONE',  ( -20.94999999999999929, 1.148907358139439339E-11, -201.0000000000015064 ) ) ;
#36160 = ORIENTED_EDGE ( 'NONE', *, *, #235168, .T. ) ;
#36161 = CIRCLE ( 'NONE', #185981, 0.1000000000000002554 ) ;
#36162 = CARTESIAN_POINT ( 'NONE',  ( -12.24999999999999822, 9.350000000011132073, -150.5185689574026355 ) ) ;
#36163 = AXIS2_PLACEMENT_3D ( 'NONE', #215667, #218229, #158320 ) ;
#36164 = ORIENTED_EDGE ( 'NONE', *, *, #143911, .T. ) ;
#36165 = VERTEX_POINT ( 'NONE', #196150 ) ;
#36166 = CYLINDRICAL_SURFACE ( 'NONE', #146161, 0.09999999999999939493 ) ;
#36167 = DIRECTION ( 'NONE',  ( 0.000000000000000000, 0.8814952561688476074, -0.4721928772777262417 ) ) ;
#36169 = EDGE_CURVE ( 'NONE', #131901, #41100, #28710, .T. ) ;
#36168 = LINE ( 'NONE', #77828, #100302 ) ;
#36170 = DIRECTION ( 'NONE',  ( 1.000000000000000000, 0.000000000000000000, 0.000000000000000000 ) ) ;
#36171 = EDGE_CURVE ( 'NONE', #201031, #31563, #3713, .T. ) ;
#36172 = CIRCLE ( 'NONE', #56968, 0.4000000000000114575 ) ;
#36173 = DIRECTION ( 'NONE',  ( 0.000000000000000000, 0.000000000000000000, -1.000000000000000000 ) ) ;
#36175 = ORIENTED_EDGE ( 'NONE', *, *, #4497, .F. ) ;
#36174 = CIRCLE ( 'NONE', #115260, 0.09999999999999939493 ) ;
#36176 = ORIENTED_EDGE ( 'NONE', *, *, #133454, .T. ) ;
#36177 = CIRCLE ( 'NONE', #256864, 4.150000000000001243 ) ;
#36179 = EDGE_CURVE ( 'NONE', #254106, #136295, #97011, .T. ) ;
#36178 = DIRECTION ( 'NONE',  ( 0.000000000000000000, 0.8814952561688430555, -0.4721928772777346239 ) ) ;
#36180 = ORIENTED_EDGE ( 'NONE', *, *, #65527, .F. ) ;
#36181 = CARTESIAN_POINT ( 'NONE',  ( 23.24999999999999289, 21.13195309841794867, -243.6318585593223816 ) ) ;
#36182 = CARTESIAN_POINT ( 'NONE',  ( -20.54999999999999716, 1.940186915899009490, -180.3291192110532961 ) ) ;
#36183 = VERTEX_POINT ( 'NONE', #114034 ) ;
#36184 = CARTESIAN_POINT ( 'NONE',  ( 20.94999999999999929, 85.00000000001197975, -112.4170766071766678 ) ) ;
#36185 = CARTESIAN_POINT ( 'NONE',  ( -22.49436431346200038, 64.35004905235818740, -69.59001101424667013 ) ) ;
#36186 = DIRECTION ( 'NONE',  ( 0.000000000000000000, 0.2128009952263485993, -0.9770955615653341697 ) ) ;
#36187 = EDGE_LOOP ( 'NONE', ( #238784, #147611, #59854, #21313 ) ) ;
#36188 = EDGE_CURVE ( 'NONE', #92906, #170452, #77459, .T. ) ;
#36189 = CARTESIAN_POINT ( 'NONE',  ( -21.05000000000000071, -11.48912529306490349, -170.5999999999999659 ) ) ;
#36191 = EDGE_CURVE ( 'NONE', #126005, #167562, #57905, .T. ) ;
#36190 = CARTESIAN_POINT ( 'NONE',  ( -16.77683809663752257, 9.950000000011138823, -154.8500000000000227 ) ) ;
#36192 = AXIS2_PLACEMENT_3D ( 'NONE', #158020, #39333, #195840 ) ;
#36193 = LINE ( 'NONE', #14061, #257297 ) ;
#36194 = EDGE_CURVE ( 'NONE', #73251, #79556, #134865, .T. ) ;
#36195 = VERTEX_POINT ( 'NONE', #214420 ) ;
#36197 = ADVANCED_FACE ( 'NONE', ( #179190 ), #187464, .T. ) ;
#36196 = EDGE_CURVE ( 'NONE', #62193, #91550, #177890, .T. ) ;
#36198 = CARTESIAN_POINT ( 'NONE',  ( -20.64999999999999858, 54.34471204062663219, -239.4366250215122420 ) ) ;
#36199 = VERTEX_POINT ( 'NONE', #78754 ) ;
#36200 = CARTESIAN_POINT ( 'NONE',  ( -18.59999999999999787, 43.17747518314618560, -245.0773422074893233 ) ) ;
#36201 = EDGE_CURVE ( 'NONE', #120584, #137554, #107762, .T. ) ;
#36202 = DIRECTION ( 'NONE',  ( 0.000000000000000000, -0.1335171055202867274, -0.9910465087640865089 ) ) ;
#36203 = DIRECTION ( 'NONE',  ( 1.000000000000000000, -7.304098846218133681E-16, 0.000000000000000000 ) ) ;
#36205 = VECTOR ( 'NONE', #4256, 1000.000000000000000 ) ;
#36204 = FACE_OUTER_BOUND ( 'NONE', #221042, .T. ) ;
#36206 = DIRECTION ( 'NONE',  ( -1.000000000000000000, 1.207181226542539700E-16, -2.694675058168174199E-16 ) ) ;
#36208 = VERTEX_POINT ( 'NONE', #104715 ) ;
#36207 = AXIS2_PLACEMENT_3D ( 'NONE', #132248, #171416, #8455 ) ;
#36209 = CARTESIAN_POINT ( 'NONE',  ( 23.15000000000000213, 69.08367151115869831, -247.5088222940653679 ) ) ;
#36210 = DIRECTION ( 'NONE',  ( 0.000000000000000000, 0.000000000000000000, -1.000000000000000000 ) ) ;
#36211 = CIRCLE ( 'NONE', #140206, 0.09999999999999939493 ) ;
#36212 = VECTOR ( 'NONE', #253887, 1000.000000000000114 ) ;
#36213 = CARTESIAN_POINT ( 'NONE',  ( 22.00356870141288823, 10.55423491370503797, -227.3381210828028713 ) ) ;
#36214 = CARTESIAN_POINT ( 'NONE',  ( -18.59999999999999787, 1.115600667400684642E-11, -208.8999999999999488 ) ) ;
#36215 = EDGE_CURVE ( 'NONE', #26533, #199652, #86894, .T. ) ;
#36216 = ADVANCED_FACE ( 'NONE', ( #143870 ), #211830, .T. ) ;
#36217 = CARTESIAN_POINT ( 'NONE',  ( 20.72390388899089686, 65.41003688158754414, -62.01175918877954274 ) ) ;
#36218 = CIRCLE ( 'NONE', #248564, 4.150000000000001243 ) ;
#36219 = ORIENTED_EDGE ( 'NONE', *, *, #83120, .F. ) ;
#36220 = ORIENTED_EDGE ( 'NONE', *, *, #472, .F. ) ;
#36221 = DIRECTION ( 'NONE',  ( 1.000000000000000000, -3.427148797533456523E-14, 5.467925025959484217E-15 ) ) ;
#36222 = CARTESIAN_POINT ( 'NONE',  ( -23.25000000000000000, 1.115600667400684642E-11, -167.5000000000000284 ) ) ;
#36224 = EDGE_CURVE ( 'NONE', #171414, #92448, #133287, .T. ) ;
#36223 = DIRECTION ( 'NONE',  ( 0.7071067811865463515, -0.7071067811865487940, 0.000000000000000000 ) ) ;
#36225 = SPHERICAL_SURFACE ( 'NONE', #222176, 0.1000000000000000056 ) ;
#36226 = FACE_OUTER_BOUND ( 'NONE', #79275, .T. ) ;
#36227 = CIRCLE ( 'NONE', #90355, 0.1000000000000124678 ) ;
#36228 = ORIENTED_EDGE ( 'NONE', *, *, #213195, .T. ) ;
#36230 = ADVANCED_FACE ( 'NONE', ( #205118 ), #125599, .F. ) ;
#36229 = DIRECTION ( 'NONE',  ( 0.000000000000000000, -1.000000000000000000, -6.982962677686265922E-15 ) ) ;
#36231 = AXIS2_PLACEMENT_3D ( 'NONE', #18125, #153841, #233352 ) ;
#36232 = ADVANCED_FACE ( 'NONE', ( #145149 ), #184286, .T. ) ;
#36233 = LINE ( 'NONE', #14094, #96567 ) ;
#36234 = AXIS2_PLACEMENT_3D ( 'NONE', #3821, #247566, #205866 ) ;
#36235 = EDGE_LOOP ( 'NONE', ( #225423, #245232, #206117 ) ) ;
#36236 = CYLINDRICAL_SURFACE ( 'NONE', #225491, 0.09999999999999939493 ) ;
#36237 = CARTESIAN_POINT ( 'NONE',  ( 21.14261333020286671, 13.07706791821966696, -210.6891105688758046 ) ) ;
#36238 = AXIS2_PLACEMENT_3D ( 'NONE', #96766, #154256, #156809 ) ;
#36239 = ORIENTED_EDGE ( 'NONE', *, *, #63547, .T. ) ;
#36240 = CARTESIAN_POINT ( 'NONE',  ( 21.14999999999999858, 65.28660755661168480, -57.17310748452439384 ) ) ;
#36241 = ORIENTED_EDGE ( 'NONE', *, *, #166195, .F. ) ;
#36242 = ADVANCED_FACE ( 'NONE', ( #106013 ), #149486, .T. ) ;
#36243 = DIRECTION ( 'NONE',  ( 0.000000000000000000, 0.000000000000000000, -1.000000000000000000 ) ) ;
#36244 = FACE_OUTER_BOUND ( 'NONE', #185453, .T. ) ;
#36245 = DIRECTION ( 'NONE',  ( 0.000000000000000000, 0.008583690987127625890, 0.9999631594459055250 ) ) ;
#36246 = DIRECTION ( 'NONE',  ( 1.000000000000000000, -0.000000000000000000, -0.000000000000000000 ) ) ;
#36247 = PLANE ( 'NONE',  #57207 ) ;
#36248 = DIRECTION ( 'NONE',  ( 0.000000000000000000, 0.000000000000000000, -1.000000000000000000 ) ) ;
#36249 = CARTESIAN_POINT ( 'NONE',  ( 21.05000000000000071, 74.63912941281984104, -94.95010955743335046 ) ) ;
#36250 = CARTESIAN_POINT ( 'NONE',  ( -21.05000000000000071, 77.83534155023627932, -91.36795619196132634 ) ) ;
#36251 = DIRECTION ( 'NONE',  ( -1.000000000000000000, 0.000000000000000000, 0.000000000000000000 ) ) ;
#36252 = EDGE_CURVE ( 'NONE', #246715, #186847, #166064, .T. ) ;
#36253 = CARTESIAN_POINT ( 'NONE',  ( 18.42555734704284731, -7.781548346777066527, -209.8995918847530788 ) ) ;
#36254 = DIRECTION ( 'NONE',  ( -0.000000000000000000, -0.000000000000000000, -1.000000000000000000 ) ) ;
#36255 = CARTESIAN_POINT ( 'NONE',  ( -18.59999999999999787, 11.65000000001115232, -107.4148057706540271 ) ) ;
#36256 = DIRECTION ( 'NONE',  ( -1.000000000000000000, 1.207181226542539700E-16, -2.694675058168174199E-16 ) ) ;
#36257 = CIRCLE ( 'NONE', #69563, 0.1000000000000013933 ) ;
#36258 = ORIENTED_EDGE ( 'NONE', *, *, #252988, .F. ) ;
#36259 = TOROIDAL_SURFACE ( 'NONE', #23798, 11.70000000000000462, 0.1000000000000000056 ) ;
#36260 = AXIS2_PLACEMENT_3D ( 'NONE', #230004, #9672, #70971 ) ;
#36261 = AXIS2_PLACEMENT_3D ( 'NONE', #172804, #153232, #228887 ) ;
#36262 = CARTESIAN_POINT ( 'NONE',  ( -21.05000000000000071, 6.277629359189121239, -229.8243190661787878 ) ) ;
#36263 = LINE ( 'NONE', #192756, #20224 ) ;
#36264 = ORIENTED_EDGE ( 'NONE', *, *, #232293, .T. ) ;
#36265 = CARTESIAN_POINT ( 'NONE',  ( 22.60000000000000142, 25.89494711235935043, -254.2627752153468350 ) ) ;
#36266 = EDGE_CURVE ( 'NONE', #22968, #205612, #70390, .T. ) ;
#36267 = DIRECTION ( 'NONE',  ( 0.000000000000000000, -1.000000000000000000, 0.000000000000000000 ) ) ;
#36268 = ORIENTED_EDGE ( 'NONE', *, *, #250852, .F. ) ;
#36269 = CARTESIAN_POINT ( 'NONE',  ( -23.25000000000000000, 1.148907358139439339E-11, -201.0000000000015064 ) ) ;
#36270 = CIRCLE ( 'NONE', #181996, 0.1000000000000033501 ) ;
#36271 = ORIENTED_EDGE ( 'NONE', *, *, #163659, .T. ) ;
#36272 = DIRECTION ( 'NONE',  ( 0.000000000000000000, -0.4721928772777383987, -0.8814952561688410571 ) ) ;
#36273 = DIRECTION ( 'NONE',  ( 0.000000000000000000, 0.4088369013363281623, -0.9126074666063771490 ) ) ;
#36274 = AXIS2_PLACEMENT_3D ( 'NONE', #193333, #72106, #113776 ) ;
#36275 = CIRCLE ( 'NONE', #57066, 11.65000000000000036 ) ;
#36276 = EDGE_CURVE ( 'NONE', #257664, #71259, #60476, .T. ) ;
#36277 = AXIS2_PLACEMENT_3D ( 'NONE', #30853, #66094, #206894 ) ;
#36278 = ORIENTED_EDGE ( 'NONE', *, *, #208715, .T. ) ;
#36279 = DIRECTION ( 'NONE',  ( 0.000000000000000000, -0.8700118002898359348, 0.4930308989875165082 ) ) ;
#36280 = ORIENTED_EDGE ( 'NONE', *, *, #40743, .F. ) ;
#36281 = CARTESIAN_POINT ( 'NONE',  ( 21.05000000000000071, -0.09999993530598326463, 6.478078221094742517 ) ) ;
#36282 = CARTESIAN_POINT ( 'NONE',  ( -18.59999999999999787, 77.14957036958736580, -61.70719500002233815 ) ) ;
#36283 = DIRECTION ( 'NONE',  ( -1.000000000000000000, -1.541880601228652843E-16, -2.878400969107353907E-16 ) ) ;
#36284 = DIRECTION ( 'NONE',  ( -1.000000000000000000, -0.000000000000000000, -0.000000000000000000 ) ) ;
#36285 = DIRECTION ( 'NONE',  ( 0.000000000000000000, -7.124650136758317602E-15, 1.000000000000000000 ) ) ;
#36286 = CARTESIAN_POINT ( 'NONE',  ( -21.45000000000000284, 7.708578643773852157, -88.15000000000004832 ) ) ;
#36287 = CYLINDRICAL_SURFACE ( 'NONE', #195560, 0.09999999999999986677 ) ;
#36289 = ORIENTED_EDGE ( 'NONE', *, *, #215764, .F. ) ;
#36288 = CARTESIAN_POINT ( 'NONE',  ( -23.25000000000000000, 73.40000000001205649, -123.2984855617622202 ) ) ;
#36290 = EDGE_LOOP ( 'NONE', ( #116524, #177793, #197525, #226464 ) ) ;
#36292 = CARTESIAN_POINT ( 'NONE',  ( -21.14999999893415250, 64.25000000001161027, -62.67861214099805522 ) ) ;
#36291 = DIRECTION ( 'NONE',  ( 0.000000000000000000, 0.000000000000000000, -1.000000000000000000 ) ) ;
#36294 = ORIENTED_EDGE ( 'NONE', *, *, #253435, .T. ) ;
#36293 = DIRECTION ( 'NONE',  ( 0.000000000000000000, 0.000000000000000000, 1.000000000000000000 ) ) ;
#36295 = AXIS2_PLACEMENT_3D ( 'NONE', #142559, #43481, #184263 ) ;
#36296 = ORIENTED_EDGE ( 'NONE', *, *, #257764, .F. ) ;
#36297 = DIRECTION ( 'NONE',  ( -1.000000000000000000, 0.000000000000000000, 0.000000000000000000 ) ) ;
#36298 = LINE ( 'NONE', #19280, #138673 ) ;
#36299 = CARTESIAN_POINT ( 'NONE',  ( 23.24999999999999645, 67.17743825834568838, -127.2731074845243597 ) ) ;
#36300 = DIRECTION ( 'NONE',  ( 1.000000000000000000, -7.304098846218134667E-16, 4.607487905232622991E-31 ) ) ;
#36301 = LINE ( 'NONE', #255270, #102556 ) ;
#36302 = CARTESIAN_POINT ( 'NONE',  ( 21.05000000000000071, 64.35000000001194564, -103.0231074845244024 ) ) ;
#36303 = DIRECTION ( 'NONE',  ( -1.000000000000000000, -0.000000000000000000, -0.000000000000000000 ) ) ;
#36304 = EDGE_CURVE ( 'NONE', #10010, #256387, #8392, .T. ) ;
#36306 = AXIS2_PLACEMENT_3D ( 'NONE', #153021, #232546, #34347 ) ;
#36305 = CARTESIAN_POINT ( 'NONE',  ( 20.94999999999999929, -9.400000000000000355, -23.60603087734755690 ) ) ;
#36307 = ORIENTED_EDGE ( 'NONE', *, *, #15509, .F. ) ;
#36308 = ORIENTED_EDGE ( 'NONE', *, *, #86373, .F. ) ;
#36309 = DIRECTION ( 'NONE',  ( 1.000000000000000000, -0.000000000000000000, -0.000000000000000000 ) ) ;
#36310 = CIRCLE ( 'NONE', #157111, 0.09999999999999939493 ) ;
#36311 = AXIS2_PLACEMENT_3D ( 'NONE', #85111, #207684, #245522 ) ;
#36312 = ORIENTED_EDGE ( 'NONE', *, *, #46602, .F. ) ;
#36313 = LINE ( 'NONE', #255280, #180273 ) ;
#36314 = EDGE_LOOP ( 'NONE', ( #246517, #82333 ) ) ;
#36315 = AXIS2_PLACEMENT_3D ( 'NONE', #184024, #210031, #130471 ) ;
#36316 = CIRCLE ( 'NONE', #248680, 0.09999999999999999167 ) ;
#36317 = DIRECTION ( 'NONE',  ( -1.000000000000000000, -0.000000000000000000, -0.000000000000000000 ) ) ;
#36318 = CARTESIAN_POINT ( 'NONE',  ( 18.59999999999999076, 10.20857864377385127, -125.2500000000000284 ) ) ;
#36319 = ADVANCED_FACE ( 'NONE', ( #85154, #222106 ), #43509, .T. ) ;
#36320 = CIRCLE ( 'NONE', #123604, 0.1000000000000028644 ) ;
#36322 = ORIENTED_EDGE ( 'NONE', *, *, #65338, .T. ) ;
#36321 = CARTESIAN_POINT ( 'NONE',  ( 18.39999999999999858, -9.682403433465241349, -207.6568433774127413 ) ) ;
#36323 = CARTESIAN_POINT ( 'NONE',  ( 19.97071067811863898, 34.44376430008541945, -235.0681652939917115 ) ) ;
#36324 = ORIENTED_EDGE ( 'NONE', *, *, #102635, .F. ) ;
#36325 = DIRECTION ( 'NONE',  ( 1.000000000000000000, 0.000000000000000000, 0.000000000000000000 ) ) ;
#36326 = EDGE_CURVE ( 'NONE', #7208, #198087, #81303, .T. ) ;
#36327 = CARTESIAN_POINT ( 'NONE',  ( 21.05000000000000071, 5.000000000011153745, -54.99473398108690958 ) ) ;
#36328 = CARTESIAN_POINT ( 'NONE',  ( -21.64999999999999858, 66.65000000001191438, -93.77310748452437394 ) ) ;
#36329 = CARTESIAN_POINT ( 'NONE',  ( -21.53551880898957904, 75.90103026544106513, -210.3079052459406739 ) ) ;
#36330 = DIRECTION ( 'NONE',  ( 0.000000000000000000, -1.000000000000000000, -7.272083257015735086E-15 ) ) ;
#36331 = VERTEX_POINT ( 'NONE', #22680 ) ;
#36333 = CARTESIAN_POINT ( 'NONE',  ( -18.58744394320951798, 85.56638515455998117, -29.20025943064833740 ) ) ;
#36332 = CARTESIAN_POINT ( 'NONE',  ( -17.01764560440540919, 60.96553306569528274, -220.9452142467251576 ) ) ;
#36335 = ADVANCED_FACE ( 'NONE', ( #102152 ), #103449, .F. ) ;
#36334 = CIRCLE ( 'NONE', #15489, 0.2000000000000119182 ) ;
#36336 = ORIENTED_EDGE ( 'NONE', *, *, #153925, .T. ) ;
#36339 = ORIENTED_EDGE ( 'NONE', *, *, #25799, .T. ) ;
#36338 = LINE ( 'NONE', #174606, #29815 ) ;
#36337 = FACE_OUTER_BOUND ( 'NONE', #254668, .T. ) ;
#36340 = CARTESIAN_POINT ( 'NONE',  ( 22.60000000000000142, 75.89914163091332000, -114.7726746080137019 ) ) ;
#36341 = AXIS2_PLACEMENT_3D ( 'NONE', #219435, #162070, #182914 ) ;
#36342 = EDGE_CURVE ( 'NONE', #211751, #52, #212415, .T. ) ;
#36343 = CIRCLE ( 'NONE', #144432, 12.87499999999999822 ) ;
#36344 = CARTESIAN_POINT ( 'NONE',  ( -22.50014994444008209, 64.25028026811935433, -69.60618764124372149 ) ) ;
#36345 = EDGE_LOOP ( 'NONE', ( #65662, #168322, #21506, #68213 ) ) ;
#36346 = CARTESIAN_POINT ( 'NONE',  ( -20.64999999999999858, 53.03738849591485405, -234.3791188517465400 ) ) ;
#36347 = EDGE_CURVE ( 'NONE', #1827, #15704, #220214, .T. ) ;
#36348 = PRESENTATION_LAYER_ASSIGNMENT (  '', '', ( #148764 ) ) ;
#36349 = CARTESIAN_POINT ( 'NONE',  ( -20.64999999999999858, 7.150000000011155876, -79.35000000000005116 ) ) ;
#36350 = AXIS2_PLACEMENT_3D ( 'NONE', #157919, #96580, #33144 ) ;
#36351 = EDGE_CURVE ( 'NONE', #71888, #165845, #108352, .T. ) ;
#36352 = CARTESIAN_POINT ( 'NONE',  ( -20.94999999999999929, 13.71992543034163958, -238.5823796952984992 ) ) ;
#36353 = CIRCLE ( 'NONE', #227855, 0.5000000000000004441 ) ;
#36355 = VERTEX_POINT ( 'NONE', #186885 ) ;
#36354 = CARTESIAN_POINT ( 'NONE',  ( -21.65000000000000213, 9.950000000011140600, -113.1500000000000341 ) ) ;
#36356 = DIRECTION ( 'NONE',  ( -0.000000000000000000, 0.000000000000000000, 1.000000000000000000 ) ) ;
#36357 = EDGE_CURVE ( 'NONE', #201727, #120967, #61984, .T. ) ;
#36358 = ORIENTED_EDGE ( 'NONE', *, *, #74980, .T. ) ;
#36359 = CARTESIAN_POINT ( 'NONE',  ( -16.92570016628984320, 9.958788957751020021, -180.1206506700389411 ) ) ;
#36360 = CARTESIAN_POINT ( 'NONE',  ( 20.94999999999999929, 0.000000000000000000, -33.50000000000000000 ) ) ;
#36361 = DIRECTION ( 'NONE',  ( 1.000000000000000000, 0.000000000000000000, 0.000000000000000000 ) ) ;
#36362 = CIRCLE ( 'NONE', #173764, 0.6000000000000033085 ) ;
#36363 = ORIENTED_EDGE ( 'NONE', *, *, #14661, .T. ) ;
#36364 = CARTESIAN_POINT ( 'NONE',  ( -21.05000000000000071, -4.714262876194486473, -233.3440214805475819 ) ) ;
#36365 = ORIENTED_EDGE ( 'NONE', *, *, #119828, .F. ) ;
#36367 = AXIS2_PLACEMENT_3D ( 'NONE', #252630, #16619, #251349 ) ;
#36366 = CARTESIAN_POINT ( 'NONE',  ( 23.14999999999999858, 28.46934351190515855, -239.7465010792843714 ) ) ;
#36368 = CARTESIAN_POINT ( 'NONE',  ( -18.59999999999999787, 11.65000000001115232, -179.6499999999999773 ) ) ;
#36369 = DIRECTION ( 'NONE',  ( -0.000000000000000000, 0.4721928772777345684, 0.8814952561688429444 ) ) ;
#36370 = B_SPLINE_CURVE_WITH_KNOTS ( 'NONE', 3,
 ( #42033, #144945, #202373, #250168, #25045, #224494, #71550, #45861, #121589, #64149 ),
 .UNSPECIFIED., .F., .F.,
 ( 4, 3, 3, 4 ),
 ( 0.000000000000000000, 0.0002000000000002908468, 0.001000000000045115191, 0.001967863649472098748 ),
 .UNSPECIFIED. ) ;
#36371 = ORIENTED_EDGE ( 'NONE', *, *, #91991, .T. ) ;
#36372 = DIRECTION ( 'NONE',  ( 1.000000000000000000, -0.000000000000000000, 0.000000000000000000 ) ) ;
#36373 = ADVANCED_FACE ( 'NONE', ( #190750 ), #9501, .F. ) ;
#36374 = DIRECTION ( 'NONE',  ( 1.000000000000000000, 0.000000000000000000, -0.000000000000000000 ) ) ;
#36375 = AXIS2_PLACEMENT_3D ( 'NONE', #58854, #241385, #139678 ) ;
#36376 = VECTOR ( 'NONE', #6594, 1000.000000000000000 ) ;
#36377 = ORIENTED_EDGE ( 'NONE', *, *, #96784, .T. ) ;
#36378 = CARTESIAN_POINT ( 'NONE',  ( -21.05000000000000071, 87.39257802171813694, -173.0970570643562212 ) ) ;
#36379 = CARTESIAN_POINT ( 'NONE',  ( -23.25000000000000000, 77.25000000001185185, -95.22262673010921219 ) ) ;
#36380 = CARTESIAN_POINT ( 'NONE',  ( -20.64999999999999858, 1.999999999999998224, -20.67537807723790166 ) ) ;
#36381 = ORIENTED_EDGE ( 'NONE', *, *, #2623, .F. ) ;
#36382 = CIRCLE ( 'NONE', #82120, 0.09999999999998898659 ) ;
#36383 = EDGE_CURVE ( 'NONE', #113855, #97476, #95301, .T. ) ;
#36384 = DIRECTION ( 'NONE',  ( -1.000000000000000000, -2.952720810173289112E-16, 0.000000000000000000 ) ) ;
#36385 = EDGE_LOOP ( 'NONE', ( #225780, #159660, #118741 ) ) ;
#36387 = VERTEX_POINT ( 'NONE', #107317 ) ;
#36386 = DIRECTION ( 'NONE',  ( 0.000000000000000000, 0.1575546449569757979, -0.9875102702516471709 ) ) ;
#36388 = CIRCLE ( 'NONE', #178034, 0.1999999999999987899 ) ;
#36389 = CIRCLE ( 'NONE', #11240, 0.1000000000000024342 ) ;
#36392 = EDGE_LOOP ( 'NONE', ( #11784, #189946, #197623 ) ) ;
#36391 = ORIENTED_EDGE ( 'NONE', *, *, #74829, .F. ) ;
#36390 = DIRECTION ( 'NONE',  ( -1.000000000000000000, 0.000000000000000000, 0.000000000000000000 ) ) ;
#36393 = AXIS2_PLACEMENT_3D ( 'NONE', #26212, #105700, #62757 ) ;
#36394 = AXIS2_PLACEMENT_3D ( 'NONE', #125922, #242030, #165067 ) ;
#36395 = CARTESIAN_POINT ( 'NONE',  ( -18.59999999999999787, 76.00000000001213607, -136.5231074845243313 ) ) ;
#36396 = CARTESIAN_POINT ( 'NONE',  ( -18.50000000000000000, -1.164121893230052995, -175.4148480855716059 ) ) ;
#36397 = CARTESIAN_POINT ( 'NONE',  ( -20.07928932188135107, 30.12641191371051264, -235.5915679455963812 ) ) ;
#36398 = DIRECTION ( 'NONE',  ( 0.000000000000000000, 0.000000000000000000, -1.000000000000000000 ) ) ;
#36399 = VECTOR ( 'NONE', #83180, 1000.000000000000114 ) ;
#36400 = EDGE_CURVE ( 'NONE', #178738, #13860, #116166, .T. ) ;
#36401 = DIRECTION ( 'NONE',  ( -1.000000000000000000, 0.000000000000000000, 0.000000000000000000 ) ) ;
#36402 = CARTESIAN_POINT ( 'NONE',  ( -23.15000000000000213, -3.664072692419560795, -226.4691047342518857 ) ) ;
#36403 = ORIENTED_EDGE ( 'NONE', *, *, #193056, .T. ) ;
#36404 = ORIENTED_EDGE ( 'NONE', *, *, #83829, .F. ) ;
#36405 = VERTEX_POINT ( 'NONE', #51172 ) ;
#36406 = DIRECTION ( 'NONE',  ( 1.000000000000000000, 0.000000000000000000, 0.000000000000000000 ) ) ;
#36408 = VERTEX_POINT ( 'NONE', #32976 ) ;
#36407 = DIRECTION ( 'NONE',  ( 0.000000000000000000, -0.9875102702516471709, 0.1575546449569757979 ) ) ;
#36409 = CARTESIAN_POINT ( 'NONE',  ( -23.15000000000000213, 1.925233644870967487, -154.7697564668738721 ) ) ;
#36410 = ORIENTED_EDGE ( 'NONE', *, *, #200265, .F. ) ;
#36411 = CYLINDRICAL_SURFACE ( 'NONE', #164325, 0.1000000000000002554 ) ;
#36412 = EDGE_CURVE ( 'NONE', #30313, #23353, #99929, .T. ) ;
#36413 = ORIENTED_EDGE ( 'NONE', *, *, #126857, .T. ) ;
#36414 = PLANE ( 'NONE',  #50419 ) ;
#36415 = CIRCLE ( 'NONE', #182144, 0.1000000000000028644 ) ;
#36416 = ADVANCED_FACE ( 'NONE', ( #192025 ), #231155, .T. ) ;
#36417 = EDGE_CURVE ( 'NONE', #102676, #39096, #20886, .T. ) ;
#36418 = VERTEX_POINT ( 'NONE', #69508 ) ;
#36419 = DIRECTION ( 'NONE',  ( 0.000000000000000000, 0.000000000000000000, -1.000000000000000000 ) ) ;
#36420 = CARTESIAN_POINT ( 'NONE',  ( -20.64999999999999858, 4.350000000011156054, -54.64999999999999858 ) ) ;
#36421 = VECTOR ( 'NONE', #87848, 1000.000000000000000 ) ;
#36423 = EDGE_LOOP ( 'NONE', ( #87802, #122295, #91640, #112261, #25590, #232539, #30227, #172643, #1205, #186695, #234743, #12280, #256000, #88334, #173716, #90715, #143444, #178359 ) ) ;
#36422 = ORIENTED_EDGE ( 'NONE', *, *, #96457, .T. ) ;
#36424 = ORIENTED_EDGE ( 'NONE', *, *, #169314, .F. ) ;
#36425 = CARTESIAN_POINT ( 'NONE',  ( 21.05000000000000071, 8.876614585087098774, -8.385080478844676222 ) ) ;
#36426 = ORIENTED_EDGE ( 'NONE', *, *, #208627, .F. ) ;
#36427 = ORIENTED_EDGE ( 'NONE', *, *, #136565, .F. ) ;
#36428 = ADVANCED_FACE ( 'NONE', ( #171203 ), #108610, .T. ) ;
#36429 = DIRECTION ( 'NONE',  ( 0.000000000000000000, -0.8660254037844411501, -0.4999999999999956701 ) ) ;
#36431 = ORIENTED_EDGE ( 'NONE', *, *, #110004, .T. ) ;
#36430 = CARTESIAN_POINT ( 'NONE',  ( -18.50000000000000000, 3.912899247244609580, -145.4818229730109920 ) ) ;
#36432 = DIRECTION ( 'NONE',  ( -4.391705002472929091E-16, 1.000000000000000000, 0.000000000000000000 ) ) ;
#36434 = CARTESIAN_POINT ( 'NONE',  ( 20.95017935633852346, 65.52451072038701341, -162.4456676871339482 ) ) ;
#36433 = CARTESIAN_POINT ( 'NONE',  ( -18.50000000000000000, 85.50000000001246292, -181.7731074845243029 ) ) ;
#36435 = CARTESIAN_POINT ( 'NONE',  ( -18.59999999999999787, 78.48087866980282001, -232.8271061603568910 ) ) ;
#36436 = CARTESIAN_POINT ( 'NONE',  ( -22.60000000000080789, 75.95218301954739104, -215.2731299156771172 ) ) ;
#36437 = DIRECTION ( 'NONE',  ( 0.000000000000000000, -1.000000000000000000, -7.272083257015735086E-15 ) ) ;
#36438 = ORIENTED_EDGE ( 'NONE', *, *, #224303, .F. ) ;
#36439 = EDGE_LOOP ( 'NONE', ( #38572, #107240, #35008, #38537 ) ) ;
#36440 = DIRECTION ( 'NONE',  ( 1.000000000000000000, 0.000000000000000000, 0.000000000000000000 ) ) ;
#36441 = DIRECTION ( 'NONE',  ( 0.000000000000000000, 0.000000000000000000, 1.000000000000000000 ) ) ;
#36442 = DIRECTION ( 'NONE',  ( -1.000000000000000000, -0.000000000000000000, -0.000000000000000000 ) ) ;
#36443 = ORIENTED_EDGE ( 'NONE', *, *, #156858, .F. ) ;
#36444 = AXIS2_PLACEMENT_3D ( 'NONE', #131438, #31101, #213534 ) ;
#36445 = AXIS2_PLACEMENT_3D ( 'NONE', #75320, #218632, #20471 ) ;
#36446 = CYLINDRICAL_SURFACE ( 'NONE', #48935, 11.80000000000000426 ) ;
#36447 = AXIS2_PLACEMENT_3D ( 'NONE', #247974, #229708, #148895 ) ;
#36448 = AXIS2_PLACEMENT_3D ( 'NONE', #203254, #5028, #28521 ) ;
#36449 = EDGE_CURVE ( 'NONE', #25213, #100977, #212020, .T. ) ;
#36450 = LINE ( 'NONE', #156404, #26312 ) ;
#36451 = CARTESIAN_POINT ( 'NONE',  ( 18.57071067811864040, 65.82071067813045318, -81.67310748452439384 ) ) ;
#36452 = EDGE_LOOP ( 'NONE', ( #197808, #95546, #42568, #84021 ) ) ;
#36453 = VERTEX_POINT ( 'NONE', #245564 ) ;
#36454 = CARTESIAN_POINT ( 'NONE',  ( 23.14999999999999858, 76.00000000001126921, -203.5231074845248997 ) ) ;
#36455 = CARTESIAN_POINT ( 'NONE',  ( -16.77683809663752257, 66.05416425680790837, -123.8591584654201512 ) ) ;
#36457 = EDGE_LOOP ( 'NONE', ( #43068, #134019, #117982, #228813, #53937 ) ) ;
#36456 = EDGE_CURVE ( 'NONE', #156548, #33205, #75397, .T. ) ;
#36458 = DIRECTION ( 'NONE',  ( 0.000000000000000000, 1.000000000000000000, 7.116814260417668513E-15 ) ) ;
#36459 = ORIENTED_EDGE ( 'NONE', *, *, #216556, .F. ) ;
#36460 = EDGE_CURVE ( 'NONE', #161032, #136223, #151623, .T. ) ;
#36461 = CARTESIAN_POINT ( 'NONE',  ( 11.60000000000006004, 67.72071067812984779, -17.05239680640613997 ) ) ;
#36462 = PLANE ( 'NONE',  #241354 ) ;
#36464 = FACE_OUTER_BOUND ( 'NONE', #101030, .T. ) ;
#36463 = DIRECTION ( 'NONE',  ( 1.000000000000000000, 0.000000000000000000, 0.000000000000000000 ) ) ;
#36465 = CARTESIAN_POINT ( 'NONE',  ( -18.50000000000000000, 42.15997144203495139, -239.2817429668763793 ) ) ;
#36466 = CARTESIAN_POINT ( 'NONE',  ( 21.05000000000000071, 65.27628289530434813, -90.87310748452438247 ) ) ;
#36467 = CIRCLE ( 'NONE', #111272, 0.09999999999999609201 ) ;
#36468 = AXIS2_PLACEMENT_3D ( 'NONE', #201389, #96185, #103556 ) ;
#36469 = FACE_OUTER_BOUND ( 'NONE', #15216, .T. ) ;
#36471 = ORIENTED_EDGE ( 'NONE', *, *, #107347, .F. ) ;
#36470 = ORIENTED_EDGE ( 'NONE', *, *, #2623, .T. ) ;
#36472 = AXIS2_PLACEMENT_3D ( 'NONE', #93057, #10965, #213008 ) ;
#36473 = ORIENTED_EDGE ( 'NONE', *, *, #225442, .F. ) ;
#36474 = CARTESIAN_POINT ( 'NONE',  ( 18.39999999999999858, -9.599999999988842347, -141.0320693966996828 ) ) ;
#36475 = DIRECTION ( 'NONE',  ( 1.000000000000000000, -1.207181226542539700E-16, 2.694675058168174199E-16 ) ) ;
#36476 = DIRECTION ( 'NONE',  ( -1.000000000000000000, 0.000000000000000000, 0.000000000000000000 ) ) ;
#36477 = CARTESIAN_POINT ( 'NONE',  ( -23.25000000000000000, 70.05000000001251692, -180.3288097895592159 ) ) ;
#36478 =( BOUNDED_SURFACE ( )  B_SPLINE_SURFACE ( 3, 2, ( 
 ( #44565, #180231, #198492 ),
 ( #237631, #103224, #25021 ),
 ( #61559, #201063, #5397 ),
 ( #163234, #1563, #121564 ),
 ( #2842, #81098, #181522 ),
 ( #160689, #19877, #240205 ),
 ( #182807, #184063, #4139 ),
 ( #101932, #84928, #124112 ),
 ( #99370, #138491, #141100 ),
 ( #220633, #161961, #40745 ) ),
 .UNSPECIFIED., .F., .F., .F. ) 
 B_SPLINE_SURFACE_WITH_KNOTS ( ( 4, 2, 2, 2, 4 ),
 ( 3, 3 ),
 ( 0.002161241639767792072, 0.002579950749617453305, 0.002789305304542283922, 0.002893982582004699447, 0.002998659859467114538 ),
 ( 0.000000000000000000, 1.000000000000000000 ),
 .UNSPECIFIED. ) 
 GEOMETRIC_REPRESENTATION_ITEM ( )  RATIONAL_B_SPLINE_SURFACE ( (
 ( 1.000000000000000000, 0.7071067811864985009, 1.000000000000000000),
 ( 1.000000000000000000, 0.7632447400665891557, 1.000000000000000000),
 ( 1.000000000000000000, 0.8158073005106942777, 1.000000000000000000),
 ( 1.000000000000000000, 0.8906973462396924335, 1.000000000000000000),
 ( 1.000000000000000000, 0.9149408947797951219, 1.000000000000000000),
 ( 1.000000000000000000, 0.9493368785276811161, 1.000000000000000000),
 ( 1.000000000000000000, 0.9605194247156072507, 1.000000000000000000),
 ( 1.000000000000000000, 0.9803630264781720838, 1.000000000000000000),
 ( 1.000000000000000000, 0.9900844824270710332, 1.000000000000000000),
 ( 1.000000000000000000, 0.9894588281429290699, 1.000000000000000000) ) ) 
 REPRESENTATION_ITEM ( '' )  SURFACE ( )  );
#36480 = DIRECTION ( 'NONE',  ( 0.000000000000000000, 0.2128009952263485993, -0.9770955615653341697 ) ) ;
#36479 = CARTESIAN_POINT ( 'NONE',  ( 20.22516295850462598, 9.899364295449302631, -7.910065712091376433 ) ) ;
#36481 = CARTESIAN_POINT ( 'NONE',  ( -16.79140778683510504, 66.05505840115696969, -48.69337025075360259 ) ) ;
#36482 = VERTEX_POINT ( 'NONE', #188155 ) ;
#36483 = CARTESIAN_POINT ( 'NONE',  ( -21.05000000000000071, -11.64999999998884306, -130.9000000000000341 ) ) ;
#36484 = ORIENTED_EDGE ( 'NONE', *, *, #222834, .T. ) ;
#36486 = EDGE_CURVE ( 'NONE', #44866, #70684, #135502, .T. ) ;
#36485 = ORIENTED_EDGE ( 'NONE', *, *, #231563, .T. ) ;
#36487 = CARTESIAN_POINT ( 'NONE',  ( -20.64999999999999858, 74.05981308412415842, -115.8522266955776416 ) ) ;
#36488 = PLANE ( 'NONE',  #93261 ) ;
#36489 = ADVANCED_FACE ( 'NONE', ( #149042 ), #224473, .T. ) ;
#36490 = CIRCLE ( 'NONE', #107539, 2.000000000000001776 ) ;
#36492 = CARTESIAN_POINT ( 'NONE',  ( -21.13614978966382196, 60.95876181140594952, -234.1539663637506123 ) ) ;
#36491 = VECTOR ( 'NONE', #223609, 1000.000000000000000 ) ;
#36493 = DIRECTION ( 'NONE',  ( 0.000000000000000000, 0.000000000000000000, -1.000000000000000000 ) ) ;
#36494 = ORIENTED_EDGE ( 'NONE', *, *, #252667, .T. ) ;
#36495 = ORIENTED_EDGE ( 'NONE', *, *, #144830, .T. ) ;
#36496 = DIRECTION ( 'NONE',  ( 0.000000000000000000, -0.9188841341108708871, -0.3945274997757635127 ) ) ;
#36498 = ADVANCED_FACE ( 'NONE', ( #10800 ), #90314, .T. ) ;
#36497 = CARTESIAN_POINT ( 'NONE',  ( -18.52139480978223318, -9.481358845055737561, -40.52455656711906329 ) ) ;
#36499 = DIRECTION ( 'NONE',  ( -1.000000000000000000, 0.000000000000000000, 0.000000000000000000 ) ) ;
#36500 = CARTESIAN_POINT ( 'NONE',  ( 21.05000000000000071, 76.00000000001197975, -107.3231074845243427 ) ) ;
#36501 = AXIS2_PLACEMENT_3D ( 'NONE', #183106, #224770, #163529 ) ;
#36502 = CARTESIAN_POINT ( 'NONE',  ( -18.50000000000000000, 66.85000000001245724, -181.7731074845244166 ) ) ;
#36503 = CARTESIAN_POINT ( 'NONE',  ( -22.59999999999999787, 11.45898712536580177, -198.4011321578509808 ) ) ;
#36504 = ADVANCED_FACE ( 'NONE', ( #111184 ), #178730, .F. ) ;
#36506 = CARTESIAN_POINT ( 'NONE',  ( -20.94999999999999929, 11.75000000001115197, -174.5148057706539930 ) ) ;
#36505 = CARTESIAN_POINT ( 'NONE',  ( 20.85000000000000142, 0.000000000000000000, -41.40000000000000568 ) ) ;
#36507 = CARTESIAN_POINT ( 'NONE',  ( -22.39999999999999858, 75.90000000001273861, -211.3138870828977645 ) ) ;
#36508 = CIRCLE ( 'NONE', #48929, 0.09999999999999976963 ) ;
#36509 = DIRECTION ( 'NONE',  ( 0.000000000000000000, -0.2128009952263604232, 0.9770955615653316162 ) ) ;
#36511 = EDGE_CURVE ( 'NONE', #242970, #199921, #115035, .T. ) ;
#36510 = DIRECTION ( 'NONE',  ( 0.000000000000000000, 0.9126074666063769270, 0.4088369013363284399 ) ) ;
#36512 = CARTESIAN_POINT ( 'NONE',  ( 21.09316766718127667, 69.62984668753827577, -203.5623708868390906 ) ) ;
#36513 = AXIS2_PLACEMENT_3D ( 'NONE', #25413, #67090, #47507 ) ;
#36515 = EDGE_LOOP ( 'NONE', ( #238762, #15576, #251619, #206031 ) ) ;
#36514 = DIRECTION ( 'NONE',  ( 0.000000000000000000, 1.265107689135680095E-16, -1.000000000000000000 ) ) ;
#36516 = TOROIDAL_SURFACE ( 'NONE', #73922, 4.150000000000000355, 0.1000000000000000056 ) ;
#36517 = CIRCLE ( 'NONE', #128629, 0.5000000000000004441 ) ;
#36518 =( BOUNDED_CURVE ( )  B_SPLINE_CURVE ( 3, ( #241389, #67867, #105684, #163140 ),
 .UNSPECIFIED., .F., .F. ) 
 B_SPLINE_CURVE_WITH_KNOTS ( ( 4, 4 ),
 ( 4.712388980384689674, 6.283185307179586232 ),
 .UNSPECIFIED. ) 
 CURVE ( )  GEOMETRIC_REPRESENTATION_ITEM ( )  RATIONAL_B_SPLINE_CURVE ( ( 1.000000000000000000, 0.8047378541243649375, 0.8047378541243649375, 1.000000000000000000 ) ) 
 REPRESENTATION_ITEM ( '' )  );
#36519 = EDGE_CURVE ( 'NONE', #20391, #69086, #212859, .T. ) ;
#36521 = ADVANCED_FACE ( 'NONE', ( #98008 ), #232437, .T. ) ;
#36520 = AXIS2_PLACEMENT_3D ( 'NONE', #134835, #73639, #213115 ) ;
#36522 = CARTESIAN_POINT ( 'NONE',  ( 20.95052659398289308, 10.47982436779105875, -41.07523875586560536 ) ) ;
#36523 = CIRCLE ( 'NONE', #165500, 0.09999999999998898659 ) ;
#36524 = ORIENTED_EDGE ( 'NONE', *, *, #83752, .T. ) ;
#36525 = DIRECTION ( 'NONE',  ( -7.304098846217948299E-16, -1.000000000000000000, 0.000000000000000000 ) ) ;
#36526 = CARTESIAN_POINT ( 'NONE',  ( 20.94999999999999929, 76.00000000001170974, -69.52310748452431710 ) ) ;
#36527 = EDGE_LOOP ( 'NONE', ( #78486, #246618, #255392, #47106 ) ) ;
#36528 = CARTESIAN_POINT ( 'NONE',  ( -18.59999999999999787, 85.40000000001138858, -29.14106563635158764 ) ) ;
#36529 = CARTESIAN_POINT ( 'NONE',  ( 21.03675099975491136, 8.875180032795963569, -45.82554213677805421 ) ) ;
#36530 = CARTESIAN_POINT ( 'NONE',  ( -22.47071067811865319, 76.00000000001237765, -170.0231074845243597 ) ) ;
#36531 = VECTOR ( 'NONE', #14112, 1000.000000000000114 ) ;
#36532 = ADVANCED_FACE ( 'NONE', ( #215413 ), #232875, .T. ) ;
#36533 = DIRECTION ( 'NONE',  ( 0.000000000000000000, 0.000000000000000000, -1.000000000000000000 ) ) ;
#36535 = ADVANCED_FACE ( 'NONE', ( #94172 ), #12124, .F. ) ;
#36534 = AXIS2_PLACEMENT_3D ( 'NONE', #224920, #247054, #11034 ) ;
#36536 = CARTESIAN_POINT ( 'NONE',  ( -23.15000000000000213, 76.00000000001212186, -134.4231074845243370 ) ) ;
#36537 = CARTESIAN_POINT ( 'NONE',  ( -18.50000000000000000, 11.75000000001115197, -21.75000000000000355 ) ) ;
#36538 = AXIS2_PLACEMENT_3D ( 'NONE', #11730, #9145, #52097 ) ;
#36539 = AXIS2_PLACEMENT_3D ( 'NONE', #130967, #90541, #72290 ) ;
#36540 = ORIENTED_EDGE ( 'NONE', *, *, #147888, .T. ) ;
#36541 = CARTESIAN_POINT ( 'NONE',  ( 20.94999999999999929, 6.846123162363745074, -137.7377262668498759 ) ) ;
#36544 = VERTEX_POINT ( 'NONE', #56324 ) ;
#36543 = CARTESIAN_POINT ( 'NONE',  ( 21.05000000000000071, 5.500000000011153745, -155.0947339810869323 ) ) ;
#36542 = CIRCLE ( 'NONE', #78184, 0.09999999999998898659 ) ;
#36545 = DIRECTION ( 'NONE',  ( 0.000000000000000000, 0.8660254037844420383, -0.4999999999999943379 ) ) ;
#36546 = EDGE_CURVE ( 'NONE', #207912, #45068, #16390, .T. ) ;
#36547 = DIRECTION ( 'NONE',  ( 0.000000000000000000, 0.2128009952263237581, -0.9770955615653394988 ) ) ;
#36548 = AXIS2_PLACEMENT_3D ( 'NONE', #136693, #76721, #251512 ) ;
#36549 = CARTESIAN_POINT ( 'NONE',  ( -22.49544290803669000, 31.79553970091675907, -238.8548453295646823 ) ) ;
#36550 = ORIENTED_EDGE ( 'NONE', *, *, #66638, .T. ) ;
#36551 = CYLINDRICAL_SURFACE ( 'NONE', #138743, 5.000000000000004441 ) ;
#36552 = APPLICATION_PROTOCOL_DEFINITION ( 'draft international standard', 'automotive_design', 1998, #179206 ) ;
#36553 = EDGE_CURVE ( 'NONE', #178255, #156566, #182980, .T. ) ;
#36554 = CARTESIAN_POINT ( 'NONE',  ( 22.59066674512273920, 11.47438154053713077, -198.4697828622833242 ) ) ;
#36555 = DIRECTION ( 'NONE',  ( -2.952720810173289112E-16, 1.000000000000000000, 0.000000000000000000 ) ) ;
#36556 = ORIENTED_EDGE ( 'NONE', *, *, #58218, .F. ) ;
#36557 = DIRECTION ( 'NONE',  ( -0.000000000000000000, 0.2128009952263604232, -0.9770955615653316162 ) ) ;
#36558 = CARTESIAN_POINT ( 'NONE',  ( 21.05000000000000071, 23.45160524131172153, -253.2535058871250726 ) ) ;
#36559 = EDGE_CURVE ( 'NONE', #39027, #122601, #118905, .T. ) ;
#36560 = VECTOR ( 'NONE', #83223, 1000.000000000000000 ) ;
#36561 = AXIS2_PLACEMENT_3D ( 'NONE', #172248, #152671, #53538 ) ;
#36562 = VECTOR ( 'NONE', #33326, 1000.000000000000000 ) ;
#36563 = FILL_AREA_STYLE_COLOUR ( '', #145386 ) ;
#36564 = EDGE_LOOP ( 'NONE', ( #136153, #206172, #49780, #93433 ) ) ;
#36565 = ORIENTED_EDGE ( 'NONE', *, *, #37990, .T. ) ;
#36566 = EDGE_CURVE ( 'NONE', #71259, #125186, #174645, .T. ) ;
#36567 = CARTESIAN_POINT ( 'NONE',  ( -22.50000000000088463, 75.95463834342417897, -114.6736163187350002 ) ) ;
#36568 = CARTESIAN_POINT ( 'NONE',  ( -21.05000000000000071, 76.00000000001264766, -199.2231074845243768 ) ) ;
#36569 = FACE_OUTER_BOUND ( 'NONE', #237870, .T. ) ;
#36570 = DIRECTION ( 'NONE',  ( 0.000000000000000000, 0.2128009952263621163, -0.9770955615653311721 ) ) ;
#36571 = DIRECTION ( 'NONE',  ( 0.000000000000000000, 0.000000000000000000, -1.000000000000000000 ) ) ;
#36572 = CIRCLE ( 'NONE', #182289, 11.64999999999999325 ) ;
#36574 = CARTESIAN_POINT ( 'NONE',  ( -18.50000000000000000, 21.13195309841794867, -243.6318585593224100 ) ) ;
#36573 = CARTESIAN_POINT ( 'NONE',  ( 21.11825140030103043, -1.364550518801973977, -194.7006879377100006 ) ) ;
#36575 = ADVANCED_FACE ( 'NONE', ( #55035 ), #195877, .F. ) ;
#36576 = DIRECTION ( 'NONE',  ( -1.000000000000000000, -0.000000000000000000, -0.000000000000000000 ) ) ;
#36577 = AXIS2_PLACEMENT_3D ( 'NONE', #109959, #90394, #169990 ) ;
#36578 = CARTESIAN_POINT ( 'NONE',  ( 18.39999999999999503, 5.650000000011139001, -121.3500000000000369 ) ) ;
#36579 = CARTESIAN_POINT ( 'NONE',  ( -18.59999999999999787, 9.350000000011156942, -45.85000000000000142 ) ) ;
#36580 = CARTESIAN_POINT ( 'NONE',  ( 20.94999999999999929, 8.433899723187009201, -209.4150263691077782 ) ) ;
#36581 = ORIENTED_EDGE ( 'NONE', *, *, #124514, .T. ) ;
#36582 = VERTEX_POINT ( 'NONE', #253246 ) ;
#36583 = DIRECTION ( 'NONE',  ( 1.000000000000000000, -3.265361837132813093E-16, -2.280189983783949500E-30 ) ) ;
#36584 = CARTESIAN_POINT ( 'NONE',  ( -21.65000000000000213, 7.708578643773852157, -188.7499999999999716 ) ) ;
#36586 = CARTESIAN_POINT ( 'NONE',  ( -20.64999999999999858, 7.150000000011155876, -112.8500000000000369 ) ) ;
#36585 = CARTESIAN_POINT ( 'NONE',  ( 23.24999999999999645, 5.600000000011153389, -54.59473398108690390 ) ) ;
#36587 = CYLINDRICAL_SURFACE ( 'NONE', #105920, 0.1000000000000106498 ) ;
#36588 = DIRECTION ( 'NONE',  ( 0.000000000000000000, 0.000000000000000000, 1.000000000000000000 ) ) ;
#36589 = EDGE_CURVE ( 'NONE', #139686, #117646, #87087, .T. ) ;
#36590 = CARTESIAN_POINT ( 'NONE',  ( 14.88075390448863544, 13.10551310878183706, -216.8535402360471949 ) ) ;
#36591 = ORIENTED_EDGE ( 'NONE', *, *, #119729, .T. ) ;
#36592 = VECTOR ( 'NONE', #50443, 1000.000000000000000 ) ;
#36593 = EDGE_LOOP ( 'NONE', ( #178185, #176724 ) ) ;
#36594 = AXIS2_PLACEMENT_3D ( 'NONE', #227942, #210949, #111852 ) ;
#36595 = AXIS2_PLACEMENT_3D ( 'NONE', #140037, #37133, #35844 ) ;
#36596 = DIRECTION ( 'NONE',  ( -1.000000000000000000, 0.000000000000000000, 0.000000000000000000 ) ) ;
#36597 = VECTOR ( 'NONE', #146582, 1000.000000000000000 ) ;
#36598 = ORIENTED_EDGE ( 'NONE', *, *, #149687, .T. ) ;
#36599 = DIRECTION ( 'NONE',  ( 1.000000000000000000, 0.000000000000000000, -0.000000000000000000 ) ) ;
#36600 = VECTOR ( 'NONE', #178183, 1000.000000000000000 ) ;
#36601 = CARTESIAN_POINT ( 'NONE',  ( 23.24999999999999645, 76.00000000001190870, -103.0231074845243029 ) ) ;
#36602 = DIRECTION ( 'NONE',  ( 0.000000000000000000, -6.982962677686266711E-15, 1.000000000000000000 ) ) ;
#36603 = ORIENTED_EDGE ( 'NONE', *, *, #61390, .T. ) ;
#36604 = LINE ( 'NONE', #70593, #180655 ) ;
#36605 = ORIENTED_EDGE ( 'NONE', *, *, #11194, .T. ) ;
#36606 = CARTESIAN_POINT ( 'NONE',  ( 20.94999999999999929, 7.021664781911246322, -104.3335654018973315 ) ) ;
#36607 = DIRECTION ( 'NONE',  ( 0.000000000000000000, -0.8814952561688430555, 0.4721928772777346239 ) ) ;
#36609 = AXIS2_PLACEMENT_3D ( 'NONE', #75071, #76304, #98404 ) ;
#36608 = CARTESIAN_POINT ( 'NONE',  ( -21.05000000000000071, 77.83534155023646406, -124.9679561919613064 ) ) ;
#36610 = LINE ( 'NONE', #174853, #24961 ) ;
#36611 = DIRECTION ( 'NONE',  ( -0.000000000000000000, 0.000000000000000000, -1.000000000000000000 ) ) ;
#36612 = DIRECTION ( 'NONE',  ( -0.000000000000000000, -0.000000000000000000, -1.000000000000000000 ) ) ;
#36613 = CARTESIAN_POINT ( 'NONE',  ( -16.80891096016306108, 66.05000000001224691, -149.1554446772547635 ) ) ;
#36614 = VERTEX_POINT ( 'NONE', #38085 ) ;
#36616 = DIRECTION ( 'NONE',  ( 0.000000000000000000, 0.000000000000000000, -1.000000000000000000 ) ) ;
#36615 = DIRECTION ( 'NONE',  ( 1.000000000000000000, 0.000000000000000000, 0.000000000000000000 ) ) ;
#36617 = ORIENTED_EDGE ( 'NONE', *, *, #8178, .F. ) ;
#36619 = EDGE_LOOP ( 'NONE', ( #183884, #167924, #178292, #152997 ) ) ;
#36618 = LINE ( 'NONE', #152714, #123443 ) ;
#36620 = AXIS2_PLACEMENT_3D ( 'NONE', #191841, #133124, #36622 ) ;
#36621 = ORIENTED_EDGE ( 'NONE', *, *, #97874, .F. ) ;
#36622 = DIRECTION ( 'NONE',  ( 0.000000000000000000, 0.9394191166662618775, 0.3427706569150580362 ) ) ;
#36623 = DIRECTION ( 'NONE',  ( 0.000000000000000000, 0.000000000000000000, -1.000000000000000000 ) ) ;
#36624 = CARTESIAN_POINT ( 'NONE',  ( -23.25000000000000000, 8.653397185701672711, -220.7611668973962367 ) ) ;
#36625 = DIRECTION ( 'NONE',  ( -1.000000000000000000, 0.000000000000000000, 0.000000000000000000 ) ) ;
#36626 = ORIENTED_EDGE ( 'NONE', *, *, #166485, .T. ) ;
#36627 = CARTESIAN_POINT ( 'NONE',  ( -20.94999999999999929, 46.45388641681647357, -243.1520440498138385 ) ) ;
#36628 = CARTESIAN_POINT ( 'NONE',  ( -18.59999999999999787, 5.341242989991650703, 9.806650206488024324 ) ) ;
#36629 = CARTESIAN_POINT ( 'NONE',  ( -21.06715728752538652, 64.25000000001264766, -196.5083017138704236 ) ) ;
#36630 = ORIENTED_EDGE ( 'NONE', *, *, #153882, .F. ) ;
#36631 = CARTESIAN_POINT ( 'NONE',  ( -17.11825945287482753, 44.22674245267958781, -235.2580479164738279 ) ) ;
#36632 = EDGE_CURVE ( 'NONE', #46505, #141039, #77182, .T. ) ;
#36633 = CARTESIAN_POINT ( 'NONE',  ( -16.97683809663752186, 66.05000000001226113, -149.9254715027207681 ) ) ;
#36634 = TOROIDAL_SURFACE ( 'NONE', #236497, 12.97499999999999609, 0.1000000000000000056 ) ;
#36635 = ORIENTED_EDGE ( 'NONE', *, *, #176831, .T. ) ;
#36637 = ORIENTED_EDGE ( 'NONE', *, *, #199609, .T. ) ;
#36636 = AXIS2_PLACEMENT_3D ( 'NONE', #9866, #252311, #132386 ) ;
#36638 = DIRECTION ( 'NONE',  ( 0.000000000000000000, -0.000000000000000000, 1.000000000000000000 ) ) ;
#36639 = AXIS2_PLACEMENT_3D ( 'NONE', #63423, #43876, #244629 ) ;
#36640 = ORIENTED_EDGE ( 'NONE', *, *, #62588, .F. ) ;
#36641 = DIRECTION ( 'NONE',  ( 0.000000000000000000, -6.454785026890489601E-15, 1.000000000000000000 ) ) ;
#36642 = VERTEX_POINT ( 'NONE', #234992 ) ;
#36643 = CARTESIAN_POINT ( 'NONE',  ( 21.05000000000000071, 75.96513199699931818, -176.2931933482134923 ) ) ;
#36644 = CARTESIAN_POINT ( 'NONE',  ( 21.05000000000000071, 67.92720994251783395, -214.1870976236629929 ) ) ;
#36645 = CARTESIAN_POINT ( 'NONE',  ( 23.14999999999999858, 5.000000000011153745, -79.40526601891313874 ) ) ;
#36646 = CARTESIAN_POINT ( 'NONE',  ( -21.65000000000000213, 68.29142135624915966, -90.77310748452437394 ) ) ;
#36647 = EDGE_CURVE ( 'NONE', #248809, #216685, #136990, .T. ) ;
#36648 = CIRCLE ( 'NONE', #86465, 11.65000000000000036 ) ;
#36650 = AXIS2_PLACEMENT_3D ( 'NONE', #153025, #216798, #117704 ) ;
#36649 = CYLINDRICAL_SURFACE ( 'NONE', #137875, 0.09999999999999939493 ) ;
#36651 = LINE ( 'NONE', #233551, #72518 ) ;
#36652 = VERTEX_POINT ( 'NONE', #173781 ) ;
#36654 = CYLINDRICAL_SURFACE ( 'NONE', #210597, 0.09999999999999939493 ) ;
#36653 = DIRECTION ( 'NONE',  ( 1.000000000000000000, 0.000000000000000000, 0.000000000000000000 ) ) ;
#36655 = VERTEX_POINT ( 'NONE', #96721 ) ;
#36658 = ORIENTED_EDGE ( 'NONE', *, *, #92096, .T. ) ;
#36657 = DIRECTION ( 'NONE',  ( -1.000000000000000000, 0.000000000000000000, 0.000000000000000000 ) ) ;
#36656 = CARTESIAN_POINT ( 'NONE',  ( -21.07928932188134041, 0.09889514566555068775, -27.17148334360670958 ) ) ;
#36659 = ORIENTED_EDGE ( 'NONE', *, *, #250280, .T. ) ;
#36660 = AXIS2_PLACEMENT_3D ( 'NONE', #204760, #81263, #105645 ) ;
#36661 = DIRECTION ( 'NONE',  ( 0.000000000000000000, 0.9999176327611370985, -0.01283462868041286391 ) ) ;
#36662 = CARTESIAN_POINT ( 'NONE',  ( 13.12220780326570768, 66.56936653093944756, -154.7913416897003174 ) ) ;
#36663 = CARTESIAN_POINT ( 'NONE',  ( 18.59999999999999787, 0.000000000000000000, 0.000000000000000000 ) ) ;
#36664 = ADVANCED_FACE ( 'NONE', ( #156759, #236262, #217960 ), #57610, .F. ) ;
#36665 = CARTESIAN_POINT ( 'NONE',  ( 20.94999999999999574, 77.73625713161000306, -191.9544551555068495 ) ) ;
#36666 = VERTEX_POINT ( 'NONE', #224393 ) ;
#36668 = ORIENTED_EDGE ( 'NONE', *, *, #254579, .F. ) ;
#36667 = FACE_OUTER_BOUND ( 'NONE', #54574, .T. ) ;
#36669 = EDGE_CURVE ( 'NONE', #148687, #164610, #95477, .T. ) ;
#36670 = ADVANCED_FACE ( 'NONE', ( #180160 ), #221809, .F. ) ;
#36672 = FACE_OUTER_BOUND ( 'NONE', #137804, .T. ) ;
#36671 = CARTESIAN_POINT ( 'NONE',  ( 19.97071067811864609, 11.72071067811865674, -24.65000000000000213 ) ) ;
#36674 = ORIENTED_EDGE ( 'NONE', *, *, #96406, .T. ) ;
#36673 = CARTESIAN_POINT ( 'NONE',  ( 23.24999999999999289, 31.94635157770351341, -238.7871412784868710 ) ) ;
#36675 = EDGE_CURVE ( 'NONE', #180615, #66806, #107958, .T. ) ;
#36676 = ORIENTED_EDGE ( 'NONE', *, *, #13931, .F. ) ;
#36677 = AXIS2_PLACEMENT_3D ( 'NONE', #51826, #251321, #88384 ) ;
#36678 = CIRCLE ( 'NONE', #132503, 0.09999999999999963085 ) ;
#36679 = VECTOR ( 'NONE', #178325, 1000.000000000000114 ) ;
#36680 = CARTESIAN_POINT ( 'NONE',  ( 20.95325940946048249, 11.89208280016391583, -206.1518144919116651 ) ) ;
#36681 = CARTESIAN_POINT ( 'NONE',  ( -20.05000000000000426, 9.250000000011157297, -88.15000000000004832 ) ) ;
#36682 = ORIENTED_EDGE ( 'NONE', *, *, #38099, .F. ) ;
#36683 = DIRECTION ( 'NONE',  ( 0.000000000000000000, 0.9651348961777158619, -0.2617529984165031243 ) ) ;
#36684 = EDGE_CURVE ( 'NONE', #42158, #129497, #178900, .T. ) ;
#36685 = ORIENTED_EDGE ( 'NONE', *, *, #99249, .T. ) ;
#36686 = CARTESIAN_POINT ( 'NONE',  ( -20.85000000000000142, 79.15532900748003442, -196.2806010913881778 ) ) ;
#36687 = DIRECTION ( 'NONE',  ( 0.000000000000000000, -0.1022405907414443982, -0.9947597004326425019 ) ) ;
#36688 = AXIS2_PLACEMENT_3D ( 'NONE', #116691, #18872, #160977 ) ;
#36689 = EDGE_LOOP ( 'NONE', ( #23560, #50621, #253483 ) ) ;
#36690 = DIRECTION ( 'NONE',  ( 0.000000000000000000, 0.000000000000000000, 1.000000000000000000 ) ) ;
#36691 = EDGE_CURVE ( 'NONE', #197787, #183680, #1494, .T. ) ;
#36692 = VECTOR ( 'NONE', #227135, 1000.000000000000000 ) ;
#36693 = VECTOR ( 'NONE', #8532, 1000.000000000000000 ) ;
#36694 = DIRECTION ( 'NONE',  ( -1.000000000000000000, 0.000000000000000000, 0.000000000000000000 ) ) ;
#36695 = AXIS2_PLACEMENT_3D ( 'NONE', #226419, #49083, #115478 ) ;
#36696 = VERTEX_POINT ( 'NONE', #4069 ) ;
#36697 = ORIENTED_EDGE ( 'NONE', *, *, #176052, .T. ) ;
#36699 = CARTESIAN_POINT ( 'NONE',  ( 20.72390388899194136, 18.75055638538003322, -227.9445042245518209 ) ) ;
#36698 = VECTOR ( 'NONE', #61541, 1000.000000000000000 ) ;
#36700 = EDGE_LOOP ( 'NONE', ( #28933, #37671, #95510, #25406 ) ) ;
#36701 = EDGE_LOOP ( 'NONE', ( #114808, #209586, #5664, #224072 ) ) ;
#36703 = EDGE_LOOP ( 'NONE', ( #121744, #16073, #169454, #56547 ) ) ;
#36702 = DIRECTION ( 'NONE',  ( 0.000000000000000000, 0.8700118002898357128, -0.4930308989875170633 ) ) ;
#36704 = ORIENTED_EDGE ( 'NONE', *, *, #11374, .T. ) ;
#36705 = CARTESIAN_POINT ( 'NONE',  ( -21.14999999999999858, 76.10000000001276987, -215.1726782920691505 ) ) ;
#36708 = EDGE_LOOP ( 'NONE', ( #48915, #113114, #84453, #129194 ) ) ;
#36707 = EDGE_LOOP ( 'NONE', ( #183125, #221018, #50564, #54388 ) ) ;
#36706 = LINE ( 'NONE', #54928, #243524 ) ;
#36710 = EDGE_LOOP ( 'NONE', ( #83037, #61671, #35994, #22539 ) ) ;
#36709 = AXIS2_PLACEMENT_3D ( 'NONE', #165156, #189551, #66043 ) ;
#36711 = CARTESIAN_POINT ( 'NONE',  ( 20.85000000000000142, 69.15387683765983695, -166.2853812176745691 ) ) ;
#36712 = TOROIDAL_SURFACE ( 'NONE', #140731, 0.2000000000000000111, 0.1000000000000000056 ) ;
#36713 = FACE_OUTER_BOUND ( 'NONE', #44328, .T. ) ;
#36714 = ADVANCED_FACE ( 'NONE', ( #142294 ), #143586, .T. ) ;
#36715 = CIRCLE ( 'NONE', #186538, 0.1000000000000028644 ) ;
#36716 = CARTESIAN_POINT ( 'NONE',  ( -23.15000000000000213, -3.770473190032741062, -225.9805569534692324 ) ) ;
#36718 = EDGE_CURVE ( 'NONE', #53624, #2075, #49699, .T. ) ;
#36717 = VECTOR ( 'NONE', #251880, 1000.000000000000000 ) ;
#36719 = ORIENTED_EDGE ( 'NONE', *, *, #200167, .F. ) ;
#36720 = AXIS2_PLACEMENT_3D ( 'NONE', #155006, #137961, #160137 ) ;
#36722 = ORIENTED_EDGE ( 'NONE', *, *, #194198, .T. ) ;
#36721 = DIRECTION ( 'NONE',  ( -1.073024830501117725E-15, 0.000000000000000000, 1.000000000000000000 ) ) ;
#36723 = DIRECTION ( 'NONE',  ( 1.000000000000000000, 2.952720810173289112E-16, -0.000000000000000000 ) ) ;
#36724 = ORIENTED_EDGE ( 'NONE', *, *, #11361, .T. ) ;
#36725 = AXIS2_PLACEMENT_3D ( 'NONE', #115536, #215905, #111696 ) ;
#36726 = EDGE_CURVE ( 'NONE', #79169, #171172, #132906, .T. ) ;
#36727 = EDGE_CURVE ( 'NONE', #69371, #188456, #81021, .T. ) ;
#36728 = ORIENTED_EDGE ( 'NONE', *, *, #83625, .T. ) ;
#36729 = DIRECTION ( 'NONE',  ( 1.000000000000000000, -1.156482317317869556E-14, 0.000000000000000000 ) ) ;
#36730 = EDGE_CURVE ( 'NONE', #104197, #99499, #40678, .T. ) ;
#36731 = ORIENTED_EDGE ( 'NONE', *, *, #220299, .F. ) ;
#36732 = ORIENTED_EDGE ( 'NONE', *, *, #148365, .T. ) ;
#36733 = DIRECTION ( 'NONE',  ( 1.000000000000000000, 0.000000000000000000, 0.000000000000000000 ) ) ;
#36735 = EDGE_CURVE ( 'NONE', #56714, #250188, #116349, .T. ) ;
#36734 = CARTESIAN_POINT ( 'NONE',  ( -23.25000000000000000, 64.25000000001215028, -136.5231074845244166 ) ) ;
#36737 = EDGE_CURVE ( 'NONE', #185852, #163770, #57856, .T. ) ;
#36736 = CIRCLE ( 'NONE', #124203, 0.09999999999998898659 ) ;
#36738 = CIRCLE ( 'NONE', #182470, 0.1000000000000028644 ) ;
#36740 = ORIENTED_EDGE ( 'NONE', *, *, #115048, .T. ) ;
#36739 = ORIENTED_EDGE ( 'NONE', *, *, #118921, .T. ) ;
#36741 = ORIENTED_EDGE ( 'NONE', *, *, #131347, .F. ) ;
#36742 = PLANE ( 'NONE',  #7652 ) ;
#36743 = ORIENTED_EDGE ( 'NONE', *, *, #198891, .F. ) ;
#36744 = ORIENTED_EDGE ( 'NONE', *, *, #25762, .T. ) ;
#36745 = ADVANCED_FACE ( 'NONE', ( #181447 ), #242676, .T. ) ;
#36746 = DIRECTION ( 'NONE',  ( 2.840903330521631775E-16, 0.8700118002898354908, -0.4930308989875170078 ) ) ;
#36747 = VERTEX_POINT ( 'NONE', #202281 ) ;
#36748 = DIRECTION ( 'NONE',  ( -4.391705002472927119E-16, -1.000000000000000000, -7.026728003956683390E-15 ) ) ;
#36750 = LINE ( 'NONE', #139639, #81656 ) ;
#36749 = CARTESIAN_POINT ( 'NONE',  ( -22.50000000000000000, 11.38316329224757872, -198.5208684056144079 ) ) ;
#36751 = EDGE_LOOP ( 'NONE', ( #230220, #108539, #187295, #63285 ) ) ;
#36752 = AXIS2_PLACEMENT_3D ( 'NONE', #76534, #175656, #96088 ) ;
#36753 = EDGE_CURVE ( 'NONE', #238847, #221268, #141029, .T. ) ;
#36754 = AXIS2_PLACEMENT_3D ( 'NONE', #53111, #59169, #113097 ) ;
#36755 = VERTEX_POINT ( 'NONE', #84854 ) ;
#36756 = DIRECTION ( 'NONE',  ( 1.000000000000000000, -1.186688945009009831E-16, -8.286604613020806758E-31 ) ) ;
#36757 = AXIS2_PLACEMENT_3D ( 'NONE', #61554, #25017, #204893 ) ;
#36758 = ADVANCED_FACE ( 'NONE', ( #159318 ), #5326, .T. ) ;
#36759 = EDGE_CURVE ( 'NONE', #1820, #64056, #53789, .T. ) ;
#36760 = EDGE_LOOP ( 'NONE', ( #90548, #136489, #125104, #158110 ) ) ;
#36761 = AXIS2_PLACEMENT_3D ( 'NONE', #243915, #64006, #105672 ) ;
#36762 = EDGE_CURVE ( 'NONE', #126637, #2822, #153798, .T. ) ;
#36763 = EDGE_LOOP ( 'NONE', ( #129007, #38564, #67896, #80029 ) ) ;
#36764 = EDGE_LOOP ( 'NONE', ( #255086, #245446, #231726, #198254 ) ) ;
#36765 = DIRECTION ( 'NONE',  ( -1.000000000000000000, 0.000000000000000000, 0.000000000000000000 ) ) ;
#36768 = EDGE_CURVE ( 'NONE', #55828, #66671, #41344, .T. ) ;
#36767 = ORIENTED_EDGE ( 'NONE', *, *, #237163, .F. ) ;
#36766 = DIRECTION ( 'NONE',  ( 0.000000000000000000, 1.000000000000000000, 6.982962677686266711E-15 ) ) ;
#36769 = DIRECTION ( 'NONE',  ( 0.000000000000000000, 0.000000000000000000, -1.000000000000000000 ) ) ;
#36770 = CARTESIAN_POINT ( 'NONE',  ( -16.94107738177414291, 30.32481141862674079, -234.7976376674202186 ) ) ;
#36771 = ORIENTED_EDGE ( 'NONE', *, *, #54896, .F. ) ;
#36772 = EDGE_CURVE ( 'NONE', #8189, #203841, #237131, .T. ) ;
#36773 = AXIS2_PLACEMENT_3D ( 'NONE', #227066, #221914, #184095 ) ;
#36774 = DIRECTION ( 'NONE',  ( 1.000000000000000000, -0.000000000000000000, 0.000000000000000000 ) ) ;
#36775 = DIRECTION ( 'NONE',  ( 0.000000000000000000, -6.982962677686266711E-15, 1.000000000000000000 ) ) ;
#36776 = DIRECTION ( 'NONE',  ( 0.000000000000000000, 0.000000000000000000, 1.000000000000000000 ) ) ;
#36777 = PLANE ( 'NONE',  #152384 ) ;
#36778 = CARTESIAN_POINT ( 'NONE',  ( -21.10000000000000142, 11.99999999999999822, 12.00000000000000000 ) ) ;
#36780 = VECTOR ( 'NONE', #3433, 1000.000000000000000 ) ;
#36779 = DIRECTION ( 'NONE',  ( 0.000000000000000000, 0.4999999999999956701, -0.8660254037844411501 ) ) ;
#36781 = AXIS2_PLACEMENT_3D ( 'NONE', #144876, #64067, #143604 ) ;
#36782 = CARTESIAN_POINT ( 'NONE',  ( -21.22070241538126112, 69.53005372714204668, -69.62202651505938888 ) ) ;
#36783 = CARTESIAN_POINT ( 'NONE',  ( 21.05000000000000071, 76.10000000001218723, -143.0637644362255401 ) ) ;
#36785 = CARTESIAN_POINT ( 'NONE',  ( 20.94999999999999929, 70.15000000001148805, -46.15560470880229360 ) ) ;
#36784 = CIRCLE ( 'NONE', #207634, 7.900000000000003908 ) ;
#36787 = ORIENTED_EDGE ( 'NONE', *, *, #171652, .T. ) ;
#36786 = VECTOR ( 'NONE', #2357, 1000.000000000000227 ) ;
#36789 = ORIENTED_EDGE ( 'NONE', *, *, #128903, .T. ) ;
#36788 = ORIENTED_EDGE ( 'NONE', *, *, #127046, .F. ) ;
#36790 = ORIENTED_EDGE ( 'NONE', *, *, #189634, .T. ) ;
#36791 = LINE ( 'NONE', #116305, #11416 ) ;
#36792 = DIRECTION ( 'NONE',  ( 1.000000000000000000, 0.000000000000000000, 0.000000000000000000 ) ) ;
#36794 = CARTESIAN_POINT ( 'NONE',  ( 22.59999999999999787, 11.64957080755595520, -66.90000000000004832 ) ) ;
#36793 = LINE ( 'NONE', #51147, #74321 ) ;
#36795 = ORIENTED_EDGE ( 'NONE', *, *, #256305, .F. ) ;
#36796 = CONICAL_SURFACE ( 'NONE', #232415, 4.049999999999998046, 0.7853981633974604915 ) ;
#36797 = DIRECTION ( 'NONE',  ( 0.000000000000000000, 0.000000000000000000, -1.000000000000000000 ) ) ;
#36798 =( NAMED_UNIT ( * ) SI_UNIT ( $, .STERADIAN. ) SOLID_ANGLE_UNIT ( ) );
#36799 = DIRECTION ( 'NONE',  ( -1.000000000000000000, -0.000000000000000000, -0.000000000000000000 ) ) ;
#36800 = CARTESIAN_POINT ( 'NONE',  ( 18.59999999999999432, 77.16270174994961906, -61.42310748452431568 ) ) ;
#36801 = DIRECTION ( 'NONE',  ( -1.000000000000000000, 0.000000000000000000, -0.000000000000000000 ) ) ;
#36802 = ORIENTED_EDGE ( 'NONE', *, *, #67398, .T. ) ;
#36803 = ORIENTED_EDGE ( 'NONE', *, *, #174791, .T. ) ;
#36804 = AXIS2_PLACEMENT_3D ( 'NONE', #76988, #156570, #217764 ) ;
#36805 = DIRECTION ( 'NONE',  ( 0.000000000000000000, -1.000000000000000000, -6.982962677686265922E-15 ) ) ;
#36806 = ORIENTED_EDGE ( 'NONE', *, *, #157447, .F. ) ;
#36807 = FACE_OUTER_BOUND ( 'NONE', #171134, .T. ) ;
#36808 = CARTESIAN_POINT ( 'NONE',  ( -20.85000000000000142, 68.97833521811159585, -65.68954208262705663 ) ) ;
#36809 = DIRECTION ( 'NONE',  ( 1.000000000000000000, 0.000000000000000000, -0.000000000000000000 ) ) ;
#36810 = DIRECTION ( 'NONE',  ( -1.000000000000000000, 0.000000000000000000, 0.000000000000000000 ) ) ;
#36811 = LINE ( 'NONE', #53767, #120929 ) ;
#36812 = ORIENTED_EDGE ( 'NONE', *, *, #56155, .F. ) ;
#36813 = LINE ( 'NONE', #98004, #186161 ) ;
#36814 = CARTESIAN_POINT ( 'NONE',  ( 18.59999999999999076, 62.96704557978079464, -212.5773704035085814 ) ) ;
#36815 = DIRECTION ( 'NONE',  ( 0.000000000000000000, 0.000000000000000000, 1.000000000000000000 ) ) ;
#36816 = EDGE_CURVE ( 'NONE', #135854, #35027, #249789, .T. ) ;
#36818 = DIRECTION ( 'NONE',  ( 0.000000000000000000, 0.000000000000000000, 1.000000000000000000 ) ) ;
#36817 = DIRECTION ( 'NONE',  ( 1.000000000000000000, 0.000000000000000000, 0.000000000000000000 ) ) ;
#36819 = CARTESIAN_POINT ( 'NONE',  ( -23.25000000000000000, 0.000000000000000000, -33.50000000000000000 ) ) ;
#36820 = CARTESIAN_POINT ( 'NONE',  ( -16.94333152882355975, 9.990342011468824168, -121.3920315311015230 ) ) ;
#36821 = AXIS2_PLACEMENT_3D ( 'NONE', #168408, #10577, #167106 ) ;
#36822 = VECTOR ( 'NONE', #202318, 1000.000000000000114 ) ;
#36823 = AXIS2_PLACEMENT_3D ( 'NONE', #178158, #36068, #97266 ) ;
#36825 = EDGE_CURVE ( 'NONE', #201070, #19723, #7940, .T. ) ;
#36824 = DIRECTION ( 'NONE',  ( 0.000000000000000000, 0.000000000000000000, -1.000000000000000000 ) ) ;
#36826 = CARTESIAN_POINT ( 'NONE',  ( 22.42196299218230493, 75.99755832602473049, -114.6727191871737830 ) ) ;
#36827 = CIRCLE ( 'NONE', #99301, 0.6000000000000015321 ) ;
#36828 = ORIENTED_EDGE ( 'NONE', *, *, #173338, .T. ) ;
#36829 = ORIENTED_EDGE ( 'NONE', *, *, #32150, .F. ) ;
#36830 = ADVANCED_FACE ( 'NONE', ( #226976 ), #127882, .F. ) ;
#36831 = DIRECTION ( 'NONE',  ( 0.000000000000000000, 0.9908441862701600211, -0.1350103645451876666 ) ) ;
#36832 = EDGE_CURVE ( 'NONE', #147377, #230733, #48333, .T. ) ;
#36833 = EDGE_LOOP ( 'NONE', ( #165947, #167010, #165513, #135955 ) ) ;
#36834 = LINE ( 'NONE', #257072, #159402 ) ;
#36835 = PRESENTATION_STYLE_ASSIGNMENT (( #155500 ) ) ;
#36836 = CIRCLE ( 'NONE', #182566, 0.1000000000000002554 ) ;
#36837 = DIRECTION ( 'NONE',  ( 0.000000000000000000, 6.982962677686266711E-15, -1.000000000000000000 ) ) ;
#36838 = ORIENTED_EDGE ( 'NONE', *, *, #36768, .F. ) ;
#36839 =( BOUNDED_CURVE ( )  B_SPLINE_CURVE ( 3, ( #86970, #165256, #106541, #149569 ),
 .UNSPECIFIED., .F., .T. ) 
 B_SPLINE_CURVE_WITH_KNOTS ( ( 4, 4 ),
 ( 5.733388419619901200, 5.983100554402347449 ),
 .UNSPECIFIED. ) 
 CURVE ( )  GEOMETRIC_REPRESENTATION_ITEM ( )  RATIONAL_B_SPLINE_CURVE ( ( 1.000000000000000000, 0.9948104011409417691, 0.9948104011409417691, 1.000000000000000000 ) ) 
 REPRESENTATION_ITEM ( '' )  );
#36840 = DIRECTION ( 'NONE',  ( 0.000000000000000000, 0.000000000000000000, -1.000000000000000000 ) ) ;
#36841 = ADVANCED_FACE ( 'NONE', ( #187870 ), #110880, .T. ) ;
#36842 = CARTESIAN_POINT ( 'NONE',  ( -12.60829076262179527, 9.389529397477895500, -51.31710791289368956 ) ) ;
#36843 = CARTESIAN_POINT ( 'NONE',  ( 23.14999999999999503, 64.35000000001228670, -157.8731074845244393 ) ) ;
#36844 = DIRECTION ( 'NONE',  ( 0.000000000000000000, -6.789366196018718420E-15, 1.000000000000000000 ) ) ;
#36846 = ORIENTED_EDGE ( 'NONE', *, *, #204520, .F. ) ;
#36845 = CARTESIAN_POINT ( 'NONE',  ( -18.50000000000000000, 9.350000000011156942, -45.65000000000000568 ) ) ;
#36848 = CARTESIAN_POINT ( 'NONE',  ( 20.00000000000000355, 11.75000000001116263, -192.1499999999999488 ) ) ;
#36847 = CARTESIAN_POINT ( 'NONE',  ( 18.50000000000000000, 38.28679861725831302, -261.0868692510649680 ) ) ;
#36849 = DIRECTION ( 'NONE',  ( 1.000000000000000000, 3.265361837132813093E-16, -0.000000000000000000 ) ) ;
#36850 = CARTESIAN_POINT ( 'NONE',  ( 20.94999999999999929, 64.35000000001195986, -109.8069731475024753 ) ) ;
#36851 = CARTESIAN_POINT ( 'NONE',  ( 18.59999999999999432, 86.96699927712941758, -199.3055931863049182 ) ) ;
#36852 = DIRECTION ( 'NONE',  ( 1.000000000000000000, 0.000000000000000000, 0.000000000000000000 ) ) ;
#36853 = ORIENTED_EDGE ( 'NONE', *, *, #146853, .F. ) ;
#36854 = DIRECTION ( 'NONE',  ( 1.000000000000000000, 0.000000000000000000, 0.000000000000000000 ) ) ;
#36855 = CYLINDRICAL_SURFACE ( 'NONE', #87637, 0.09999999999999939493 ) ;
#36856 = ADVANCED_FACE ( 'NONE', ( #69212 ), #168335, .T. ) ;
#36857 = ORIENTED_EDGE ( 'NONE', *, *, #252022, .F. ) ;
#36858 = AXIS2_PLACEMENT_3D ( 'NONE', #239484, #41305, #120845 ) ;
#36859 = DIRECTION ( 'NONE',  ( 0.000000000000000000, 7.116814260417676401E-15, -1.000000000000000000 ) ) ;
#36860 = EDGE_CURVE ( 'NONE', #166025, #49789, #66622, .T. ) ;
#36861 = EDGE_LOOP ( 'NONE', ( #43131, #159615, #112666, #154852 ) ) ;
#36862 = TOROIDAL_SURFACE ( 'NONE', #24370, 11.65000000000000036, 0.1000000000000000056 ) ;
#36863 = TOROIDAL_SURFACE ( 'NONE', #144960, 3.899999999999999467, 0.1000000000000000056 ) ;
#36864 = CARTESIAN_POINT ( 'NONE',  ( 18.49999999999999289, 54.98105481382776816, -230.1569079895687366 ) ) ;
#36865 = DIRECTION ( 'NONE',  ( 0.000000000000000000, 0.000000000000000000, -1.000000000000000000 ) ) ;
#36866 = LINE ( 'NONE', #21147, #32836 ) ;
#36867 = ORIENTED_EDGE ( 'NONE', *, *, #200392, .T. ) ;
#36868 = AXIS2_PLACEMENT_3D ( 'NONE', #103229, #27604, #184066 ) ;
#36869 = ORIENTED_EDGE ( 'NONE', *, *, #214868, .T. ) ;
#36870 = ADVANCED_FACE ( 'NONE', ( #126592 ), #67900, .T. ) ;
#36871 = EDGE_CURVE ( 'NONE', #50484, #80866, #191378, .T. ) ;
#36872 = DIRECTION ( 'NONE',  ( 0.000000000000000000, -0.2617529984165031243, -0.9651348961777157509 ) ) ;
#36873 = CARTESIAN_POINT ( 'NONE',  ( 20.94999999999999929, 74.63912941282003999, -128.4501095574333647 ) ) ;
#36874 = LINE ( 'NONE', #177664, #240976 ) ;
#36875 = CARTESIAN_POINT ( 'NONE',  ( 18.59999999999999076, 65.75000000001222134, -145.2731074845244450 ) ) ;
#36877 = DIRECTION ( 'NONE',  ( -0.000000000000000000, -0.6132151058540604716, 0.7899159663865477077 ) ) ;
#36876 = FACE_OUTER_BOUND ( 'NONE', #257694, .T. ) ;
#36878 = EDGE_CURVE ( 'NONE', #225002, #401, #87272, .T. ) ;
#36879 = CIRCLE ( 'NONE', #182605, 0.09999999999999939493 ) ;
#36881 = CARTESIAN_POINT ( 'NONE',  ( -23.15000000000000213, -11.41227409413852811, -197.9999999999999432 ) ) ;
#36880 = AXIS2_PLACEMENT_3D ( 'NONE', #250678, #108608, #146429 ) ;
#36882 = CARTESIAN_POINT ( 'NONE',  ( 20.97468175916167255, 65.37473483564083665, -90.76834604911159943 ) ) ;
#36883 = DIRECTION ( 'NONE',  ( 0.000000000000000000, 0.8814952561688476074, -0.4721928772777262417 ) ) ;
#36884 = TOROIDAL_SURFACE ( 'NONE', #182608, 0.2000000000000000111, 0.1000000000000000056 ) ;
#36885 = ORIENTED_EDGE ( 'NONE', *, *, #102121, .F. ) ;
#36886 = DIRECTION ( 'NONE',  ( 0.000000000000000000, -1.000000000000000000, -6.982962677686265922E-15 ) ) ;
#36888 = VERTEX_POINT ( 'NONE', #167038 ) ;
#36887 = CARTESIAN_POINT ( 'NONE',  ( -23.25000000000000000, 87.65000000001192859, -106.1231074845242262 ) ) ;
#36889 = AXIS2_PLACEMENT_3D ( 'NONE', #102898, #200744, #179914 ) ;
#36890 = CARTESIAN_POINT ( 'NONE',  ( 18.59999999999999076, 69.60000000001157616, -59.59268285446279378 ) ) ;
#36892 = DIRECTION ( 'NONE',  ( 0.000000000000000000, 0.000000000000000000, -1.000000000000000000 ) ) ;
#36891 = FACE_OUTER_BOUND ( 'NONE', #148241, .T. ) ;
#36893 = ORIENTED_EDGE ( 'NONE', *, *, #59158, .T. ) ;
#36895 = PLANE ( 'NONE',  #84153 ) ;
#36894 = DIRECTION ( 'NONE',  ( 1.000000000000000000, 0.000000000000000000, -0.000000000000000000 ) ) ;
#36896 = LINE ( 'NONE', #61561, #16560 ) ;
#36897 = ADVANCED_FACE ( 'NONE', ( #10509 ), #213965, .T. ) ;
#36898 = CARTESIAN_POINT ( 'NONE',  ( 20.95512820512820440, 12.96604748760834092, -210.6109454999921411 ) ) ;
#36899 = CARTESIAN_POINT ( 'NONE',  ( 21.14999999999999858, -3.187427350888460076, -228.3200064793908837 ) ) ;
#36901 = DIRECTION ( 'NONE',  ( 0.000000000000000000, -1.000000000000000000, 0.000000000000000000 ) ) ;
#36900 = SHAPE_REPRESENTATION ( 'MAS-200', ( #36315, #206984, #36132, #111123, #194368, #94538, #81859, #115215, #44510, #52846, #131965, #169433, #144408, #181865, #161022, #177785, #69450, #244390, #236027, #206804, #11171, #215183, #94356, #227636, #127708, #190248, #23681, #19562, #15288, #2781, #165285, #123598, #148554, #156939 ), #77788 ) ;
#36902 = ORIENTED_EDGE ( 'NONE', *, *, #145426, .F. ) ;
#36903 = DIRECTION ( 'NONE',  ( 0.000000000000000000, -0.9770955615653316162, -0.2128009952263604232 ) ) ;
#36904 = AXIS2_PLACEMENT_3D ( 'NONE', #32724, #190498, #131777 ) ;
#36905 = ORIENTED_EDGE ( 'NONE', *, *, #206076, .T. ) ;
#36906 = EDGE_CURVE ( 'NONE', #115616, #126399, #216464, .T. ) ;
#36907 = FACE_OUTER_BOUND ( 'NONE', #128744, .T. ) ;
#36908 = VECTOR ( 'NONE', #59957, 1000.000000000000114 ) ;
#36909 = ORIENTED_EDGE ( 'NONE', *, *, #234368, .F. ) ;
#36910 = VERTEX_POINT ( 'NONE', #14377 ) ;
#36911 = CIRCLE ( 'NONE', #144996, 0.1000000000000016709 ) ;
#36912 = CARTESIAN_POINT ( 'NONE',  ( -14.00000000000000178, 47.91805600923872532, -233.7139610577891631 ) ) ;
#36914 = CYLINDRICAL_SURFACE ( 'NONE', #83408, 0.09999999999999520384 ) ;
#36913 = AXIS2_PLACEMENT_3D ( 'NONE', #101917, #116389, #195936 ) ;
#36915 = VECTOR ( 'NONE', #242633, 1000.000000000000114 ) ;
#36916 = AXIS2_PLACEMENT_3D ( 'NONE', #138362, #39311, #215347 ) ;
#36917 = PLANE ( 'NONE',  #143018 ) ;
#36918 = ORIENTED_EDGE ( 'NONE', *, *, #85312, .T. ) ;
#36919 = CIRCLE ( 'NONE', #203654, 0.1000000000000028644 ) ;
#36920 = CARTESIAN_POINT ( 'NONE',  ( -21.07928932188134041, -1.250084634896336366, -194.7953894783290423 ) ) ;
#36921 = DIRECTION ( 'NONE',  ( 0.000000000000000000, 0.2128009952263603677, -0.9770955615653313941 ) ) ;
#36922 = DIRECTION ( 'NONE',  ( 0.000000000000000000, 0.000000000000000000, 1.000000000000000000 ) ) ;
#36923 = CARTESIAN_POINT ( 'NONE',  ( -23.25000000000000000, 11.65000000001115588, -122.2500000000000284 ) ) ;
#36924 = CARTESIAN_POINT ( 'NONE',  ( 20.02499999999999858, 9.750000000011153745, -188.7499999999999716 ) ) ;
#36925 = ORIENTED_EDGE ( 'NONE', *, *, #67027, .T. ) ;
#36927 = AXIS2_PLACEMENT_3D ( 'NONE', #42748, #122291, #44035 ) ;
#36926 = FACE_OUTER_BOUND ( 'NONE', #84054, .T. ) ;
#36928 = AXIS2_PLACEMENT_3D ( 'NONE', #216741, #194653, #219310 ) ;
#36929 = ORIENTED_EDGE ( 'NONE', *, *, #199095, .F. ) ;
#36931 = ORIENTED_EDGE ( 'NONE', *, *, #51942, .F. ) ;
#36930 = CARTESIAN_POINT ( 'NONE',  ( -1.820710678118658388, 85.92928932189384739, -178.8731074845242972 ) ) ;
#36932 = EDGE_LOOP ( 'NONE', ( #93789, #47347, #107617, #40775 ) ) ;
#36933 = CARTESIAN_POINT ( 'NONE',  ( 21.15000000000005187, 83.90000000001120384, -34.77310748452479316 ) ) ;
#36934 = CLOSED_SHELL ( 'NONE', ( #79948, #107676, #41369, #217398, #152620, #219378, #112841, #59185, #38821, #255864, #122761, #168584, #33836, #233655, #46341, #61137, #115523, #226844, #226917, #103127, #86989, #71687, #91185, #122129, #41386, #131259, #10330, #55106, #1766, #68910, #90326, #119124, #178924, #151361, #213782, #118985, #24371, #92409, #227987, #129657, #192615, #110201, #156343, #142198, #59309, #217145, #221575, #64756, #204344, #148407, #253722, #97249, #196693 ) ) ;
#36935 = DIRECTION ( 'NONE',  ( 0.7071067811865475727, -0.7071067811865475727, -4.937700262164531476E-15 ) ) ;
#36937 = DIRECTION ( 'NONE',  ( 0.000000000000000000, 0.000000000000000000, -1.000000000000000000 ) ) ;
#36936 = B_SPLINE_CURVE_WITH_KNOTS ( 'NONE', 3,
 ( #128324, #85298, #24102, #184425, #147885, #227404 ),
 .UNSPECIFIED., .F., .F.,
 ( 4, 2, 4 ),
 ( 0.000000000000000000, 0.0002113392456165965911, 0.0004226784912331931821 ),
 .UNSPECIFIED. ) ;
#36938 = CARTESIAN_POINT ( 'NONE',  ( 23.14999999999999858, 76.00000000001190870, -103.0231074845243029 ) ) ;
#36939 = ORIENTED_EDGE ( 'NONE', *, *, #69746, .T. ) ;
#36940 = DIRECTION ( 'NONE',  ( 0.000000000000000000, -0.9770955615653301729, -0.2128009952263661964 ) ) ;
#36941 = DIRECTION ( 'NONE',  ( 1.000000000000000000, 0.000000000000000000, 0.000000000000000000 ) ) ;
#36942 = EDGE_LOOP ( 'NONE', ( #91248, #150473, #213588, #98109, #171404 ) ) ;
#36943 = AXIS2_PLACEMENT_3D ( 'NONE', #117912, #240445, #158378 ) ;
#36945 = VERTEX_POINT ( 'NONE', #95166 ) ;
#36944 = CARTESIAN_POINT ( 'NONE',  ( -16.89797118371550511, 66.02361927736761515, -115.5858141169661621 ) ) ;
#36946 = AXIS2_PLACEMENT_3D ( 'NONE', #202139, #23539, #103017 ) ;
#36947 = DIRECTION ( 'NONE',  ( 0.000000000000000000, 0.2128009952263403282, -0.9770955615653358350 ) ) ;
#36948 = VECTOR ( 'NONE', #89777, 1000.000000000000000 ) ;
#36949 = CARTESIAN_POINT ( 'NONE',  ( -16.82055514392378726, 9.950000000011137047, -79.67679807454184981 ) ) ;
#36950 = ORIENTED_EDGE ( 'NONE', *, *, #168436, .F. ) ;
#36951 = AXIS2_PLACEMENT_3D ( 'NONE', #244563, #28121, #145461 ) ;
#36952 = CARTESIAN_POINT ( 'NONE',  ( -2.995603634470829482E-16, 6.650000000011155876, -155.2500000000000284 ) ) ;
#36953 = ORIENTED_EDGE ( 'NONE', *, *, #173646, .F. ) ;
#36954 = FACE_OUTER_BOUND ( 'NONE', #34930, .T. ) ;
#36955 = EDGE_CURVE ( 'NONE', #174669, #253265, #241426, .T. ) ;
#36956 = CARTESIAN_POINT ( 'NONE',  ( 14.88075390448864610, 66.56831044948744136, -51.24381745228834006 ) ) ;
#36957 = VECTOR ( 'NONE', #182699, 1000.000000000000000 ) ;
#36958 = CARTESIAN_POINT ( 'NONE',  ( 23.14999999999999858, 55.39363411790989034, -234.6384634766556303 ) ) ;
#36959 = ADVANCED_FACE ( 'NONE', ( #133023 ), #256752, .F. ) ;
#36961 = EDGE_CURVE ( 'NONE', #158817, #215723, #74851, .T. ) ;
#36960 = AXIS2_PLACEMENT_3D ( 'NONE', #3118, #241746, #80066 ) ;
#36962 = CIRCLE ( 'NONE', #53669, 0.09999999999999789613 ) ;
#36963 = CIRCLE ( 'NONE', #215959, 0.09999999999999939493 ) ;
#36964 = ORIENTED_EDGE ( 'NONE', *, *, #162028, .T. ) ;
#36965 = PLANE ( 'NONE',  #194570 ) ;
#36966 = ORIENTED_EDGE ( 'NONE', *, *, #96761, .T. ) ;
#36967 = DIRECTION ( 'NONE',  ( -1.000000000000000000, -0.000000000000000000, -0.000000000000000000 ) ) ;
#36968 = EDGE_CURVE ( 'NONE', #232210, #63287, #208115, .T. ) ;
#36969 = CARTESIAN_POINT ( 'NONE',  ( 21.13736287352038445, 64.92272921553191622, -213.6258311519692086 ) ) ;
#36971 = EDGE_LOOP ( 'NONE', ( #150936, #175204, #173672 ) ) ;
#36970 = CARTESIAN_POINT ( 'NONE',  ( -17.11825945287482753, 44.18585876254595490, -235.1667871698132046 ) ) ;
#36972 = DIRECTION ( 'NONE',  ( 1.000000000000000000, 0.000000000000000000, 0.000000000000000000 ) ) ;
#36973 = DIRECTION ( 'NONE',  ( 1.000000000000000000, 0.000000000000000000, 0.000000000000000000 ) ) ;
#36974 = CARTESIAN_POINT ( 'NONE',  ( 21.05000000000000071, 6.304516329275108077, -33.52110330805914629 ) ) ;
#36975 = VECTOR ( 'NONE', #209769, 1000.000000000000000 ) ;
#36976 = PLANE ( 'NONE',  #1628 ) ;
#36977 = CARTESIAN_POINT ( 'NONE',  ( 23.14999999999999858, 28.36802138732021206, -238.7571110118315971 ) ) ;
#36979 = ORIENTED_EDGE ( 'NONE', *, *, #87933, .F. ) ;
#36978 = CARTESIAN_POINT ( 'NONE',  ( -18.59999999999999787, 11.75000000001115197, -21.75000000000000355 ) ) ;
#36980 = FACE_OUTER_BOUND ( 'NONE', #97330, .T. ) ;
#36981 = EDGE_CURVE ( 'NONE', #154130, #61931, #158080, .T. ) ;
#36982 = EDGE_CURVE ( 'NONE', #181665, #176716, #224646, .T. ) ;
#36983 = DIRECTION ( 'NONE',  ( 0.000000000000000000, 0.000000000000000000, -1.000000000000000000 ) ) ;
#36984 = CARTESIAN_POINT ( 'NONE',  ( -21.64999999999999858, 10.05000000001113847, -54.35000000000000142 ) ) ;
#36985 = EDGE_LOOP ( 'NONE', ( #107971, #24693, #17297, #55050 ) ) ;
#36987 = EDGE_CURVE ( 'NONE', #138354, #110167, #166434, .T. ) ;
#36986 = DIRECTION ( 'NONE',  ( 0.000000000000000000, 6.938893903907030216E-14, -1.000000000000000000 ) ) ;
#36988 = AXIS2_PLACEMENT_3D ( 'NONE', #78228, #161655, #62533 ) ;
#36989 = CIRCLE ( 'NONE', #128546, 0.09999999999998898659 ) ;
#36990 = ORIENTED_EDGE ( 'NONE', *, *, #106225, .T. ) ;
#36991 = AXIS2_PLACEMENT_3D ( 'NONE', #237612, #58931, #159368 ) ;
#36992 = LINE ( 'NONE', #117779, #18885 ) ;
#36993 = DIRECTION ( 'NONE',  ( 0.000000000000000000, 0.2741185865636956431, 0.9616958981405304696 ) ) ;
#36994 = ORIENTED_EDGE ( 'NONE', *, *, #173324, .T. ) ;
#36995 = DIRECTION ( 'NONE',  ( 0.000000000000000000, 0.000000000000000000, -1.000000000000000000 ) ) ;
#36996 = ORIENTED_EDGE ( 'NONE', *, *, #53096, .F. ) ;
#36997 = CARTESIAN_POINT ( 'NONE',  ( -20.64999999999999858, -8.999999999988844479, -191.1060308773475356 ) ) ;
#36999 = VERTEX_POINT ( 'NONE', #73079 ) ;
#36998 = CARTESIAN_POINT ( 'NONE',  ( 21.07954763557436806, 6.329290990048848542, -133.9341240813815546 ) ) ;
#37000 = CARTESIAN_POINT ( 'NONE',  ( 20.99999999999997868, 1.115600667400684642E-11, -33.50000000000000000 ) ) ;
#37001 = ORIENTED_EDGE ( 'NONE', *, *, #73680, .F. ) ;
#37002 = DIRECTION ( 'NONE',  ( -1.000000000000000000, 0.000000000000000000, 0.000000000000000000 ) ) ;
#37003 = VECTOR ( 'NONE', #210501, 1000.000000000000227 ) ;
#37004 = AXIS2_PLACEMENT_3D ( 'NONE', #207401, #9180, #28795 ) ;
#37005 = ORIENTED_EDGE ( 'NONE', *, *, #142107, .F. ) ;
#37007 = ORIENTED_EDGE ( 'NONE', *, *, #77146, .F. ) ;
#37006 = ORIENTED_EDGE ( 'NONE', *, *, #24137, .T. ) ;
#37009 = FACE_OUTER_BOUND ( 'NONE', #237681, .T. ) ;
#37008 = AXIS2_PLACEMENT_3D ( 'NONE', #21848, #57088, #156249 ) ;
#37010 = VERTEX_POINT ( 'NONE', #235949 ) ;
#37011 = DIRECTION ( 'NONE',  ( 0.000000000000000000, -1.000000000000000000, -8.717686153663073805E-15 ) ) ;
#37012 = EDGE_LOOP ( 'NONE', ( #167976, #39300, #21523, #102465 ) ) ;
#37013 = AXIS2_PLACEMENT_3D ( 'NONE', #222392, #161179, #144153 ) ;
#37014 = ADVANCED_FACE ( 'NONE', ( #112185 ), #54747, .T. ) ;
#37015 = ADVANCED_FACE ( 'NONE', ( #213830 ), #196824, .T. ) ;
#37016 = ORIENTED_EDGE ( 'NONE', *, *, #17070, .T. ) ;
#37017 = CYLINDRICAL_SURFACE ( 'NONE', #195348, 12.87499999999999822 ) ;
#37018 = CARTESIAN_POINT ( 'NONE',  ( -23.15000000000000213, 4.150000000011156764, -55.25000000000004974 ) ) ;
#37019 = DIRECTION ( 'NONE',  ( 0.000000000000000000, 0.1568667991644355497, 0.9876197685951332295 ) ) ;
#37020 = ORIENTED_EDGE ( 'NONE', *, *, #215104, .F. ) ;
#37021 = EDGE_CURVE ( 'NONE', #9718, #80932, #245517, .T. ) ;
#37022 = ADVANCED_FACE ( 'NONE', ( #174752 ), #75629, .F. ) ;
#37023 = CARTESIAN_POINT ( 'NONE',  ( -18.54159361262942696, -9.463132135481979290, -74.04912221629291480 ) ) ;
#37024 = DIRECTION ( 'NONE',  ( -1.000000000000000000, -7.304098846218134667E-16, 0.000000000000000000 ) ) ;
#37025 = ORIENTED_EDGE ( 'NONE', *, *, #38621, .T. ) ;
#37026 = CARTESIAN_POINT ( 'NONE',  ( -20.94999999999999929, 79.13126459505528487, -235.8705213229730191 ) ) ;
#37027 = CARTESIAN_POINT ( 'NONE',  ( -18.50000000000000000, 38.28679861725832012, -261.0868692510649680 ) ) ;
#37028 = CARTESIAN_POINT ( 'NONE',  ( 21.05000000000000426, 65.27628289530457550, -128.9286900929112392 ) ) ;
#37029 = ORIENTED_EDGE ( 'NONE', *, *, #78697, .T. ) ;
#37030 = CARTESIAN_POINT ( 'NONE',  ( -17.11825945287482043, 14.15900158805610509, -219.2550725561364402 ) ) ;
#37031 = ORIENTED_EDGE ( 'NONE', *, *, #241781, .F. ) ;
#37032 = VECTOR ( 'NONE', #126169, 1000.000000000000000 ) ;
#37033 = ORIENTED_EDGE ( 'NONE', *, *, #145546, .F. ) ;
#37034 = VECTOR ( 'NONE', #111599, 1000.000000000000000 ) ;
#37035 = EDGE_CURVE ( 'NONE', #45747, #181045, #255470, .T. ) ;
#37037 = EDGE_CURVE ( 'NONE', #167394, #50141, #57299, .T. ) ;
#37036 = EDGE_CURVE ( 'NONE', #611, #203688, #56007, .T. ) ;
#37038 = CARTESIAN_POINT ( 'NONE',  ( 20.94999999999999929, 11.65000000001115943, -127.2161343370219413 ) ) ;
#37039 = ORIENTED_EDGE ( 'NONE', *, *, #135755, .T. ) ;
#37040 = ORIENTED_EDGE ( 'NONE', *, *, #64935, .F. ) ;
#37041 = DIRECTION ( 'NONE',  ( -1.000000000000000000, -3.265361837132813093E-16, 0.000000000000000000 ) ) ;
#37042 = CARTESIAN_POINT ( 'NONE',  ( -20.85000000000000142, 1.115600667400684642E-11, -134.0000000000000284 ) ) ;
#37043 = EDGE_LOOP ( 'NONE', ( #221408, #47836, #33378, #68936, #72954, #24554, #15517 ) ) ;
#37044 = AXIS2_PLACEMENT_3D ( 'NONE', #49238, #68823, #225286 ) ;
#37045 = ADVANCED_FACE ( 'NONE', ( #58586 ), #4081, .T. ) ;
#37046 = VERTEX_POINT ( 'NONE', #92583 ) ;
#37047 = DIRECTION ( 'NONE',  ( 1.000000000000000000, 0.000000000000000000, -0.000000000000000000 ) ) ;
#37048 = CARTESIAN_POINT ( 'NONE',  ( 20.94999999999999929, 71.00000000001199396, -115.4283735034374274 ) ) ;
#37049 = ORIENTED_EDGE ( 'NONE', *, *, #246193, .F. ) ;
#37050 = ADVANCED_FACE ( 'NONE', ( #239826 ), #102840, .T. ) ;
#37051 = VERTEX_POINT ( 'NONE', #23366 ) ;
#37052 = AXIS2_PLACEMENT_3D ( 'NONE', #63266, #45000, #123250 ) ;
#37053 = AXIS2_PLACEMENT_3D ( 'NONE', #212562, #75628, #54746 ) ;
#37054 = ADVANCED_FACE ( 'NONE', ( #100274 ), #203805, .T. ) ;
#37055 = EDGE_CURVE ( 'NONE', #58001, #151185, #53960, .T. ) ;
#37057 = ORIENTED_EDGE ( 'NONE', *, *, #219186, .T. ) ;
#37056 = AXIS2_PLACEMENT_3D ( 'NONE', #121329, #125150, #200830 ) ;
#37059 = LINE ( 'NONE', #182656, #143278 ) ;
#37058 = AXIS2_PLACEMENT_3D ( 'NONE', #219010, #134328, #178644 ) ;
#37060 = EDGE_CURVE ( 'NONE', #8664, #257983, #199745, .T. ) ;
#37061 = DIRECTION ( 'NONE',  ( -1.000000000000000000, -0.000000000000000000, -0.000000000000000000 ) ) ;
#37062 = LINE ( 'NONE', #196113, #55170 ) ;
#37063 = SPHERICAL_SURFACE ( 'NONE', #76653, 0.1000000000000000056 ) ;
#37064 = EDGE_CURVE ( 'NONE', #163189, #146973, #120633, .T. ) ;
#37065 = TOROIDAL_SURFACE ( 'NONE', #241068, 11.90000000000000391, 0.1000000000000000056 ) ;
#37067 = AXIS2_PLACEMENT_3D ( 'NONE', #166784, #165478, #188882 ) ;
#37066 = CARTESIAN_POINT ( 'NONE',  ( 23.25000000000000000, 86.27712145182582049, -209.5223386573213702 ) ) ;
#37068 = CARTESIAN_POINT ( 'NONE',  ( -20.94999999999999929, -10.58757034444203704, -206.3761839813444396 ) ) ;
#37069 = LINE ( 'NONE', #236511, #240137 ) ;
#37070 = DIRECTION ( 'NONE',  ( 0.000000000000000000, 0.000000000000000000, -1.000000000000000000 ) ) ;
#37072 = EDGE_CURVE ( 'NONE', #31770, #221017, #8193, .T. ) ;
#37071 = CARTESIAN_POINT ( 'NONE',  ( 23.14999999999999147, 1.115600667400684642E-11, -67.00000000000004263 ) ) ;
#37073 = CIRCLE ( 'NONE', #232693, 0.09999999999999939493 ) ;
#37074 = CARTESIAN_POINT ( 'NONE',  ( 23.14999999999999858, 36.65892442174935439, -249.5511627012433848 ) ) ;
#37075 = DIRECTION ( 'NONE',  ( -1.000000000000000000, 0.000000000000000000, 0.000000000000000000 ) ) ;
#37076 = VERTEX_POINT ( 'NONE', #20784 ) ;
#37077 = CIRCLE ( 'NONE', #91034, 0.1000000000000013933 ) ;
#37078 = AXIS2_PLACEMENT_3D ( 'NONE', #62521, #221562, #45520 ) ;
#37079 = AXIS2_PLACEMENT_3D ( 'NONE', #191698, #235906, #15622 ) ;
#37080 = AXIS2_PLACEMENT_3D ( 'NONE', #99239, #237492, #217898 ) ;
#37082 = ORIENTED_EDGE ( 'NONE', *, *, #122782, .T. ) ;
#37081 = DIRECTION ( 'NONE',  ( -1.000000000000000000, -0.000000000000000000, -0.000000000000000000 ) ) ;
#37083 = ADVANCED_FACE ( 'NONE', ( #178587 ), #42902, .F. ) ;
#37084 = AXIS2_PLACEMENT_3D ( 'NONE', #66875, #108571, #51133 ) ;
#37085 = DIRECTION ( 'NONE',  ( 0.000000000000000000, -6.982962677686266711E-15, 1.000000000000000000 ) ) ;
#37086 = DIRECTION ( 'NONE',  ( 0.000000000000000000, 0.000000000000000000, 1.000000000000000000 ) ) ;
#37087 = VERTEX_POINT ( 'NONE', #63738 ) ;
#37088 = DIRECTION ( 'NONE',  ( 0.000000000000000000, -1.000000000000000000, -6.982962677686265922E-15 ) ) ;
#37089 = PRODUCT_DEFINITION_SHAPE ( 'NONE', 'NONE',  #258116 ) ;
#37090 = DIRECTION ( 'NONE',  ( 0.000000000000000000, -0.9910827722268049644, 0.1332476588733589318 ) ) ;
#37091 = TOROIDAL_SURFACE ( 'NONE', #186940, 0.2000000000000000111, 0.1000000000000000056 ) ;
#37092 = EDGE_LOOP ( 'NONE', ( #28954, #181901, #214703, #29041 ) ) ;
#37093 = CARTESIAN_POINT ( 'NONE',  ( 23.24999999999999645, 1.115600667400684642E-11, -167.4999999999999716 ) ) ;
#37094 = DIRECTION ( 'NONE',  ( 0.000000000000000000, 0.000000000000000000, 1.000000000000000000 ) ) ;
#37095 = CARTESIAN_POINT ( 'NONE',  ( -18.59999999999999787, 0.000000000000000000, -33.50000000000000000 ) ) ;
#37097 = ORIENTED_EDGE ( 'NONE', *, *, #71042, .F. ) ;
#37096 = DIRECTION ( 'NONE',  ( -0.000000000000000000, 0.1350103645451945777, -0.9908441862701590219 ) ) ;
#37099 = ORIENTED_EDGE ( 'NONE', *, *, #170997, .T. ) ;
#37098 = CARTESIAN_POINT ( 'NONE',  ( -21.07928932188134041, 75.90110485435759813, -109.3516241409176075 ) ) ;
#37100 = AXIS2_PLACEMENT_3D ( 'NONE', #35241, #95177, #174765 ) ;
#37101 = DIRECTION ( 'NONE',  ( 3.616040088954497272E-32, -1.224646799147352961E-16, 1.000000000000000000 ) ) ;
#37102 = CYLINDRICAL_SURFACE ( 'NONE', #108257, 0.09999999999999939493 ) ;
#37103 = DIRECTION ( 'NONE',  ( 0.000000000000000000, -0.4930308989875575865, -0.8700118002898125091 ) ) ;
#37104 = CIRCLE ( 'NONE', #103684, 0.1000000000000052097 ) ;
#37105 = CARTESIAN_POINT ( 'NONE',  ( 20.94999999999999929, 64.35000000001245724, -170.0231074845244166 ) ) ;
#37106 = ADVANCED_FACE ( 'NONE', ( #122441 ), #138122, .T. ) ;
#37107 = CARTESIAN_POINT ( 'NONE',  ( -16.87683809663752399, 9.865889849343238538, -154.2325731929306016 ) ) ;
#37108 = CARTESIAN_POINT ( 'NONE',  ( -18.50000000000000000, 64.35000000001190301, -96.00830171387039513 ) ) ;
#37109 = LINE ( 'NONE', #239138, #249626 ) ;
#37110 = CARTESIAN_POINT ( 'NONE',  ( -18.46919391072059113, 85.67072438829022474, -163.3493039527248811 ) ) ;
#37111 = ADVANCED_FACE ( 'NONE', ( #160304 ), #83143, .T. ) ;
#37112 = DIRECTION ( 'NONE',  ( -1.000000000000000000, 0.000000000000000000, 0.000000000000000000 ) ) ;
#37114 = EDGE_LOOP ( 'NONE', ( #110959, #129865, #162740, #24491 ) ) ;
#37113 = AXIS2_PLACEMENT_3D ( 'NONE', #240421, #177891, #117892 ) ;
#37115 = DIRECTION ( 'NONE',  ( 0.000000000000000000, 0.8660254037844377084, 0.5000000000000016653 ) ) ;
#37116 = ORIENTED_EDGE ( 'NONE', *, *, #125912, .F. ) ;
#37117 = ORIENTED_EDGE ( 'NONE', *, *, #250407, .F. ) ;
#37118 = ADVANCED_FACE ( 'NONE', ( #222797 ), #249966, .F. ) ;
#37119 = CYLINDRICAL_SURFACE ( 'NONE', #202632, 0.1000000000000028644 ) ;
#37120 = ADVANCED_FACE ( 'NONE', ( #44194 ), #123723, .T. ) ;
#37121 = PLANE ( 'NONE',  #223386 ) ;
#37122 = ORIENTED_EDGE ( 'NONE', *, *, #193622, .F. ) ;
#37123 = VECTOR ( 'NONE', #47383, 1000.000000000000000 ) ;
#37124 = ORIENTED_EDGE ( 'NONE', *, *, #170655, .T. ) ;
#37125 = AXIS2_PLACEMENT_3D ( 'NONE', #66829, #146344, #47238 ) ;
#37126 = CARTESIAN_POINT ( 'NONE',  ( 21.05000000000000071, 67.23127455305841238, -235.8551265064783991 ) ) ;
#37127 = ORIENTED_EDGE ( 'NONE', *, *, #199566, .F. ) ;
#37128 = AXIS2_PLACEMENT_3D ( 'NONE', #28978, #150178, #65478 ) ;
#37129 = EDGE_LOOP ( 'NONE', ( #22834, #48780, #129313, #102775 ) ) ;
#37130 = CARTESIAN_POINT ( 'NONE',  ( -23.39999999999994529, 74.83745509109094485, -43.82310748452479743 ) ) ;
#37131 = CARTESIAN_POINT ( 'NONE',  ( -21.53699400384793705, -1.597579023731851126E-12, 6.787711793239012081 ) ) ;
#37132 = SPHERICAL_SURFACE ( 'NONE', #205244, 0.1000000000000000056 ) ;
#37133 = DIRECTION ( 'NONE',  ( -1.000000000000000000, -2.952720810173289112E-16, 0.000000000000000000 ) ) ;
#37134 = CYLINDRICAL_SURFACE ( 'NONE', #156702, 0.09999999999999938105 ) ;
#37135 = LINE ( 'NONE', #174103, #50061 ) ;
#37136 = DIRECTION ( 'NONE',  ( 1.000000000000000000, -2.952720810173289112E-16, -2.061873921506763405E-30 ) ) ;
#37138 = ORIENTED_EDGE ( 'NONE', *, *, #30199, .T. ) ;
#37137 = DIRECTION ( 'NONE',  ( 0.000000000000000000, 0.1397316906016290161, -0.9901894034181595305 ) ) ;
#37140 = CARTESIAN_POINT ( 'NONE',  ( -21.07928932188134041, 65.47931918658504458, -241.9371126717015841 ) ) ;
#37139 = CARTESIAN_POINT ( 'NONE',  ( -17.78043020864321022, 21.36579535192818824, -229.0463459100317323 ) ) ;
#37141 = DIRECTION ( 'NONE',  ( -2.915501640297154283E-16, 1.000000000000000000, 0.000000000000000000 ) ) ;
#37142 = EDGE_LOOP ( 'NONE', ( #154522, #105486, #231738, #148627 ) ) ;
#37143 = CARTESIAN_POINT ( 'NONE',  ( -18.59999999999999787, 7.070967871798842452, -37.24656422186831151 ) ) ;
#37144 = FACE_OUTER_BOUND ( 'NONE', #221287, .T. ) ;
#37145 = ORIENTED_EDGE ( 'NONE', *, *, #50828, .F. ) ;
#37147 = CARTESIAN_POINT ( 'NONE',  ( 20.94999999999999929, 69.35000000001200249, -115.2731074845243455 ) ) ;
#37146 = CARTESIAN_POINT ( 'NONE',  ( -15.55912972643740488, 67.50912972644997012, -182.6731074845244223 ) ) ;
#37148 = FACE_OUTER_BOUND ( 'NONE', #83811, .T. ) ;
#37149 = ADVANCED_FACE ( 'NONE', ( #5022 ), #203249, .T. ) ;
#37150 = DIRECTION ( 'NONE',  ( 0.000000000000000000, 0.2617529984165031243, 0.9651348961777158619 ) ) ;
#37151 = ORIENTED_EDGE ( 'NONE', *, *, #242193, .T. ) ;
#37152 = ORIENTED_EDGE ( 'NONE', *, *, #158306, .F. ) ;
#37153 = DIRECTION ( 'NONE',  ( 1.000000000000000000, 0.000000000000000000, 0.000000000000000000 ) ) ;
#37154 = CARTESIAN_POINT ( 'NONE',  ( -18.50000000000000000, -0.6576273345615585297, -242.5323337003318898 ) ) ;
#37155 = DIRECTION ( 'NONE',  ( -1.000000000000000000, -0.000000000000000000, -0.000000000000000000 ) ) ;
#37156 = CARTESIAN_POINT ( 'NONE',  ( -18.59999999999999787, -1.162701749938009677, -8.099999999999999645 ) ) ;
#37157 = ORIENTED_EDGE ( 'NONE', *, *, #13479, .F. ) ;
#37158 = EDGE_CURVE ( 'NONE', #111271, #162073, #108332, .T. ) ;
#37159 = CARTESIAN_POINT ( 'NONE',  ( 18.39999999999999503, 11.47316190337363828, -191.7499999999999716 ) ) ;
#37160 = EDGE_CURVE ( 'NONE', #71963, #24859, #241592, .T. ) ;
#37161 = CYLINDRICAL_SURFACE ( 'NONE', #148377, 0.09999999999999781286 ) ;
#37162 = AXIS2_PLACEMENT_3D ( 'NONE', #51922, #252700, #214866 ) ;
#37163 = DIRECTION ( 'NONE',  ( 0.000000000000000000, 0.000000000000000000, -1.000000000000000000 ) ) ;
#37164 = CIRCLE ( 'NONE', #216193, 0.09999999999999971412 ) ;
#37165 = FACE_OUTER_BOUND ( 'NONE', #199915, .T. ) ;
#37166 = ADVANCED_FACE ( 'NONE', ( #183700 ), #62467, .T. ) ;
#37168 = ORIENTED_EDGE ( 'NONE', *, *, #137590, .T. ) ;
#37167 = DIRECTION ( 'NONE',  ( 0.000000000000000000, 1.000000000000000000, 0.000000000000000000 ) ) ;
#37169 = AXIS2_PLACEMENT_3D ( 'NONE', #154238, #233738, #55060 ) ;
#37170 = DIRECTION ( 'NONE',  ( 0.000000000000000000, -1.000000000000000000, -0.000000000000000000 ) ) ;
#37171 = CARTESIAN_POINT ( 'NONE',  ( -16.88783316861822215, 66.05000000001187743, -90.27084344254458870 ) ) ;
#37172 = DIRECTION ( 'NONE',  ( -1.000000000000000000, 7.304098846218134667E-16, 5.100424963727256530E-30 ) ) ;
#37173 = DIRECTION ( 'NONE',  ( 3.469446951953635015E-14, -0.000000000000000000, 1.000000000000000000 ) ) ;
#37174 = CARTESIAN_POINT ( 'NONE',  ( 18.55857864376267941, 10.36715728752537835, -24.75000000000000355 ) ) ;
#37175 = EDGE_CURVE ( 'NONE', #221590, #158004, #183343, .T. ) ;
#37177 = ORIENTED_EDGE ( 'NONE', *, *, #123537, .F. ) ;
#37176 = DIRECTION ( 'NONE',  ( 0.000000000000000000, 1.000000000000000000, 6.688090509790097607E-15 ) ) ;
#37178 = EDGE_CURVE ( 'NONE', #103686, #7048, #246236, .T. ) ;
#37179 = CARTESIAN_POINT ( 'NONE',  ( -23.15000000000000213, 1.115600667400684642E-11, -200.9999999999999432 ) ) ;
#37180 = LINE ( 'NONE', #189822, #57294 ) ;
#37181 = ORIENTED_EDGE ( 'NONE', *, *, #43109, .F. ) ;
#37182 = DIRECTION ( 'NONE',  ( 1.000000000000000000, 0.000000000000000000, 0.000000000000000000 ) ) ;
#37183 = DIRECTION ( 'NONE',  ( 0.000000000000000000, -0.000000000000000000, -1.000000000000000000 ) ) ;
#37184 = CARTESIAN_POINT ( 'NONE',  ( -20.64999999999999858, 2.000000000011154189, -180.7246219227620543 ) ) ;
#37185 = CIRCLE ( 'NONE', #166197, 11.75000000000001066 ) ;
#37186 = AXIS2_PLACEMENT_3D ( 'NONE', #1186, #78158, #238531 ) ;
#37187 = CARTESIAN_POINT ( 'NONE',  ( -18.40000000000000213, 65.08943781962308606, -222.1672656287770451 ) ) ;
#37188 = AXIS2_PLACEMENT_3D ( 'NONE', #60638, #56770, #140174 ) ;
#37189 = EDGE_CURVE ( 'NONE', #217337, #58261, #244941, .T. ) ;
#37190 = DIRECTION ( 'NONE',  ( 0.000000000000000000, 0.008583690987128059571, -0.9999631594459056361 ) ) ;
#37191 = LINE ( 'NONE', #116702, #25919 ) ;
#37192 = VECTOR ( 'NONE', #159307, 1000.000000000000000 ) ;
#37193 = EDGE_LOOP ( 'NONE', ( #246796, #8858, #101149, #45944 ) ) ;
#37194 = VERTEX_POINT ( 'NONE', #7624 ) ;
#37195 = DIRECTION ( 'NONE',  ( -7.304098846217608103E-16, 0.4721928772776973204, 0.8814952561688629284 ) ) ;
#37196 = CARTESIAN_POINT ( 'NONE',  ( -17.05016517656014940, 66.05000000001014371, -115.6958054805232621 ) ) ;
#37197 = ADVANCED_FACE ( 'NONE', ( #149726 ), #227953, .T. ) ;
#37198 =( BOUNDED_SURFACE ( )  B_SPLINE_SURFACE ( 3, 2, ( 
 ( #163305, #242822, #64200 ),
 ( #143722, #25097, #223252 ),
 ( #5472, #85009, #51013 ),
 ( #105860, #65470, #188001 ),
 ( #168483, #91468, #146289 ),
 ( #8085, #185427, #45914 ) ),
 .UNSPECIFIED., .F., .F., .F. ) 
 B_SPLINE_SURFACE_WITH_KNOTS ( ( 4, 2, 4 ),
 ( 3, 3 ),
 ( 0.0001300404313046710908, 0.0003183318589266651835, 0.0005066232865486592490 ),
 ( 0.000000000000000000, 1.000000000000000000 ),
 .UNSPECIFIED. ) 
 GEOMETRIC_REPRESENTATION_ITEM ( )  RATIONAL_B_SPLINE_SURFACE ( (
 ( 1.000000000000000000, 0.7071067811865475727, 1.000000000000000000),
 ( 1.000000000000000000, 0.7625113560553226089, 1.000000000000000000),
 ( 1.000000000000000000, 0.8126073484671799685, 1.000000000000000000),
 ( 1.000000000000000000, 0.8923049332749427576, 1.000000000000000000),
 ( 1.000000000000000000, 0.9231914937756658945, 1.000000000000000000),
 ( 1.000000000000000000, 0.9238795325112945100, 1.000000000000000000) ) ) 
 REPRESENTATION_ITEM ( '' )  SURFACE ( )  );
#37199 = DIRECTION ( 'NONE',  ( 0.000000000000000000, -0.9126074666063769270, -0.4088369013363280513 ) ) ;
#37200 = DIRECTION ( 'NONE',  ( -0.000000000000000000, 0.8814952561688430555, -0.4721928772777346239 ) ) ;
#37201 = ORIENTED_EDGE ( 'NONE', *, *, #250051, .T. ) ;
#37202 = CARTESIAN_POINT ( 'NONE',  ( -18.59999999999999787, -10.80884033489985363, 6.100000000000002309 ) ) ;
#37203 = CARTESIAN_POINT ( 'NONE',  ( 20.96937028524354929, 11.97530479700835393, -206.0589415372148778 ) ) ;
#37204 = FACE_OUTER_BOUND ( 'NONE', #162075, .T. ) ;
#37206 = LINE ( 'NONE', #217081, #23674 ) ;
#37205 = CIRCLE ( 'NONE', #182955, 0.09999999999998898659 ) ;
#37207 = EDGE_LOOP ( 'NONE', ( #103039, #162411, #142885, #237950 ) ) ;
#37208 = FACE_OUTER_BOUND ( 'NONE', #28939, .T. ) ;
#37209 = ORIENTED_EDGE ( 'NONE', *, *, #112447, .T. ) ;
#37210 = EDGE_LOOP ( 'NONE', ( #39735, #247515, #190953, #80035 ) ) ;
#37211 = CARTESIAN_POINT ( 'NONE',  ( -21.05000000000000071, 6.478078221105989520, -100.5999999353071246 ) ) ;
#37212 = PLANE ( 'NONE',  #228864 ) ;
#37213 = AXIS2_PLACEMENT_3D ( 'NONE', #211861, #48910, #248406 ) ;
#37214 = VERTEX_POINT ( 'NONE', #66316 ) ;
#37215 = CARTESIAN_POINT ( 'NONE',  ( 18.59999999999999432, 74.73821383144760944, -195.4366085209788935 ) ) ;
#37216 = DIRECTION ( 'NONE',  ( 0.000000000000000000, 0.000000000000000000, 1.000000000000000000 ) ) ;
#37217 = DIRECTION ( 'NONE',  ( -1.000000000000000000, 0.000000000000000000, -0.000000000000000000 ) ) ;
#37218 = EDGE_LOOP ( 'NONE', ( #9315, #195986, #21360, #80851 ) ) ;
#37219 = CARTESIAN_POINT ( 'NONE',  ( -23.25000000000000000, 4.350000000011156054, -112.8500000000000369 ) ) ;
#37221 = ORIENTED_EDGE ( 'NONE', *, *, #150995, .T. ) ;
#37220 = CARTESIAN_POINT ( 'NONE',  ( 18.49999999999999289, 65.62657994473259748, -145.2573193598993839 ) ) ;
#37222 = CARTESIAN_POINT ( 'NONE',  ( 23.14999999999999503, 61.90000000001175096, -75.12340509566377023 ) ) ;
#37223 = CARTESIAN_POINT ( 'NONE',  ( -18.59999999999999787, -1.162701749926853712, -142.1000000000000227 ) ) ;
#37224 = CIRCLE ( 'NONE', #74670, 0.1000000000000089567 ) ;
#37225 = EDGE_CURVE ( 'NONE', #44645, #129552, #204525, .T. ) ;
#37226 = AXIS2_PLACEMENT_3D ( 'NONE', #53884, #173878, #33081 ) ;
#37227 = ORIENTED_EDGE ( 'NONE', *, *, #26353, .T. ) ;
#37228 = CARTESIAN_POINT ( 'NONE',  ( -18.69999999999999929, -1.212568896937008089, -8.000000000000000000 ) ) ;
#37229 = DIRECTION ( 'NONE',  ( 1.000000000000000000, -7.304098846218134667E-16, -5.100424963727255829E-30 ) ) ;
#37230 = CARTESIAN_POINT ( 'NONE',  ( -20.94999999999999929, 1.261786168576181755, -108.5864989635455089 ) ) ;
#37231 = ORIENTED_EDGE ( 'NONE', *, *, #31224, .T. ) ;
#37232 = DIRECTION ( 'NONE',  ( 8.673617379884087537E-15, -0.000000000000000000, 1.000000000000000000 ) ) ;
#37233 = ADVANCED_FACE ( 'NONE', ( #91004 ), #190119, .F. ) ;
#37234 = DIRECTION ( 'NONE',  ( 0.000000000000000000, 1.000000000000000000, 0.000000000000000000 ) ) ;
#37235 = CARTESIAN_POINT ( 'NONE',  ( 18.59999999999999076, 1.835341550235567887, -179.1551512925629197 ) ) ;
#37236 = VECTOR ( 'NONE', #39385, 1000.000000000000000 ) ;
#37237 = AXIS2_PLACEMENT_3D ( 'NONE', #110311, #115442, #209408 ) ;
#37238 = EDGE_CURVE ( 'NONE', #77194, #55547, #133266, .T. ) ;
#37239 = ORIENTED_EDGE ( 'NONE', *, *, #152818, .F. ) ;
#37240 = ADVANCED_FACE ( 'NONE', ( #229248 ), #127571, .F. ) ;
#37241 = CARTESIAN_POINT ( 'NONE',  ( -22.39999999999999858, 55.91711482281189660, -232.6830152854666949 ) ) ;
#37242 = ORIENTED_EDGE ( 'NONE', *, *, #2812, .F. ) ;
#37243 = CIRCLE ( 'NONE', #112074, 0.5000000000000004441 ) ;
#37244 = AXIS2_PLACEMENT_3D ( 'NONE', #150732, #186004, #89457 ) ;
#37245 = AXIS2_PLACEMENT_3D ( 'NONE', #73670, #192312, #243614 ) ;
#37246 = AXIS2_PLACEMENT_3D ( 'NONE', #67522, #229180, #8842 ) ;
#37247 = ORIENTED_EDGE ( 'NONE', *, *, #109799, .F. ) ;
#37248 = DIRECTION ( 'NONE',  ( -1.000000000000000000, 0.000000000000000000, 0.000000000000000000 ) ) ;
#37249 = EDGE_CURVE ( 'NONE', #121012, #175390, #55507, .T. ) ;
#37250 = TOROIDAL_SURFACE ( 'NONE', #182997, 0.2000000000000000111, 0.1000000000000000056 ) ;
#37251 = CARTESIAN_POINT ( 'NONE',  ( -20.54999999999999716, 68.85000000001222986, -148.8731074845244109 ) ) ;
#37253 = ORIENTED_EDGE ( 'NONE', *, *, #142306, .T. ) ;
#37252 = DIRECTION ( 'NONE',  ( 0.000000000000000000, 0.000000000000000000, -1.000000000000000000 ) ) ;
#37254 = CARTESIAN_POINT ( 'NONE',  ( -20.94999999999999929, 14.81796439977981272, -236.5325475414793743 ) ) ;
#37255 = DIRECTION ( 'NONE',  ( -0.000000000000000000, 0.4088369013363276072, -0.9126074666063772600 ) ) ;
#37256 = ADVANCED_FACE ( 'NONE', ( #25912 ), #85837, .T. ) ;
#37257 = CARTESIAN_POINT ( 'NONE',  ( -21.05000000000000071, 74.16465844978745281, -91.46795619196133487 ) ) ;
#37258 = CARTESIAN_POINT ( 'NONE',  ( -18.44448725179913851, 85.49008171549498059, -62.89414719046176572 ) ) ;
#37259 = CARTESIAN_POINT ( 'NONE',  ( 20.85000000000000142, 76.00000000001244871, -170.0231074845243597 ) ) ;
#37260 = FACE_OUTER_BOUND ( 'NONE', #27450, .T. ) ;
#37261 = FACE_OUTER_BOUND ( 'NONE', #216819, .T. ) ;
#37263 = ORIENTED_EDGE ( 'NONE', *, *, #195890, .F. ) ;
#37262 = CARTESIAN_POINT ( 'NONE',  ( 20.94999999999999929, 71.00000000001158185, -57.11784146561126363 ) ) ;
#37265 = ORIENTED_EDGE ( 'NONE', *, *, #150565, .T. ) ;
#37264 = CARTESIAN_POINT ( 'NONE',  ( 18.79999999999999716, 11.59510167572422112, -1.901609089591594470 ) ) ;
#37267 = CARTESIAN_POINT ( 'NONE',  ( -16.88783316861814043, 51.52553600391507160, -231.9882783296907576 ) ) ;
#37266 = FACE_OUTER_BOUND ( 'NONE', #257672, .T. ) ;
#37269 = ORIENTED_EDGE ( 'NONE', *, *, #34357, .T. ) ;
#37268 = CARTESIAN_POINT ( 'NONE',  ( 21.05000000000000071, 8.776282895303630482, -75.55862899514100661 ) ) ;
#37270 = ORIENTED_EDGE ( 'NONE', *, *, #72035, .T. ) ;
#37271 = AXIS2_PLACEMENT_3D ( 'NONE', #157148, #197523, #18890 ) ;
#37272 = CARTESIAN_POINT ( 'NONE',  ( -20.94999999999999929, 1.360870587203197646, -108.5729979270909951 ) ) ;
#37274 = ADVANCED_FACE ( 'NONE', ( #130125 ), #29791, .T. ) ;
#37273 = CARTESIAN_POINT ( 'NONE',  ( -21.05000000000000071, 48.04585786805223080, -246.4610531646956417 ) ) ;
#37275 = CARTESIAN_POINT ( 'NONE',  ( 20.94999999999999929, 65.65271564877468791, -222.5736063831752176 ) ) ;
#37276 = EDGE_CURVE ( 'NONE', #9997, #228810, #31074, .T. ) ;
#37277 = ADVANCED_FACE ( 'NONE', ( #166728 ), #37606, .T. ) ;
#37278 = CARTESIAN_POINT ( 'NONE',  ( -18.50000000000000000, 67.49462292596869872, -195.5612049585272700 ) ) ;
#37279 = CARTESIAN_POINT ( 'NONE',  ( 18.69999999999999929, -8.250000000000005329, 32.89999999999999858 ) ) ;
#37280 = AXIS2_PLACEMENT_3D ( 'NONE', #10338, #89844, #211092 ) ;
#37281 = CARTESIAN_POINT ( 'NONE',  ( -16.97048361161167662, 66.05000000001203375, -116.1642231400940091 ) ) ;
#37282 = ORIENTED_EDGE ( 'NONE', *, *, #210109, .T. ) ;
#37283 = ORIENTED_EDGE ( 'NONE', *, *, #65378, .F. ) ;
#37284 = DIRECTION ( 'NONE',  ( 0.7071067811865302533, -0.6909108974501196876, -0.1504730267679053324 ) ) ;
#37285 = EDGE_CURVE ( 'NONE', #214793, #89225, #229120, .T. ) ;
#37286 = ORIENTED_EDGE ( 'NONE', *, *, #66396, .F. ) ;
#37287 = DIRECTION ( 'NONE',  ( 1.000000000000000000, -3.151514657663852580E-16, 8.547182517843351137E-17 ) ) ;
#37288 = CARTESIAN_POINT ( 'NONE',  ( -16.95709691156038446, 51.60968432554658847, -231.9505809183468727 ) ) ;
#37289 = CARTESIAN_POINT ( 'NONE',  ( -23.15000000000000213, 76.00000000001213607, -136.5231074845243313 ) ) ;
#37290 =( BOUNDED_SURFACE ( )  B_SPLINE_SURFACE ( 3, 2, ( 
 ( #118062, #254942, #115490 ),
 ( #161056, #80184, #653 ),
 ( #136311, #159771, #236710 ),
 ( #58066, #120660, #155937 ) ),
 .UNSPECIFIED., .F., .F., .T. ) 
 B_SPLINE_SURFACE_WITH_KNOTS ( ( 4, 4 ),
 ( 3, 3 ),
 ( 0.0008258556059633741101, 0.0009616864997632722234 ),
 ( 0.000000000000000000, 1.000000000000000000 ),
 .UNSPECIFIED. ) 
 GEOMETRIC_REPRESENTATION_ITEM ( )  RATIONAL_B_SPLINE_SURFACE ( (
 ( 1.000000000000000000, 0.9152888060719065466, 1.000000000000000000),
 ( 1.000000000000000000, 0.9327727094138433817, 1.000000000000000000),
 ( 1.000000000000000000, 0.9369023509258295190, 1.000000000000000000),
 ( 1.000000000000000000, 0.9246339933864298199, 1.000000000000000000) ) ) 
 REPRESENTATION_ITEM ( '' )  SURFACE ( )  );
#37291 = DIRECTION ( 'NONE',  ( 2.952720810173289112E-16, 1.000000000000000000, 6.982962677686266711E-15 ) ) ;
#37292 = ORIENTED_EDGE ( 'NONE', *, *, #136050, .T. ) ;
#37293 = DIRECTION ( 'NONE',  ( 0.000000000000000000, 0.8814952561688448318, -0.4721928772777310157 ) ) ;
#37294 = EDGE_LOOP ( 'NONE', ( #130349, #95382, #198127, #151376 ) ) ;
#37295 = CARTESIAN_POINT ( 'NONE',  ( -18.41431012584569160, 11.48747202921933130, -91.27323601310172307 ) ) ;
#37296 = ORIENTED_EDGE ( 'NONE', *, *, #57199, .T. ) ;
#37297 = CIRCLE ( 'NONE', #166489, 0.1999999999999987899 ) ;
#37298 = DIRECTION ( 'NONE',  ( -0.000000000000000000, -1.000000000000000000, 0.000000000000000000 ) ) ;
#37299 = ADVANCED_FACE ( 'NONE', ( #111864 ), #92281, .F. ) ;
#37300 = CARTESIAN_POINT ( 'NONE',  ( 23.14999999999999503, 64.25000000001185185, -90.87310748452438247 ) ) ;
#37301 = AXIS2_PLACEMENT_3D ( 'NONE', #137069, #39281, #3973 ) ;
#37302 = CARTESIAN_POINT ( 'NONE',  ( -16.86578989773641979, 9.984809801269951990, -113.0353351133777977 ) ) ;
#37303 = ORIENTED_EDGE ( 'NONE', *, *, #34555, .T. ) ;
#37304 = DIRECTION ( 'NONE',  ( 1.020425574104003999E-15, -0.2128009952263603677, 0.9770955615653313941 ) ) ;
#37306 = ORIENTED_EDGE ( 'NONE', *, *, #192717, .T. ) ;
#37305 = CARTESIAN_POINT ( 'NONE',  ( 17.74533788810830615, 10.81849979147079210, -10.31362267494758100 ) ) ;
#37307 = CARTESIAN_POINT ( 'NONE',  ( -21.05000000000000071, 64.25000000001146816, -42.86470817442145176 ) ) ;
#37308 = CIRCLE ( 'NONE', #162213, 0.1999999999999987899 ) ;
#37309 = EDGE_LOOP ( 'NONE', ( #54924, #70869, #74214, #81340 ) ) ;
#37310 = EDGE_CURVE ( 'NONE', #119449, #159714, #215745, .T. ) ;
#37311 = CARTESIAN_POINT ( 'NONE',  ( 21.07016717457011623, -5.802175688691957323E-16, 6.320940838100908010 ) ) ;
#37312 = VERTEX_POINT ( 'NONE', #231819 ) ;
#37313 = FACE_OUTER_BOUND ( 'NONE', #42554, .T. ) ;
#37314 = CARTESIAN_POINT ( 'NONE',  ( -23.49999999999994316, 84.00000000001119815, -34.86056257560453986 ) ) ;
#37315 = DIRECTION ( 'NONE',  ( -1.000000000000000000, 0.000000000000000000, 0.000000000000000000 ) ) ;
#37316 = SPHERICAL_SURFACE ( 'NONE', #235161, 0.1000000000000000056 ) ;
#37317 = ADVANCED_FACE ( 'NONE', ( #71470 ), #87459, .T. ) ;
#37318 = CARTESIAN_POINT ( 'NONE',  ( -20.54999999999999716, 74.00000000001259082, -190.2984855617622770 ) ) ;
#37319 = ORIENTED_EDGE ( 'NONE', *, *, #197234, .F. ) ;
#37320 = CYLINDRICAL_SURFACE ( 'NONE', #152743, 11.74999999999999289 ) ;
#37321 = CARTESIAN_POINT ( 'NONE',  ( -20.94560253601877164, 64.25000000001195133, -110.0130239720089094 ) ) ;
#37322 = AXIS2_PLACEMENT_3D ( 'NONE', #252730, #74144, #248909 ) ;
#37323 = CARTESIAN_POINT ( 'NONE',  ( -20.94560253601877164, 11.75000000001115197, -160.5100835125150809 ) ) ;
#37324 = VERTEX_POINT ( 'NONE', #140054 ) ;
#37325 = CARTESIAN_POINT ( 'NONE',  ( -18.50000000000000000, 74.65925378207832352, -113.2959699899454904 ) ) ;
#37326 = ORIENTED_EDGE ( 'NONE', *, *, #248462, .T. ) ;
#37327 = CARTESIAN_POINT ( 'NONE',  ( -18.59999999999999787, -1.249999999999999334, -8.000000000000000000 ) ) ;
#37328 = ORIENTED_EDGE ( 'NONE', *, *, #152678, .T. ) ;
#37329 = EDGE_CURVE ( 'NONE', #9718, #187977, #120821, .T. ) ;
#37330 = EDGE_CURVE ( 'NONE', #77200, #104626, #8378, .T. ) ;
#37331 = CARTESIAN_POINT ( 'NONE',  ( 23.24999999999999289, 64.35000000001164722, -69.52310748452440237 ) ) ;
#37332 = CARTESIAN_POINT ( 'NONE',  ( -20.94999999999999929, 46.54514716347711101, -243.1111603596801842 ) ) ;
#37334 = ORIENTED_EDGE ( 'NONE', *, *, #68975, .F. ) ;
#37333 = CARTESIAN_POINT ( 'NONE',  ( -18.50000000000000000, 7.021664781900089913, -37.33356540189728889 ) ) ;
#37335 = CARTESIAN_POINT ( 'NONE',  ( -18.50000000000000711, 9.064267525453134411, -245.4573321305639126 ) ) ;
#37336 = ORIENTED_EDGE ( 'NONE', *, *, #42020, .T. ) ;
#37337 = CARTESIAN_POINT ( 'NONE',  ( 18.57071067811864040, 10.17928932189250091, -54.85000000000000142 ) ) ;
#37338 = CARTESIAN_POINT ( 'NONE',  ( -21.14999999999994174, 74.73834681386826162, -44.00978271863746016 ) ) ;
#37339 = VERTEX_POINT ( 'NONE', #77505 ) ;
#37340 = VERTEX_POINT ( 'NONE', #177935 ) ;
#37341 = AXIS2_PLACEMENT_3D ( 'NONE', #85280, #125716, #106136 ) ;
#37343 = CIRCLE ( 'NONE', #53907, 0.1000000000000028644 ) ;
#37342 = CARTESIAN_POINT ( 'NONE',  ( -23.15000000000000213, -11.65000000000000036, 3.469446951953614189E-15 ) ) ;
#37344 = ORIENTED_EDGE ( 'NONE', *, *, #141720, .F. ) ;
#37345 = AXIS2_PLACEMENT_3D ( 'NONE', #111290, #50022, #73475 ) ;
#37347 = FACE_OUTER_BOUND ( 'NONE', #93393, .T. ) ;
#37346 = CIRCLE ( 'NONE', #183089, 0.1000000000000028644 ) ;
#37348 = EDGE_CURVE ( 'NONE', #107985, #62912, #98336, .T. ) ;
#37349 = ORIENTED_EDGE ( 'NONE', *, *, #13983, .F. ) ;
#37350 = CARTESIAN_POINT ( 'NONE',  ( -21.44999999999999929, 68.65000000001205649, -124.1731074845243512 ) ) ;
#37351 = FACE_OUTER_BOUND ( 'NONE', #88452, .T. ) ;
#37352 = EDGE_CURVE ( 'NONE', #94397, #241131, #212391, .T. ) ;
#37354 = ORIENTED_EDGE ( 'NONE', *, *, #221045, .T. ) ;
#37353 = DIRECTION ( 'NONE',  ( 0.000000000000000000, 0.9908441862701596881, 0.1350103645451904977 ) ) ;
#37355 = CARTESIAN_POINT ( 'NONE',  ( 20.94999999999999929, 5.850000000011160495, -90.36750277572211587 ) ) ;
#37356 = VECTOR ( 'NONE', #132717, 1000.000000000000000 ) ;
#37357 = DIRECTION ( 'NONE',  ( 0.000000000000000000, -6.982962677686266711E-15, 1.000000000000000000 ) ) ;
#37358 = EDGE_CURVE ( 'NONE', #176779, #88139, #185480, .T. ) ;
#37359 = DIRECTION ( 'NONE',  ( -0.000000000000000000, 0.2617529984165031243, 0.9651348961777157509 ) ) ;
#37360 = AXIS2_PLACEMENT_3D ( 'NONE', #87899, #102314, #24128 ) ;
#37362 = CARTESIAN_POINT ( 'NONE',  ( -18.59999999999999787, 7.021664781911246322, -137.8335654018973457 ) ) ;
#37361 = LINE ( 'NONE', #133869, #115212 ) ;
#37363 = CARTESIAN_POINT ( 'NONE',  ( 20.05000000000002913, 68.75000000001206502, -127.2731074845243597 ) ) ;
#37365 = EDGE_CURVE ( 'NONE', #44063, #222155, #171870, .T. ) ;
#37364 = DIRECTION ( 'NONE',  ( 0.000000000000000000, -0.9651348961777157509, 0.2617529984165031243 ) ) ;
#37366 = DIRECTION ( 'NONE',  ( 0.000000000000000000, -0.2617529984165152257, -0.9651348961777124202 ) ) ;
#37367 = CARTESIAN_POINT ( 'NONE',  ( 22.40000000000010516, -3.140208063161409324, -228.2318569537746953 ) ) ;
#37368 = CIRCLE ( 'NONE', #87412, 11.79999999999999716 ) ;
#37369 = ORIENTED_EDGE ( 'NONE', *, *, #159690, .T. ) ;
#37370 = ORIENTED_EDGE ( 'NONE', *, *, #180054, .F. ) ;
#37371 = CARTESIAN_POINT ( 'NONE',  ( -20.64999999999999858, -6.438379425586759908, -212.1495692908769684 ) ) ;
#37373 = ORIENTED_EDGE ( 'NONE', *, *, #102002, .F. ) ;
#37372 = DIRECTION ( 'NONE',  ( 0.000000000000000000, -1.000000000000000000, 0.000000000000000000 ) ) ;
#37374 = EDGE_LOOP ( 'NONE', ( #15558, #149906, #150509, #127558 ) ) ;
#37375 = CARTESIAN_POINT ( 'NONE',  ( -13.39999999999994529, 67.72071067812984779, -24.99381816264344991 ) ) ;
#37376 = ORIENTED_EDGE ( 'NONE', *, *, #114140, .F. ) ;
#37377 = DIRECTION ( 'NONE',  ( 0.000000000000000000, -6.982962677686266711E-15, 1.000000000000000000 ) ) ;
#37378 = EDGE_CURVE ( 'NONE', #118480, #20778, #39725, .T. ) ;
#37379 = EDGE_CURVE ( 'NONE', #24249, #139103, #70944, .T. ) ;
#37380 = ORIENTED_EDGE ( 'NONE', *, *, #82285, .F. ) ;
#37381 =( NAMED_UNIT ( * ) SI_UNIT ( $, .STERADIAN. ) SOLID_ANGLE_UNIT ( ) );
#37382 = CARTESIAN_POINT ( 'NONE',  ( -16.94107738177415712, 65.98576071487524075, -90.47310748452437679 ) ) ;
#37383 = AXIS2_PLACEMENT_3D ( 'NONE', #246324, #67680, #147218 ) ;
#37385 = ORIENTED_EDGE ( 'NONE', *, *, #207847, .F. ) ;
#37384 = ORIENTED_EDGE ( 'NONE', *, *, #103269, .T. ) ;
#37386 = ORIENTED_EDGE ( 'NONE', *, *, #245045, .T. ) ;
#37387 = ORIENTED_EDGE ( 'NONE', *, *, #251071, .T. ) ;
#37388 = EDGE_LOOP ( 'NONE', ( #26013, #57193, #33247, #29366 ) ) ;
#37389 = CARTESIAN_POINT ( 'NONE',  ( -21.44999999999999929, 7.350000000011155166, -54.75000000000000000 ) ) ;
#37390 = CARTESIAN_POINT ( 'NONE',  ( 18.49999999999999645, 74.27191306321800823, -183.1386724793566145 ) ) ;
#37392 = ORIENTED_EDGE ( 'NONE', *, *, #221852, .T. ) ;
#37391 = DIRECTION ( 'NONE',  ( 0.000000000000000000, 0.000000000000000000, -1.000000000000000000 ) ) ;
#37393 = CIRCLE ( 'NONE', #112230, 0.09999999999999939493 ) ;
#37394 = CARTESIAN_POINT ( 'NONE',  ( -22.00411653962173730, 33.60306640061016026, -242.9721070132478076 ) ) ;
#37395 = CARTESIAN_POINT ( 'NONE',  ( 13.88302573338719093, 12.43282705614461925, -213.6439690125878883 ) ) ;
#37397 = ORIENTED_EDGE ( 'NONE', *, *, #111600, .F. ) ;
#37396 = CARTESIAN_POINT ( 'NONE',  ( 23.24999999999999289, 63.22596473392088967, -234.7688515630498785 ) ) ;
#37398 = LINE ( 'NONE', #236852, #158373 ) ;
#37399 = EDGE_LOOP ( 'NONE', ( #247895, #132383, #41039, #30188 ) ) ;
#37400 = DIRECTION ( 'NONE',  ( 1.000000000000000000, 1.186688945009010077E-16, 0.000000000000000000 ) ) ;
#37402 = ORIENTED_EDGE ( 'NONE', *, *, #141759, .F. ) ;
#37401 = FACE_OUTER_BOUND ( 'NONE', #231220, .T. ) ;
#37403 = DIRECTION ( 'NONE',  ( -0.000000000000000000, -0.01283462868040327436, 0.9999176327611370985 ) ) ;
#37404 = CARTESIAN_POINT ( 'NONE',  ( -16.91256925476571027, 9.985731158139330432, -113.0323575109947569 ) ) ;
#37405 = CARTESIAN_POINT ( 'NONE',  ( -16.97092634996655747, 10.00088896635952196, -87.86985723370234780 ) ) ;
#37406 = ORIENTED_EDGE ( 'NONE', *, *, #119188, .T. ) ;
#37408 = DIRECTION ( 'NONE',  ( 0.000000000000000000, -7.147358527629766941E-15, 1.000000000000000000 ) ) ;
#37407 = CARTESIAN_POINT ( 'NONE',  ( -16.87683809663750978, 9.950000000011137047, -46.90236401819647227 ) ) ;
#37409 = CIRCLE ( 'NONE', #91558, 4.150000000000001243 ) ;
#37410 = DIRECTION ( 'NONE',  ( 0.000000000000000000, 0.3999834006488773852, 0.9165223833629813077 ) ) ;
#37411 = EDGE_CURVE ( 'NONE', #106243, #65120, #53162, .T. ) ;
#37412 = CARTESIAN_POINT ( 'NONE',  ( -18.59999999999999787, 64.25000000001179501, -81.67310748452439384 ) ) ;
#37413 = LINE ( 'NONE', #58216, #22552 ) ;
#37414 = AXIS2_PLACEMENT_3D ( 'NONE', #84959, #242773, #164546 ) ;
#37415 = VERTEX_POINT ( 'NONE', #219599 ) ;
#37416 = ORIENTED_EDGE ( 'NONE', *, *, #107684, .T. ) ;
#37417 = CARTESIAN_POINT ( 'NONE',  ( -17.11825945287482753, 10.05000000001113847, -180.1499999999999773 ) ) ;
#37418 = DIRECTION ( 'NONE',  ( 0.000000000000000000, 0.000000000000000000, 1.000000000000000000 ) ) ;
#37419 = ORIENTED_EDGE ( 'NONE', *, *, #44960, .F. ) ;
#37420 = CIRCLE ( 'NONE', #70745, 0.1000000000000055844 ) ;
#37421 = ORIENTED_EDGE ( 'NONE', *, *, #254499, .T. ) ;
#37422 = CARTESIAN_POINT ( 'NONE',  ( -20.64999999999999858, -8.663551401858004652, -143.5241011180673070 ) ) ;
#37423 = CARTESIAN_POINT ( 'NONE',  ( -21.46681500598105430, 76.00000000001243450, -176.8806186439499299 ) ) ;
#37424 = VECTOR ( 'NONE', #234773, 1000.000000000000000 ) ;
#37425 = ORIENTED_EDGE ( 'NONE', *, *, #144413, .F. ) ;
#37426 = CARTESIAN_POINT ( 'NONE',  ( -23.25000000000000000, -3.770473190032741062, -225.9805569534692324 ) ) ;
#37427 = EDGE_CURVE ( 'NONE', #106654, #66484, #33350, .T. ) ;
#37429 = ORIENTED_EDGE ( 'NONE', *, *, #88801, .F. ) ;
#37428 = VECTOR ( 'NONE', #139047, 1000.000000000000000 ) ;
#37430 = EDGE_LOOP ( 'NONE', ( #73978, #24835, #82471, #3983 ) ) ;
#37431 = CIRCLE ( 'NONE', #94728, 2.000000000000001776 ) ;
#37432 = VECTOR ( 'NONE', #105713, 1000.000000000000000 ) ;
#37433 = ORIENTED_EDGE ( 'NONE', *, *, #96368, .F. ) ;
#37434 = CIRCLE ( 'NONE', #158261, 0.09999999999999949207 ) ;
#37435 = VECTOR ( 'NONE', #134079, 1000.000000000000000 ) ;
#37436 = CARTESIAN_POINT ( 'NONE',  ( 21.05000000000000071, -11.48912529306489994, -164.5000000000000000 ) ) ;
#37437 = LINE ( 'NONE', #219902, #7481 ) ;
#37438 = FACE_OUTER_BOUND ( 'NONE', #118708, .T. ) ;
#37439 = CARTESIAN_POINT ( 'NONE',  ( -20.94999999999999929, -1.835341550213257733, -78.55515129256303908 ) ) ;
#37440 = CARTESIAN_POINT ( 'NONE',  ( 15.51872946208854920, 66.62341902196808974, -118.8961612375124446 ) ) ;
#37442 = FACE_OUTER_BOUND ( 'NONE', #169529, .T. ) ;
#37441 = DIRECTION ( 'NONE',  ( 6.484947573744954877E-15, -0.9274965247785555977, 0.3738317757009190223 ) ) ;
#37443 = CYLINDRICAL_SURFACE ( 'NONE', #249735, 0.5000000000000004441 ) ;
#37445 = ORIENTED_EDGE ( 'NONE', *, *, #166756, .T. ) ;
#37444 = DIRECTION ( 'NONE',  ( 0.000000000000000000, -0.4999999999999949485, 0.8660254037844415942 ) ) ;
#37446 = DIRECTION ( 'NONE',  ( 1.000000000000000000, 0.000000000000000000, 0.000000000000000000 ) ) ;
#37447 = VERTEX_POINT ( 'NONE', #136188 ) ;
#37448 = CARTESIAN_POINT ( 'NONE',  ( -16.89268316805466341, 22.97380970494227626, -230.9308293615217451 ) ) ;
#37449 = ORIENTED_EDGE ( 'NONE', *, *, #113774, .F. ) ;
#37450 = EDGE_LOOP ( 'NONE', ( #156674, #109395, #97056, #161312, #139798 ) ) ;
#37451 = CARTESIAN_POINT ( 'NONE',  ( 18.59999999999999076, 1.115600667400684642E-11, -167.5000000000000284 ) ) ;
#37452 = DIRECTION ( 'NONE',  ( 0.000000000000000000, -0.9910465087640860649, 0.1335171055202901413 ) ) ;
#37453 = CYLINDRICAL_SURFACE ( 'NONE', #220927, 0.09999999999999976963 ) ;
#37454 = ORIENTED_EDGE ( 'NONE', *, *, #70285, .T. ) ;
#37455 = DIRECTION ( 'NONE',  ( 0.000000000000000000, 0.9126074666063660468, 0.4088369013363524762 ) ) ;
#37456 = DIRECTION ( 'NONE',  ( 0.000000000000000000, 0.2128009952263485993, -0.9770955615653341697 ) ) ;
#37457 = ORIENTED_EDGE ( 'NONE', *, *, #30531, .F. ) ;
#37458 = ORIENTED_EDGE ( 'NONE', *, *, #183813, .T. ) ;
#37459 = CARTESIAN_POINT ( 'NONE',  ( -16.81744102076748959, 9.950000000011138823, -87.85000000000005116 ) ) ;
#37460 = ORIENTED_EDGE ( 'NONE', *, *, #180929, .F. ) ;
#37461 = DIRECTION ( 'NONE',  ( 1.000000000000000000, 0.000000000000000000, 0.000000000000000000 ) ) ;
#37462 = DIRECTION ( 'NONE',  ( 1.000000000000000000, 0.000000000000000000, 0.000000000000000000 ) ) ;
#37463 = ORIENTED_EDGE ( 'NONE', *, *, #122168, .T. ) ;
#37464 = CARTESIAN_POINT ( 'NONE',  ( 23.14999999999999858, 21.15538238767524604, -233.7023398932965108 ) ) ;
#37465 = CARTESIAN_POINT ( 'NONE',  ( -16.80100914604134132, 9.943149094114721365, -121.3170441272877014 ) ) ;
#37466 = CARTESIAN_POINT ( 'NONE',  ( 22.49999999999999645, 11.74956712350054744, -133.8991416309012834 ) ) ;
#37467 = ORIENTED_EDGE ( 'NONE', *, *, #91654, .F. ) ;
#37468 = CIRCLE ( 'NONE', #162360, 0.09999999999999939493 ) ;
#37469 = FACE_OUTER_BOUND ( 'NONE', #51061, .T. ) ;
#37470 = DIRECTION ( 'NONE',  ( 0.000000000000000000, -0.000000000000000000, -1.000000000000000000 ) ) ;
#37471 = TOROIDAL_SURFACE ( 'NONE', #66679, 0.2000000000000000111, 0.1000000000000000056 ) ;
#37472 = ADVANCED_FACE ( 'NONE', ( #57950 ), #158394, .F. ) ;
#37473 = CARTESIAN_POINT ( 'NONE',  ( -21.05000000000000071, 61.95000000001265050, -198.0094124137634708 ) ) ;
#37474 = EDGE_LOOP ( 'NONE', ( #75760, #16349, #90928, #250273 ) ) ;
#37475 = EDGE_CURVE ( 'NONE', #130548, #107243, #132338, .T. ) ;
#37476 = DIRECTION ( 'NONE',  ( 0.000000000000000000, 0.000000000000000000, -1.000000000000000000 ) ) ;
#37477 = ORIENTED_EDGE ( 'NONE', *, *, #117834, .F. ) ;
#37478 = CARTESIAN_POINT ( 'NONE',  ( 20.95512820512820440, 18.86447962780959386, -229.9497396848627204 ) ) ;
#37479 = FACE_OUTER_BOUND ( 'NONE', #48186, .T. ) ;
#37480 = EDGE_CURVE ( 'NONE', #62294, #77834, #22725, .T. ) ;
#37481 = LINE ( 'NONE', #156158, #46424 ) ;
#37482 = LINE ( 'NONE', #16635, #173264 ) ;
#37483 = DIRECTION ( 'NONE',  ( -1.000000000000000000, -0.000000000000000000, -0.000000000000000000 ) ) ;
#37484 = DIRECTION ( 'NONE',  ( 1.000000000000000000, 0.000000000000000000, 0.000000000000000000 ) ) ;
#37485 = AXIS2_PLACEMENT_3D ( 'NONE', #254872, #217072, #231538 ) ;
#37486 = ORIENTED_EDGE ( 'NONE', *, *, #148673, .T. ) ;
#37487 = CARTESIAN_POINT ( 'NONE',  ( -16.94445028196808778, 66.00793639031432747, -123.9157773061059231 ) ) ;
#37488 = CIRCLE ( 'NONE', #183218, 0.09999999999999943656 ) ;
#37489 = DIRECTION ( 'NONE',  ( -2.578261006436898806E-14, 0.9371753822965325220, -0.3488585713686107592 ) ) ;
#37490 = CARTESIAN_POINT ( 'NONE',  ( -18.49372193242259499, 77.26530055437073941, -241.7067161772392865 ) ) ;
#37491 = DIRECTION ( 'NONE',  ( 1.000000000000000000, -1.809991526360996944E-16, 4.908854824437060108E-17 ) ) ;
#37492 = EDGE_CURVE ( 'NONE', #134706, #136972, #185628, .T. ) ;
#37493 = VECTOR ( 'NONE', #231132, 1000.000000000000000 ) ;
#37494 = DIRECTION ( 'NONE',  ( 0.000000000000000000, 0.000000000000000000, 1.000000000000000000 ) ) ;
#37495 = EDGE_LOOP ( 'NONE', ( #254727, #28874, #162662, #163960 ) ) ;
#37496 = ORIENTED_EDGE ( 'NONE', *, *, #228508, .F. ) ;
#37497 = DIRECTION ( 'NONE',  ( 0.000000000000000000, 0.9889818879709272315, 0.1480365673253073999 ) ) ;
#37498 = CARTESIAN_POINT ( 'NONE',  ( -21.00000000000000000, 6.258114003436813455, 11.90000000000000036 ) ) ;
#37499 = DIRECTION ( 'NONE',  ( 1.000000000000000000, -2.986185139342070877E-16, 6.665775143889692774E-16 ) ) ;
#37500 = DIRECTION ( 'NONE',  ( 0.000000000000000000, -0.9316174814283004757, -0.3634403228828503307 ) ) ;
#37501 = DIRECTION ( 'NONE',  ( 0.000000000000000000, 0.9623856809447771665, 0.2716869542551821892 ) ) ;
#37502 = EDGE_CURVE ( 'NONE', #83073, #131237, #104208, .T. ) ;
#37503 = VERTEX_POINT ( 'NONE', #65668 ) ;
#37504 = DIRECTION ( 'NONE',  ( 1.000000000000000000, 0.000000000000000000, 0.000000000000000000 ) ) ;
#37505 = DIRECTION ( 'NONE',  ( 0.000000000000000000, -1.000000000000000000, 0.000000000000000000 ) ) ;
#37506 = VERTEX_POINT ( 'NONE', #106057 ) ;
#37507 = CARTESIAN_POINT ( 'NONE',  ( 23.15000000000000213, 85.60000000001251408, -179.9170766071767389 ) ) ;
#37508 = CIRCLE ( 'NONE', #212298, 0.1000000000000028644 ) ;
#37509 = CIRCLE ( 'NONE', #41623, 0.09999999999999939493 ) ;
#37510 = DIRECTION ( 'NONE',  ( 1.000000000000000000, 0.000000000000000000, 0.000000000000000000 ) ) ;
#37511 = B_SPLINE_CURVE_WITH_KNOTS ( 'NONE', 3,
 ( #73331, #211528, #154163, #54989, #32933, #152872, #228533, #13331, #90268, #207688 ),
 .UNSPECIFIED., .F., .F.,
 ( 4, 3, 3, 4 ),
 ( 0.000000000000000000, 0.0002000000000002886513, 0.001000000000045113023, 0.001967863649472102652 ),
 .UNSPECIFIED. ) ;
#37512 = ORIENTED_EDGE ( 'NONE', *, *, #131462, .T. ) ;
#37513 = CARTESIAN_POINT ( 'NONE',  ( -20.94999999999999929, 12.97363049771892207, -205.3537238898406940 ) ) ;
#37514 = ORIENTED_EDGE ( 'NONE', *, *, #6884, .T. ) ;
#37515 = DIRECTION ( 'NONE',  ( 0.000000000000000000, -1.000000000000000000, -6.982962677686266711E-15 ) ) ;
#37516 = DIRECTION ( 'NONE',  ( 0.000000000000000000, -1.000000000000000000, -6.982962677686265922E-15 ) ) ;
#37517 = CARTESIAN_POINT ( 'NONE',  ( -20.85000000000000142, 87.75000000001216449, -139.4231074845242802 ) ) ;
#37518 = DIRECTION ( 'NONE',  ( 1.000000000000000000, 0.000000000000000000, 0.000000000000000000 ) ) ;
#37519 = CARTESIAN_POINT ( 'NONE',  ( 21.14999999999999858, 6.257814610487280937, -100.4022097086912311 ) ) ;
#37520 = CARTESIAN_POINT ( 'NONE',  ( 21.05000000000254090, 18.87203871602090643, -227.9647184347600160 ) ) ;
#37521 = CARTESIAN_POINT ( 'NONE',  ( -20.94999999999999929, 77.73625713161000306, -191.9544551555068495 ) ) ;
#37522 = DIRECTION ( 'NONE',  ( -0.000000000000000000, -0.8700118002898321601, 0.4930308989875230030 ) ) ;
#37523 = LINE ( 'NONE', #909, #95663 ) ;
#37524 = DIRECTION ( 'NONE',  ( 1.000000000000000000, 0.000000000000000000, 0.000000000000000000 ) ) ;
#37525 = AXIS2_PLACEMENT_3D ( 'NONE', #104709, #60471, #25234 ) ;
#37526 = CARTESIAN_POINT ( 'NONE',  ( 21.06277459767462545, 22.07630317885907800, -231.6739566574008506 ) ) ;
#37528 = DIRECTION ( 'NONE',  ( 0.000000000000000000, -1.000000000000000000, -6.982962677686265922E-15 ) ) ;
#37527 = AXIS2_PLACEMENT_3D ( 'NONE', #237654, #218060, #99398 ) ;
#37530 = LINE ( 'NONE', #55754, #169748 ) ;
#37529 = CIRCLE ( 'NONE', #183264, 2.000000000000001776 ) ;
#37531 = DIRECTION ( 'NONE',  ( -1.000000000000000000, -0.000000000000000000, -0.000000000000000000 ) ) ;
#37532 = DIRECTION ( 'NONE',  ( 0.000000000000000000, 0.000000000000000000, 1.000000000000000000 ) ) ;
#37533 = EDGE_CURVE ( 'NONE', #111529, #157651, #45776, .T. ) ;
#37534 = AXIS2_PLACEMENT_3D ( 'NONE', #217381, #23078, #60882 ) ;
#37535 = VERTEX_POINT ( 'NONE', #42270 ) ;
#37536 = CARTESIAN_POINT ( 'NONE',  ( 21.05000000000000071, 6.540656951701244282, -9.351243737687475743E-16 ) ) ;
#37537 = CARTESIAN_POINT ( 'NONE',  ( -23.15000000000000213, 85.00000000001149658, -45.91707660717669626 ) ) ;
#37538 = DIRECTION ( 'NONE',  ( 0.000000000000000000, -0.9654727137038715545, -0.2605042016806676242 ) ) ;
#37539 = APPLICATION_CONTEXT ( 'automotive_design' ) ;
#37540 = EDGE_CURVE ( 'NONE', #234897, #48993, #1829, .T. ) ;
#37541 = ORIENTED_EDGE ( 'NONE', *, *, #216869, .F. ) ;
#37542 = CARTESIAN_POINT ( 'NONE',  ( -22.39999999999999858, 12.76524917372336709, -223.4223513401831553 ) ) ;
#37543 = AXIS2_PLACEMENT_3D ( 'NONE', #175703, #80390, #141676 ) ;
#37545 = AXIS2_PLACEMENT_3D ( 'NONE', #190266, #192830, #194127 ) ;
#37544 = CARTESIAN_POINT ( 'NONE',  ( -20.94999999999999929, 74.73821383144729680, -161.9366085209788935 ) ) ;
#37546 = ADVANCED_FACE ( 'NONE', ( #245603 ), #97393, .F. ) ;
#37547 = VERTEX_POINT ( 'NONE', #126937 ) ;
#37549 = EDGE_CURVE ( 'NONE', #182139, #149370, #85199, .T. ) ;
#37548 = DIRECTION ( 'NONE',  ( 0.000000000000000000, 0.000000000000000000, -1.000000000000000000 ) ) ;
#37550 = CARTESIAN_POINT ( 'NONE',  ( -20.94999999999999929, 36.52237217006333481, -249.3317055962219229 ) ) ;
#37551 = EDGE_LOOP ( 'NONE', ( #115, #244892, #57062, #165619 ) ) ;
#37552 = ORIENTED_EDGE ( 'NONE', *, *, #75278, .T. ) ;
#37553 = LINE ( 'NONE', #117082, #47855 ) ;
#37554 = ADVANCED_FACE ( 'NONE', ( #160943 ), #201334, .F. ) ;
#37555 = ORIENTED_EDGE ( 'NONE', *, *, #69482, .T. ) ;
#37556 = ADVANCED_FACE ( 'NONE', ( #241742 ), #61833, .T. ) ;
#37557 = CARTESIAN_POINT ( 'NONE',  ( 21.13435531349779239, -1.328411718110899122E-15, 6.493721063592196252 ) ) ;
#37558 = CARTESIAN_POINT ( 'NONE',  ( -16.97683809663752186, 9.950000000011138823, -143.2500000000000284 ) ) ;
#37560 = DIRECTION ( 'NONE',  ( 4.336808689942128965E-15, -0.8660254037844367092, 0.5000000000000037748 ) ) ;
#37559 = UNCERTAINTY_MEASURE_WITH_UNIT (LENGTH_MEASURE( 1.000000000000000082E-05 ), #240756, 'distance_accuracy_value', 'NONE');
#37561 = EDGE_CURVE ( 'NONE', #139380, #202001, #254053, .T. ) ;
#37562 = DIRECTION ( 'NONE',  ( 0.000000000000000000, 0.000000000000000000, -1.000000000000000000 ) ) ;
#37563 = DIRECTION ( 'NONE',  ( 0.000000000000000000, 0.8068669527897009974, 0.5907332058517299478 ) ) ;
#37564 = CARTESIAN_POINT ( 'NONE',  ( -12.93407622233967658, 46.82384836101675063, -234.6777522051880851 ) ) ;
#37565 = FACE_OUTER_BOUND ( 'NONE', #253775, .T. ) ;
#37566 = FACE_OUTER_BOUND ( 'NONE', #44314, .T. ) ;
#37568 = ORIENTED_EDGE ( 'NONE', *, *, #76993, .F. ) ;
#37567 = CARTESIAN_POINT ( 'NONE',  ( -18.50000000000000000, -9.399999999988850163, -40.79725975966329088 ) ) ;
#37569 = ORIENTED_EDGE ( 'NONE', *, *, #54750, .T. ) ;
#37571 = DIRECTION ( 'NONE',  ( 0.000000000000000000, -0.2617529984165152257, -0.9651348961777124202 ) ) ;
#37570 = DIRECTION ( 'NONE',  ( 0.000000000000000000, 0.2617529984165031243, 0.9651348961777157509 ) ) ;
#37573 = ORIENTED_EDGE ( 'NONE', *, *, #189185, .F. ) ;
#37572 = CARTESIAN_POINT ( 'NONE',  ( -18.79999999999999716, 1.250000000000000000, 0.000000000000000000 ) ) ;
#37574 = AXIS2_PLACEMENT_3D ( 'NONE', #188592, #210734, #169079 ) ;
#37575 = ORIENTED_EDGE ( 'NONE', *, *, #123570, .T. ) ;
#37576 = PLANE ( 'NONE',  #149874 ) ;
#37577 = DIRECTION ( 'NONE',  ( 1.000000000000000000, 0.000000000000000000, 0.000000000000000000 ) ) ;
#37578 = EDGE_CURVE ( 'NONE', #120355, #14005, #210442, .T. ) ;
#37579 = CARTESIAN_POINT ( 'NONE',  ( -20.94999999999999929, 4.436385504674529301, -245.3241086753762659 ) ) ;
#37580 = CARTESIAN_POINT ( 'NONE',  ( 18.50000000000000355, -9.421456145495524126, -7.241982084019278787 ) ) ;
#37581 = AXIS2_PLACEMENT_3D ( 'NONE', #42885, #5007, #183685 ) ;
#37582 = DIRECTION ( 'NONE',  ( 1.000000000000000000, -2.849773892568378313E-16, 7.728835255496647986E-17 ) ) ;
#37583 = ADVANCED_FACE ( 'NONE', ( #51215 ), #149084, .F. ) ;
#37584 = ADVANCED_FACE ( 'NONE', ( #228619 ), #72113, .T. ) ;
#37585 = CARTESIAN_POINT ( 'NONE',  ( -22.94999999999999929, -1.885425182446134107, -11.49641995933507843 ) ) ;
#37586 = CARTESIAN_POINT ( 'NONE',  ( -20.54999999999999716, 74.00000000001205080, -123.2984855617622060 ) ) ;
#37587 = DIRECTION ( 'NONE',  ( 0.000000000000000000, 1.000000000000000000, 6.982962677686266711E-15 ) ) ;
#37588 = VERTEX_POINT ( 'NONE', #152957 ) ;
#37589 = ORIENTED_EDGE ( 'NONE', *, *, #12032, .F. ) ;
#37590 = CARTESIAN_POINT ( 'NONE',  ( 21.93642651522410603, 7.159341611308064124, -199.4407717320839879 ) ) ;
#37591 = CIRCLE ( 'NONE', #212379, 0.1000000000000013933 ) ;
#37592 = ORIENTED_EDGE ( 'NONE', *, *, #99960, .F. ) ;
#37593 = CARTESIAN_POINT ( 'NONE',  ( 20.95289811251229750, 8.893168004469753640, -142.5018094939185573 ) ) ;
#37595 = ORIENTED_EDGE ( 'NONE', *, *, #172799, .T. ) ;
#37594 = VECTOR ( 'NONE', #217442, 1000.000000000000000 ) ;
#37596 = FACE_OUTER_BOUND ( 'NONE', #237241, .T. ) ;
#37597 = EDGE_CURVE ( 'NONE', #199454, #9026, #70843, .T. ) ;
#37598 = AXIS2_PLACEMENT_3D ( 'NONE', #20140, #123090, #60517 ) ;
#37599 = CARTESIAN_POINT ( 'NONE',  ( -14.77538296656416072, 49.52260852254784140, -233.4480600891349127 ) ) ;
#37600 = FACE_OUTER_BOUND ( 'NONE', #192363, .T. ) ;
#37601 = ADVANCED_FACE ( 'NONE', ( #189484 ), #92930, .T. ) ;
#37603 = ORIENTED_EDGE ( 'NONE', *, *, #101397, .T. ) ;
#37602 = DIRECTION ( 'NONE',  ( 1.000000000000000000, -0.000000000000000000, -0.000000000000000000 ) ) ;
#37604 = CARTESIAN_POINT ( 'NONE',  ( 21.14999999999999858, 69.35000000001228670, -157.8731074845244109 ) ) ;
#37605 = ORIENTED_EDGE ( 'NONE', *, *, #34578, .T. ) ;
#37606 = TOROIDAL_SURFACE ( 'NONE', #195834, 0.2000000000000000111, 0.1000000000000000056 ) ;
#37607 = CARTESIAN_POINT ( 'NONE',  ( 18.59999999999999076, 1.835341550235567887, -45.05515129256298223 ) ) ;
#37608 = CARTESIAN_POINT ( 'NONE',  ( 21.00000000000000000, 63.35728523183471594, -212.8904317177587870 ) ) ;
#37609 = DIRECTION ( 'NONE',  ( 0.000000000000000000, 0.000000000000000000, -1.000000000000000000 ) ) ;
#37610 = ADVANCED_FACE ( 'NONE', ( #232476 ), #209039, .F. ) ;
#37611 = PLANE ( 'NONE',  #229852 ) ;
#37612 = LINE ( 'NONE', #175842, #94868 ) ;
#37613 = ORIENTED_EDGE ( 'NONE', *, *, #246966, .F. ) ;
#37614 = FACE_OUTER_BOUND ( 'NONE', #131182, .T. ) ;
#37615 = B_SPLINE_CURVE_WITH_KNOTS ( 'NONE', 3,
 ( #154838, #234337, #96101, #55667, #156127, #235618, #116971, #196493, #17854, #97365, #51835, #131390, #210938, #81652, #101207, #238182 ),
 .UNSPECIFIED., .F., .F.,
 ( 4, 3, 3, 3, 3, 4 ),
 ( 0.000000000000000000, 1.810570668010038676E-05, 2.740575833571286165E-05, 4.256816319435689587E-05, 5.213463471024805661E-05, 6.641585710717877651E-05 ),
 .UNSPECIFIED. ) ;
#37616 = VERTEX_POINT ( 'NONE', #53817 ) ;
#37619 = ORIENTED_EDGE ( 'NONE', *, *, #182516, .T. ) ;
#37618 = CARTESIAN_POINT ( 'NONE',  ( -21.44999999999999929, 11.70367352607683564, -220.1991933683510467 ) ) ;
#37617 = CARTESIAN_POINT ( 'NONE',  ( -22.49544290803757107, 64.25012976215539595, -203.5884194437828114 ) ) ;
#37620 = VECTOR ( 'NONE', #244285, 1000.000000000000000 ) ;
#37621 = FACE_OUTER_BOUND ( 'NONE', #113662, .T. ) ;
#37622 = AXIS2_PLACEMENT_3D ( 'NONE', #35587, #129525, #189503 ) ;
#37623 = AXIS2_PLACEMENT_3D ( 'NONE', #251672, #56009, #95170 ) ;
#37624 = VECTOR ( 'NONE', #29115, 1000.000000000000000 ) ;
#37625 = AXIS2_PLACEMENT_3D ( 'NONE', #17234, #101862, #219257 ) ;
#37626 = PLANE ( 'NONE',  #233513 ) ;
#37627 = VERTEX_POINT ( 'NONE', #48672 ) ;
#37628 = FACE_OUTER_BOUND ( 'NONE', #64729, .T. ) ;
#37629 = CARTESIAN_POINT ( 'NONE',  ( 21.05000000000000071, 0.000000000000000000, 4.300000000000032685 ) ) ;
#37631 = VERTEX_POINT ( 'NONE', #108652 ) ;
#37630 = DIRECTION ( 'NONE',  ( -1.000000000000000000, -0.000000000000000000, -0.000000000000000000 ) ) ;
#37632 = EDGE_CURVE ( 'NONE', #17556, #110910, #112610, .T. ) ;
#37633 = LINE ( 'NONE', #157605, #168567 ) ;
#37634 = VECTOR ( 'NONE', #215017, 1000.000000000000000 ) ;
#37635 = ORIENTED_EDGE ( 'NONE', *, *, #237862, .T. ) ;
#37636 = EDGE_CURVE ( 'NONE', #54157, #191015, #58400, .T. ) ;
#37637 = CARTESIAN_POINT ( 'NONE',  ( -20.94999999999999929, 7.070967871809997973, -204.7465642218682547 ) ) ;
#37638 = FACE_OUTER_BOUND ( 'NONE', #154613, .T. ) ;
#37639 = FACE_OUTER_BOUND ( 'NONE', #93, .T. ) ;
#37640 = ORIENTED_EDGE ( 'NONE', *, *, #205750, .T. ) ;
#37641 = CARTESIAN_POINT ( 'NONE',  ( 20.94999999999999574, 77.73625713160897988, -57.95445515550681392 ) ) ;
#37642 = VERTEX_POINT ( 'NONE', #133362 ) ;
#37643 = DIRECTION ( 'NONE',  ( 1.000000000000000000, 0.000000000000000000, 0.000000000000000000 ) ) ;
#37644 = EDGE_CURVE ( 'NONE', #82553, #253318, #37798, .T. ) ;
#37645 = EDGE_CURVE ( 'NONE', #46758, #198608, #141807, .T. ) ;
#37646 = DIRECTION ( 'NONE',  ( 3.469446951953634384E-14, -0.8814952561688430555, 0.4721928772777346239 ) ) ;
#37647 = CARTESIAN_POINT ( 'NONE',  ( -21.44999999999999929, 68.75000000001230660, -157.6731074845243938 ) ) ;
#37648 = ORIENTED_EDGE ( 'NONE', *, *, #61717, .T. ) ;
#37649 = FACE_OUTER_BOUND ( 'NONE', #93974, .T. ) ;
#37650 = EDGE_CURVE ( 'NONE', #190860, #154754, #4440, .T. ) ;
#37651 = AXIS2_PLACEMENT_3D ( 'NONE', #31559, #94051, #172365 ) ;
#37652 = DIRECTION ( 'NONE',  ( 0.000000000000000000, -0.8660254037844377084, -0.5000000000000016653 ) ) ;
#37653 = DIRECTION ( 'NONE',  ( 0.000000000000000000, -1.000000000000000000, 0.000000000000000000 ) ) ;
#37654 = CIRCLE ( 'NONE', #245929, 4.000000000000003553 ) ;
#37655 = ORIENTED_EDGE ( 'NONE', *, *, #75139, .F. ) ;
#37656 = CARTESIAN_POINT ( 'NONE',  ( -5.900000000000002132, -11.25000000000000000, 13.90000000000000213 ) ) ;
#37657 = CARTESIAN_POINT ( 'NONE',  ( 23.24999999999999289, 64.35000000001228670, -157.8731074845244393 ) ) ;
#37658 = DIRECTION ( 'NONE',  ( 0.000000000000000000, -1.000000000000000000, 0.000000000000000000 ) ) ;
#37659 = AXIS2_PLACEMENT_3D ( 'NONE', #92282, #109271, #229249 ) ;
#37660 = ADVANCED_FACE ( 'NONE', ( #132072 ), #208486, .T. ) ;
#37661 = ORIENTED_EDGE ( 'NONE', *, *, #83808, .T. ) ;
#37662 = EDGE_CURVE ( 'NONE', #162824, #87320, #233431, .T. ) ;
#37663 = DIRECTION ( 'NONE',  ( 0.000000000000000000, 0.000000000000000000, -1.000000000000000000 ) ) ;
#37664 = ORIENTED_EDGE ( 'NONE', *, *, #79637, .F. ) ;
#37666 = ORIENTED_EDGE ( 'NONE', *, *, #207799, .F. ) ;
#37665 = CARTESIAN_POINT ( 'NONE',  ( -20.00857864376270001, 9.350000000011156942, -88.15000000000004832 ) ) ;
#37667 = EDGE_CURVE ( 'NONE', #139340, #49350, #155, .T. ) ;
#37668 = AXIS2_PLACEMENT_3D ( 'NONE', #186988, #128280, #106110 ) ;
#37671 = ORIENTED_EDGE ( 'NONE', *, *, #116113, .F. ) ;
#37670 = ORIENTED_EDGE ( 'NONE', *, *, #70126, .T. ) ;
#37669 = DIRECTION ( 'NONE',  ( 0.000000000000000000, 6.982962677686266711E-15, -1.000000000000000000 ) ) ;
#37672 = AXIS2_PLACEMENT_3D ( 'NONE', #173059, #252533, #73945 ) ;
#37673 = DIRECTION ( 'NONE',  ( 0.000000000000000000, -0.000000000000000000, 1.000000000000000000 ) ) ;
#37674 = CARTESIAN_POINT ( 'NONE',  ( -21.08884785362073089, 0.04978309507788075683, -161.1428066325743487 ) ) ;
#37675 = CARTESIAN_POINT ( 'NONE',  ( -18.59999999999999787, 64.40000000001234071, -163.0949042542488883 ) ) ;
#37676 = CARTESIAN_POINT ( 'NONE',  ( -16.80070461187888498, 12.41338732702360659, -211.2399223222487308 ) ) ;
#37677 = CARTESIAN_POINT ( 'NONE',  ( -21.05000000000000071, 77.25000000001263345, -195.5231074845243313 ) ) ;
#37678 = EDGE_CURVE ( 'NONE', #212402, #50885, #211616, .T. ) ;
#37679 = CIRCLE ( 'NONE', #125156, 0.09999999999998898659 ) ;
#37680 = VECTOR ( 'NONE', #39016, 1000.000000000000000 ) ;
#37681 = DIRECTION ( 'NONE',  ( 0.000000000000000000, -1.000000000000000000, 0.000000000000000000 ) ) ;
#37683 = CARTESIAN_POINT ( 'NONE',  ( -23.25000000000000000, 25.94586868676353575, -241.5435999122864530 ) ) ;
#37682 = CARTESIAN_POINT ( 'NONE',  ( -20.85000000000000497, 17.13730476842946615, -224.4716215546871467 ) ) ;
#37684 = ORIENTED_EDGE ( 'NONE', *, *, #243685, .F. ) ;
#37686 = ORIENTED_EDGE ( 'NONE', *, *, #104860, .F. ) ;
#37685 = AXIS2_PLACEMENT_3D ( 'NONE', #36084, #19067, #215969 ) ;
#37687 = ORIENTED_EDGE ( 'NONE', *, *, #236033, .F. ) ;
#37688 = EDGE_CURVE ( 'NONE', #238213, #247693, #91760, .T. ) ;
#37689 = DIRECTION ( 'NONE',  ( 0.000000000000000000, -1.000000000000000000, -0.000000000000000000 ) ) ;
#37691 = EDGE_LOOP ( 'NONE', ( #136654, #34292, #218971, #158657 ) ) ;
#37690 = CARTESIAN_POINT ( 'NONE',  ( 23.25000000000000000, 41.42187432231295219, -260.1830396872097140 ) ) ;
#37692 = LINE ( 'NONE', #195486, #171583 ) ;
#37693 = ORIENTED_EDGE ( 'NONE', *, *, #160356, .F. ) ;
#37694 = DIRECTION ( 'NONE',  ( -1.000000000000000000, 0.000000000000000000, 0.000000000000000000 ) ) ;
#37695 = ORIENTED_EDGE ( 'NONE', *, *, #134953, .F. ) ;
#37696 = EDGE_CURVE ( 'NONE', #134779, #126467, #94214, .T. ) ;
#37697 = CARTESIAN_POINT ( 'NONE',  ( 21.00000000000000000, 9.750000000011153745, -146.3500000000000227 ) ) ;
#37698 = EDGE_CURVE ( 'NONE', #173665, #65394, #96759, .T. ) ;
#37699 = ORIENTED_EDGE ( 'NONE', *, *, #209753, .F. ) ;
#37700 = CIRCLE ( 'NONE', #54226, 0.09999999999999939493 ) ;
#37701 = AXIS2_PLACEMENT_3D ( 'NONE', #60028, #114884, #177458 ) ;
#37702 = DIRECTION ( 'NONE',  ( 1.000000000000000000, 0.000000000000000000, 0.000000000000000000 ) ) ;
#37703 = DIRECTION ( 'NONE',  ( 0.000000000000000000, 0.000000000000000000, -1.000000000000000000 ) ) ;
#37705 = VERTEX_POINT ( 'NONE', #95505 ) ;
#37704 = ORIENTED_EDGE ( 'NONE', *, *, #119658, .T. ) ;
#37706 = ORIENTED_EDGE ( 'NONE', *, *, #149888, .T. ) ;
#37707 = FACE_OUTER_BOUND ( 'NONE', #97001, .T. ) ;
#37708 = ORIENTED_EDGE ( 'NONE', *, *, #86373, .T. ) ;
#37709 = ORIENTED_EDGE ( 'NONE', *, *, #248273, .T. ) ;
#37710 = DIRECTION ( 'NONE',  ( 0.000000000000000000, 0.9915357197604973694, -0.1298341882519105928 ) ) ;
#37712 = ORIENTED_EDGE ( 'NONE', *, *, #75035, .T. ) ;
#37711 = DIRECTION ( 'NONE',  ( 0.000000000000000000, 0.000000000000000000, -1.000000000000000000 ) ) ;
#37713 = EDGE_CURVE ( 'NONE', #152046, #194536, #121004, .T. ) ;
#37715 = CARTESIAN_POINT ( 'NONE',  ( -23.15000000000000213, 7.128833340094563376, -233.7327013124401276 ) ) ;
#37714 = DIRECTION ( 'NONE',  ( 0.000000000000000000, 0.2617529984165031243, 0.9651348961777157509 ) ) ;
#37716 = CARTESIAN_POINT ( 'NONE',  ( -23.25000000000000000, -11.74999999998884448, -67.00000000000004263 ) ) ;
#37717 = DIRECTION ( 'NONE',  ( -1.000000000000000000, 0.000000000000000000, 0.000000000000000000 ) ) ;
#37718 = CARTESIAN_POINT ( 'NONE',  ( 21.30000000000002558, 1.115600667400684642E-11, -100.5000000000000284 ) ) ;
#37719 = VERTEX_POINT ( 'NONE', #113783 ) ;
#37720 = VERTEX_POINT ( 'NONE', #175099 ) ;
#37721 = CARTESIAN_POINT ( 'NONE',  ( 18.44208962362753468, 85.55234049691941323, -96.18093442906038604 ) ) ;
#37723 = VECTOR ( 'NONE', #188591, 1000.000000000000000 ) ;
#37722 = DIRECTION ( 'NONE',  ( 0.000000000000000000, 0.000000000000000000, 1.000000000000000000 ) ) ;
#37724 = CYLINDRICAL_SURFACE ( 'NONE', #82987, 0.1000000000000078187 ) ;
#37725 = TOROIDAL_SURFACE ( 'NONE', #183449, 11.70000000000000462, 0.1000000000000000056 ) ;
#37726 = CIRCLE ( 'NONE', #8483, 0.09999999999999939493 ) ;
#37727 = ORIENTED_EDGE ( 'NONE', *, *, #149771, .T. ) ;
#37728 = PLANE ( 'NONE',  #140326 ) ;
#37729 = CARTESIAN_POINT ( 'NONE',  ( -16.93294127766158752, 51.67000402742814202, -231.8651761569155099 ) ) ;
#37730 = VECTOR ( 'NONE', #171284, 1000.000000000000000 ) ;
#37731 = CARTESIAN_POINT ( 'NONE',  ( -14.11697426661281440, 12.43282705614461747, -213.6439690125878315 ) ) ;
#37732 = ORIENTED_EDGE ( 'NONE', *, *, #36772, .T. ) ;
#37733 = ORIENTED_EDGE ( 'NONE', *, *, #150856, .T. ) ;
#37734 = SPHERICAL_SURFACE ( 'NONE', #88537, 0.1000000000000000056 ) ;
#37735 = EDGE_CURVE ( 'NONE', #255664, #60411, #16001, .T. ) ;
#37736 = DIRECTION ( 'NONE',  ( -2.940209281316621016E-16, -1.000000000000000000, -9.408669700213187250E-15 ) ) ;
#37737 = ORIENTED_EDGE ( 'NONE', *, *, #110029, .T. ) ;
#37738 = DIRECTION ( 'NONE',  ( -0.000000000000000000, 1.000000000000000000, -0.000000000000000000 ) ) ;
#37739 = ORIENTED_EDGE ( 'NONE', *, *, #53736, .F. ) ;
#37740 = CARTESIAN_POINT ( 'NONE',  ( -18.59999999999999787, 8.882751598337863541, -187.0399955572217721 ) ) ;
#37741 = LINE ( 'NONE', #23314, #58144 ) ;
#37743 = CARTESIAN_POINT ( 'NONE',  ( -20.89878130938411616, 68.09900309800710261, -224.1499508721967970 ) ) ;
#37742 = CARTESIAN_POINT ( 'NONE',  ( 20.94999999999999574, 1.736257131608553550, -78.56865232901755292 ) ) ;
#37744 = AXIS2_PLACEMENT_3D ( 'NONE', #101903, #203599, #139748 ) ;
#37745 = DIRECTION ( 'NONE',  ( -1.000000000000000000, 0.000000000000000000, -0.000000000000000000 ) ) ;
#37746 = LINE ( 'NONE', #256717, #44259 ) ;
#37747 = ADVANCED_FACE ( 'NONE', ( #215452 ), #66811, .T. ) ;
#37748 = B_SPLINE_CURVE_WITH_KNOTS ( 'NONE', 3,
 ( #58527, #252892, #13032, #194239, #35178, #37729, #196762, #177246, #114674, #211205, #256696, #32610, #53414, #112129, #15606, #132970 ),
 .UNSPECIFIED., .F., .F.,
 ( 4, 3, 3, 3, 3, 4 ),
 ( 0.000000000000000000, 1.810570668010520807E-05, 2.740575833571303106E-05, 4.256816319437020446E-05, 5.213463471026028777E-05, 6.641585710718293713E-05 ),
 .UNSPECIFIED. ) ;
#37750 = ORIENTED_EDGE ( 'NONE', *, *, #152780, .T. ) ;
#37749 = ORIENTED_EDGE ( 'NONE', *, *, #13618, .T. ) ;
#37751 = ORIENTED_EDGE ( 'NONE', *, *, #64005, .T. ) ;
#37752 = DIRECTION ( 'NONE',  ( 1.000000000000000000, 0.000000000000000000, 0.000000000000000000 ) ) ;
#37753 = CARTESIAN_POINT ( 'NONE',  ( -16.79814274880124358, 60.94069671524907505, -221.0395699407627887 ) ) ;
#37754 = DIRECTION ( 'NONE',  ( 0.000000000000000000, 0.000000000000000000, -1.000000000000000000 ) ) ;
#37755 = FACE_BOUND ( 'NONE', #165345, .T. ) ;
#37756 = AXIS2_PLACEMENT_3D ( 'NONE', #177975, #121851, #198799 ) ;
#37758 = CARTESIAN_POINT ( 'NONE',  ( -12.93407622233968723, 66.58221053305966564, -87.66572294054749648 ) ) ;
#37757 = CARTESIAN_POINT ( 'NONE',  ( 20.75572585718224872, 8.882316728398945926, -8.497258398706687643 ) ) ;
#37759 = CARTESIAN_POINT ( 'NONE',  ( -16.87372397896796272, 66.11940046336980004, -49.17238297448864870 ) ) ;
#37760 = ORIENTED_EDGE ( 'NONE', *, *, #225671, .T. ) ;
#37761 = CARTESIAN_POINT ( 'NONE',  ( 20.12500000000000000, 9.750000000011153745, -75.11177128211431864 ) ) ;
#37762 = ORIENTED_EDGE ( 'NONE', *, *, #58711, .T. ) ;
#37763 = ORIENTED_EDGE ( 'NONE', *, *, #153591, .F. ) ;
#37764 = CYLINDRICAL_SURFACE ( 'NONE', #154405, 0.09999999999999939493 ) ;
#37765 = AXIS2_PLACEMENT_3D ( 'NONE', #59548, #4725, #127267 ) ;
#37766 = CYLINDRICAL_SURFACE ( 'NONE', #176677, 0.09999999999999939493 ) ;
#37767 = DIRECTION ( 'NONE',  ( 1.000000000000000000, -2.952720810173289112E-16, -2.061873921506763405E-30 ) ) ;
#37768 = CARTESIAN_POINT ( 'NONE',  ( 22.39999999999999503, 76.00000000001273293, -211.3138870828977360 ) ) ;
#37769 = AXIS2_PLACEMENT_3D ( 'NONE', #215844, #257498, #37252 ) ;
#37770 = DIRECTION ( 'NONE',  ( -4.282643121434362058E-15, 0.9875102702516478370, 0.1575546449569727447 ) ) ;
#37771 = VERTEX_POINT ( 'NONE', #254550 ) ;
#37772 = VERTEX_POINT ( 'NONE', #238875 ) ;
#37773 = CARTESIAN_POINT ( 'NONE',  ( -21.03571358705787020, 11.75000000001115197, -40.32510682205884933 ) ) ;
#37774 = VECTOR ( 'NONE', #225972, 1000.000000000000000 ) ;
#37775 = DIRECTION ( 'NONE',  ( -1.000000000000000000, 0.000000000000000000, 0.000000000000000000 ) ) ;
#37776 = EDGE_LOOP ( 'NONE', ( #254551, #63318, #55210, #219016, #73505 ) ) ;
#37777 = CARTESIAN_POINT ( 'NONE',  ( -16.97092634996494454, 22.98459280967489704, -230.8808285843816464 ) ) ;
#37778 = CARTESIAN_POINT ( 'NONE',  ( -21.05000000000000071, 46.54514716347711101, -243.1111603596801842 ) ) ;
#37779 = DIRECTION ( 'NONE',  ( -3.265361837132813093E-16, 1.000000000000000000, 0.000000000000000000 ) ) ;
#37780 = DIRECTION ( 'NONE',  ( 0.000000000000000000, 6.982962677686266711E-15, -1.000000000000000000 ) ) ;
#37781 = CARTESIAN_POINT ( 'NONE',  ( 21.13461538461538325, 65.38541703798632909, -90.67310748452437963 ) ) ;
#37783 = CARTESIAN_POINT ( 'NONE',  ( 21.05000000000000071, 74.65091558138487926, -95.03660852097883094 ) ) ;
#37782 = CARTESIAN_POINT ( 'NONE',  ( -18.50000000000000000, 74.83729825007462466, -195.4231074845243654 ) ) ;
#37785 = ADVANCED_FACE ( 'NONE', ( #60220 ), #34287, .F. ) ;
#37784 = CYLINDRICAL_SURFACE ( 'NONE', #195705, 0.5000000000000004441 ) ;
#37786 = DIRECTION ( 'NONE',  ( 1.000000000000000000, 0.000000000000000000, 0.000000000000000000 ) ) ;
#37787 = CARTESIAN_POINT ( 'NONE',  ( 21.30000000000002558, 76.00000000001264766, -199.4731074845243484 ) ) ;
#37788 = CARTESIAN_POINT ( 'NONE',  ( 21.09813707148777340, 69.61493789427618140, -203.5544589840539231 ) ) ;
#37789 = VECTOR ( 'NONE', #251101, 1000.000000000000114 ) ;
#37791 = ORIENTED_EDGE ( 'NONE', *, *, #189869, .T. ) ;
#37790 = CARTESIAN_POINT ( 'NONE',  ( -16.87036670365548474, 9.989418819312799513, -54.47956011730205006 ) ) ;
#37792 = AXIS2_PLACEMENT_3D ( 'NONE', #138863, #55473, #157216 ) ;
#37793 = VECTOR ( 'NONE', #150464, 1000.000000000000000 ) ;
#37794 = AXIS2_PLACEMENT_3D ( 'NONE', #67929, #129199, #108353 ) ;
#37795 = ADVANCED_FACE ( 'NONE', ( #14720 ), #233751, .T. ) ;
#37796 = CARTESIAN_POINT ( 'NONE',  ( -20.85000000000000142, -1.835859311432481045, -78.50443916879852679 ) ) ;
#37797 = EDGE_LOOP ( 'NONE', ( #119108, #91543, #38905, #178264 ) ) ;
#37798 = CIRCLE ( 'NONE', #129346, 0.09999999999999939493 ) ;
#37799 = AXIS2_PLACEMENT_3D ( 'NONE', #75110, #191205, #52938 ) ;
#37800 = EDGE_CURVE ( 'NONE', #126560, #216334, #235031, .T. ) ;
#37801 = CARTESIAN_POINT ( 'NONE',  ( -20.85000000000000142, -1.164121893230052995, -74.91484808557160591 ) ) ;
#37802 = DIRECTION ( 'NONE',  ( -0.000000000000000000, -6.982962677686266711E-15, 1.000000000000000000 ) ) ;
#37803 = ORIENTED_EDGE ( 'NONE', *, *, #177821, .T. ) ;
#37804 = CARTESIAN_POINT ( 'NONE',  ( -12.25000000000000178, 13.18880795147152440, -215.2702608532411830 ) ) ;
#37805 = DIRECTION ( 'NONE',  ( 0.000000000000000000, 6.982962677686266711E-15, -1.000000000000000000 ) ) ;
#37806 = DIRECTION ( 'NONE',  ( -1.000000000000000000, 0.000000000000000000, -0.000000000000000000 ) ) ;
#37807 = ADVANCED_FACE ( 'NONE', ( #216733 ), #156800, .T. ) ;
#37808 = TOROIDAL_SURFACE ( 'NONE', #208494, 2.100000000000002309, 0.1000000000000000056 ) ;
#37809 = DIRECTION ( 'NONE',  ( -1.000000000000000000, -0.000000000000000000, -0.000000000000000000 ) ) ;
#37810 = CIRCLE ( 'NONE', #162896, 0.09999999999999939493 ) ;
#37811 = CARTESIAN_POINT ( 'NONE',  ( 18.49999999999999289, 10.49142135623730709, -24.85000000000000142 ) ) ;
#37812 = CARTESIAN_POINT ( 'NONE',  ( 23.24999999999999645, 71.00000000001205080, -124.1178414656112352 ) ) ;
#37813 = AXIS2_PLACEMENT_3D ( 'NONE', #96412, #196804, #231147 ) ;
#37814 = TOROIDAL_SURFACE ( 'NONE', #191940, 0.6000000000000009770, 0.1000000000000000056 ) ;
#37815 = EDGE_CURVE ( 'NONE', #165316, #224878, #162674, .T. ) ;
#37816 = ORIENTED_EDGE ( 'NONE', *, *, #217683, .F. ) ;
#37817 = CARTESIAN_POINT ( 'NONE',  ( 21.13461538461538325, 12.99955419111918253, -210.8083363671015604 ) ) ;
#37819 = ORIENTED_EDGE ( 'NONE', *, *, #94872, .F. ) ;
#37818 = DIRECTION ( 'NONE',  ( 0.000000000000000000, 0.000000000000000000, 1.000000000000000000 ) ) ;
#37820 = CARTESIAN_POINT ( 'NONE',  ( 21.30000000000002558, 76.00000000001270450, -207.5731074845243427 ) ) ;
#37821 = CARTESIAN_POINT ( 'NONE',  ( 23.15000000000000213, 86.43238724539048690, -209.5644480942280836 ) ) ;
#37822 = ADVANCED_FACE ( 'NONE', ( #135898 ), #217998, .T. ) ;
#37823 = DIRECTION ( 'NONE',  ( 2.952720810173289605E-16, 1.000000000000000000, 7.086529944415894657E-15 ) ) ;
#37824 = ORIENTED_EDGE ( 'NONE', *, *, #251905, .F. ) ;
#37825 = PLANE ( 'NONE',  #255249 ) ;
#37826 = SHAPE_DEFINITION_REPRESENTATION ( #232711, #171686 ) ;
#37827 = AXIS2_PLACEMENT_3D ( 'NONE', #62375, #160213, #21972 ) ;
#37828 = DIRECTION ( 'NONE',  ( 0.000000000000000000, 6.982962677686266711E-15, -1.000000000000000000 ) ) ;
#37830 = ADVANCED_FACE ( 'NONE', ( #134612 ), #133452, .T. ) ;
#37829 = DIRECTION ( 'NONE',  ( 0.000000000000000000, 0.000000000000000000, 1.000000000000000000 ) ) ;
#37831 = ORIENTED_EDGE ( 'NONE', *, *, #179036, .F. ) ;
#37832 = DIRECTION ( 'NONE',  ( 1.000000000000000000, 0.000000000000000000, 0.000000000000000000 ) ) ;
#37833 = CARTESIAN_POINT ( 'NONE',  ( -18.40000000000000213, 15.50909414388701890, -218.9610367925635330 ) ) ;
#37834 = DIRECTION ( 'NONE',  ( 0.000000000000000000, -0.8660254037844383745, 0.5000000000000003331 ) ) ;
#37835 = ORIENTED_EDGE ( 'NONE', *, *, #41119, .F. ) ;
#37836 = ORIENTED_EDGE ( 'NONE', *, *, #193503, .F. ) ;
#37837 = DIRECTION ( 'NONE',  ( -0.000000000000000000, -1.000000000000000000, -6.982962677686266711E-15 ) ) ;
#37838 = CARTESIAN_POINT ( 'NONE',  ( 20.04999999999999716, 67.25000000001155342, -56.87310748452438247 ) ) ;
#37839 = CIRCLE ( 'NONE', #45996, 0.2000000000000057288 ) ;
#37840 = ADVANCED_FACE ( 'NONE', ( #214177 ), #36855, .T. ) ;
#37841 = DIRECTION ( 'NONE',  ( -1.000000000000000000, -2.952720810173289112E-16, 0.000000000000000000 ) ) ;
#37842 = DIRECTION ( 'NONE',  ( 0.000000000000000000, -1.000000000000000000, -7.272083257015735086E-15 ) ) ;
#37843 = CARTESIAN_POINT ( 'NONE',  ( -20.54999999999999716, 4.350000000011156054, -121.6500000000000341 ) ) ;
#37844 = DIRECTION ( 'NONE',  ( 1.000000000000000000, 0.000000000000000000, -0.000000000000000000 ) ) ;
#37845 = CARTESIAN_POINT ( 'NONE',  ( 20.93975676684922504, 65.68895814178191017, -30.50265578621382190 ) ) ;
#37846 = CARTESIAN_POINT ( 'NONE',  ( -18.59999999999999787, 69.01799029515598249, -166.3269553662681233 ) ) ;
#37847 = CARTESIAN_POINT ( 'NONE',  ( 20.94999999999999929, 1.115600667400684642E-11, -167.4999999999999716 ) ) ;
#37848 = DIRECTION ( 'NONE',  ( -1.000000000000000000, 0.000000000000000000, 0.000000000000000000 ) ) ;
#37849 = ORIENTED_EDGE ( 'NONE', *, *, #139456, .F. ) ;
#37850 = AXIS2_PLACEMENT_3D ( 'NONE', #71015, #250895, #193521 ) ;
#37851 = VERTEX_POINT ( 'NONE', #137199 ) ;
#37852 = DIRECTION ( 'NONE',  ( 0.000000000000000000, 0.1332476588733589040, 0.9910827722268048534 ) ) ;
#37853 = CARTESIAN_POINT ( 'NONE',  ( 21.05000000000000071, 68.22930980752001062, -227.7331931781284879 ) ) ;
#37855 = CARTESIAN_POINT ( 'NONE',  ( 21.14999999999999858, 1.115600667400684642E-11, -100.5000000000000284 ) ) ;
#37854 = CARTESIAN_POINT ( 'NONE',  ( 21.08198257630413508, 69.66340326599659249, -69.59575080830897775 ) ) ;
#37856 = EDGE_CURVE ( 'NONE', #138330, #226447, #116871, .T. ) ;
#37857 = CIRCLE ( 'NONE', #112656, 0.1999999999999985401 ) ;
#37858 = CARTESIAN_POINT ( 'NONE',  ( 23.24999999999999645, 11.75000000001113953, -154.8500000000000227 ) ) ;
#37859 = CARTESIAN_POINT ( 'NONE',  ( 12.60873083341396850, 12.96612044530440677, -216.4114274690425361 ) ) ;
#37860 = ORIENTED_EDGE ( 'NONE', *, *, #40124, .F. ) ;
#37861 = VERTEX_POINT ( 'NONE', #178937 ) ;
#37862 = AXIS2_PLACEMENT_3D ( 'NONE', #143523, #159263, #198366 ) ;
#37863 = CARTESIAN_POINT ( 'NONE',  ( -16.97683809663752186, 66.15000000001158753, -56.12074346632790878 ) ) ;
#37864 = EDGE_LOOP ( 'NONE', ( #102482, #183876, #116941, #249431 ) ) ;
#37865 = EDGE_CURVE ( 'NONE', #221, #168716, #249, .T. ) ;
#37866 = CARTESIAN_POINT ( 'NONE',  ( -23.15000000000000213, 71.65000000001222702, -148.8731074845244109 ) ) ;
#37867 = CIRCLE ( 'NONE', #183588, 0.09999999999998862577 ) ;
#37868 = EDGE_CURVE ( 'NONE', #84341, #185932, #137694, .T. ) ;
#37869 = CIRCLE ( 'NONE', #145986, 0.1000000000000000472 ) ;
#37870 = CARTESIAN_POINT ( 'NONE',  ( 18.43466021071409600, 85.49419069046793140, -29.40604592439644094 ) ) ;
#37871 = AXIS2_PLACEMENT_3D ( 'NONE', #58436, #36361, #74219 ) ;
#37872 = VERTEX_POINT ( 'NONE', #220599 ) ;
#37873 = FACE_OUTER_BOUND ( 'NONE', #150366, .T. ) ;
#37874 = EDGE_CURVE ( 'NONE', #117062, #102375, #204343, .T. ) ;
#37875 = VERTEX_POINT ( 'NONE', #141062 ) ;
#37876 = CARTESIAN_POINT ( 'NONE',  ( -18.52139480978223318, 85.48135884507924231, -162.9985509174052538 ) ) ;
#37877 = CARTESIAN_POINT ( 'NONE',  ( -18.59999999999999787, 16.60731133254646963, -240.9277311905271688 ) ) ;
#37878 = DIRECTION ( 'NONE',  ( 0.000000000000000000, 1.000000000000000000, 0.000000000000000000 ) ) ;
#37879 = ADVANCED_FACE ( 'NONE', ( #41975 ), #8551, .F. ) ;
#37880 = CYLINDRICAL_SURFACE ( 'NONE', #233252, 0.09999999999999939493 ) ;
#37881 = ADVANCED_FACE ( 'NONE', ( #142326 ), #203594, .T. ) ;
#37882 = CARTESIAN_POINT ( 'NONE',  ( -16.89020380669787258, 9.949999999999985079, -12.75741114811056853 ) ) ;
#37884 = CARTESIAN_POINT ( 'NONE',  ( 18.50211644919734866, 65.69792220476341527, -131.0335554128461695 ) ) ;
#37883 = DIRECTION ( 'NONE',  ( 0.000000000000000000, -0.9908441862701783398, 0.1350103645450536627 ) ) ;
#37885 = CARTESIAN_POINT ( 'NONE',  ( -20.64999999999999858, 2.326828918379974323E-16, -31.59999999999999787 ) ) ;
#37886 = ORIENTED_EDGE ( 'NONE', *, *, #199225, .F. ) ;
#37888 = CARTESIAN_POINT ( 'NONE',  ( -16.81931177881022421, 66.06300394050809643, -115.7498896059071853 ) ) ;
#37887 = CARTESIAN_POINT ( 'NONE',  ( -18.58735405345343850, 38.15589195147379087, -261.2056054829760683 ) ) ;
#37889 = ORIENTED_EDGE ( 'NONE', *, *, #185399, .F. ) ;
#37891 = ORIENTED_EDGE ( 'NONE', *, *, #86453, .T. ) ;
#37890 = CYLINDRICAL_SURFACE ( 'NONE', #235672, 0.1000000000000124678 ) ;
#37892 = ORIENTED_EDGE ( 'NONE', *, *, #233641, .F. ) ;
#37893 = CARTESIAN_POINT ( 'NONE',  ( 18.50000000000000000, 77.13860723519891849, -241.8264964602988982 ) ) ;
#37894 = LINE ( 'NONE', #100382, #25935 ) ;
#37895 = CARTESIAN_POINT ( 'NONE',  ( -18.59999999999999787, 43.21392023178790964, -245.1418509714632421 ) ) ;
#37896 = ADVANCED_FACE ( 'NONE', ( #125349 ), #22414, .T. ) ;
#37897 = CARTESIAN_POINT ( 'NONE',  ( -18.44085059012131822, 20.72804496316922851, -227.9555157940418439 ) ) ;
#37898 = ORIENTED_EDGE ( 'NONE', *, *, #98231, .T. ) ;
#37899 = DIRECTION ( 'NONE',  ( 0.000000000000000000, 0.8660254037844482555, 0.4999999999999837907 ) ) ;
#37900 = PRESENTATION_STYLE_ASSIGNMENT (( #216508 ) ) ;
#37901 = CARTESIAN_POINT ( 'NONE',  ( 22.48660254037844197, 64.35000000001267040, -203.5731074845244564 ) ) ;
#37902 = ORIENTED_EDGE ( 'NONE', *, *, #138928, .T. ) ;
#37903 = CARTESIAN_POINT ( 'NONE',  ( 20.94999999999999929, 70.50000000001199396, -115.4283735034374274 ) ) ;
#37904 = CIRCLE ( 'NONE', #116990, 0.09999999999998898659 ) ;
#37905 = TOROIDAL_SURFACE ( 'NONE', #41993, 11.89999999999999858, 0.1000000000000000056 ) ;
#37906 = CIRCLE ( 'NONE', #92595, 11.64999999999999325 ) ;
#37908 = CIRCLE ( 'NONE', #192030, 0.09999999999999248379 ) ;
#37907 = DIRECTION ( 'NONE',  ( 0.000000000000000000, 0.9126074666063769270, 0.4088369013363280513 ) ) ;
#37909 = VERTEX_POINT ( 'NONE', #199770 ) ;
#37910 = EDGE_LOOP ( 'NONE', ( #42618, #130167, #168519, #202299 ) ) ;
#37911 = CARTESIAN_POINT ( 'NONE',  ( -23.15000000000000213, 68.76204065042992397, -214.3562485088912126 ) ) ;
#37912 = ORIENTED_EDGE ( 'NONE', *, *, #186669, .T. ) ;
#37913 = TOROIDAL_SURFACE ( 'NONE', #146206, 11.90000000000000213, 0.1000000000000000056 ) ;
#37914 = CARTESIAN_POINT ( 'NONE',  ( 23.14999999999999858, 7.128833340094563376, -233.7327013124401276 ) ) ;
#37915 = ORIENTED_EDGE ( 'NONE', *, *, #157840, .T. ) ;
#37916 = CARTESIAN_POINT ( 'NONE',  ( 20.94983749550516450, 10.29766095125295244, -172.9743663933275855 ) ) ;
#37917 = EDGE_CURVE ( 'NONE', #19773, #125918, #122794, .T. ) ;
#37918 = CARTESIAN_POINT ( 'NONE',  ( -18.40000000000000213, 11.47867410001105526, -191.7253067836593630 ) ) ;
#37919 = CARTESIAN_POINT ( 'NONE',  ( 21.14999999999999858, 69.45934304831143891, -203.5231074845243882 ) ) ;
#37920 = EDGE_CURVE ( 'NONE', #22410, #135145, #75202, .T. ) ;
#37921 = CARTESIAN_POINT ( 'NONE',  ( 20.95483826173900255, 60.90159005582668073, -225.2834546194827965 ) ) ;
#37922 = AXIS2_PLACEMENT_3D ( 'NONE', #18244, #235993, #131764 ) ;
#37923 = ADVANCED_FACE ( 'NONE', ( #105749 ), #202312, .F. ) ;
#37924 = CARTESIAN_POINT ( 'NONE',  ( -23.15000000000000213, 87.48912529308822172, -139.6231074845242688 ) ) ;
#37925 = CARTESIAN_POINT ( 'NONE',  ( 18.49999999999999289, 69.55000000001199112, -115.3731074845243398 ) ) ;
#37926 = DIRECTION ( 'NONE',  ( 0.000000000000000000, 0.5000000000000144329, 0.8660254037844302699 ) ) ;
#37927 = ORIENTED_EDGE ( 'NONE', *, *, #227766, .T. ) ;
#37929 = CARTESIAN_POINT ( 'NONE',  ( -22.39999999999999858, 7.790779598384560245, -33.50000000000000000 ) ) ;
#37928 = DIRECTION ( 'NONE',  ( 1.000000000000000000, 0.000000000000000000, 0.000000000000000000 ) ) ;
#37930 = VERTEX_POINT ( 'NONE', #84891 ) ;
#37933 = ORIENTED_EDGE ( 'NONE', *, *, #238606, .T. ) ;
#37932 = DIRECTION ( 'NONE',  ( -0.000000000000000000, -0.000000000000000000, 1.000000000000000000 ) ) ;
#37931 = DIRECTION ( 'NONE',  ( -0.000000000000000000, 1.000000000000000000, -0.000000000000000000 ) ) ;
#37934 = ORIENTED_EDGE ( 'NONE', *, *, #34532, .T. ) ;
#37935 = DIRECTION ( 'NONE',  ( 0.000000000000000000, 0.000000000000000000, 1.000000000000000000 ) ) ;
#37936 = CARTESIAN_POINT ( 'NONE',  ( 21.05000000000000071, 0.03201369319893290072, -60.74115727646245233 ) ) ;
#37937 = LINE ( 'NONE', #35387, #36078 ) ;
#37938 = CARTESIAN_POINT ( 'NONE',  ( -18.38204789744325396, 64.52049896284712815, -145.7731074845244450 ) ) ;
#37940 = ORIENTED_EDGE ( 'NONE', *, *, #75312, .F. ) ;
#37939 =( BOUNDED_SURFACE ( )  B_SPLINE_SURFACE ( 3, 2, ( 
 ( #116716, #217078, #159707 ),
 ( #239236, #201385, #118001 ),
 ( #155873, #102250, #60582 ),
 ( #254878, #235371, #176711 ),
 ( #98390, #197529, #18896 ),
 ( #177994, #76292, #257451 ),
 ( #158446, #157154, #61887 ),
 ( #1883, #138806, #196248 ),
 ( #56705, #237942, #59264 ),
 ( #179291, #120593, #80114 ),
 ( #141411, #215798, #81408 ),
 ( #140111, #37203, #220937 ) ),
 .UNSPECIFIED., .F., .F., .F. ) 
 B_SPLINE_SURFACE_WITH_KNOTS ( ( 4, 2, 2, 2, 2, 4 ),
 ( 3, 3 ),
 ( 3.174653483277204646, 3.943930578431714018, 4.713207673586222946, 5.482484768740731873, 5.867123316317986337, 6.251761863895240801 ),
 ( 0.000000000000000000, 1.000000000000000000 ),
 .UNSPECIFIED. ) 
 GEOMETRIC_REPRESENTATION_ITEM ( )  RATIONAL_B_SPLINE_SURFACE ( (
 ( 1.000000000000000000, 0.8659465255642173620, 1.000000000000000000),
 ( 1.000000000000000000, 0.8648614068495104057, 1.000000000000000000),
 ( 1.000000000000000000, 0.8489031841315631821, 1.000000000000000000),
 ( 1.000000000000000000, 0.7927507630169553510, 1.000000000000000000),
 ( 1.000000000000000000, 0.7523013859136092885, 1.000000000000000000),
 ( 1.000000000000000000, 0.6616226951069902329, 1.000000000000000000),
 ( 1.000000000000000000, 0.6112214368811986764, 1.000000000000000000),
 ( 1.000000000000000000, 0.5507684314454389662, 1.000000000000000000),
 ( 1.000000000000000000, 0.5333267243029248261, 1.000000000000000000),
 ( 1.000000000000000000, 0.5084565446606316153, 1.000000000000000000),
 ( 1.000000000000000000, 0.5010722703356487173, 1.000000000000000000),
 ( 1.000000000000000000, 0.5001234037138250210, 1.000000000000000000) ) ) 
 REPRESENTATION_ITEM ( '' )  SURFACE ( )  );
#37941 = CARTESIAN_POINT ( 'NONE',  ( 20.95159278453404283, 67.09210366206356468, -195.0383872994151773 ) ) ;
#37942 = AXIS2_PLACEMENT_3D ( 'NONE', #113507, #193057, #173537 ) ;
#37943 = FACE_BOUND ( 'NONE', #31533, .T. ) ;
#37945 = CARTESIAN_POINT ( 'NONE',  ( 20.95576188350343116, 10.60898054496340137, -7.611233722754299436 ) ) ;
#37944 = DIRECTION ( 'NONE',  ( 0.000000000000000000, -0.2617529984165152257, -0.9651348961777124202 ) ) ;
#37947 = ORIENTED_EDGE ( 'NONE', *, *, #74067, .F. ) ;
#37946 = CARTESIAN_POINT ( 'NONE',  ( -16.92563707711778065, 9.968990694407935393, -54.38075829952398266 ) ) ;
#37948 = VECTOR ( 'NONE', #223474, 1000.000000000000000 ) ;
#37949 = VERTEX_POINT ( 'NONE', #21136 ) ;
#37950 = CIRCLE ( 'NONE', #25459, 0.09999999999999939493 ) ;
#37951 = ADVANCED_FACE ( 'NONE', ( #23710 ), #103191, .T. ) ;
#37952 = CARTESIAN_POINT ( 'NONE',  ( 20.95035502843362707, 11.84989802294387218, -206.1731169549366598 ) ) ;
#37953 = LINE ( 'NONE', #99160, #201277 ) ;
#37955 = ORIENTED_EDGE ( 'NONE', *, *, #249904, .F. ) ;
#37954 = AXIS2_PLACEMENT_3D ( 'NONE', #194633, #175088, #250715 ) ;
#37956 = LINE ( 'NONE', #134439, #122531 ) ;
#37957 = EDGE_LOOP ( 'NONE', ( #130985, #96310, #152198, #71007 ) ) ;
#37958 = FACE_OUTER_BOUND ( 'NONE', #105282, .T. ) ;
#37959 = AXIS2_PLACEMENT_3D ( 'NONE', #236280, #40697, #254532 ) ;
#37960 = EDGE_CURVE ( 'NONE', #251285, #155798, #137884, .T. ) ;
#37961 = DIRECTION ( 'NONE',  ( 0.000000000000000000, 0.000000000000000000, -1.000000000000000000 ) ) ;
#37962 = ORIENTED_EDGE ( 'NONE', *, *, #20345, .T. ) ;
#37963 = LINE ( 'NONE', #20974, #191783 ) ;
#37964 = EDGE_CURVE ( 'NONE', #226867, #111850, #79447, .T. ) ;
#37965 = EDGE_CURVE ( 'NONE', #50227, #178804, #54516, .T. ) ;
#37966 = AXIS2_PLACEMENT_3D ( 'NONE', #88164, #131169, #227695 ) ;
#37967 = CARTESIAN_POINT ( 'NONE',  ( -16.79140778683510149, 9.944941598865719712, -54.32973723377079978 ) ) ;
#37968 = VECTOR ( 'NONE', #190575, 1000.000000000000000 ) ;
#37969 = EDGE_CURVE ( 'NONE', #101145, #70073, #100287, .T. ) ;
#37971 = ORIENTED_EDGE ( 'NONE', *, *, #158669, .T. ) ;
#37970 = VECTOR ( 'NONE', #66757, 1000.000000000000000 ) ;
#37972 = ORIENTED_EDGE ( 'NONE', *, *, #147360, .F. ) ;
#37975 = EDGE_CURVE ( 'NONE', #214529, #3198, #200263, .T. ) ;
#37974 = ADVANCED_FACE ( 'NONE', ( #45805 ), #185319, .T. ) ;
#37973 = CARTESIAN_POINT ( 'NONE',  ( 21.05000000000000071, -11.74999999998883560, -136.9000000000000341 ) ) ;
#37976 = CIRCLE ( 'NONE', #183708, 0.1000000000000024342 ) ;
#37977 = ORIENTED_EDGE ( 'NONE', *, *, #17909, .F. ) ;
#37978 = ORIENTED_EDGE ( 'NONE', *, *, #249604, .T. ) ;
#37980 = ORIENTED_EDGE ( 'NONE', *, *, #52829, .F. ) ;
#37979 = CARTESIAN_POINT ( 'NONE',  ( 20.94999999999999929, 62.46832465249013921, -225.2232495205141731 ) ) ;
#37981 = VECTOR ( 'NONE', #32233, 1000.000000000000000 ) ;
#37982 = AXIS2_PLACEMENT_3D ( 'NONE', #209145, #189606, #172652 ) ;
#37983 = ORIENTED_EDGE ( 'NONE', *, *, #49809, .F. ) ;
#37986 = VERTEX_POINT ( 'NONE', #207465 ) ;
#37985 = ORIENTED_EDGE ( 'NONE', *, *, #212566, .F. ) ;
#37984 = DIRECTION ( 'NONE',  ( -0.000000000000000000, 0.4721928772777345684, 0.8814952561688429444 ) ) ;
#37987 = ORIENTED_EDGE ( 'NONE', *, *, #21267, .T. ) ;
#37988 = CYLINDRICAL_SURFACE ( 'NONE', #256239, 0.09999999999999939493 ) ;
#37989 = CIRCLE ( 'NONE', #62903, 0.1000000000000002692 ) ;
#37990 = EDGE_CURVE ( 'NONE', #141039, #60627, #171289, .T. ) ;
#37992 = ADVANCED_FACE ( 'NONE', ( #126625 ), #96200, .T. ) ;
#37991 = CIRCLE ( 'NONE', #50407, 0.1000000000000055844 ) ;
#37993 = DIRECTION ( 'NONE',  ( 0.000000000000000000, -6.982962677686266711E-15, 1.000000000000000000 ) ) ;
#37994 = CIRCLE ( 'NONE', #108709, 11.65000000000000036 ) ;
#37995 = CARTESIAN_POINT ( 'NONE',  ( 20.73486653747088582, 68.75000000001185185, -93.77310748452435973 ) ) ;
#37996 = ORIENTED_EDGE ( 'NONE', *, *, #5732, .F. ) ;
#37997 = EDGE_CURVE ( 'NONE', #236893, #245147, #25486, .T. ) ;
#37998 = DIRECTION ( 'NONE',  ( 0.000000000000000000, 0.000000000000000000, -1.000000000000000000 ) ) ;
#38000 = ORIENTED_EDGE ( 'NONE', *, *, #83123, .F. ) ;
#37999 = CARTESIAN_POINT ( 'NONE',  ( 6.099999999999997868, -11.65000000000000036, 13.90000000000000213 ) ) ;
#38001 = DIRECTION ( 'NONE',  ( 0.000000000000000000, 0.000000000000000000, -1.000000000000000000 ) ) ;
#38003 = ORIENTED_EDGE ( 'NONE', *, *, #45296, .F. ) ;
#38002 = DIRECTION ( 'NONE',  ( 0.000000000000000000, 0.4999999999999943379, 0.8660254037844420383 ) ) ;
#38004 =( BOUNDED_SURFACE ( )  B_SPLINE_SURFACE ( 3, 2, ( 
 ( #250548, #109747, #229713 ),
 ( #150189, #172357, #95337 ),
 ( #71932, #208863, #151482 ),
 ( #214007, #34119, #154075 ) ),
 .UNSPECIFIED., .F., .F., .F. ) 
 B_SPLINE_SURFACE_WITH_KNOTS ( ( 4, 4 ),
 ( 3, 3 ),
 ( 0.0002700421466196863498, 0.0004789321604330981771 ),
 ( 0.000000000000000000, 1.000000000000000000 ),
 .UNSPECIFIED. ) 
 GEOMETRIC_REPRESENTATION_ITEM ( )  RATIONAL_B_SPLINE_SURFACE ( (
 ( 1.000000000000000000, 0.7071067811865475727, 1.000000000000000000),
 ( 1.000000000000000000, 0.7163411249511595358, 1.000000000000000000),
 ( 1.000000000000000000, 0.7221957104842121611, 1.000000000000000000),
 ( 1.000000000000000000, 0.7250110520819756932, 1.000000000000000000) ) ) 
 REPRESENTATION_ITEM ( '' )  SURFACE ( )  );
#38005 = ORIENTED_EDGE ( 'NONE', *, *, #117332, .F. ) ;
#38007 = EDGE_CURVE ( 'NONE', #81634, #34173, #49655, .T. ) ;
#38006 = CARTESIAN_POINT ( 'NONE',  ( 20.94999999999999929, 86.32947205150912851, -209.3293116780858156 ) ) ;
#38008 = CARTESIAN_POINT ( 'NONE',  ( 20.94999999999999929, -9.499999999988844479, -124.1060308773475924 ) ) ;
#38009 = VERTEX_POINT ( 'NONE', #130472 ) ;
#38010 = EDGE_CURVE ( 'NONE', #53595, #128962, #253803, .T. ) ;
#38011 = VERTEX_POINT ( 'NONE', #30117 ) ;
#38012 = CARTESIAN_POINT ( 'NONE',  ( 21.72449340488910252, 10.28395627750227703, -113.1500000000000483 ) ) ;
#38013 = DIRECTION ( 'NONE',  ( 1.000000000000000000, -0.000000000000000000, -0.000000000000000000 ) ) ;
#38015 = VERTEX_POINT ( 'NONE', #225691 ) ;
#38014 = ORIENTED_EDGE ( 'NONE', *, *, #257077, .F. ) ;
#38016 = VERTEX_POINT ( 'NONE', #11845 ) ;
#38017 = DIRECTION ( 'NONE',  ( 0.000000000000000000, -0.000000000000000000, -1.000000000000000000 ) ) ;
#38018 = ORIENTED_EDGE ( 'NONE', *, *, #237023, .F. ) ;
#38019 = ORIENTED_EDGE ( 'NONE', *, *, #83120, .T. ) ;
#38020 = CARTESIAN_POINT ( 'NONE',  ( 18.49999999999999289, 64.75617845954087670, -200.4736850529726269 ) ) ;
#38021 = ORIENTED_EDGE ( 'NONE', *, *, #134465, .F. ) ;
#38022 = EDGE_CURVE ( 'NONE', #67207, #227353, #33725, .T. ) ;
#38023 = PLANE ( 'NONE',  #247973 ) ;
#38025 = CYLINDRICAL_SURFACE ( 'NONE', #169209, 1.500000000000001332 ) ;
#38024 = CARTESIAN_POINT ( 'NONE',  ( -23.25000000000000355, 10.05000000001113847, -79.75000000000004263 ) ) ;
#38026 = CIRCLE ( 'NONE', #75443, 0.5000000000000004441 ) ;
#38027 = ORIENTED_EDGE ( 'NONE', *, *, #215351, .T. ) ;
#38028 = ORIENTED_EDGE ( 'NONE', *, *, #5773, .F. ) ;
#38029 = EDGE_CURVE ( 'NONE', #140889, #12289, #88925, .T. ) ;
#38030 = DIRECTION ( 'NONE',  ( 1.000000000000000000, 0.000000000000000000, 0.000000000000000000 ) ) ;
#38031 = ORIENTED_EDGE ( 'NONE', *, *, #204189, .F. ) ;
#38032 =( BOUNDED_SURFACE ( )  B_SPLINE_SURFACE ( 3, 2, ( 
 ( #183224, #123241, #202776 ),
 ( #4560, #244465, #86650 ),
 ( #64546, #102354, #8439 ),
 ( #141514, #7132, #124537 ),
 ( #125798, #146633, #205323 ),
 ( #3272, #28027, #67119 ) ),
 .UNSPECIFIED., .F., .F., .F. ) 
 B_SPLINE_SURFACE_WITH_KNOTS ( ( 4, 2, 4 ),
 ( 3, 3 ),
 ( 0.0001381104793128061785, 0.0002947094729387477754, 0.0004513084665646893722 ),
 ( 0.000000000000000000, 1.000000000000000000 ),
 .UNSPECIFIED. ) 
 GEOMETRIC_REPRESENTATION_ITEM ( )  RATIONAL_B_SPLINE_SURFACE ( (
 ( 1.000000000000000000, 0.7071067811865494601, 1.000000000000000000),
 ( 1.000000000000000000, 0.6919563088098275028, 1.000000000000000000),
 ( 1.000000000000000000, 0.6959445945718949478, 1.000000000000000000),
 ( 1.000000000000000000, 0.7137882985310208817, 1.000000000000000000),
 ( 1.000000000000000000, 0.7257496306098795147, 1.000000000000000000),
 ( 1.000000000000000000, 0.7250110520819876836, 1.000000000000000000) ) ) 
 REPRESENTATION_ITEM ( '' )  SURFACE ( )  );
#38033 = TOROIDAL_SURFACE ( 'NONE', #58651, 0.2000000000000000111, 0.1000000000000000056 ) ;
#38034 = CARTESIAN_POINT ( 'NONE',  ( -18.42554971533678199, 85.49715966944965828, -95.98328057097560873 ) ) ;
#38035 = ORIENTED_EDGE ( 'NONE', *, *, #255479, .T. ) ;
#38036 = VERTEX_POINT ( 'NONE', #148774 ) ;
#38037 = DIRECTION ( 'NONE',  ( 0.000000000000000000, 0.000000000000000000, -1.000000000000000000 ) ) ;
#38038 = ADVANCED_FACE ( 'NONE', ( #147474 ), #44132, .T. ) ;
#38039 = EDGE_LOOP ( 'NONE', ( #238620, #256698 ) ) ;
#38040 = PLANE ( 'NONE',  #26553 ) ;
#38041 = CARTESIAN_POINT ( 'NONE',  ( -17.73285935861300544, 32.75820691008978258, -235.1439690831322480 ) ) ;
#38042 = EDGE_LOOP ( 'NONE', ( #218798, #109738, #20020, #94722 ) ) ;
#38043 = DIRECTION ( 'NONE',  ( 1.000000000000000000, 0.000000000000000000, 0.000000000000000000 ) ) ;
#38044 = DIRECTION ( 'NONE',  ( -2.812466655313719426E-14, 0.1350103645451904977, 0.9908441862701596881 ) ) ;
#38046 = CARTESIAN_POINT ( 'NONE',  ( -16.88705144915409306, 9.950000000011199219, -121.0690214052879980 ) ) ;
#38045 = CARTESIAN_POINT ( 'NONE',  ( -23.15000000000000213, 1.999999999999998224, -20.87537807723790095 ) ) ;
#38047 = SPHERICAL_SURFACE ( 'NONE', #19073, 0.1000000000000000056 ) ;
#38048 = DIRECTION ( 'NONE',  ( -1.000000000000000000, 7.304098846218134667E-16, -4.217023435051678980E-16 ) ) ;
#38049 = CARTESIAN_POINT ( 'NONE',  ( 21.05000000000000071, 65.27628289530476025, -157.8731074845244393 ) ) ;
#38050 = CARTESIAN_POINT ( 'NONE',  ( -18.40000000000000213, 64.52683809665012404, -190.9731074845244621 ) ) ;
#38051 = CARTESIAN_POINT ( 'NONE',  ( -21.05000000000000071, -11.48912529306489994, -97.60000000000005116 ) ) ;
#38052 = VECTOR ( 'NONE', #231486, 1000.000000000000000 ) ;
#38053 = ORIENTED_EDGE ( 'NONE', *, *, #108515, .F. ) ;
#38054 = AXIS2_PLACEMENT_3D ( 'NONE', #119485, #21665, #89315 ) ;
#38055 = CIRCLE ( 'NONE', #175430, 0.09999999999998898659 ) ;
#38057 = VERTEX_POINT ( 'NONE', #200574 ) ;
#38056 = ORIENTED_EDGE ( 'NONE', *, *, #155862, .F. ) ;
#38058 = EDGE_LOOP ( 'NONE', ( #207533, #222931, #134196, #164091 ) ) ;
#38059 = ORIENTED_EDGE ( 'NONE', *, *, #75288, .T. ) ;
#38060 = CARTESIAN_POINT ( 'NONE',  ( -21.07933241753356413, 0.09337959043042065588, -94.17135405162028405 ) ) ;
#38061 = CYLINDRICAL_SURFACE ( 'NONE', #199301, 0.09999999999999939493 ) ;
#38063 = DIRECTION ( 'NONE',  ( 0.000000000000000000, 0.9126074666063660468, 0.4088369013363524762 ) ) ;
#38062 = CARTESIAN_POINT ( 'NONE',  ( 23.14999999999998437, 76.00000000001195133, -103.0231074845243171 ) ) ;
#38064 = VERTEX_POINT ( 'NONE', #242258 ) ;
#38065 = DIRECTION ( 'NONE',  ( -1.000000000000000000, -0.000000000000000000, 0.000000000000000000 ) ) ;
#38066 = SURFACE_STYLE_USAGE ( .BOTH. , #27180 ) ;
#38067 = CARTESIAN_POINT ( 'NONE',  ( 18.49999999999998934, 10.25000000001115552, -91.65000000000004832 ) ) ;
#38069 = VECTOR ( 'NONE', #56505, 1000.000000000000000 ) ;
#38068 = DIRECTION ( 'NONE',  ( 1.000000000000000000, 0.000000000000000000, 0.000000000000000000 ) ) ;
#38070 = DIRECTION ( 'NONE',  ( 1.000000000000000000, 0.000000000000000000, 0.000000000000000000 ) ) ;
#38071 = VERTEX_POINT ( 'NONE', #203141 ) ;
#38072 = B_SPLINE_CURVE_WITH_KNOTS ( 'NONE', 3,
 ( #229616, #172251, #67966, #50944, #112249, #9275, #147505, #52235, #189207, #148800, #91391, #193065, #130498, #210062, #251740, #168406, #228335, #230916, #71840 ),
 .UNSPECIFIED., .F., .F.,
 ( 4, 3, 3, 3, 3, 3, 4 ),
 ( 0.000000000000000000, 1.655171619025965957E-05, 2.773500582848639000E-05, 5.941817267379636262E-05, 0.0001114174635873664597, 0.0001914169455916642400, 0.0002627181070751139673 ),
 .UNSPECIFIED. ) ;
#38073 = LINE ( 'NONE', #41928, #138905 ) ;
#38074 = ORIENTED_EDGE ( 'NONE', *, *, #177783, .T. ) ;
#38075 = CARTESIAN_POINT ( 'NONE',  ( 20.05000000000002913, 45.23934133962702475, -237.7629717664446503 ) ) ;
#38076 = CARTESIAN_POINT ( 'NONE',  ( -21.14999999999994174, 74.16448838626247664, -47.52760213295649550 ) ) ;
#38077 = DIRECTION ( 'NONE',  ( 0.000000000000000000, -7.056502275159890832E-15, 1.000000000000000000 ) ) ;
#38078 = LINE ( 'NONE', #154201, #48164 ) ;
#38079 = DIRECTION ( 'NONE',  ( 1.186688945009010077E-16, 0.9651348961777157509, -0.2617529984165031243 ) ) ;
#38080 = ORIENTED_EDGE ( 'NONE', *, *, #207080, .T. ) ;
#38081 = CARTESIAN_POINT ( 'NONE',  ( 20.94999999999999574, 44.58277672189309015, -247.4925639031954745 ) ) ;
#38082 = FACE_OUTER_BOUND ( 'NONE', #231524, .T. ) ;
#38083 = DIRECTION ( 'NONE',  ( 0.7071067811865493491, -0.7071067811865456854, -4.937700262164518065E-15 ) ) ;
#38085 = CARTESIAN_POINT ( 'NONE',  ( -20.94999999999999929, 74.26374286841490857, -158.4544551555068779 ) ) ;
#38084 = CYLINDRICAL_SURFACE ( 'NONE', #253310, 0.09999999999999939493 ) ;
#38088 = EDGE_CURVE ( 'NONE', #40984, #196505, #62897, .T. ) ;
#38087 = DIRECTION ( 'NONE',  ( 0.7071067811865487940, -4.937700262164522799E-15, 0.7071067811865463515 ) ) ;
#38086 = VECTOR ( 'NONE', #212024, 1000.000000000000114 ) ;
#38089 = DIRECTION ( 'NONE',  ( 0.000000000000000000, -5.551115123125777653E-14, 1.000000000000000000 ) ) ;
#38090 = DIRECTION ( 'NONE',  ( 0.000000000000000000, 0.000000000000000000, -1.000000000000000000 ) ) ;
#38091 = DIRECTION ( 'NONE',  ( 1.186688945009009831E-16, 1.000000000000000000, 6.982962677686266711E-15 ) ) ;
#38092 = VERTEX_POINT ( 'NONE', #222685 ) ;
#38093 = ORIENTED_EDGE ( 'NONE', *, *, #119979, .F. ) ;
#38094 = CARTESIAN_POINT ( 'NONE',  ( -20.94999999999999929, 70.15000000001163016, -59.39061026024639034 ) ) ;
#38095 = VERTEX_POINT ( 'NONE', #147002 ) ;
#38096 = ADVANCED_FACE ( 'NONE', ( #145720 ), #21951, .T. ) ;
#38097 = CARTESIAN_POINT ( 'NONE',  ( 22.88900146558018989, 8.703904791123973084, -76.25000000000004263 ) ) ;
#38098 = VECTOR ( 'NONE', #152339, 1000.000000000000000 ) ;
#38099 = EDGE_CURVE ( 'NONE', #231649, #161130, #121075, .T. ) ;
#38100 = CARTESIAN_POINT ( 'NONE',  ( 20.94999999999999929, 8.876614585098254295, -41.88508047884467800 ) ) ;
#38101 = CARTESIAN_POINT ( 'NONE',  ( -18.50000000000000000, -9.399999999988850163, -207.9146583429696307 ) ) ;
#38102 = ORIENTED_EDGE ( 'NONE', *, *, #7291, .T. ) ;
#38103 = CARTESIAN_POINT ( 'NONE',  ( -20.85000000000000142, 7.120270961708750512, -104.1595630418393768 ) ) ;
#38104 = CARTESIAN_POINT ( 'NONE',  ( -15.31895204843005409, 9.396533993965080711, -51.40593977917331614 ) ) ;
#38105 = CARTESIAN_POINT ( 'NONE',  ( -18.51697539158856998, 65.68434038414356735, -97.48668807260654035 ) ) ;
#38106 = EDGE_CURVE ( 'NONE', #11036, #220463, #141998, .T. ) ;
#38107 = EDGE_CURVE ( 'NONE', #237997, #121941, #183586, .T. ) ;
#38108 = FACE_BOUND ( 'NONE', #114635, .T. ) ;
#38110 = ORIENTED_EDGE ( 'NONE', *, *, #71892, .F. ) ;
#38109 = DIRECTION ( 'NONE',  ( 0.000000000000000000, 0.000000000000000000, 1.000000000000000000 ) ) ;
#38112 = DIRECTION ( 'NONE',  ( 0.000000000000000000, 0.1298341882519953583, 0.9915357197604862671 ) ) ;
#38111 = FACE_OUTER_BOUND ( 'NONE', #12332, .T. ) ;
#38114 = LINE ( 'NONE', #178931, #156928 ) ;
#38113 = AXIS2_PLACEMENT_3D ( 'NONE', #123784, #202036, #142048 ) ;
#38115 = DIRECTION ( 'NONE',  ( 0.000000000000000000, -0.000000000000000000, 1.000000000000000000 ) ) ;
#38117 = EDGE_CURVE ( 'NONE', #110815, #257268, #241947, .T. ) ;
#38116 = CYLINDRICAL_SURFACE ( 'NONE', #156402, 0.09999999999999811817 ) ;
#38118 = CARTESIAN_POINT ( 'NONE',  ( -21.14999999999999858, 11.75000000001115552, -40.28386566297815108 ) ) ;
#38119 = ORIENTED_EDGE ( 'NONE', *, *, #150110, .T. ) ;
#38120 = AXIS2_PLACEMENT_3D ( 'NONE', #209988, #49616, #9203 ) ;
#38121 = CARTESIAN_POINT ( 'NONE',  ( 18.59999999999999787, 76.00000000001237765, -170.0231074845243597 ) ) ;
#38122 = ADVANCED_FACE ( 'NONE', ( #165300 ), #161473, .T. ) ;
#38123 = ORIENTED_EDGE ( 'NONE', *, *, #155894, .F. ) ;
#38124 = AXIS2_PLACEMENT_3D ( 'NONE', #181925, #82774, #162375 ) ;
#38125 = CARTESIAN_POINT ( 'NONE',  ( -20.64999999999999858, 68.75000000001199396, -115.2731074845243455 ) ) ;
#38126 = ORIENTED_EDGE ( 'NONE', *, *, #222057, .F. ) ;
#38127 = CARTESIAN_POINT ( 'NONE',  ( 18.59999999999999076, 64.25000000001173817, -81.27310748452440237 ) ) ;
#38128 = AXIS2_PLACEMENT_3D ( 'NONE', #215146, #133055, #233451 ) ;
#38129 = ADVANCED_FACE ( 'NONE', ( #141878 ), #24533, .F. ) ;
#38130 = FACE_OUTER_BOUND ( 'NONE', #175475, .T. ) ;
#38131 = CARTESIAN_POINT ( 'NONE',  ( -24.30000000000000071, 3.175288713399619933, -347.0000000000001137 ) ) ;
#38132 = ORIENTED_EDGE ( 'NONE', *, *, #116606, .T. ) ;
#38133 = ORIENTED_EDGE ( 'NONE', *, *, #20837, .T. ) ;
#38134 = AXIS2_PLACEMENT_3D ( 'NONE', #175323, #34519, #218244 ) ;
#38135 = EDGE_CURVE ( 'NONE', #130475, #87594, #349, .T. ) ;
#38136 = CARTESIAN_POINT ( 'NONE',  ( -23.25000000000000000, 76.10085836911147794, -215.2726746080137445 ) ) ;
#38137 = CARTESIAN_POINT ( 'NONE',  ( 22.88900146558018989, 67.29609520889943042, -149.1731074845244223 ) ) ;
#38138 = CARTESIAN_POINT ( 'NONE',  ( -16.79270642812317504, 63.08646044285087839, -213.1392855534523676 ) ) ;
#38139 = CARTESIAN_POINT ( 'NONE',  ( -16.89268316805465986, 9.951721813253337601, -121.3557524785455826 ) ) ;
#38141 = CARTESIAN_POINT ( 'NONE',  ( 21.14999999999999858, 64.35000000001186038, -90.87310748452438247 ) ) ;
#38140 = DIRECTION ( 'NONE',  ( -0.5932847527679298016, -0.3291107096594085846, 0.7346423231209707749 ) ) ;
#38142 = VECTOR ( 'NONE', #130231, 1000.000000000000114 ) ;
#38143 = DIRECTION ( 'NONE',  ( 0.000000000000000000, 0.5283051335749160415, -0.8490545835447742551 ) ) ;
#38144 = FACE_OUTER_BOUND ( 'NONE', #248839, .T. ) ;
#38146 = CYLINDRICAL_SURFACE ( 'NONE', #155531, 0.09999999999999543976 ) ;
#38145 = CIRCLE ( 'NONE', #254575, 0.9000000000000014655 ) ;
#38147 = ORIENTED_EDGE ( 'NONE', *, *, #232062, .F. ) ;
#38148 = CARTESIAN_POINT ( 'NONE',  ( -21.14999999999999858, 64.35000000001166143, -69.42310748452440805 ) ) ;
#38150 = ORIENTED_EDGE ( 'NONE', *, *, #117914, .T. ) ;
#38149 = DIRECTION ( 'NONE',  ( -0.000000000000000000, -1.000000000000000000, -6.982962677686266711E-15 ) ) ;
#38151 = CARTESIAN_POINT ( 'NONE',  ( -23.15000000000000213, 76.00000000001162448, -65.37310748452432563 ) ) ;
#38152 = DIRECTION ( 'NONE',  ( 3.616040088954497272E-32, -1.224646799147352961E-16, 1.000000000000000000 ) ) ;
#38154 = DIRECTION ( 'NONE',  ( 0.000000000000000000, -0.2617529984165152257, -0.9651348961777124202 ) ) ;
#38153 = DIRECTION ( 'NONE',  ( 0.000000000000000000, 0.000000000000000000, -1.000000000000000000 ) ) ;
#38155 = CIRCLE ( 'NONE', #67168, 0.09999999999999939493 ) ;
#38156 = ORIENTED_EDGE ( 'NONE', *, *, #30871, .T. ) ;
#38158 = CARTESIAN_POINT ( 'NONE',  ( -18.59999999999999787, 9.150000000011157653, -146.3500000000000227 ) ) ;
#38157 = DIRECTION ( 'NONE',  ( 0.000000000000000000, 0.9126074666063844765, 0.4088369013363114535 ) ) ;
#38159 = CARTESIAN_POINT ( 'NONE',  ( 20.02499999999999858, 9.750000000011153745, -121.7500000000000426 ) ) ;
#38160 = CARTESIAN_POINT ( 'NONE',  ( 21.05000000000000071, 76.00000000001170974, -69.52310748452431710 ) ) ;
#38161 = DIRECTION ( 'NONE',  ( -1.000000000000000000, 7.510212038922846022E-17, -1.676432719286211941E-16 ) ) ;
#38163 = DIRECTION ( 'NONE',  ( 1.000000000000000000, -1.836970198721029934E-16, -1.601412966608202925E-30 ) ) ;
#38162 = VECTOR ( 'NONE', #218773, 1000.000000000000000 ) ;
#38164 = ORIENTED_EDGE ( 'NONE', *, *, #35662, .F. ) ;
#38165 = CARTESIAN_POINT ( 'NONE',  ( -20.85000000000000142, -4.871452838297996024, -233.3782557782877518 ) ) ;
#38166 = EDGE_LOOP ( 'NONE', ( #46710, #32, #192899, #54703 ) ) ;
#38167 = CARTESIAN_POINT ( 'NONE',  ( 20.94999999999999574, 18.24178995542692050, -237.7003448530951459 ) ) ;
#38168 = ORIENTED_EDGE ( 'NONE', *, *, #4497, .T. ) ;
#38170 = CARTESIAN_POINT ( 'NONE',  ( -20.94788355080264353, 46.36250628750308778, -243.0620573837410063 ) ) ;
#38169 = VECTOR ( 'NONE', #222182, 1000.000000000000000 ) ;
#38171 = CIRCLE ( 'NONE', #104741, 7.791421356237316687 ) ;
#38172 = ORIENTED_EDGE ( 'NONE', *, *, #198815, .T. ) ;
#38173 = AXIS2_PLACEMENT_3D ( 'NONE', #228992, #109020, #88153 ) ;
#38174 = ADVANCED_FACE ( 'NONE', ( #46613 ), #150406, .F. ) ;
#38175 = DIRECTION ( 'NONE',  ( 0.000000000000000000, 0.8814952561688437216, -0.4721928772777334582 ) ) ;
#38176 = CIRCLE ( 'NONE', #59529, 0.09999999999999939493 ) ;
#38177 = DIRECTION ( 'NONE',  ( 0.000000000000000000, -0.2128009952263605342, 0.9770955615653316162 ) ) ;
#38178 = ORIENTED_EDGE ( 'NONE', *, *, #150503, .T. ) ;
#38179 = EDGE_CURVE ( 'NONE', #163978, #230076, #219141, .T. ) ;
#38180 = ADVANCED_FACE ( 'NONE', ( #212144 ), #227834, .F. ) ;
#38181 = CARTESIAN_POINT ( 'NONE',  ( 21.72449340488909897, 10.28395627750227703, -87.85000000000003695 ) ) ;
#38182 = DIRECTION ( 'NONE',  ( 1.000000000000000000, 0.000000000000000000, 0.000000000000000000 ) ) ;
#38183 = EDGE_CURVE ( 'NONE', #123360, #26051, #50391, .T. ) ;
#38184 = CARTESIAN_POINT ( 'NONE',  ( 20.94999999999999929, 79.11538813396778380, -196.3722783875038544 ) ) ;
#38185 = EDGE_CURVE ( 'NONE', #76578, #156526, #8729, .T. ) ;
#38186 = DIRECTION ( 'NONE',  ( 1.000000000000000000, 0.000000000000000000, 0.000000000000000000 ) ) ;
#38187 = FACE_OUTER_BOUND ( 'NONE', #17039, .T. ) ;
#38188 = CARTESIAN_POINT ( 'NONE',  ( 13.12220780326573788, 62.11640146696787923, -218.6859212199908029 ) ) ;
#38189 = EDGE_CURVE ( 'NONE', #74170, #117682, #154514, .T. ) ;
#38190 = ORIENTED_EDGE ( 'NONE', *, *, #22927, .T. ) ;
#38191 = TOROIDAL_SURFACE ( 'NONE', #171474, 11.65000000000000036, 0.1000000000000000056 ) ;
#38192 = EDGE_CURVE ( 'NONE', #81489, #129962, #210850, .T. ) ;
#38193 = ORIENTED_EDGE ( 'NONE', *, *, #227439, .T. ) ;
#38195 = ORIENTED_EDGE ( 'NONE', *, *, #241298, .F. ) ;
#38194 = CARTESIAN_POINT ( 'NONE',  ( 21.14999999999999503, 76.10085836911093793, -148.2726746080136877 ) ) ;
#38196 = ORIENTED_EDGE ( 'NONE', *, *, #183299, .F. ) ;
#38197 = DIRECTION ( 'NONE',  ( 1.000000000000000000, 0.000000000000000000, 0.000000000000000000 ) ) ;
#38198 = DIRECTION ( 'NONE',  ( -1.020425574104004196E-15, -0.2617529984165031243, -0.9651348961777157509 ) ) ;
#38199 = CARTESIAN_POINT ( 'NONE',  ( -21.14999999999999858, -11.64999999998884483, -69.90000000000004832 ) ) ;
#38200 = ADVANCED_FACE ( 'NONE', ( #209565 ), #229503, .T. ) ;
#38201 = DIRECTION ( 'NONE',  ( 0.000000000000000000, -0.5000000000000078826, 0.8660254037844340447 ) ) ;
#38202 = VERTEX_POINT ( 'NONE', #49201 ) ;
#38203 = CARTESIAN_POINT ( 'NONE',  ( 23.14999999999999858, 1.115600667400684642E-11, -134.0000000000000284 ) ) ;
#38204 = CARTESIAN_POINT ( 'NONE',  ( -18.50000000000000711, 12.87592094156238609, -205.3750039893633073 ) ) ;
#38206 = VERTEX_POINT ( 'NONE', #109160 ) ;
#38205 = CIRCLE ( 'NONE', #183928, 11.74999999999999645 ) ;
#38208 = ORIENTED_EDGE ( 'NONE', *, *, #93923, .T. ) ;
#38207 = DIRECTION ( 'NONE',  ( 0.000000000000000000, -1.000000000000000000, -0.000000000000000000 ) ) ;
#38209 = CARTESIAN_POINT ( 'NONE',  ( 18.39999999999999503, 11.75000000001113953, -121.3500000000000369 ) ) ;
#38210 = CARTESIAN_POINT ( 'NONE',  ( 23.14999999999999858, 76.00000000001126921, -203.5231074845248997 ) ) ;
#38211 = VERTEX_POINT ( 'NONE', #110456 ) ;
#38212 = EDGE_CURVE ( 'NONE', #66847, #239682, #10077, .T. ) ;
#38213 = AXIS2_PLACEMENT_3D ( 'NONE', #163475, #87767, #225975 ) ;
#38214 = CARTESIAN_POINT ( 'NONE',  ( 20.99749315643148151, 64.25000000001195133, -110.0379132532841453 ) ) ;
#38215 = ORIENTED_EDGE ( 'NONE', *, *, #173587, .T. ) ;
#38216 = DIRECTION ( 'NONE',  ( 0.000000000000000000, -0.9651348961777157509, 0.2617529984165030132 ) ) ;
#38217 = EDGE_CURVE ( 'NONE', #104319, #144042, #187448, .T. ) ;
#38218 = DIRECTION ( 'NONE',  ( 0.000000000000000000, 0.000000000000000000, 1.000000000000000000 ) ) ;
#38219 = DIRECTION ( 'NONE',  ( 0.000000000000000000, -1.000000000000000000, 0.000000000000000000 ) ) ;
#38220 = EDGE_CURVE ( 'NONE', #82481, #48218, #237691, .T. ) ;
#38221 = CARTESIAN_POINT ( 'NONE',  ( 20.94999999999999929, 76.00000000001213607, -136.5231074845242745 ) ) ;
#38222 = AXIS2_PLACEMENT_3D ( 'NONE', #38100, #117619, #197144 ) ;
#38223 = AXIS2_PLACEMENT_3D ( 'NONE', #6917, #8223, #23945 ) ;
#38225 = ORIENTED_EDGE ( 'NONE', *, *, #9111, .F. ) ;
#38224 = AXIS2_PLACEMENT_3D ( 'NONE', #75066, #225429, #154604 ) ;
#38226 = LINE ( 'NONE', #175206, #119542 ) ;
#38227 = VERTEX_POINT ( 'NONE', #190004 ) ;
#38228 = CARTESIAN_POINT ( 'NONE',  ( -17.29158576265544056, 12.55694934947041119, -209.9501076257347734 ) ) ;
#38229 = LINE ( 'NONE', #59022, #95730 ) ;
#38231 = ORIENTED_EDGE ( 'NONE', *, *, #39474, .F. ) ;
#38230 = CARTESIAN_POINT ( 'NONE',  ( -21.56666275994539816, 1.115600667400684642E-11, -60.04263159310671938 ) ) ;
#38232 = CARTESIAN_POINT ( 'NONE',  ( 19.99999999999998934, 64.25000000001148237, -44.67310748452440095 ) ) ;
#38233 = DIRECTION ( 'NONE',  ( -1.000000000000000000, 1.349229370204181174E-14, 0.000000000000000000 ) ) ;
#38234 = DIRECTION ( 'NONE',  ( -1.000000000000000000, -8.674042436075348305E-17, -1.619280515896124405E-16 ) ) ;
#38235 = CARTESIAN_POINT ( 'NONE',  ( -0.8999999999999437339, 64.35000000001120668, -12.72310748452478890 ) ) ;
#38236 = DIRECTION ( 'NONE',  ( 0.000000000000000000, 0.000000000000000000, -1.000000000000000000 ) ) ;
#38237 = DIRECTION ( 'NONE',  ( -0.000000000000000000, 1.000000000000000000, 6.982962677686266711E-15 ) ) ;
#38238 = CARTESIAN_POINT ( 'NONE',  ( -18.59999996769639097, 85.36327376984259274, -129.3416135690586373 ) ) ;
#38240 = ORIENTED_EDGE ( 'NONE', *, *, #62626, .T. ) ;
#38239 = DIRECTION ( 'NONE',  ( 1.186688945009010077E-16, 1.000000000000000000, 6.982962677686266711E-15 ) ) ;
#38241 = AXIS2_PLACEMENT_3D ( 'NONE', #29832, #225411, #10250 ) ;
#38242 = CARTESIAN_POINT ( 'NONE',  ( 18.59999999999999787, 77.73670573947964613, -125.0056848969006182 ) ) ;
#38243 = EDGE_LOOP ( 'NONE', ( #93638, #93287, #198045, #122876 ) ) ;
#38244 = CARTESIAN_POINT ( 'NONE',  ( -21.44999999999999929, 7.150000000011155876, -188.6499999999999488 ) ) ;
#38245 = CARTESIAN_POINT ( 'NONE',  ( -18.47079683080343315, 85.47166410525755964, -196.4142469435320777 ) ) ;
#38246 = EDGE_LOOP ( 'NONE', ( #167600, #80397, #254341, #2689 ) ) ;
#38247 = CARTESIAN_POINT ( 'NONE',  ( 21.05000000000000071, 65.57661458509869590, -62.03105556065429482 ) ) ;
#38248 = EDGE_CURVE ( 'NONE', #4098, #135260, #170492, .T. ) ;
#38249 = B_SPLINE_CURVE_WITH_KNOTS ( 'NONE', 3,
 ( #58309, #80421, #43906, #217388, #62194, #137851, #60889, #23085, #158749, #79161 ),
 .UNSPECIFIED., .F., .F.,
 ( 4, 2, 2, 2, 4 ),
 ( 0.000000000000000000, 3.990160268009109807E-05, 7.980320536018219613E-05, 0.0001596064107204557634, 0.0003192128214410053103 ),
 .UNSPECIFIED. ) ;
#38250 = CIRCLE ( 'NONE', #150673, 0.09999999999999939493 ) ;
#38251 = CIRCLE ( 'NONE', #163166, 0.2000000000000057288 ) ;
#38252 = CARTESIAN_POINT ( 'NONE',  ( -18.48550754432060472, 85.46339977857157066, -62.47431773210951178 ) ) ;
#38253 = CIRCLE ( 'NONE', #113258, 0.09999999999998898659 ) ;
#38254 = EDGE_CURVE ( 'NONE', #66395, #242362, #131302, .T. ) ;
#38255 = ORIENTED_EDGE ( 'NONE', *, *, #58933, .F. ) ;
#38256 = LINE ( 'NONE', #181623, #156302 ) ;
#38257 = CARTESIAN_POINT ( 'NONE',  ( -16.93262454970420094, 65.99797953208224044, -190.9501837107617632 ) ) ;
#38258 = ADVANCED_FACE ( 'NONE', ( #12670 ), #183713, .T. ) ;
#38259 = EDGE_LOOP ( 'NONE', ( #61457, #228634, #558, #119293 ) ) ;
#38261 = EDGE_CURVE ( 'NONE', #17816, #208385, #246061, .T. ) ;
#38260 = DIRECTION ( 'NONE',  ( 0.000000000000000000, -1.000000000000000000, 0.000000000000000000 ) ) ;
#38262 = VERTEX_POINT ( 'NONE', #213397 ) ;
#38263 = LINE ( 'NONE', #156943, #33810 ) ;
#38265 = ORIENTED_EDGE ( 'NONE', *, *, #144059, .T. ) ;
#38264 = DIRECTION ( 'NONE',  ( 0.000000000000000000, 0.8814952561688429444, -0.4721928772777349570 ) ) ;
#38266 = AXIS2_PLACEMENT_3D ( 'NONE', #47738, #183427, #204251 ) ;
#38267 = DIRECTION ( 'NONE',  ( 0.000000000000000000, 0.4999999999999088507, -0.8660254037844913322 ) ) ;
#38268 = ORIENTED_EDGE ( 'NONE', *, *, #118586, .T. ) ;
#38269 = DIRECTION ( 'NONE',  ( -3.469446951953515108E-14, -1.000000000000000000, 0.000000000000000000 ) ) ;
#38270 = ORIENTED_EDGE ( 'NONE', *, *, #230460, .F. ) ;
#38272 = ORIENTED_EDGE ( 'NONE', *, *, #246090, .F. ) ;
#38271 = ORIENTED_EDGE ( 'NONE', *, *, #236125, .F. ) ;
#38273 = DIRECTION ( 'NONE',  ( 0.000000000000000000, -0.4721928772776973204, -0.8814952561688629284 ) ) ;
#38274 = ORIENTED_EDGE ( 'NONE', *, *, #206141, .T. ) ;
#38275 = DIRECTION ( 'NONE',  ( -1.000000000000000000, 0.000000000000000000, 0.000000000000000000 ) ) ;
#38276 = ORIENTED_EDGE ( 'NONE', *, *, #85505, .F. ) ;
#38277 = ADVANCED_FACE ( 'NONE', ( #54323 ), #253808, .T. ) ;
#38278 = EDGE_CURVE ( 'NONE', #45367, #85652, #17733, .T. ) ;
#38279 = VERTEX_POINT ( 'NONE', #58164 ) ;
#38280 = FACE_OUTER_BOUND ( 'NONE', #72906, .T. ) ;
#38282 = DIRECTION ( 'NONE',  ( -0.000000000000000000, -0.9126074666063770380, -0.4088369013363281068 ) ) ;
#38281 = AXIS2_PLACEMENT_3D ( 'NONE', #194503, #35443, #174970 ) ;
#38284 = EDGE_LOOP ( 'NONE', ( #235790, #165673, #98591, #225878 ) ) ;
#38283 = CARTESIAN_POINT ( 'NONE',  ( -20.64999999999999858, 7.150000000011155876, -146.3500000000000227 ) ) ;
#38285 = CARTESIAN_POINT ( 'NONE',  ( -22.59999999999999787, 64.35042919246716053, -103.1231074845243825 ) ) ;
#38286 = ORIENTED_EDGE ( 'NONE', *, *, #2706, .F. ) ;
#38287 = CARTESIAN_POINT ( 'NONE',  ( -20.94999999999999929, 13.60254931771583387, -238.7443143987590304 ) ) ;
#38288 = CARTESIAN_POINT ( 'NONE',  ( -23.25000000000000355, 66.05000000001160743, -60.27310748452439526 ) ) ;
#38289 = CARTESIAN_POINT ( 'NONE',  ( 23.14999999999999858, 62.92003201576280702, -207.2439188921395612 ) ) ;
#38290 = AXIS2_PLACEMENT_3D ( 'NONE', #208713, #190437, #30085 ) ;
#38291 = ORIENTED_EDGE ( 'NONE', *, *, #136408, .T. ) ;
#38292 = DIRECTION ( 'NONE',  ( 0.000000000000000000, -0.9770955615653316162, -0.2128009952263604232 ) ) ;
#38294 = EDGE_CURVE ( 'NONE', #47404, #228403, #130171, .T. ) ;
#38293 = CARTESIAN_POINT ( 'NONE',  ( -18.48408745364643835, 37.98660231122499908, -261.2259190080672511 ) ) ;
#38295 = DIRECTION ( 'NONE',  ( -1.000000000000000000, 0.000000000000000000, 0.000000000000000000 ) ) ;
#38296 = CIRCLE ( 'NONE', #151309, 0.09999999999999939493 ) ;
#38297 = AXIS2_PLACEMENT_3D ( 'NONE', #229598, #193047, #73123 ) ;
#38298 = ORIENTED_EDGE ( 'NONE', *, *, #208401, .T. ) ;
#38299 = ADVANCED_FACE ( 'NONE', ( #34807 ), #76457, .F. ) ;
#38300 = CARTESIAN_POINT ( 'NONE',  ( -17.01764560440201990, 14.13772148870163647, -219.1573630007518432 ) ) ;
#38301 = ORIENTED_EDGE ( 'NONE', *, *, #239591, .T. ) ;
#38302 = VERTEX_POINT ( 'NONE', #99849 ) ;
#38303 = AXIS2_PLACEMENT_3D ( 'NONE', #71503, #12809, #111904 ) ;
#38304 = DIRECTION ( 'NONE',  ( 2.952720810173289112E-16, 1.000000000000000000, 6.467318590049456648E-15 ) ) ;
#38305 = ORIENTED_EDGE ( 'NONE', *, *, #231116, .F. ) ;
#38306 = AXIS2_PLACEMENT_3D ( 'NONE', #250109, #71493, #191454 ) ;
#38307 = VERTEX_POINT ( 'NONE', #196407 ) ;
#38308 = DIRECTION ( 'NONE',  ( 0.000000000000000000, 0.8777080977375072424, -0.4791956752371691608 ) ) ;
#38309 = ORIENTED_EDGE ( 'NONE', *, *, #38822, .T. ) ;
#38310 = ORIENTED_EDGE ( 'NONE', *, *, #23725, .F. ) ;
#38311 = EDGE_CURVE ( 'NONE', #167673, #148669, #51042, .T. ) ;
#38312 = CARTESIAN_POINT ( 'NONE',  ( -20.64999999999999858, 6.375212254182287097, -220.8739277186596155 ) ) ;
#38313 = AXIS2_PLACEMENT_3D ( 'NONE', #85798, #87106, #3731 ) ;
#38314 = DIRECTION ( 'NONE',  ( -1.000000000000000000, -0.000000000000000000, -0.000000000000000000 ) ) ;
#38315 = EDGE_CURVE ( 'NONE', #133447, #113811, #238096, .T. ) ;
#38317 = ORIENTED_EDGE ( 'NONE', *, *, #235973, .F. ) ;
#38316 = AXIS2_PLACEMENT_3D ( 'NONE', #54101, #131075, #37137 ) ;
#38318 = ORIENTED_EDGE ( 'NONE', *, *, #100871, .T. ) ;
#38320 = ADVANCED_FACE ( 'NONE', ( #116879 ), #79004, .T. ) ;
#38319 = TOROIDAL_SURFACE ( 'NONE', #25846, 0.2000000000000000111, 0.1000000000000000056 ) ;
#38321 = AXIS2_PLACEMENT_3D ( 'NONE', #121010, #89536, #127400 ) ;
#38322 = ORIENTED_EDGE ( 'NONE', *, *, #70900, .T. ) ;
#38323 = CARTESIAN_POINT ( 'NONE',  ( -20.94999999999999929, 28.50120599808395028, -258.2149742250584268 ) ) ;
#38324 = TOROIDAL_SURFACE ( 'NONE', #117435, 0.4000000000000003553, 0.1000000000000000056 ) ;
#38325 = B_SPLINE_CURVE_WITH_KNOTS ( 'NONE', 3,
 ( #180044, #101746, #3961, #83468, #2666, #181340, #182620, #82184 ),
 .UNSPECIFIED., .F., .F.,
 ( 4, 2, 2, 4 ),
 ( 0.000000000000000000, 0.0002114466876441958789, 0.0003171700314663007301, 0.0004228933752884056355 ),
 .UNSPECIFIED. ) ;
#38326 = LINE ( 'NONE', #136094, #163734 ) ;
#38327 = EDGE_CURVE ( 'NONE', #144564, #83024, #175585, .T. ) ;
#38328 = CIRCLE ( 'NONE', #159156, 2.000000000000001776 ) ;
#38329 = CYLINDRICAL_SURFACE ( 'NONE', #142672, 0.5000000000000004441 ) ;
#38330 = DIRECTION ( 'NONE',  ( 1.000000000000000000, 0.000000000000000000, 0.000000000000000000 ) ) ;
#38331 = DIRECTION ( 'NONE',  ( -1.000000000000000000, 0.000000000000000000, -0.000000000000000000 ) ) ;
#38332 = DIRECTION ( 'NONE',  ( 1.000000000000000000, 0.000000000000000000, 0.000000000000000000 ) ) ;
#38333 = DIRECTION ( 'NONE',  ( -6.938893903907222856E-15, -1.000000000000000000, -7.272083257015735086E-15 ) ) ;
#38334 = EDGE_CURVE ( 'NONE', #105518, #164553, #119915, .T. ) ;
#38336 = LINE ( 'NONE', #77423, #74525 ) ;
#38335 = CARTESIAN_POINT ( 'NONE',  ( -16.87845715379269507, 9.957858113897010810, -12.62380065105889493 ) ) ;
#38337 = DIRECTION ( 'NONE',  ( 0.000000000000000000, 0.000000000000000000, 1.000000000000000000 ) ) ;
#38338 = CARTESIAN_POINT ( 'NONE',  ( -22.39999999999999858, 64.35000000001214460, -136.5231074845243597 ) ) ;
#38339 = DIRECTION ( 'NONE',  ( 0.000000000000000000, -0.8814952561688476074, 0.4721928772777262417 ) ) ;
#38340 = CIRCLE ( 'NONE', #246434, 0.09999999999999939493 ) ;
#38341 = CARTESIAN_POINT ( 'NONE',  ( 21.07964655665547582, 44.22523807184186495, -236.5463624157991944 ) ) ;
#38342 = CIRCLE ( 'NONE', #146634, 0.1000000000000038219 ) ;
#38343 =( BOUNDED_CURVE ( )  B_SPLINE_CURVE ( 3, ( #138760, #176666, #203592, #557 ),
 .UNSPECIFIED., .F., .T. ) 
 B_SPLINE_CURVE_WITH_KNOTS ( ( 4, 4 ),
 ( 2.589852378279005940, 2.850972632318390598 ),
 .UNSPECIFIED. ) 
 CURVE ( )  GEOMETRIC_REPRESENTATION_ITEM ( )  RATIONAL_B_SPLINE_CURVE ( ( 1.000000000000000000, 0.9943260843901261525, 0.9943260843901261525, 1.000000000000000000 ) ) 
 REPRESENTATION_ITEM ( '' )  );
#38345 = ORIENTED_EDGE ( 'NONE', *, *, #102652, .T. ) ;
#38344 = AXIS2_PLACEMENT_3D ( 'NONE', #180572, #181857, #1908 ) ;
#38346 = AXIS2_PLACEMENT_3D ( 'NONE', #75311, #175682, #234344 ) ;
#38348 = ORIENTED_EDGE ( 'NONE', *, *, #186698, .T. ) ;
#38347 = DIRECTION ( 'NONE',  ( 0.000000000000000000, -0.9651348961777157509, 0.2617529984165031243 ) ) ;
#38349 = FACE_OUTER_BOUND ( 'NONE', #21833, .T. ) ;
#38350 = CARTESIAN_POINT ( 'NONE',  ( -21.05000000000000071, 77.36087058720436005, -161.9501095574333931 ) ) ;
#38351 = VERTEX_POINT ( 'NONE', #136406 ) ;
#38352 = DIRECTION ( 'NONE',  ( -0.000000000000000000, -0.9770955615653316162, -0.2128009952263604232 ) ) ;
#38353 = CARTESIAN_POINT ( 'NONE',  ( -16.88593481969334320, 9.950560090084310971, -20.85187225694449609 ) ) ;
#38354 = AXIS2_PLACEMENT_3D ( 'NONE', #244918, #105370, #246212 ) ;
#38355 = ORIENTED_EDGE ( 'NONE', *, *, #212684, .F. ) ;
#38356 = FACE_OUTER_BOUND ( 'NONE', #73640, .T. ) ;
#38357 = FACE_OUTER_BOUND ( 'NONE', #117722, .T. ) ;
#38358 = DIRECTION ( 'NONE',  ( 0.000000000000000000, -0.7092521942343286145, -0.7049548389604757270 ) ) ;
#38359 = FACE_OUTER_BOUND ( 'NONE', #11676, .T. ) ;
#38361 = ORIENTED_EDGE ( 'NONE', *, *, #62102, .F. ) ;
#38360 = DIRECTION ( 'NONE',  ( 0.000000000000000000, -0.2617529984165030132, -0.9651348961777157509 ) ) ;
#38363 = VERTEX_POINT ( 'NONE', #20372 ) ;
#38362 = DIRECTION ( 'NONE',  ( -1.000000000000000000, 0.000000000000000000, 0.000000000000000000 ) ) ;
#38364 = DIRECTION ( 'NONE',  ( 1.000000000000000000, 0.000000000000000000, 0.000000000000000000 ) ) ;
#38365 = CARTESIAN_POINT ( 'NONE',  ( 21.09696443733127325, 10.72400988391847676, -12.23477752704822130 ) ) ;
#38366 = DIRECTION ( 'NONE',  ( 0.000000000000000000, -1.000000000000000000, -0.000000000000000000 ) ) ;
#38367 = CARTESIAN_POINT ( 'NONE',  ( -17.01825945287481545, 63.05955705323258798, -213.2241350765465882 ) ) ;
#38369 = CARTESIAN_POINT ( 'NONE',  ( 21.14999999999999858, 64.25000000001172396, -81.27310748452440237 ) ) ;
#38368 = CARTESIAN_POINT ( 'NONE',  ( 18.46858270002953972, 8.915580963857621555, -245.4376901980162131 ) ) ;
#38371 = EDGE_CURVE ( 'NONE', #200872, #250359, #96840, .T. ) ;
#38370 = CARTESIAN_POINT ( 'NONE',  ( 12.25000000000000000, 9.850000000011137402, -117.2500000000000284 ) ) ;
#38372 = CARTESIAN_POINT ( 'NONE',  ( -23.15000000000000213, 84.59626168225550202, -179.4732350016745954 ) ) ;
#38373 = CYLINDRICAL_SURFACE ( 'NONE', #145552, 0.09999999999999939493 ) ;
#38374 = CARTESIAN_POINT ( 'NONE',  ( -23.25000000000000000, 76.00000000001145395, -39.92310748452432279 ) ) ;
#38375 = FACE_OUTER_BOUND ( 'NONE', #193715, .T. ) ;
#38376 = ORIENTED_EDGE ( 'NONE', *, *, #112639, .F. ) ;
#38378 = AXIS2_PLACEMENT_3D ( 'NONE', #170951, #130477, #165783 ) ;
#38377 = DIRECTION ( 'NONE',  ( 1.000000000000000000, 0.000000000000000000, 0.000000000000000000 ) ) ;
#38379 = ORIENTED_EDGE ( 'NONE', *, *, #45168, .F. ) ;
#38380 = VERTEX_POINT ( 'NONE', #233002 ) ;
#38381 = FACE_OUTER_BOUND ( 'NONE', #171746, .T. ) ;
#38382 = ADVANCED_FACE ( 'NONE', ( #77730 ), #236816, .T. ) ;
#38383 = DIRECTION ( 'NONE',  ( 0.000000000000000000, 6.982962677686266711E-15, -1.000000000000000000 ) ) ;
#38384 = ORIENTED_EDGE ( 'NONE', *, *, #122054, .F. ) ;
#38385 =( BOUNDED_CURVE ( )  B_SPLINE_CURVE ( 3, ( #127538, #152262, #226619, #113107 ),
 .UNSPECIFIED., .F., .F. ) 
 B_SPLINE_CURVE_WITH_KNOTS ( ( 4, 4 ),
 ( 0.3000847527772390055, 0.5517402753107889524 ),
 .UNSPECIFIED. ) 
 CURVE ( )  GEOMETRIC_REPRESENTATION_ITEM ( )  RATIONAL_B_SPLINE_CURVE ( ( 1.000000000000000000, 0.9947294176030464508, 0.9947294176030464508, 1.000000000000000000 ) ) 
 REPRESENTATION_ITEM ( '' )  );
#38386 = EDGE_CURVE ( 'NONE', #140176, #228115, #242605, .T. ) ;
#38387 = EDGE_CURVE ( 'NONE', #16536, #125531, #9374, .T. ) ;
#38388 = ORIENTED_EDGE ( 'NONE', *, *, #250987, .T. ) ;
#38389 = AXIS2_PLACEMENT_3D ( 'NONE', #23383, #222818, #1194 ) ;
#38390 = EDGE_LOOP ( 'NONE', ( #195455, #130990, #188766, #37263 ) ) ;
#38391 = ORIENTED_EDGE ( 'NONE', *, *, #195541, .F. ) ;
#38392 = DIRECTION ( 'NONE',  ( 0.000000000000000000, 0.000000000000000000, 1.000000000000000000 ) ) ;
#38393 = CARTESIAN_POINT ( 'NONE',  ( -22.00356870068735660, -2.403239590344364268E-12, 7.254242361757839319 ) ) ;
#38394 = CARTESIAN_POINT ( 'NONE',  ( 23.24999999999999645, 67.17743825834591576, -160.7731074845244166 ) ) ;
#38395 = DIRECTION ( 'NONE',  ( -1.000000000000000000, -7.304098846218135653E-16, -5.100424963727256530E-30 ) ) ;
#38396 = CARTESIAN_POINT ( 'NONE',  ( 15.70340296795548518, 9.355888454502546026, -16.28864289677800059 ) ) ;
#38397 = EDGE_CURVE ( 'NONE', #137697, #10751, #14140, .T. ) ;
#38398 = CARTESIAN_POINT ( 'NONE',  ( -18.59999999999999787, 77.44184265367995579, -241.6694879557322508 ) ) ;
#38399 = CARTESIAN_POINT ( 'NONE',  ( 21.15000000000000213, 76.00000000001217870, -143.0637644362255401 ) ) ;
#38401 = EDGE_LOOP ( 'NONE', ( #155166, #99335 ) ) ;
#38400 = DIRECTION ( 'NONE',  ( 1.000000000000000000, -7.304098846218163263E-16, 4.217023435051626718E-16 ) ) ;
#38403 = DIRECTION ( 'NONE',  ( 0.000000000000000000, 0.000000000000000000, -1.000000000000000000 ) ) ;
#38402 = LINE ( 'NONE', #175374, #229656 ) ;
#38404 = CARTESIAN_POINT ( 'NONE',  ( 23.14999999999998437, 55.89093952297024970, -232.7795287750844579 ) ) ;
#38405 = ORIENTED_EDGE ( 'NONE', *, *, #65045, .T. ) ;
#38406 = CARTESIAN_POINT ( 'NONE',  ( -18.50000000000000000, 9.122720154857367092, -245.4644708025848558 ) ) ;
#38407 = DIRECTION ( 'NONE',  ( -0.000000000000000000, -1.734723475976817507E-14, 1.000000000000000000 ) ) ;
#38408 = ORIENTED_EDGE ( 'NONE', *, *, #173940, .T. ) ;
#38409 = AXIS2_PLACEMENT_3D ( 'NONE', #5903, #202836, #108874 ) ;
#38412 = CARTESIAN_POINT ( 'NONE',  ( -21.05000000000000071, 77.16270174994961906, -61.42310748452431568 ) ) ;
#38411 = VECTOR ( 'NONE', #41807, 1000.000000000000000 ) ;
#38410 = DIRECTION ( 'NONE',  ( 0.000000000000000000, -1.565658005757035267E-14, 1.000000000000000000 ) ) ;
#38413 = DIRECTION ( 'NONE',  ( -0.7071067811865474617, -0.3338907855510734324, -0.6233112732207618523 ) ) ;
#38414 = CARTESIAN_POINT ( 'NONE',  ( 22.50014994444006433, 64.25028026811959592, -69.60618764124355096 ) ) ;
#38415 = ORIENTED_EDGE ( 'NONE', *, *, #58195, .T. ) ;
#38416 = ORIENTED_EDGE ( 'NONE', *, *, #192329, .T. ) ;
#38417 = CARTESIAN_POINT ( 'NONE',  ( -20.94999999999999929, 11.69999999999999574, -26.74500185048138334 ) ) ;
#38418 = EDGE_CURVE ( 'NONE', #26537, #176380, #184337, .T. ) ;
#38419 = CARTESIAN_POINT ( 'NONE',  ( -18.33981767444511490, -0.7704322632317684993, -242.4320893355032638 ) ) ;
#38420 = DIRECTION ( 'NONE',  ( 1.000000000000000000, 0.000000000000000000, 0.000000000000000000 ) ) ;
#38421 = DIRECTION ( 'NONE',  ( 0.000000000000000000, 0.000000000000000000, -1.000000000000000000 ) ) ;
#38422 = ORIENTED_EDGE ( 'NONE', *, *, #3560, .F. ) ;
#38423 = CARTESIAN_POINT ( 'NONE',  ( -20.85000000000000142, 43.35377423437995503, -245.1717807829448930 ) ) ;
#38424 = VECTOR ( 'NONE', #71594, 1000.000000000000000 ) ;
#38425 = AXIS2_PLACEMENT_3D ( 'NONE', #13461, #33067, #147839 ) ;
#38426 = EDGE_CURVE ( 'NONE', #96705, #200797, #51537, .T. ) ;
#38427 = VECTOR ( 'NONE', #152992, 1000.000000000000000 ) ;
#38428 = CARTESIAN_POINT ( 'NONE',  ( -16.94107738177414291, 10.01423928514777373, -121.4500000000000313 ) ) ;
#38429 = CARTESIAN_POINT ( 'NONE',  ( -21.05000000000000071, 70.10000000001251408, -180.2422072491807796 ) ) ;
#38430 = CARTESIAN_POINT ( 'NONE',  ( -18.59999999999999787, 64.35000000001157616, -57.37310748452440379 ) ) ;
#38432 = ORIENTED_EDGE ( 'NONE', *, *, #17045, .F. ) ;
#38431 = DIRECTION ( 'NONE',  ( 0.000000000000000000, 0.000000000000000000, -1.000000000000000000 ) ) ;
#38433 = CARTESIAN_POINT ( 'NONE',  ( 20.85000000000000142, 74.93036000061670165, -233.6816308724374949 ) ) ;
#38434 = CARTESIAN_POINT ( 'NONE',  ( -16.89935556175729658, 66.05000000001187743, -89.88343112163957471 ) ) ;
#38435 = DIRECTION ( 'NONE',  ( -1.000000000000000000, 0.000000000000000000, -0.000000000000000000 ) ) ;
#38436 = CARTESIAN_POINT ( 'NONE',  ( 23.04999999999999716, 67.17743825834583049, -149.1731074845244223 ) ) ;
#38437 = DIRECTION ( 'NONE',  ( -1.000000000000000000, -0.000000000000000000, -0.000000000000000000 ) ) ;
#38439 = ORIENTED_EDGE ( 'NONE', *, *, #207117, .T. ) ;
#38438 = SPHERICAL_SURFACE ( 'NONE', #106741, 0.1000000000000000056 ) ;
#38440 = CARTESIAN_POINT ( 'NONE',  ( -18.59999999999999787, 77.16270174994990327, -94.92310748452430857 ) ) ;
#38441 = FACE_OUTER_BOUND ( 'NONE', #152842, .T. ) ;
#38442 = DIRECTION ( 'NONE',  ( 1.000000000000000000, 0.000000000000000000, 0.000000000000000000 ) ) ;
#38443 = CIRCLE ( 'NONE', #184175, 12.97499999999998721 ) ;
#38444 = ORIENTED_EDGE ( 'NONE', *, *, #130866, .F. ) ;
#38445 = CARTESIAN_POINT ( 'NONE',  ( -12.30589683808040924, 66.64325398293399871, -152.8197477631601657 ) ) ;
#38446 = FACE_OUTER_BOUND ( 'NONE', #110211, .T. ) ;
#38448 = EDGE_CURVE ( 'NONE', #3727, #110167, #134446, .T. ) ;
#38447 = CARTESIAN_POINT ( 'NONE',  ( -0.8999999999999993561, -11.65000000000000036, 23.30000000000000426 ) ) ;
#38449 = LINE ( 'NONE', #37187, #116833 ) ;
#38450 = DIRECTION ( 'NONE',  ( -1.000000000000000000, -0.000000000000000000, 0.000000000000000000 ) ) ;
#38451 = TOROIDAL_SURFACE ( 'NONE', #134676, 11.89999999999999858, 0.1000000000000000056 ) ;
#38452 = DIRECTION ( 'NONE',  ( -0.000000000000000000, 0.4791956752371484551, 0.8777080977375184556 ) ) ;
#38453 = VERTEX_POINT ( 'NONE', #165110 ) ;
#38454 = ORIENTED_EDGE ( 'NONE', *, *, #233844, .T. ) ;
#38455 = ADVANCED_FACE ( 'NONE', ( #30757 ), #71160, .T. ) ;
#38456 = FACE_OUTER_BOUND ( 'NONE', #139628, .T. ) ;
#38458 = EDGE_CURVE ( 'NONE', #227551, #248008, #88101, .T. ) ;
#38457 = CARTESIAN_POINT ( 'NONE',  ( -16.87242674293849731, 66.05000000001201954, -115.6720172381520229 ) ) ;
#38459 = DIRECTION ( 'NONE',  ( -1.000000000000000000, -0.000000000000000000, -0.000000000000000000 ) ) ;
#38460 = CARTESIAN_POINT ( 'NONE',  ( 23.15000000000000213, 85.60000000001261355, -193.6291383618718385 ) ) ;
#38461 = ORIENTED_EDGE ( 'NONE', *, *, #187650, .T. ) ;
#38462 = EDGE_CURVE ( 'NONE', #101407, #225681, #50272, .T. ) ;
#38463 = ADVANCED_FACE ( 'NONE', ( #209358 ), #129820, .F. ) ;
#38464 = CARTESIAN_POINT ( 'NONE',  ( 20.95575313997065336, 10.61455330328599089, -175.1212907019447869 ) ) ;
#38465 = AXIS2_PLACEMENT_3D ( 'NONE', #6319, #247514, #48017 ) ;
#38466 = LINE ( 'NONE', #100950, #225669 ) ;
#38467 = AXIS2_PLACEMENT_3D ( 'NONE', #152453, #190286, #87301 ) ;
#38468 = EDGE_CURVE ( 'NONE', #224599, #140260, #84335, .T. ) ;
#38469 = DIRECTION ( 'NONE',  ( -0.000000000000000000, 1.000000000000000000, -0.000000000000000000 ) ) ;
#38470 = CIRCLE ( 'NONE', #225876, 12.87499999999999822 ) ;
#38471 = CARTESIAN_POINT ( 'NONE',  ( 23.04999999999999716, 67.17743825834548943, -93.77310748452437394 ) ) ;
#38472 = EDGE_CURVE ( 'NONE', #61003, #68228, #230135, .T. ) ;
#38475 = EDGE_CURVE ( 'NONE', #64282, #138184, #63534, .T. ) ;
#38474 = EDGE_CURVE ( 'NONE', #12568, #47711, #185954, .T. ) ;
#38473 = AXIS2_PLACEMENT_3D ( 'NONE', #61207, #39100, #179888 ) ;
#38476 = VERTEX_POINT ( 'NONE', #236615 ) ;
#38477 = CARTESIAN_POINT ( 'NONE',  ( 18.49999999999999645, 77.13501884592227498, -128.8061306010920362 ) ) ;
#38478 = AXIS2_PLACEMENT_3D ( 'NONE', #3575, #139219, #217478 ) ;
#38479 = B_SPLINE_CURVE_WITH_KNOTS ( 'NONE', 3,
 ( #55901, #33853, #15552, #95053, #117194, #76772, #156351, #93765, #173364, #135453, #53367, #153806, #214997, #174652, #57189, #252838 ),
 .UNSPECIFIED., .F., .F.,
 ( 4, 3, 3, 3, 3, 4 ),
 ( 0.000000000000000000, 3.357088238233684694E-05, 6.714213034887935657E-05, 0.0001007408646121008016, 0.0001343627955914262746, 0.0001573956632896011476 ),
 .UNSPECIFIED. ) ;
#38480 = ORIENTED_EDGE ( 'NONE', *, *, #90094, .F. ) ;
#38481 = VERTEX_POINT ( 'NONE', #52845 ) ;
#38482 = CARTESIAN_POINT ( 'NONE',  ( -21.05000000000000071, 0.05132743235267277215, -27.19981666373291773 ) ) ;
#38483 = CARTESIAN_POINT ( 'NONE',  ( -21.65000000000000213, 62.99793053463489656, -222.0144804547670390 ) ) ;
#38484 = FACE_OUTER_BOUND ( 'NONE', #73972, .T. ) ;
#38485 = ORIENTED_EDGE ( 'NONE', *, *, #72129, .T. ) ;
#38486 = CARTESIAN_POINT ( 'NONE',  ( 18.49999999999999289, 69.55000000001179217, -81.87310748452435405 ) ) ;
#38487 = CARTESIAN_POINT ( 'NONE',  ( -18.59999999999999787, 77.13501884592203339, -95.30613060109196510 ) ) ;
#38489 = PLANE ( 'NONE',  #82974 ) ;
#38488 = AXIS2_PLACEMENT_3D ( 'NONE', #217313, #17838, #253886 ) ;
#38490 = ORIENTED_EDGE ( 'NONE', *, *, #154004, .F. ) ;
#38491 = DIRECTION ( 'NONE',  ( -1.000000000000000000, 0.000000000000000000, 0.000000000000000000 ) ) ;
#38492 = AXIS2_PLACEMENT_3D ( 'NONE', #144880, #84880, #47060 ) ;
#38493 = ADVANCED_FACE ( 'NONE', ( #54129 ), #17566, .F. ) ;
#38495 = ORIENTED_EDGE ( 'NONE', *, *, #158945, .F. ) ;
#38494 = DIRECTION ( 'NONE',  ( 0.000000000000000000, 0.000000000000000000, 1.000000000000000000 ) ) ;
#38496 = DIRECTION ( 'NONE',  ( 0.000000000000000000, -0.8814952561688431665, 0.4721928772777346794 ) ) ;
#38497 = DIRECTION ( 'NONE',  ( 1.000000000000000000, 0.000000000000000000, 0.000000000000000000 ) ) ;
#38498 = AXIS2_PLACEMENT_3D ( 'NONE', #42388, #141483, #224861 ) ;
#38499 = TOROIDAL_SURFACE ( 'NONE', #21930, 4.149999999999999467, 0.1000000000000000056 ) ;
#38500 = EDGE_CURVE ( 'NONE', #91491, #173345, #137507, .T. ) ;
#38502 = EDGE_CURVE ( 'NONE', #135423, #119397, #197446, .T. ) ;
#38501 = CIRCLE ( 'NONE', #46849, 0.5999999999999998668 ) ;
#38503 = EDGE_LOOP ( 'NONE', ( #122046, #42019, #159482, #136620 ) ) ;
#38504 = CIRCLE ( 'NONE', #9278, 0.1000000000000028644 ) ;
#38505 = CARTESIAN_POINT ( 'NONE',  ( 21.08489834409762054, 65.37767610527707518, -191.1731074845243370 ) ) ;
#38507 = EDGE_CURVE ( 'NONE', #56413, #79382, #226008, .T. ) ;
#38506 = CARTESIAN_POINT ( 'NONE',  ( -16.79139129368505223, 66.05505583755018506, -90.35286285169856058 ) ) ;
#38508 = FACE_OUTER_BOUND ( 'NONE', #143908, .T. ) ;
#38509 = ORIENTED_EDGE ( 'NONE', *, *, #142255, .T. ) ;
#38510 = CARTESIAN_POINT ( 'NONE',  ( 23.14999999999999858, 5.500000000011153745, -112.9052660189131245 ) ) ;
#38511 = CIRCLE ( 'NONE', #113522, 0.09999999999998898659 ) ;
#38512 = CARTESIAN_POINT ( 'NONE',  ( 13.22461703343585349, 49.52260852254784140, -233.4480600891348558 ) ) ;
#38513 = DIRECTION ( 'NONE',  ( 0.000000000000000000, -6.982962677686266711E-15, 1.000000000000000000 ) ) ;
#38514 = ADVANCED_FACE ( 'NONE', ( #37165 ), #171556, .T. ) ;
#38515 = EDGE_LOOP ( 'NONE', ( #70347, #106593, #132638, #144758 ) ) ;
#38516 = ORIENTED_EDGE ( 'NONE', *, *, #181576, .T. ) ;
#38517 = CIRCLE ( 'NONE', #42609, 0.09999999999999817368 ) ;
#38518 = CIRCLE ( 'NONE', #171830, 12.87499999999999822 ) ;
#38519 = ORIENTED_EDGE ( 'NONE', *, *, #108987, .F. ) ;
#38520 = CARTESIAN_POINT ( 'NONE',  ( 21.05000000000000071, 68.03191114188443578, -213.8010436651919122 ) ) ;
#38521 = CARTESIAN_POINT ( 'NONE',  ( -23.25000000000000355, 64.25000000001264766, -194.2731074845244450 ) ) ;
#38523 = ORIENTED_EDGE ( 'NONE', *, *, #31691, .F. ) ;
#38522 = CARTESIAN_POINT ( 'NONE',  ( 19.75857864376268935, 11.75000000001115907, -192.3499999999999659 ) ) ;
#38524 = DIRECTION ( 'NONE',  ( -0.7071067811865388020, 0.7071067811865561215, 0.000000000000000000 ) ) ;
#38525 = DIRECTION ( 'NONE',  ( -1.000000000000000000, -0.000000000000000000, -0.000000000000000000 ) ) ;
#38526 = DIRECTION ( 'NONE',  ( -1.000000000000000000, -1.652117596168391700E-15, -1.153667551319263085E-29 ) ) ;
#38527 = CARTESIAN_POINT ( 'NONE',  ( -23.25000000000000000, 77.83585931145526615, -58.01866831572577610 ) ) ;
#38528 = CARTESIAN_POINT ( 'NONE',  ( -23.15000000000000213, 71.75000000001156764, -57.27310748452435263 ) ) ;
#38529 = CARTESIAN_POINT ( 'NONE',  ( 20.94999999999999929, 1.115624548013267999E-11, -65.10000000000000853 ) ) ;
#38531 = ORIENTED_EDGE ( 'NONE', *, *, #240435, .T. ) ;
#38530 = CARTESIAN_POINT ( 'NONE',  ( 23.15000000000000213, -8.596261682242985813, -24.04987248284971812 ) ) ;
#38533 = ORIENTED_EDGE ( 'NONE', *, *, #122678, .F. ) ;
#38532 = CARTESIAN_POINT ( 'NONE',  ( 23.14999999999999503, 6.550000000011156231, -121.6500000000000341 ) ) ;
#38535 = CARTESIAN_POINT ( 'NONE',  ( -18.40000000000000213, 11.47316190337364183, -87.95000000000004547 ) ) ;
#38534 = CARTESIAN_POINT ( 'NONE',  ( 18.79999999999999716, 11.50977166988710820, 1.786320531569725478 ) ) ;
#38537 = ORIENTED_EDGE ( 'NONE', *, *, #2516, .F. ) ;
#38536 = CYLINDRICAL_SURFACE ( 'NONE', #179277, 0.1000000000000124678 ) ;
#38538 = ORIENTED_EDGE ( 'NONE', *, *, #189707, .F. ) ;
#38539 = CARTESIAN_POINT ( 'NONE',  ( -18.54148534481894117, 10.32532329027886320, -106.0699343018360139 ) ) ;
#38540 = AXIS2_PLACEMENT_3D ( 'NONE', #199, #233993, #99285 ) ;
#38541 = DIRECTION ( 'NONE',  ( 0.000000000000000000, 0.9908441862701596881, 0.1350103645451904977 ) ) ;
#38542 = CARTESIAN_POINT ( 'NONE',  ( -20.85000000000000142, 1.115600667400684642E-11, -167.5000000000000284 ) ) ;
#38543 = CIRCLE ( 'NONE', #146842, 4.049999999999998046 ) ;
#38544 = CARTESIAN_POINT ( 'NONE',  ( -23.15000000000000213, 1.115600667400684642E-11, -100.5000000000000284 ) ) ;
#38545 = CARTESIAN_POINT ( 'NONE',  ( -23.25000000000000000, 41.42187432231295219, -260.1830396872097140 ) ) ;
#38546 = CARTESIAN_POINT ( 'NONE',  ( -23.25000000000000000, 62.12679871018153932, -248.6611778639222337 ) ) ;
#38547 = CARTESIAN_POINT ( 'NONE',  ( -18.59999999999999787, 42.94477010600543565, -254.3363632230312703 ) ) ;
#38549 = VERTEX_POINT ( 'NONE', #211948 ) ;
#38548 = EDGE_CURVE ( 'NONE', #57850, #174398, #176012, .T. ) ;
#38550 = EDGE_LOOP ( 'NONE', ( #144470, #14173, #141872, #108516 ) ) ;
#38551 = SPHERICAL_SURFACE ( 'NONE', #176842, 0.1000000000000000056 ) ;
#38552 = EDGE_CURVE ( 'NONE', #213781, #230224, #111552, .T. ) ;
#38553 = EDGE_LOOP ( 'NONE', ( #164370, #12184, #54406, #175239 ) ) ;
#38554 = DIRECTION ( 'NONE',  ( 0.000000000000000000, 0.000000000000000000, -1.000000000000000000 ) ) ;
#38555 = CARTESIAN_POINT ( 'NONE',  ( 18.59999999999999076, 69.55000000001223270, -148.8731074845244109 ) ) ;
#38556 = CARTESIAN_POINT ( 'NONE',  ( -15.06774609480955363, 66.58234804117054750, -54.16432009208396892 ) ) ;
#38557 = FACE_OUTER_BOUND ( 'NONE', #58917, .T. ) ;
#38558 = ADVANCED_FACE ( 'NONE', ( #157114 ), #180271, .F. ) ;
#38559 = VERTEX_POINT ( 'NONE', #12469 ) ;
#38561 = EDGE_CURVE ( 'NONE', #207244, #111449, #151045, .T. ) ;
#38560 = CARTESIAN_POINT ( 'NONE',  ( -13.77083647240106501, 66.54258906972185628, -118.0231915757780854 ) ) ;
#38562 = EDGE_LOOP ( 'NONE', ( #138606, #51692, #163599, #62692 ) ) ;
#38563 = DIRECTION ( 'NONE',  ( 0.000000000000000000, 1.000000000000000000, 0.000000000000000000 ) ) ;
#38564 = ORIENTED_EDGE ( 'NONE', *, *, #61929, .T. ) ;
#38565 = DIRECTION ( 'NONE',  ( 0.000000000000000000, 0.000000000000000000, 1.000000000000000000 ) ) ;
#38566 = DIRECTION ( 'NONE',  ( 0.000000000000000000, -1.000000000000000000, 0.000000000000000000 ) ) ;
#38567 = CYLINDRICAL_SURFACE ( 'NONE', #234487, 0.09999999999999939493 ) ;
#38568 = VERTEX_POINT ( 'NONE', #72442 ) ;
#38570 = CARTESIAN_POINT ( 'NONE',  ( -21.14999999999994174, 84.00000000001119815, -37.18565239344504647 ) ) ;
#38569 = AXIS2_PLACEMENT_3D ( 'NONE', #6339, #106718, #227973 ) ;
#38572 = ORIENTED_EDGE ( 'NONE', *, *, #90006, .F. ) ;
#38571 = DIRECTION ( 'NONE',  ( -0.000000000000000000, 1.000000000000000000, -5.204170427930272977E-14 ) ) ;
#38573 = DIRECTION ( 'NONE',  ( 0.000000000000000000, 0.8814952561688437216, -0.4721928772777334582 ) ) ;
#38574 = ORIENTED_EDGE ( 'NONE', *, *, #96633, .F. ) ;
#38575 = TOROIDAL_SURFACE ( 'NONE', #59189, 4.149999999999999467, 0.1000000000000000056 ) ;
#38576 = EDGE_CURVE ( 'NONE', #123705, #89984, #33337, .T. ) ;
#38577 = EDGE_CURVE ( 'NONE', #31357, #222338, #205179, .T. ) ;
#38578 = TOROIDAL_SURFACE ( 'NONE', #96812, 7.800000000000000711, 0.1000000000000000056 ) ;
#38579 = CARTESIAN_POINT ( 'NONE',  ( -20.00857864376270001, 66.75000000001179501, -81.77310748452437394 ) ) ;
#38580 = ORIENTED_EDGE ( 'NONE', *, *, #124829, .F. ) ;
#38581 = DIRECTION ( 'NONE',  ( 1.000000000000000000, 0.000000000000000000, 0.000000000000000000 ) ) ;
#38582 = CARTESIAN_POINT ( 'NONE',  ( 22.50000000000000000, 64.08545097430041437, -247.0723585184913986 ) ) ;
#38583 = CARTESIAN_POINT ( 'NONE',  ( 18.57399277249656322, 67.49230083716666684, -195.4236814984208479 ) ) ;
#38584 = DIRECTION ( 'NONE',  ( 0.000000000000000000, 0.000000000000000000, 1.000000000000000000 ) ) ;
#38585 = VECTOR ( 'NONE', #78716, 1000.000000000000227 ) ;
#38586 = ORIENTED_EDGE ( 'NONE', *, *, #194959, .T. ) ;
#38587 = CIRCLE ( 'NONE', #225820, 0.1000000000000054040 ) ;
#38589 = EDGE_CURVE ( 'NONE', #109372, #93529, #238522, .T. ) ;
#38588 = CARTESIAN_POINT ( 'NONE',  ( 18.59999999999998721, 6.846123162352588665, -37.23772626684986164 ) ) ;
#38590 = CARTESIAN_POINT ( 'NONE',  ( -21.04999999999994387, 67.85000000001119247, -25.49719488170504533 ) ) ;
#38591 = CARTESIAN_POINT ( 'NONE',  ( -20.87155475150660777, 11.75000000001115197, -160.5955865291576572 ) ) ;
#38592 = ORIENTED_EDGE ( 'NONE', *, *, #222303, .T. ) ;
#38593 = ADVANCED_FACE ( 'NONE', ( #95811 ), #174135, .T. ) ;
#38594 = DIRECTION ( 'NONE',  ( -0.000000000000000000, -6.982962677686266711E-15, 1.000000000000000000 ) ) ;
#38595 = ORIENTED_EDGE ( 'NONE', *, *, #29878, .T. ) ;
#38596 = DIRECTION ( 'NONE',  ( 1.073024830501117725E-15, -0.000000000000000000, -1.000000000000000000 ) ) ;
#38597 = ORIENTED_EDGE ( 'NONE', *, *, #156278, .T. ) ;
#38598 = DIRECTION ( 'NONE',  ( -0.000000000000000000, 1.000000000000000000, 6.982962677686267499E-15 ) ) ;
#38599 = LINE ( 'NONE', #118134, #101981 ) ;
#38600 = AXIS2_PLACEMENT_3D ( 'NONE', #182557, #219079, #136986 ) ;
#38602 = ORIENTED_EDGE ( 'NONE', *, *, #129172, .T. ) ;
#38601 = DIRECTION ( 'NONE',  ( 0.000000000000000000, -0.4099100576505548821, -0.9121259477928028714 ) ) ;
#38603 = DIRECTION ( 'NONE',  ( -1.000000000000000000, 0.000000000000000000, 0.000000000000000000 ) ) ;
#38604 = ORIENTED_EDGE ( 'NONE', *, *, #59909, .F. ) ;
#38605 = ADVANCED_FACE ( 'NONE', ( #215765 ), #21860, .F. ) ;
#38606 = PLANE ( 'NONE',  #81723 ) ;
#38607 = AXIS2_PLACEMENT_3D ( 'NONE', #115590, #215961, #137703 ) ;
#38608 = CIRCLE ( 'NONE', #184338, 0.1000000000000002554 ) ;
#38609 = VECTOR ( 'NONE', #43291, 1000.000000000000000 ) ;
#38610 = DIRECTION ( 'NONE',  ( 0.000000000000000000, 0.000000000000000000, 1.000000000000000000 ) ) ;
#38611 = EDGE_CURVE ( 'NONE', #68814, #47203, #179251, .T. ) ;
#38612 = ORIENTED_EDGE ( 'NONE', *, *, #186865, .T. ) ;
#38613 = AXIS2_PLACEMENT_3D ( 'NONE', #80642, #83199, #1101 ) ;
#38614 = VERTEX_POINT ( 'NONE', #222170 ) ;
#38615 = CARTESIAN_POINT ( 'NONE',  ( 20.94999999999999574, -11.64999999999999147, -3.000000000000002665 ) ) ;
#38616 = LINE ( 'NONE', #114290, #77676 ) ;
#38617 = VERTEX_POINT ( 'NONE', #197490 ) ;
#38618 = CARTESIAN_POINT ( 'NONE',  ( 18.60000000000000142, -9.321008403350125704, -141.2359382490778899 ) ) ;
#38619 = VERTEX_POINT ( 'NONE', #119267 ) ;
#38620 = EDGE_LOOP ( 'NONE', ( #1763, #82397, #63020, #22930 ) ) ;
#38621 = EDGE_CURVE ( 'NONE', #103860, #181359, #192741, .T. ) ;
#38622 = DIRECTION ( 'NONE',  ( 0.000000000000000000, 0.9651348961777157509, -0.2617529984165031243 ) ) ;
#38623 = EDGE_CURVE ( 'NONE', #223175, #82512, #20162, .T. ) ;
#38625 = ORIENTED_EDGE ( 'NONE', *, *, #102448, .T. ) ;
#38624 = CARTESIAN_POINT ( 'NONE',  ( 18.47654891039378455, 85.46527494839416761, -95.89713157932956733 ) ) ;
#38626 = DIRECTION ( 'NONE',  ( 0.000000000000000000, 0.000000000000000000, 1.000000000000000000 ) ) ;
#38627 = CARTESIAN_POINT ( 'NONE',  ( -20.64999999999999858, 7.150000000011155876, -79.35000000000005116 ) ) ;
#38628 = EDGE_CURVE ( 'NONE', #49350, #15058, #1177, .T. ) ;
#38629 = DIRECTION ( 'NONE',  ( 1.000000000000000000, 0.000000000000000000, 0.000000000000000000 ) ) ;
#38630 = DIRECTION ( 'NONE',  ( 1.000000000000000000, -0.000000000000000000, -0.000000000000000000 ) ) ;
#38631 = CARTESIAN_POINT ( 'NONE',  ( 23.15000000000000213, 87.65000000001172964, -72.62310748452422615 ) ) ;
#38632 = CIRCLE ( 'NONE', #100936, 0.09999999999999939493 ) ;
#38633 = DIRECTION ( 'NONE',  ( -1.444674012291107001E-15, 0.1332476588733650935, -0.9910827722268042983 ) ) ;
#38634 = CIRCLE ( 'NONE', #234250, 0.1000000000000028644 ) ;
#38635 = DIRECTION ( 'NONE',  ( 0.000000000000000000, -0.4088369013363281068, 0.9126074666063770380 ) ) ;
#38636 = B_SPLINE_CURVE_WITH_KNOTS ( 'NONE', 3,
 ( #17322, #138503, #55114, #115126, #197220, #38170, #154301, #77265, #233800, #16052, #173867, #95553, #176403, #253338, #60272, #19892, #99385, #156850, #98089 ),
 .UNSPECIFIED., .F., .F.,
 ( 4, 3, 3, 3, 3, 3, 4 ),
 ( -2.000416914651719952E-06, 0.000000000000000000, 4.714008503744950701E-05, 9.979203887777911156E-05, 0.0001372215519229559935, 0.0001635031576221014160, 0.0001900083748504201547 ),
 .UNSPECIFIED. ) ;
#38637 = VERTEX_POINT ( 'NONE', #80080 ) ;
#38638 = ORIENTED_EDGE ( 'NONE', *, *, #157185, .T. ) ;
#38639 = LINE ( 'NONE', #44744, #99976 ) ;
#38641 = ORIENTED_EDGE ( 'NONE', *, *, #36519, .T. ) ;
#38640 = LINE ( 'NONE', #16524, #96086 ) ;
#38642 = ORIENTED_EDGE ( 'NONE', *, *, #206763, .F. ) ;
#38643 = EDGE_CURVE ( 'NONE', #216335, #239176, #213565, .T. ) ;
#38645 = CARTESIAN_POINT ( 'NONE',  ( -18.36973785203555920, 64.52449679952829342, -179.2731074845244450 ) ) ;
#38644 = AXIS2_PLACEMENT_3D ( 'NONE', #257303, #237803, #82540 ) ;
#38646 = ORIENTED_EDGE ( 'NONE', *, *, #177558, .T. ) ;
#38647 = CARTESIAN_POINT ( 'NONE',  ( 20.85000000000000142, -1.851617760457748618, -212.6031897196036198 ) ) ;
#38648 = CIRCLE ( 'NONE', #84377, 0.1000000000000028644 ) ;
#38649 = ORIENTED_EDGE ( 'NONE', *, *, #509, .T. ) ;
#38650 = AXIS2_PLACEMENT_3D ( 'NONE', #129062, #252843, #33856 ) ;
#38651 = FACE_OUTER_BOUND ( 'NONE', #107634, .T. ) ;
#38652 = VECTOR ( 'NONE', #83501, 1000.000000000000000 ) ;
#38654 = ORIENTED_EDGE ( 'NONE', *, *, #57799, .F. ) ;
#38653 = ORIENTED_EDGE ( 'NONE', *, *, #86413, .F. ) ;
#38655 = EDGE_LOOP ( 'NONE', ( #65974, #17431, #161496, #151413 ) ) ;
#38656 = ORIENTED_EDGE ( 'NONE', *, *, #60262, .F. ) ;
#38657 = AXIS2_PLACEMENT_3D ( 'NONE', #127387, #4836, #187375 ) ;
#38658 = B_SPLINE_CURVE_WITH_KNOTS ( 'NONE', 3,
 ( #255634, #238687, #137022, #216553 ),
 .UNSPECIFIED., .F., .F.,
 ( 4, 4 ),
 ( 0.000000000000000000, 7.713889350927971339E-05 ),
 .UNSPECIFIED. ) ;
#38659 = CARTESIAN_POINT ( 'NONE',  ( -18.50000000000000000, 68.97833521811203639, -132.6895420826271277 ) ) ;
#38660 = VERTEX_POINT ( 'NONE', #63110 ) ;
#38661 = CARTESIAN_POINT ( 'NONE',  ( -21.05000000000000071, 87.65000000001192859, -100.1231074845242262 ) ) ;
#38662 = CARTESIAN_POINT ( 'NONE',  ( 12.93225390519045170, 12.47031117194349292, -214.0029172826438071 ) ) ;
#38664 = ORIENTED_EDGE ( 'NONE', *, *, #192882, .T. ) ;
#38663 = CARTESIAN_POINT ( 'NONE',  ( 18.49999999999999645, 1.637172712981537659, -112.0821533654720525 ) ) ;
#38665 = DIRECTION ( 'NONE',  ( -4.239556034732056743E-17, -0.1298341882519953583, -0.9915357197604862671 ) ) ;
#38666 = ORIENTED_EDGE ( 'NONE', *, *, #198572, .T. ) ;
#38667 = CARTESIAN_POINT ( 'NONE',  ( 20.94999999999999574, 18.90448995781211750, -232.7802074516171444 ) ) ;
#38668 = VECTOR ( 'NONE', #95775, 1000.000000000000000 ) ;
#38670 = ORIENTED_EDGE ( 'NONE', *, *, #139697, .T. ) ;
#38669 = DIRECTION ( 'NONE',  ( 1.000000000000000000, 0.000000000000000000, 0.000000000000000000 ) ) ;
#38671 = DIRECTION ( 'NONE',  ( 1.000000000000000000, 0.000000000000000000, 0.000000000000000000 ) ) ;
#38672 = CARTESIAN_POINT ( 'NONE',  ( 23.14999999999999858, 70.05000000001149374, -46.32880978955918039 ) ) ;
#38673 = DIRECTION ( 'NONE',  ( 0.000000000000000000, -0.3848449534832867891, -0.9229812358755983270 ) ) ;
#38674 = ORIENTED_EDGE ( 'NONE', *, *, #174750, .T. ) ;
#38675 = AXIS2_PLACEMENT_3D ( 'NONE', #183241, #201504, #84075 ) ;
#38677 = DIRECTION ( 'NONE',  ( 0.000000000000000000, -0.01562499999999307672, 0.9998779222360100194 ) ) ;
#38676 = CARTESIAN_POINT ( 'NONE',  ( -16.83233564386402037, 9.930221796595741779, -46.27547933652439838 ) ) ;
#38678 = CARTESIAN_POINT ( 'NONE',  ( -20.54999999999999716, -8.999999999988846255, -43.39396912265245021 ) ) ;
#38679 = B_SPLINE_CURVE_WITH_KNOTS ( 'NONE', 3,
 ( #15342, #72761, #152287, #231815, #94844, #53159, #96118, #175696 ),
 .UNSPECIFIED., .F., .F.,
 ( 4, 2, 2, 4 ),
 ( 0.000000000000000000, 9.550056980125026785E-05, 0.0001910011396025005357, 0.0003820022792049986319 ),
 .UNSPECIFIED. ) ;
#38680 = FACE_OUTER_BOUND ( 'NONE', #164115, .T. ) ;
#38681 = DIRECTION ( 'NONE',  ( 0.000000000000000000, 4.440892098500631684E-15, -1.000000000000000000 ) ) ;
#38682 = DIRECTION ( 'NONE',  ( 0.000000000000000000, -0.8660254037844383745, 0.5000000000000003331 ) ) ;
#38684 = ORIENTED_EDGE ( 'NONE', *, *, #22937, .F. ) ;
#38683 = CIRCLE ( 'NONE', #30318, 0.1000000000000028644 ) ;
#38685 = ORIENTED_EDGE ( 'NONE', *, *, #111895, .T. ) ;
#38686 = AXIS2_PLACEMENT_3D ( 'NONE', #55399, #39758, #20175 ) ;
#38688 = VERTEX_POINT ( 'NONE', #24025 ) ;
#38687 = CIRCLE ( 'NONE', #184420, 0.1000000000000028644 ) ;
#38689 = CARTESIAN_POINT ( 'NONE',  ( 21.00000000000000000, 22.53103078161933936, -230.9224853114453140 ) ) ;
#38690 = AXIS2_PLACEMENT_3D ( 'NONE', #206477, #6984, #12155 ) ;
#38691 = ORIENTED_EDGE ( 'NONE', *, *, #204426, .F. ) ;
#38692 = DIRECTION ( 'NONE',  ( 1.000000000000000000, 0.000000000000000000, 0.000000000000000000 ) ) ;
#38693 = ORIENTED_EDGE ( 'NONE', *, *, #131888, .T. ) ;
#38694 = CARTESIAN_POINT ( 'NONE',  ( -20.94999999999999929, -4.639171910822553535, -233.3276674689317076 ) ) ;
#38695 = EDGE_CURVE ( 'NONE', #100214, #16283, #64418, .T. ) ;
#38696 = CARTESIAN_POINT ( 'NONE',  ( -22.00411653889225505, 75.90096189422567363, -177.2765503521648895 ) ) ;
#38697 = ADVANCED_FACE ( 'NONE', ( #22743 ), #142644, .T. ) ;
#38698 = EDGE_CURVE ( 'NONE', #23382, #237933, #55496, .T. ) ;
#38699 = ORIENTED_EDGE ( 'NONE', *, *, #174578, .F. ) ;
#38700 = DIRECTION ( 'NONE',  ( 1.000000000000000000, 0.000000000000000000, 0.000000000000000000 ) ) ;
#38701 = PRESENTATION_STYLE_ASSIGNMENT (( #197761 ) ) ;
#38702 = CIRCLE ( 'NONE', #30335, 0.5000000000000004441 ) ;
#38703 = AXIS2_PLACEMENT_3D ( 'NONE', #254015, #157540, #75423 ) ;
#38704 = ORIENTED_EDGE ( 'NONE', *, *, #52022, .T. ) ;
#38706 = VERTEX_POINT ( 'NONE', #162252 ) ;
#38705 = CIRCLE ( 'NONE', #67920, 0.1000000000000013933 ) ;
#38707 = VERTEX_POINT ( 'NONE', #219621 ) ;
#38708 = DIRECTION ( 'NONE',  ( -0.000000000000000000, 1.000000000000000000, 6.982962677686266711E-15 ) ) ;
#38709 = CARTESIAN_POINT ( 'NONE',  ( -21.05000000000000071, 77.16270174995064224, -195.5231074845243313 ) ) ;
#38710 = DIRECTION ( 'NONE',  ( 0.000000000000000000, 0.8814952561688476074, -0.4721928772777262417 ) ) ;
#38711 = CARTESIAN_POINT ( 'NONE',  ( -22.39999999999999858, 11.65000000000000036, 0.09999999999999592548 ) ) ;
#38712 = CARTESIAN_POINT ( 'NONE',  ( -23.15000000000000213, 64.35000000001180354, -81.77310748452438816 ) ) ;
#38713 = EDGE_CURVE ( 'NONE', #249890, #118730, #226189, .T. ) ;
#38714 =( BOUNDED_SURFACE ( )  B_SPLINE_SURFACE ( 3, 2, ( 
 ( #196659, #242204, #995 ),
 ( #119713, #18028, #197942 ),
 ( #42726, #37617, #102674 ),
 ( #157592, #40196, #216220 ) ),
 .UNSPECIFIED., .F., .F., .F. ) 
 B_SPLINE_SURFACE_WITH_KNOTS ( ( 4, 4 ),
 ( 3, 3 ),
 ( 0.0006461284895273765793, 0.0007503702773986202284 ),
 ( 0.000000000000000000, 1.000000000000000000 ),
 .UNSPECIFIED. ) 
 GEOMETRIC_REPRESENTATION_ITEM ( )  RATIONAL_B_SPLINE_SURFACE ( (
 ( 1.000000000000000000, 0.7071067811865483499, 1.000000000000000000),
 ( 1.000000000000000000, 0.7076476444648377440, 1.000000000000000000),
 ( 1.000000000000000000, 0.7075727925192694112, 1.000000000000000000),
 ( 1.000000000000000000, 0.7071067811865581199, 1.000000000000000000) ) ) 
 REPRESENTATION_ITEM ( '' )  SURFACE ( )  );
#38716 = DIRECTION ( 'NONE',  ( 0.000000000000000000, 0.000000000000000000, -1.000000000000000000 ) ) ;
#38715 = CARTESIAN_POINT ( 'NONE',  ( 21.04999999999999716, -0.01454569055804403460, -161.0029822135684867 ) ) ;
#38717 = CARTESIAN_POINT ( 'NONE',  ( -12.25000000000000178, 9.350000000011139178, -150.7500000000000284 ) ) ;
#38719 = ORIENTED_EDGE ( 'NONE', *, *, #7637, .F. ) ;
#38718 = CARTESIAN_POINT ( 'NONE',  ( 21.05000000000000071, 85.00000000001159606, -59.62913836187181715 ) ) ;
#38720 = DIRECTION ( 'NONE',  ( 1.000000000000000000, 0.000000000000000000, 0.000000000000000000 ) ) ;
#38721 = EDGE_LOOP ( 'NONE', ( #178997, #16406, #251022, #223042 ) ) ;
#38722 = CARTESIAN_POINT ( 'NONE',  ( -18.59999999999999787, 1.637172712981537659, -179.0821533654719815 ) ) ;
#38723 = ORIENTED_EDGE ( 'NONE', *, *, #88006, .T. ) ;
#38724 = EDGE_LOOP ( 'NONE', ( #108239, #195940, #130204, #179754 ) ) ;
#38725 = DIRECTION ( 'NONE',  ( 1.000000000000000000, 0.000000000000000000, -0.000000000000000000 ) ) ;
#38726 = DIRECTION ( 'NONE',  ( 0.000000000000000000, -1.000000000000000000, 0.000000000000000000 ) ) ;
#38727 = LINE ( 'NONE', #178259, #33736 ) ;
#38728 = EDGE_LOOP ( 'NONE', ( #63992, #22078, #205238, #42054 ) ) ;
#38729 = AXIS2_PLACEMENT_3D ( 'NONE', #64033, #182717, #198408 ) ;
#38730 = CARTESIAN_POINT ( 'NONE',  ( -20.94999999999999929, 12.80863705670245700, -205.3010250813005655 ) ) ;
#38731 = VERTEX_POINT ( 'NONE', #102213 ) ;
#38732 = ORIENTED_EDGE ( 'NONE', *, *, #165971, .F. ) ;
#38733 = VECTOR ( 'NONE', #4480, 1000.000000000000227 ) ;
#38734 = CARTESIAN_POINT ( 'NONE',  ( -23.25000000000000000, 6.982009704867601307, -70.69615211825629331 ) ) ;
#38736 = ORIENTED_EDGE ( 'NONE', *, *, #104029, .F. ) ;
#38735 = EDGE_CURVE ( 'NONE', #167673, #191399, #63736, .T. ) ;
#38737 = CARTESIAN_POINT ( 'NONE',  ( 23.14999999999999503, 31.44980407958351876, -233.5445995079518582 ) ) ;
#38738 = DIRECTION ( 'NONE',  ( 1.000000000000000000, 0.000000000000000000, 0.000000000000000000 ) ) ;
#38739 = EDGE_LOOP ( 'NONE', ( #139695, #157056, #178377, #59298 ) ) ;
#38740 = EDGE_CURVE ( 'NONE', #11705, #168403, #21457, .T. ) ;
#38741 = LINE ( 'NONE', #136524, #248818 ) ;
#38742 = CARTESIAN_POINT ( 'NONE',  ( 22.39999999999999503, 68.20922040163827660, -69.62310748452438247 ) ) ;
#38743 = DIRECTION ( 'NONE',  ( -0.000000000000000000, 0.2128009952263603677, -0.9770955615653313941 ) ) ;
#38744 = ORIENTED_EDGE ( 'NONE', *, *, #65496, .T. ) ;
#38745 = CYLINDRICAL_SURFACE ( 'NONE', #54527, 0.09999999999999939493 ) ;
#38746 = DIRECTION ( 'NONE',  ( 0.000000000000000000, -1.000000000000000000, 0.000000000000000000 ) ) ;
#38747 = ADVANCED_FACE ( 'NONE', ( #43572 ), #218323, .T. ) ;
#38748 = PLANE ( 'NONE',  #169928 ) ;
#38750 = EDGE_LOOP ( 'NONE', ( #151249, #652, #129271, #118389 ) ) ;
#38749 = AXIS2_PLACEMENT_3D ( 'NONE', #232529, #107412, #149132 ) ;
#38752 = ORIENTED_EDGE ( 'NONE', *, *, #97664, .T. ) ;
#38751 = DIRECTION ( 'NONE',  ( 0.000000000000000000, 0.000000000000000000, -1.000000000000000000 ) ) ;
#38753 = ORIENTED_EDGE ( 'NONE', *, *, #152466, .T. ) ;
#38754 = DIRECTION ( 'NONE',  ( 0.000000000000000000, 1.000000000000000000, 0.000000000000000000 ) ) ;
#38755 = CARTESIAN_POINT ( 'NONE',  ( 23.15000000000000213, 88.41227409416111982, -39.02310748452423894 ) ) ;
#38756 = CARTESIAN_POINT ( 'NONE',  ( 21.30000000000002558, 76.00000000001210765, -132.4731074845242915 ) ) ;
#38757 = CARTESIAN_POINT ( 'NONE',  ( -23.15000000000000213, 46.15118611352045974, -240.5321844900040844 ) ) ;
#38758 = CARTESIAN_POINT ( 'NONE',  ( -16.92570016628985030, 9.958788957751016468, -46.12065067003899799 ) ) ;
#38759 = CARTESIAN_POINT ( 'NONE',  ( -18.59999999999999787, 44.55458850188623643, -247.3966190010231969 ) ) ;
#38760 = ORIENTED_EDGE ( 'NONE', *, *, #213084, .T. ) ;
#38761 = EDGE_CURVE ( 'NONE', #123398, #93811, #107407, .T. ) ;
#38762 = FACE_OUTER_BOUND ( 'NONE', #38856, .T. ) ;
#38763 = FACE_OUTER_BOUND ( 'NONE', #16974, .T. ) ;
#38764 = CARTESIAN_POINT ( 'NONE',  ( -18.70000000000000284, 7.986648289447971116, -1.311673547813416718 ) ) ;
#38765 = CARTESIAN_POINT ( 'NONE',  ( 23.14999999999999503, 21.10816309994747186, -233.7904894189133813 ) ) ;
#38766 = AXIS2_PLACEMENT_3D ( 'NONE', #150694, #247213, #244645 ) ;
#38768 = CYLINDRICAL_SURFACE ( 'NONE', #124096, 12.87499999999999467 ) ;
#38767 = CIRCLE ( 'NONE', #101054, 0.09999999999999939493 ) ;
#38769 = ORIENTED_EDGE ( 'NONE', *, *, #146101, .F. ) ;
#38770 = EDGE_LOOP ( 'NONE', ( #251893, #249151, #167261 ) ) ;
#38771 = CARTESIAN_POINT ( 'NONE',  ( -21.05000000000000071, 64.25000000001196554, -110.0379132551783243 ) ) ;
#38772 = DIRECTION ( 'NONE',  ( 0.000000000000000000, -6.853228547068871147E-15, 1.000000000000000000 ) ) ;
#38774 = EDGE_CURVE ( 'NONE', #136069, #212664, #242794, .T. ) ;
#38773 = DIRECTION ( 'NONE',  ( 2.694716079187272946E-16, -1.000000000000000000, 0.000000000000000000 ) ) ;
#38775 = DIRECTION ( 'NONE',  ( 0.7071067811865127117, 0.7071067811865821007, 0.000000000000000000 ) ) ;
#38776 = CARTESIAN_POINT ( 'NONE',  ( -20.85000000000000142, 74.73788286442776041, -233.7359682632885267 ) ) ;
#38777 = ORIENTED_EDGE ( 'NONE', *, *, #80620, .F. ) ;
#38778 = LINE ( 'NONE', #257761, #222317 ) ;
#38779 = EDGE_CURVE ( 'NONE', #162952, #135929, #126271, .T. ) ;
#38780 = ADVANCED_FACE ( 'NONE', ( #10869 ), #66978, .F. ) ;
#38781 = CARTESIAN_POINT ( 'NONE',  ( -21.14999999999999858, 6.540656951712397138, -100.6000000000000369 ) ) ;
#38782 = EDGE_LOOP ( 'NONE', ( #7711, #144404, #135113, #138228 ) ) ;
#38783 = CIRCLE ( 'NONE', #113610, 0.3999999999999975797 ) ;
#38784 = AXIS2_PLACEMENT_3D ( 'NONE', #170332, #131150, #210691 ) ;
#38785 = DIRECTION ( 'NONE',  ( 1.000000000000000000, 0.000000000000000000, 0.000000000000000000 ) ) ;
#38786 = EDGE_CURVE ( 'NONE', #194489, #34148, #147117, .T. ) ;
#38787 = EDGE_CURVE ( 'NONE', #177157, #178346, #168705, .T. ) ;
#38788 = ORIENTED_EDGE ( 'NONE', *, *, #25886, .F. ) ;
#38789 = DIRECTION ( 'NONE',  ( -1.000000000000000000, 1.335000415235278971E-16, -2.979993593738921214E-16 ) ) ;
#38790 = VECTOR ( 'NONE', #158660, 1000.000000000000227 ) ;
#38791 = EDGE_LOOP ( 'NONE', ( #1317, #162971, #157222, #90027 ) ) ;
#38792 = DIRECTION ( 'NONE',  ( -0.000000000000000000, -0.2617529984165031243, -0.9651348961777157509 ) ) ;
#38793 = DIRECTION ( 'NONE',  ( -3.265361837132813093E-16, 1.000000000000000000, 0.000000000000000000 ) ) ;
#38795 = EDGE_CURVE ( 'NONE', #197646, #129441, #209473, .T. ) ;
#38794 = PLANE ( 'NONE',  #69984 ) ;
#38796 = CARTESIAN_POINT ( 'NONE',  ( 18.59999999999996945, 65.66751761918648356, -63.92826094061123143 ) ) ;
#38798 = AXIS2_PLACEMENT_3D ( 'NONE', #73434, #96781, #17296 ) ;
#38797 = CARTESIAN_POINT ( 'NONE',  ( 18.49999999999999645, 76.00000000001170974, -69.52310748452431710 ) ) ;
#38799 = DIRECTION ( 'NONE',  ( 0.000000000000000000, 0.000000000000000000, -1.000000000000000000 ) ) ;
#38801 = FACE_OUTER_BOUND ( 'NONE', #52399, .T. ) ;
#38800 = AXIS2_PLACEMENT_3D ( 'NONE', #58085, #137627, #133792 ) ;
#38802 = CIRCLE ( 'NONE', #51229, 0.09999999999999976963 ) ;
#38803 = CARTESIAN_POINT ( 'NONE',  ( -18.60000000000000142, -9.523954320741632174, -107.3820170568273795 ) ) ;
#38804 = LINE ( 'NONE', #157494, #74865 ) ;
#38805 = ADVANCED_FACE ( 'NONE', ( #25306 ), #201108, .F. ) ;
#38806 = CARTESIAN_POINT ( 'NONE',  ( 18.50000000000000355, -7.661135498422202872, -210.0861805852114514 ) ) ;
#38807 = DIRECTION ( 'NONE',  ( 1.000000000000000000, 0.000000000000000000, 0.000000000000000000 ) ) ;
#38808 = DIRECTION ( 'NONE',  ( 0.000000000000000000, -0.9126074666063660468, -0.4088369013363524762 ) ) ;
#38809 = EDGE_CURVE ( 'NONE', #220045, #75643, #230314, .T. ) ;
#38810 = EDGE_CURVE ( 'NONE', #256646, #113878, #76183, .T. ) ;
#38811 = DIRECTION ( 'NONE',  ( 0.000000000000000000, -2.255140518769784599E-13, 1.000000000000000000 ) ) ;
#38812 = DIRECTION ( 'NONE',  ( 1.000000000000000000, 0.000000000000000000, 0.000000000000000000 ) ) ;
#38813 = EDGE_LOOP ( 'NONE', ( #190694, #208642, #53782, #235912 ) ) ;
#38814 =( BOUNDED_SURFACE ( )  B_SPLINE_SURFACE ( 3, 2, ( 
 ( #23102, #145581, #225102 ),
 ( #46473, #126018, #205549 ),
 ( #26961, #182162, #83015 ),
 ( #162601, #63475, #28248 ) ),
 .UNSPECIFIED., .F., .F., .T. ) 
 B_SPLINE_SURFACE_WITH_KNOTS ( ( 4, 4 ),
 ( 3, 3 ),
 ( -3.469446951953614189E-18, 0.001979672783031532438 ),
 ( 0.000000000000000000, 1.000000000000000000 ),
 .UNSPECIFIED. ) 
 GEOMETRIC_REPRESENTATION_ITEM ( )  RATIONAL_B_SPLINE_SURFACE ( (
 ( 1.000000000000000000, 0.7103081912008198939, 1.000000000000000000),
 ( 1.000000000000000000, 0.7104998333558888435, 1.000000000000000000),
 ( 1.000000000000000000, 0.7107238315754828006, 1.000000000000000000),
 ( 1.000000000000000000, 0.7110073749539717047, 1.000000000000000000) ) ) 
 REPRESENTATION_ITEM ( '' )  SURFACE ( )  );
#38815 = CARTESIAN_POINT ( 'NONE',  ( 20.94999999999999929, 1.115600667400684642E-11, -134.0000000000000000 ) ) ;
#38817 = ADVANCED_FACE ( 'NONE', ( #164803 ), #101270, .T. ) ;
#38816 = CARTESIAN_POINT ( 'NONE',  ( -20.64999999999999858, 2.399999999999999467, -20.27537807723789953 ) ) ;
#38818 = CARTESIAN_POINT ( 'NONE',  ( 20.11144452914042091, 9.933610851134151432, -41.39029345395471893 ) ) ;
#38819 = ORIENTED_EDGE ( 'NONE', *, *, #221686, .F. ) ;
#38820 = FACE_OUTER_BOUND ( 'NONE', #236458, .T. ) ;
#38821 = ADVANCED_FACE ( 'NONE', ( #107380 ), #169982, .F. ) ;
#38822 = EDGE_CURVE ( 'NONE', #70992, #172403, #47143, .T. ) ;
#38823 = FACE_OUTER_BOUND ( 'NONE', #153184, .T. ) ;
#38824 = AXIS2_PLACEMENT_3D ( 'NONE', #224489, #4157, #206220 ) ;
#38825 = VERTEX_POINT ( 'NONE', #68271 ) ;
#38826 = DIRECTION ( 'NONE',  ( 0.000000000000000000, -0.000000000000000000, -1.000000000000000000 ) ) ;
#38827 = CARTESIAN_POINT ( 'NONE',  ( -23.15000000000000213, 1.115600667400684642E-11, -200.9999999999999432 ) ) ;
#38828 = EDGE_CURVE ( 'NONE', #168421, #138590, #221926, .T. ) ;
#38829 = TOROIDAL_SURFACE ( 'NONE', #246913, 0.2000000000000000111, 0.1000000000000000056 ) ;
#38830 = ORIENTED_EDGE ( 'NONE', *, *, #97948, .F. ) ;
#38831 = ORIENTED_EDGE ( 'NONE', *, *, #245208, .T. ) ;
#38833 = DIRECTION ( 'NONE',  ( -1.000000000000000000, 0.000000000000000000, -0.000000000000000000 ) ) ;
#38832 = AXIS2_PLACEMENT_3D ( 'NONE', #142800, #223631, #28051 ) ;
#38834 = AXIS2_PLACEMENT_3D ( 'NONE', #32924, #154154, #54981 ) ;
#38835 = ORIENTED_EDGE ( 'NONE', *, *, #22113, .T. ) ;
#38836 = EDGE_CURVE ( 'NONE', #247898, #129691, #129531, .T. ) ;
#38837 = CARTESIAN_POINT ( 'NONE',  ( -23.15000000000000213, 23.68770167995059595, -252.8127582590406348 ) ) ;
#38838 = EDGE_CURVE ( 'NONE', #231120, #175831, #92944, .T. ) ;
#38839 = CARTESIAN_POINT ( 'NONE',  ( -20.85000000000000142, 68.97833521811233481, -166.2895420826271220 ) ) ;
#38841 = CIRCLE ( 'NONE', #142845, 0.09999999999999939493 ) ;
#38840 = CARTESIAN_POINT ( 'NONE',  ( 21.14999999999999858, 33.98486250090727623, -243.5821103306120108 ) ) ;
#38842 = CYLINDRICAL_SURFACE ( 'NONE', #212752, 0.09999999999999939493 ) ;
#38843 = DIRECTION ( 'NONE',  ( -1.000000000000000000, -0.000000000000000000, -0.000000000000000000 ) ) ;
#38844 = CARTESIAN_POINT ( 'NONE',  ( 21.05000000000000071, 49.36776662947724503, -253.7196102226803021 ) ) ;
#38845 = CARTESIAN_POINT ( 'NONE',  ( -21.05000000000000071, 8.780520186313289344, -245.4165333277510115 ) ) ;
#38847 = CARTESIAN_POINT ( 'NONE',  ( 22.88900146558018989, 8.703904791123973084, -146.6500000000000341 ) ) ;
#38846 = CIRCLE ( 'NONE', #147165, 2.000000000000012879 ) ;
#38848 = AXIS2_PLACEMENT_3D ( 'NONE', #238449, #62385, #141907 ) ;
#38850 = ORIENTED_EDGE ( 'NONE', *, *, #118886, .F. ) ;
#38849 = CARTESIAN_POINT ( 'NONE',  ( -18.45037301276669339, -9.490200447530787287, -40.51267413641429727 ) ) ;
#38851 = ORIENTED_EDGE ( 'NONE', *, *, #151758, .F. ) ;
#38852 = CARTESIAN_POINT ( 'NONE',  ( -21.05000000000000071, 64.25000000001161027, -62.73924182154625129 ) ) ;
#38855 = ORIENTED_EDGE ( 'NONE', *, *, #250962, .F. ) ;
#38854 = CARTESIAN_POINT ( 'NONE',  ( 18.59999999999999076, 68.92903212821283887, -65.77654326265606244 ) ) ;
#38853 = LINE ( 'NONE', #37572, #2798 ) ;
#38856 = EDGE_LOOP ( 'NONE', ( #88927, #53878, #118832 ) ) ;
#38857 = CYLINDRICAL_SURFACE ( 'NONE', #195665, 1.749999999999999778 ) ;
#38858 = CARTESIAN_POINT ( 'NONE',  ( 20.04142135623730070, 64.35000000001254250, -182.1731074845244507 ) ) ;
#38859 = VECTOR ( 'NONE', #229416, 1000.000000000000000 ) ;
#38860 = CARTESIAN_POINT ( 'NONE',  ( 20.94999999999999929, 7.128833340094563376, -233.7327013124401276 ) ) ;
#38861 = CARTESIAN_POINT ( 'NONE',  ( 18.54147908293617775, -9.463261657928100590, -7.048948896755796945 ) ) ;
#38862 = DIRECTION ( 'NONE',  ( -0.000000000000000000, -0.8660254037844411501, -0.4999999999999956701 ) ) ;
#38863 = FACE_OUTER_BOUND ( 'NONE', #40628, .T. ) ;
#38864 = AXIS2_PLACEMENT_3D ( 'NONE', #60206, #4090, #139733 ) ;
#38865 = DIRECTION ( 'NONE',  ( 0.000000000000000000, -0.4721928772777346239, -0.8814952561688430555 ) ) ;
#38866 = AXIS2_PLACEMENT_3D ( 'NONE', #41135, #63219, #159781 ) ;
#38867 = DIRECTION ( 'NONE',  ( 0.000000000000000000, 0.9209589331071864615, -0.3896596508878908960 ) ) ;
#38868 = AXIS2_PLACEMENT_3D ( 'NONE', #170803, #11691, #32561 ) ;
#38870 = ORIENTED_EDGE ( 'NONE', *, *, #160481, .F. ) ;
#38869 = EDGE_CURVE ( 'NONE', #130685, #227551, #184347, .T. ) ;
#38871 = EDGE_LOOP ( 'NONE', ( #63338, #223007, #89737, #211927 ) ) ;
#38872 = CYLINDRICAL_SURFACE ( 'NONE', #168703, 1.500000000000001332 ) ;
#38873 = EDGE_CURVE ( 'NONE', #183570, #126269, #46123, .T. ) ;
#38874 = ORIENTED_EDGE ( 'NONE', *, *, #202106, .F. ) ;
#38875 = CARTESIAN_POINT ( 'NONE',  ( -21.05000000000000071, 76.25610579210386675, -69.55800392619661920 ) ) ;
#38876 = ORIENTED_EDGE ( 'NONE', *, *, #77298, .F. ) ;
#38878 = AXIS2_PLACEMENT_3D ( 'NONE', #37665, #95044, #195460 ) ;
#38877 = DIRECTION ( 'NONE',  ( -1.836970198721029934E-16, -1.000000000000000000, -6.982962677686266711E-15 ) ) ;
#38879 = AXIS2_PLACEMENT_3D ( 'NONE', #224469, #5399, #79809 ) ;
#38880 = CIRCLE ( 'NONE', #76260, 0.2000000000000057288 ) ;
#38881 = AXIS2_PLACEMENT_3D ( 'NONE', #152327, #154897, #125356 ) ;
#38882 = CARTESIAN_POINT ( 'NONE',  ( -18.59999999999999787, 2.859758780633683273, -208.6670499591424459 ) ) ;
#38883 = DIRECTION ( 'NONE',  ( 0.000000000000000000, -6.982962677686266711E-15, 1.000000000000000000 ) ) ;
#38884 = CARTESIAN_POINT ( 'NONE',  ( 18.60000000000000142, -9.523946312306554418, -207.8820279953382055 ) ) ;
#38885 = DIRECTION ( 'NONE',  ( 1.000000000000000000, -0.000000000000000000, -0.000000000000000000 ) ) ;
#38886 = VERTEX_POINT ( 'NONE', #109950 ) ;
#38887 = CARTESIAN_POINT ( 'NONE',  ( 20.94999999999999929, 1.115600667400684642E-11, -67.00000000000000000 ) ) ;
#38888 = CARTESIAN_POINT ( 'NONE',  ( 18.59999999999999076, 11.65000000001115943, -200.9999999999999432 ) ) ;
#38889 = LINE ( 'NONE', #54579, #139495 ) ;
#38890 = CARTESIAN_POINT ( 'NONE',  ( -23.15000000000000213, -3.770473190032741062, -225.9805569534692324 ) ) ;
#38891 = DIRECTION ( 'NONE',  ( 0.000000000000000000, 0.9126074666063791474, 0.4088369013363231663 ) ) ;
#38892 = EDGE_CURVE ( 'NONE', #20386, #247339, #1360, .T. ) ;
#38893 = ORIENTED_EDGE ( 'NONE', *, *, #46841, .T. ) ;
#38894 = DIRECTION ( 'NONE',  ( -0.000000000000000000, 1.000000000000000000, 6.982962677686266711E-15 ) ) ;
#38895 = AXIS2_PLACEMENT_3D ( 'NONE', #72919, #251510, #152451 ) ;
#38896 = ORIENTED_EDGE ( 'NONE', *, *, #83781, .T. ) ;
#38899 = VERTEX_POINT ( 'NONE', #70868 ) ;
#38898 = CARTESIAN_POINT ( 'NONE',  ( -20.64999999999999858, 74.05981308412442843, -157.1939882734710352 ) ) ;
#38897 = DIRECTION ( 'NONE',  ( 0.000000000000000000, 0.8659859643398412077, -0.5000683049008356473 ) ) ;
#38900 = VECTOR ( 'NONE', #191208, 1000.000000000000000 ) ;
#38901 = AXIS2_PLACEMENT_3D ( 'NONE', #18029, #197943, #192835 ) ;
#38902 = DIRECTION ( 'NONE',  ( -1.000000000000000000, -0.000000000000000000, -0.000000000000000000 ) ) ;
#38903 = AXIS2_PLACEMENT_3D ( 'NONE', #88289, #171745, #54316 ) ;
#38904 = DIRECTION ( 'NONE',  ( 1.000000000000000000, 0.000000000000000000, 0.000000000000000000 ) ) ;
#38905 = ORIENTED_EDGE ( 'NONE', *, *, #13341, .F. ) ;
#38906 = DIRECTION ( 'NONE',  ( 0.000000000000000000, -0.4930308989874653269, -0.8700118002898649117 ) ) ;
#38907 = CARTESIAN_POINT ( 'NONE',  ( 20.09999999999999787, 9.749999999999982236, -12.65000000000000391 ) ) ;
#38908 = CARTESIAN_POINT ( 'NONE',  ( -16.97092634996667471, 10.00088896634854052, -12.63014276629761135 ) ) ;
#38910 = EDGE_LOOP ( 'NONE', ( #160492, #53391, #79954, #37463 ) ) ;
#38909 = CARTESIAN_POINT ( 'NONE',  ( 23.14999999999999858, 1.115600667400684642E-11, -200.9999999999999432 ) ) ;
#38911 = DIRECTION ( 'NONE',  ( 0.000000000000000000, 0.000000000000000000, -1.000000000000000000 ) ) ;
#38912 = EDGE_LOOP ( 'NONE', ( #214633, #11531, #107837, #231440 ) ) ;
#38913 = CARTESIAN_POINT ( 'NONE',  ( 23.15000000000000213, 60.94692742449272771, -251.5456325903398067 ) ) ;
#38914 = CARTESIAN_POINT ( 'NONE',  ( 20.94999999999999929, -8.730841121495322099, -23.90192528101566438 ) ) ;
#38915 = CARTESIAN_POINT ( 'NONE',  ( -15.55912972643740488, 67.50912972644923116, -82.07310748452437110 ) ) ;
#38916 = VERTEX_POINT ( 'NONE', #166121 ) ;
#38917 = CARTESIAN_POINT ( 'NONE',  ( 20.85000000000000142, -1.835859311432481045, -78.50443916879852679 ) ) ;
#38918 = ORIENTED_EDGE ( 'NONE', *, *, #182863, .F. ) ;
#38919 = LINE ( 'NONE', #101389, #148008 ) ;
#38920 = AXIS2_PLACEMENT_3D ( 'NONE', #158178, #236379, #57729 ) ;
#38921 = CARTESIAN_POINT ( 'NONE',  ( 18.59999999999999076, 65.79142135624982757, -178.7731074845244450 ) ) ;
#38922 = CARTESIAN_POINT ( 'NONE',  ( -16.93388492042258875, 9.988541822527059466, -46.09945487681383014 ) ) ;
#38923 = EDGE_LOOP ( 'NONE', ( #33363, #181667, #21981, #41316 ) ) ;
#38924 = CARTESIAN_POINT ( 'NONE',  ( -18.59999999999999787, 47.95459712139159336, -246.5019368548292675 ) ) ;
#38925 = EDGE_CURVE ( 'NONE', #206263, #220667, #121995, .T. ) ;
#38926 = DIRECTION ( 'NONE',  ( 1.000000000000000000, 0.000000000000000000, 0.000000000000000000 ) ) ;
#38927 = CARTESIAN_POINT ( 'NONE',  ( -20.94999999999999929, 64.25000000001250555, -176.8069731475025890 ) ) ;
#38928 = EDGE_CURVE ( 'NONE', #227981, #248454, #94432, .T. ) ;
#38929 = ORIENTED_EDGE ( 'NONE', *, *, #185988, .F. ) ;
#38930 = CARTESIAN_POINT ( 'NONE',  ( 21.05000000000000071, 71.00000000001180922, -81.42837350343744163 ) ) ;
#38931 = LINE ( 'NONE', #196698, #27305 ) ;
#38933 = CARTESIAN_POINT ( 'NONE',  ( 21.05000000000000071, 69.45934304831041572, -69.42310748452437963 ) ) ;
#38932 = TOROIDAL_SURFACE ( 'NONE', #68142, 11.65000000000000036, 0.1000000000000000056 ) ;
#38934 = CIRCLE ( 'NONE', #118026, 11.65000000000000036 ) ;
#38935 = ORIENTED_EDGE ( 'NONE', *, *, #62930, .T. ) ;
#38936 = AXIS2_PLACEMENT_3D ( 'NONE', #36800, #214119, #74647 ) ;
#38937 = ADVANCED_FACE ( 'NONE', ( #92958 ), #68017, .F. ) ;
#38938 = DIRECTION ( 'NONE',  ( 0.000000000000000000, -0.1350103645451835865, -0.9908441862701605762 ) ) ;
#38939 = VERTEX_POINT ( 'NONE', #172558 ) ;
#38941 = ORIENTED_EDGE ( 'NONE', *, *, #247649, .T. ) ;
#38940 = DIRECTION ( 'NONE',  ( -0.000000000000000000, 0.4088369013363281623, -0.9126074666063771490 ) ) ;
#38942 = EDGE_CURVE ( 'NONE', #67930, #142779, #63933, .T. ) ;
#38945 = VERTEX_POINT ( 'NONE', #232501 ) ;
#38944 = EDGE_LOOP ( 'NONE', ( #125206, #228912, #18051, #187040 ) ) ;
#38943 = CARTESIAN_POINT ( 'NONE',  ( -21.14250536705909411, -1.950243336657294609E-16, 6.518172176880757895 ) ) ;
#38946 = DIRECTION ( 'NONE',  ( 4.377807931758638000E-15, -0.7280513885558889120, 0.6855225566105335178 ) ) ;
#38947 = CARTESIAN_POINT ( 'NONE',  ( -20.94403535211772294, 65.69367753730607262, -30.51892380663481674 ) ) ;
#38948 = CARTESIAN_POINT ( 'NONE',  ( 16.87683809663750267, 9.950000000011138823, -113.1500000000000341 ) ) ;
#38949 = VECTOR ( 'NONE', #30460, 999.9999999999998863 ) ;
#38950 = EDGE_CURVE ( 'NONE', #8389, #113973, #192924, .T. ) ;
#38951 = CARTESIAN_POINT ( 'NONE',  ( -16.77308656112214180, 12.41407453858650278, -211.2430777180555026 ) ) ;
#38952 = CARTESIAN_POINT ( 'NONE',  ( 21.14999999999999858, 34.01125473725045367, -243.8802146427659352 ) ) ;
#38953 = CYLINDRICAL_SURFACE ( 'NONE', #80719, 4.000000000000003553 ) ;
#38954 = CIRCLE ( 'NONE', #72272, 0.09999999999999854838 ) ;
#38955 = CYLINDRICAL_SURFACE ( 'NONE', #138926, 0.09999999999999939493 ) ;
#38957 = DIRECTION ( 'NONE',  ( 0.000000000000000000, 0.000000000000000000, 1.000000000000000000 ) ) ;
#38956 = CARTESIAN_POINT ( 'NONE',  ( -18.59999999999999787, 74.93036000061670165, -233.6816308724374949 ) ) ;
#38958 = AXIS2_PLACEMENT_3D ( 'NONE', #124040, #101868, #219263 ) ;
#38959 = ORIENTED_EDGE ( 'NONE', *, *, #179077, .T. ) ;
#38960 = ORIENTED_EDGE ( 'NONE', *, *, #141279, .F. ) ;
#38961 = AXIS2_PLACEMENT_3D ( 'NONE', #41499, #157618, #21926 ) ;
#38962 = CARTESIAN_POINT ( 'NONE',  ( -21.00000000000000000, -1.885425182446133885, -11.49641995933507843 ) ) ;
#38964 = ORIENTED_EDGE ( 'NONE', *, *, #13639, .T. ) ;
#38963 = CARTESIAN_POINT ( 'NONE',  ( -23.15000000000000213, -11.48912529306489994, -197.8999999999999773 ) ) ;
#38965 = CARTESIAN_POINT ( 'NONE',  ( 20.94999999999999929, 71.18691588786226987, -81.46462524104816794 ) ) ;
#38966 = ORIENTED_EDGE ( 'NONE', *, *, #184685, .F. ) ;
#38967 = ADVANCED_FACE ( 'NONE', ( #53842 ), #251146, .T. ) ;
#38968 = FACE_OUTER_BOUND ( 'NONE', #82031, .T. ) ;
#38969 = VERTEX_POINT ( 'NONE', #171273 ) ;
#38970 = DIRECTION ( 'NONE',  ( 0.000000000000000000, -1.000000000000000000, -6.982962677686266711E-15 ) ) ;
#38971 = AXIS2_PLACEMENT_3D ( 'NONE', #59482, #43815, #200319 ) ;
#38972 = AXIS2_PLACEMENT_3D ( 'NONE', #104642, #5556, #44719 ) ;
#38973 = ORIENTED_EDGE ( 'NONE', *, *, #175200, .T. ) ;
#38974 = CIRCLE ( 'NONE', #142981, 0.1000000000000013933 ) ;
#38975 = FACE_OUTER_BOUND ( 'NONE', #23122, .T. ) ;
#38976 = CARTESIAN_POINT ( 'NONE',  ( 23.15000000000000213, 87.48912529308779540, -72.62310748452422615 ) ) ;
#38978 = ORIENTED_EDGE ( 'NONE', *, *, #90164, .T. ) ;
#38977 = ORIENTED_EDGE ( 'NONE', *, *, #32228, .T. ) ;
#38979 = ORIENTED_EDGE ( 'NONE', *, *, #193434, .T. ) ;
#38980 = PLANE ( 'NONE',  #102914 ) ;
#38981 = ORIENTED_EDGE ( 'NONE', *, *, #1338, .F. ) ;
#38982 = VERTEX_POINT ( 'NONE', #215475 ) ;
#38984 = DIRECTION ( 'NONE',  ( 0.000000000000000000, 1.000000000000000000, 0.000000000000000000 ) ) ;
#38983 = CIRCLE ( 'NONE', #242959, 0.5000000000000004441 ) ;
#38986 = EDGE_LOOP ( 'NONE', ( #194711, #253125, #136962, #235214 ) ) ;
#38985 = FACE_OUTER_BOUND ( 'NONE', #170860, .T. ) ;
#38988 = CARTESIAN_POINT ( 'NONE',  ( 20.95325940946048249, 65.47660992931604085, -162.4586453552843466 ) ) ;
#38987 = FACE_OUTER_BOUND ( 'NONE', #24150, .T. ) ;
#38989 = DIRECTION ( 'NONE',  ( 0.000000000000000000, 0.1022405907414316584, 0.9947597004326437231 ) ) ;
#38990 = DIRECTION ( 'NONE',  ( 1.000000000000000000, -0.000000000000000000, 0.000000000000000000 ) ) ;
#38991 = FACE_OUTER_BOUND ( 'NONE', #168885, .T. ) ;
#38992 = ORIENTED_EDGE ( 'NONE', *, *, #201553, .F. ) ;
#38993 = AXIS2_PLACEMENT_3D ( 'NONE', #79498, #116089, #136921 ) ;
#38994 = CIRCLE ( 'NONE', #150829, 0.09999999999999967248 ) ;
#38995 = TOROIDAL_SURFACE ( 'NONE', #184708, 0.4000000000000003553, 0.1000000000000000056 ) ;
#38996 = VERTEX_POINT ( 'NONE', #192086 ) ;
#38997 = DIRECTION ( 'NONE',  ( -1.000000000000000000, 0.000000000000000000, 0.000000000000000000 ) ) ;
#38998 = DIRECTION ( 'NONE',  ( -1.073024830501117923E-15, 0.9126074666063771490, 0.4088369013363281623 ) ) ;
#38999 = CARTESIAN_POINT ( 'NONE',  ( -20.54999999999999716, 1.925233644870967487, -121.2697564668739005 ) ) ;
#39000 = ORIENTED_EDGE ( 'NONE', *, *, #214254, .T. ) ;
#39001 = DIRECTION ( 'NONE',  ( 0.000000000000000000, 0.4721928772777346239, 0.8814952561688430555 ) ) ;
#39002 = EDGE_CURVE ( 'NONE', #48376, #85650, #252034, .T. ) ;
#39003 = LINE ( 'NONE', #118547, #96982 ) ;
#39004 = DIRECTION ( 'NONE',  ( -1.000000000000000000, -0.000000000000000000, -0.000000000000000000 ) ) ;
#39005 = EDGE_LOOP ( 'NONE', ( #30638, #185903, #51224, #11639 ) ) ;
#39006 = ORIENTED_EDGE ( 'NONE', *, *, #119360, .F. ) ;
#39007 = DIRECTION ( 'NONE',  ( 0.000000000000000000, -1.000000000000000000, 0.000000000000000000 ) ) ;
#39008 = CARTESIAN_POINT ( 'NONE',  ( -16.77977881697927032, 66.05339806647916134, -123.8617289114093154 ) ) ;
#39009 = ORIENTED_EDGE ( 'NONE', *, *, #248590, .T. ) ;
#39010 = DIRECTION ( 'NONE',  ( 0.000000000000000000, -8.326672684688666480E-14, 1.000000000000000000 ) ) ;
#39011 = ORIENTED_EDGE ( 'NONE', *, *, #209001, .T. ) ;
#39012 = DIRECTION ( 'NONE',  ( -0.000000000000000000, 0.08413937888704771384, -0.9964539953858891908 ) ) ;
#39014 = ADVANCED_FACE ( 'NONE', ( #16025 ), #155544, .F. ) ;
#39013 = CARTESIAN_POINT ( 'NONE',  ( -21.14999999999999858, 64.35000000001214460, -136.5231074845243597 ) ) ;
#39016 = DIRECTION ( 'NONE',  ( 6.938893903907224433E-15, -1.000000000000000000, -2.891205793294679805E-16 ) ) ;
#39015 = CARTESIAN_POINT ( 'NONE',  ( -20.94999999999999929, 76.25610579210437834, -136.5580039261965908 ) ) ;
#39017 = CARTESIAN_POINT ( 'NONE',  ( 18.53317502108576775, 65.67736539654997330, -164.4625116876572406 ) ) ;
#39018 = DIRECTION ( 'NONE',  ( 2.952720810173289112E-16, -1.000000000000000000, 0.000000000000000000 ) ) ;
#39019 = AXIS2_PLACEMENT_3D ( 'NONE', #221276, #243419, #64780 ) ;
#39020 = EDGE_CURVE ( 'NONE', #57105, #156346, #247059, .T. ) ;
#39021 = EDGE_CURVE ( 'NONE', #93118, #176327, #176188, .T. ) ;
#39022 = AXIS2_PLACEMENT_3D ( 'NONE', #2757, #236246, #40666 ) ;
#39023 = CARTESIAN_POINT ( 'NONE',  ( 23.14999999999999858, 78.10000000001245724, -170.0231074845243313 ) ) ;
#39024 = VECTOR ( 'NONE', #195363, 1000.000000000000000 ) ;
#39026 = ORIENTED_EDGE ( 'NONE', *, *, #7011, .T. ) ;
#39025 = VERTEX_POINT ( 'NONE', #231214 ) ;
#39027 = VERTEX_POINT ( 'NONE', #132096 ) ;
#39028 = CARTESIAN_POINT ( 'NONE',  ( 23.24999999999999645, 76.00000000001267608, -203.5231074845243597 ) ) ;
#39029 = DIRECTION ( 'NONE',  ( 0.000000000000000000, -6.982962677686266711E-15, 1.000000000000000000 ) ) ;
#39030 = AXIS2_PLACEMENT_3D ( 'NONE', #63997, #50825, #73027 ) ;
#39031 = DIRECTION ( 'NONE',  ( -1.000000000000000000, -0.000000000000000000, -0.000000000000000000 ) ) ;
#39032 = CARTESIAN_POINT ( 'NONE',  ( -23.24999999999999645, -9.599999999988845900, -140.6001893912220737 ) ) ;
#39033 = ADVANCED_FACE ( 'NONE', ( #34306 ), #26335, .T. ) ;
#39035 = DIRECTION ( 'NONE',  ( 0.000000000000000000, 0.000000000000000000, -1.000000000000000000 ) ) ;
#39034 = CARTESIAN_POINT ( 'NONE',  ( 20.53930447207976684, 8.977148687524273640, -8.442507141577925367 ) ) ;
#39036 = VERTEX_POINT ( 'NONE', #212917 ) ;
#39037 = CARTESIAN_POINT ( 'NONE',  ( 20.85000000000000142, 0.000000000000000000, -41.30000000000000426 ) ) ;
#39038 = ORIENTED_EDGE ( 'NONE', *, *, #3115, .F. ) ;
#39039 = CIRCLE ( 'NONE', #122220, 0.1000000000000072220 ) ;
#39040 = ADVANCED_FACE ( 'NONE', ( #154275 ), #254576, .T. ) ;
#39041 = CARTESIAN_POINT ( 'NONE',  ( -23.25000000000000000, 87.75000000001173817, -81.27310748452423184 ) ) ;
#39042 = ORIENTED_EDGE ( 'NONE', *, *, #60726, .T. ) ;
#39043 = EDGE_LOOP ( 'NONE', ( #251823, #126220, #60794, #234875 ) ) ;
#39044 = CARTESIAN_POINT ( 'NONE',  ( 21.04999999999999716, 69.69554417806445201, -136.5020720079842249 ) ) ;
#39045 = AXIS2_PLACEMENT_3D ( 'NONE', #95670, #77382, #136061 ) ;
#39046 = FACE_OUTER_BOUND ( 'NONE', #207361, .T. ) ;
#39047 = CARTESIAN_POINT ( 'NONE',  ( -16.87683809663752399, 66.13411015067963206, -49.29053429159418442 ) ) ;
#39048 = AXIS2_PLACEMENT_3D ( 'NONE', #252842, #251562, #233317 ) ;
#39049 = CARTESIAN_POINT ( 'NONE',  ( -23.15000000000000213, -11.64999999998884483, -63.89999999999999858 ) ) ;
#39050 = AXIS2_PLACEMENT_3D ( 'NONE', #4031, #82250, #19765 ) ;
#39051 = CYLINDRICAL_SURFACE ( 'NONE', #146637, 0.1000000000000028644 ) ;
#39052 = VERTEX_POINT ( 'NONE', #35592 ) ;
#39053 = ORIENTED_EDGE ( 'NONE', *, *, #231761, .F. ) ;
#39054 = DIRECTION ( 'NONE',  ( 0.000000000000000000, -0.3945274997758418944, 0.9188841341108372474 ) ) ;
#39055 = EDGE_CURVE ( 'NONE', #107243, #76307, #170611, .T. ) ;
#39056 = FACE_OUTER_BOUND ( 'NONE', #135533, .T. ) ;
#39058 = ORIENTED_EDGE ( 'NONE', *, *, #105567, .T. ) ;
#39057 = ADVANCED_FACE ( 'NONE', ( #178963 ), #42001, .F. ) ;
#39059 = DIRECTION ( 'NONE',  ( 0.000000000000000000, -1.000000000000000000, -6.860497997771532351E-15 ) ) ;
#39060 = ADVANCED_FACE ( 'NONE', ( #161948 ), #221869, .F. ) ;
#39062 = CIRCLE ( 'NONE', #68448, 0.09999999999998898659 ) ;
#39061 = DIRECTION ( 'NONE',  ( 0.000000000000000000, -6.938893903907229955E-15, 1.000000000000000000 ) ) ;
#39063 = CARTESIAN_POINT ( 'NONE',  ( -21.07928932188134041, 75.90110485435778287, -142.8516241409176075 ) ) ;
#39064 = FACE_OUTER_BOUND ( 'NONE', #49002, .T. ) ;
#39065 = CARTESIAN_POINT ( 'NONE',  ( 20.73486653747088582, 9.052352027204005225, -208.4953267290897259 ) ) ;
#39067 = CARTESIAN_POINT ( 'NONE',  ( 20.94999999999999929, 19.00443933019177223, -232.7770257915295531 ) ) ;
#39066 = CARTESIAN_POINT ( 'NONE',  ( -16.92563707711778420, 30.24240912587386276, -234.8048286477303179 ) ) ;
#39068 = CARTESIAN_POINT ( 'NONE',  ( -23.15000000000000213, 6.268811756569107274, -220.3853799378769622 ) ) ;
#39069 = CARTESIAN_POINT ( 'NONE',  ( 21.05000000000000071, 76.00000000001195133, -103.0231074845243171 ) ) ;
#39070 = CIRCLE ( 'NONE', #22501, 0.09999999999999939493 ) ;
#39071 = DIRECTION ( 'NONE',  ( 1.000000000000000000, 0.000000000000000000, 0.000000000000000000 ) ) ;
#39073 = ORIENTED_EDGE ( 'NONE', *, *, #78103, .T. ) ;
#39072 = LINE ( 'NONE', #98987, #165430 ) ;
#39074 = VECTOR ( 'NONE', #33218, 1000.000000000000000 ) ;
#39075 = CIRCLE ( 'NONE', #51482, 11.64999999999999325 ) ;
#39076 = EDGE_LOOP ( 'NONE', ( #124924, #239437, #142218, #21110 ) ) ;
#39077 = AXIS2_PLACEMENT_3D ( 'NONE', #168732, #10902, #248223 ) ;
#39078 = CARTESIAN_POINT ( 'NONE',  ( 20.95203847575071521, 10.50106053928516303, -41.06707134862356412 ) ) ;
#39079 = ORIENTED_EDGE ( 'NONE', *, *, #33590, .F. ) ;
#39080 = APPLICATION_CONTEXT ( 'automotive_design' ) ;
#39081 = DIRECTION ( 'NONE',  ( -1.000000000000000000, 0.000000000000000000, 0.000000000000000000 ) ) ;
#39082 = CARTESIAN_POINT ( 'NONE',  ( -22.32929514600008503, 0.09907567812507747651, -92.92135243462352889 ) ) ;
#39083 = DIRECTION ( 'NONE',  ( 1.000000000000000000, -0.000000000000000000, -0.000000000000000000 ) ) ;
#39084 = ORIENTED_EDGE ( 'NONE', *, *, #129279, .F. ) ;
#39085 = ADVANCED_FACE ( 'NONE', ( #58940 ), #153858, .T. ) ;
#39086 = DIRECTION ( 'NONE',  ( 0.7071067811865388020, -0.7071067811865561215, 0.000000000000000000 ) ) ;
#39087 = CARTESIAN_POINT ( 'NONE',  ( 21.05000000000000071, 0.000000000000000000, -33.50000000000000000 ) ) ;
#39088 = DIRECTION ( 'NONE',  ( 0.000000000000000000, -0.8814952561688430555, 0.4721928772777346239 ) ) ;
#39089 = CIRCLE ( 'NONE', #51495, 0.1000000000000096922 ) ;
#39090 = TOROIDAL_SURFACE ( 'NONE', #51496, 3.900000000000000355, 0.1000000000000000056 ) ;
#39091 = AXIS2_PLACEMENT_3D ( 'NONE', #240618, #219758, #241893 ) ;
#39093 = LINE ( 'NONE', #1199, #172546 ) ;
#39092 = CIRCLE ( 'NONE', #184805, 12.87499999999999822 ) ;
#39094 = CARTESIAN_POINT ( 'NONE',  ( -20.54999999999999716, 78.08573236070779444, -228.9307947190811774 ) ) ;
#39095 = SPHERICAL_SURFACE ( 'NONE', #98727, 0.1000000000000000056 ) ;
#39096 = VERTEX_POINT ( 'NONE', #18570 ) ;
#39097 = FACE_OUTER_BOUND ( 'NONE', #142826, .T. ) ;
#39099 = ORIENTED_EDGE ( 'NONE', *, *, #3245, .F. ) ;
#39098 = DIRECTION ( 'NONE',  ( -1.000000000000000000, -0.000000000000000000, -0.000000000000000000 ) ) ;
#39100 = DIRECTION ( 'NONE',  ( -1.000000000000000000, -0.000000000000000000, -0.000000000000000000 ) ) ;
#39101 = EDGE_CURVE ( 'NONE', #33613, #252227, #77238, .T. ) ;
#39102 = DIRECTION ( 'NONE',  ( 0.000000000000000000, 6.982962677686266711E-15, -1.000000000000000000 ) ) ;
#39103 = DIRECTION ( 'NONE',  ( 0.000000000000000000, 0.000000000000000000, -1.000000000000000000 ) ) ;
#39104 = ORIENTED_EDGE ( 'NONE', *, *, #13164, .F. ) ;
#39105 = CARTESIAN_POINT ( 'NONE',  ( -22.42253884134832020, 75.99806764887692623, -148.1727131818727230 ) ) ;
#39106 = EDGE_CURVE ( 'NONE', #222832, #75372, #93130, .T. ) ;
#39107 = PRODUCT_CONTEXT ( 'NONE', #140721, 'mechanical' ) ;
#39108 = CARTESIAN_POINT ( 'NONE',  ( -18.59999996769639097, 85.36327376984216642, -95.84161356905833884 ) ) ;
#39109 = ORIENTED_EDGE ( 'NONE', *, *, #202421, .T. ) ;
#39111 = EDGE_CURVE ( 'NONE', #136961, #13313, #209426, .T. ) ;
#39110 = DIRECTION ( 'NONE',  ( 0.000000000000000000, 0.000000000000000000, 1.000000000000000000 ) ) ;
#39112 = CARTESIAN_POINT ( 'NONE',  ( 15.66039659514495419, 9.360749169926259938, -184.8145701406072021 ) ) ;
#39113 = EDGE_CURVE ( 'NONE', #104459, #210671, #141087, .T. ) ;
#39114 = MECHANICAL_DESIGN_GEOMETRIC_PRESENTATION_REPRESENTATION (  '', ( #197476 ), #26641 ) ;
#39115 = EDGE_CURVE ( 'NONE', #94226, #84007, #234797, .T. ) ;
#39116 = PRESENTATION_STYLE_ASSIGNMENT (( #76925 ) ) ;
#39117 = VERTEX_POINT ( 'NONE', #57671 ) ;
#39118 = ORIENTED_EDGE ( 'NONE', *, *, #56475, .T. ) ;
#39119 = DIRECTION ( 'NONE',  ( 1.000000000000000000, 2.952720810173289112E-16, -0.000000000000000000 ) ) ;
#39120 = DIRECTION ( 'NONE',  ( -1.000000000000000000, 2.952720810173289112E-16, 2.061873921506763405E-30 ) ) ;
#39121 = DIRECTION ( 'NONE',  ( 1.000000000000000000, 0.000000000000000000, 0.000000000000000000 ) ) ;
#39122 = FACE_OUTER_BOUND ( 'NONE', #44431, .T. ) ;
#39123 = CARTESIAN_POINT ( 'NONE',  ( 23.14999999999998437, 1.148907358139439339E-11, -201.0000000000015064 ) ) ;
#39125 = DIRECTION ( 'NONE',  ( 1.000000000000000000, 2.986185139342070877E-16, -6.665775143889692774E-16 ) ) ;
#39124 = FACE_OUTER_BOUND ( 'NONE', #69189, .T. ) ;
#39126 = CARTESIAN_POINT ( 'NONE',  ( 20.94788355080264353, 65.69792220476271893, -30.53355541284615526 ) ) ;
#39127 = DIRECTION ( 'NONE',  ( 1.000000000000000000, -0.000000000000000000, -0.000000000000000000 ) ) ;
#39128 = DIRECTION ( 'NONE',  ( 0.000000000000000000, 0.9126074666063769270, 0.4088369013363280513 ) ) ;
#39130 = CARTESIAN_POINT ( 'NONE',  ( -16.87036670365549895, 9.989418819312803066, -146.5204398826979855 ) ) ;
#39129 = AXIS2_PLACEMENT_3D ( 'NONE', #24825, #161761, #45646 ) ;
#39131 = EDGE_LOOP ( 'NONE', ( #99596, #85693, #2171, #91464 ) ) ;
#39132 = ADVANCED_FACE ( 'NONE', ( #216756 ), #38146, .T. ) ;
#39133 = CIRCLE ( 'NONE', #130677, 0.1000000000000000472 ) ;
#39134 = ORIENTED_EDGE ( 'NONE', *, *, #6994, .F. ) ;
#39135 = ADVANCED_FACE ( 'NONE', ( #274 ), #249004, .T. ) ;
#39136 = DIRECTION ( 'NONE',  ( 0.000000000000000000, 0.000000000000000000, 1.000000000000000000 ) ) ;
#39139 = DIRECTION ( 'NONE',  ( -0.000000000000000000, -0.000000000000000000, 1.000000000000000000 ) ) ;
#39138 = CARTESIAN_POINT ( 'NONE',  ( 20.94999999999999929, 1.115600667400684642E-11, -67.00000000000000000 ) ) ;
#39137 = CIRCLE ( 'NONE', #159933, 0.1000000000000028644 ) ;
#39140 = DIRECTION ( 'NONE',  ( 0.7071067811865475727, -0.2890913453342130457, 0.6453109281988448354 ) ) ;
#39142 = EDGE_CURVE ( 'NONE', #7658, #153790, #244018, .T. ) ;
#39141 = DIRECTION ( 'NONE',  ( -0.7071067811865389130, 0.000000000000000000, 0.7071067811865561215 ) ) ;
#39143 = DIRECTION ( 'NONE',  ( 0.000000000000000000, 0.000000000000000000, 1.000000000000000000 ) ) ;
#39144 = ORIENTED_EDGE ( 'NONE', *, *, #81410, .F. ) ;
#39145 = ORIENTED_EDGE ( 'NONE', *, *, #211512, .T. ) ;
#39146 = EDGE_CURVE ( 'NONE', #90111, #21530, #201456, .T. ) ;
#39148 = AXIS2_PLACEMENT_3D ( 'NONE', #31818, #12244, #229982 ) ;
#39147 = DIRECTION ( 'NONE',  ( -2.952720810173288619E-16, 1.000000000000000000, 0.000000000000000000 ) ) ;
#39149 = VERTEX_POINT ( 'NONE', #65391 ) ;
#39150 = DIRECTION ( 'NONE',  ( -2.978066053179067751E-16, 1.000000000000000000, 0.000000000000000000 ) ) ;
#39151 = EDGE_CURVE ( 'NONE', #157067, #147354, #48386, .T. ) ;
#39152 = AXIS2_PLACEMENT_3D ( 'NONE', #233126, #174460, #115719 ) ;
#39154 = CARTESIAN_POINT ( 'NONE',  ( -18.50000000000000000, 66.85000000001150511, -48.37310748452438247 ) ) ;
#39153 = VECTOR ( 'NONE', #180943, 1000.000000000000000 ) ;
#39155 = AXIS2_PLACEMENT_3D ( 'NONE', #168205, #246417, #109450 ) ;
#39156 = EDGE_CURVE ( 'NONE', #83655, #57200, #113975, .T. ) ;
#39157 = ORIENTED_EDGE ( 'NONE', *, *, #211864, .T. ) ;
#39158 = CARTESIAN_POINT ( 'NONE',  ( -20.64999999999999858, 11.46684968301824448, -245.9610388612851750 ) ) ;
#39159 = VERTEX_POINT ( 'NONE', #28887 ) ;
#39160 = DIRECTION ( 'NONE',  ( 0.000000000000000000, -0.8660254037844343777, 0.5000000000000074385 ) ) ;
#39161 = EDGE_CURVE ( 'NONE', #193316, #32161, #45828, .T. ) ;
#39162 = DIRECTION ( 'NONE',  ( 0.000000000000000000, 0.6046243595031880469, 0.7965107556683460599 ) ) ;
#39163 = LINE ( 'NONE', #241207, #90909 ) ;
#39164 = CIRCLE ( 'NONE', #68369, 0.09999999999999939493 ) ;
#39166 = CARTESIAN_POINT ( 'NONE',  ( -18.59999999999999787, 66.65000000001253966, -182.1731074845244223 ) ) ;
#39165 = CIRCLE ( 'NONE', #9910, 11.80000000000000426 ) ;
#39167 = CARTESIAN_POINT ( 'NONE',  ( -16.86132326855786090, 9.949999999999983302, -12.69863578466831910 ) ) ;
#39170 = DIRECTION ( 'NONE',  ( 0.000000000000000000, 1.000000000000000000, 0.000000000000000000 ) ) ;
#39169 = AXIS2_PLACEMENT_3D ( 'NONE', #79542, #23479, #139526 ) ;
#39168 = DIRECTION ( 'NONE',  ( -1.000000000000000000, 0.000000000000000000, -0.000000000000000000 ) ) ;
#39171 = LINE ( 'NONE', #76980, #257180 ) ;
#39172 = ORIENTED_EDGE ( 'NONE', *, *, #78192, .F. ) ;
#39174 = CARTESIAN_POINT ( 'NONE',  ( -16.85939681242906119, 66.09477481408670485, -115.9831855293328857 ) ) ;
#39173 = CARTESIAN_POINT ( 'NONE',  ( 20.85000000000000142, 64.35000000001214460, -136.5231074845244166 ) ) ;
#39175 = CIRCLE ( 'NONE', #235153, 0.09999999999999939493 ) ;
#39176 = VERTEX_POINT ( 'NONE', #185342 ) ;
#39178 = ORIENTED_EDGE ( 'NONE', *, *, #26945, .F. ) ;
#39177 = SPHERICAL_SURFACE ( 'NONE', #210730, 0.1000000000000000056 ) ;
#39179 = ORIENTED_EDGE ( 'NONE', *, *, #215818, .T. ) ;
#39180 = CARTESIAN_POINT ( 'NONE',  ( -20.54999999999999716, 26.18196512540240661, -241.1028522842020152 ) ) ;
#39181 = CARTESIAN_POINT ( 'NONE',  ( -21.07094088545368749, 0.09889370256337755294, -27.17983277808286857 ) ) ;
#39182 = DIRECTION ( 'NONE',  ( 1.000000000000000000, -0.000000000000000000, -0.000000000000000000 ) ) ;
#39183 = CIRCLE ( 'NONE', #93305, 4.049999999999998046 ) ;
#39184 = CARTESIAN_POINT ( 'NONE',  ( -16.94445028196808778, 9.992063609697733995, -12.60733017841845438 ) ) ;
#39185 = ORIENTED_EDGE ( 'NONE', *, *, #186209, .T. ) ;
#39186 = CARTESIAN_POINT ( 'NONE',  ( 21.72449340488910607, 51.48232928251994167, -231.6416980232910987 ) ) ;
#39187 = CARTESIAN_POINT ( 'NONE',  ( -18.69999999999999929, -8.250000000000005329, 32.89999999999999858 ) ) ;
#39188 = AXIS2_PLACEMENT_3D ( 'NONE', #221671, #23534, #139567 ) ;
#39190 = VERTEX_POINT ( 'NONE', #86210 ) ;
#39189 = B_SPLINE_CURVE_WITH_KNOTS ( 'NONE', 3,
 ( #44302, #202085, #222912, #245056, #224197, #228067, #23477, #182537 ),
 .UNSPECIFIED., .F., .F.,
 ( 4, 2, 2, 4 ),
 ( 0.000000000000000000, 0.0002114466876442284862, 0.0003171700314663216010, 0.0004228933752884147970 ),
 .UNSPECIFIED. ) ;
#39191 = AXIS2_PLACEMENT_3D ( 'NONE', #189265, #148859, #34072 ) ;
#39192 = B_SPLINE_CURVE_WITH_KNOTS ( 'NONE', 3,
 ( #196223, #56682, #237920, #236628, #18870, #136224, #215774 ),
 .UNSPECIFIED., .F., .F.,
 ( 4, 3, 4 ),
 ( 0.000000000000000000, 3.357501770816500864E-05, 5.199112466352410285E-05 ),
 .UNSPECIFIED. ) ;
#39193 = CARTESIAN_POINT ( 'NONE',  ( -18.59117750673697245, 46.46967969402478360, -243.0849751855955674 ) ) ;
#39194 = VECTOR ( 'NONE', #106428, 999.9999999999998863 ) ;
#39195 = CARTESIAN_POINT ( 'NONE',  ( 21.08376601933332495, 6.341947271275658160, 0.06377601093000156984 ) ) ;
#39196 = VERTEX_POINT ( 'NONE', #126651 ) ;
#39197 = EDGE_LOOP ( 'NONE', ( #151826, #230246, #159815, #242471 ) ) ;
#39198 = DIRECTION ( 'NONE',  ( -1.000000000000000000, 0.000000000000000000, 0.000000000000000000 ) ) ;
#39199 = ORIENTED_EDGE ( 'NONE', *, *, #63270, .F. ) ;
#39200 = CARTESIAN_POINT ( 'NONE',  ( 18.39999999999999858, 8.841736820195473356, -245.4273993276876240 ) ) ;
#39201 = ORIENTED_EDGE ( 'NONE', *, *, #212387, .F. ) ;
#39202 = DIRECTION ( 'NONE',  ( -1.000000000000000000, 0.000000000000000000, 0.000000000000000000 ) ) ;
#39203 = ADVANCED_FACE ( 'NONE', ( #165805 ), #206189, .T. ) ;
#39204 = DIRECTION ( 'NONE',  ( -1.000000000000000000, 0.000000000000000000, 0.000000000000000000 ) ) ;
#39205 = CARTESIAN_POINT ( 'NONE',  ( -23.15000000000000213, -8.999999999988846255, -177.3939691226524076 ) ) ;
#39206 = FACE_OUTER_BOUND ( 'NONE', #188703, .T. ) ;
#39207 = VECTOR ( 'NONE', #176314, 1000.000000000000000 ) ;
#39208 = CIRCLE ( 'NONE', #18332, 0.1999999999999987899 ) ;
#39209 = LINE ( 'NONE', #101687, #146081 ) ;
#39210 = DIRECTION ( 'NONE',  ( -1.000000000000000000, -0.000000000000000000, -0.000000000000000000 ) ) ;
#39212 = EDGE_CURVE ( 'NONE', #235384, #113827, #247879, .T. ) ;
#39211 = FACE_OUTER_BOUND ( 'NONE', #241639, .T. ) ;
#39213 = AXIS2_PLACEMENT_3D ( 'NONE', #189894, #88191, #107783 ) ;
#39214 = ORIENTED_EDGE ( 'NONE', *, *, #11750, .T. ) ;
#39216 = CARTESIAN_POINT ( 'NONE',  ( -21.51976009735018991, 6.910458441670358276, -33.50000000000000000 ) ) ;
#39215 = CARTESIAN_POINT ( 'NONE',  ( -21.07928932188134041, 75.90110485435802445, -176.3516241409176644 ) ) ;
#39217 = ORIENTED_EDGE ( 'NONE', *, *, #118881, .T. ) ;
#39220 = ORIENTED_EDGE ( 'NONE', *, *, #88663, .T. ) ;
#39219 = CARTESIAN_POINT ( 'NONE',  ( 21.05000000000000071, -6.688413578037176066, -212.5825622730469036 ) ) ;
#39218 = DIRECTION ( 'NONE',  ( 0.000000000000000000, 0.000000000000000000, 1.000000000000000000 ) ) ;
#39221 = ORIENTED_EDGE ( 'NONE', *, *, #206222, .T. ) ;
#39222 = DIRECTION ( 'NONE',  ( 0.000000000000000000, 0.000000000000000000, -1.000000000000000000 ) ) ;
#39223 = FACE_OUTER_BOUND ( 'NONE', #248037, .T. ) ;
#39224 = AXIS2_PLACEMENT_3D ( 'NONE', #185116, #3913, #142132 ) ;
#39225 = CYLINDRICAL_SURFACE ( 'NONE', #102671, 0.09999999999999939493 ) ;
#39226 = CARTESIAN_POINT ( 'NONE',  ( -16.83199030136658081, 9.930648033124622742, -113.2724010226575047 ) ) ;
#39227 = AXIS2_PLACEMENT_3D ( 'NONE', #47968, #104073, #6266 ) ;
#39228 = ORIENTED_EDGE ( 'NONE', *, *, #70550, .F. ) ;
#39229 = DIRECTION ( 'NONE',  ( 1.000000000000000000, 0.000000000000000000, 0.000000000000000000 ) ) ;
#39230 = FACE_OUTER_BOUND ( 'NONE', #124352, .T. ) ;
#39231 = CIRCLE ( 'NONE', #247280, 4.049999999999990941 ) ;
#39233 = CARTESIAN_POINT ( 'NONE',  ( 20.95575313997065336, 10.61455330327483537, -7.621290701944819723 ) ) ;
#39232 = FACE_OUTER_BOUND ( 'NONE', #2413, .T. ) ;
#39235 = ORIENTED_EDGE ( 'NONE', *, *, #210773, .F. ) ;
#39234 = CARTESIAN_POINT ( 'NONE',  ( -16.94052228080551359, 9.986279733109993728, -54.39037550266942844 ) ) ;
#39236 = VECTOR ( 'NONE', #53083, 1000.000000000000000 ) ;
#39237 = AXIS2_PLACEMENT_3D ( 'NONE', #42957, #181200, #2523 ) ;
#39238 = AXIS2_PLACEMENT_3D ( 'NONE', #148355, #89647, #248745 ) ;
#39239 = PRODUCT_DEFINITION_SHAPE ( 'NONE', 'NONE',  #258121 ) ;
#39240 = ORIENTED_EDGE ( 'NONE', *, *, #113681, .F. ) ;
#39241 = VECTOR ( 'NONE', #47872, 1000.000000000000000 ) ;
#39242 = DIRECTION ( 'NONE',  ( -0.000000000000000000, 6.982962677686266711E-15, -1.000000000000000000 ) ) ;
#39243 = EDGE_LOOP ( 'NONE', ( #119869, #40535, #68603, #90090 ) ) ;
#39244 = CYLINDRICAL_SURFACE ( 'NONE', #201996, 0.09999999999999520384 ) ;
#39245 = ORIENTED_EDGE ( 'NONE', *, *, #49482, .T. ) ;
#39246 = CYLINDRICAL_SURFACE ( 'NONE', #126634, 0.09999999999999939493 ) ;
#39247 = CARTESIAN_POINT ( 'NONE',  ( 22.50000000000000000, 75.95437663941565631, -114.6736118230756887 ) ) ;
#39248 = DIRECTION ( 'NONE',  ( 0.000000000000000000, 0.000000000000000000, 1.000000000000000000 ) ) ;
#39249 = TOROIDAL_SURFACE ( 'NONE', #60056, 0.6000000000000009770, 0.1000000000000000056 ) ;
#39250 = ORIENTED_EDGE ( 'NONE', *, *, #216352, .T. ) ;
#39251 = CYLINDRICAL_SURFACE ( 'NONE', #112647, 0.5000000000000004441 ) ;
#39252 = ADVANCED_FACE ( 'NONE', ( #224458 ), #44557, .F. ) ;
#39253 = AXIS2_PLACEMENT_3D ( 'NONE', #39942, #118169, #75215 ) ;
#39254 = ADVANCED_FACE ( 'NONE', ( #66684 ), #215484, .T. ) ;
#39255 = CARTESIAN_POINT ( 'NONE',  ( -20.00857864376270001, 66.85000000001259934, -191.1731074845244223 ) ) ;
#39256 = VECTOR ( 'NONE', #137397, 1000.000000000000000 ) ;
#39257 = CIRCLE ( 'NONE', #126717, 0.5000000000000004441 ) ;
#39258 = VERTEX_POINT ( 'NONE', #31440 ) ;
#39259 = AXIS2_PLACEMENT_3D ( 'NONE', #201379, #106108, #7033 ) ;
#39260 = ORIENTED_EDGE ( 'NONE', *, *, #117340, .T. ) ;
#39261 = VERTEX_POINT ( 'NONE', #233479 ) ;
#39262 = ADVANCED_FACE ( 'NONE', ( #112242 ), #97179, .F. ) ;
#39263 = DIRECTION ( 'NONE',  ( -1.000000000000000000, 0.000000000000000000, 0.000000000000000000 ) ) ;
#39264 = ORIENTED_EDGE ( 'NONE', *, *, #244529, .F. ) ;
#39266 = ORIENTED_EDGE ( 'NONE', *, *, #128534, .T. ) ;
#39265 = DIRECTION ( 'NONE',  ( -0.000000000000000000, -0.000000000000000000, -1.000000000000000000 ) ) ;
#39267 = EDGE_CURVE ( 'NONE', #256994, #233248, #184705, .T. ) ;
#39268 = ORIENTED_EDGE ( 'NONE', *, *, #92631, .T. ) ;
#39271 = ORIENTED_EDGE ( 'NONE', *, *, #31759, .T. ) ;
#39270 = ORIENTED_EDGE ( 'NONE', *, *, #165971, .T. ) ;
#39269 = DIRECTION ( 'NONE',  ( 0.000000000000000000, 0.000000000000000000, -1.000000000000000000 ) ) ;
#39273 = EDGE_CURVE ( 'NONE', #143932, #64265, #84725, .T. ) ;
#39272 = ORIENTED_EDGE ( 'NONE', *, *, #179107, .T. ) ;
#39274 = AXIS2_PLACEMENT_3D ( 'NONE', #228435, #125474, #26376 ) ;
#39275 = DIRECTION ( 'NONE',  ( 1.000000000000000000, 0.000000000000000000, 0.000000000000000000 ) ) ;
#39276 = AXIS2_PLACEMENT_3D ( 'NONE', #86921, #127363, #166518 ) ;
#39277 = VECTOR ( 'NONE', #453, 1000.000000000000000 ) ;
#39278 = CARTESIAN_POINT ( 'NONE',  ( 20.09999999999999787, 66.25000000001259082, -190.8731074845244393 ) ) ;
#39279 = CARTESIAN_POINT ( 'NONE',  ( -27.30103769104855971, 12.19999999999999574, -347.0000000000001137 ) ) ;
#39280 = EDGE_LOOP ( 'NONE', ( #76657, #214846, #219029, #76127 ) ) ;
#39281 = DIRECTION ( 'NONE',  ( -4.336808689941752679E-15, 0.8660254037844482555, 0.4999999999999837907 ) ) ;
#39283 = VERTEX_POINT ( 'NONE', #113508 ) ;
#39282 = CARTESIAN_POINT ( 'NONE',  ( -23.39999999999994529, 74.16448838626247664, -47.52760213295649550 ) ) ;
#39284 = DIRECTION ( 'NONE',  ( 0.000000000000000000, -1.000000000000000000, 0.000000000000000000 ) ) ;
#39286 = EDGE_LOOP ( 'NONE', ( #93215, #254461, #72465 ) ) ;
#39285 = CARTESIAN_POINT ( 'NONE',  ( 22.84999999999999787, 0.000000000000000000, 0.000000000000000000 ) ) ;
#39287 = EDGE_CURVE ( 'NONE', #140297, #179663, #213890, .T. ) ;
#39288 = EDGE_LOOP ( 'NONE', ( #195741, #80677, #65666 ) ) ;
#39289 = CARTESIAN_POINT ( 'NONE',  ( 20.94999999999999574, 74.14897176987071248, -57.86919421510183525 ) ) ;
#39290 = CARTESIAN_POINT ( 'NONE',  ( -11.59999999999994458, 67.72071067812984779, -24.99381816264344991 ) ) ;
#39291 = ORIENTED_EDGE ( 'NONE', *, *, #168603, .T. ) ;
#39292 = ORIENTED_EDGE ( 'NONE', *, *, #6804, .T. ) ;
#39293 = DIRECTION ( 'NONE',  ( 1.000000000000000000, 0.000000000000000000, 0.000000000000000000 ) ) ;
#39294 = CARTESIAN_POINT ( 'NONE',  ( -21.07954763557309619, 0.06587591862965960776, -161.1707090099635593 ) ) ;
#39296 = VERTEX_POINT ( 'NONE', #215174 ) ;
#39295 = ORIENTED_EDGE ( 'NONE', *, *, #93888, .F. ) ;
#39297 = VECTOR ( 'NONE', #232600, 999.9999999999998863 ) ;
#39298 = ORIENTED_EDGE ( 'NONE', *, *, #7954, .F. ) ;
#39299 = DIRECTION ( 'NONE',  ( -0.000000000000000000, 1.000000000000000000, 6.982962677686266711E-15 ) ) ;
#39300 = ORIENTED_EDGE ( 'NONE', *, *, #236138, .F. ) ;
#39301 = ORIENTED_EDGE ( 'NONE', *, *, #164436, .F. ) ;
#39302 = CARTESIAN_POINT ( 'NONE',  ( 20.95392731769792150, 18.83565523496773864, -229.9264601087687652 ) ) ;
#39303 = ORIENTED_EDGE ( 'NONE', *, *, #218646, .F. ) ;
#39305 = DIRECTION ( 'NONE',  ( -0.000000000000000000, -0.1350103645451876666, 0.9908441862701600211 ) ) ;
#39304 = CARTESIAN_POINT ( 'NONE',  ( -23.15000000000000213, 81.86853375790846599, -214.9828603846715964 ) ) ;
#39306 = EDGE_CURVE ( 'NONE', #53190, #255801, #93939, .T. ) ;
#39307 = ORIENTED_EDGE ( 'NONE', *, *, #81527, .T. ) ;
#39309 = ORIENTED_EDGE ( 'NONE', *, *, #25797, .T. ) ;
#39308 = ORIENTED_EDGE ( 'NONE', *, *, #136590, .T. ) ;
#39310 = CARTESIAN_POINT ( 'NONE',  ( -18.40000000000000213, 16.35463830854640932, -222.1788605317357224 ) ) ;
#39311 = DIRECTION ( 'NONE',  ( -0.000000000000000000, 1.000000000000000000, 6.982962677686266711E-15 ) ) ;
#39312 = AXIS2_PLACEMENT_3D ( 'NONE', #134144, #194155, #257898 ) ;
#39313 = EDGE_LOOP ( 'NONE', ( #103973, #66145, #228859, #72116 ) ) ;
#39314 = AXIS2_PLACEMENT_3D ( 'NONE', #187328, #246006, #248561 ) ;
#39315 = AXIS2_PLACEMENT_3D ( 'NONE', #124991, #67572, #8888 ) ;
#39316 = CIRCLE ( 'NONE', #201599, 0.09999999999998807065 ) ;
#39317 = ADVANCED_FACE ( 'NONE', ( #189202 ), #130551, .T. ) ;
#39318 = CARTESIAN_POINT ( 'NONE',  ( -23.25000000000000000, 87.75000000001213607, -136.5231074845242176 ) ) ;
#39319 = ORIENTED_EDGE ( 'NONE', *, *, #201924, .T. ) ;
#39320 = VERTEX_POINT ( 'NONE', #232194 ) ;
#39321 = CARTESIAN_POINT ( 'NONE',  ( 21.30000000000002558, 68.29137419664525055, -231.9463301769586394 ) ) ;
#39322 = ORIENTED_EDGE ( 'NONE', *, *, #91206, .T. ) ;
#39323 = FACE_OUTER_BOUND ( 'NONE', #194730, .T. ) ;
#39324 = FACE_OUTER_BOUND ( 'NONE', #174555, .T. ) ;
#39325 = ORIENTED_EDGE ( 'NONE', *, *, #89388, .F. ) ;
#39326 = DIRECTION ( 'NONE',  ( 0.000000000000000000, 0.9126074666063773710, 0.4088369013363274407 ) ) ;
#39328 = EDGE_CURVE ( 'NONE', #144652, #112987, #162202, .T. ) ;
#39327 = CARTESIAN_POINT ( 'NONE',  ( -23.25000000000000000, 76.00000000001190870, -103.0231074845243029 ) ) ;
#39329 = CARTESIAN_POINT ( 'NONE',  ( -16.87998658237740912, 9.950000000011137047, -121.1363604322620375 ) ) ;
#39330 = DIRECTION ( 'NONE',  ( 0.000000000000000000, -1.000000000000000000, 0.000000000000000000 ) ) ;
#39331 = CARTESIAN_POINT ( 'NONE',  ( -21.64999999999999858, 12.53302308287915245, -211.3193184079345883 ) ) ;
#39332 = CARTESIAN_POINT ( 'NONE',  ( 6.000000000000060396, 64.35000000001120668, -26.02310748452479316 ) ) ;
#39333 = DIRECTION ( 'NONE',  ( 1.000000000000000000, 0.000000000000000000, 0.000000000000000000 ) ) ;
#39334 = CIRCLE ( 'NONE', #176696, 0.09999999999999939493 ) ;
#39335 = DIRECTION ( 'NONE',  ( 0.000000000000000000, 0.8814952561688388366, -0.4721928772777424510 ) ) ;
#39336 = DIRECTION ( 'NONE',  ( 0.000000000000000000, 1.000000000000000000, 6.982962677686266711E-15 ) ) ;
#39337 = EDGE_CURVE ( 'NONE', #178251, #112934, #194359, .T. ) ;
#39338 = VECTOR ( 'NONE', #234611, 999.9999999999998863 ) ;
#39339 = VERTEX_POINT ( 'NONE', #210057 ) ;
#39340 = AXIS2_PLACEMENT_3D ( 'NONE', #229062, #129929, #209484 ) ;
#39341 = AXIS2_PLACEMENT_3D ( 'NONE', #239689, #2335, #161450 ) ;
#39343 = VERTEX_POINT ( 'NONE', #174816 ) ;
#39342 = EDGE_LOOP ( 'NONE', ( #252368, #91867, #54968 ) ) ;
#39344 = ORIENTED_EDGE ( 'NONE', *, *, #185519, .T. ) ;
#39346 = ORIENTED_EDGE ( 'NONE', *, *, #42449, .F. ) ;
#39345 = AXIS2_PLACEMENT_3D ( 'NONE', #26288, #105782, #65400 ) ;
#39347 = FACE_OUTER_BOUND ( 'NONE', #57894, .T. ) ;
#39348 = ADVANCED_FACE ( 'NONE', ( #249180 ), #159784, .T. ) ;
#39349 = CARTESIAN_POINT ( 'NONE',  ( -18.59999999999999787, 77.16270174994990327, -94.92310748452430857 ) ) ;
#39351 = DIRECTION ( 'NONE',  ( 0.7071359030028089299, 0.6232856014206507034, -0.3338770338704052376 ) ) ;
#39350 = DIRECTION ( 'NONE',  ( 0.000000000000000000, -6.982962677686266711E-15, 1.000000000000000000 ) ) ;
#39352 = EDGE_LOOP ( 'NONE', ( #15904, #252138, #167191 ) ) ;
#39353 = AXIS2_PLACEMENT_3D ( 'NONE', #175066, #149051, #169927 ) ;
#39354 = EDGE_CURVE ( 'NONE', #182621, #70011, #138880, .T. ) ;
#39355 = CARTESIAN_POINT ( 'NONE',  ( -20.94999027547553894, 10.29326151435327219, -105.9592822510415431 ) ) ;
#39356 = CIRCLE ( 'NONE', #101641, 7.900000000000010125 ) ;
#39357 = EDGE_CURVE ( 'NONE', #234608, #165014, #197178, .T. ) ;
#39359 = AXIS2_PLACEMENT_3D ( 'NONE', #178044, #636, #116761 ) ;
#39358 = DIRECTION ( 'NONE',  ( 0.000000000000000000, -6.853228547068871147E-15, 1.000000000000000000 ) ) ;
#39360 = DIRECTION ( 'NONE',  ( 1.000000000000000000, 0.000000000000000000, 0.000000000000000000 ) ) ;
#39361 = DIRECTION ( 'NONE',  ( 0.000000000000000000, 0.000000000000000000, 1.000000000000000000 ) ) ;
#39363 = VERTEX_POINT ( 'NONE', #150091 ) ;
#39362 = TOROIDAL_SURFACE ( 'NONE', #5994, 0.2000000000000000111, 0.1000000000000000056 ) ;
#39364 = B_SPLINE_CURVE_WITH_KNOTS ( 'NONE', 3,
 ( #247107, #128462, #245842, #68493, #243253, #148028, #69790, #228851, #48913, #26822 ),
 .UNSPECIFIED., .F., .F.,
 ( 4, 3, 3, 4 ),
 ( 0.000000000000000000, 4.874959354401679605E-05, 9.785140065120807406E-05, 0.0001360444631935947134 ),
 .UNSPECIFIED. ) ;
#39365 = LINE ( 'NONE', #121471, #30647 ) ;
#39366 = EDGE_CURVE ( 'NONE', #31307, #58852, #151426, .T. ) ;
#39367 = CIRCLE ( 'NONE', #218371, 0.5000000000000004441 ) ;
#39368 = CARTESIAN_POINT ( 'NONE',  ( 0.9000000000000547562, 64.35000000001120668, -12.62310748452478926 ) ) ;
#39369 = ORIENTED_EDGE ( 'NONE', *, *, #1753, .T. ) ;
#39370 = DIRECTION ( 'NONE',  ( -2.827886303505249259E-16, -0.8103668758649578141, 0.5859227990963213895 ) ) ;
#39371 = CARTESIAN_POINT ( 'NONE',  ( -23.15000000000000213, 4.250000000011156409, -121.7500000000000426 ) ) ;
#39372 = EDGE_CURVE ( 'NONE', #187441, #248700, #5617, .T. ) ;
#39373 = FACE_OUTER_BOUND ( 'NONE', #79920, .T. ) ;
#39374 = DIRECTION ( 'NONE',  ( 0.000000000000000000, 1.000000000000000000, 1.626303258728238113E-15 ) ) ;
#39375 = EDGE_CURVE ( 'NONE', #23846, #132498, #213949, .T. ) ;
#39376 = VECTOR ( 'NONE', #140546, 1000.000000000000000 ) ;
#39377 = PLANE ( 'NONE',  #212502 ) ;
#39379 = ORIENTED_EDGE ( 'NONE', *, *, #130214, .F. ) ;
#39378 = AXIS2_PLACEMENT_3D ( 'NONE', #125135, #185095, #182546 ) ;
#39380 = CARTESIAN_POINT ( 'NONE',  ( 18.47654891039377389, 47.03189691987548571, -255.2758813845442774 ) ) ;
#39381 = CARTESIAN_POINT ( 'NONE',  ( -18.69999999999999929, 7.799999999999999822, -1.212568896937008089 ) ) ;
#39382 = DIRECTION ( 'NONE',  ( 0.000000000000000000, -0.8814952561688430555, 0.4721928772777346239 ) ) ;
#39383 = AXIS2_PLACEMENT_3D ( 'NONE', #89448, #69924, #110304 ) ;
#39385 = DIRECTION ( 'NONE',  ( 1.000000000000000000, 0.000000000000000000, 0.000000000000000000 ) ) ;
#39384 = CARTESIAN_POINT ( 'NONE',  ( -23.25000000000000000, 1.115600667400684642E-11, -100.5000000000000284 ) ) ;
#39386 = DIRECTION ( 'NONE',  ( -1.000000000000000000, -0.000000000000000000, 0.000000000000000000 ) ) ;
#39387 = DIRECTION ( 'NONE',  ( -0.5932847527679296906, 0.3801118060259206510, 0.7095972217059544063 ) ) ;
#39388 = DIRECTION ( 'NONE',  ( -1.000000000000000000, -0.000000000000000000, -0.000000000000000000 ) ) ;
#39389 = FACE_OUTER_BOUND ( 'NONE', #31400, .T. ) ;
#39390 = ORIENTED_EDGE ( 'NONE', *, *, #244456, .F. ) ;
#39391 = ORIENTED_EDGE ( 'NONE', *, *, #244189, .F. ) ;
#39392 = DIRECTION ( 'NONE',  ( 0.000000000000000000, -6.982962677686266711E-15, 1.000000000000000000 ) ) ;
#39393 = ADVANCED_FACE ( 'NONE', ( #52228 ), #68197, .T. ) ;
#39394 = EDGE_LOOP ( 'NONE', ( #98893, #19277, #71084, #146332 ) ) ;
#39395 = ADVANCED_FACE ( 'NONE', ( #131782 ), #20854, .F. ) ;
#39396 = DIRECTION ( 'NONE',  ( 0.000000000000000000, 0.9126074666063545004, 0.4088369013363783999 ) ) ;
#39397 = VECTOR ( 'NONE', #170701, 1000.000000000000000 ) ;
#39398 = VECTOR ( 'NONE', #87288, 1000.000000000000000 ) ;
#39399 = EDGE_CURVE ( 'NONE', #41111, #172698, #101605, .T. ) ;
#39400 = CARTESIAN_POINT ( 'NONE',  ( -18.54159361262948380, -9.463132135481973961, -174.5491222162928580 ) ) ;
#39401 = AXIS2_PLACEMENT_3D ( 'NONE', #94332, #190912, #12264 ) ;
#39402 = FACE_OUTER_BOUND ( 'NONE', #165975, .T. ) ;
#39403 = ORIENTED_EDGE ( 'NONE', *, *, #125401, .T. ) ;
#39404 = CARTESIAN_POINT ( 'NONE',  ( 20.95512820512820440, 67.12384868372450342, -194.9644784893834810 ) ) ;
#39405 = DIRECTION ( 'NONE',  ( 0.000000000000000000, -1.000000000000000000, -6.982962677686266711E-15 ) ) ;
#39406 = AXIS2_PLACEMENT_3D ( 'NONE', #108151, #9044, #69040 ) ;
#39407 = CIRCLE ( 'NONE', #51821, 0.1000000000000124678 ) ;
#39408 = CARTESIAN_POINT ( 'NONE',  ( -23.25000000000000000, 2.600000000011156054, -80.22462192276213955 ) ) ;
#39410 = EDGE_LOOP ( 'NONE', ( #235812, #65144, #34556, #57222 ) ) ;
#39409 = CARTESIAN_POINT ( 'NONE',  ( 18.39999999999997371, 64.52683809664972614, -145.7731074845244450 ) ) ;
#39412 = DIRECTION ( 'NONE',  ( -1.000000000000000000, -3.265361837132813093E-16, 0.000000000000000000 ) ) ;
#39411 = DIRECTION ( 'NONE',  ( -1.000000000000000000, 0.000000000000000000, 0.000000000000000000 ) ) ;
#39413 = CARTESIAN_POINT ( 'NONE',  ( 23.50000000000005684, 74.94272479589878344, -3.123107484524795474 ) ) ;
#39414 = CARTESIAN_POINT ( 'NONE',  ( -20.94999999999999929, 11.65000000001115232, -134.0000000000000284 ) ) ;
#39415 = CIRCLE ( 'NONE', #185133, 0.09999999999999939493 ) ;
#39416 = DIRECTION ( 'NONE',  ( 1.000000000000000000, 0.000000000000000000, 0.000000000000000000 ) ) ;
#39417 = ORIENTED_EDGE ( 'NONE', *, *, #42636, .F. ) ;
#39418 = AXIS2_PLACEMENT_3D ( 'NONE', #253531, #14953, #210573 ) ;
#39419 = EDGE_CURVE ( 'NONE', #49647, #205311, #205542, .T. ) ;
#39420 = CARTESIAN_POINT ( 'NONE',  ( 0.000000000000000000, 0.000000000000000000, 0.000000000000000000 ) ) ;
#39421 = TOROIDAL_SURFACE ( 'NONE', #110109, 2.100000000000002309, 0.1000000000000000056 ) ;
#39422 = AXIS2_PLACEMENT_3D ( 'NONE', #197431, #134868, #214424 ) ;
#39423 = ORIENTED_EDGE ( 'NONE', *, *, #120739, .T. ) ;
#39424 = ADVANCED_FACE ( 'NONE', ( #258103 ), #117365, .F. ) ;
#39425 = DIRECTION ( 'NONE',  ( 0.000000000000000000, 0.2617529984165031243, 0.9651348961777157509 ) ) ;
#39426 = VERTEX_POINT ( 'NONE', #181205 ) ;
#39427 = DIRECTION ( 'NONE',  ( 1.000000000000000000, 0.000000000000000000, 0.000000000000000000 ) ) ;
#39428 = DIRECTION ( 'NONE',  ( 0.000000000000000000, -6.517943393102682774E-15, 1.000000000000000000 ) ) ;
#39429 = EDGE_CURVE ( 'NONE', #72835, #189461, #22428, .T. ) ;
#39430 = CARTESIAN_POINT ( 'NONE',  ( -16.89268316805465986, 30.21221237062500720, -234.8082435139909592 ) ) ;
#39431 = ORIENTED_EDGE ( 'NONE', *, *, #230518, .F. ) ;
#39432 = VECTOR ( 'NONE', #51245, 1000.000000000000000 ) ;
#39433 = ORIENTED_EDGE ( 'NONE', *, *, #48980, .T. ) ;
#39434 = EDGE_CURVE ( 'NONE', #194529, #146536, #188820, .T. ) ;
#39435 = DIRECTION ( 'NONE',  ( 0.000000000000000000, -0.9126074666063767049, -0.4088369013363286619 ) ) ;
#39437 = CIRCLE ( 'NONE', #193540, 0.09999999999999939493 ) ;
#39436 = CARTESIAN_POINT ( 'NONE',  ( 18.52928932188133970, 10.27928932189250411, -158.6500000000000057 ) ) ;
#39438 = CARTESIAN_POINT ( 'NONE',  ( -16.83233564386394931, 63.07197639479962703, -213.2539030774048570 ) ) ;
#39439 = DIRECTION ( 'NONE',  ( 1.000000000000000000, 0.000000000000000000, 0.000000000000000000 ) ) ;
#39440 = EDGE_CURVE ( 'NONE', #55413, #196163, #161648, .T. ) ;
#39442 = DIRECTION ( 'NONE',  ( 1.040834085586049673E-13, 0.7899159663865300551, 0.6132151058540831201 ) ) ;
#39441 = CARTESIAN_POINT ( 'NONE',  ( -22.00411653889203123, 75.90096189422509099, -143.7765503521646338 ) ) ;
#39443 = LINE ( 'NONE', #139769, #123222 ) ;
#39444 = DIRECTION ( 'NONE',  ( -0.000000000000000000, -0.9875102702516493913, 0.1575546449569621699 ) ) ;
#39445 = CARTESIAN_POINT ( 'NONE',  ( 18.45139536634707511, -9.486081720270043149, -107.1405116178107164 ) ) ;
#39446 = AXIS2_PLACEMENT_3D ( 'NONE', #215036, #135480, #13015 ) ;
#39447 = ORIENTED_EDGE ( 'NONE', *, *, #27338, .T. ) ;
#39448 = DIRECTION ( 'NONE',  ( 0.000000000000000000, 6.982962677686266711E-15, -1.000000000000000000 ) ) ;
#39449 = AXIS2_PLACEMENT_3D ( 'NONE', #39951, #195177, #116895 ) ;
#39450 = ADVANCED_FACE ( 'NONE', ( #217721 ), #239885, .T. ) ;
#39452 = ORIENTED_EDGE ( 'NONE', *, *, #255519, .F. ) ;
#39451 = CARTESIAN_POINT ( 'NONE',  ( -22.94999999999999929, 1.885425182446134107, -11.49641995933507843 ) ) ;
#39453 = AXIS2_PLACEMENT_3D ( 'NONE', #132126, #51265, #186987 ) ;
#39454 = CARTESIAN_POINT ( 'NONE',  ( 22.57320508075688537, 11.75000000000000000, 4.930004492955712146E-16 ) ) ;
#39456 = EDGE_CURVE ( 'NONE', #222175, #140980, #19555, .T. ) ;
#39455 = EDGE_CURVE ( 'NONE', #138980, #49221, #63491, .T. ) ;
#39457 = SPHERICAL_SURFACE ( 'NONE', #53481, 0.1000000000000000056 ) ;
#39459 = DIRECTION ( 'NONE',  ( 0.000000000000000000, 1.000000000000000000, 1.626303258728238113E-15 ) ) ;
#39458 = CARTESIAN_POINT ( 'NONE',  ( -21.05000000000000071, 44.18518595211054389, -258.7688298343402380 ) ) ;
#39460 = ORIENTED_EDGE ( 'NONE', *, *, #159936, .T. ) ;
#39462 = DIRECTION ( 'NONE',  ( 1.000000000000000000, 0.000000000000000000, 0.000000000000000000 ) ) ;
#39461 = CARTESIAN_POINT ( 'NONE',  ( -23.15000000000000213, 19.73066058418984170, -238.2142830767208466 ) ) ;
#39463 = CARTESIAN_POINT ( 'NONE',  ( -18.50000000000000000, -1.835859311432484375, -145.5044391687985694 ) ) ;
#39464 = DIRECTION ( 'NONE',  ( -1.836970198721029934E-16, 1.000000000000000000, 0.000000000000000000 ) ) ;
#39465 = DIRECTION ( 'NONE',  ( 0.000000000000000000, -7.034366652768095332E-15, 1.000000000000000000 ) ) ;
#39466 = CARTESIAN_POINT ( 'NONE',  ( -15.39126916658603861, 66.61042836546617707, -185.7054667721552903 ) ) ;
#39467 = VERTEX_POINT ( 'NONE', #97763 ) ;
#39468 = CARTESIAN_POINT ( 'NONE',  ( -18.59999999999999787, 9.350000000011156942, -155.3500000000000227 ) ) ;
#39469 = VERTEX_POINT ( 'NONE', #255530 ) ;
#39470 = CARTESIAN_POINT ( 'NONE',  ( -18.42637059832564361, -9.496945461889701789, -40.10907730979983654 ) ) ;
#39471 = B_SPLINE_CURVE_WITH_KNOTS ( 'NONE', 3,
 ( #161864, #167014, #246505, #202253, #45739, #224371, #23649, #204797, #220537, #125286, #41919, #121462, #122735, #64023, #84830, #43183, #200963, #243933, #103129, #182704, #22353, #83552, #4041, #181424, #62744, #142269 ),
 .UNSPECIFIED., .F., .F.,
 ( 4, 2, 2, 2, 2, 2, 2, 2, 2, 2, 2, 2, 4 ),
 ( 0.005476422646581358654, 0.006160811967703566129, 0.006845201288825772737, 0.007187395949386878209, 0.007529590609947983681, 0.007871785270509090021, 0.008213979931070194626, 0.008556174591631299231, 0.008898369252192405571, 0.009240563912753511910, 0.009582758573314616515, 0.01026714789443683093, 0.01095153721555904534 ),
 .UNSPECIFIED. ) ;
#39472 = ORIENTED_EDGE ( 'NONE', *, *, #193644, .T. ) ;
#39473 = CARTESIAN_POINT ( 'NONE',  ( 18.49999999999999289, 68.97833521811159585, -65.68954208262705663 ) ) ;
#39474 = EDGE_CURVE ( 'NONE', #133516, #236311, #176366, .T. ) ;
#39475 = VECTOR ( 'NONE', #93500, 1000.000000000000000 ) ;
#39476 = ADVANCED_FACE ( 'NONE', ( #119962 ), #200751, .F. ) ;
#39477 = EDGE_LOOP ( 'NONE', ( #27870, #90152, #82934, #50124, #198239 ) ) ;
#39478 = CARTESIAN_POINT ( 'NONE',  ( -22.24259225415828567, 7.491937870576586889, -167.4009341165471199 ) ) ;
#39479 = EDGE_CURVE ( 'NONE', #3284, #116043, #16993, .T. ) ;
#39480 =( BOUNDED_SURFACE ( )  B_SPLINE_SURFACE ( 3, 2, ( 
 ( #71413, #115654, #34862 ),
 ( #209619, #33598, #16568 ),
 ( #110509, #250027, #170549 ),
 ( #96067, #132655, #213462 ) ),
 .UNSPECIFIED., .F., .F., .F. ) 
 B_SPLINE_SURFACE_WITH_KNOTS ( ( 4, 4 ),
 ( 3, 3 ),
 ( 0.0002700421466196735562, 0.0004789321604330922682 ),
 ( 0.000000000000000000, 1.000000000000000000 ),
 .UNSPECIFIED. ) 
 GEOMETRIC_REPRESENTATION_ITEM ( )  RATIONAL_B_SPLINE_SURFACE ( (
 ( 1.000000000000000000, 0.7071067811865475727, 1.000000000000000000),
 ( 1.000000000000000000, 0.7163411249511749679, 1.000000000000000000),
 ( 1.000000000000000000, 0.7221957104841917330, 1.000000000000000000),
 ( 1.000000000000000000, 0.7250110520819876836, 1.000000000000000000) ) ) 
 REPRESENTATION_ITEM ( '' )  SURFACE ( )  );
#39481 = DIRECTION ( 'NONE',  ( 1.000000000000000000, 0.000000000000000000, 0.000000000000000000 ) ) ;
#39482 = EDGE_LOOP ( 'NONE', ( #61649, #151980, #167263, #122401 ) ) ;
#39483 = EDGE_CURVE ( 'NONE', #236905, #64897, #156524, .T. ) ;
#39484 = CARTESIAN_POINT ( 'NONE',  ( -18.45140287520616695, -9.486077739518414376, -174.1405231266861051 ) ) ;
#39485 = EDGE_CURVE ( 'NONE', #24624, #257729, #237314, .T. ) ;
#39486 = DIRECTION ( 'NONE',  ( 0.000000000000000000, -6.982962677686266711E-15, 1.000000000000000000 ) ) ;
#39487 = CARTESIAN_POINT ( 'NONE',  ( 21.00000000000000000, 43.94346684630428967, -235.6041041703296344 ) ) ;
#39488 = CARTESIAN_POINT ( 'NONE',  ( 18.59999999999999432, 70.30054753569044124, -115.5653814410941891 ) ) ;
#39489 = DIRECTION ( 'NONE',  ( -1.000000000000000000, -1.836970198721029934E-16, 0.000000000000000000 ) ) ;
#39490 = CARTESIAN_POINT ( 'NONE',  ( 22.49806830649814060, 12.56154382881637943, -223.4268007483960616 ) ) ;
#39491 = ORIENTED_EDGE ( 'NONE', *, *, #117642, .F. ) ;
#39492 = FACE_OUTER_BOUND ( 'NONE', #108180, .T. ) ;
#39493 = ORIENTED_EDGE ( 'NONE', *, *, #225795, .F. ) ;
#39495 = ORIENTED_EDGE ( 'NONE', *, *, #101176, .F. ) ;
#39494 = CARTESIAN_POINT ( 'NONE',  ( -16.86379686415369861, 66.02478224075871083, -90.45649737361466691 ) ) ;
#39496 = AXIS2_PLACEMENT_3D ( 'NONE', #230018, #224868, #28003 ) ;
#39497 = ORIENTED_EDGE ( 'NONE', *, *, #17392, .T. ) ;
#39498 = CIRCLE ( 'NONE', #152090, 0.1000000000000043493 ) ;
#39499 = DIRECTION ( 'NONE',  ( 0.000000000000000000, -6.938893903907222067E-15, 1.000000000000000000 ) ) ;
#39500 = DIRECTION ( 'NONE',  ( 1.000000000000000000, -3.151514657663852580E-16, 8.547182517843351137E-17 ) ) ;
#39501 = CARTESIAN_POINT ( 'NONE',  ( 14.11444803880197441, 66.54256847116367624, -188.5231905466248179 ) ) ;
#39502 = CARTESIAN_POINT ( 'NONE',  ( 23.14999999999999503, 64.35000000001204512, -124.3731074845243825 ) ) ;
#39503 = CARTESIAN_POINT ( 'NONE',  ( -23.25000000000000000, 76.00000000001244871, -170.0231074845243597 ) ) ;
#39504 = ORIENTED_EDGE ( 'NONE', *, *, #234376, .T. ) ;
#39505 = ADVANCED_FACE ( 'NONE', ( #243727 ), #162929, .F. ) ;
#39506 = DIRECTION ( 'NONE',  ( 0.000000000000000000, 0.9908441862701596881, -0.1350103645451904977 ) ) ;
#39507 = DIRECTION ( 'NONE',  ( 0.000000000000000000, 6.982962677686266711E-15, -1.000000000000000000 ) ) ;
#39508 = ORIENTED_EDGE ( 'NONE', *, *, #214019, .T. ) ;
#39510 = VERTEX_POINT ( 'NONE', #5079 ) ;
#39509 = DIRECTION ( 'NONE',  ( 1.000000000000000000, 0.000000000000000000, 0.000000000000000000 ) ) ;
#39511 = CARTESIAN_POINT ( 'NONE',  ( 18.59999999999999787, -9.321008403350148797, -174.7359382490778330 ) ) ;
#39512 = EDGE_CURVE ( 'NONE', #187169, #25173, #224151, .T. ) ;
#39514 = CONICAL_SURFACE ( 'NONE', #185219, 4.299999999999970512, 0.7853981633974466137 ) ;
#39513 = CARTESIAN_POINT ( 'NONE',  ( -16.84793658983432607, 9.950000000011140600, -79.73364667781054038 ) ) ;
#39515 = VERTEX_POINT ( 'NONE', #205874 ) ;
#39516 = AXIS2_PLACEMENT_3D ( 'NONE', #212683, #34075, #8066 ) ;
#39517 = CIRCLE ( 'NONE', #76884, 0.09999999999999939493 ) ;
#39518 = AXIS2_PLACEMENT_3D ( 'NONE', #236680, #200144, #197559 ) ;
#39519 = DIRECTION ( 'NONE',  ( 0.000000000000000000, -0.4834676483507011624, -0.8753622295931228203 ) ) ;
#39520 = ORIENTED_EDGE ( 'NONE', *, *, #82379, .T. ) ;
#39521 = DIRECTION ( 'NONE',  ( -1.000000000000000000, 0.000000000000000000, 0.000000000000000000 ) ) ;
#39522 = EDGE_CURVE ( 'NONE', #171717, #122037, #187621, .T. ) ;
#39523 = CARTESIAN_POINT ( 'NONE',  ( 21.05000000000000071, 68.96522873961046685, -235.0783363939394235 ) ) ;
#39524 = CARTESIAN_POINT ( 'NONE',  ( 15.07585980824113747, 66.58236703690523939, -51.37415901879214175 ) ) ;
#39525 = CARTESIAN_POINT ( 'NONE',  ( -18.59999999999999787, -9.499999999988849808, -108.6000000000000227 ) ) ;
#39527 = B_SPLINE_CURVE_WITH_KNOTS ( 'NONE', 3,
 ( #237891, #198759, #236595, #102198, #200059, #59212, #121816, #123096, #197473, #180498 ),
 .UNSPECIFIED., .F., .F.,
 ( 4, 3, 3, 4 ),
 ( 0.000000000000000000, 0.0002000000000002884074, 0.001000000000045107602, 0.001967863649472132576 ),
 .UNSPECIFIED. ) ;
#39526 = CIRCLE ( 'NONE', #185243, 0.1000000000000013933 ) ;
#39528 = EDGE_CURVE ( 'NONE', #97490, #98150, #7188, .T. ) ;
#39529 = AXIS2_PLACEMENT_3D ( 'NONE', #77050, #156636, #236130 ) ;
#39530 = EDGE_LOOP ( 'NONE', ( #133654, #138887, #248770, #189325 ) ) ;
#39531 = CARTESIAN_POINT ( 'NONE',  ( -18.40000000000000213, 64.51332499825441857, -127.2731074845243882 ) ) ;
#39532 = TOROIDAL_SURFACE ( 'NONE', #93658, 11.70000000000000107, 0.1000000000000000056 ) ;
#39533 = AXIS2_PLACEMENT_3D ( 'NONE', #46798, #126353, #207192 ) ;
#39534 = ORIENTED_EDGE ( 'NONE', *, *, #194647, .T. ) ;
#39535 = CARTESIAN_POINT ( 'NONE',  ( -21.05000000000000071, -11.39257802169451672, -36.57394957983193251 ) ) ;
#39536 = DIRECTION ( 'NONE',  ( 1.000000000000000000, -0.000000000000000000, -0.000000000000000000 ) ) ;
#39538 = ORIENTED_EDGE ( 'NONE', *, *, #45596, .F. ) ;
#39537 = DIRECTION ( 'NONE',  ( -1.000000000000000000, 0.000000000000000000, -0.000000000000000000 ) ) ;
#39539 = CARTESIAN_POINT ( 'NONE',  ( 20.95512820512820440, 67.12384868372345181, -57.37310748452438247 ) ) ;
#39540 = CARTESIAN_POINT ( 'NONE',  ( -11.60000000000000320, -11.65000000000000036, 12.30000000000000426 ) ) ;
#39541 = LINE ( 'NONE', #40821, #143688 ) ;
#39543 = CARTESIAN_POINT ( 'NONE',  ( 21.10257677756355932, 75.97504925044398760, -109.4214892270570658 ) ) ;
#39542 =( BOUNDED_CURVE ( )  B_SPLINE_CURVE ( 3, ( #249346, #53693, #133234, #212782 ),
 .UNSPECIFIED., .F., .F. ) 
 B_SPLINE_CURVE_WITH_KNOTS ( ( 4, 4 ),
 ( 0.06456096931748350753, 3.077031684272309775 ),
 .UNSPECIFIED. ) 
 CURVE ( )  GEOMETRIC_REPRESENTATION_ITEM ( )  RATIONAL_B_SPLINE_CURVE ( ( 1.000000000000000000, 0.3763440860215095940, 0.3763440860215095940, 1.000000000000000000 ) ) 
 REPRESENTATION_ITEM ( '' )  );
#39544 = CARTESIAN_POINT ( 'NONE',  ( -16.92507428761702926, 9.950000000011137047, -180.2133974596215467 ) ) ;
#39545 = AXIS2_PLACEMENT_3D ( 'NONE', #48751, #73492, #192147 ) ;
#39546 = DIRECTION ( 'NONE',  ( 0.000000000000000000, 0.9126074666064812879, 0.4088369013360954596 ) ) ;
#39547 = CIRCLE ( 'NONE', #251878, 2.000000000000009326 ) ;
#39548 = CARTESIAN_POINT ( 'NONE',  ( -18.39999999999999858, 85.50000000001209344, -129.4910380878245917 ) ) ;
#39550 = ORIENTED_EDGE ( 'NONE', *, *, #237255, .F. ) ;
#39549 = CARTESIAN_POINT ( 'NONE',  ( 21.14999999999999858, 13.96869538424789070, -210.3925794786331949 ) ) ;
#39551 = TOROIDAL_SURFACE ( 'NONE', #226954, 0.9750000000000019762, 0.1000000000000000056 ) ;
#39552 = AXIS2_PLACEMENT_3D ( 'NONE', #17243, #231160, #250686 ) ;
#39553 = DIRECTION ( 'NONE',  ( 1.000000000000000000, 0.000000000000000000, 0.000000000000000000 ) ) ;
#39554 = AXIS2_PLACEMENT_3D ( 'NONE', #64865, #23209, #141835 ) ;
#39555 = VERTEX_POINT ( 'NONE', #144605 ) ;
#39556 = ORIENTED_EDGE ( 'NONE', *, *, #222009, .T. ) ;
#39557 = AXIS2_PLACEMENT_3D ( 'NONE', #175756, #3497, #45202 ) ;
#39558 = LINE ( 'NONE', #241569, #153405 ) ;
#39559 = DIRECTION ( 'NONE',  ( -0.000000000000000000, -0.9887567792719339499, -0.1495327102803676589 ) ) ;
#39560 = VECTOR ( 'NONE', #155371, 1000.000000000000000 ) ;
#39562 = VERTEX_POINT ( 'NONE', #68964 ) ;
#39561 = VECTOR ( 'NONE', #11281, 1000.000000000000000 ) ;
#39563 = FACE_OUTER_BOUND ( 'NONE', #257678, .T. ) ;
#39564 = ADVANCED_FACE ( 'NONE', ( #67653 ), #223850, .T. ) ;
#39565 =( NAMED_UNIT ( * ) SI_UNIT ( $, .STERADIAN. ) SOLID_ANGLE_UNIT ( ) );
#39566 = ORIENTED_EDGE ( 'NONE', *, *, #148262, .T. ) ;
#39567 = DIRECTION ( 'NONE',  ( -1.000000000000000000, 0.000000000000000000, 0.000000000000000000 ) ) ;
#39568 =( BOUNDED_SURFACE ( )  B_SPLINE_SURFACE ( 3, 2, ( 
 ( #48744, #153035, #34359 ),
 ( #51290, #232558, #53894 ),
 ( #250800, #113865, #193422 ),
 ( #30497, #173890, #210417 ) ),
 .UNSPECIFIED., .F., .F., .F. ) 
 B_SPLINE_SURFACE_WITH_KNOTS ( ( 4, 4 ),
 ( 3, 3 ),
 ( -5.827586677109586333E-19, 0.0003124336117481331431 ),
 ( 0.000000000000000000, 1.000000000000000000 ),
 .UNSPECIFIED. ) 
 GEOMETRIC_REPRESENTATION_ITEM ( )  RATIONAL_B_SPLINE_SURFACE ( (
 ( 1.000000000000000000, 0.7040654476015839602, 1.000000000000000000),
 ( 1.000000000000000000, 0.7039193538781748360, 1.000000000000000000),
 ( 1.000000000000000000, 0.7089171279145581872, 1.000000000000000000),
 ( 1.000000000000000000, 0.7071067811865509034, 1.000000000000000000) ) ) 
 REPRESENTATION_ITEM ( '' )  SURFACE ( )  );
#39569 = CARTESIAN_POINT ( 'NONE',  ( -16.93583594267724379, 65.99137656496040449, -190.9637166452036752 ) ) ;
#39570 = ORIENTED_EDGE ( 'NONE', *, *, #155723, .T. ) ;
#39571 = CARTESIAN_POINT ( 'NONE',  ( -18.37013991200266005, 64.50025238379953407, -45.23008447400728471 ) ) ;
#39572 = EDGE_LOOP ( 'NONE', ( #237391, #221442, #136934, #59098 ) ) ;
#39573 = EDGE_CURVE ( 'NONE', #232297, #57850, #186330, .T. ) ;
#39574 = CARTESIAN_POINT ( 'NONE',  ( -16.97683809663753252, 9.950000000011140600, -46.77152476866995556 ) ) ;
#39576 = ORIENTED_EDGE ( 'NONE', *, *, #159199, .T. ) ;
#39575 = DIRECTION ( 'NONE',  ( 0.000000000000000000, 0.4088369013363287729, -0.9126074666063767049 ) ) ;
#39578 = ADVANCED_FACE ( 'NONE', ( #65084 ), #190576, .T. ) ;
#39577 = PLANE ( 'NONE',  #73631 ) ;
#39579 = EDGE_LOOP ( 'NONE', ( #100467, #210871, #40036, #255029 ) ) ;
#39580 = CIRCLE ( 'NONE', #23006, 0.09999999999999939493 ) ;
#39581 = CARTESIAN_POINT ( 'NONE',  ( -22.39999999999999858, 75.90000000001273861, -211.3138870828977645 ) ) ;
#39582 = ORIENTED_EDGE ( 'NONE', *, *, #101289, .T. ) ;
#39583 = CIRCLE ( 'NONE', #72901, 0.1000000000000028783 ) ;
#39585 = EDGE_LOOP ( 'NONE', ( #134600, #175889, #38595, #196617 ) ) ;
#39584 = ORIENTED_EDGE ( 'NONE', *, *, #182222, .F. ) ;
#39586 = CARTESIAN_POINT ( 'NONE',  ( 21.09096482362058111, 69.63645563460765686, -136.5625557632984624 ) ) ;
#39587 = ORIENTED_EDGE ( 'NONE', *, *, #152429, .T. ) ;
#39588 = CIRCLE ( 'NONE', #39401, 0.09999999999999939493 ) ;
#39589 = DIRECTION ( 'NONE',  ( -0.000000000000000000, 0.2128009952263604232, -0.9770955615653316162 ) ) ;
#39591 = EDGE_CURVE ( 'NONE', #12734, #44233, #240440, .T. ) ;
#39590 = ORIENTED_EDGE ( 'NONE', *, *, #43194, .T. ) ;
#39592 = EDGE_CURVE ( 'NONE', #29887, #151973, #248835, .T. ) ;
#39593 = AXIS2_PLACEMENT_3D ( 'NONE', #148059, #228879, #48942 ) ;
#39594 = EDGE_CURVE ( 'NONE', #16498, #201210, #105459, .T. ) ;
#39595 = ORIENTED_EDGE ( 'NONE', *, *, #132156, .F. ) ;
#39596 = CARTESIAN_POINT ( 'NONE',  ( 20.94999999999999929, 14.05000000001115623, -195.4863049292390542 ) ) ;
#39597 = DIRECTION ( 'NONE',  ( -1.000000000000000000, -0.000000000000000000, 0.000000000000000000 ) ) ;
#39599 = ORIENTED_EDGE ( 'NONE', *, *, #235926, .F. ) ;
#39598 = CARTESIAN_POINT ( 'NONE',  ( 20.73486653747088937, 62.17269434303373288, -224.8990429791066106 ) ) ;
#39600 = FACE_OUTER_BOUND ( 'NONE', #2456, .T. ) ;
#39601 = EDGE_LOOP ( 'NONE', ( #100469, #50117, #78629, #178357 ) ) ;
#39602 = EDGE_CURVE ( 'NONE', #25623, #8352, #66377, .T. ) ;
#39603 = CARTESIAN_POINT ( 'NONE',  ( 21.14999999999999858, -11.75000000000000000, -12.25000000000000000 ) ) ;
#39604 = FACE_OUTER_BOUND ( 'NONE', #7581, .T. ) ;
#39605 = VECTOR ( 'NONE', #218248, 1000.000000000000000 ) ;
#39606 = EDGE_LOOP ( 'NONE', ( #103083, #210435, #250986, #96131, #140529, #199645, #250132 ) ) ;
#39607 = DIRECTION ( 'NONE',  ( 0.000000000000000000, 0.2128009952263603954, -0.9770955615653316162 ) ) ;
#39608 = CARTESIAN_POINT ( 'NONE',  ( 23.15000000000000213, -6.388372595096674544, -212.0629706944429813 ) ) ;
#39609 = DIRECTION ( 'NONE',  ( 1.000000000000000000, 0.000000000000000000, 0.000000000000000000 ) ) ;
#39610 = EDGE_CURVE ( 'NONE', #131734, #7066, #178097, .T. ) ;
#39611 = AXIS2_PLACEMENT_3D ( 'NONE', #163457, #82590, #22684 ) ;
#39612 = VERTEX_POINT ( 'NONE', #225422 ) ;
#39613 = DIRECTION ( 'NONE',  ( 0.000000000000000000, -8.881784197001250746E-15, 1.000000000000000000 ) ) ;
#39614 = ORIENTED_EDGE ( 'NONE', *, *, #243178, .F. ) ;
#39615 = ORIENTED_EDGE ( 'NONE', *, *, #165592, .F. ) ;
#39616 = CARTESIAN_POINT ( 'NONE',  ( -18.40000000000000213, 64.51332499825412015, -78.77310748452438816 ) ) ;
#39617 = ORIENTED_EDGE ( 'NONE', *, *, #216232, .T. ) ;
#39618 = ORIENTED_EDGE ( 'NONE', *, *, #97223, .T. ) ;
#39619 = DIRECTION ( 'NONE',  ( 1.000000000000000000, 0.000000000000000000, 0.000000000000000000 ) ) ;
#39620 = CARTESIAN_POINT ( 'NONE',  ( -16.93826681692523195, 10.01142872029886632, -188.4454584673594013 ) ) ;
#39621 = ORIENTED_EDGE ( 'NONE', *, *, #165027, .F. ) ;
#39622 = AXIS2_PLACEMENT_3D ( 'NONE', #170132, #249638, #190961 ) ;
#39623 = ORIENTED_EDGE ( 'NONE', *, *, #94311, .F. ) ;
#39624 = DIRECTION ( 'NONE',  ( -0.000000000000000000, 1.000000000000000000, 0.000000000000000000 ) ) ;
#39625 = CARTESIAN_POINT ( 'NONE',  ( -33.72168855820451938, 66.05000000001156479, -56.87310748452444642 ) ) ;
#39626 = ADVANCED_FACE ( 'NONE', ( #46790 ), #147189, .F. ) ;
#39627 = EDGE_LOOP ( 'NONE', ( #18681, #30988, #38405, #203410 ) ) ;
#39628 = ORIENTED_EDGE ( 'NONE', *, *, #68638, .T. ) ;
#39629 = ORIENTED_EDGE ( 'NONE', *, *, #229735, .T. ) ;
#39630 = CIRCLE ( 'NONE', #77006, 0.09999999999999609201 ) ;
#39631 = VECTOR ( 'NONE', #15749, 1000.000000000000000 ) ;
#39632 = EDGE_CURVE ( 'NONE', #203844, #103016, #161347, .T. ) ;
#39633 = CARTESIAN_POINT ( 'NONE',  ( 21.07928932188134397, 69.67148334361937145, -203.6220026301788266 ) ) ;
#39634 = DIRECTION ( 'NONE',  ( -1.000000000000000000, -0.000000000000000000, -0.000000000000000000 ) ) ;
#39635 = CARTESIAN_POINT ( 'NONE',  ( -5.999999999999938716, 64.65000000001120384, -22.12310748452479103 ) ) ;
#39636 = DIRECTION ( 'NONE',  ( 0.000000000000000000, 1.000000000000000000, 0.000000000000000000 ) ) ;
#39637 = CARTESIAN_POINT ( 'NONE',  ( 21.05000000000000071, 65.52661458509942349, -162.4444530202758870 ) ) ;
#39638 = DIRECTION ( 'NONE',  ( 0.000000000000000000, 0.9651348961777157509, -0.2617529984165031243 ) ) ;
#39639 = CARTESIAN_POINT ( 'NONE',  ( 23.14999999999999503, 64.35000000001146248, -43.03791325517834565 ) ) ;
#39641 = CARTESIAN_POINT ( 'NONE',  ( -18.40000000000000213, 70.35000000001207354, -123.8731074845243398 ) ) ;
#39640 = DIRECTION ( 'NONE',  ( 0.000000000000000000, -0.9126074666063844765, -0.4088369013363114535 ) ) ;
#39642 = CARTESIAN_POINT ( 'NONE',  ( -20.94999999999999929, -11.48912529306489994, -97.60000000000005116 ) ) ;
#39643 = CARTESIAN_POINT ( 'NONE',  ( -16.96982749440685012, 23.39658237464075796, -231.1592503940484846 ) ) ;
#39644 = SPHERICAL_SURFACE ( 'NONE', #97639, 0.1000000000000000056 ) ;
#39645 = DIRECTION ( 'NONE',  ( 1.000000000000000000, -0.000000000000000000, -0.000000000000000000 ) ) ;
#39646 = AXIS2_PLACEMENT_3D ( 'NONE', #103737, #201579, #141609 ) ;
#39647 = ORIENTED_EDGE ( 'NONE', *, *, #38261, .F. ) ;
#39648 = EDGE_CURVE ( 'NONE', #172354, #134581, #47770, .T. ) ;
#39649 = CIRCLE ( 'NONE', #231182, 0.1000000000000028644 ) ;
#39650 = EDGE_LOOP ( 'NONE', ( #14279, #155882, #148205, #197748 ) ) ;
#39651 = CARTESIAN_POINT ( 'NONE',  ( -23.25000000000000000, -1.149570369575693807, -41.31591248450196474 ) ) ;
#39652 = EDGE_CURVE ( 'NONE', #186897, #111851, #98944, .T. ) ;
#39653 = LINE ( 'NONE', #257322, #94390 ) ;
#39654 = CARTESIAN_POINT ( 'NONE',  ( -22.41119224318417125, 64.18196446391819165, -247.0985338183330668 ) ) ;
#39655 = ORIENTED_EDGE ( 'NONE', *, *, #102530, .T. ) ;
#39656 = ADVANCED_FACE ( 'NONE', ( #74109 ), #15402, .F. ) ;
#39657 = ADVANCED_FACE ( 'NONE', ( #252692 ), #228016, .F. ) ;
#39658 = DIRECTION ( 'NONE',  ( 1.000000000000000000, 0.000000000000000000, -0.000000000000000000 ) ) ;
#39659 = CARTESIAN_POINT ( 'NONE',  ( 23.24999999999999289, 4.149999999999999467, 5.082284216461512198E-16 ) ) ;
#39660 = ADVANCED_FACE ( 'NONE', ( #54502 ), #130182, .T. ) ;
#39661 = ORIENTED_EDGE ( 'NONE', *, *, #71346, .F. ) ;
#39663 = CARTESIAN_POINT ( 'NONE',  ( -18.50596464788227635, 10.30632246271647112, -206.5041836778895572 ) ) ;
#39662 = AXIS2_PLACEMENT_3D ( 'NONE', #156009, #78978, #98526 ) ;
#39664 = CARTESIAN_POINT ( 'NONE',  ( 21.70464131381650219, 68.90464198104380955, -69.52310748452435973 ) ) ;
#39665 = CARTESIAN_POINT ( 'NONE',  ( -23.15000000000000213, 0.000000000000000000, 0.000000000000000000 ) ) ;
#39666 = EDGE_CURVE ( 'NONE', #80661, #2887, #53186, .T. ) ;
#39667 = DIRECTION ( 'NONE',  ( 0.000000000000000000, -1.000000000000000000, -6.982962677686266711E-15 ) ) ;
#39669 = VERTEX_POINT ( 'NONE', #251428 ) ;
#39668 = CARTESIAN_POINT ( 'NONE',  ( -21.55000000000000071, 7.350000000011155166, -79.25000000000004263 ) ) ;
#39671 = ORIENTED_EDGE ( 'NONE', *, *, #181576, .F. ) ;
#39670 = DIRECTION ( 'NONE',  ( 1.836970198721029934E-16, -1.000000000000000000, -0.000000000000000000 ) ) ;
#39672 = CARTESIAN_POINT ( 'NONE',  ( -22.49806830649814415, 11.64988965485023620, -167.4225356836744538 ) ) ;
#39673 = CYLINDRICAL_SURFACE ( 'NONE', #58328, 0.1000000000000028644 ) ;
#39674 = DIRECTION ( 'NONE',  ( 0.000000000000000000, 0.000000000000000000, -1.000000000000000000 ) ) ;
#39675 = CARTESIAN_POINT ( 'NONE',  ( -15.06774609480955718, 9.417651958852163219, -182.8587873924404335 ) ) ;
#39677 = CARTESIAN_POINT ( 'NONE',  ( -18.59999999999999787, 9.122720154857397290, -245.4644708025847990 ) ) ;
#39676 = DIRECTION ( 'NONE',  ( 0.000000000000000000, 0.2128009952264065807, -0.9770955615653215132 ) ) ;
#39678 = CARTESIAN_POINT ( 'NONE',  ( 22.47071067811865319, 7.720074744498043096, 0.09909245470260744093 ) ) ;
#39679 = DIRECTION ( 'NONE',  ( 0.000000000000000000, -0.9126074666063660468, -0.4088369013363524762 ) ) ;
#39680 = AXIS2_PLACEMENT_3D ( 'NONE', #146971, #205666, #209533 ) ;
#39681 = DIRECTION ( 'NONE',  ( 0.000000000000000000, 0.1618390714546129594, 0.9868171638914214894 ) ) ;
#39682 = DIRECTION ( 'NONE',  ( 0.000000000000000000, -1.000000000000000000, 0.000000000000000000 ) ) ;
#39683 = AXIS2_PLACEMENT_3D ( 'NONE', #136980, #93993, #138246 ) ;
#39684 = CARTESIAN_POINT ( 'NONE',  ( -23.15000000000000213, 4.250000000011156409, -155.2500000000000284 ) ) ;
#39685 = AXIS2_PLACEMENT_3D ( 'NONE', #191089, #12447, #15011 ) ;
#39686 = ORIENTED_EDGE ( 'NONE', *, *, #29647, .T. ) ;
#39687 = CIRCLE ( 'NONE', #27227, 0.1000000000000021289 ) ;
#39688 = EDGE_CURVE ( 'NONE', #96459, #104969, #148875, .T. ) ;
#39689 = CARTESIAN_POINT ( 'NONE',  ( 21.05000000000000071, 0.03201369319892944515, -94.24115727646220364 ) ) ;
#39690 = ORIENTED_EDGE ( 'NONE', *, *, #148362, .T. ) ;
#39691 = ORIENTED_EDGE ( 'NONE', *, *, #36553, .F. ) ;
#39692 = DIRECTION ( 'NONE',  ( 1.000000000000000000, 0.000000000000000000, 0.000000000000000000 ) ) ;
#39693 = CARTESIAN_POINT ( 'NONE',  ( 20.94999999999999929, 19.68370618165487329, -225.3554403480446240 ) ) ;
#39694 = ADVANCED_FACE ( 'NONE', ( #229309 ), #151056, .T. ) ;
#39695 = VERTEX_POINT ( 'NONE', #128924 ) ;
#39696 = EDGE_CURVE ( 'NONE', #171051, #160189, #232273, .T. ) ;
#39697 = VERTEX_POINT ( 'NONE', #114484 ) ;
#39698 =( NAMED_UNIT ( * ) PLANE_ANGLE_UNIT ( ) SI_UNIT ( $, .RADIAN. ) );
#39699 = ORIENTED_EDGE ( 'NONE', *, *, #30754, .F. ) ;
#39700 = CIRCLE ( 'NONE', #156224, 0.1999999999999987899 ) ;
#39701 = EDGE_LOOP ( 'NONE', ( #101210, #77159, #200581, #244767, #187786 ) ) ;
#39702 = AXIS2_PLACEMENT_3D ( 'NONE', #80625, #2374, #221415 ) ;
#39703 = DIRECTION ( 'NONE',  ( -0.000000000000000000, 6.982962677686266711E-15, -1.000000000000000000 ) ) ;
#39704 = CARTESIAN_POINT ( 'NONE',  ( -21.07016717457011268, -5.827586677109586333E-16, 6.320940838100898240 ) ) ;
#39705 = DIRECTION ( 'NONE',  ( 0.000000000000000000, 0.008583690987124399305, -0.9999631594459055250 ) ) ;
#39706 = CIRCLE ( 'NONE', #185430, 4.299999999999956302 ) ;
#39707 = FACE_OUTER_BOUND ( 'NONE', #65017, .T. ) ;
#39708 = DIRECTION ( 'NONE',  ( -1.000000000000000000, 8.673617379884087537E-15, 0.000000000000000000 ) ) ;
#39709 = DIRECTION ( 'NONE',  ( 0.000000000000000000, 0.1350103645451945777, -0.9908441862701591329 ) ) ;
#39710 = FACE_OUTER_BOUND ( 'NONE', #136016, .T. ) ;
#39712 = ORIENTED_EDGE ( 'NONE', *, *, #112093, .T. ) ;
#39711 = CARTESIAN_POINT ( 'NONE',  ( -21.65000000000000213, 7.708578643762696636, -12.25000000000000000 ) ) ;
#39714 = DIRECTION ( 'NONE',  ( -2.952720810173289112E-16, 1.000000000000000000, 0.000000000000000000 ) ) ;
#39713 = DIRECTION ( 'NONE',  ( 0.000000000000000000, -0.4088369013363783999, 0.9126074666063545004 ) ) ;
#39715 = CARTESIAN_POINT ( 'NONE',  ( 23.14999999999999858, 79.90000000001190017, -103.0231074845242745 ) ) ;
#39716 = ORIENTED_EDGE ( 'NONE', *, *, #56135, .T. ) ;
#39717 = CIRCLE ( 'NONE', #85428, 0.1000000000000000472 ) ;
#39718 = FACE_OUTER_BOUND ( 'NONE', #191416, .T. ) ;
#39719 = DIRECTION ( 'NONE',  ( 0.000000000000000000, 1.000000000000000000, 1.734723475976817507E-14 ) ) ;
#39720 = CIRCLE ( 'NONE', #85429, 0.09999999999999983902 ) ;
#39722 = ORIENTED_EDGE ( 'NONE', *, *, #64176, .F. ) ;
#39721 = AXIS2_PLACEMENT_3D ( 'NONE', #59108, #240365, #139946 ) ;
#39723 = ADVANCED_FACE ( 'NONE', ( #190183 ), #208474, .T. ) ;
#39725 = LINE ( 'NONE', #256104, #4247 ) ;
#39724 = CARTESIAN_POINT ( 'NONE',  ( 21.05000000000000071, 69.65000000001187175, -93.17928539484123007 ) ) ;
#39726 = CARTESIAN_POINT ( 'NONE',  ( -16.97683809663752186, 66.05000000001182059, -82.92547150272069700 ) ) ;
#39727 = FACE_OUTER_BOUND ( 'NONE', #202680, .T. ) ;
#39728 = ORIENTED_EDGE ( 'NONE', *, *, #208662, .F. ) ;
#39729 = CIRCLE ( 'NONE', #2263, 0.09999999999998898659 ) ;
#39730 = DIRECTION ( 'NONE',  ( -1.000000000000000000, -0.000000000000000000, 0.000000000000000000 ) ) ;
#39731 = VECTOR ( 'NONE', #171275, 1000.000000000000000 ) ;
#39732 = CARTESIAN_POINT ( 'NONE',  ( -18.31331870001017137, -0.7273975225635296304, -242.4732920726780208 ) ) ;
#39733 = CARTESIAN_POINT ( 'NONE',  ( -20.54999999999999716, 71.09390016509016164, -212.4439151503019900 ) ) ;
#39734 = CARTESIAN_POINT ( 'NONE',  ( -20.94999999999999929, 18.92285928089247804, -233.3572654221044900 ) ) ;
#39735 = ORIENTED_EDGE ( 'NONE', *, *, #80674, .T. ) ;
#39736 = AXIS2_PLACEMENT_3D ( 'NONE', #64768, #62217, #41389 ) ;
#39737 = CIRCLE ( 'NONE', #60713, 2.099999999999990763 ) ;
#39738 = CYLINDRICAL_SURFACE ( 'NONE', #250523, 0.09999999999998898659 ) ;
#39739 = EDGE_CURVE ( 'NONE', #241011, #32549, #194046, .T. ) ;
#39740 = LINE ( 'NONE', #236610, #190070 ) ;
#39741 = CARTESIAN_POINT ( 'NONE',  ( 21.05000000000000071, 65.71172719659838890, -223.0701118083454446 ) ) ;
#39742 = DIRECTION ( 'NONE',  ( -1.000000000000000000, 1.387778780781454006E-13, 0.000000000000000000 ) ) ;
#39743 = EDGE_CURVE ( 'NONE', #114996, #124577, #140469, .T. ) ;
#39744 = DIRECTION ( 'NONE',  ( 0.000000000000000000, -7.056502275159890832E-15, -1.000000000000000000 ) ) ;
#39745 = CARTESIAN_POINT ( 'NONE',  ( -18.47653818581421348, 85.46528038777530867, -162.8971466683844653 ) ) ;
#39746 = EDGE_CURVE ( 'NONE', #126149, #132220, #28085, .T. ) ;
#39748 = ORIENTED_EDGE ( 'NONE', *, *, #164623, .F. ) ;
#39747 = DIRECTION ( 'NONE',  ( 0.000000000000000000, 0.000000000000000000, -1.000000000000000000 ) ) ;
#39749 = CARTESIAN_POINT ( 'NONE',  ( 18.49999999999999645, -1.866714910046153308, -45.25267524628200988 ) ) ;
#39750 = EDGE_CURVE ( 'NONE', #235986, #119433, #207139, .T. ) ;
#39751 = CYLINDRICAL_SURFACE ( 'NONE', #61490, 0.1000000000000028644 ) ;
#39752 = DIRECTION ( 'NONE',  ( 0.000000000000000000, 1.000000000000000000, 0.000000000000000000 ) ) ;
#39753 = CARTESIAN_POINT ( 'NONE',  ( 21.04999999999999716, -0.08561306079281386094, -94.08624026618971925 ) ) ;
#39754 = CARTESIAN_POINT ( 'NONE',  ( 20.94999999999999929, 10.47338541492405106, -175.0786544642485012 ) ) ;
#39756 = EDGE_LOOP ( 'NONE', ( #95402, #218047, #208242, #56597 ) ) ;
#39755 = FACE_OUTER_BOUND ( 'NONE', #119806, .T. ) ;
#39757 = CARTESIAN_POINT ( 'NONE',  ( 20.95512820512820440, 8.876151316288114046, -12.15000000000000036 ) ) ;
#39758 = DIRECTION ( 'NONE',  ( -0.000000000000000000, -0.000000000000000000, 1.000000000000000000 ) ) ;
#39759 = FACE_BOUND ( 'NONE', #45272, .T. ) ;
#39760 = ORIENTED_EDGE ( 'NONE', *, *, #14021, .T. ) ;
#39761 = DIRECTION ( 'NONE',  ( 0.000000000000000000, 0.9875102702516498354, 0.1575546449569600882 ) ) ;
#39762 = AXIS2_PLACEMENT_3D ( 'NONE', #2615, #225499, #46871 ) ;
#39763 = FACE_OUTER_BOUND ( 'NONE', #61953, .T. ) ;
#39764 = CARTESIAN_POINT ( 'NONE',  ( -18.50000000000000000, 9.150000000011157653, -54.65000000000000568 ) ) ;
#39766 = TOROIDAL_SURFACE ( 'NONE', #189590, 11.65000000000000036, 0.1000000000000000056 ) ;
#39765 = CARTESIAN_POINT ( 'NONE',  ( -21.05000000000000071, -1.162701749938009677, -8.000000000000000000 ) ) ;
#39767 = AXIS2_PLACEMENT_3D ( 'NONE', #79258, #177129, #77986 ) ;
#39768 = LINE ( 'NONE', #158433, #25966 ) ;
#39769 = DIRECTION ( 'NONE',  ( 1.000000000000000000, -0.000000000000000000, -0.000000000000000000 ) ) ;
#39770 = EDGE_CURVE ( 'NONE', #95048, #184932, #112908, .T. ) ;
#39771 = EDGE_CURVE ( 'NONE', #31018, #116760, #94677, .T. ) ;
#39772 = ORIENTED_EDGE ( 'NONE', *, *, #216275, .F. ) ;
#39773 = ORIENTED_EDGE ( 'NONE', *, *, #124362, .F. ) ;
#39774 = AXIS2_PLACEMENT_3D ( 'NONE', #113319, #14246, #252818 ) ;
#39775 = CARTESIAN_POINT ( 'NONE',  ( 21.05000000000000071, -2.576749817950531707, -189.6385361693310756 ) ) ;
#39776 = VECTOR ( 'NONE', #241111, 1000.000000000000000 ) ;
#39777 = DIRECTION ( 'NONE',  ( -1.000000000000000000, 0.000000000000000000, 0.000000000000000000 ) ) ;
#39778 = LINE ( 'NONE', #137544, #241282 ) ;
#39779 = DIRECTION ( 'NONE',  ( -1.000000000000000000, -2.952720810173289112E-16, 0.000000000000000000 ) ) ;
#39780 = EDGE_LOOP ( 'NONE', ( #254474, #162230, #22844, #28377 ) ) ;
#39781 = CIRCLE ( 'NONE', #168975, 0.1000000000000028644 ) ;
#39783 = TOROIDAL_SURFACE ( 'NONE', #97987, 4.149999999999999467, 0.1000000000000000056 ) ;
#39782 = CARTESIAN_POINT ( 'NONE',  ( -18.40000000000000213, 64.52683809665003878, -179.3490535513324176 ) ) ;
#39784 = DIRECTION ( 'NONE',  ( 0.000000000000000000, 0.06835365183351375939, -0.9976611540402997580 ) ) ;
#39785 = EDGE_CURVE ( 'NONE', #5557, #17415, #202674, .T. ) ;
#39786 = AXIS2_PLACEMENT_3D ( 'NONE', #54456, #88422, #49324 ) ;
#39787 = DIRECTION ( 'NONE',  ( 0.000000000000000000, 0.000000000000000000, 1.000000000000000000 ) ) ;
#39788 = EDGE_CURVE ( 'NONE', #4373, #185096, #115528, .T. ) ;
#39789 = CARTESIAN_POINT ( 'NONE',  ( 18.49999999999998934, 28.86532135423329493, -237.9457867389574517 ) ) ;
#39791 = VECTOR ( 'NONE', #119683, 1000.000000000000000 ) ;
#39790 = CARTESIAN_POINT ( 'NONE',  ( 21.05000000000000071, 1.115650877919449575E-11, -129.9000000000000341 ) ) ;
#39792 = VERTEX_POINT ( 'NONE', #102255 ) ;
#39793 = EDGE_LOOP ( 'NONE', ( #225587, #63086, #247735, #76844 ) ) ;
#39794 = LINE ( 'NONE', #98398, #32144 ) ;
#39795 = ORIENTED_EDGE ( 'NONE', *, *, #10929, .F. ) ;
#39796 = CARTESIAN_POINT ( 'NONE',  ( -21.07954763557430056, 0.06587591862962487166, -27.17070900996239047 ) ) ;
#39797 = CARTESIAN_POINT ( 'NONE',  ( -23.25000000000000000, 76.00000000001237765, -170.0231074845243597 ) ) ;
#39798 = CARTESIAN_POINT ( 'NONE',  ( -21.05000000000000071, 77.83534155023599510, -57.96795619196132776 ) ) ;
#39799 = ORIENTED_EDGE ( 'NONE', *, *, #221673, .F. ) ;
#39800 = EDGE_CURVE ( 'NONE', #45677, #83250, #184392, .T. ) ;
#39801 = CARTESIAN_POINT ( 'NONE',  ( -20.54999999999999716, 47.45383559552796271, -242.5236527704543334 ) ) ;
#39802 = DIRECTION ( 'NONE',  ( -0.000000000000000000, 1.000000000000000000, -0.000000000000000000 ) ) ;
#39803 = ORIENTED_EDGE ( 'NONE', *, *, #15424, .F. ) ;
#39804 = LINE ( 'NONE', #124457, #145728 ) ;
#39806 = ORIENTED_EDGE ( 'NONE', *, *, #253484, .T. ) ;
#39805 = CARTESIAN_POINT ( 'NONE',  ( -21.65000000000000213, 66.05000000001187743, -90.27310748452438816 ) ) ;
#39807 = DIRECTION ( 'NONE',  ( 0.000000000000000000, 0.9654727137038715545, -0.2605042016806676242 ) ) ;
#39808 = CARTESIAN_POINT ( 'NONE',  ( -18.51555513499511463, 85.35265705451770657, -162.8279375888266998 ) ) ;
#39809 = ADVANCED_FACE ( 'NONE', ( #141417 ), #135312, .F. ) ;
#39810 = AXIS2_PLACEMENT_3D ( 'NONE', #202231, #11756, #112138 ) ;
#39811 = AXIS2_PLACEMENT_3D ( 'NONE', #133730, #178022, #38497 ) ;
#39812 = VERTEX_POINT ( 'NONE', #143977 ) ;
#39813 = DIRECTION ( 'NONE',  ( 0.000000000000000000, 7.026728003956683390E-15, -1.000000000000000000 ) ) ;
#39814 = DIRECTION ( 'NONE',  ( 0.000000000000000000, 1.000000000000000000, 7.272083257015735086E-15 ) ) ;
#39815 = DIRECTION ( 'NONE',  ( -1.000000000000000000, 0.000000000000000000, 0.000000000000000000 ) ) ;
#39816 = EDGE_LOOP ( 'NONE', ( #58151, #186485, #167571, #77373 ) ) ;
#39817 = CARTESIAN_POINT ( 'NONE',  ( -20.94999999999999929, 36.02918351690955490, -236.0543695120161374 ) ) ;
#39818 = EDGE_CURVE ( 'NONE', #224632, #142820, #136346, .T. ) ;
#39819 = CARTESIAN_POINT ( 'NONE',  ( 15.66039659514495774, 48.63331072832806967, -233.9296379114950923 ) ) ;
#39820 = CARTESIAN_POINT ( 'NONE',  ( 20.94999999999999929, 69.45000000001205365, -124.3731074845243540 ) ) ;
#39821 = ORIENTED_EDGE ( 'NONE', *, *, #257839, .F. ) ;
#39822 = ORIENTED_EDGE ( 'NONE', *, *, #20438, .T. ) ;
#39823 = VECTOR ( 'NONE', #117593, 1000.000000000000000 ) ;
#39824 = ORIENTED_EDGE ( 'NONE', *, *, #158554, .T. ) ;
#39825 = CIRCLE ( 'NONE', #81454, 0.09999999999999938105 ) ;
#39826 = ORIENTED_EDGE ( 'NONE', *, *, #167771, .T. ) ;
#39827 = CARTESIAN_POINT ( 'NONE',  ( -21.64999999999999858, 68.65000000001222702, -148.7731074845244166 ) ) ;
#39828 = CARTESIAN_POINT ( 'NONE',  ( -21.05000000000000071, 74.83729825007388570, -95.02310748452431710 ) ) ;
#39830 = VERTEX_POINT ( 'NONE', #181838 ) ;
#39829 = CARTESIAN_POINT ( 'NONE',  ( -20.94999999999999929, 67.70174932746996888, -211.7710791003628401 ) ) ;
#39831 = CARTESIAN_POINT ( 'NONE',  ( 18.39999999999999503, 11.75000000001113953, -113.1500000000000341 ) ) ;
#39832 = DIRECTION ( 'NONE',  ( 1.000000000000000000, 0.000000000000000000, 0.000000000000000000 ) ) ;
#39833 = CARTESIAN_POINT ( 'NONE',  ( 23.25000000000000000, -11.74999999998883560, -21.75000000000000355 ) ) ;
#39834 = CARTESIAN_POINT ( 'NONE',  ( -18.50000000000000000, -1.866714910046153308, -179.2526752462819672 ) ) ;
#39835 = CYLINDRICAL_SURFACE ( 'NONE', #246050, 0.09999999999999520384 ) ;
#39836 = CARTESIAN_POINT ( 'NONE',  ( 13.99999999999999822, 13.18880795147152618, -215.2702608532411830 ) ) ;
#39838 = ORIENTED_EDGE ( 'NONE', *, *, #8078, .F. ) ;
#39837 = DIRECTION ( 'NONE',  ( -1.000000000000000000, -0.000000000000000000, -0.000000000000000000 ) ) ;
#39840 = ORIENTED_EDGE ( 'NONE', *, *, #26496, .F. ) ;
#39839 = SPHERICAL_SURFACE ( 'NONE', #90189, 0.1000000000000000056 ) ;
#39841 = DIRECTION ( 'NONE',  ( 0.000000000000000000, 0.8660254037844352659, -0.5000000000000058842 ) ) ;
#39842 = ORIENTED_EDGE ( 'NONE', *, *, #224744, .F. ) ;
#39843 = VERTEX_POINT ( 'NONE', #235704 ) ;
#39844 = DIRECTION ( 'NONE',  ( 0.000000000000000000, 0.9126074666063768159, 0.4088369013363282178 ) ) ;
#39845 = DIRECTION ( 'NONE',  ( -0.000000000000000000, 0.2128009952263603677, -0.9770955615653313941 ) ) ;
#39846 = AXIS2_PLACEMENT_3D ( 'NONE', #65868, #84093, #64577 ) ;
#39847 = CIRCLE ( 'NONE', #35573, 4.000000000000003553 ) ;
#39848 = DIRECTION ( 'NONE',  ( -1.000000000000000000, 0.000000000000000000, -0.000000000000000000 ) ) ;
#39849 = DIRECTION ( 'NONE',  ( -1.073024830501117725E-15, -0.2617529984165031243, -0.9651348961777157509 ) ) ;
#39850 = CARTESIAN_POINT ( 'NONE',  ( 20.94999999999999929, 1.115600667400684642E-11, -134.0000000000000284 ) ) ;
#39851 = DIRECTION ( 'NONE',  ( -1.000000000000000000, 0.000000000000000000, 0.000000000000000000 ) ) ;
#39852 = CARTESIAN_POINT ( 'NONE',  ( 21.05000000000000071, 10.45765418377745881, -207.3040725013013912 ) ) ;
#39853 = EDGE_LOOP ( 'NONE', ( #27154, #87091, #246094, #41802, #210762 ) ) ;
#39854 = ORIENTED_EDGE ( 'NONE', *, *, #123221, .F. ) ;
#39855 = EDGE_CURVE ( 'NONE', #17165, #237745, #37530, .T. ) ;
#39856 = FACE_OUTER_BOUND ( 'NONE', #250590, .T. ) ;
#39857 = AXIS2_PLACEMENT_3D ( 'NONE', #48862, #168863, #226180 ) ;
#39858 = AXIS2_PLACEMENT_3D ( 'NONE', #249893, #150791, #71278 ) ;
#39859 = ORIENTED_EDGE ( 'NONE', *, *, #195676, .F. ) ;
#39860 = CARTESIAN_POINT ( 'NONE',  ( 20.94999999999999929, 7.467768556382911704, -241.6289316175765407 ) ) ;
#39861 = CARTESIAN_POINT ( 'NONE',  ( -16.87242674293849376, 51.61985789917108747, -231.9460232827009918 ) ) ;
#39862 = AXIS2_PLACEMENT_3D ( 'NONE', #217023, #21437, #61828 ) ;
#39863 = VECTOR ( 'NONE', #238730, 1000.000000000000000 ) ;
#39864 = CARTESIAN_POINT ( 'NONE',  ( -15.15766958671842701, 66.58946139148265786, -54.09041948738348538 ) ) ;
#39865 = FACE_BOUND ( 'NONE', #174938, .T. ) ;
#39866 =( GEOMETRIC_REPRESENTATION_CONTEXT ( 3 ) GLOBAL_UNCERTAINTY_ASSIGNED_CONTEXT ( ( #55782 ) ) GLOBAL_UNIT_ASSIGNED_CONTEXT ( ( #14008, #238161, #139034 ) ) REPRESENTATION_CONTEXT ( 'NONE', 'WORKASPACE' ) );
#39867 = ORIENTED_EDGE ( 'NONE', *, *, #138799, .T. ) ;
#39868 = DIRECTION ( 'NONE',  ( 0.000000000000000000, -0.9770955615653320603, -0.2128009952263585081 ) ) ;
#39869 = ORIENTED_EDGE ( 'NONE', *, *, #94, .F. ) ;
#39870 = CARTESIAN_POINT ( 'NONE',  ( -16.87036670365548474, 9.989418819312799513, -87.97956011730209980 ) ) ;
#39871 = ORIENTED_EDGE ( 'NONE', *, *, #36647, .T. ) ;
#39872 = ADVANCED_FACE ( 'NONE', ( #223510 ), #117056, .F. ) ;
#39873 = DIRECTION ( 'NONE',  ( 0.000000000000000000, -0.2617529984165152257, -0.9651348961777124202 ) ) ;
#39874 = CARTESIAN_POINT ( 'NONE',  ( -16.87036670365549895, 9.989418819312803066, -113.0204398826979855 ) ) ;
#39875 = VERTEX_POINT ( 'NONE', #24069 ) ;
#39876 = CARTESIAN_POINT ( 'NONE',  ( -18.59999999999999787, 7.021664781911246322, -70.83356540189728889 ) ) ;
#39878 = EDGE_LOOP ( 'NONE', ( #6813, #230069, #62584, #217769 ) ) ;
#39877 = LINE ( 'NONE', #21585, #26621 ) ;
#39879 = CARTESIAN_POINT ( 'NONE',  ( 23.24999999999999645, 68.82573846827003194, -239.4142956262433302 ) ) ;
#39881 = VERTEX_POINT ( 'NONE', #43614 ) ;
#39880 = TOROIDAL_SURFACE ( 'NONE', #185602, 0.2000000000000000111, 0.1000000000000000056 ) ;
#39882 =( BOUNDED_SURFACE ( )  B_SPLINE_SURFACE ( 3, 2, ( 
 ( #167299, #149014, #111151 ),
 ( #47296, #109849, #70772 ),
 ( #8214, #250643, #190718 ),
 ( #147714, #208962, #189410 ) ),
 .UNSPECIFIED., .F., .F., .T. ) 
 B_SPLINE_SURFACE_WITH_KNOTS ( ( 4, 4 ),
 ( 3, 3 ),
 ( 5.727910411845712702, 5.983100554402349225 ),
 ( 0.000000000000000000, 1.000000000000000000 ),
 .UNSPECIFIED. ) 
 GEOMETRIC_REPRESENTATION_ITEM ( )  RATIONAL_B_SPLINE_SURFACE ( (
 ( 1.000000000000000000, 0.8946697475932264831, 1.000000000000000000),
 ( 1.000000000000000000, 0.9035312726220648960, 1.000000000000000000),
 ( 1.000000000000000000, 0.9104333467450290707, 1.000000000000000000),
 ( 1.000000000000000000, 0.9152888060719445162, 1.000000000000000000) ) ) 
 REPRESENTATION_ITEM ( '' )  SURFACE ( )  );
#39883 = AXIS2_PLACEMENT_3D ( 'NONE', #12918, #92412, #110704 ) ;
#39884 = EDGE_CURVE ( 'NONE', #151518, #118038, #203013, .T. ) ;
#39885 = CARTESIAN_POINT ( 'NONE',  ( -18.59999999999999787, 85.40000000001258229, -196.2258477248610120 ) ) ;
#39886 = EDGE_CURVE ( 'NONE', #7281, #129441, #4468, .T. ) ;
#39887 = VERTEX_POINT ( 'NONE', #115766 ) ;
#39888 = CIRCLE ( 'NONE', #185613, 0.09999999999999939493 ) ;
#39889 = DIRECTION ( 'NONE',  ( 1.000000000000000000, 0.000000000000000000, -0.000000000000000000 ) ) ;
#39890 = CARTESIAN_POINT ( 'NONE',  ( 19.94784844284962233, 64.28691006698339550, -178.8209087672258022 ) ) ;
#39891 = DIRECTION ( 'NONE',  ( -0.000000000000000000, -1.000000000000000000, -0.000000000000000000 ) ) ;
#39892 = CARTESIAN_POINT ( 'NONE',  ( 22.39999999999999503, -2.479040261793999722, -189.6172560698084624 ) ) ;
#39893 = AXIS2_PLACEMENT_3D ( 'NONE', #196941, #18311, #97817 ) ;
#39894 = EDGE_CURVE ( 'NONE', #119497, #147150, #169058, .T. ) ;
#39895 = AXIS2_PLACEMENT_3D ( 'NONE', #30207, #191866, #75748 ) ;
#39896 = VECTOR ( 'NONE', #253181, 1000.000000000000000 ) ;
#39897 = DIRECTION ( 'NONE',  ( 1.000000000000000000, 0.000000000000000000, -0.000000000000000000 ) ) ;
#39898 = VERTEX_POINT ( 'NONE', #175763 ) ;
#39899 = DIRECTION ( 'NONE',  ( 0.000000000000000000, -0.6728971962616412394, -0.7397360091703134577 ) ) ;
#39900 = CARTESIAN_POINT ( 'NONE',  ( 18.59999999999999432, -1.299733671219632791, -23.52812952286940273 ) ) ;
#39901 = DIRECTION ( 'NONE',  ( 0.000000000000000000, 0.000000000000000000, -1.000000000000000000 ) ) ;
#39902 = ORIENTED_EDGE ( 'NONE', *, *, #149215, .T. ) ;
#39903 = CARTESIAN_POINT ( 'NONE',  ( 21.53752568617696639, 6.610297987518621632, -199.4590530230506999 ) ) ;
#39904 = ORIENTED_EDGE ( 'NONE', *, *, #93092, .T. ) ;
#39905 = DIRECTION ( 'NONE',  ( 1.000000000000000000, -1.207181226542539700E-16, 2.694675058168174199E-16 ) ) ;
#39906 = ORIENTED_EDGE ( 'NONE', *, *, #185296, .F. ) ;
#39907 = CIRCLE ( 'NONE', #139827, 0.1000000000000002554 ) ;
#39908 = EDGE_CURVE ( 'NONE', #237997, #20437, #182379, .T. ) ;
#39909 = AXIS2_PLACEMENT_3D ( 'NONE', #38148, #21167, #100633 ) ;
#39910 = DIRECTION ( 'NONE',  ( 0.000000000000000000, 0.2617529984164947421, 0.9651348961777179714 ) ) ;
#39911 = DIRECTION ( 'NONE',  ( 0.000000000000000000, -0.9915357197604982575, 0.1298341882519033486 ) ) ;
#39912 = ORIENTED_EDGE ( 'NONE', *, *, #221345, .F. ) ;
#39914 = EDGE_LOOP ( 'NONE', ( #22482, #836, #169903, #224214 ) ) ;
#39913 = CARTESIAN_POINT ( 'NONE',  ( -20.85000000000000142, -1.164121893241208960, -41.41484808557160591 ) ) ;
#39915 = LINE ( 'NONE', #99820, #171483 ) ;
#39916 = ORIENTED_EDGE ( 'NONE', *, *, #245097, .T. ) ;
#39917 = FACE_BOUND ( 'NONE', #249044, .T. ) ;
#39918 = LINE ( 'NONE', #176852, #6493 ) ;
#39920 = EDGE_CURVE ( 'NONE', #175899, #243017, #120037, .T. ) ;
#39919 = ORIENTED_EDGE ( 'NONE', *, *, #79651, .T. ) ;
#39921 = ORIENTED_EDGE ( 'NONE', *, *, #5548, .F. ) ;
#39922 = CYLINDRICAL_SURFACE ( 'NONE', #1696, 1.500000000000001332 ) ;
#39923 = CARTESIAN_POINT ( 'NONE',  ( 20.95083306685154056, 67.08315735812169578, -94.54578263126602167 ) ) ;
#39924 = ORIENTED_EDGE ( 'NONE', *, *, #246509, .T. ) ;
#39925 = DIRECTION ( 'NONE',  ( -0.000000000000000000, -0.1335171055202867274, 0.9910465087640865089 ) ) ;
#39926 = EDGE_LOOP ( 'NONE', ( #8068, #211227, #197109, #53360 ) ) ;
#39927 = ORIENTED_EDGE ( 'NONE', *, *, #144012, .T. ) ;
#39928 = DIRECTION ( 'NONE',  ( -1.000000000000000000, -0.000000000000000000, 0.000000000000000000 ) ) ;
#39929 =( BOUNDED_SURFACE ( )  B_SPLINE_SURFACE ( 3, 2, ( 
 ( #39852, #257525, #3246 ),
 ( #180628, #144043, #63224 ),
 ( #24136, #82761, #1962 ),
 ( #81481, #183200, #78920 ) ),
 .UNSPECIFIED., .F., .F., .F. ) 
 B_SPLINE_SURFACE_WITH_KNOTS ( ( 4, 4 ),
 ( 3, 3 ),
 ( 0.0002700421466196776762, 0.0004789321604330829441 ),
 ( 0.000000000000000000, 1.000000000000000000 ),
 .UNSPECIFIED. ) 
 GEOMETRIC_REPRESENTATION_ITEM ( )  RATIONAL_B_SPLINE_SURFACE ( (
 ( 1.000000000000000000, 0.7071067811864790720, 1.000000000000000000),
 ( 1.000000000000000000, 0.7163411249512339207, 1.000000000000000000),
 ( 1.000000000000000000, 0.7221957104841457697, 1.000000000000000000),
 ( 1.000000000000000000, 0.7250110520819958992, 1.000000000000000000) ) ) 
 REPRESENTATION_ITEM ( '' )  SURFACE ( )  );
#39931 = ORIENTED_EDGE ( 'NONE', *, *, #466, .T. ) ;
#39930 = CARTESIAN_POINT ( 'NONE',  ( -20.54999999999999716, 2.500000000011156409, -113.7246219227621395 ) ) ;
#39932 = CIRCLE ( 'NONE', #223070, 0.1000000000000028644 ) ;
#39933 = PLANE ( 'NONE',  #29014 ) ;
#39934 = CARTESIAN_POINT ( 'NONE',  ( -23.15000000000000213, 74.00000000001223555, -149.7477294072864709 ) ) ;
#39935 = CARTESIAN_POINT ( 'NONE',  ( -18.50000000000000000, 7.021664781911246322, -204.6335654018972434 ) ) ;
#39937 = DIRECTION ( 'NONE',  ( -1.000000000000000000, 0.000000000000000000, 0.000000000000000000 ) ) ;
#39936 = CARTESIAN_POINT ( 'NONE',  ( -21.14999999999999858, 1.580567032079710055, -244.0902705724231794 ) ) ;
#39939 = AXIS2_PLACEMENT_3D ( 'NONE', #135505, #33911, #113398 ) ;
#39938 = DIRECTION ( 'NONE',  ( 0.8049926720990051576, 0.5932847527679298016, -0.000000000000000000 ) ) ;
#39940 = AXIS2_PLACEMENT_3D ( 'NONE', #93391, #15157, #58098 ) ;
#39941 = CARTESIAN_POINT ( 'NONE',  ( 20.85000000000000142, 36.65892442174935439, -249.5511627012433848 ) ) ;
#39942 = CARTESIAN_POINT ( 'NONE',  ( 20.85000000000000142, 77.36242903720540198, -128.6342262366031548 ) ) ;
#39943 = DIRECTION ( 'NONE',  ( -0.000000000000000000, 0.9770955615653313941, 0.2128009952263603954 ) ) ;
#39945 = ORIENTED_EDGE ( 'NONE', *, *, #237608, .F. ) ;
#39944 = CIRCLE ( 'NONE', #89983, 0.1000000000000028644 ) ;
#39946 = EDGE_CURVE ( 'NONE', #104599, #157387, #57445, .T. ) ;
#39947 = EDGE_CURVE ( 'NONE', #39515, #125649, #210404, .T. ) ;
#39949 = ORIENTED_EDGE ( 'NONE', *, *, #204395, .T. ) ;
#39948 = FACE_OUTER_BOUND ( 'NONE', #213682, .T. ) ;
#39950 = EDGE_LOOP ( 'NONE', ( #57841, #41766, #159056, #125239 ) ) ;
#39951 = CARTESIAN_POINT ( 'NONE',  ( -20.85000000000000142, 43.08613539620618837, -254.3146655184800409 ) ) ;
#39952 = ORIENTED_EDGE ( 'NONE', *, *, #203819, .F. ) ;
#39953 = CARTESIAN_POINT ( 'NONE',  ( -23.15000000000000213, 0.000000000000000000, 0.000000000000000000 ) ) ;
#39954 = EDGE_CURVE ( 'NONE', #145261, #28934, #86646, .T. ) ;
#39955 = EDGE_CURVE ( 'NONE', #164361, #27007, #115731, .T. ) ;
#39956 = AXIS2_PLACEMENT_3D ( 'NONE', #168970, #148081, #188481 ) ;
#39957 = VERTEX_POINT ( 'NONE', #29228 ) ;
#39958 = VECTOR ( 'NONE', #48682, 1000.000000000000000 ) ;
#39959 = ADVANCED_FACE ( 'NONE', ( #10917 ), #94871, .T. ) ;
#39960 = LINE ( 'NONE', #199003, #103175 ) ;
#39961 = ADVANCED_FACE ( 'NONE', ( #224796 ), #111296, .T. ) ;
#39963 = ORIENTED_EDGE ( 'NONE', *, *, #221267, .T. ) ;
#39962 = EDGE_LOOP ( 'NONE', ( #14636, #226550, #17108, #149156 ) ) ;
#39964 = VERTEX_POINT ( 'NONE', #246932 ) ;
#39966 = EDGE_CURVE ( 'NONE', #183080, #197777, #69609, .T. ) ;
#39965 = EDGE_CURVE ( 'NONE', #75205, #89756, #146535, .T. ) ;
#39967 = ORIENTED_EDGE ( 'NONE', *, *, #201895, .F. ) ;
#39968 = DIRECTION ( 'NONE',  ( 0.000000000000000000, 0.000000000000000000, -1.000000000000000000 ) ) ;
#39969 = CARTESIAN_POINT ( 'NONE',  ( -20.94999999999999929, -1.135018845899022466, -208.7169768834322952 ) ) ;
#39971 = ORIENTED_EDGE ( 'NONE', *, *, #120981, .T. ) ;
#39970 = CARTESIAN_POINT ( 'NONE',  ( -21.05000000000000071, 1.115600667400684642E-11, -37.79999999999996163 ) ) ;
#39972 = CIRCLE ( 'NONE', #185704, 0.1000000000000028644 ) ;
#39973 = CARTESIAN_POINT ( 'NONE',  ( -18.59999999999999787, 64.35000000001254250, -182.1731074845244507 ) ) ;
#39974 = CARTESIAN_POINT ( 'NONE',  ( -20.64999999999999858, 85.00000000001232081, -160.1291383618718385 ) ) ;
#39976 = VERTEX_POINT ( 'NONE', #27932 ) ;
#39975 = CARTESIAN_POINT ( 'NONE',  ( -21.05000000000000071, 67.23127455305841238, -235.8551265064783991 ) ) ;
#39977 = CARTESIAN_POINT ( 'NONE',  ( 19.94784844284930969, 11.71308993304057999, -125.2021987172991260 ) ) ;
#39978 = VERTEX_POINT ( 'NONE', #87843 ) ;
#39979 = CARTESIAN_POINT ( 'NONE',  ( 23.40000000000005187, 76.00000000001119815, -36.02310748452479316 ) ) ;
#39981 = ORIENTED_EDGE ( 'NONE', *, *, #142924, .T. ) ;
#39980 = DIRECTION ( 'NONE',  ( 0.000000000000000000, 0.000000000000000000, 1.000000000000000000 ) ) ;
#39982 = FACE_OUTER_BOUND ( 'NONE', #149172, .T. ) ;
#39984 = ADVANCED_FACE ( 'NONE', ( #125707 ), #226064, .F. ) ;
#39983 = CARTESIAN_POINT ( 'NONE',  ( -16.92778301347269121, 10.00094491684630960, -113.0714818920312723 ) ) ;
#39985 = FACE_OUTER_BOUND ( 'NONE', #187477, .T. ) ;
#39986 = ORIENTED_EDGE ( 'NONE', *, *, #174044, .T. ) ;
#39988 = LINE ( 'NONE', #257651, #237342 ) ;
#39987 = CARTESIAN_POINT ( 'NONE',  ( -16.82055514392384765, 9.950000000011135270, -46.17679807454214114 ) ) ;
#39989 = CARTESIAN_POINT ( 'NONE',  ( -13.77083647240106501, 66.54258906972165732, -84.52319157577809960 ) ) ;
#39990 = ADVANCED_FACE ( 'NONE', ( #207851 ), #209099, .F. ) ;
#39991 = EDGE_CURVE ( 'NONE', #51884, #241599, #253081, .T. ) ;
#39992 = CARTESIAN_POINT ( 'NONE',  ( 18.43466021071417060, 85.49419069046894037, -163.4060459243964374 ) ) ;
#39993 = AXIS2_PLACEMENT_3D ( 'NONE', #129786, #188475, #226298 ) ;
#39994 = DIRECTION ( 'NONE',  ( 0.000000000000000000, 0.4999999999999088507, -0.8660254037844913322 ) ) ;
#39995 = VECTOR ( 'NONE', #252097, 1000.000000000000114 ) ;
#39997 = CARTESIAN_POINT ( 'NONE',  ( -16.94445028196808778, 44.07934375239701552, -235.2779890399608576 ) ) ;
#39996 = CIRCLE ( 'NONE', #19109, 0.1000000000000008937 ) ;
#39998 = EDGE_LOOP ( 'NONE', ( #117638, #221740, #100877, #223236 ) ) ;
#39999 = ORIENTED_EDGE ( 'NONE', *, *, #190365, .T. ) ;
#40000 = ORIENTED_EDGE ( 'NONE', *, *, #248933, .T. ) ;
#40001 = EDGE_CURVE ( 'NONE', #136488, #155989, #149150, .T. ) ;
#40002 = DIRECTION ( 'NONE',  ( 0.000000000000000000, 0.000000000000000000, -1.000000000000000000 ) ) ;
#40003 = ORIENTED_EDGE ( 'NONE', *, *, #110922, .T. ) ;
#40004 = DIRECTION ( 'NONE',  ( 1.000000000000000000, 0.000000000000000000, 0.000000000000000000 ) ) ;
#40005 = ORIENTED_EDGE ( 'NONE', *, *, #241089, .F. ) ;
#40006 = CARTESIAN_POINT ( 'NONE',  ( -21.64999999999999858, 44.92467540951147953, -237.7943620901849613 ) ) ;
#40007 = DIRECTION ( 'NONE',  ( -1.000000000000000000, -0.000000000000000000, -0.000000000000000000 ) ) ;
#40008 = EDGE_CURVE ( 'NONE', #58504, #211306, #46167, .T. ) ;
#40009 = ADVANCED_FACE ( 'NONE', ( #7043 ), #86554, .F. ) ;
#40010 = ORIENTED_EDGE ( 'NONE', *, *, #125412, .F. ) ;
#40011 = AXIS2_PLACEMENT_3D ( 'NONE', #53482, #168339, #233422 ) ;
#40012 = DIRECTION ( 'NONE',  ( 1.000000000000000000, 0.000000000000000000, 0.000000000000000000 ) ) ;
#40013 =( NAMED_UNIT ( * ) PLANE_ANGLE_UNIT ( ) SI_UNIT ( $, .RADIAN. ) );
#40014 = CIRCLE ( 'NONE', #135826, 0.1000000000000028644 ) ;
#40015 = ORIENTED_EDGE ( 'NONE', *, *, #222490, .F. ) ;
#40016 = ORIENTED_EDGE ( 'NONE', *, *, #141502, .F. ) ;
#40017 = ORIENTED_EDGE ( 'NONE', *, *, #223409, .F. ) ;
#40018 = DIRECTION ( 'NONE',  ( 0.000000000000000000, -1.000000000000000000, 0.000000000000000000 ) ) ;
#40019 = DIRECTION ( 'NONE',  ( 1.000000000000000000, -0.000000000000000000, -0.000000000000000000 ) ) ;
#40020 = AXIS2_PLACEMENT_3D ( 'NONE', #75080, #55445, #129869 ) ;
#40021 = DIRECTION ( 'NONE',  ( -3.469446951953772592E-14, 0.9651348961777379554, -0.2617529984164210233 ) ) ;
#40022 = CARTESIAN_POINT ( 'NONE',  ( 23.14999999999999503, 20.97908333644147660, -233.6079013178409411 ) ) ;
#40023 = DIRECTION ( 'NONE',  ( 0.000000000000000000, -0.9160831752668552319, -0.4009882990724247809 ) ) ;
#40025 = CARTESIAN_POINT ( 'NONE',  ( 23.24999999999999645, 70.40000000001261071, -191.1178414656113205 ) ) ;
#40024 = CARTESIAN_POINT ( 'NONE',  ( -18.79999999999999716, 11.49641995933507843, 1.885425182446133885 ) ) ;
#40026 = CARTESIAN_POINT ( 'NONE',  ( -21.05000000000000071, 68.48451787451661232, -224.2224406095231757 ) ) ;
#40028 = ORIENTED_EDGE ( 'NONE', *, *, #225541, .F. ) ;
#40027 = DIRECTION ( 'NONE',  ( 0.000000000000000000, 0.1332476588733589318, -0.9910827722268049644 ) ) ;
#40029 = CARTESIAN_POINT ( 'NONE',  ( 18.59999999999999076, 54.57427006634497957, -228.7596887170734306 ) ) ;
#40030 = ORIENTED_EDGE ( 'NONE', *, *, #130920, .T. ) ;
#40031 = ORIENTED_EDGE ( 'NONE', *, *, #152151, .T. ) ;
#40032 = ORIENTED_EDGE ( 'NONE', *, *, #56466, .T. ) ;
#40033 = LINE ( 'NONE', #178256, #192167 ) ;
#40034 = DIRECTION ( 'NONE',  ( 0.000000000000000000, 0.000000000000000000, -1.000000000000000000 ) ) ;
#40035 = CARTESIAN_POINT ( 'NONE',  ( 20.04142135623730070, 11.65000000000000391, -21.25000000000000000 ) ) ;
#40036 = ORIENTED_EDGE ( 'NONE', *, *, #139850, .F. ) ;
#40037 = AXIS2_PLACEMENT_3D ( 'NONE', #228507, #231088, #232369 ) ;
#40038 = CARTESIAN_POINT ( 'NONE',  ( -23.15000000000000213, 30.73962027982165779, -265.0781340245722504 ) ) ;
#40039 = ORIENTED_EDGE ( 'NONE', *, *, #134276, .F. ) ;
#40040 = ORIENTED_EDGE ( 'NONE', *, *, #196112, .T. ) ;
#40041 = CARTESIAN_POINT ( 'NONE',  ( -18.59999999999999787, 77.16412189325330928, -128.6082593989527254 ) ) ;
#40042 = VERTEX_POINT ( 'NONE', #35641 ) ;
#40043 = FACE_OUTER_BOUND ( 'NONE', #53070, .T. ) ;
#40044 = CARTESIAN_POINT ( 'NONE',  ( -18.59999999999999787, 57.82359945636609666, -226.0354702357591350 ) ) ;
#40045 = VERTEX_POINT ( 'NONE', #252077 ) ;
#40046 = CARTESIAN_POINT ( 'NONE',  ( 21.05000000000000071, 9.374458193048763377, -220.5475659691911119 ) ) ;
#40047 = CARTESIAN_POINT ( 'NONE',  ( 21.05000000000000071, 45.58907629467868361, -240.2765730862633404 ) ) ;
#40048 = CARTESIAN_POINT ( 'NONE',  ( -23.15000000000000213, 1.115600667400684642E-11, -104.5500000000000256 ) ) ;
#40049 = EDGE_LOOP ( 'NONE', ( #114709, #192207, #40723, #256982 ) ) ;
#40050 = CARTESIAN_POINT ( 'NONE',  ( -20.94999999999999929, 44.34387878855809362, -247.3824414791181994 ) ) ;
#40051 = EDGE_CURVE ( 'NONE', #147767, #3546, #228160, .T. ) ;
#40052 = LINE ( 'NONE', #99962, #16698 ) ;
#40053 = AXIS2_PLACEMENT_3D ( 'NONE', #132468, #149485, #33403 ) ;
#40054 = DIRECTION ( 'NONE',  ( 0.000000000000000000, -0.09425075112712516523, -0.9955484899852807823 ) ) ;
#40055 = EDGE_CURVE ( 'NONE', #221470, #14167, #49075, .T. ) ;
#40056 = VECTOR ( 'NONE', #147929, 1000.000000000000114 ) ;
#40057 = CIRCLE ( 'NONE', #114856, 0.5000000000000004441 ) ;
#40058 = AXIS2_PLACEMENT_3D ( 'NONE', #218838, #255356, #19378 ) ;
#40059 = VERTEX_POINT ( 'NONE', #33085 ) ;
#40060 = EDGE_CURVE ( 'NONE', #253940, #38262, #244897, .T. ) ;
#40062 = ORIENTED_EDGE ( 'NONE', *, *, #157953, .T. ) ;
#40061 = DIRECTION ( 'NONE',  ( 0.000000000000000000, 0.000000000000000000, -1.000000000000000000 ) ) ;
#40063 = ADVANCED_FACE ( 'NONE', ( #73479 ), #90758, .T. ) ;
#40064 = EDGE_LOOP ( 'NONE', ( #194397, #61448, #238085, #153307 ) ) ;
#40065 = CARTESIAN_POINT ( 'NONE',  ( 20.12500000000000000, 18.88320179786139619, -228.9684431863134932 ) ) ;
#40066 = CARTESIAN_POINT ( 'NONE',  ( -22.50000000000000000, 12.55148283907650608, -223.4215551264213104 ) ) ;
#40067 = FACE_OUTER_BOUND ( 'NONE', #112593, .T. ) ;
#40068 = LINE ( 'NONE', #158730, #221448 ) ;
#40069 = DIRECTION ( 'NONE',  ( 0.000000000000000000, -0.9229812358756199764, 0.3848449534832346086 ) ) ;
#40070 = ORIENTED_EDGE ( 'NONE', *, *, #49437, .T. ) ;
#40071 = DIRECTION ( 'NONE',  ( 1.000000000000000000, 0.000000000000000000, 0.000000000000000000 ) ) ;
#40072 = CARTESIAN_POINT ( 'NONE',  ( 20.04142135623730070, 64.35000000001150511, -48.17310748452440095 ) ) ;
#40073 = CARTESIAN_POINT ( 'NONE',  ( -18.44232395689850534, 77.38089040410972075, -241.7752457915469506 ) ) ;
#40074 = AXIS2_PLACEMENT_3D ( 'NONE', #197484, #138765, #98347 ) ;
#40075 = DIRECTION ( 'NONE',  ( -0.000000000000000000, 0.01283462868039629209, -0.9999176327611372095 ) ) ;
#40076 = EDGE_CURVE ( 'NONE', #187747, #165490, #215659, .T. ) ;
#40078 = EDGE_CURVE ( 'NONE', #171414, #83713, #3268, .T. ) ;
#40077 = AXIS2_PLACEMENT_3D ( 'NONE', #225176, #106511, #186081 ) ;
#40079 = EDGE_LOOP ( 'NONE', ( #138867, #80124, #234792, #120152 ) ) ;
#40080 = ORIENTED_EDGE ( 'NONE', *, *, #18115, .T. ) ;
#40081 = DIRECTION ( 'NONE',  ( 1.000000000000000000, 0.000000000000000000, 0.000000000000000000 ) ) ;
#40082 = DIRECTION ( 'NONE',  ( -1.000000000000000000, 0.000000000000000000, 0.000000000000000000 ) ) ;
#40083 = CARTESIAN_POINT ( 'NONE',  ( 21.05000000000000071, 10.72371710471867701, -179.6499999999999773 ) ) ;
#40084 = CARTESIAN_POINT ( 'NONE',  ( 21.05000000000000426, 58.98862984610919824, -225.8934610823798437 ) ) ;
#40085 = CARTESIAN_POINT ( 'NONE',  ( 21.05000000000000071, 17.15380675273574695, -224.5473919504296703 ) ) ;
#40086 = TOROIDAL_SURFACE ( 'NONE', #144071, 11.70000000000000107, 0.1000000000000000056 ) ;
#40087 = ORIENTED_EDGE ( 'NONE', *, *, #119145, .F. ) ;
#40088 = VECTOR ( 'NONE', #3558, 1000.000000000000000 ) ;
#40089 = CIRCLE ( 'NONE', #210739, 0.5000000000000004441 ) ;
#40090 = LINE ( 'NONE', #180860, #163421 ) ;
#40091 = DIRECTION ( 'NONE',  ( 1.000000000000000000, 0.000000000000000000, 0.000000000000000000 ) ) ;
#40092 = ADVANCED_FACE ( 'NONE', ( #235097 ), #80657, .T. ) ;
#40093 = FACE_OUTER_BOUND ( 'NONE', #185412, .T. ) ;
#40094 = EDGE_CURVE ( 'NONE', #128109, #129320, #214246, .T. ) ;
#40095 = AXIS2_PLACEMENT_3D ( 'NONE', #76454, #156027, #97267 ) ;
#40096 = AXIS2_PLACEMENT_3D ( 'NONE', #116631, #38383, #218274 ) ;
#40097 = ORIENTED_EDGE ( 'NONE', *, *, #248130, .T. ) ;
#40099 = CARTESIAN_POINT ( 'NONE',  ( -20.95000000000000284, 12.93677228415563896, -205.1844859741924836 ) ) ;
#40098 = AXIS2_PLACEMENT_3D ( 'NONE', #202980, #66038, #225091 ) ;
#40100 = ORIENTED_EDGE ( 'NONE', *, *, #109616, .F. ) ;
#40101 = CARTESIAN_POINT ( 'NONE',  ( 20.94999999999999574, 77.83534155023646406, -124.9679561919612922 ) ) ;
#40102 = DIRECTION ( 'NONE',  ( 3.265361837132813093E-16, 1.000000000000000000, 6.982962677686266711E-15 ) ) ;
#40103 = TOROIDAL_SURFACE ( 'NONE', #131651, 7.800000000000000711, 0.1000000000000000056 ) ;
#40104 = ADVANCED_FACE ( 'NONE', ( #36926 ), #140666, .F. ) ;
#40105 = LINE ( 'NONE', #43918, #53051 ) ;
#40106 = DIRECTION ( 'NONE',  ( 1.836970198721029934E-16, -0.9770955615653316162, -0.2128009952263604232 ) ) ;
#40107 = CARTESIAN_POINT ( 'NONE',  ( 21.05000000000000071, 67.12338541492522381, -161.6380270056797599 ) ) ;
#40108 = DIRECTION ( 'NONE',  ( -1.000000000000000000, -0.000000000000000000, -0.000000000000000000 ) ) ;
#40109 = DIRECTION ( 'NONE',  ( 1.000000000000000000, 0.000000000000000000, 0.000000000000000000 ) ) ;
#40110 = EDGE_CURVE ( 'NONE', #236598, #411, #32557, .T. ) ;
#40112 = CARTESIAN_POINT ( 'NONE',  ( -18.40000000000000213, 15.66855642289968031, -219.0286517433665381 ) ) ;
#40111 = B_SPLINE_CURVE_WITH_KNOTS ( 'NONE', 3,
 ( #186343, #204596, #5086, #45536, #88483, #166802, #49391, #29852, #106779, #168098, #224160, #247586, #85911, #68972, #225432, #25982, #185042, #148494, #6401, #7706, #165497, #108086 ),
 .UNSPECIFIED., .F., .F.,
 ( 4, 3, 3, 3, 3, 3, 3, 4 ),
 ( 0.000000000000000000, 7.307836821075696998E-06, 4.161455748547338501E-05, 7.576591810648398973E-05, 0.0001098090429817408253, 0.0001438003617351054644, 0.0001777914035423563022, 0.0002117966137402873411 ),
 .UNSPECIFIED. ) ;
#40113 = CYLINDRICAL_SURFACE ( 'NONE', #96393, 0.1000000000000028644 ) ;
#40114 = CARTESIAN_POINT ( 'NONE',  ( 21.05000000000005400, 66.15000000001120384, -4.523107484524794053 ) ) ;
#40115 = AXIS2_PLACEMENT_3D ( 'NONE', #58796, #112391, #236173 ) ;
#40116 = DIRECTION ( 'NONE',  ( -0.000000000000000000, -0.1298341882520022694, -0.9915357197604853789 ) ) ;
#40117 = ADVANCED_FACE ( 'NONE', ( #99403 ), #40773, .T. ) ;
#40118 = DIRECTION ( 'NONE',  ( -0.000000000000000000, 1.000000000000000000, -0.000000000000000000 ) ) ;
#40119 = CARTESIAN_POINT ( 'NONE',  ( 20.85000000106584750, 56.18110340670159530, -227.9302710413118689 ) ) ;
#40120 = EDGE_LOOP ( 'NONE', ( #153878, #142177, #50541, #162915 ) ) ;
#40121 = DIRECTION ( 'NONE',  ( 0.000000000000000000, -8.881784197001840025E-16, -1.000000000000000000 ) ) ;
#40122 = LINE ( 'NONE', #199164, #12842 ) ;
#40123 = CARTESIAN_POINT ( 'NONE',  ( 20.30466543256828160, 9.304236939266303352, -41.75366265139219024 ) ) ;
#40124 = EDGE_CURVE ( 'NONE', #101872, #177565, #53363, .T. ) ;
#40125 = VERTEX_POINT ( 'NONE', #257160 ) ;
#40126 = DIRECTION ( 'NONE',  ( 0.000000000000000000, 0.2617529984165024026, 0.9651348961777158619 ) ) ;
#40127 = AXIS2_PLACEMENT_3D ( 'NONE', #29922, #74199, #12931 ) ;
#40128 = VECTOR ( 'NONE', #192534, 1000.000000000000000 ) ;
#40129 = EDGE_CURVE ( 'NONE', #64183, #3872, #232455, .T. ) ;
#40130 = ORIENTED_EDGE ( 'NONE', *, *, #23536, .F. ) ;
#40131 = AXIS2_PLACEMENT_3D ( 'NONE', #12731, #32293, #114371 ) ;
#40132 = DIRECTION ( 'NONE',  ( 0.000000000000000000, 1.000000000000000000, 0.000000000000000000 ) ) ;
#40133 = AXIS2_PLACEMENT_3D ( 'NONE', #29310, #248316, #5829 ) ;
#40134 = ORIENTED_EDGE ( 'NONE', *, *, #198580, .F. ) ;
#40135 = CIRCLE ( 'NONE', #27680, 0.09999999999998464284 ) ;
#40136 = ORIENTED_EDGE ( 'NONE', *, *, #74252, .F. ) ;
#40137 = SPHERICAL_SURFACE ( 'NONE', #73054, 0.1000000000000000056 ) ;
#40138 = VERTEX_POINT ( 'NONE', #64158 ) ;
#40140 = AXIS2_PLACEMENT_3D ( 'NONE', #192308, #214418, #13663 ) ;
#40139 = FACE_OUTER_BOUND ( 'NONE', #66694, .T. ) ;
#40141 = DIRECTION ( 'NONE',  ( -1.000000000000000000, -0.000000000000000000, -0.000000000000000000 ) ) ;
#40143 = CARTESIAN_POINT ( 'NONE',  ( -21.00000000000000000, -11.65000000000000036, 0.000000000000000000 ) ) ;
#40142 = PRODUCT_DEFINITION_CONTEXT ( 'detailed design', #232514, 'design' ) ;
#40144 = DIRECTION ( 'NONE',  ( -0.000000000000000000, -0.000000000000000000, -1.000000000000000000 ) ) ;
#40145 = CIRCLE ( 'NONE', #160939, 2.099999999999990763 ) ;
#40146 = CARTESIAN_POINT ( 'NONE',  ( 20.94999999999999574, 6.350000000011161383, -143.8438220896831581 ) ) ;
#40147 = CARTESIAN_POINT ( 'NONE',  ( 21.07928932188134397, 69.67148334361938566, -203.6220026301787982 ) ) ;
#40148 = CIRCLE ( 'NONE', #169345, 0.09999999999999939493 ) ;
#40149 = FACE_OUTER_BOUND ( 'NONE', #68552, .T. ) ;
#40150 = CARTESIAN_POINT ( 'NONE',  ( -17.71734398241073905, 65.15764277154723061, -79.79796923151879184 ) ) ;
#40151 = ORIENTED_EDGE ( 'NONE', *, *, #218569, .F. ) ;
#40152 = ORIENTED_EDGE ( 'NONE', *, *, #153434, .T. ) ;
#40154 = CARTESIAN_POINT ( 'NONE',  ( -20.07928932188135107, 63.89429612639829514, -212.9324612951732831 ) ) ;
#40153 = CARTESIAN_POINT ( 'NONE',  ( 18.43709777086140988, 37.95493834378066822, -261.2294694241335264 ) ) ;
#40157 = VERTEX_POINT ( 'NONE', #201094 ) ;
#40156 = CARTESIAN_POINT ( 'NONE',  ( -16.92280123533700120, 60.99187387584997566, -220.8480904879614855 ) ) ;
#40155 = FACE_OUTER_BOUND ( 'NONE', #117662, .T. ) ;
#40158 = ORIENTED_EDGE ( 'NONE', *, *, #146497, .T. ) ;
#40159 = FACE_BOUND ( 'NONE', #180530, .T. ) ;
#40160 = DIRECTION ( 'NONE',  ( 0.000000000000000000, 0.4721928772776973204, 0.8814952561688629284 ) ) ;
#40161 = DIRECTION ( 'NONE',  ( -1.000000000000000000, 0.000000000000000000, 0.000000000000000000 ) ) ;
#40163 = DIRECTION ( 'NONE',  ( 0.000000000000000000, 0.2617529984165031243, 0.9651348961777157509 ) ) ;
#40162 = AXIS2_PLACEMENT_3D ( 'NONE', #71353, #150866, #99846 ) ;
#40164 = CARTESIAN_POINT ( 'NONE',  ( -20.94999999999999929, 87.48912529308822172, -139.6231074845242688 ) ) ;
#40165 = PLANE ( 'NONE',  #44674 ) ;
#40166 = FACE_OUTER_BOUND ( 'NONE', #12324, .T. ) ;
#40167 = ORIENTED_EDGE ( 'NONE', *, *, #233329, .F. ) ;
#40168 = VERTEX_POINT ( 'NONE', #23777 ) ;
#40169 = FACE_BOUND ( 'NONE', #88632, .T. ) ;
#40170 = AXIS2_PLACEMENT_3D ( 'NONE', #223435, #158380, #39708 ) ;
#40171 = AXIS2_PLACEMENT_3D ( 'NONE', #12420, #208049, #248445 ) ;
#40172 = ORIENTED_EDGE ( 'NONE', *, *, #183614, .F. ) ;
#40173 = CIRCLE ( 'NONE', #119265, 12.87499999999999822 ) ;
#40175 = DIRECTION ( 'NONE',  ( 0.000000000000000000, -0.9770955615653201809, -0.2128009952264121873 ) ) ;
#40174 = CIRCLE ( 'NONE', #190191, 0.5000000000000031086 ) ;
#40176 = ORIENTED_EDGE ( 'NONE', *, *, #157575, .T. ) ;
#40177 = CARTESIAN_POINT ( 'NONE',  ( -22.48660254037843487, 64.35000000001214460, -136.5731074845243711 ) ) ;
#40178 = CARTESIAN_POINT ( 'NONE',  ( -12.60829076262180237, 49.08016403251640725, -233.6979168753148599 ) ) ;
#40179 = CARTESIAN_POINT ( 'NONE',  ( 20.90000000000000213, 0.000000000000000000, 0.000000000000000000 ) ) ;
#40180 = ADVANCED_FACE ( 'NONE', ( #122856 ), #61587, .F. ) ;
#40181 = CARTESIAN_POINT ( 'NONE',  ( -20.15000000000000568, 30.15980099226561606, -235.5292368182743132 ) ) ;
#40182 = EDGE_LOOP ( 'NONE', ( #257637, #88340, #208008, #9748 ) ) ;
#40183 = DIRECTION ( 'NONE',  ( -1.000000000000000000, 0.000000000000000000, 0.000000000000000000 ) ) ;
#40184 = ADVANCED_FACE ( 'NONE', ( #39492 ), #139823, .F. ) ;
#40185 = CYLINDRICAL_SURFACE ( 'NONE', #155059, 0.1000000000000028644 ) ;
#40186 = EDGE_CURVE ( 'NONE', #205489, #241008, #136554, .T. ) ;
#40187 = CARTESIAN_POINT ( 'NONE',  ( -21.07016717457009136, 30.89038661691667542, -252.1353965670249693 ) ) ;
#40188 = CARTESIAN_POINT ( 'NONE',  ( 18.59999999999999076, 8.433899723187009201, -209.4150263691077782 ) ) ;
#40189 = VECTOR ( 'NONE', #150661, 1000.000000000000000 ) ;
#40190 = FACE_OUTER_BOUND ( 'NONE', #88620, .T. ) ;
#40191 = EDGE_LOOP ( 'NONE', ( #165727, #46376, #194117, #13958 ) ) ;
#40192 = AXIS2_PLACEMENT_3D ( 'NONE', #70500, #30082, #109573 ) ;
#40194 = CARTESIAN_POINT ( 'NONE',  ( -21.05000000000000071, 67.23127455305835554, -235.8551265064784559 ) ) ;
#40193 = AXIS2_PLACEMENT_3D ( 'NONE', #171057, #225811, #32822 ) ;
#40195 = EDGE_LOOP ( 'NONE', ( #132909, #81155, #98304, #2034 ) ) ;
#40198 = VERTEX_POINT ( 'NONE', #18610 ) ;
#40197 = CYLINDRICAL_SURFACE ( 'NONE', #101186, 0.09999999999999854838 ) ;
#40196 = CARTESIAN_POINT ( 'NONE',  ( -22.48660254037843131, 64.25000000001267608, -203.5731074845243995 ) ) ;
#40199 = DIRECTION ( 'NONE',  ( 1.000000000000000000, 0.000000000000000000, 0.000000000000000000 ) ) ;
#40200 = LINE ( 'NONE', #155012, #21138 ) ;
#40201 = AXIS2_PLACEMENT_3D ( 'NONE', #105498, #169405, #207220 ) ;
#40202 = ORIENTED_EDGE ( 'NONE', *, *, #50756, .F. ) ;
#40203 = CARTESIAN_POINT ( 'NONE',  ( 18.54271179734072561, 85.62408429011051680, -129.7821426318235183 ) ) ;
#40204 = EDGE_CURVE ( 'NONE', #95961, #192664, #169939, .T. ) ;
#40205 = CARTESIAN_POINT ( 'NONE',  ( -16.93589915522259304, 10.00862525870701170, -54.44056010196031536 ) ) ;
#40206 = DIRECTION ( 'NONE',  ( 0.000000000000000000, 6.997203936713175802E-15, -1.000000000000000000 ) ) ;
#40208 = EDGE_LOOP ( 'NONE', ( #190545, #122737, #246358, #90850 ) ) ;
#40207 = CARTESIAN_POINT ( 'NONE',  ( -18.46902351632712325, 8.797055283856513697, -245.4142078959211517 ) ) ;
#40209 = DIRECTION ( 'NONE',  ( 0.000000000000000000, 1.000000000000000000, 6.938893903907222067E-15 ) ) ;
#40210 = ORIENTED_EDGE ( 'NONE', *, *, #3146, .T. ) ;
#40211 = CARTESIAN_POINT ( 'NONE',  ( -16.92973740335371247, 9.992503814478531865, -180.0939409647977527 ) ) ;
#40212 = DIRECTION ( 'NONE',  ( -1.000000000000000000, -0.000000000000000000, -0.000000000000000000 ) ) ;
#40213 = DIRECTION ( 'NONE',  ( 0.000000000000000000, 0.9999631594459053030, 0.008583690987162899758 ) ) ;
#40214 = VECTOR ( 'NONE', #209926, 1000.000000000000114 ) ;
#40215 = ORIENTED_EDGE ( 'NONE', *, *, #118094, .F. ) ;
#40216 = CARTESIAN_POINT ( 'NONE',  ( -18.50000000000000000, 66.65000000001222702, -148.6731074845244223 ) ) ;
#40217 = ORIENTED_EDGE ( 'NONE', *, *, #209307, .F. ) ;
#40218 = DIRECTION ( 'NONE',  ( -1.000000000000000000, 0.000000000000000000, 0.000000000000000000 ) ) ;
#40219 = EDGE_CURVE ( 'NONE', #192641, #239804, #158167, .T. ) ;
#40220 = CARTESIAN_POINT ( 'NONE',  ( -20.54999999999999716, 46.15118611352045974, -240.5321844900040844 ) ) ;
#40221 = ADVANCED_FACE ( 'NONE', ( #160722 ), #237660, .T. ) ;
#40222 = VERTEX_POINT ( 'NONE', #199835 ) ;
#40223 = CARTESIAN_POINT ( 'NONE',  ( -21.05000000000000071, 1.835341550235567887, -45.05515129256298223 ) ) ;
#40224 = VECTOR ( 'NONE', #51513, 1000.000000000000000 ) ;
#40225 = FACE_OUTER_BOUND ( 'NONE', #10993, .T. ) ;
#40226 = FACE_OUTER_BOUND ( 'NONE', #163635, .T. ) ;
#40228 = EDGE_CURVE ( 'NONE', #187434, #112788, #44990, .T. ) ;
#40227 = ORIENTED_EDGE ( 'NONE', *, *, #255749, .T. ) ;
#40229 = AXIS2_PLACEMENT_3D ( 'NONE', #213886, #230908, #130489 ) ;
#40230 = PLANE ( 'NONE',  #39341 ) ;
#40231 = CARTESIAN_POINT ( 'NONE',  ( 20.94999999999999929, 43.36285386911620776, -234.7972500504784534 ) ) ;
#40232 = VERTEX_POINT ( 'NONE', #198524 ) ;
#40233 = CARTESIAN_POINT ( 'NONE',  ( 20.94999999999999574, 70.10000000001267040, -193.3040077198679967 ) ) ;
#40234 = CIRCLE ( 'NONE', #73554, 0.09999999999999982514 ) ;
#40235 = ORIENTED_EDGE ( 'NONE', *, *, #99413, .T. ) ;
#40236 = COLOUR_RGB ( '', 0.09019608, 0.27058824, 0.51372549) ;
#40237 = DIRECTION ( 'NONE',  ( -0.000000000000000000, 0.2617529984165031243, 0.9651348961777157509 ) ) ;
#40238 = ORIENTED_EDGE ( 'NONE', *, *, #47457, .T. ) ;
#40240 = ORIENTED_EDGE ( 'NONE', *, *, #209427, .F. ) ;
#40239 = DIRECTION ( 'NONE',  ( -1.000000000000000000, 0.000000000000000000, 0.000000000000000000 ) ) ;
#40244 = EDGE_CURVE ( 'NONE', #46294, #159190, #19908, .T. ) ;
#40243 = ORIENTED_EDGE ( 'NONE', *, *, #46101, .F. ) ;
#40242 = ORIENTED_EDGE ( 'NONE', *, *, #29714, .T. ) ;
#40241 = CARTESIAN_POINT ( 'NONE',  ( 20.94999999999999929, 5.000000000011153745, -121.5947339810869465 ) ) ;
#40245 = CARTESIAN_POINT ( 'NONE',  ( 21.05000000000000071, 62.99095723518624368, -207.1734234082435080 ) ) ;
#40246 = CARTESIAN_POINT ( 'NONE',  ( -20.93302460841142931, 65.68434038414308418, -30.48668807260656521 ) ) ;
#40247 = DIRECTION ( 'NONE',  ( 2.940209281316622495E-16, -1.000000000000000000, 0.000000000000000000 ) ) ;
#40248 = CARTESIAN_POINT ( 'NONE',  ( 20.88420186297724257, 46.46179379974390855, -243.0832762246653260 ) ) ;
#40249 = DIRECTION ( 'NONE',  ( 0.000000000000000000, -0.7071067811865472397, -0.7071067811865479058 ) ) ;
#40250 = AXIS2_PLACEMENT_3D ( 'NONE', #117654, #212908, #176370 ) ;
#40251 = CARTESIAN_POINT ( 'NONE',  ( 20.94999999999999929, 65.52661458509973613, -195.9444530202758870 ) ) ;
#40252 = DIRECTION ( 'NONE',  ( -1.000000000000000000, 0.000000000000000000, -0.000000000000000000 ) ) ;
#40254 = CARTESIAN_POINT ( 'NONE',  ( 20.94999999999999574, 1.115600667400684642E-11, -67.00000000000004263 ) ) ;
#40253 = FACE_OUTER_BOUND ( 'NONE', #93501, .T. ) ;
#40255 = AXIS2_PLACEMENT_3D ( 'NONE', #10983, #28011, #86634 ) ;
#40256 = ORIENTED_EDGE ( 'NONE', *, *, #234197, .T. ) ;
#40257 = EDGE_LOOP ( 'NONE', ( #227275, #10711, #255707, #25070 ) ) ;
#40258 = ADVANCED_FACE ( 'NONE', ( #62867 ), #120319, .F. ) ;
#40260 = CARTESIAN_POINT ( 'NONE',  ( -23.25000000000000000, 1.115600667400684642E-11, -167.4999999999999716 ) ) ;
#40259 = AXIS2_PLACEMENT_3D ( 'NONE', #184283, #206422, #87739 ) ;
#40261 = EDGE_CURVE ( 'NONE', #45859, #206465, #65825, .T. ) ;
#40263 = VERTEX_POINT ( 'NONE', #220666 ) ;
#40262 = DIRECTION ( 'NONE',  ( 1.000000000000000000, 0.000000000000000000, 0.000000000000000000 ) ) ;
#40265 = CARTESIAN_POINT ( 'NONE',  ( 20.93284271247462414, 64.25000000001175238, -76.53791325517833855 ) ) ;
#40264 = MECHANICAL_DESIGN_GEOMETRIC_PRESENTATION_REPRESENTATION (  '', ( #231784 ), #161039 ) ;
#40266 = ORIENTED_EDGE ( 'NONE', *, *, #133347, .F. ) ;
#40267 = CARTESIAN_POINT ( 'NONE',  ( -20.85000000000000142, 1.115600667400684642E-11, -175.4000000000000341 ) ) ;
#40268 =( BOUNDED_SURFACE ( )  B_SPLINE_SURFACE ( 3, 2, ( 
 ( #40913, #100806, #202521 ),
 ( #241646, #120453, #22623 ),
 ( #102104, #64294, #23913 ),
 ( #103392, #83810, #242922 ) ),
 .UNSPECIFIED., .F., .F., .F. ) 
 B_SPLINE_SURFACE_WITH_KNOTS ( ( 4, 4 ),
 ( 3, 3 ),
 ( 0.0008258556059633768206, 0.0009616864997632838244 ),
 ( 0.000000000000000000, 1.000000000000000000 ),
 .UNSPECIFIED. ) 
 GEOMETRIC_REPRESENTATION_ITEM ( )  RATIONAL_B_SPLINE_SURFACE ( (
 ( 1.000000000000000000, 0.9152888060719408525, 1.000000000000000000),
 ( 1.000000000000000000, 0.9327727094138034136, 1.000000000000000000),
 ( 1.000000000000000000, 0.9369023509258638249, 1.000000000000000000),
 ( 1.000000000000000000, 0.9246339933864352600, 1.000000000000000000) ) ) 
 REPRESENTATION_ITEM ( '' )  SURFACE ( )  );
#40269 = EDGE_LOOP ( 'NONE', ( #229709, #183898, #19469, #255139 ) ) ;
#40270 = DIRECTION ( 'NONE',  ( 0.000000000000000000, 0.9893560106964510714, -0.1455152366551481502 ) ) ;
#40271 = CIRCLE ( 'NONE', #173567, 12.97499999999999964 ) ;
#40272 = ADVANCED_FACE ( 'NONE', ( #42042 ), #101961, .F. ) ;
#40273 = EDGE_CURVE ( 'NONE', #175607, #247253, #11887, .T. ) ;
#40274 = TOROIDAL_SURFACE ( 'NONE', #36163, 7.791421356237316687, 0.1000000000000000056 ) ;
#40275 = ORIENTED_EDGE ( 'NONE', *, *, #241334, .F. ) ;
#40276 = CARTESIAN_POINT ( 'NONE',  ( 18.59999999999999076, 10.49142135624846439, -125.3500000000000512 ) ) ;
#40277 = EDGE_CURVE ( 'NONE', #15545, #147029, #6742, .T. ) ;
#40280 = ORIENTED_EDGE ( 'NONE', *, *, #93623, .T. ) ;
#40279 = ORIENTED_EDGE ( 'NONE', *, *, #137120, .T. ) ;
#40278 = VECTOR ( 'NONE', #102111, 1000.000000000000000 ) ;
#40281 = EDGE_LOOP ( 'NONE', ( #126557, #202385, #197571, #187106 ) ) ;
#40283 = EDGE_CURVE ( 'NONE', #166990, #159227, #225771, .T. ) ;
#40282 = CARTESIAN_POINT ( 'NONE',  ( 21.05000000000000071, 70.42128727326085880, -228.5349014959848262 ) ) ;
#40284 = AXIS2_PLACEMENT_3D ( 'NONE', #98307, #197441, #17516 ) ;
#40285 = ORIENTED_EDGE ( 'NONE', *, *, #16079, .T. ) ;
#40286 = TOROIDAL_SURFACE ( 'NONE', #223571, 4.099999999999999645, 0.1000000000000000056 ) ;
#40287 = EDGE_LOOP ( 'NONE', ( #165941, #40000, #26771, #35341 ) ) ;
#40288 = CARTESIAN_POINT ( 'NONE',  ( -16.98495255085916611, 12.46505164876903216, -211.2160343393914559 ) ) ;
#40290 = ORIENTED_EDGE ( 'NONE', *, *, #197169, .F. ) ;
#40289 = FACE_OUTER_BOUND ( 'NONE', #102401, .T. ) ;
#40291 = ADVANCED_FACE ( 'NONE', ( #204929 ), #167140, .T. ) ;
#40293 = CARTESIAN_POINT ( 'NONE',  ( -16.87435696428308063, 60.93935323350471833, -221.0417350386312876 ) ) ;
#40292 = FACE_OUTER_BOUND ( 'NONE', #67350, .T. ) ;
#40294 = DIRECTION ( 'NONE',  ( -1.000000000000000000, 0.000000000000000000, 0.000000000000000000 ) ) ;
#40295 = CYLINDRICAL_SURFACE ( 'NONE', #73827, 0.09999999999999939493 ) ;
#40296 = DIRECTION ( 'NONE',  ( -0.000000000000000000, 1.000000000000000000, -0.000000000000000000 ) ) ;
#40297 = VERTEX_POINT ( 'NONE', #125421 ) ;
#40298 = ORIENTED_EDGE ( 'NONE', *, *, #107879, .F. ) ;
#40299 = CYLINDRICAL_SURFACE ( 'NONE', #178993, 0.1000000000000028644 ) ;
#40300 = DIRECTION ( 'NONE',  ( 0.000000000000000000, 0.000000000000000000, 1.000000000000000000 ) ) ;
#40302 = EDGE_CURVE ( 'NONE', #56169, #82821, #82550, .T. ) ;
#40301 = CARTESIAN_POINT ( 'NONE',  ( -20.54999999999999716, 53.03738849591485405, -234.3791188517465400 ) ) ;
#40303 = VECTOR ( 'NONE', #241957, 1000.000000000000114 ) ;
#40304 = VERTEX_POINT ( 'NONE', #88824 ) ;
#40305 = CARTESIAN_POINT ( 'NONE',  ( -18.40000000000000213, 64.25000000001207923, -123.8731074845243683 ) ) ;
#40306 = EDGE_CURVE ( 'NONE', #18395, #239536, #143822, .T. ) ;
#40307 = EDGE_CURVE ( 'NONE', #114431, #212495, #47129, .T. ) ;
#40308 = CARTESIAN_POINT ( 'NONE',  ( -20.00857864376270001, 66.75000000001151079, -48.37310748452438247 ) ) ;
#40309 = ORIENTED_EDGE ( 'NONE', *, *, #141257, .T. ) ;
#40310 = VERTEX_POINT ( 'NONE', #168445 ) ;
#40311 = EDGE_CURVE ( 'NONE', #175607, #130829, #126696, .T. ) ;
#40312 = DIRECTION ( 'NONE',  ( 1.000000000000000000, -0.000000000000000000, 0.000000000000000000 ) ) ;
#40313 = FACE_OUTER_BOUND ( 'NONE', #242037, .T. ) ;
#40314 = ORIENTED_EDGE ( 'NONE', *, *, #229771, .T. ) ;
#40315 = DIRECTION ( 'NONE',  ( 0.000000000000000000, 0.000000000000000000, -1.000000000000000000 ) ) ;
#40316 = ORIENTED_EDGE ( 'NONE', *, *, #16749, .T. ) ;
#40317 = FACE_OUTER_BOUND ( 'NONE', #199020, .T. ) ;
#40318 = FACE_OUTER_BOUND ( 'NONE', #93998, .T. ) ;
#40320 = LINE ( 'NONE', #175970, #16828 ) ;
#40319 = DIRECTION ( 'NONE',  ( 1.000000000000000000, -1.875376730785737719E-16, -1.309568571767809260E-30 ) ) ;
#40321 = EDGE_CURVE ( 'NONE', #176232, #49225, #28468, .T. ) ;
#40322 = VECTOR ( 'NONE', #210785, 1000.000000000000000 ) ;
#40324 = ADVANCED_FACE ( 'NONE', ( #49722 ), #195035, .F. ) ;
#40323 = CARTESIAN_POINT ( 'NONE',  ( 22.45301702632625762, 0.01521087972134078925, -55.35020777573965489 ) ) ;
#40325 = CIRCLE ( 'NONE', #223422, 0.1999999999999987899 ) ;
#40326 = DIRECTION ( 'NONE',  ( -1.000000000000000000, 0.000000000000000000, -0.000000000000000000 ) ) ;
#40327 = AXIS2_PLACEMENT_3D ( 'NONE', #156097, #196461, #72704 ) ;
#40328 = AXIS2_PLACEMENT_3D ( 'NONE', #62955, #257249, #220748 ) ;
#40329 = EDGE_CURVE ( 'NONE', #78910, #121993, #187960, .T. ) ;
#40330 = EDGE_LOOP ( 'NONE', ( #117826, #68214, #101998, #21945 ) ) ;
#40331 = DIRECTION ( 'NONE',  ( 0.000000000000000000, 0.000000000000000000, 1.000000000000000000 ) ) ;
#40332 = CIRCLE ( 'NONE', #57008, 0.09999999999998898659 ) ;
#40334 = VERTEX_POINT ( 'NONE', #203664 ) ;
#40333 = VERTEX_POINT ( 'NONE', #247914 ) ;
#40335 = EDGE_LOOP ( 'NONE', ( #225775, #162497, #133546, #161689 ) ) ;
#40336 = DIRECTION ( 'NONE',  ( 0.000000000000000000, 0.000000000000000000, 1.000000000000000000 ) ) ;
#40337 = DIRECTION ( 'NONE',  ( 0.000000000000000000, 0.000000000000000000, -1.000000000000000000 ) ) ;
#40338 = CARTESIAN_POINT ( 'NONE',  ( 20.94999999999999929, 64.35000000001176090, -76.30697314750248950 ) ) ;
#40339 = DIRECTION ( 'NONE',  ( -1.000000000000000000, -0.000000000000000000, -0.000000000000000000 ) ) ;
#40340 = CARTESIAN_POINT ( 'NONE',  ( 20.85000000000000142, 11.75000000001115907, -67.00000000000000000 ) ) ;
#40341 = EDGE_CURVE ( 'NONE', #234233, #153145, #74249, .T. ) ;
#40342 = AXIS2_PLACEMENT_3D ( 'NONE', #85151, #104713, #224687 ) ;
#40344 = DIRECTION ( 'NONE',  ( 1.000000000000000000, 0.000000000000000000, 0.000000000000000000 ) ) ;
#40343 = CARTESIAN_POINT ( 'NONE',  ( 20.87631937322882791, 10.47149503676486226, -7.579745874581184317 ) ) ;
#40345 = ORIENTED_EDGE ( 'NONE', *, *, #150216, .T. ) ;
#40346 = DIRECTION ( 'NONE',  ( -1.000000000000000000, 0.000000000000000000, 0.000000000000000000 ) ) ;
#40347 = ORIENTED_EDGE ( 'NONE', *, *, #153047, .F. ) ;
#40348 = DIRECTION ( 'NONE',  ( 1.000000000000000000, 0.000000000000000000, 0.000000000000000000 ) ) ;
#40349 = AXIS2_PLACEMENT_3D ( 'NONE', #89954, #147371, #108251 ) ;
#40350 = ORIENTED_EDGE ( 'NONE', *, *, #226869, .F. ) ;
#40351 = VERTEX_POINT ( 'NONE', #147542 ) ;
#40352 = CARTESIAN_POINT ( 'NONE',  ( 21.97500000000000497, 30.37633856152204359, -235.1250019192171408 ) ) ;
#40353 = AXIS2_PLACEMENT_3D ( 'NONE', #87186, #209731, #34981 ) ;
#40354 = DIRECTION ( 'NONE',  ( 0.000000000000000000, -0.9770955615653316162, -0.2128009952263604232 ) ) ;
#40355 = CARTESIAN_POINT ( 'NONE',  ( 20.94999999999999929, 69.45000000001260787, -193.5060803140843859 ) ) ;
#40356 = DIRECTION ( 'NONE',  ( 1.000000000000000000, 0.000000000000000000, 0.000000000000000000 ) ) ;
#40357 = CARTESIAN_POINT ( 'NONE',  ( -20.64999999999999858, -8.999999999988844479, -57.10603087734755690 ) ) ;
#40358 = EDGE_LOOP ( 'NONE', ( #98339, #48148, #166881, #114940, #159191 ) ) ;
#40359 = ORIENTED_EDGE ( 'NONE', *, *, #135608, .F. ) ;
#40360 = CIRCLE ( 'NONE', #119431, 0.09999999999999939493 ) ;
#40361 = CARTESIAN_POINT ( 'NONE',  ( -20.94999999999999929, -1.360870587180885716, -108.5729979270909951 ) ) ;
#40362 = ORIENTED_EDGE ( 'NONE', *, *, #197254, .T. ) ;
#40363 = CARTESIAN_POINT ( 'NONE',  ( -16.91049119928364064, 22.95010608342089498, -230.9200852673934605 ) ) ;
#40364 = CARTESIAN_POINT ( 'NONE',  ( 18.59999999999999787, 1.148907358139439339E-11, -201.0000000000015064 ) ) ;
#40365 = SPHERICAL_SURFACE ( 'NONE', #129462, 0.1000000000000000056 ) ;
#40366 = DIRECTION ( 'NONE',  ( 0.000000000000000000, -0.9126074666063772600, -0.4088369013363274407 ) ) ;
#40367 = CARTESIAN_POINT ( 'NONE',  ( 20.94999999999999929, 71.18691588786271041, -148.4646252410481964 ) ) ;
#40368 = CARTESIAN_POINT ( 'NONE',  ( -20.94999999999999929, -10.82118976317943826, -206.5294079347637819 ) ) ;
#40370 = CARTESIAN_POINT ( 'NONE',  ( -23.15000000000000213, 11.75000000001115552, -130.9000000000000341 ) ) ;
#40369 = DIRECTION ( 'NONE',  ( 0.000000000000000000, 0.000000000000000000, -1.000000000000000000 ) ) ;
#40371 = CARTESIAN_POINT ( 'NONE',  ( -20.54999999999999716, 74.00000000001156764, -56.29848556176223440 ) ) ;
#40372 = EDGE_CURVE ( 'NONE', #251836, #97348, #136736, .T. ) ;
#40373 = DIRECTION ( 'NONE',  ( -1.000000000000000000, -0.000000000000000000, -0.000000000000000000 ) ) ;
#40374 = AXIS2_PLACEMENT_3D ( 'NONE', #36843, #14707, #115062 ) ;
#40376 = VECTOR ( 'NONE', #57920, 1000.000000000000000 ) ;
#40375 = CARTESIAN_POINT ( 'NONE',  ( -23.25000000000000000, 87.75000000001276135, -215.2731074845242745 ) ) ;
#40377 = EDGE_CURVE ( 'NONE', #816, #82768, #17460, .T. ) ;
#40378 = VECTOR ( 'NONE', #190235, 1000.000000000000000 ) ;
#40379 = VECTOR ( 'NONE', #107018, 1000.000000000000000 ) ;
#40380 = VERTEX_POINT ( 'NONE', #30183 ) ;
#40381 = EDGE_CURVE ( 'NONE', #23148, #218469, #32768, .T. ) ;
#40382 = CARTESIAN_POINT ( 'NONE',  ( -21.29999999999995808, 1.115650265596050101E-11, -62.95000000000004547 ) ) ;
#40383 = ADVANCED_FACE ( 'NONE', ( #71873 ), #152711, .F. ) ;
#40384 = ORIENTED_EDGE ( 'NONE', *, *, #130602, .T. ) ;
#40385 = CARTESIAN_POINT ( 'NONE',  ( 18.49505832270840955, 85.43802806279497020, -129.3246343096303690 ) ) ;
#40386 = DIRECTION ( 'NONE',  ( 0.000000000000000000, 0.2605042016806715099, 0.9654727137038706664 ) ) ;
#40387 = LINE ( 'NONE', #2481, #131210 ) ;
#40388 = EDGE_LOOP ( 'NONE', ( #157794, #73391, #225708, #117784, #123962 ) ) ;
#40389 = DIRECTION ( 'NONE',  ( 3.469446951953620500E-14, 0.000000000000000000, 1.000000000000000000 ) ) ;
#40390 = VECTOR ( 'NONE', #172539, 1000.000000000000114 ) ;
#40391 = CARTESIAN_POINT ( 'NONE',  ( -20.54999999999999716, 54.73010456436290383, -239.3295147855486107 ) ) ;
#40392 = FACE_OUTER_BOUND ( 'NONE', #236160, .T. ) ;
#40393 = CIRCLE ( 'NONE', #144361, 0.1000000000000028644 ) ;
#40394 = AXIS2_PLACEMENT_3D ( 'NONE', #72131, #166117, #188210 ) ;
#40395 = DIRECTION ( 'NONE',  ( 0.000000000000000000, -0.4999999999999088507, -0.8660254037844913322 ) ) ;
#40396 = DIRECTION ( 'NONE',  ( 1.000000000000000000, 2.952720810173289112E-16, -0.000000000000000000 ) ) ;
#40397 = ORIENTED_EDGE ( 'NONE', *, *, #134654, .F. ) ;
#40398 = CARTESIAN_POINT ( 'NONE',  ( -20.94999999999999929, 6.846123162363745074, -204.7377262668498190 ) ) ;
#40400 = EDGE_LOOP ( 'NONE', ( #210496, #21191, #193928, #215997 ) ) ;
#40399 = CARTESIAN_POINT ( 'NONE',  ( -21.29999999999995808, 3.558777552609279304, -231.8203201594644725 ) ) ;
#40401 = LINE ( 'NONE', #37820, #75893 ) ;
#40402 = CARTESIAN_POINT ( 'NONE',  ( 18.59999999999999076, 69.45000000001222418, -148.7731074845244166 ) ) ;
#40403 = DIRECTION ( 'NONE',  ( 1.000000000000000000, -0.000000000000000000, -0.000000000000000000 ) ) ;
#40404 = ORIENTED_EDGE ( 'NONE', *, *, #161052, .F. ) ;
#40405 = DIRECTION ( 'NONE',  ( 0.000000000000000000, 0.000000000000000000, 1.000000000000000000 ) ) ;
#40406 = APPLICATION_PROTOCOL_DEFINITION ( 'draft international standard', 'automotive_design', 1998, #20799 ) ;
#40407 = DIRECTION ( 'NONE',  ( -1.000000000000000000, 0.000000000000000000, 0.000000000000000000 ) ) ;
#40408 = ORIENTED_EDGE ( 'NONE', *, *, #70623, .F. ) ;
#40409 = CARTESIAN_POINT ( 'NONE',  ( -22.94999999999999929, -1.467286812112899463, 33.00000000000000000 ) ) ;
#40410 = LINE ( 'NONE', #199467, #54917 ) ;
#40411 = ADVANCED_FACE ( 'NONE', ( #76982 ), #114830, .F. ) ;
#40412 = FACE_OUTER_BOUND ( 'NONE', #169665, .T. ) ;
#40413 = EDGE_LOOP ( 'NONE', ( #82945, #164081, #27055, #112229, #222948 ) ) ;
#40414 = ORIENTED_EDGE ( 'NONE', *, *, #111879, .T. ) ;
#40415 = DIRECTION ( 'NONE',  ( 1.000000000000000000, -0.000000000000000000, -0.000000000000000000 ) ) ;
#40416 = AXIS2_PLACEMENT_3D ( 'NONE', #54458, #151007, #195287 ) ;
#40417 = DIRECTION ( 'NONE',  ( 1.000000000000000000, -0.000000000000000000, -0.000000000000000000 ) ) ;
#40418 = EDGE_CURVE ( 'NONE', #84512, #242965, #156562, .T. ) ;
#40419 = DIRECTION ( 'NONE',  ( 1.000000000000000000, -0.000000000000000000, -0.000000000000000000 ) ) ;
#40420 = DIRECTION ( 'NONE',  ( -0.000000000000000000, 1.000000000000000000, 0.000000000000000000 ) ) ;
#40421 = DIRECTION ( 'NONE',  ( 0.000000000000000000, 0.000000000000000000, -1.000000000000000000 ) ) ;
#40422 = CARTESIAN_POINT ( 'NONE',  ( -20.64999999999999858, 47.91013932883114990, -242.3192343197862044 ) ) ;
#40423 = ADVANCED_FACE ( 'NONE', ( #194395 ), #92691, .F. ) ;
#40426 = LINE ( 'NONE', #234735, #7839 ) ;
#40425 = VECTOR ( 'NONE', #159079, 1000.000000000000000 ) ;
#40424 = CARTESIAN_POINT ( 'NONE',  ( 18.52928932188133970, 65.72071067813043044, -78.37310748452438247 ) ) ;
#40427 = CARTESIAN_POINT ( 'NONE',  ( 23.14999999999999858, 34.89593390941166007, -248.6067769466879156 ) ) ;
#40428 = CARTESIAN_POINT ( 'NONE',  ( 23.15000000000000213, 87.65000000001215597, -139.6231074845242688 ) ) ;
#40429 = AXIS2_PLACEMENT_3D ( 'NONE', #87380, #164376, #204764 ) ;
#40430 = ORIENTED_EDGE ( 'NONE', *, *, #61673, .T. ) ;
#40431 = CIRCLE ( 'NONE', #186133, 0.09999999999998898659 ) ;
#40432 = EDGE_LOOP ( 'NONE', ( #107881, #120484, #158109, #224988 ) ) ;
#40433 = CARTESIAN_POINT ( 'NONE',  ( -20.85000000000000142, 7.021664781911246322, -171.3335654018973173 ) ) ;
#40435 = FACE_OUTER_BOUND ( 'NONE', #160182, .T. ) ;
#40434 = CARTESIAN_POINT ( 'NONE',  ( -18.59999999999999787, 64.35000000001264198, -196.5083017138704236 ) ) ;
#40436 = EDGE_CURVE ( 'NONE', #175428, #175330, #91425, .T. ) ;
#40437 = TOROIDAL_SURFACE ( 'NONE', #65899, 0.4000000000000010214, 0.1000000000000000056 ) ;
#40438 = DIRECTION ( 'NONE',  ( -1.000000000000000000, -0.000000000000000000, 0.000000000000000000 ) ) ;
#40439 = CARTESIAN_POINT ( 'NONE',  ( -13.39999999999994529, 67.75000000001118394, -18.42310748452479174 ) ) ;
#40440 = AXIS2_PLACEMENT_3D ( 'NONE', #99953, #119568, #240785 ) ;
#40441 = CYLINDRICAL_SURFACE ( 'NONE', #56594, 0.1000000000000028644 ) ;
#40442 = EDGE_CURVE ( 'NONE', #231084, #13871, #66021, .T. ) ;
#40443 = EDGE_LOOP ( 'NONE', ( #55341, #175644, #35403, #40602 ) ) ;
#40444 = EDGE_CURVE ( 'NONE', #7823, #221901, #251774, .T. ) ;
#40445 = CARTESIAN_POINT ( 'NONE',  ( 22.57320508075687115, 11.75000000001115552, -67.00000000000004263 ) ) ;
#40446 = ORIENTED_EDGE ( 'NONE', *, *, #34027, .T. ) ;
#40447 = FACE_OUTER_BOUND ( 'NONE', #222870, .T. ) ;
#40448 = EDGE_CURVE ( 'NONE', #75879, #147930, #115914, .T. ) ;
#40449 = VERTEX_POINT ( 'NONE', #130536 ) ;
#40450 = CARTESIAN_POINT ( 'NONE',  ( 23.04999999999999716, 8.822561741677553471, -124.7500000000000284 ) ) ;
#40451 = CIRCLE ( 'NONE', #227837, 0.5000000000000051070 ) ;
#40452 = VECTOR ( 'NONE', #141208, 1000.000000000000114 ) ;
#40453 = DIRECTION ( 'NONE',  ( 0.7071067811865475727, 0.7071067811865475727, 4.937700262164531476E-15 ) ) ;
#40454 = VECTOR ( 'NONE', #175055, 1000.000000000000000 ) ;
#40456 = ORIENTED_EDGE ( 'NONE', *, *, #25258, .T. ) ;
#40455 = AXIS2_PLACEMENT_3D ( 'NONE', #250824, #151765, #116471 ) ;
#40457 = DIRECTION ( 'NONE',  ( -7.304098846218134667E-16, -1.000000000000000000, 0.000000000000000000 ) ) ;
#40458 = EDGE_CURVE ( 'NONE', #194487, #45940, #199304, .T. ) ;
#40459 = ORIENTED_EDGE ( 'NONE', *, *, #99840, .F. ) ;
#40460 = AXIS2_PLACEMENT_3D ( 'NONE', #122610, #241274, #199592 ) ;
#40461 = CARTESIAN_POINT ( 'NONE',  ( -20.94999999999999929, 4.252251777740766236, -211.8999245327126744 ) ) ;
#40462 = AXIS2_PLACEMENT_3D ( 'NONE', #96686, #61453, #158033 ) ;
#40463 = CARTESIAN_POINT ( 'NONE',  ( -21.07016717456947319, 69.67905916191141102, -69.52310748452435973 ) ) ;
#40464 = CARTESIAN_POINT ( 'NONE',  ( -18.50000000000000000, 38.31554990269469840, -261.1022705275898943 ) ) ;
#40465 = DIRECTION ( 'NONE',  ( -0.000000000000000000, -0.8660254037844420383, 0.4999999999999943379 ) ) ;
#40466 = DIRECTION ( 'NONE',  ( 0.000000000000000000, -0.2128009952263603954, 0.9770955615653315052 ) ) ;
#40468 = CARTESIAN_POINT ( 'NONE',  ( -20.64999999999999858, 6.659649981195239654, -220.3002595397864241 ) ) ;
#40467 = DIRECTION ( 'NONE',  ( 1.000000000000000000, 0.000000000000000000, 0.000000000000000000 ) ) ;
#40469 = DIRECTION ( 'NONE',  ( 1.000000000000000000, -0.000000000000000000, -0.000000000000000000 ) ) ;
#40471 = ORIENTED_EDGE ( 'NONE', *, *, #2706, .T. ) ;
#40470 = CARTESIAN_POINT ( 'NONE',  ( 21.13507111622889667, 65.28231661301421695, -191.2739388981636353 ) ) ;
#40473 = CARTESIAN_POINT ( 'NONE',  ( 20.85000000000000142, 67.74990736105834799, -227.9721689390126755 ) ) ;
#40472 = CARTESIAN_POINT ( 'NONE',  ( 20.94999999999999929, 65.61821452928846554, -164.5152621206402728 ) ) ;
#40474 = ORIENTED_EDGE ( 'NONE', *, *, #197713, .T. ) ;
#40476 = ORIENTED_EDGE ( 'NONE', *, *, #256937, .T. ) ;
#40475 = DIRECTION ( 'NONE',  ( 1.000000000000000000, -0.000000000000000000, 0.000000000000000000 ) ) ;
#40477 = CIRCLE ( 'NONE', #252801, 0.09999999999999939493 ) ;
#40478 = ORIENTED_EDGE ( 'NONE', *, *, #22113, .F. ) ;
#40479 = LINE ( 'NONE', #57413, #61709 ) ;
#40480 = CIRCLE ( 'NONE', #186182, 2.600000000000001421 ) ;
#40481 = DIRECTION ( 'NONE',  ( -0.000000000000000000, -0.2814428106787469352, -0.9595780032479105381 ) ) ;
#40482 = FACE_OUTER_BOUND ( 'NONE', #255571, .T. ) ;
#40483 = VERTEX_POINT ( 'NONE', #174860 ) ;
#40484 = DIRECTION ( 'NONE',  ( 0.000000000000000000, 0.000000000000000000, 1.000000000000000000 ) ) ;
#40485 = CARTESIAN_POINT ( 'NONE',  ( 21.05000000000000071, 8.776282889879928106, -112.6762151410681696 ) ) ;
#40486 = DIRECTION ( 'NONE',  ( 0.000000000000000000, -6.982962677686266711E-15, 1.000000000000000000 ) ) ;
#40487 = EDGE_LOOP ( 'NONE', ( #105220, #128449, #27816, #161491 ) ) ;
#40488 = DIRECTION ( 'NONE',  ( 1.000000000000000000, 0.000000000000000000, 0.000000000000000000 ) ) ;
#40489 = AXIS2_PLACEMENT_3D ( 'NONE', #13630, #172749, #129720 ) ;
#40490 = CARTESIAN_POINT ( 'NONE',  ( 20.94999999999999929, 6.450000000011156587, -43.51702717044002355 ) ) ;
#40491 = ORIENTED_EDGE ( 'NONE', *, *, #21743, .T. ) ;
#40492 = ORIENTED_EDGE ( 'NONE', *, *, #116935, .F. ) ;
#40493 = LINE ( 'NONE', #56142, #106074 ) ;
#40494 = ADVANCED_FACE ( 'NONE', ( #193098 ), #75719, .F. ) ;
#40495 = ORIENTED_EDGE ( 'NONE', *, *, #225133, .T. ) ;
#40496 = DIRECTION ( 'NONE',  ( 0.000000000000000000, 0.9915357197604792727, -0.1298341882520473722 ) ) ;
#40497 = ORIENTED_EDGE ( 'NONE', *, *, #51216, .T. ) ;
#40498 = CARTESIAN_POINT ( 'NONE',  ( 20.89878130938411616, 10.32747123227773045, -173.0774032850249569 ) ) ;
#40499 = AXIS2_PLACEMENT_3D ( 'NONE', #235531, #171753, #114310 ) ;
#40500 = CARTESIAN_POINT ( 'NONE',  ( 22.50000000000000000, 76.00000000001237765, -170.0231074845243597 ) ) ;
#40501 = CARTESIAN_POINT ( 'NONE',  ( -21.05000000000000071, 69.06797323185276127, -247.4100621602722470 ) ) ;
#40502 = ADVANCED_FACE ( 'NONE', ( #135660 ), #35337, .T. ) ;
#40503 = FACE_OUTER_BOUND ( 'NONE', #188985, .T. ) ;
#40504 = VECTOR ( 'NONE', #239338, 1000.000000000000114 ) ;
#40505 = AXIS2_PLACEMENT_3D ( 'NONE', #61704, #220776, #160827 ) ;
#40506 = ADVANCED_FACE ( 'NONE', ( #131823 ), #93972, .T. ) ;
#40508 = ADVANCED_FACE ( 'NONE', ( #253050 ), #74461, .T. ) ;
#40507 = CIRCLE ( 'NONE', #173801, 0.09999999999998898659 ) ;
#40509 = AXIS2_PLACEMENT_3D ( 'NONE', #132679, #34886, #193940 ) ;
#40510 = DIRECTION ( 'NONE',  ( -1.000000000000000000, -0.000000000000000000, -0.000000000000000000 ) ) ;
#40511 = CARTESIAN_POINT ( 'NONE',  ( -22.50047199487802274, 0.04490605193189570188, -88.74995258108347684 ) ) ;
#40512 = CARTESIAN_POINT ( 'NONE',  ( -23.15000000000000213, 11.65000000001115588, -55.25000000000004974 ) ) ;
#40513 = ORIENTED_EDGE ( 'NONE', *, *, #202771, .T. ) ;
#40515 = DIRECTION ( 'NONE',  ( 0.000000000000000000, 0.9126074666063770380, 0.4088369013363281068 ) ) ;
#40514 = DIRECTION ( 'NONE',  ( 0.000000000000000000, 0.8700118002898356018, -0.4930308989875170078 ) ) ;
#40516 = EDGE_LOOP ( 'NONE', ( #243557, #99012, #150302, #211466 ) ) ;
#40519 = ORIENTED_EDGE ( 'NONE', *, *, #221361, .T. ) ;
#40518 = CARTESIAN_POINT ( 'NONE',  ( -18.45068461519106506, 85.48650652910070846, -62.45433031561956483 ) ) ;
#40517 = DIRECTION ( 'NONE',  ( 0.000000000000000000, 0.8660254037844424824, 0.4999999999999934497 ) ) ;
#40520 = TOROIDAL_SURFACE ( 'NONE', #186225, 2.100000000000002309, 0.1000000000000000056 ) ;
#40521 = EDGE_LOOP ( 'NONE', ( #77756, #160034, #83489, #191312, #162061, #170126 ) ) ;
#40522 = DIRECTION ( 'NONE',  ( 1.000000000000000000, 0.000000000000000000, 0.000000000000000000 ) ) ;
#40523 = DIRECTION ( 'NONE',  ( -3.265361837132813093E-16, 1.000000000000000000, 0.000000000000000000 ) ) ;
#40524 = DIRECTION ( 'NONE',  ( 0.000000000000000000, 0.9209589331071864615, -0.3896596508878908960 ) ) ;
#40525 = CARTESIAN_POINT ( 'NONE',  ( -18.36973785203556275, 64.52449679952799499, -145.7731074845244450 ) ) ;
#40526 = ORIENTED_EDGE ( 'NONE', *, *, #247156, .T. ) ;
#40527 = DIRECTION ( 'NONE',  ( -0.000000000000000000, 1.000000000000000000, -0.000000000000000000 ) ) ;
#40528 = EDGE_CURVE ( 'NONE', #47348, #219843, #149245, .T. ) ;
#40529 = CARTESIAN_POINT ( 'NONE',  ( -21.05000000000000071, 76.00000000001126921, -203.5231074845248997 ) ) ;
#40530 = EDGE_CURVE ( 'NONE', #154572, #1714, #124891, .T. ) ;
#40532 = CARTESIAN_POINT ( 'NONE',  ( 20.95568717954149562, 10.60199405389181848, -7.602508368268654060 ) ) ;
#40531 = DIRECTION ( 'NONE',  ( 0.000000000000000000, -0.1332476588733589040, -0.9910827722268049644 ) ) ;
#40533 = VECTOR ( 'NONE', #212516, 1000.000000000000000 ) ;
#40535 = ORIENTED_EDGE ( 'NONE', *, *, #54712, .T. ) ;
#40534 = DIRECTION ( 'NONE',  ( -1.000000000000000000, 0.000000000000000000, -0.000000000000000000 ) ) ;
#40536 = VECTOR ( 'NONE', #230584, 1000.000000000000000 ) ;
#40537 = PRODUCT_DEFINITION ( 'UNKNOWN', '', #248677, #199189 ) ;
#40538 = ORIENTED_EDGE ( 'NONE', *, *, #49497, .F. ) ;
#40539 = VECTOR ( 'NONE', #8353, 1000.000000000000000 ) ;
#40540 = CARTESIAN_POINT ( 'NONE',  ( -16.91256925476569606, 44.01351207619228489, -235.3144196755796429 ) ) ;
#40541 = VERTEX_POINT ( 'NONE', #43008 ) ;
#40542 = LINE ( 'NONE', #217826, #131062 ) ;
#40543 = ORIENTED_EDGE ( 'NONE', *, *, #210585, .T. ) ;
#40544 = EDGE_CURVE ( 'NONE', #23353, #238821, #36836, .T. ) ;
#40545 = DIRECTION ( 'NONE',  ( 0.000000000000000000, -0.5954378521545836689, -0.8034013718071036925 ) ) ;
#40547 = EDGE_CURVE ( 'NONE', #7533, #62695, #45172, .T. ) ;
#40546 = DIRECTION ( 'NONE',  ( -1.073024830501117725E-15, 0.2128009952263604232, -0.9770955615653316162 ) ) ;
#40548 = PLANE ( 'NONE',  #47460 ) ;
#40549 = EDGE_CURVE ( 'NONE', #136469, #118259, #215836, .T. ) ;
#40550 = VERTEX_POINT ( 'NONE', #122552 ) ;
#40551 = DIRECTION ( 'NONE',  ( 0.000000000000000000, -6.454785026890489601E-15, 1.000000000000000000 ) ) ;
#40552 = EDGE_CURVE ( 'NONE', #184383, #213072, #19122, .T. ) ;
#40553 = TOROIDAL_SURFACE ( 'NONE', #186273, 11.90000000000000391, 0.1000000000000000056 ) ;
#40554 = AXIS2_PLACEMENT_3D ( 'NONE', #148419, #54434, #34918 ) ;
#40555 = DIRECTION ( 'NONE',  ( 0.000000000000000000, 0.000000000000000000, 1.000000000000000000 ) ) ;
#40556 = VECTOR ( 'NONE', #209998, 1000.000000000000000 ) ;
#40557 = VERTEX_POINT ( 'NONE', #97803 ) ;
#40558 = EDGE_LOOP ( 'NONE', ( #162912, #206672, #220961, #132691, #30279, #226450, #160997, #118471 ) ) ;
#40559 = ORIENTED_EDGE ( 'NONE', *, *, #23889, .T. ) ;
#40560 = FACE_OUTER_BOUND ( 'NONE', #226939, .T. ) ;
#40561 = EDGE_LOOP ( 'NONE', ( #247428, #22871, #188177, #96589 ) ) ;
#40563 = ORIENTED_EDGE ( 'NONE', *, *, #45161, .F. ) ;
#40562 = CARTESIAN_POINT ( 'NONE',  ( -21.05000000000000071, 1.835341550235567887, -112.0551512925630249 ) ) ;
#40564 = ORIENTED_EDGE ( 'NONE', *, *, #113275, .T. ) ;
#40568 = EDGE_CURVE ( 'NONE', #81511, #10689, #153559, .T. ) ;
#40567 = ORIENTED_EDGE ( 'NONE', *, *, #114790, .F. ) ;
#40566 = VERTEX_POINT ( 'NONE', #117401 ) ;
#40565 = DIRECTION ( 'NONE',  ( 0.000000000000000000, 0.000000000000000000, 1.000000000000000000 ) ) ;
#40569 = TOROIDAL_SURFACE ( 'NONE', #190398, 11.70000000000000639, 0.1000000000000000056 ) ;
#40570 = AXIS2_PLACEMENT_3D ( 'NONE', #34990, #53228, #131480 ) ;
#40571 = ORIENTED_EDGE ( 'NONE', *, *, #126182, .T. ) ;
#40572 = DIRECTION ( 'NONE',  ( 1.000000000000000000, 0.000000000000000000, -0.000000000000000000 ) ) ;
#40573 = DIRECTION ( 'NONE',  ( 1.000000000000000000, 0.000000000000000000, 0.000000000000000000 ) ) ;
#40574 = CIRCLE ( 'NONE', #132289, 0.1000000000000013933 ) ;
#40575 = CARTESIAN_POINT ( 'NONE',  ( 20.94999999999999929, 28.60154115857409352, -258.4512230915049713 ) ) ;
#40576 = ORIENTED_EDGE ( 'NONE', *, *, #164466, .F. ) ;
#40577 = EDGE_CURVE ( 'NONE', #144435, #135406, #139517, .T. ) ;
#40578 = DIRECTION ( 'NONE',  ( 0.000000000000000000, -0.03181660087581233282, 0.9994937237965575427 ) ) ;
#40580 = VERTEX_POINT ( 'NONE', #256851 ) ;
#40579 = CARTESIAN_POINT ( 'NONE',  ( 21.30740335185486245, 6.556657922039159203, -167.4010654742241115 ) ) ;
#40581 = DIRECTION ( 'NONE',  ( 0.000000000000000000, 1.000000000000000000, 2.775557561562888827E-14 ) ) ;
#40583 = ORIENTED_EDGE ( 'NONE', *, *, #4028, .F. ) ;
#40582 = DIRECTION ( 'NONE',  ( -0.000000000000000000, 0.4088369013363281623, -0.9126074666063771490 ) ) ;
#40584 = ORIENTED_EDGE ( 'NONE', *, *, #60970, .T. ) ;
#40585 = ADVANCED_FACE ( 'NONE', ( #157856 ), #142088, .F. ) ;
#40586 = DIRECTION ( 'NONE',  ( 2.952720810173288619E-16, -0.4721928772777346239, -0.8814952561688430555 ) ) ;
#40587 = DIRECTION ( 'NONE',  ( 0.7071067811865388020, -0.7071067811865561215, 0.000000000000000000 ) ) ;
#40588 = ORIENTED_EDGE ( 'NONE', *, *, #97645, .F. ) ;
#40589 = ORIENTED_EDGE ( 'NONE', *, *, #212153, .T. ) ;
#40590 = CARTESIAN_POINT ( 'NONE',  ( -16.93230518875208546, 10.00075036143099894, -180.0757783481014940 ) ) ;
#40591 = LINE ( 'NONE', #256975, #31936 ) ;
#40592 = CIRCLE ( 'NONE', #127866, 0.9750000000000036415 ) ;
#40593 = EDGE_CURVE ( 'NONE', #171646, #253610, #57629, .T. ) ;
#40595 = ORIENTED_EDGE ( 'NONE', *, *, #165458, .F. ) ;
#40594 = ORIENTED_EDGE ( 'NONE', *, *, #155929, .T. ) ;
#40596 = ORIENTED_EDGE ( 'NONE', *, *, #235228, .T. ) ;
#40598 = EDGE_CURVE ( 'NONE', #74110, #52138, #245086, .T. ) ;
#40597 = CARTESIAN_POINT ( 'NONE',  ( 21.07964655665547227, 61.96144568752238513, -221.7624746465921817 ) ) ;
#40599 = EDGE_LOOP ( 'NONE', ( #114250, #186347, #156606, #182065, #257317, #621, #34991 ) ) ;
#40600 = ORIENTED_EDGE ( 'NONE', *, *, #229178, .F. ) ;
#40601 = CARTESIAN_POINT ( 'NONE',  ( 18.42636655943174162, 85.49694431578303977, -163.4140269133687866 ) ) ;
#40602 = ORIENTED_EDGE ( 'NONE', *, *, #169333, .F. ) ;
#40603 = FACE_OUTER_BOUND ( 'NONE', #109562, .T. ) ;
#40604 = AXIS2_PLACEMENT_3D ( 'NONE', #163840, #107705, #248505 ) ;
#40606 = CARTESIAN_POINT ( 'NONE',  ( -21.05000000000000071, -11.64999999998884483, -103.5000000000000426 ) ) ;
#40605 = DIRECTION ( 'NONE',  ( 1.000000000000000000, 0.000000000000000000, 0.000000000000000000 ) ) ;
#40607 = ORIENTED_EDGE ( 'NONE', *, *, #48420, .T. ) ;
#40609 = ORIENTED_EDGE ( 'NONE', *, *, #88099, .T. ) ;
#40608 = ORIENTED_EDGE ( 'NONE', *, *, #214154, .T. ) ;
#40610 = LINE ( 'NONE', #157995, #81855 ) ;
#40611 = DIRECTION ( 'NONE',  ( 1.000000000000000000, -0.000000000000000000, 0.000000000000000000 ) ) ;
#40612 = ORIENTED_EDGE ( 'NONE', *, *, #12239, .T. ) ;
#40613 = TOROIDAL_SURFACE ( 'NONE', #207182, 4.099999999999999645, 0.1000000000000000056 ) ;
#40614 = CIRCLE ( 'NONE', #236391, 0.09999999999999543976 ) ;
#40615 = EDGE_CURVE ( 'NONE', #181967, #31330, #237353, .T. ) ;
#40616 = EDGE_CURVE ( 'NONE', #163148, #138064, #41736, .T. ) ;
#40617 = ORIENTED_EDGE ( 'NONE', *, *, #61009, .F. ) ;
#40618 = FACE_OUTER_BOUND ( 'NONE', #211330, .T. ) ;
#40619 = CIRCLE ( 'NONE', #169631, 0.1000000000000028644 ) ;
#40620 = EDGE_LOOP ( 'NONE', ( #39447, #107649, #31251, #111667 ) ) ;
#40621 = EDGE_LOOP ( 'NONE', ( #20070, #186766, #170897 ) ) ;
#40622 = EDGE_CURVE ( 'NONE', #116420, #13877, #62568, .T. ) ;
#40623 = DIRECTION ( 'NONE',  ( 1.000000000000000000, 0.000000000000000000, 0.000000000000000000 ) ) ;
#40624 = VECTOR ( 'NONE', #86802, 1000.000000000000000 ) ;
#40625 = VERTEX_POINT ( 'NONE', #217758 ) ;
#40626 = DIRECTION ( 'NONE',  ( 1.000000000000000000, 7.304098846218134667E-16, -0.000000000000000000 ) ) ;
#40627 = CARTESIAN_POINT ( 'NONE',  ( -20.64999999999999858, 7.250000000011155521, -54.65000000000000568 ) ) ;
#40628 = EDGE_LOOP ( 'NONE', ( #75369, #222730, #246077, #5907 ) ) ;
#40629 = CARTESIAN_POINT ( 'NONE',  ( 23.14999999999999858, 56.06656052939784729, -228.0911609752645290 ) ) ;
#40630 = DIRECTION ( 'NONE',  ( 0.000000000000000000, 0.000000000000000000, -1.000000000000000000 ) ) ;
#40632 = CARTESIAN_POINT ( 'NONE',  ( -16.77308656112214180, 9.950000000011135270, -121.3498068082977284 ) ) ;
#40631 = FACE_OUTER_BOUND ( 'NONE', #29424, .T. ) ;
#40633 = CARTESIAN_POINT ( 'NONE',  ( -21.05000000000000071, 14.90151243843701856, -203.3975529985363551 ) ) ;
#40634 = DIRECTION ( 'NONE',  ( -0.000000000000000000, 6.982962677686266711E-15, -1.000000000000000000 ) ) ;
#40635 = DIRECTION ( 'NONE',  ( 0.000000000000000000, 0.9998779222360102414, 0.01562499999996356907 ) ) ;
#40637 = EDGE_CURVE ( 'NONE', #240241, #91489, #107518, .T. ) ;
#40636 = PLANE ( 'NONE',  #48998 ) ;
#40638 = CARTESIAN_POINT ( 'NONE',  ( 18.69999999999999929, -10.80884033489985363, 6.100000000000002309 ) ) ;
#40639 = CARTESIAN_POINT ( 'NONE',  ( 18.59999999999999787, -10.63400887967554986, 6.002871413764276909 ) ) ;
#40640 = ADVANCED_FACE ( 'NONE', ( #19595 ), #99091, .F. ) ;
#40641 = AXIS2_PLACEMENT_3D ( 'NONE', #251417, #72812, #113190 ) ;
#40642 = ORIENTED_EDGE ( 'NONE', *, *, #242926, .F. ) ;
#40643 = AXIS2_PLACEMENT_3D ( 'NONE', #222337, #42444, #25471 ) ;
#40645 = ORIENTED_EDGE ( 'NONE', *, *, #1344, .T. ) ;
#40644 = ORIENTED_EDGE ( 'NONE', *, *, #219814, .T. ) ;
#40646 = ORIENTED_EDGE ( 'NONE', *, *, #69648, .F. ) ;
#40647 = ORIENTED_EDGE ( 'NONE', *, *, #115299, .T. ) ;
#40648 = VECTOR ( 'NONE', #79576, 1000.000000000000000 ) ;
#40649 = LINE ( 'NONE', #198392, #257057 ) ;
#40650 = CARTESIAN_POINT ( 'NONE',  ( -21.05000000000000071, 5.900000000000005684, -23.28090023534362629 ) ) ;
#40651 = EDGE_CURVE ( 'NONE', #215460, #1615, #74626, .T. ) ;
#40652 = AXIS2_PLACEMENT_3D ( 'NONE', #234517, #55854, #96277 ) ;
#40654 = DIRECTION ( 'NONE',  ( 1.000000000000000000, 0.000000000000000000, 0.000000000000000000 ) ) ;
#40653 = CARTESIAN_POINT ( 'NONE',  ( 18.59999999999999076, 77.16412189325330928, -128.6082593989527254 ) ) ;
#40655 = ADVANCED_FACE ( 'NONE', ( #106807 ), #49457, .T. ) ;
#40656 = FACE_OUTER_BOUND ( 'NONE', #196836, .T. ) ;
#40657 = EDGE_LOOP ( 'NONE', ( #246281, #68885, #107629, #200299 ) ) ;
#40658 = CARTESIAN_POINT ( 'NONE',  ( 18.49999999999999289, 69.35000000001222986, -148.8731074845244109 ) ) ;
#40659 = FACE_OUTER_BOUND ( 'NONE', #45671, .T. ) ;
#40660 = CARTESIAN_POINT ( 'NONE',  ( 23.24999999999999645, 70.40000000001204228, -114.7731074845243455 ) ) ;
#40661 = LINE ( 'NONE', #97992, #178891 ) ;
#40662 = ORIENTED_EDGE ( 'NONE', *, *, #1169, .T. ) ;
#40663 = CIRCLE ( 'NONE', #98833, 0.2000000000000057288 ) ;
#40664 = AXIS2_PLACEMENT_3D ( 'NONE', #103216, #107081, #124103 ) ;
#40665 = AXIS2_PLACEMENT_3D ( 'NONE', #218313, #100909, #239186 ) ;
#40666 = DIRECTION ( 'NONE',  ( 0.000000000000000000, 0.000000000000000000, 1.000000000000000000 ) ) ;
#40667 = CARTESIAN_POINT ( 'NONE',  ( -21.07954763557533084, 0.06587591862964220502, -94.17070900996139926 ) ) ;
#40668 = ORIENTED_EDGE ( 'NONE', *, *, #214068, .F. ) ;
#40669 = CARTESIAN_POINT ( 'NONE',  ( 23.15000000000000213, -9.500000000000000000, -23.60603087734755690 ) ) ;
#40670 = CARTESIAN_POINT ( 'NONE',  ( -21.05000000000000071, 76.00000000001195133, -103.0231074845243171 ) ) ;
#40671 = LINE ( 'NONE', #101855, #110898 ) ;
#40672 = DIRECTION ( 'NONE',  ( 0.000000000000000000, 0.000000000000000000, -1.000000000000000000 ) ) ;
#40673 = ORIENTED_EDGE ( 'NONE', *, *, #47951, .F. ) ;
#40674 = CARTESIAN_POINT ( 'NONE',  ( 18.42555734704284376, 46.96631509381553116, -255.3401978472650740 ) ) ;
#40675 = DIRECTION ( 'NONE',  ( 1.441126678808781001E-14, -0.9876197685951241256, -0.1568667991644932258 ) ) ;
#40676 = PLANE ( 'NONE',  #54160 ) ;
#40678 = LINE ( 'NONE', #223112, #166244 ) ;
#40677 = DIRECTION ( 'NONE',  ( 0.000000000000000000, 0.2617529984164915779, 0.9651348961777189706 ) ) ;
#40679 = LINE ( 'NONE', #156760, #20725 ) ;
#40680 = VECTOR ( 'NONE', #144807, 1000.000000000000000 ) ;
#40681 = CARTESIAN_POINT ( 'NONE',  ( -18.59999999999999787, 61.43991280424057777, -221.4883200034892923 ) ) ;
#40682 = DIRECTION ( 'NONE',  ( 1.000000000000000000, 0.000000000000000000, 0.000000000000000000 ) ) ;
#40684 = CARTESIAN_POINT ( 'NONE',  ( 22.40736611211992368, 76.00000000001203659, -114.6726782920691221 ) ) ;
#40683 = VECTOR ( 'NONE', #106084, 1000.000000000000000 ) ;
#40685 = VERTEX_POINT ( 'NONE', #84645 ) ;
#40686 = EDGE_CURVE ( 'NONE', #177487, #131118, #128570, .T. ) ;
#40687 = AXIS2_PLACEMENT_3D ( 'NONE', #98252, #141275, #79985 ) ;
#40688 = ORIENTED_EDGE ( 'NONE', *, *, #67321, .T. ) ;
#40689 = ORIENTED_EDGE ( 'NONE', *, *, #762, .T. ) ;
#40690 = FACE_OUTER_BOUND ( 'NONE', #54805, .T. ) ;
#40691 = AXIS2_PLACEMENT_3D ( 'NONE', #179728, #55885, #238400 ) ;
#40692 = VECTOR ( 'NONE', #161573, 1000.000000000000000 ) ;
#40693 = AXIS2_PLACEMENT_3D ( 'NONE', #209316, #71123, #51504 ) ;
#40694 = CARTESIAN_POINT ( 'NONE',  ( -18.59117750673696889, 65.66751761918619934, -30.42826094061123854 ) ) ;
#40695 = VECTOR ( 'NONE', #67076, 1000.000000000000114 ) ;
#40696 = ADVANCED_FACE ( 'NONE', ( #7734 ), #164244, .F. ) ;
#40697 = DIRECTION ( 'NONE',  ( 0.000000000000000000, -6.982962677686266711E-15, 1.000000000000000000 ) ) ;
#40698 = EDGE_LOOP ( 'NONE', ( #212093, #226320, #11255, #249007 ) ) ;
#40699 = AXIS2_PLACEMENT_3D ( 'NONE', #63646, #203159, #66226 ) ;
#40700 = DIRECTION ( 'NONE',  ( 1.000000000000000000, 0.000000000000000000, 0.000000000000000000 ) ) ;
#40701 = DIRECTION ( 'NONE',  ( -0.000000000000000000, 0.000000000000000000, 1.000000000000000000 ) ) ;
#40702 = CARTESIAN_POINT ( 'NONE',  ( -22.39999999999999503, 76.00000000001200817, -110.8138870828977218 ) ) ;
#40703 = CARTESIAN_POINT ( 'NONE',  ( 20.94999999999999929, -9.499999999988848032, -76.89396912265249284 ) ) ;
#40705 = EDGE_LOOP ( 'NONE', ( #197155, #92790, #160202, #188458, #30999 ) ) ;
#40704 = CARTESIAN_POINT ( 'NONE',  ( -16.83233564386398839, 9.930221796595855466, -188.2245206634760564 ) ) ;
#40706 = LINE ( 'NONE', #2801, #13183 ) ;
#40707 = DIRECTION ( 'NONE',  ( 2.694716079187273439E-16, 0.9651348961777159730, -0.2617529984165023471 ) ) ;
#40708 = LINE ( 'NONE', #99328, #112608 ) ;
#40709 = ORIENTED_EDGE ( 'NONE', *, *, #143062, .T. ) ;
#40710 = VECTOR ( 'NONE', #218379, 999.9999999999998863 ) ;
#40711 = DIRECTION ( 'NONE',  ( 0.000000000000000000, 0.000000000000000000, 1.000000000000000000 ) ) ;
#40712 = DIRECTION ( 'NONE',  ( 0.000000000000000000, -6.982962677686266711E-15, 1.000000000000000000 ) ) ;
#40713 = CARTESIAN_POINT ( 'NONE',  ( 20.94999999999999929, 67.07338541492498507, -128.0514244653012383 ) ) ;
#40714 = ORIENTED_EDGE ( 'NONE', *, *, #241883, .T. ) ;
#40715 = DIRECTION ( 'NONE',  ( 1.000000000000000000, -0.000000000000000000, 0.000000000000000000 ) ) ;
#40716 = DIRECTION ( 'NONE',  ( 1.000000000000000000, 0.000000000000000000, 0.000000000000000000 ) ) ;
#40717 = ORIENTED_EDGE ( 'NONE', *, *, #27317, .F. ) ;
#40718 = AXIS2_PLACEMENT_3D ( 'NONE', #257167, #83678, #57724 ) ;
#40719 = CARTESIAN_POINT ( 'NONE',  ( 20.94999999999999574, 44.15969672213208241, -258.9565289832007693 ) ) ;
#40720 = FACE_OUTER_BOUND ( 'NONE', #8562, .T. ) ;
#40721 = DIRECTION ( 'NONE',  ( 0.000000000000000000, -7.429790795770647916E-15, 1.000000000000000000 ) ) ;
#40722 = EDGE_LOOP ( 'NONE', ( #220328, #19671, #183887, #7439 ) ) ;
#40723 = ORIENTED_EDGE ( 'NONE', *, *, #239867, .F. ) ;
#40724 = DIRECTION ( 'NONE',  ( -0.000000000000000000, -0.000000000000000000, -1.000000000000000000 ) ) ;
#40725 = FACE_OUTER_BOUND ( 'NONE', #54511, .T. ) ;
#40726 = CARTESIAN_POINT ( 'NONE',  ( -16.83558968593875349, 63.08251143331946054, -213.1394977529018036 ) ) ;
#40727 = EDGE_CURVE ( 'NONE', #139626, #215553, #69004, .T. ) ;
#40729 = CARTESIAN_POINT ( 'NONE',  ( 18.59999999999999076, 68.11887992016826843, -227.8068560890359890 ) ) ;
#40728 = CARTESIAN_POINT ( 'NONE',  ( -22.00356870072698712, 76.00000000002593481, -143.7773498462425437 ) ) ;
#40730 = AXIS2_PLACEMENT_3D ( 'NONE', #175730, #255177, #119602 ) ;
#40731 = AXIS2_PLACEMENT_3D ( 'NONE', #16618, #82950, #165095 ) ;
#40732 = CARTESIAN_POINT ( 'NONE',  ( -18.39999999999999858, 85.50000000001263345, -196.5238218066854472 ) ) ;
#40733 = CARTESIAN_POINT ( 'NONE',  ( -16.77683809663752257, 66.05416425680742520, -56.85915846542017960 ) ) ;
#40734 = AXIS2_PLACEMENT_3D ( 'NONE', #150994, #55692, #230535 ) ;
#40735 = ORIENTED_EDGE ( 'NONE', *, *, #125140, .F. ) ;
#40736 = DIRECTION ( 'NONE',  ( 0.000000000000000000, -6.982962677686266711E-15, 1.000000000000000000 ) ) ;
#40738 = ORIENTED_EDGE ( 'NONE', *, *, #192441, .T. ) ;
#40737 = CARTESIAN_POINT ( 'NONE',  ( 19.90000000000000568, 1.250000000000000000, 16.60000000000000142 ) ) ;
#40739 = CARTESIAN_POINT ( 'NONE',  ( 20.95556889135987788, 65.37805641227753028, -195.8807132626668874 ) ) ;
#40740 = FACE_OUTER_BOUND ( 'NONE', #76777, .T. ) ;
#40742 = DIRECTION ( 'NONE',  ( -0.000000000000000000, 0.8660254037844377084, 0.5000000000000016653 ) ) ;
#40741 = CARTESIAN_POINT ( 'NONE',  ( 12.25000000000000000, 66.15000000001204228, -119.7731074845243739 ) ) ;
#40743 = EDGE_CURVE ( 'NONE', #43270, #256108, #168348, .T. ) ;
#40744 = ORIENTED_EDGE ( 'NONE', *, *, #48738, .T. ) ;
#40746 = DIRECTION ( 'NONE',  ( 2.952720810173289112E-16, -1.000000000000000000, 0.000000000000000000 ) ) ;
#40745 = CARTESIAN_POINT ( 'NONE',  ( -16.77431908686106965, 66.05419424549359064, -56.85894670217464153 ) ) ;
#40747 = CARTESIAN_POINT ( 'NONE',  ( -18.50000000000000000, 9.150000000000002132, -12.34999999999999964 ) ) ;
#40748 = CARTESIAN_POINT ( 'NONE',  ( -12.25000000000000178, 66.15000000001258229, -186.7731074845244166 ) ) ;
#40749 = DIRECTION ( 'NONE',  ( -1.000000000000000000, -0.000000000000000000, -0.000000000000000000 ) ) ;
#40750 = CARTESIAN_POINT ( 'NONE',  ( -12.92414019175887141, 66.58236703690630520, -185.3741590187921986 ) ) ;
#40751 = EDGE_CURVE ( 'NONE', #68824, #98041, #153748, .T. ) ;
#40752 = ORIENTED_EDGE ( 'NONE', *, *, #154120, .T. ) ;
#40753 = CARTESIAN_POINT ( 'NONE',  ( -20.85000000000000142, 1.115600667400684642E-11, -134.0000000000000284 ) ) ;
#40754 = ORIENTED_EDGE ( 'NONE', *, *, #71512, .T. ) ;
#40755 = AXIS2_PLACEMENT_3D ( 'NONE', #246070, #45295, #186090 ) ;
#40757 = VECTOR ( 'NONE', #245662, 1000.000000000000000 ) ;
#40756 = DIRECTION ( 'NONE',  ( -0.000000000000000000, 0.000000000000000000, 1.000000000000000000 ) ) ;
#40758 = ADVANCED_FACE ( 'NONE', ( #188930 ), #187037, .T. ) ;
#40759 = VERTEX_POINT ( 'NONE', #245050 ) ;
#40760 = CARTESIAN_POINT ( 'NONE',  ( 18.59999999999999076, 74.75000000001188027, -95.02310748452431710 ) ) ;
#40761 = ORIENTED_EDGE ( 'NONE', *, *, #159184, .F. ) ;
#40763 = DIRECTION ( 'NONE',  ( -1.000000000000000000, 0.000000000000000000, 0.000000000000000000 ) ) ;
#40762 = CIRCLE ( 'NONE', #132671, 0.1000000000000028644 ) ;
#40764 = DIRECTION ( 'NONE',  ( 0.000000000000000000, -0.8660254037844377084, -0.5000000000000016653 ) ) ;
#40765 = EDGE_LOOP ( 'NONE', ( #174649, #139018, #130584, #202846 ) ) ;
#40766 = EDGE_CURVE ( 'NONE', #30748, #13858, #230668, .T. ) ;
#40767 = CARTESIAN_POINT ( 'NONE',  ( -22.57848426163147693, 76.00426432929513965, -114.7731657914146552 ) ) ;
#40768 = LINE ( 'NONE', #195972, #249086 ) ;
#40769 = DIRECTION ( 'NONE',  ( -1.000000000000000000, 0.000000000000000000, 0.000000000000000000 ) ) ;
#40770 = CARTESIAN_POINT ( 'NONE',  ( 22.50000000000000000, 12.54152817314149715, -223.4164406214577241 ) ) ;
#40771 = AXIS2_PLACEMENT_3D ( 'NONE', #252920, #32643, #89992 ) ;
#40772 = ORIENTED_EDGE ( 'NONE', *, *, #165006, .T. ) ;
#40773 = PLANE ( 'NONE',  #132473 ) ;
#40775 = ORIENTED_EDGE ( 'NONE', *, *, #19022, .T. ) ;
#40774 = CIRCLE ( 'NONE', #49101, 0.1000000000000055844 ) ;
#40777 = ORIENTED_EDGE ( 'NONE', *, *, #222705, .F. ) ;
#40776 = CARTESIAN_POINT ( 'NONE',  ( -23.15000000000000213, 1.115625160336667635E-11, -169.5000000000000284 ) ) ;
#40778 = ORIENTED_EDGE ( 'NONE', *, *, #84663, .F. ) ;
#40779 = DIRECTION ( 'NONE',  ( 0.000000000000000000, 1.000000000000000000, -0.000000000000000000 ) ) ;
#40780 = DIRECTION ( 'NONE',  ( 1.000000000000000000, -2.849773892568378313E-16, 7.728835255496647986E-17 ) ) ;
#40781 = CARTESIAN_POINT ( 'NONE',  ( 15.06592377766032342, 66.58221053306037618, -188.1657229405476812 ) ) ;
#40782 = DIRECTION ( 'NONE',  ( 0.000000000000000000, 0.000000000000000000, 1.000000000000000000 ) ) ;
#40783 = PLANE ( 'NONE',  #12586 ) ;
#40784 = ORIENTED_EDGE ( 'NONE', *, *, #125244, .F. ) ;
#40785 = LINE ( 'NONE', #120335, #147236 ) ;
#40786 = CIRCLE ( 'NONE', #136379, 0.1000000000000028644 ) ;
#40787 = CARTESIAN_POINT ( 'NONE',  ( -16.87372386987899020, 66.11939976637552263, -156.8738376126579794 ) ) ;
#40788 = ORIENTED_EDGE ( 'NONE', *, *, #45036, .T. ) ;
#40789 = CARTESIAN_POINT ( 'NONE',  ( 18.50000000000000355, -9.421456145484540912, -174.7419820840196110 ) ) ;
#40790 = CIRCLE ( 'NONE', #161382, 0.09999999999998986089 ) ;
#40791 = CARTESIAN_POINT ( 'NONE',  ( -16.97683810757273193, 9.950000000011137047, -80.26357671246051950 ) ) ;
#40792 = AXIS2_PLACEMENT_3D ( 'NONE', #13546, #134742, #53941 ) ;
#40793 = ORIENTED_EDGE ( 'NONE', *, *, #137161, .T. ) ;
#40794 = CIRCLE ( 'NONE', #244739, 4.000000000000003553 ) ;
#40795 = AXIS2_PLACEMENT_3D ( 'NONE', #210736, #227718, #67375 ) ;
#40796 = ADVANCED_FACE ( 'NONE', ( #207222 ), #242469, .F. ) ;
#40797 = CARTESIAN_POINT ( 'NONE',  ( 21.14999999999999858, 11.65000000000000746, -12.25000000000000000 ) ) ;
#40799 = ORIENTED_EDGE ( 'NONE', *, *, #12293, .F. ) ;
#40798 = AXIS2_PLACEMENT_3D ( 'NONE', #229802, #245533, #208959 ) ;
#40800 = FACE_OUTER_BOUND ( 'NONE', #6563, .T. ) ;
#40801 = CIRCLE ( 'NONE', #140718, 0.09999999999999520384 ) ;
#40802 = CARTESIAN_POINT ( 'NONE',  ( -21.05000000000000071, 18.60982576078065165, -226.6665746245395496 ) ) ;
#40803 = CARTESIAN_POINT ( 'NONE',  ( 20.85000000106584750, 64.25000000001249134, -176.8676028280509911 ) ) ;
#40804 = EDGE_CURVE ( 'NONE', #19956, #8721, #63847, .T. ) ;
#40805 = DIRECTION ( 'NONE',  ( 0.000000000000000000, -7.086529944415894657E-15, 1.000000000000000000 ) ) ;
#40806 = EDGE_CURVE ( 'NONE', #191837, #103845, #246336, .T. ) ;
#40807 = VECTOR ( 'NONE', #122850, 1000.000000000000000 ) ;
#40808 = VECTOR ( 'NONE', #182959, 1000.000000000000000 ) ;
#40809 = ORIENTED_EDGE ( 'NONE', *, *, #118889, .T. ) ;
#40810 = DIRECTION ( 'NONE',  ( 0.000000000000000000, 0.000000000000000000, 1.000000000000000000 ) ) ;
#40811 = CIRCLE ( 'NONE', #32440, 0.09999999999999158173 ) ;
#40812 = ORIENTED_EDGE ( 'NONE', *, *, #97194, .F. ) ;
#40813 = CIRCLE ( 'NONE', #161617, 4.299999999999970512 ) ;
#40814 = CARTESIAN_POINT ( 'NONE',  ( -16.92973740335338917, 12.44363429718260328, -211.1790690627998970 ) ) ;
#40815 = DIRECTION ( 'NONE',  ( 0.000000000000000000, -0.9126074666063660468, -0.4088369013363524762 ) ) ;
#40818 = EDGE_CURVE ( 'NONE', #193798, #90505, #191135, .T. ) ;
#40817 = VERTEX_POINT ( 'NONE', #147228 ) ;
#40816 = CARTESIAN_POINT ( 'NONE',  ( 20.99999999999999645, 66.25000000001207923, -123.8731074845243683 ) ) ;
#40819 = DIRECTION ( 'NONE',  ( 1.000000000000000000, 1.159508501126949537E-16, 2.525285885220370376E-17 ) ) ;
#40820 = TOROIDAL_SURFACE ( 'NONE', #165713, 0.6000000000000004219, 0.1000000000000000056 ) ;
#40821 = CARTESIAN_POINT ( 'NONE',  ( 18.39999999999999503, 62.23844973457045882, -209.3750075427748527 ) ) ;
#40822 = CARTESIAN_POINT ( 'NONE',  ( -20.93284271247462058, 64.25000000001148237, -43.03791325517833855 ) ) ;
#40823 = DIRECTION ( 'NONE',  ( -1.000000000000000000, -0.000000000000000000, -0.000000000000000000 ) ) ;
#40824 = EDGE_CURVE ( 'NONE', #34745, #216063, #132858, .T. ) ;
#40825 = EDGE_CURVE ( 'NONE', #41411, #184585, #111974, .T. ) ;
#40826 = CARTESIAN_POINT ( 'NONE',  ( -18.43473496883410334, 85.49495241101142540, -129.4772359122960097 ) ) ;
#40828 = VERTEX_POINT ( 'NONE', #195370 ) ;
#40827 = CARTESIAN_POINT ( 'NONE',  ( 21.13461538461538680, 67.11458296203782936, -157.6731074845244223 ) ) ;
#40829 = AXIS2_PLACEMENT_3D ( 'NONE', #73664, #208030, #13662 ) ;
#40830 = AXIS2_PLACEMENT_3D ( 'NONE', #7539, #83191, #25828 ) ;
#40831 = AXIS2_PLACEMENT_3D ( 'NONE', #215754, #196206, #17554 ) ;
#40833 = EDGE_CURVE ( 'NONE', #241985, #13269, #3648, .T. ) ;
#40832 = FACE_OUTER_BOUND ( 'NONE', #126165, .T. ) ;
#40834 = ORIENTED_EDGE ( 'NONE', *, *, #134216, .T. ) ;
#40835 = ORIENTED_EDGE ( 'NONE', *, *, #97709, .T. ) ;
#40837 = EDGE_CURVE ( 'NONE', #211434, #157387, #72865, .T. ) ;
#40836 = DIRECTION ( 'NONE',  ( 0.000000000000000000, 0.000000000000000000, -1.000000000000000000 ) ) ;
#40838 = FACE_OUTER_BOUND ( 'NONE', #144431, .T. ) ;
#40839 = EDGE_CURVE ( 'NONE', #10632, #138584, #170308, .T. ) ;
#40840 = VERTEX_POINT ( 'NONE', #134073 ) ;
#40841 = CARTESIAN_POINT ( 'NONE',  ( -20.94999999999999929, -0.2561057920810652089, -66.96510355832775474 ) ) ;
#40842 = MECHANICAL_DESIGN_GEOMETRIC_PRESENTATION_REPRESENTATION (  '', ( #240721 ), #244996 ) ;
#40843 = AXIS2_PLACEMENT_3D ( 'NONE', #231769, #99591, #137446 ) ;
#40844 = ORIENTED_EDGE ( 'NONE', *, *, #51324, .T. ) ;
#40845 = LINE ( 'NONE', #78637, #27117 ) ;
#40847 = CARTESIAN_POINT ( 'NONE',  ( -16.93970660449832621, 65.98715860837702962, -190.9708257487299363 ) ) ;
#40846 = AXIS2_PLACEMENT_3D ( 'NONE', #133273, #168596, #108572 ) ;
#40848 = VERTEX_POINT ( 'NONE', #91108 ) ;
#40849 = ORIENTED_EDGE ( 'NONE', *, *, #67596, .T. ) ;
#40850 = DIRECTION ( 'NONE',  ( 0.000000000000000000, 0.8814952561688428334, -0.4721928772777350125 ) ) ;
#40851 = EDGE_CURVE ( 'NONE', #25217, #231047, #130221, .T. ) ;
#40852 = ORIENTED_EDGE ( 'NONE', *, *, #184710, .T. ) ;
#40853 = ADVANCED_FACE ( 'NONE', ( #152399 ), #20431, .T. ) ;
#40854 = DIRECTION ( 'NONE',  ( 0.000000000000000000, -7.189901751995755791E-15, 1.000000000000000000 ) ) ;
#40855 = ORIENTED_EDGE ( 'NONE', *, *, #181263, .T. ) ;
#40857 = EDGE_LOOP ( 'NONE', ( #246100, #4955, #187784, #221685 ) ) ;
#40856 = DIRECTION ( 'NONE',  ( 1.476360405086644309E-16, 1.000000000000000000, 0.000000000000000000 ) ) ;
#40858 = AXIS2_PLACEMENT_3D ( 'NONE', #239692, #216257, #218821 ) ;
#40859 = FACE_OUTER_BOUND ( 'NONE', #22464, .T. ) ;
#40860 = ORIENTED_EDGE ( 'NONE', *, *, #160629, .F. ) ;
#40861 = CARTESIAN_POINT ( 'NONE',  ( -21.07094088545368749, 0.09889370256337755294, -94.17983277808291120 ) ) ;
#40862 = AXIS2_PLACEMENT_3D ( 'NONE', #8588, #168986, #165091 ) ;
#40863 = ORIENTED_EDGE ( 'NONE', *, *, #90302, .T. ) ;
#40866 = EDGE_CURVE ( 'NONE', #98041, #185124, #248912, .T. ) ;
#40865 = ORIENTED_EDGE ( 'NONE', *, *, #218623, .F. ) ;
#40864 = EDGE_LOOP ( 'NONE', ( #214713, #130037, #198658, #182820 ) ) ;
#40867 = CARTESIAN_POINT ( 'NONE',  ( -18.59999999999999787, 1.835341550235567887, -78.55515129256302487 ) ) ;
#40868 = VECTOR ( 'NONE', #14835, 1000.000000000000000 ) ;
#40869 = VERTEX_POINT ( 'NONE', #170700 ) ;
#40870 = FACE_OUTER_BOUND ( 'NONE', #141950, .T. ) ;
#40871 = ORIENTED_EDGE ( 'NONE', *, *, #115526, .F. ) ;
#40872 = AXIS2_PLACEMENT_3D ( 'NONE', #20387, #156059, #154770 ) ;
#40873 = ORIENTED_EDGE ( 'NONE', *, *, #141451, .T. ) ;
#40874 = FACE_OUTER_BOUND ( 'NONE', #248392, .T. ) ;
#40875 = DIRECTION ( 'NONE',  ( 1.000000000000000000, 0.000000000000000000, 0.000000000000000000 ) ) ;
#40877 = ORIENTED_EDGE ( 'NONE', *, *, #6994, .T. ) ;
#40876 = SPHERICAL_SURFACE ( 'NONE', #224069, 0.1000000000000000056 ) ;
#40878 = DIRECTION ( 'NONE',  ( -0.000000000000000000, 0.000000000000000000, 1.000000000000000000 ) ) ;
#40879 = ORIENTED_EDGE ( 'NONE', *, *, #104510, .T. ) ;
#40880 = CARTESIAN_POINT ( 'NONE',  ( -18.50000324121759121, 65.70692517833255408, -131.0644653378303985 ) ) ;
#40881 = CARTESIAN_POINT ( 'NONE',  ( -20.94999999999999929, -1.162701749926853712, -108.6000000000000227 ) ) ;
#40882 = CIRCLE ( 'NONE', #119993, 0.1999999999999987899 ) ;
#40884 = ORIENTED_EDGE ( 'NONE', *, *, #92717, .T. ) ;
#40883 = ADVANCED_FACE ( 'NONE', ( #251460 ), #229352, .T. ) ;
#40885 = DIRECTION ( 'NONE',  ( -0.000000000000000000, 0.1298341882520022694, 0.9915357197604853789 ) ) ;
#40886 = CARTESIAN_POINT ( 'NONE',  ( 21.05000000000000071, 65.51556651037034840, -129.0663016830324352 ) ) ;
#40887 = EDGE_CURVE ( 'NONE', #192176, #205125, #214904, .T. ) ;
#40888 = ORIENTED_EDGE ( 'NONE', *, *, #76086, .F. ) ;
#40889 = CARTESIAN_POINT ( 'NONE',  ( 20.94999999999999929, 65.65271564877468791, -222.5736063831752176 ) ) ;
#40890 = ORIENTED_EDGE ( 'NONE', *, *, #120897, .T. ) ;
#40892 = EDGE_LOOP ( 'NONE', ( #62664, #146042, #207128, #78973 ) ) ;
#40891 = CIRCLE ( 'NONE', #244848, 0.09999999999999939493 ) ;
#40893 = CARTESIAN_POINT ( 'NONE',  ( -23.15000000000000213, 87.75000000001213607, -136.5231074845242176 ) ) ;
#40894 = EDGE_CURVE ( 'NONE', #225601, #74869, #14168, .T. ) ;
#40895 = ORIENTED_EDGE ( 'NONE', *, *, #119972, .T. ) ;
#40896 = ORIENTED_EDGE ( 'NONE', *, *, #103625, .T. ) ;
#40898 = ADVANCED_FACE ( 'NONE', ( #153711 ), #253626, .T. ) ;
#40897 = DIRECTION ( 'NONE',  ( 0.000000000000000000, 0.000000000000000000, -1.000000000000000000 ) ) ;
#40899 = DIRECTION ( 'NONE',  ( -1.836970198721029934E-16, -1.000000000000000000, -6.982962677686266711E-15 ) ) ;
#40900 = ORIENTED_EDGE ( 'NONE', *, *, #25852, .F. ) ;
#40901 = VERTEX_POINT ( 'NONE', #233213 ) ;
#40902 = CARTESIAN_POINT ( 'NONE',  ( -23.15000000000000213, 87.75000000001267608, -203.5231074845243029 ) ) ;
#40903 = EDGE_CURVE ( 'NONE', #222175, #101212, #78657, .T. ) ;
#40904 = DIRECTION ( 'NONE',  ( 1.000000000000000000, 0.000000000000000000, 0.000000000000000000 ) ) ;
#40905 = EDGE_LOOP ( 'NONE', ( #45967, #234576, #42753, #50948, #174946 ) ) ;
#40906 = ORIENTED_EDGE ( 'NONE', *, *, #18394, .T. ) ;
#40907 = TOROIDAL_SURFACE ( 'NONE', #232440, 7.800000000000000711, 0.1000000000000000056 ) ;
#40908 = CIRCLE ( 'NONE', #207488, 0.09999999999999939493 ) ;
#40909 = VECTOR ( 'NONE', #34803, 1000.000000000000000 ) ;
#40910 = ORIENTED_EDGE ( 'NONE', *, *, #197142, .F. ) ;
#40911 = EDGE_CURVE ( 'NONE', #53303, #213938, #87018, .T. ) ;
#40912 = EDGE_CURVE ( 'NONE', #158624, #120448, #65770, .T. ) ;
#40913 = CARTESIAN_POINT ( 'NONE',  ( -16.87036670365548474, 66.01058118071014746, -82.04354736722233099 ) ) ;
#40914 = CARTESIAN_POINT ( 'NONE',  ( 18.59999999999999787, 85.32100840337393777, -196.2871692354464130 ) ) ;
#40915 = EDGE_CURVE ( 'NONE', #213961, #191338, #224412, .T. ) ;
#40916 = CARTESIAN_POINT ( 'NONE',  ( 18.59999999999999787, 77.85102823015243700, -57.86919421510181394 ) ) ;
#40917 = DIRECTION ( 'NONE',  ( 1.476360405086644309E-16, 1.000000000000000000, 1.445602896647339410E-16 ) ) ;
#40918 = FACE_OUTER_BOUND ( 'NONE', #252249, .T. ) ;
#40919 = FACE_OUTER_BOUND ( 'NONE', #110525, .T. ) ;
#40920 = LINE ( 'NONE', #98249, #106937 ) ;
#40923 = CARTESIAN_POINT ( 'NONE',  ( 21.07954763557290079, 34.01115785052155616, -243.8019369918546317 ) ) ;
#40922 = AXIS2_PLACEMENT_3D ( 'NONE', #145218, #103516, #147811 ) ;
#40921 = DIRECTION ( 'NONE',  ( 0.000000000000000000, -6.982962677686266711E-15, 1.000000000000000000 ) ) ;
#40924 = CARTESIAN_POINT ( 'NONE',  ( -20.65000000000000568, 7.250000000011138646, -76.25000000000004263 ) ) ;
#40925 = FACE_OUTER_BOUND ( 'NONE', #97657, .T. ) ;
#40926 = AXIS2_PLACEMENT_3D ( 'NONE', #179007, #197244, #21209 ) ;
#40927 = CARTESIAN_POINT ( 'NONE',  ( -20.54999999999999716, 4.250000000011156409, -112.8500000000000369 ) ) ;
#40928 = SPHERICAL_SURFACE ( 'NONE', #192722, 0.1000000000000000056 ) ;
#40929 = ADVANCED_FACE ( 'NONE', ( #16723 ), #7957, .F. ) ;
#40930 = EDGE_CURVE ( 'NONE', #156961, #127685, #240993, .T. ) ;
#40931 = VERTEX_POINT ( 'NONE', #96231 ) ;
#40932 = TOROIDAL_SURFACE ( 'NONE', #190952, 3.899999999999999467, 0.1000000000000000056 ) ;
#40933 = ADVANCED_FACE ( 'NONE', ( #139192 ), #157546, .F. ) ;
#40935 = VERTEX_POINT ( 'NONE', #221300 ) ;
#40934 = FACE_OUTER_BOUND ( 'NONE', #17914, .T. ) ;
#40936 = EDGE_CURVE ( 'NONE', #175804, #177617, #205557, .T. ) ;
#40937 = DIRECTION ( 'NONE',  ( -0.5932847527679310229, -0.3291107096594071413, 0.7346423231209704419 ) ) ;
#40938 = DIRECTION ( 'NONE',  ( 0.000000000000000000, 0.000000000000000000, -1.000000000000000000 ) ) ;
#40939 = EDGE_CURVE ( 'NONE', #729, #202471, #175801, .T. ) ;
#40940 = ORIENTED_EDGE ( 'NONE', *, *, #132202, .F. ) ;
#40941 = DIRECTION ( 'NONE',  ( 0.000000000000000000, 0.008583690987128059571, -0.9999631594459056361 ) ) ;
#40942 = AXIS2_PLACEMENT_3D ( 'NONE', #242345, #225330, #121157 ) ;
#40943 = CARTESIAN_POINT ( 'NONE',  ( 20.94999999999999929, 67.22371710471961137, -127.9644784893834100 ) ) ;
#40944 = ORIENTED_EDGE ( 'NONE', *, *, #164843, .T. ) ;
#40945 = CIRCLE ( 'NONE', #182593, 0.1000000000000002554 ) ;
#40946 = AXIS2_PLACEMENT_3D ( 'NONE', #213562, #255206, #76621 ) ;
#40947 = DIRECTION ( 'NONE',  ( 1.000000000000000000, 0.000000000000000000, 0.000000000000000000 ) ) ;
#40948 = CARTESIAN_POINT ( 'NONE',  ( -18.40000000000000213, 70.35000000001255671, -182.6731074845243938 ) ) ;
#40949 = CARTESIAN_POINT ( 'NONE',  ( 17.23472005113826810, 52.56455255973604324, -231.1306584961272392 ) ) ;
#40950 = EDGE_CURVE ( 'NONE', #211293, #168251, #118385, .T. ) ;
#40951 = DIRECTION ( 'NONE',  ( -1.836970198721029934E-16, 1.000000000000000000, 0.000000000000000000 ) ) ;
#40953 = VERTEX_POINT ( 'NONE', #120968 ) ;
#40952 = CARTESIAN_POINT ( 'NONE',  ( 20.85000000000000142, 77.85161776048073534, -91.41991776492061206 ) ) ;
#40954 = CIRCLE ( 'NONE', #78332, 0.1000000000000070832 ) ;
#40956 = ORIENTED_EDGE ( 'NONE', *, *, #54609, .F. ) ;
#40955 = CARTESIAN_POINT ( 'NONE',  ( 20.94999999999999574, -11.74999999998883560, -36.39999999999999858 ) ) ;
#40957 = DIRECTION ( 'NONE',  ( 1.000000000000000000, 0.000000000000000000, 0.000000000000000000 ) ) ;
#40958 = DIRECTION ( 'NONE',  ( 0.000000000000000000, 0.8814952561688437216, -0.4721928772777334582 ) ) ;
#40959 = CARTESIAN_POINT ( 'NONE',  ( 23.24999999999999645, 1.115600667400684642E-11, -100.5000000000000426 ) ) ;
#40960 = CARTESIAN_POINT ( 'NONE',  ( -13.22483237240079745, 9.436674251854007878, -182.6768619309992232 ) ) ;
#40961 = EDGE_CURVE ( 'NONE', #41172, #24254, #178675, .T. ) ;
#40962 = DIRECTION ( 'NONE',  ( 0.000000000000000000, 0.000000000000000000, 1.000000000000000000 ) ) ;
#40963 = CARTESIAN_POINT ( 'NONE',  ( -18.50000000000000000, 76.00000000001237765, -170.0231074845243597 ) ) ;
#40964 = CARTESIAN_POINT ( 'NONE',  ( 20.94999999999999929, 76.00000000001244871, -170.0231074845243597 ) ) ;
#40965 = DIRECTION ( 'NONE',  ( 0.000000000000000000, -0.2617529984165031243, -0.9651348961777157509 ) ) ;
#40966 = AXIS2_PLACEMENT_3D ( 'NONE', #181613, #159479, #81190 ) ;
#40967 = DIRECTION ( 'NONE',  ( -1.000000000000000000, 0.000000000000000000, 0.000000000000000000 ) ) ;
#40968 = VECTOR ( 'NONE', #138859, 1000.000000000000000 ) ;
#40969 = ORIENTED_EDGE ( 'NONE', *, *, #227253, .F. ) ;
#40970 = CARTESIAN_POINT ( 'NONE',  ( -20.64999999999999858, 85.00000000001188027, -93.12913836187181005 ) ) ;
#40971 = CIRCLE ( 'NONE', #136600, 0.1000000000000002554 ) ;
#40972 = VERTEX_POINT ( 'NONE', #17979 ) ;
#40973 = VERTEX_POINT ( 'NONE', #97492 ) ;
#40974 = EDGE_CURVE ( 'NONE', #208826, #88741, #2255, .T. ) ;
#40975 = CARTESIAN_POINT ( 'NONE',  ( 20.74625933824084001, 67.11708647892760382, -94.46793646040403303 ) ) ;
#40976 = DIRECTION ( 'NONE',  ( -1.000000000000000000, -0.000000000000000000, 0.000000000000000000 ) ) ;
#40977 = ORIENTED_EDGE ( 'NONE', *, *, #52301, .T. ) ;
#40978 = VECTOR ( 'NONE', #232186, 1000.000000000000000 ) ;
#40979 = VERTEX_POINT ( 'NONE', #119670 ) ;
#40980 = AXIS2_PLACEMENT_3D ( 'NONE', #243753, #144641, #139506 ) ;
#40981 = EDGE_CURVE ( 'NONE', #231084, #149228, #214939, .T. ) ;
#40982 = ORIENTED_EDGE ( 'NONE', *, *, #63294, .T. ) ;
#40983 = CIRCLE ( 'NONE', #27963, 0.09999999999999817368 ) ;
#40984 = VERTEX_POINT ( 'NONE', #77948 ) ;
#40986 = DIRECTION ( 'NONE',  ( 1.000000000000000000, 0.000000000000000000, 0.000000000000000000 ) ) ;
#40985 = CIRCLE ( 'NONE', #215901, 0.1000000000000028644 ) ;
#40987 = DIRECTION ( 'NONE',  ( -0.000000000000000000, 7.172728831056617961E-15, -1.000000000000000000 ) ) ;
#40988 = DIRECTION ( 'NONE',  ( 0.000000000000000000, 6.982962677686266711E-15, -1.000000000000000000 ) ) ;
#40989 = AXIS2_PLACEMENT_3D ( 'NONE', #170096, #228755, #94347 ) ;
#40990 = AXIS2_PLACEMENT_3D ( 'NONE', #38051, #117558, #232398 ) ;
#40991 = FACE_OUTER_BOUND ( 'NONE', #183377, .T. ) ;
#40992 = DIRECTION ( 'NONE',  ( -0.000000000000000000, 0.8814952561688430555, -0.4721928772777346239 ) ) ;
#40993 = AXIS2_PLACEMENT_3D ( 'NONE', #111685, #15167, #32178 ) ;
#40994 =( BOUNDED_CURVE ( )  B_SPLINE_CURVE ( 3, ( #85380, #3292, #205350, #25463 ),
 .UNSPECIFIED., .F., .F. ) 
 B_SPLINE_CURVE_WITH_KNOTS ( ( 4, 4 ),
 ( 3.141592653589791784, 4.712388980384688786 ),
 .UNSPECIFIED. ) 
 CURVE ( )  GEOMETRIC_REPRESENTATION_ITEM ( )  RATIONAL_B_SPLINE_CURVE ( ( 1.000000000000000000, 0.8047378541243649375, 0.8047378541243649375, 1.000000000000000000 ) ) 
 REPRESENTATION_ITEM ( '' )  );
#40995 = DIRECTION ( 'NONE',  ( 0.000000000000000000, -0.9651348961777157509, 0.2617529984165031243 ) ) ;
#40996 = CARTESIAN_POINT ( 'NONE',  ( 21.05000000000000426, 75.98528214348816334, -142.8678308886149750 ) ) ;
#40998 = VERTEX_POINT ( 'NONE', #137917 ) ;
#40997 = CARTESIAN_POINT ( 'NONE',  ( -21.07928932188134041, 75.90110485435729970, -75.85162414091762173 ) ) ;
#41000 = CARTESIAN_POINT ( 'NONE',  ( -20.85000000000000142, 7.021664781911246322, -104.1335654018973287 ) ) ;
#40999 = CARTESIAN_POINT ( 'NONE',  ( -17.78241384945978965, 62.84018868124818624, -210.5733318916599046 ) ) ;
#41001 = AXIS2_PLACEMENT_3D ( 'NONE', #43286, #25026, #4144 ) ;
#41002 = CARTESIAN_POINT ( 'NONE',  ( 20.94999999999999574, 11.62071067811865888, -26.63158334765902424 ) ) ;
#41003 = ORIENTED_EDGE ( 'NONE', *, *, #126003, .F. ) ;
#41004 = CARTESIAN_POINT ( 'NONE',  ( 23.25000000000000000, 85.00000000001188027, -93.12913836187181005 ) ) ;
#41005 = EDGE_LOOP ( 'NONE', ( #218032, #133068, #184152, #218135 ) ) ;
#41007 = DIRECTION ( 'NONE',  ( 0.000000000000000000, 0.000000000000000000, -1.000000000000000000 ) ) ;
#41006 = DIRECTION ( 'NONE',  ( 0.000000000000000000, -0.1568667991644355497, 0.9876197685951332295 ) ) ;
#41008 = CARTESIAN_POINT ( 'NONE',  ( 22.48660254037843842, 64.25000000001163869, -69.57310748452439952 ) ) ;
#41009 = VECTOR ( 'NONE', #6175, 1000.000000000000000 ) ;
#41011 = ORIENTED_EDGE ( 'NONE', *, *, #105237, .F. ) ;
#41010 = AXIS2_PLACEMENT_3D ( 'NONE', #96472, #59911, #157802 ) ;
#41012 = FACE_OUTER_BOUND ( 'NONE', #184869, .T. ) ;
#41013 = CARTESIAN_POINT ( 'NONE',  ( -22.39999999999999858, 1.115488181425289271E-11, -21.85042919245520210 ) ) ;
#41014 = CARTESIAN_POINT ( 'NONE',  ( -20.94999999999999929, 1.115600667400684642E-11, -88.80000000000003979 ) ) ;
#41015 = ORIENTED_EDGE ( 'NONE', *, *, #13996, .F. ) ;
#41016 = ADVANCED_FACE ( 'NONE', ( #197899 ), #82175, .T. ) ;
#41017 = FACE_OUTER_BOUND ( 'NONE', #171781, .T. ) ;
#41018 = CARTESIAN_POINT ( 'NONE',  ( -23.25000000000000000, -11.74999999998884448, -100.5000000000000426 ) ) ;
#41019 = DIRECTION ( 'NONE',  ( -0.000000000000000000, 6.982962677686266711E-15, -1.000000000000000000 ) ) ;
#41020 = AXIS2_PLACEMENT_3D ( 'NONE', #238593, #117369, #119965 ) ;
#41021 = CARTESIAN_POINT ( 'NONE',  ( -0.8999999999999986899, -12.25000000000000355, 26.00000000000000355 ) ) ;
#41022 = CARTESIAN_POINT ( 'NONE',  ( 0.9000000000000547562, 64.35000000001120668, -12.72310748452478890 ) ) ;
#41023 = VECTOR ( 'NONE', #27495, 1000.000000000000000 ) ;
#41025 = ORIENTED_EDGE ( 'NONE', *, *, #201726, .F. ) ;
#41024 = CARTESIAN_POINT ( 'NONE',  ( 21.05281448260627641, 8.776010158548784190, -179.6735579118114003 ) ) ;
#41026 = CARTESIAN_POINT ( 'NONE',  ( -20.85000000000000142, -11.65000000000000036, -33.50000000000000000 ) ) ;
#41027 = CARTESIAN_POINT ( 'NONE',  ( -22.39999999999999858, -0.1008583690987139431, 11.74956712348939192 ) ) ;
#41028 = FACE_OUTER_BOUND ( 'NONE', #216015, .T. ) ;
#41029 = CARTESIAN_POINT ( 'NONE',  ( 21.05000000000000071, 0.09779029131994770863, -94.24218538952391100 ) ) ;
#41030 = EDGE_CURVE ( 'NONE', #16193, #44391, #12067, .T. ) ;
#41031 = CARTESIAN_POINT ( 'NONE',  ( 21.05000000000000071, 8.776282895303632259, -134.0000000000000000 ) ) ;
#41033 = ORIENTED_EDGE ( 'NONE', *, *, #143030, .T. ) ;
#41032 = FACE_OUTER_BOUND ( 'NONE', #60795, .T. ) ;
#41034 = CARTESIAN_POINT ( 'NONE',  ( -20.54999999999999716, -8.730841121484170131, -157.9019252810156786 ) ) ;
#41035 = AXIS2_PLACEMENT_3D ( 'NONE', #469, #241671, #103418 ) ;
#41036 = CARTESIAN_POINT ( 'NONE',  ( -22.50000000000000000, 68.20922040163873135, -136.6231074845243540 ) ) ;
#41037 = DIRECTION ( 'NONE',  ( 0.000000000000000000, -1.000000000000000000, 0.000000000000000000 ) ) ;
#41038 = EDGE_CURVE ( 'NONE', #69740, #236913, #141772, .T. ) ;
#41039 = ORIENTED_EDGE ( 'NONE', *, *, #14714, .T. ) ;
#41040 = CARTESIAN_POINT ( 'NONE',  ( -23.25000000000000000, 1.115600667400684642E-11, -171.6499999999999773 ) ) ;
#41041 = CARTESIAN_POINT ( 'NONE',  ( -21.05000000000000071, 4.252251777740766236, -211.8999245327126744 ) ) ;
#41042 = AXIS2_PLACEMENT_3D ( 'NONE', #4412, #39730, #83910 ) ;
#41043 = AXIS2_PLACEMENT_3D ( 'NONE', #236, #159342, #137185 ) ;
#41044 = FACE_OUTER_BOUND ( 'NONE', #191359, .T. ) ;
#41045 = VECTOR ( 'NONE', #46263, 1000.000000000000000 ) ;
#41046 = CARTESIAN_POINT ( 'NONE',  ( -22.57848426163147693, -0.004264329271961095000, -88.74994169310971870 ) ) ;
#41047 = ADVANCED_FACE ( 'NONE', ( #182207 ), #47797, .T. ) ;
#41048 = AXIS2_PLACEMENT_3D ( 'NONE', #222686, #239712, #97590 ) ;
#41049 = CARTESIAN_POINT ( 'NONE',  ( 21.05000000000000071, 13.06362847850371622, -210.5896934006125889 ) ) ;
#41050 = VERTEX_POINT ( 'NONE', #243448 ) ;
#41051 = ORIENTED_EDGE ( 'NONE', *, *, #71482, .T. ) ;
#41052 = EDGE_CURVE ( 'NONE', #240102, #182294, #257673, .T. ) ;
#41053 = DIRECTION ( 'NONE',  ( 0.000000000000000000, -0.000000000000000000, 1.000000000000000000 ) ) ;
#41054 = DIRECTION ( 'NONE',  ( 1.000000000000000000, -0.000000000000000000, 0.000000000000000000 ) ) ;
#41055 = EDGE_CURVE ( 'NONE', #63728, #230402, #91146, .T. ) ;
#41056 = CYLINDRICAL_SURFACE ( 'NONE', #132940, 0.1000000000000124678 ) ;
#41057 = DIRECTION ( 'NONE',  ( -1.000000000000000000, 3.265361837132813093E-16, 2.280189983783949500E-30 ) ) ;
#41058 = ORIENTED_EDGE ( 'NONE', *, *, #183956, .F. ) ;
#41059 = ADVANCED_FACE ( 'NONE', ( #145622 ), #82917, .F. ) ;
#41060 = CARTESIAN_POINT ( 'NONE',  ( -18.40000000000000213, 64.51332499825484490, -179.2731074845244450 ) ) ;
#41061 = CIRCLE ( 'NONE', #220103, 0.09999999999999917288 ) ;
#41062 = CARTESIAN_POINT ( 'NONE',  ( -21.04999999999994387, 83.80000000001119531, -34.86056257560453986 ) ) ;
#41063 = ADVANCED_FACE ( 'NONE', ( #165202 ), #187349, .F. ) ;
#41064 = DIRECTION ( 'NONE',  ( -1.000000000000000000, -0.000000000000000000, -0.000000000000000000 ) ) ;
#41065 = LINE ( 'NONE', #201387, #112057 ) ;
#41066 = CARTESIAN_POINT ( 'NONE',  ( -23.15000000000000213, 64.25000000001203659, -114.7731074845243882 ) ) ;
#41067 = ORIENTED_EDGE ( 'NONE', *, *, #3109, .F. ) ;
#41069 = VERTEX_POINT ( 'NONE', #24435 ) ;
#41068 = DIRECTION ( 'NONE',  ( 0.000000000000000000, 0.000000000000000000, -1.000000000000000000 ) ) ;
#41070 = VERTEX_POINT ( 'NONE', #23149 ) ;
#41071 = CYLINDRICAL_SURFACE ( 'NONE', #98708, 0.5000000000000014433 ) ;
#41072 = ORIENTED_EDGE ( 'NONE', *, *, #26096, .F. ) ;
#41073 = CARTESIAN_POINT ( 'NONE',  ( 21.14999999999999858, 76.00000000001242029, -176.5637644362255969 ) ) ;
#41074 = DIRECTION ( 'NONE',  ( -1.000000000000000000, -0.000000000000000000, 0.000000000000000000 ) ) ;
#41075 = DIRECTION ( 'NONE',  ( -1.000000000000000000, 0.000000000000000000, 0.000000000000000000 ) ) ;
#41076 = ORIENTED_EDGE ( 'NONE', *, *, #105558, .F. ) ;
#41077 = DIRECTION ( 'NONE',  ( 0.000000000000000000, -0.1350103645451974088, 0.9908441862701587999 ) ) ;
#41078 = CARTESIAN_POINT ( 'NONE',  ( -23.15000000000000213, -4.831324760611774849, -184.4696969421987376 ) ) ;
#41079 = ORIENTED_EDGE ( 'NONE', *, *, #91786, .F. ) ;
#41080 = ADVANCED_FACE ( 'NONE', ( #49093 ), #253805, .T. ) ;
#41081 = CARTESIAN_POINT ( 'NONE',  ( 22.59999999999999432, 11.74956712350054566, -100.3991416309013260 ) ) ;
#41083 = ORIENTED_EDGE ( 'NONE', *, *, #154585, .F. ) ;
#41082 = CARTESIAN_POINT ( 'NONE',  ( -20.54999999999999716, 68.85000000001257092, -186.7731074845244166 ) ) ;
#41084 = FACE_OUTER_BOUND ( 'NONE', #7115, .T. ) ;
#41085 = CARTESIAN_POINT ( 'NONE',  ( 23.14999999999999858, 1.115600667400684642E-11, -100.5000000000000426 ) ) ;
#41086 = CIRCLE ( 'NONE', #74417, 0.09999999999999961697 ) ;
#41087 = AXIS2_PLACEMENT_3D ( 'NONE', #23920, #4309, #44748 ) ;
#41088 = AXIS2_PLACEMENT_3D ( 'NONE', #193361, #33037, #172552 ) ;
#41089 = ORIENTED_EDGE ( 'NONE', *, *, #122902, .T. ) ;
#41090 =( BOUNDED_CURVE ( )  B_SPLINE_CURVE ( 3, ( #227263, #186882, #145147, #107315 ),
 .UNSPECIFIED., .F., .F. ) 
 B_SPLINE_CURVE_WITH_KNOTS ( ( 4, 4 ),
 ( 1.570796326794924536, 3.141592653589987183 ),
 .UNSPECIFIED. ) 
 CURVE ( )  GEOMETRIC_REPRESENTATION_ITEM ( )  RATIONAL_B_SPLINE_CURVE ( ( 1.000000000000000000, 0.8047378541243258576, 0.8047378541243258576, 1.000000000000000000 ) ) 
 REPRESENTATION_ITEM ( '' )  );
#41091 = CARTESIAN_POINT ( 'NONE',  ( 20.94999999999999574, 1.736257131608553550, -179.0686523290174819 ) ) ;
#41093 = ADVANCED_FACE ( 'NONE', ( #247292 ), #128751, .T. ) ;
#41092 = CARTESIAN_POINT ( 'NONE',  ( -21.05000000000000071, 61.95000000001191154, -97.50941241376341395 ) ) ;
#41094 = AXIS2_PLACEMENT_3D ( 'NONE', #89065, #227298, #168670 ) ;
#41095 = DIRECTION ( 'NONE',  ( 1.000000000000000000, 0.000000000000000000, 0.000000000000000000 ) ) ;
#41096 = ORIENTED_EDGE ( 'NONE', *, *, #229460, .F. ) ;
#41097 = CARTESIAN_POINT ( 'NONE',  ( -20.07928932188135107, 30.21456143932739380, -235.6387872333241660 ) ) ;
#41098 = CARTESIAN_POINT ( 'NONE',  ( -20.94999999999999929, 67.67657779757796277, -227.9615671787948372 ) ) ;
#41099 = CARTESIAN_POINT ( 'NONE',  ( 18.57071067811864040, 14.46815956487128574, -219.5971177848713864 ) ) ;
#41100 = VERTEX_POINT ( 'NONE', #144322 ) ;
#41101 = VECTOR ( 'NONE', #175984, 1000.000000000000000 ) ;
#41102 = AXIS2_PLACEMENT_3D ( 'NONE', #18297, #140819, #181247 ) ;
#41103 = ADVANCED_FACE ( 'NONE', ( #227733 ), #4813, .T. ) ;
#41104 = ADVANCED_FACE ( 'NONE', ( #7398, #45253 ), #148201, .F. ) ;
#41105 = AXIS2_PLACEMENT_3D ( 'NONE', #141304, #5612, #124315 ) ;
#41106 = ORIENTED_EDGE ( 'NONE', *, *, #45106, .T. ) ;
#41107 = VERTEX_POINT ( 'NONE', #102627 ) ;
#41108 = CARTESIAN_POINT ( 'NONE',  ( -21.05000000000000071, 67.23127455305841238, -235.8551265064783991 ) ) ;
#41109 = CARTESIAN_POINT ( 'NONE',  ( 13.40000000000005898, 67.75000000001118394, -21.02310748452479316 ) ) ;
#41112 = EDGE_CURVE ( 'NONE', #238489, #51379, #166376, .T. ) ;
#41111 = VERTEX_POINT ( 'NONE', #105177 ) ;
#41110 = CARTESIAN_POINT ( 'NONE',  ( -19.89999999999999858, 1.350000000000000089, 22.00000000000000355 ) ) ;
#41113 = CARTESIAN_POINT ( 'NONE',  ( 21.05000000000000071, 87.75000000001210765, -133.6231074845242119 ) ) ;
#41114 = DIRECTION ( 'NONE',  ( 0.000000000000000000, -1.734723475983068283E-15, 1.000000000000000000 ) ) ;
#41115 = LINE ( 'NONE', #217129, #164459 ) ;
#41116 = DIRECTION ( 'NONE',  ( -1.000000000000000000, -1.836970198721029934E-16, 0.000000000000000000 ) ) ;
#41117 = EDGE_CURVE ( 'NONE', #192810, #75563, #6108, .T. ) ;
#41118 = CYLINDRICAL_SURFACE ( 'NONE', #251243, 0.1000000000000000611 ) ;
#41119 = EDGE_CURVE ( 'NONE', #19733, #56467, #233000, .T. ) ;
#41121 = VERTEX_POINT ( 'NONE', #126056 ) ;
#41120 = DIRECTION ( 'NONE',  ( 0.000000000000000000, -1.000000000000000000, 0.000000000000000000 ) ) ;
#41123 = EDGE_LOOP ( 'NONE', ( #66344, #93412, #64226, #34772 ) ) ;
#41122 = DIRECTION ( 'NONE',  ( 0.000000000000000000, -0.8814952561688476074, 0.4721928772777262417 ) ) ;
#41124 = CARTESIAN_POINT ( 'NONE',  ( -18.40000000000000213, 11.75000000001113953, -113.1500000000000341 ) ) ;
#41125 = ORIENTED_EDGE ( 'NONE', *, *, #11936, .T. ) ;
#41126 = TOROIDAL_SURFACE ( 'NONE', #232657, 0.4000000000000005773, 0.1000000000000000056 ) ;
#41127 = ORIENTED_EDGE ( 'NONE', *, *, #60134, .F. ) ;
#41128 = CARTESIAN_POINT ( 'NONE',  ( -18.56579813702276027, 10.33025634372637569, -106.0870929282639423 ) ) ;
#41129 = DIRECTION ( 'NONE',  ( 0.000000000000000000, -1.000000000000000000, -1.897661533703519897E-16 ) ) ;
#41130 = AXIS2_PLACEMENT_3D ( 'NONE', #154607, #213250, #34651 ) ;
#41132 = EDGE_CURVE ( 'NONE', #198087, #143067, #67385, .T. ) ;
#41131 = DIRECTION ( 'NONE',  ( 0.000000000000000000, 0.000000000000000000, -1.000000000000000000 ) ) ;
#41133 = DIRECTION ( 'NONE',  ( 0.000000000000000000, -1.000000000000000000, 0.000000000000000000 ) ) ;
#41135 = CARTESIAN_POINT ( 'NONE',  ( 20.94999999999999574, 44.06843597547144498, -258.9974126733343951 ) ) ;
#41134 = AXIS2_PLACEMENT_3D ( 'NONE', #164067, #109201, #208342 ) ;
#41136 = DIRECTION ( 'NONE',  ( 1.000000000000000000, -0.000000000000000000, -0.000000000000000000 ) ) ;
#41137 = CARTESIAN_POINT ( 'NONE',  ( 18.59999999999999076, 69.45000000001252261, -182.3731074845244109 ) ) ;
#41138 = ORIENTED_EDGE ( 'NONE', *, *, #2397, .F. ) ;
#41139 = ORIENTED_EDGE ( 'NONE', *, *, #33133, .F. ) ;
#41140 = FILL_AREA_STYLE_COLOUR ( '', #152476 ) ;
#41141 = VECTOR ( 'NONE', #33960, 1000.000000000000000 ) ;
#41142 = VERTEX_POINT ( 'NONE', #143051 ) ;
#41143 = DIRECTION ( 'NONE',  ( -1.000000000000000000, 0.000000000000000000, 0.000000000000000000 ) ) ;
#41145 = CARTESIAN_POINT ( 'NONE',  ( 18.55121869061587958, 68.09900309800710261, -224.1499508721967686 ) ) ;
#41144 = CIRCLE ( 'NONE', #24579, 0.09999999999998898659 ) ;
#41146 = DIRECTION ( 'NONE',  ( -1.000000000000000000, 0.000000000000000000, 0.000000000000000000 ) ) ;
#41147 = CIRCLE ( 'NONE', #78531, 0.1000000000000086514 ) ;
#41148 = CARTESIAN_POINT ( 'NONE',  ( 21.05000000000000071, 71.18691588786234092, -91.08158972800052311 ) ) ;
#41149 = EDGE_LOOP ( 'NONE', ( #212661, #54918, #78325, #77571 ) ) ;
#41150 = CARTESIAN_POINT ( 'NONE',  ( -16.93415306273742260, 66.00437773999972535, -149.1130505421640180 ) ) ;
#41151 = ADVANCED_FACE ( 'NONE', ( #50360 ), #72539, .F. ) ;
#41152 = ORIENTED_EDGE ( 'NONE', *, *, #144624, .T. ) ;
#41153 = EDGE_CURVE ( 'NONE', #89267, #9358, #110355, .T. ) ;
#41154 = CARTESIAN_POINT ( 'NONE',  ( 20.94999999999999574, 1.250000000011155299, -41.50000000000000000 ) ) ;
#41155 = VERTEX_POINT ( 'NONE', #114213 ) ;
#41156 = AXIS2_PLACEMENT_3D ( 'NONE', #200013, #21395, #201285 ) ;
#41157 = AXIS2_PLACEMENT_3D ( 'NONE', #229301, #173221, #175757 ) ;
#41158 = CARTESIAN_POINT ( 'NONE',  ( 21.00000000000000000, 9.750000000011153745, -79.25000000000004263 ) ) ;
#41159 = DIRECTION ( 'NONE',  ( -1.000000000000000000, 0.000000000000000000, 0.000000000000000000 ) ) ;
#41160 = ORIENTED_EDGE ( 'NONE', *, *, #255231, .T. ) ;
#41161 = EDGE_CURVE ( 'NONE', #226600, #107823, #245471, .T. ) ;
#41162 = CARTESIAN_POINT ( 'NONE',  ( -18.50000000000000000, 64.25000000001158185, -57.37310748452440379 ) ) ;
#41163 = AXIS2_PLACEMENT_3D ( 'NONE', #170690, #188919, #248903 ) ;
#41165 = ORIENTED_EDGE ( 'NONE', *, *, #37502, .F. ) ;
#41164 = CARTESIAN_POINT ( 'NONE',  ( -18.59999999999999787, 36.65892442174472876, -249.5511627012454596 ) ) ;
#41166 = LINE ( 'NONE', #179385, #164640 ) ;
#41167 = EDGE_LOOP ( 'NONE', ( #205966, #53786, #24570, #111384 ) ) ;
#41168 = AXIS2_PLACEMENT_3D ( 'NONE', #26191, #225630, #48307 ) ;
#41169 = TOROIDAL_SURFACE ( 'NONE', #191191, 11.65000000000000036, 0.1000000000000000056 ) ;
#41170 = AXIS2_PLACEMENT_3D ( 'NONE', #62707, #87382, #142233 ) ;
#41171 = DIRECTION ( 'NONE',  ( 1.000000000000000000, 0.000000000000000000, -0.000000000000000000 ) ) ;
#41172 = VERTEX_POINT ( 'NONE', #154655 ) ;
#41174 = AXIS2_PLACEMENT_3D ( 'NONE', #189394, #26477, #49872 ) ;
#41173 = CARTESIAN_POINT ( 'NONE',  ( -22.94999999999999929, 0.000000000000000000, 0.000000000000000000 ) ) ;
#41175 = CARTESIAN_POINT ( 'NONE',  ( 22.50000000000000000, 25.98655542988603173, -254.2226763854395983 ) ) ;
#41176 = CARTESIAN_POINT ( 'NONE',  ( -18.40000000000000213, 67.17743825834548943, -93.77310748452437394 ) ) ;
#41177 = CARTESIAN_POINT ( 'NONE',  ( 18.56579813702274961, 67.49234744263520724, -195.4268335588911327 ) ) ;
#41178 = CARTESIAN_POINT ( 'NONE',  ( -14.11697426661282684, 66.54258905524518752, -188.5230235107343901 ) ) ;
#41179 = ORIENTED_EDGE ( 'NONE', *, *, #58053, .T. ) ;
#41180 = DIRECTION ( 'NONE',  ( 0.000000000000000000, -0.000000000000000000, 1.000000000000000000 ) ) ;
#41181 = DIRECTION ( 'NONE',  ( 0.000000000000000000, -1.000000000000000000, 0.000000000000000000 ) ) ;
#41182 = EDGE_CURVE ( 'NONE', #73870, #90836, #52946, .T. ) ;
#41183 = EDGE_LOOP ( 'NONE', ( #40799, #140376, #47841, #62121 ) ) ;
#41184 = CARTESIAN_POINT ( 'NONE',  ( 18.49999999999999289, 10.29270135741298731, -105.9573618871519756 ) ) ;
#41186 = ORIENTED_EDGE ( 'NONE', *, *, #105338, .T. ) ;
#41185 = CIRCLE ( 'NONE', #49540, 0.09999999999998898659 ) ;
#41187 = DIRECTION ( 'NONE',  ( -0.000000000000000000, 0.2438576117979275315, -0.9698110461157942730 ) ) ;
#41188 = ORIENTED_EDGE ( 'NONE', *, *, #37645, .T. ) ;
#41189 = DIRECTION ( 'NONE',  ( 1.000000000000000000, 3.448943450116727512E-16, 6.438528483529605672E-16 ) ) ;
#41190 = CARTESIAN_POINT ( 'NONE',  ( -22.94999999999999929, 11.50977166988710820, -1.786320531569725478 ) ) ;
#41191 = ORIENTED_EDGE ( 'NONE', *, *, #70809, .F. ) ;
#41194 = VERTEX_POINT ( 'NONE', #71260 ) ;
#41193 = EDGE_CURVE ( 'NONE', #81104, #23713, #112205, .T. ) ;
#41192 = DIRECTION ( 'NONE',  ( -1.000000000000000000, 0.000000000000000000, 0.000000000000000000 ) ) ;
#41195 = PLANE ( 'NONE',  #63104 ) ;
#41196 = VERTEX_POINT ( 'NONE', #75118 ) ;
#41197 = DIRECTION ( 'NONE',  ( 0.000000000000000000, 0.000000000000000000, -1.000000000000000000 ) ) ;
#41198 = AXIS2_PLACEMENT_3D ( 'NONE', #144558, #229258, #127579 ) ;
#41199 = EDGE_CURVE ( 'NONE', #82836, #209151, #44066, .T. ) ;
#41200 = FACE_OUTER_BOUND ( 'NONE', #123876, .T. ) ;
#41201 = VECTOR ( 'NONE', #152741, 1000.000000000000000 ) ;
#41202 = EDGE_LOOP ( 'NONE', ( #240517, #26106, #123627, #90400 ) ) ;
#41203 = ORIENTED_EDGE ( 'NONE', *, *, #40593, .T. ) ;
#41204 = DIRECTION ( 'NONE',  ( 0.000000000000000000, 1.000000000000000000, 0.000000000000000000 ) ) ;
#41206 = ADVANCED_FACE ( 'NONE', ( #112935 ), #11269, .T. ) ;
#41205 = DIRECTION ( 'NONE',  ( 0.000000000000000000, -1.000000000000000000, -6.982962677686265922E-15 ) ) ;
#41207 = AXIS2_PLACEMENT_3D ( 'NONE', #79502, #253015, #76946 ) ;
#41208 = ORIENTED_EDGE ( 'NONE', *, *, #43336, .T. ) ;
#41209 = CARTESIAN_POINT ( 'NONE',  ( -16.86337532320261801, 66.02003279578769934, -123.9720319535071695 ) ) ;
#41210 = ORIENTED_EDGE ( 'NONE', *, *, #244547, .F. ) ;
#41211 = ORIENTED_EDGE ( 'NONE', *, *, #6774, .T. ) ;
#41212 = CIRCLE ( 'NONE', #174526, 0.09999999999999939493 ) ;
#41213 = EDGE_CURVE ( 'NONE', #52039, #169096, #132495, .T. ) ;
#41216 = EDGE_CURVE ( 'NONE', #117567, #14406, #41467, .T. ) ;
#41215 = EDGE_CURVE ( 'NONE', #243832, #106026, #13835, .T. ) ;
#41214 = CARTESIAN_POINT ( 'NONE',  ( 20.94999999999999929, 87.48912529308779540, -72.52310748452423184 ) ) ;
#41218 = ORIENTED_EDGE ( 'NONE', *, *, #166895, .T. ) ;
#41217 = CARTESIAN_POINT ( 'NONE',  ( -16.81453046979149590, 9.939102281452072418, -46.21172652360304767 ) ) ;
#41219 = CARTESIAN_POINT ( 'NONE',  ( -18.50000000000000000, 7.021664781911246322, -171.3335654018973173 ) ) ;
#41220 = AXIS2_PLACEMENT_3D ( 'NONE', #223455, #44836, #203903 ) ;
#41221 = DIRECTION ( 'NONE',  ( -0.000000000000000000, 0.1350103645451876666, 0.9908441862701600211 ) ) ;
#41222 = VECTOR ( 'NONE', #168357, 999.9999999999998863 ) ;
#41223 = DIRECTION ( 'NONE',  ( 0.000000000000000000, -1.000000000000000000, -7.813886390323680189E-15 ) ) ;
#41224 = VECTOR ( 'NONE', #14882, 1000.000000000000114 ) ;
#41226 = CYLINDRICAL_SURFACE ( 'NONE', #145007, 0.09999999999999939493 ) ;
#41225 = DIRECTION ( 'NONE',  ( 1.000000000000000000, 0.000000000000000000, 0.000000000000000000 ) ) ;
#41227 = CARTESIAN_POINT ( 'NONE',  ( 21.72449340488910252, 10.28395627749111974, -9.250000000000001776 ) ) ;
#41228 = CARTESIAN_POINT ( 'NONE',  ( -21.14999999999999858, 76.10000000001203091, -114.6726782920691079 ) ) ;
#41229 = DIRECTION ( 'NONE',  ( 0.000000000000000000, 0.000000000000000000, 1.000000000000000000 ) ) ;
#41230 = DIRECTION ( 'NONE',  ( -1.000000000000000000, 0.000000000000000000, 0.000000000000000000 ) ) ;
#41231 = ADVANCED_FACE ( 'NONE', ( #15123 ), #253709, .T. ) ;
#41232 = EDGE_CURVE ( 'NONE', #134638, #72318, #124655, .T. ) ;
#41233 = ORIENTED_EDGE ( 'NONE', *, *, #38294, .T. ) ;
#41234 = ORIENTED_EDGE ( 'NONE', *, *, #93560, .F. ) ;
#41236 = ORIENTED_EDGE ( 'NONE', *, *, #165081, .F. ) ;
#41235 = B_SPLINE_CURVE_WITH_KNOTS ( 'NONE', 3,
 ( #156824, #79792, #22439, #96779, #219320, #138478, #81082 ),
 .UNSPECIFIED., .F., .F.,
 ( 4, 3, 4 ),
 ( 0.000000000000000000, 4.520325912680747552E-05, 5.794988040901532806E-05 ),
 .UNSPECIFIED. ) ;
#41237 = ADVANCED_FACE ( 'NONE', ( #51639 ), #24730, .F. ) ;
#41238 = CARTESIAN_POINT ( 'NONE',  ( 21.14999999999999858, -3.140208063160686791, -228.2318569537739847 ) ) ;
#41239 = ORIENTED_EDGE ( 'NONE', *, *, #110067, .T. ) ;
#41240 = CARTESIAN_POINT ( 'NONE',  ( 20.02499999999999858, 66.25000000001253397, -182.3731074845244393 ) ) ;
#41241 = CIRCLE ( 'NONE', #178040, 0.09999999999999939493 ) ;
#41242 = EDGE_CURVE ( 'NONE', #211645, #135773, #220526, .T. ) ;
#41243 = VERTEX_POINT ( 'NONE', #92075 ) ;
#41244 = CARTESIAN_POINT ( 'NONE',  ( 20.94999999999999929, 65.70729864261026876, -131.0657455973724836 ) ) ;
#41246 = EDGE_CURVE ( 'NONE', #12448, #201039, #213301, .T. ) ;
#41245 = B_SPLINE_CURVE_WITH_KNOTS ( 'NONE', 3,
 ( #20816, #238551, #23395, #79466, #102871, #182451, #242396 ),
 .UNSPECIFIED., .F., .F.,
 ( 4, 3, 4 ),
 ( 0.000000000000000000, 0.0007844235214594318627, 0.001767853679404347454 ),
 .UNSPECIFIED. ) ;
#41248 = VERTEX_POINT ( 'NONE', #34701 ) ;
#41247 = ORIENTED_EDGE ( 'NONE', *, *, #184371, .F. ) ;
#41249 = ORIENTED_EDGE ( 'NONE', *, *, #162743, .F. ) ;
#41250 = VERTEX_POINT ( 'NONE', #234150 ) ;
#41251 = CARTESIAN_POINT ( 'NONE',  ( 20.85000000000000142, 77.83585931145546510, -91.51866831572576189 ) ) ;
#41252 = CARTESIAN_POINT ( 'NONE',  ( -18.59999999999999787, 1.637172712981537659, -112.0821533654720525 ) ) ;
#41254 = VERTEX_POINT ( 'NONE', #98453 ) ;
#41253 = CARTESIAN_POINT ( 'NONE',  ( -20.85000000000000142, 70.08587962373171365, -198.1273832143211848 ) ) ;
#41255 = CARTESIAN_POINT ( 'NONE',  ( 20.19326291201523205, 39.59028495805256398, -237.1093300823515619 ) ) ;
#41256 = EDGE_CURVE ( 'NONE', #111234, #175346, #81470, .T. ) ;
#41257 = CARTESIAN_POINT ( 'NONE',  ( 14.45204356427542258, 12.43804190223350936, -213.6995959073539950 ) ) ;
#41259 = VERTEX_POINT ( 'NONE', #119359 ) ;
#41258 = CARTESIAN_POINT ( 'NONE',  ( 21.13736287352038445, 67.95335762362854837, -182.6731074845244223 ) ) ;
#41260 = DIRECTION ( 'NONE',  ( 0.000000000000000000, -0.8814952561688429444, 0.4721928772777350680 ) ) ;
#41261 = ORIENTED_EDGE ( 'NONE', *, *, #205610, .T. ) ;
#41262 = DIRECTION ( 'NONE',  ( 0.000000000000000000, -0.2128009952263485993, 0.9770955615653341697 ) ) ;
#41264 = ORIENTED_EDGE ( 'NONE', *, *, #116481, .T. ) ;
#41263 = CARTESIAN_POINT ( 'NONE',  ( -23.15000000000000213, 11.65000000001115588, -79.15000000000004832 ) ) ;
#41265 = DIRECTION ( 'NONE',  ( 1.387778780781405791E-13, 0.9999176327611370985, 0.01283462868040226822 ) ) ;
#41266 = DIRECTION ( 'NONE',  ( 0.000000000000000000, -1.000000000000000000, -6.982962677686266711E-15 ) ) ;
#41267 = DIRECTION ( 'NONE',  ( 0.000000000000000000, 0.000000000000000000, -1.000000000000000000 ) ) ;
#41269 = EDGE_CURVE ( 'NONE', #150801, #157238, #99759, .T. ) ;
#41268 = ORIENTED_EDGE ( 'NONE', *, *, #26488, .F. ) ;
#41270 = CIRCLE ( 'NONE', #124630, 0.1000000000000028644 ) ;
#41273 = CARTESIAN_POINT ( 'NONE',  ( -22.39999999999999858, 7.790779598384560245, -100.4000000000000341 ) ) ;
#41272 = CIRCLE ( 'NONE', #120384, 6.258578643762687577 ) ;
#41271 = CARTESIAN_POINT ( 'NONE',  ( -20.94999999999999929, 11.65000000001115232, -67.00000000000000000 ) ) ;
#41274 = CARTESIAN_POINT ( 'NONE',  ( -12.48127053791145080, 66.62341902196787657, -85.39616123751244459 ) ) ;
#41275 = VECTOR ( 'NONE', #157476, 1000.000000000000000 ) ;
#41276 = CARTESIAN_POINT ( 'NONE',  ( 21.53551880898956838, 6.784797761427480367, -133.9010302654283748 ) ) ;
#41277 = DIRECTION ( 'NONE',  ( 0.000000000000000000, 1.000000000000000000, 0.000000000000000000 ) ) ;
#41278 = CARTESIAN_POINT ( 'NONE',  ( 20.94999999999999574, 14.64166534854604507, -236.4381089660238331 ) ) ;
#41279 = VERTEX_POINT ( 'NONE', #77625 ) ;
#41280 = ORIENTED_EDGE ( 'NONE', *, *, #148987, .T. ) ;
#41281 = ORIENTED_EDGE ( 'NONE', *, *, #4078, .F. ) ;
#41282 = CARTESIAN_POINT ( 'NONE',  ( -21.05000000000000071, -0.09999999998884476216, -127.4593430482987912 ) ) ;
#41283 = CIRCLE ( 'NONE', #7953, 7.899999999999990585 ) ;
#41284 = ORIENTED_EDGE ( 'NONE', *, *, #96264, .F. ) ;
#41285 = CYLINDRICAL_SURFACE ( 'NONE', #80871, 4.049999999999998046 ) ;
#41286 = ORIENTED_EDGE ( 'NONE', *, *, #69667, .T. ) ;
#41287 = ADVANCED_FACE ( 'NONE', ( #198884 ), #78838, .T. ) ;
#41288 = CARTESIAN_POINT ( 'NONE',  ( -20.85000000000000142, 77.36242903720467723, -28.13422623660311217 ) ) ;
#41289 = CARTESIAN_POINT ( 'NONE',  ( -21.53699400384945051, 76.00000000001243450, -176.8108192777617660 ) ) ;
#41290 = VECTOR ( 'NONE', #231704, 1000.000000000000000 ) ;
#41291 = AXIS2_PLACEMENT_3D ( 'NONE', #113449, #95171, #173485 ) ;
#41292 = VERTEX_POINT ( 'NONE', #38534 ) ;
#41293 = CARTESIAN_POINT ( 'NONE',  ( 22.39999999999999503, -0.09999999998884338825, -21.85042919245520210 ) ) ;
#41294 = ORIENTED_EDGE ( 'NONE', *, *, #99618, .T. ) ;
#41295 = AXIS2_PLACEMENT_3D ( 'NONE', #74939, #55306, #76178 ) ;
#41296 = ORIENTED_EDGE ( 'NONE', *, *, #224557, .F. ) ;
#41297 = ORIENTED_EDGE ( 'NONE', *, *, #214017, .F. ) ;
#41298 = FACE_OUTER_BOUND ( 'NONE', #58920, .T. ) ;
#41299 = DIRECTION ( 'NONE',  ( 0.000000000000000000, 0.000000000000000000, 1.000000000000000000 ) ) ;
#41300 = CARTESIAN_POINT ( 'NONE',  ( -16.89268316805466341, 66.04827818676939444, -56.87885996306994230 ) ) ;
#41301 = DIRECTION ( 'NONE',  ( 1.000000000000000000, 0.000000000000000000, -0.000000000000000000 ) ) ;
#41302 = CARTESIAN_POINT ( 'NONE',  ( -21.12230431290521082, 60.99748793727087559, -234.1698672821734988 ) ) ;
#41303 = CARTESIAN_POINT ( 'NONE',  ( -18.40000000000000213, 67.17743825834557470, -112.2731074845243597 ) ) ;
#41305 = DIRECTION ( 'NONE',  ( 0.000000000000000000, 1.000000000000000000, 0.000000000000000000 ) ) ;
#41304 = CARTESIAN_POINT ( 'NONE',  ( 21.05000000000000071, -0.08559286335121364664, -161.0863372651298846 ) ) ;
#41306 = DIRECTION ( 'NONE',  ( 1.000000000000000000, 0.000000000000000000, 0.000000000000000000 ) ) ;
#41308 = VERTEX_POINT ( 'NONE', #197592 ) ;
#41307 = CARTESIAN_POINT ( 'NONE',  ( 21.53551880898957194, 69.21520223859563714, -103.1220772190960275 ) ) ;
#41309 = CARTESIAN_POINT ( 'NONE',  ( 21.10320863425824811, 69.59972261355278533, -103.0481297357514876 ) ) ;
#41310 = CARTESIAN_POINT ( 'NONE',  ( -18.51555513499593175, -9.352657054493597855, -141.1951698956972052 ) ) ;
#41311 = ORIENTED_EDGE ( 'NONE', *, *, #236764, .T. ) ;
#41312 = VERTEX_POINT ( 'NONE', #76351 ) ;
#41313 = CARTESIAN_POINT ( 'NONE',  ( 18.59999999999999076, -1.835859311432481045, -145.5044391687985694 ) ) ;
#41314 = CARTESIAN_POINT ( 'NONE',  ( -20.54999999999999716, 1.115600667400684642E-11, -100.5000000000000426 ) ) ;
#41315 = DIRECTION ( 'NONE',  ( 0.000000000000000000, -6.982962677686266711E-15, 1.000000000000000000 ) ) ;
#41316 = ORIENTED_EDGE ( 'NONE', *, *, #70962, .F. ) ;
#41317 = CIRCLE ( 'NONE', #208084, 0.1000000000000072220 ) ;
#41318 = CARTESIAN_POINT ( 'NONE',  ( -21.04999999999994387, 65.15000000001120384, -4.423107484524790856 ) ) ;
#41319 = ORIENTED_EDGE ( 'NONE', *, *, #235985, .F. ) ;
#41320 = EDGE_LOOP ( 'NONE', ( #83838, #109552, #68029, #164983 ) ) ;
#41321 = CARTESIAN_POINT ( 'NONE',  ( -22.39999999999999858, -1.657885652111596109, -193.3876638332971254 ) ) ;
#41322 = ORIENTED_EDGE ( 'NONE', *, *, #161012, .T. ) ;
#41323 = CARTESIAN_POINT ( 'NONE',  ( -16.93440969289731157, 60.88036584781310978, -221.0866173190812276 ) ) ;
#41324 = CYLINDRICAL_SURFACE ( 'NONE', #106975, 0.1000000000000001443 ) ;
#41326 = DIRECTION ( 'NONE',  ( 0.000000000000000000, -0.4721928772776973204, -0.8814952561688629284 ) ) ;
#41325 = CIRCLE ( 'NONE', #162119, 0.1000000000000028644 ) ;
#41327 = DIRECTION ( 'NONE',  ( 0.000000000000000000, 1.000000000000000000, 0.000000000000000000 ) ) ;
#41328 = DIRECTION ( 'NONE',  ( 0.000000000000000000, -0.9908441862701600211, -0.1350103645451876666 ) ) ;
#41329 = VERTEX_POINT ( 'NONE', #35977 ) ;
#41330 = CYLINDRICAL_SURFACE ( 'NONE', #208682, 0.09999999999999939493 ) ;
#41332 = ADVANCED_FACE ( 'NONE', ( #175494 ), #141222, .T. ) ;
#41331 = CARTESIAN_POINT ( 'NONE',  ( 21.15000000000005542, 74.16448838626247664, -47.52760213295649550 ) ) ;
#41333 = DIRECTION ( 'NONE',  ( -0.000000000000000000, 0.9910827722268039652, 0.1332476588733670919 ) ) ;
#41334 = CIRCLE ( 'NONE', #132895, 0.09999999999998898659 ) ;
#41335 = VECTOR ( 'NONE', #249500, 1000.000000000000000 ) ;
#41336 = ORIENTED_EDGE ( 'NONE', *, *, #117088, .F. ) ;
#41337 = AXIS2_PLACEMENT_3D ( 'NONE', #218063, #199830, #39489 ) ;
#41339 = ORIENTED_EDGE ( 'NONE', *, *, #202106, .T. ) ;
#41338 = DIRECTION ( 'NONE',  ( 1.000000000000000000, 0.000000000000000000, 0.000000000000000000 ) ) ;
#41340 = LINE ( 'NONE', #42595, #105730 ) ;
#41341 = DIRECTION ( 'NONE',  ( -0.000000000000000000, -0.2128009952263603677, 0.9770955615653313941 ) ) ;
#41342 = CARTESIAN_POINT ( 'NONE',  ( -18.59999999999999787, 66.65000000001222702, -148.8731074845244393 ) ) ;
#41343 = DIRECTION ( 'NONE',  ( 0.000000000000000000, -0.2617529984165031243, -0.9651348961777157509 ) ) ;
#41344 = CIRCLE ( 'NONE', #16577, 12.97499999999999964 ) ;
#41345 = CARTESIAN_POINT ( 'NONE',  ( -21.64999999999999858, 68.65000000001205649, -124.2731074845243455 ) ) ;
#41346 = CARTESIAN_POINT ( 'NONE',  ( 22.50000000000000000, 76.00000000001213607, -136.5231074845242745 ) ) ;
#41347 = AXIS2_PLACEMENT_3D ( 'NONE', #142998, #227683, #49050 ) ;
#41348 = ADVANCED_FACE ( 'NONE', ( #256216 ), #37290, .T. ) ;
#41349 = ORIENTED_EDGE ( 'NONE', *, *, #76768, .F. ) ;
#41350 = CARTESIAN_POINT ( 'NONE',  ( -16.89797118371611973, 63.08312069776565068, -213.0364664784391664 ) ) ;
#41351 = DIRECTION ( 'NONE',  ( 0.000000000000000000, -0.8814952561688429444, 0.4721928772777349570 ) ) ;
#41352 = DIRECTION ( 'NONE',  ( 1.000000000000000000, 0.000000000000000000, 0.000000000000000000 ) ) ;
#41353 = CARTESIAN_POINT ( 'NONE',  ( 21.53752568617686691, 6.786807874514976469, -133.9010255387156008 ) ) ;
#41354 = CARTESIAN_POINT ( 'NONE',  ( 20.53930447208010790, 67.02285131248657990, -61.08060034294610574 ) ) ;
#41355 = AXIS2_PLACEMENT_3D ( 'NONE', #96092, #37441, #116961 ) ;
#41356 = AXIS2_PLACEMENT_3D ( 'NONE', #143328, #24703, #202033 ) ;
#41358 = ORIENTED_EDGE ( 'NONE', *, *, #143252, .T. ) ;
#41357 = AXIS2_PLACEMENT_3D ( 'NONE', #152914, #52473, #151626 ) ;
#41359 = ORIENTED_EDGE ( 'NONE', *, *, #13530, .F. ) ;
#41360 = DIRECTION ( 'NONE',  ( 6.938893903907270030E-14, 0.000000000000000000, -1.000000000000000000 ) ) ;
#41361 = AXIS2_PLACEMENT_3D ( 'NONE', #126205, #105327, #66249 ) ;
#41362 = EDGE_CURVE ( 'NONE', #129546, #169137, #149613, .T. ) ;
#41363 = DIRECTION ( 'NONE',  ( 0.000000000000000000, -1.000000000000000000, 0.000000000000000000 ) ) ;
#41364 = DIRECTION ( 'NONE',  ( 0.000000000000000000, 1.000000000000000000, 0.000000000000000000 ) ) ;
#41365 = ADVANCED_FACE ( 'NONE', ( #137604 ), #78909, .T. ) ;
#41366 = CIRCLE ( 'NONE', #49714, 0.1000000000000028644 ) ;
#41367 = ORIENTED_EDGE ( 'NONE', *, *, #101645, .T. ) ;
#41368 = CARTESIAN_POINT ( 'NONE',  ( 20.09999999999999787, 44.21724908628621620, -235.4814530999287285 ) ) ;
#41369 = ADVANCED_FACE ( 'NONE', ( #18952 ), #239303, .F. ) ;
#41370 = DIRECTION ( 'NONE',  ( 1.000000000000000000, 3.448943450116723568E-16, 6.438528483529607644E-16 ) ) ;
#41371 = EDGE_CURVE ( 'NONE', #62504, #164965, #238001, .T. ) ;
#41372 = PRODUCT_DEFINITION_SHAPE ( 'NONE', 'NONE',  #258108 ) ;
#41373 = DIRECTION ( 'NONE',  ( 0.000000000000000000, -0.2617529984165031243, -0.9651348961777157509 ) ) ;
#41374 = AXIS2_PLACEMENT_3D ( 'NONE', #170320, #134962, #231540 ) ;
#41375 = EDGE_CURVE ( 'NONE', #49254, #126928, #158021, .T. ) ;
#41376 = ORIENTED_EDGE ( 'NONE', *, *, #168711, .F. ) ;
#41377 = ORIENTED_EDGE ( 'NONE', *, *, #24989, .T. ) ;
#41378 = DIRECTION ( 'NONE',  ( 0.000000000000000000, 6.982962677686266711E-15, -1.000000000000000000 ) ) ;
#41379 = CARTESIAN_POINT ( 'NONE',  ( 21.05000000000000071, 69.58602111852397343, -169.9373083682504273 ) ) ;
#41380 = LINE ( 'NONE', #251087, #86862 ) ;
#41381 = DIRECTION ( 'NONE',  ( 0.000000000000000000, 0.000000000000000000, 1.000000000000000000 ) ) ;
#41382 = DIRECTION ( 'NONE',  ( -1.000000000000000000, 0.000000000000000000, 0.000000000000000000 ) ) ;
#41383 = CARTESIAN_POINT ( 'NONE',  ( 20.94999999999999574, 69.60000000001187459, -93.09268285446279378 ) ) ;
#41384 = DIRECTION ( 'NONE',  ( 2.915501640297155269E-16, 0.4088369013363274962, -0.9126074666063773710 ) ) ;
#41385 = VECTOR ( 'NONE', #179989, 1000.000000000000000 ) ;
#41386 = ADVANCED_FACE ( 'NONE', ( #37266 ), #116779, .F. ) ;
#41387 = DIRECTION ( 'NONE',  ( 1.000000000000000000, 0.000000000000000000, 0.000000000000000000 ) ) ;
#41388 = CARTESIAN_POINT ( 'NONE',  ( 21.05000000000000071, 65.27628289530476025, -157.8731074845244393 ) ) ;
#41389 = DIRECTION ( 'NONE',  ( -1.000000000000000000, 0.000000000000000000, 0.000000000000000000 ) ) ;
#41390 = DIRECTION ( 'NONE',  ( 1.000000000000000000, 0.000000000000000000, 0.000000000000000000 ) ) ;
#41391 = CARTESIAN_POINT ( 'NONE',  ( 20.95512820512820440, 8.876151316299271343, -155.2500000000000284 ) ) ;
#41392 = VECTOR ( 'NONE', #219260, 1000.000000000000000 ) ;
#41393 = ORIENTED_EDGE ( 'NONE', *, *, #250932, .T. ) ;
#41394 = CYLINDRICAL_SURFACE ( 'NONE', #181166, 12.87499999999999822 ) ;
#41395 = DIRECTION ( 'NONE',  ( 0.000000000000000000, -6.982962677686266711E-15, 1.000000000000000000 ) ) ;
#41396 = VERTEX_POINT ( 'NONE', #97167 ) ;
#41397 = CARTESIAN_POINT ( 'NONE',  ( -22.49917693094574389, 0.08522996423282767908, -55.35020421546937541 ) ) ;
#41398 = CIRCLE ( 'NONE', #187144, 0.09999999999999481526 ) ;
#41399 = CARTESIAN_POINT ( 'NONE',  ( -21.05000000000000071, 76.00000000001237765, -170.0231074845243597 ) ) ;
#41400 = CIRCLE ( 'NONE', #257802, 7.899999999999990585 ) ;
#41401 = ORIENTED_EDGE ( 'NONE', *, *, #92717, .F. ) ;
#41402 = CARTESIAN_POINT ( 'NONE',  ( -16.89268316805465986, 9.951721813253337601, -188.3557524785454973 ) ) ;
#41403 = CARTESIAN_POINT ( 'NONE',  ( 22.59066674512252604, 31.82725254005531212, -238.8404961800036688 ) ) ;
#41404 = ORIENTED_EDGE ( 'NONE', *, *, #237772, .F. ) ;
#41405 = VECTOR ( 'NONE', #247964, 1000.000000000000000 ) ;
#41406 =( BOUNDED_CURVE ( )  B_SPLINE_CURVE ( 3, ( #145821, #27208, #188809, #46721 ),
 .UNSPECIFIED., .F., .T. ) 
 B_SPLINE_CURVE_WITH_KNOTS ( ( 4, 4 ),
 ( 3.752122642744613046, 4.712388980384671910 ),
 .UNSPECIFIED. ) 
 CURVE ( )  GEOMETRIC_REPRESENTATION_ITEM ( )  RATIONAL_B_SPLINE_CURVE ( ( 1.000000000000000000, 0.9246222802177266331, 0.9246222802177266331, 1.000000000000000000 ) ) 
 REPRESENTATION_ITEM ( '' )  );
#41407 = EDGE_CURVE ( 'NONE', #216782, #183838, #241195, .T. ) ;
#41408 = EDGE_CURVE ( 'NONE', #118232, #79366, #49635, .T. ) ;
#41409 = ORIENTED_EDGE ( 'NONE', *, *, #204351, .T. ) ;
#41410 = FACE_OUTER_BOUND ( 'NONE', #97877, .T. ) ;
#41411 = VERTEX_POINT ( 'NONE', #46224 ) ;
#41412 = EDGE_CURVE ( 'NONE', #214434, #159346, #182930, .T. ) ;
#41414 = EDGE_CURVE ( 'NONE', #104099, #95314, #9393, .T. ) ;
#41413 = DIRECTION ( 'NONE',  ( 0.000000000000000000, -0.8814952561688439436, 0.4721928772777329586 ) ) ;
#41415 = CARTESIAN_POINT ( 'NONE',  ( -21.14999999999999858, 1.115600667400684642E-11, -33.50000000000000000 ) ) ;
#41416 = DIRECTION ( 'NONE',  ( 3.469446951953635015E-14, -0.000000000000000000, 1.000000000000000000 ) ) ;
#41417 = CYLINDRICAL_SURFACE ( 'NONE', #183518, 0.1000000000000028644 ) ;
#41418 = DIRECTION ( 'NONE',  ( 0.000000000000000000, -0.1350103645451807555, -0.9908441862701609093 ) ) ;
#41419 = CARTESIAN_POINT ( 'NONE',  ( 23.14999999999999503, 64.25000000001220712, -148.2731074845243882 ) ) ;
#41420 = ADVANCED_FACE ( 'NONE', ( #84022 ), #103768, .T. ) ;
#41421 = CARTESIAN_POINT ( 'NONE',  ( 21.05000000000000071, -1.249999999999999334, -7.900000000000000355 ) ) ;
#41422 = CARTESIAN_POINT ( 'NONE',  ( -17.22361732159831504, 65.65484434140937253, -80.89389201039151089 ) ) ;
#41424 = ORIENTED_EDGE ( 'NONE', *, *, #190414, .F. ) ;
#41423 = CARTESIAN_POINT ( 'NONE',  ( -18.46093223321773280, -9.480682968263375088, -40.58455051392668622 ) ) ;
#41425 = ORIENTED_EDGE ( 'NONE', *, *, #208626, .F. ) ;
#41427 = DIRECTION ( 'NONE',  ( -0.000000000000000000, 0.8814952561688430555, -0.4721928772777346239 ) ) ;
#41426 = CARTESIAN_POINT ( 'NONE',  ( -21.05000000000000071, 1.116121084443477685E-11, -69.90000000000003411 ) ) ;
#41429 = ORIENTED_EDGE ( 'NONE', *, *, #99597, .F. ) ;
#41428 = CARTESIAN_POINT ( 'NONE',  ( -16.83233564386401326, 60.99129099293333667, -220.9258002532045566 ) ) ;
#41430 = EDGE_CURVE ( 'NONE', #151973, #121203, #221003, .T. ) ;
#41431 = ORIENTED_EDGE ( 'NONE', *, *, #21741, .T. ) ;
#41432 = CARTESIAN_POINT ( 'NONE',  ( 18.49999999999999289, 65.75000000001199396, -115.1731074845243796 ) ) ;
#41433 = ADVANCED_FACE ( 'NONE', ( #125759 ), #170490, .T. ) ;
#41434 = CARTESIAN_POINT ( 'NONE',  ( -18.59999999999999787, 7.021664781900089913, -37.23356540189728747 ) ) ;
#41436 = EDGE_CURVE ( 'NONE', #133183, #46365, #183112, .T. ) ;
#41435 = DIRECTION ( 'NONE',  ( 0.000000000000000000, 0.000000000000000000, -1.000000000000000000 ) ) ;
#41437 = DIRECTION ( 'NONE',  ( 0.000000000000000000, 0.9126074666063783702, 0.4088369013363252757 ) ) ;
#41438 = DIRECTION ( 'NONE',  ( 0.000000000000000000, 0.000000000000000000, 1.000000000000000000 ) ) ;
#41439 = CARTESIAN_POINT ( 'NONE',  ( -20.64999999999999858, 4.350000000011156054, -79.35000000000005116 ) ) ;
#41440 = ADVANCED_FACE ( 'NONE', ( #44956 ), #3234, .T. ) ;
#41441 = CARTESIAN_POINT ( 'NONE',  ( -20.54999999999999716, 76.00000000001243450, -168.1231074845243540 ) ) ;
#41442 = AXIS2_PLACEMENT_3D ( 'NONE', #42337, #63164, #183142 ) ;
#41443 = VERTEX_POINT ( 'NONE', #86617 ) ;
#41444 = ORIENTED_EDGE ( 'NONE', *, *, #64035, .F. ) ;
#41445 = CARTESIAN_POINT ( 'NONE',  ( 23.25000000000000000, 75.49601185175264106, -250.2710592679604531 ) ) ;
#41446 = ADVANCED_FACE ( 'NONE', ( #184454 ), #245724, .F. ) ;
#41447 = AXIS2_PLACEMENT_3D ( 'NONE', #172594, #252073, #17331 ) ;
#41448 = TOROIDAL_SURFACE ( 'NONE', #128923, 12.77500000000000036, 0.1000000000000000056 ) ;
#41449 = ORIENTED_EDGE ( 'NONE', *, *, #14971, .F. ) ;
#41450 = DIRECTION ( 'NONE',  ( -1.000000000000000000, 0.000000000000000000, 0.000000000000000000 ) ) ;
#41451 = EDGE_LOOP ( 'NONE', ( #231163, #55202, #109086, #6111, #68097 ) ) ;
#41452 = CARTESIAN_POINT ( 'NONE',  ( -18.40000000000000213, 40.40436687347765599, -235.2865959907995546 ) ) ;
#41453 = EDGE_CURVE ( 'NONE', #160579, #6554, #79002, .T. ) ;
#41454 = CARTESIAN_POINT ( 'NONE',  ( -15.57281606413133801, 48.82205200898362563, -233.8342296612540281 ) ) ;
#41455 = DIRECTION ( 'NONE',  ( 0.000000000000000000, 0.000000000000000000, -1.000000000000000000 ) ) ;
#41456 = DIRECTION ( 'NONE',  ( 0.000000000000000000, 0.000000000000000000, -1.000000000000000000 ) ) ;
#41457 = EDGE_CURVE ( 'NONE', #221934, #5552, #212338, .T. ) ;
#41458 = DIRECTION ( 'NONE',  ( 0.000000000000000000, -7.272083257015735086E-15, 1.000000000000000000 ) ) ;
#41459 = ORIENTED_EDGE ( 'NONE', *, *, #226132, .T. ) ;
#41460 = EDGE_CURVE ( 'NONE', #68492, #128109, #149804, .T. ) ;
#41461 = LINE ( 'NONE', #235778, #154476 ) ;
#41462 = ORIENTED_EDGE ( 'NONE', *, *, #172685, .F. ) ;
#41464 = CARTESIAN_POINT ( 'NONE',  ( -20.64999999999999858, 73.50000000001223555, -149.7477294072864709 ) ) ;
#41463 = VECTOR ( 'NONE', #214681, 1000.000000000000000 ) ;
#41465 = CIRCLE ( 'NONE', #203941, 0.1000000000000028644 ) ;
#41467 = CIRCLE ( 'NONE', #212142, 11.80000000000000426 ) ;
#41466 = CARTESIAN_POINT ( 'NONE',  ( -22.42357213249529480, 75.90091303601117545, -211.1960398708842774 ) ) ;
#41468 = CARTESIAN_POINT ( 'NONE',  ( -23.25000000000000000, 11.31726856452598184, -246.8669175193824969 ) ) ;
#41469 = EDGE_LOOP ( 'NONE', ( #220691, #178036, #5502 ) ) ;
#41470 = CARTESIAN_POINT ( 'NONE',  ( 20.94999999999999929, 76.00000000001244871, -170.0231074845243597 ) ) ;
#41471 = ORIENTED_EDGE ( 'NONE', *, *, #256119, .T. ) ;
#41474 = EDGE_LOOP ( 'NONE', ( #17044, #131109, #240740, #25140 ) ) ;
#41473 = FACE_OUTER_BOUND ( 'NONE', #29680, .T. ) ;
#41472 = CARTESIAN_POINT ( 'NONE',  ( 18.59999999999999787, 47.07326788871596790, -255.0992659944397758 ) ) ;
#41475 = VECTOR ( 'NONE', #64036, 1000.000000000000000 ) ;
#41476 = CARTESIAN_POINT ( 'NONE',  ( -22.37643362114956602, 0.09908137369253962323, -159.8742100060415794 ) ) ;
#41477 = DIRECTION ( 'NONE',  ( 0.000000000000000000, 1.224646799142015331E-16, 1.000000000000000000 ) ) ;
#41478 = ORIENTED_EDGE ( 'NONE', *, *, #192409, .T. ) ;
#41479 = SPHERICAL_SURFACE ( 'NONE', #13942, 0.1000000000000000056 ) ;
#41480 = DIRECTION ( 'NONE',  ( -0.000000000000000000, -0.000000000000000000, -1.000000000000000000 ) ) ;
#41481 = CARTESIAN_POINT ( 'NONE',  ( -22.41119224318417125, -3.140208063160686791, -228.2318569537739847 ) ) ;
#41483 = VERTEX_POINT ( 'NONE', #146592 ) ;
#41482 = CARTESIAN_POINT ( 'NONE',  ( -18.50000000000000000, 64.75617845954087670, -200.4736850529726269 ) ) ;
#41484 = CARTESIAN_POINT ( 'NONE',  ( -23.15000000000000213, 2.000000000011154189, -80.22462192276213955 ) ) ;
#41485 = ORIENTED_EDGE ( 'NONE', *, *, #148501, .T. ) ;
#41486 = CARTESIAN_POINT ( 'NONE',  ( 18.59999999999999787, -1.835341550213255957, -78.55515129256302487 ) ) ;
#41487 = CARTESIAN_POINT ( 'NONE',  ( -16.93301857435213620, 9.976309354746611291, -188.3857755711613891 ) ) ;
#41488 = DIRECTION ( 'NONE',  ( -0.000000000000000000, 1.000000000000000000, -0.000000000000000000 ) ) ;
#41489 = AXIS2_PLACEMENT_3D ( 'NONE', #208502, #174543, #110659 ) ;
#41490 = ORIENTED_EDGE ( 'NONE', *, *, #111257, .T. ) ;
#41491 = CARTESIAN_POINT ( 'NONE',  ( -20.94999999999999929, 76.25610579210459150, -170.0580039261966192 ) ) ;
#41492 = ORIENTED_EDGE ( 'NONE', *, *, #152746, .F. ) ;
#41493 = DIRECTION ( 'NONE',  ( -4.336808689942017736E-16, 0.000000000000000000, -1.000000000000000000 ) ) ;
#41494 = FACE_OUTER_BOUND ( 'NONE', #202125, .T. ) ;
#41495 = DIRECTION ( 'NONE',  ( -1.000000000000000000, -1.836970198721029934E-16, 0.000000000000000000 ) ) ;
#41496 = CIRCLE ( 'NONE', #58196, 0.1000000000000028644 ) ;
#41497 = ORIENTED_EDGE ( 'NONE', *, *, #86453, .F. ) ;
#41498 = DIRECTION ( 'NONE',  ( 1.000000000000000000, 0.000000000000000000, 0.000000000000000000 ) ) ;
#41499 = CARTESIAN_POINT ( 'NONE',  ( -20.64999999999999858, 85.00000000001251976, -179.9170766071767389 ) ) ;
#41500 = EDGE_CURVE ( 'NONE', #161077, #18698, #174961, .T. ) ;
#41501 = CARTESIAN_POINT ( 'NONE',  ( -21.02374657821590631, 64.39999999919233176, -176.9513107143264108 ) ) ;
#41502 = ORIENTED_EDGE ( 'NONE', *, *, #33969, .F. ) ;
#41503 = DIRECTION ( 'NONE',  ( -0.7071067811865474617, -0.7071067811865474617, -0.000000000000000000 ) ) ;
#41505 = EDGE_CURVE ( 'NONE', #43099, #146650, #62287, .T. ) ;
#41504 = DIRECTION ( 'NONE',  ( 0.000000000000000000, 0.000000000000000000, 1.000000000000000000 ) ) ;
#41506 = EDGE_LOOP ( 'NONE', ( #26591, #100726, #113671, #10822, #121953 ) ) ;
#41507 = CARTESIAN_POINT ( 'NONE',  ( 21.05000000000000426, 69.74118280533018321, -69.55674021985801403 ) ) ;
#41508 = VECTOR ( 'NONE', #62837, 1000.000000000000000 ) ;
#41509 = ORIENTED_EDGE ( 'NONE', *, *, #93372, .F. ) ;
#41510 = AXIS2_PLACEMENT_3D ( 'NONE', #159114, #156558, #194391 ) ;
#41511 = ORIENTED_EDGE ( 'NONE', *, *, #76058, .T. ) ;
#41512 = ADVANCED_FACE ( 'NONE', ( #164902 ), #127059, .F. ) ;
#41513 = DIRECTION ( 'NONE',  ( 0.000000000000000000, 0.000000000000000000, 1.000000000000000000 ) ) ;
#41514 = VERTEX_POINT ( 'NONE', #183192 ) ;
#41517 = ADVANCED_FACE ( 'NONE', ( #135701 ), #66587, .F. ) ;
#41516 = VERTEX_POINT ( 'NONE', #65796 ) ;
#41515 = LINE ( 'NONE', #83140, #80516 ) ;
#41518 = VECTOR ( 'NONE', #110231, 1000.000000000000114 ) ;
#41519 = VECTOR ( 'NONE', #207430, 1000.000000000000114 ) ;
#41520 = VECTOR ( 'NONE', #93966, 1000.000000000000114 ) ;
#41523 = ORIENTED_EDGE ( 'NONE', *, *, #92262, .F. ) ;
#41522 = ORIENTED_EDGE ( 'NONE', *, *, #3023, .T. ) ;
#41521 = DIRECTION ( 'NONE',  ( 0.000000000000000000, 0.2128009952263403282, -0.9770955615653358350 ) ) ;
#41524 = DIRECTION ( 'NONE',  ( -1.000000000000000000, 0.000000000000000000, 0.000000000000000000 ) ) ;
#41525 = CARTESIAN_POINT ( 'NONE',  ( -21.07933241753356413, 0.09337959043041976770, -161.1713540516202272 ) ) ;
#41526 = CARTESIAN_POINT ( 'NONE',  ( 23.14999999999999858, 1.115600667400684642E-11, -167.5000000000000284 ) ) ;
#41527 = CARTESIAN_POINT ( 'NONE',  ( 20.94983749550516450, 46.34703458179515678, -243.0587802416264651 ) ) ;
#41528 = DIRECTION ( 'NONE',  ( -1.000000000000000000, 0.000000000000000000, -0.000000000000000000 ) ) ;
#41529 = CARTESIAN_POINT ( 'NONE',  ( 20.95595012432474391, 65.39582078693628375, -195.9273381543061987 ) ) ;
#41530 = AXIS2_PLACEMENT_3D ( 'NONE', #111517, #68544, #9844 ) ;
#41531 = CARTESIAN_POINT ( 'NONE',  ( 20.94999999999999929, 67.49463558145296815, -195.5618716440587548 ) ) ;
#41533 = CARTESIAN_POINT ( 'NONE',  ( 18.59999999999999787, 77.83585931145526615, -58.01866831572577610 ) ) ;
#41532 = CARTESIAN_POINT ( 'NONE',  ( -16.87036670365549895, 9.989418819312803066, -46.02043988269794994 ) ) ;
#41535 = EDGE_CURVE ( 'NONE', #151810, #171180, #191506, .T. ) ;
#41534 = VECTOR ( 'NONE', #158769, 1000.000000000000000 ) ;
#41536 = VECTOR ( 'NONE', #237558, 1000.000000000000114 ) ;
#41537 = VERTEX_POINT ( 'NONE', #89207 ) ;
#41538 = AXIS2_PLACEMENT_3D ( 'NONE', #142872, #182034, #140314 ) ;
#41540 = ORIENTED_EDGE ( 'NONE', *, *, #238538, .F. ) ;
#41539 = AXIS2_PLACEMENT_3D ( 'NONE', #33759, #192793, #213623 ) ;
#41541 = FACE_OUTER_BOUND ( 'NONE', #179097, .T. ) ;
#41543 = EDGE_LOOP ( 'NONE', ( #5500, #250073, #4855 ) ) ;
#41542 = CARTESIAN_POINT ( 'NONE',  ( 21.14999999999999503, 1.619487989037824871, -230.7814958294534335 ) ) ;
#41544 = DIRECTION ( 'NONE',  ( 1.000000000000000000, 0.000000000000000000, 0.000000000000000000 ) ) ;
#41545 = VERTEX_POINT ( 'NONE', #117447 ) ;
#41546 = CIRCLE ( 'NONE', #216482, 0.1000000000000028644 ) ;
#41547 = CARTESIAN_POINT ( 'NONE',  ( 23.14999999999999503, 69.35000000001254250, -182.3731074845244109 ) ) ;
#41548 = ORIENTED_EDGE ( 'NONE', *, *, #155449, .T. ) ;
#41549 = EDGE_CURVE ( 'NONE', #161837, #214123, #58162, .T. ) ;
#41550 = ORIENTED_EDGE ( 'NONE', *, *, #230612, .F. ) ;
#41551 = CARTESIAN_POINT ( 'NONE',  ( -21.44999999999999929, 68.75000000001199396, -115.3731074845243540 ) ) ;
#41552 = DIRECTION ( 'NONE',  ( 0.000000000000000000, 1.000000000000000000, 0.000000000000000000 ) ) ;
#41553 = EDGE_CURVE ( 'NONE', #213760, #237540, #57449, .T. ) ;
#41555 = ORIENTED_EDGE ( 'NONE', *, *, #148810, .F. ) ;
#41554 = ORIENTED_EDGE ( 'NONE', *, *, #19049, .F. ) ;
#41556 = VERTEX_POINT ( 'NONE', #215258 ) ;
#41557 = CARTESIAN_POINT ( 'NONE',  ( -20.64999999999999858, 11.48697431424113446, -220.1440440112397994 ) ) ;
#41558 = EDGE_LOOP ( 'NONE', ( #96267, #219670, #235115, #129440 ) ) ;
#41559 = ORIENTED_EDGE ( 'NONE', *, *, #186631, .T. ) ;
#41560 = CARTESIAN_POINT ( 'NONE',  ( -23.25000000000000000, 76.00000000001237765, -170.0231074845243597 ) ) ;
#41562 = ORIENTED_EDGE ( 'NONE', *, *, #155188, .F. ) ;
#41561 = DIRECTION ( 'NONE',  ( -0.7071067811865475727, 0.7071067811865475727, 4.937700262164531476E-15 ) ) ;
#41564 = CARTESIAN_POINT ( 'NONE',  ( 20.95539060131842746, 65.37613784235668390, -162.3693736708682422 ) ) ;
#41563 = LINE ( 'NONE', #160231, #103299 ) ;
#41565 = EDGE_CURVE ( 'NONE', #251832, #81533, #68376, .T. ) ;
#41566 = DIRECTION ( 'NONE',  ( 0.000000000000000000, 0.4088369013363281623, -0.9126074666063771490 ) ) ;
#41567 = CARTESIAN_POINT ( 'NONE',  ( -23.15000000000000213, 8.882751598337867094, -187.0399955572217721 ) ) ;
#41568 = DIRECTION ( 'NONE',  ( 3.469446951953498700E-14, -0.7899159663865300551, -0.6132151058540831201 ) ) ;
#41569 = ORIENTED_EDGE ( 'NONE', *, *, #51428, .F. ) ;
#41570 = ADVANCED_FACE ( 'NONE', ( #29289 ), #176154, .T. ) ;
#41571 = AXIS2_PLACEMENT_3D ( 'NONE', #114559, #216205, #179674 ) ;
#41572 = ORIENTED_EDGE ( 'NONE', *, *, #40544, .T. ) ;
#41573 = CARTESIAN_POINT ( 'NONE',  ( -16.87331047859649757, 66.05000000001182059, -82.17310748452439384 ) ) ;
#41574 = CARTESIAN_POINT ( 'NONE',  ( 18.59999999999999787, -1.835341550213255957, -78.65515129256301918 ) ) ;
#41575 = DIRECTION ( 'NONE',  ( 1.000000000000000000, 0.000000000000000000, 0.000000000000000000 ) ) ;
#41576 = TOROIDAL_SURFACE ( 'NONE', #58083, 0.2000000000000000111, 0.1000000000000000056 ) ;
#41578 = EDGE_CURVE ( 'NONE', #221067, #252116, #152302, .T. ) ;
#41577 = ORIENTED_EDGE ( 'NONE', *, *, #63786, .F. ) ;
#41579 = CARTESIAN_POINT ( 'NONE',  ( 20.94999999999999929, 13.54362637910787370, -238.4879411198429580 ) ) ;
#41580 = CIRCLE ( 'NONE', #104065, 12.97499999999998721 ) ;
#41581 = DIRECTION ( 'NONE',  ( 1.000000000000000000, -0.000000000000000000, -0.000000000000000000 ) ) ;
#41582 = CARTESIAN_POINT ( 'NONE',  ( -23.25000000000000000, 65.66751761918722252, -164.4282609406112670 ) ) ;
#41583 = ORIENTED_EDGE ( 'NONE', *, *, #228926, .F. ) ;
#41584 = ORIENTED_EDGE ( 'NONE', *, *, #2086, .F. ) ;
#41585 = CARTESIAN_POINT ( 'NONE',  ( -23.25000000000000000, 1.115600667400684642E-11, -138.0500000000000114 ) ) ;
#41586 = VERTEX_POINT ( 'NONE', #154053 ) ;
#41587 = CYLINDRICAL_SURFACE ( 'NONE', #114003, 3.999999999999994671 ) ;
#41588 = ORIENTED_EDGE ( 'NONE', *, *, #73547, .T. ) ;
#41589 = ADVANCED_FACE ( 'NONE', ( #50083 ), #255614, .F. ) ;
#41590 = DIRECTION ( 'NONE',  ( 0.000000000000000000, -7.429790795770644761E-15, 1.000000000000000000 ) ) ;
#41591 = CARTESIAN_POINT ( 'NONE',  ( -23.25000000000000000, 0.000000000000000000, -33.50000000000000000 ) ) ;
#41593 = CARTESIAN_POINT ( 'NONE',  ( -21.05000000000000071, 64.25000000001250555, -177.0379132551784096 ) ) ;
#41592 = CARTESIAN_POINT ( 'NONE',  ( -18.59999999999999787, 7.021664781911246322, -204.8335654018972605 ) ) ;
#41594 = TOROIDAL_SURFACE ( 'NONE', #170793, 11.90000000000000391, 0.1000000000000000056 ) ;
#41595 = CARTESIAN_POINT ( 'NONE',  ( 22.49436431346199683, 0.06690352973341695542, -55.35004905234658423 ) ) ;
#41597 = EDGE_CURVE ( 'NONE', #186763, #6765, #193138, .T. ) ;
#41596 = DIRECTION ( 'NONE',  ( -7.304098846218134667E-16, 1.000000000000000000, 6.982962677686267499E-15 ) ) ;
#41598 = ORIENTED_EDGE ( 'NONE', *, *, #42292, .T. ) ;
#41599 = AXIS2_PLACEMENT_3D ( 'NONE', #71069, #133584, #148022 ) ;
#41601 = ORIENTED_EDGE ( 'NONE', *, *, #11976, .F. ) ;
#41600 = VERTEX_POINT ( 'NONE', #94009 ) ;
#41602 = ORIENTED_EDGE ( 'NONE', *, *, #63015, .F. ) ;
#41603 = ORIENTED_EDGE ( 'NONE', *, *, #48546, .F. ) ;
#41604 = FACE_OUTER_BOUND ( 'NONE', #166671, .T. ) ;
#41605 = CARTESIAN_POINT ( 'NONE',  ( -20.64999999999999858, 1.940186915899004161, -87.67088078894671810 ) ) ;
#41606 = CARTESIAN_POINT ( 'NONE',  ( -18.50000000000000000, 11.64999999999999680, -21.35000000000000142 ) ) ;
#41607 = CARTESIAN_POINT ( 'NONE',  ( -20.94999999999999929, 76.00000000001242029, -166.0231074845243597 ) ) ;
#41608 = LINE ( 'NONE', #121154, #42666 ) ;
#41610 = CARTESIAN_POINT ( 'NONE',  ( 21.05000000000000071, 59.10678033798690478, -225.7992625810339575 ) ) ;
#41609 = CARTESIAN_POINT ( 'NONE',  ( 18.59999999999999787, 47.95459712139159336, -246.5019368548292675 ) ) ;
#41612 = ORIENTED_EDGE ( 'NONE', *, *, #203463, .F. ) ;
#41611 = DIRECTION ( 'NONE',  ( -1.000000000000000000, 0.000000000000000000, -0.000000000000000000 ) ) ;
#41613 = CARTESIAN_POINT ( 'NONE',  ( -20.65000000000000568, 5.650000000011139001, -176.7499999999999716 ) ) ;
#41614 = ORIENTED_EDGE ( 'NONE', *, *, #212395, .T. ) ;
#41615 = DIRECTION ( 'NONE',  ( -1.000000000000000000, 1.836970198721029934E-16, 1.282749433769087582E-30 ) ) ;
#41616 = ORIENTED_EDGE ( 'NONE', *, *, #190877, .F. ) ;
#41617 = VERTEX_POINT ( 'NONE', #194434 ) ;
#41618 = CARTESIAN_POINT ( 'NONE',  ( 21.05000000000000426, 69.74118280533069480, -136.5567402198579998 ) ) ;
#41619 = LINE ( 'NONE', #221491, #172624 ) ;
#41620 = CARTESIAN_POINT ( 'NONE',  ( -18.50000000000000000, 68.97833521811203639, -132.6895420826271277 ) ) ;
#41621 = CARTESIAN_POINT ( 'NONE',  ( 14.56326696814971022, 9.446648990640017729, -82.08916329592322825 ) ) ;
#41622 = AXIS2_PLACEMENT_3D ( 'NONE', #189897, #12565, #8693 ) ;
#41623 = AXIS2_PLACEMENT_3D ( 'NONE', #201136, #125467, #146296 ) ;
#41624 = DIRECTION ( 'NONE',  ( -1.000000000000000000, -1.541880601228652843E-16, -2.878400969107353907E-16 ) ) ;
#41625 = EDGE_LOOP ( 'NONE', ( #220450, #24008, #129517 ) ) ;
#41626 = ORIENTED_EDGE ( 'NONE', *, *, #257812, .T. ) ;
#41627 = CARTESIAN_POINT ( 'NONE',  ( 16.27683809663749770, 9.350000000011137402, -143.2500000000000284 ) ) ;
#41628 = ORIENTED_EDGE ( 'NONE', *, *, #256019, .F. ) ;
#41629 = CARTESIAN_POINT ( 'NONE',  ( -21.65000000000000213, 68.75000000001202238, -115.6731074845243512 ) ) ;
#41630 = CARTESIAN_POINT ( 'NONE',  ( 23.24999999999999645, 76.00000000001165290, -69.52310748452431710 ) ) ;
#41631 = DIRECTION ( 'NONE',  ( 2.952720810173289112E-16, 0.9651348961777159730, -0.2617529984165024026 ) ) ;
#41632 = DIRECTION ( 'NONE',  ( -1.000000000000000000, -0.000000000000000000, 0.000000000000000000 ) ) ;
#41633 = DIRECTION ( 'NONE',  ( -2.952720810173289112E-16, -1.000000000000000000, -6.982962677686266711E-15 ) ) ;
#41634 = CARTESIAN_POINT ( 'NONE',  ( -20.64999999999999858, 82.48249193998721296, -215.5326005316167084 ) ) ;
#41635 = FACE_OUTER_BOUND ( 'NONE', #25836, .T. ) ;
#41636 = CARTESIAN_POINT ( 'NONE',  ( 18.49999999999999289, 65.65621891165940838, -178.6946622066474504 ) ) ;
#41637 = AXIS2_PLACEMENT_3D ( 'NONE', #197252, #77295, #58995 ) ;
#41639 = ADVANCED_FACE ( 'NONE', ( #75758 ), #10634, .F. ) ;
#41638 = DIRECTION ( 'NONE',  ( 1.000000000000000000, -0.000000000000000000, -0.000000000000000000 ) ) ;
#41640 = AXIS2_PLACEMENT_3D ( 'NONE', #128469, #222398, #105002 ) ;
#41641 = VECTOR ( 'NONE', #55662, 1000.000000000000000 ) ;
#41642 = DIRECTION ( 'NONE',  ( 1.000000000000000000, 0.000000000000000000, 0.000000000000000000 ) ) ;
#41643 = ORIENTED_EDGE ( 'NONE', *, *, #87223, .F. ) ;
#41644 = TOROIDAL_SURFACE ( 'NONE', #174947, 0.6000000000000006439, 0.1000000000000000056 ) ;
#41645 = DIRECTION ( 'NONE',  ( 1.000000000000000000, 2.952720810173289112E-16, -0.000000000000000000 ) ) ;
#41646 = ADVANCED_FACE ( 'NONE', ( #174905 ), #216410, .T. ) ;
#41647 = ORIENTED_EDGE ( 'NONE', *, *, #162049, .F. ) ;
#41648 = FACE_OUTER_BOUND ( 'NONE', #49537, .T. ) ;
#41649 = DIRECTION ( 'NONE',  ( 0.000000000000000000, -0.05689261644169250898, 0.9983803033886528011 ) ) ;
#41651 = ADVANCED_FACE ( 'NONE', ( #61322 ), #20938, .F. ) ;
#41650 = CARTESIAN_POINT ( 'NONE',  ( -22.47071067811865319, 33.41224047107334627, -242.5462774987836383 ) ) ;
#41653 = ADVANCED_FACE ( 'NONE', ( #138263 ), #79573, .T. ) ;
#41652 = AXIS2_PLACEMENT_3D ( 'NONE', #103816, #187250, #167695 ) ;
#41654 = VERTEX_POINT ( 'NONE', #44334 ) ;
#41656 = AXIS2_PLACEMENT_3D ( 'NONE', #222270, #124498, #47500 ) ;
#41655 = CARTESIAN_POINT ( 'NONE',  ( -21.64999999999999858, 63.66481329078087015, -213.2846733859786923 ) ) ;
#41657 = DIRECTION ( 'NONE',  ( -0.000000000000000000, 0.1298341882520022694, 0.9915357197604853789 ) ) ;
#41658 = CARTESIAN_POINT ( 'NONE',  ( -18.59999999999999787, 1.835341550235567887, -145.6551512925629766 ) ) ;
#41659 = CARTESIAN_POINT ( 'NONE',  ( 21.14999999999999858, 87.65000000001194280, -103.0231074845242318 ) ) ;
#41660 = CARTESIAN_POINT ( 'NONE',  ( -16.84421487269768747, 66.05000000001159322, -56.85360536207942772 ) ) ;
#41661 = ORIENTED_EDGE ( 'NONE', *, *, #105039, .F. ) ;
#41662 = DIRECTION ( 'NONE',  ( 1.000000000000000000, 0.000000000000000000, -0.000000000000000000 ) ) ;
#41664 = VERTEX_POINT ( 'NONE', #3915 ) ;
#41663 = CARTESIAN_POINT ( 'NONE',  ( 20.85000000000000142, -1.135018845899022466, -108.2169768834323662 ) ) ;
#41665 = DIRECTION ( 'NONE',  ( -1.000000000000000000, 0.000000000000000000, -0.000000000000000000 ) ) ;
#41666 = ADVANCED_FACE ( 'NONE', ( #22211 ), #19635, .T. ) ;
#41667 = CYLINDRICAL_SURFACE ( 'NONE', #157778, 2.000000000000001776 ) ;
#41668 = ORIENTED_EDGE ( 'NONE', *, *, #167821, .T. ) ;
#41669 = CARTESIAN_POINT ( 'NONE',  ( -23.25000000000000000, 1.115600667400684642E-11, -134.0000000000000000 ) ) ;
#41670 = PRODUCT_CONTEXT ( 'NONE', #78994, 'mechanical' ) ;
#41671 = DIRECTION ( 'NONE',  ( 0.000000000000000000, 0.000000000000000000, 1.000000000000000000 ) ) ;
#41672 = ORIENTED_EDGE ( 'NONE', *, *, #251909, .T. ) ;
#41673 = CARTESIAN_POINT ( 'NONE',  ( 18.59999999999999787, -1.835859311443637010, -45.00443916879852679 ) ) ;
#41674 = DIRECTION ( 'NONE',  ( 0.000000000000000000, 6.982962677686266711E-15, -1.000000000000000000 ) ) ;
#41675 = VECTOR ( 'NONE', #138857, 1000.000000000000000 ) ;
#41676 = EDGE_CURVE ( 'NONE', #31810, #170631, #99847, .T. ) ;
#41677 = VERTEX_POINT ( 'NONE', #241257 ) ;
#41678 = AXIS2_PLACEMENT_3D ( 'NONE', #39049, #35215, #114714 ) ;
#41679 = ORIENTED_EDGE ( 'NONE', *, *, #158432, .T. ) ;
#41680 = DIRECTION ( 'NONE',  ( 1.000000000000000000, 0.000000000000000000, 0.000000000000000000 ) ) ;
#41681 = CARTESIAN_POINT ( 'NONE',  ( -18.59999999999999787, -1.835341550213255957, -112.0551512925630107 ) ) ;
#41682 = DIRECTION ( 'NONE',  ( 0.000000000000000000, 0.1569827930593259702, -0.9876013379310970564 ) ) ;
#41683 = CARTESIAN_POINT ( 'NONE',  ( 21.05000000000000071, 87.65000000001144542, -39.12310748452424747 ) ) ;
#41684 = DIRECTION ( 'NONE',  ( 0.000000000000000000, -0.4999999999999689138, -0.8660254037844565822 ) ) ;
#41685 = CARTESIAN_POINT ( 'NONE',  ( 22.39999999999999503, -3.275978944802467652, -228.2735455795363748 ) ) ;
#41686 = ADVANCED_FACE ( 'NONE', ( #239967 ), #62611, .F. ) ;
#41688 = CARTESIAN_POINT ( 'NONE',  ( -20.64999999999999858, 19.98118924431957311, -235.6825596947570602 ) ) ;
#41687 = CARTESIAN_POINT ( 'NONE',  ( 20.94999999999999574, 65.52661458509899717, -95.44445302027583011 ) ) ;
#41689 = DIRECTION ( 'NONE',  ( 1.000000000000000000, 0.000000000000000000, 0.000000000000000000 ) ) ;
#41690 = LINE ( 'NONE', #181203, #222957 ) ;
#41691 = CARTESIAN_POINT ( 'NONE',  ( 22.43288208788031568, 0.004899854896538673524, -155.8503481562808872 ) ) ;
#41692 = DIRECTION ( 'NONE',  ( 1.186688945009010077E-16, -1.000000000000000000, -0.000000000000000000 ) ) ;
#41693 = AXIS2_PLACEMENT_3D ( 'NONE', #113207, #8975, #148495 ) ;
#41694 = EDGE_LOOP ( 'NONE', ( #78101, #126170, #131053 ) ) ;
#41695 = ORIENTED_EDGE ( 'NONE', *, *, #80970, .T. ) ;
#41696 = VECTOR ( 'NONE', #116124, 1000.000000000000000 ) ;
#41697 = DIRECTION ( 'NONE',  ( 0.000000000000000000, 0.000000000000000000, 1.000000000000000000 ) ) ;
#41699 = CARTESIAN_POINT ( 'NONE',  ( -21.44999999999999929, 68.65000000001229807, -157.6731074845243938 ) ) ;
#41698 = CARTESIAN_POINT ( 'NONE',  ( -22.39999999999999858, 76.00000000001273293, -211.3138870828977645 ) ) ;
#41700 = AXIS2_PLACEMENT_3D ( 'NONE', #87781, #206469, #126935 ) ;
#41701 = DIRECTION ( 'NONE',  ( 0.000000000000000000, -0.2768012769485524438, -0.9609271840673728748 ) ) ;
#41702 = DIRECTION ( 'NONE',  ( 0.000000000000000000, 0.000000000000000000, -1.000000000000000000 ) ) ;
#41703 = CARTESIAN_POINT ( 'NONE',  ( 22.39999999999999503, 11.65000000000000746, -0.1000000000000028644 ) ) ;
#41704 = EDGE_LOOP ( 'NONE', ( #138727, #170878, #247738, #197920 ) ) ;
#41705 = VECTOR ( 'NONE', #99633, 1000.000000000000000 ) ;
#41706 = CARTESIAN_POINT ( 'NONE',  ( -16.97683809663752186, 66.05000000001261640, -190.1207434663279514 ) ) ;
#41707 = AXIS2_PLACEMENT_3D ( 'NONE', #95259, #75712, #52261 ) ;
#41708 = ORIENTED_EDGE ( 'NONE', *, *, #191441, .F. ) ;
#41709 = DIRECTION ( 'NONE',  ( 0.000000000000000000, 0.000000000000000000, -1.000000000000000000 ) ) ;
#41710 = ORIENTED_EDGE ( 'NONE', *, *, #78112, .F. ) ;
#41711 = DIRECTION ( 'NONE',  ( 0.000000000000000000, 0.000000000000000000, 1.000000000000000000 ) ) ;
#41712 = CIRCLE ( 'NONE', #179101, 4.099999999999992539 ) ;
#41714 = TOROIDAL_SURFACE ( 'NONE', #20881, 11.65000000000000036, 0.1000000000000000056 ) ;
#41713 = DIRECTION ( 'NONE',  ( 0.000000000000000000, -6.982962677686266711E-15, 1.000000000000000000 ) ) ;
#41715 = AXIS2_PLACEMENT_3D ( 'NONE', #236545, #57899, #117883 ) ;
#41716 = CIRCLE ( 'NONE', #45971, 0.09999999999999328870 ) ;
#41717 = ADVANCED_FACE ( 'NONE', ( #179996 ), #43047, .T. ) ;
#41718 = ADVANCED_FACE ( 'NONE', ( #220404 ), #83091, .F. ) ;
#41719 = ORIENTED_EDGE ( 'NONE', *, *, #252346, .F. ) ;
#41720 = CYLINDRICAL_SURFACE ( 'NONE', #234967, 4.000000000000003553 ) ;
#41721 = VECTOR ( 'NONE', #175336, 1000.000000000000000 ) ;
#41722 = ORIENTED_EDGE ( 'NONE', *, *, #123801, .F. ) ;
#41723 = EDGE_CURVE ( 'NONE', #121092, #133367, #23514, .T. ) ;
#41725 = EDGE_CURVE ( 'NONE', #190614, #229669, #157902, .T. ) ;
#41724 = CYLINDRICAL_SURFACE ( 'NONE', #145325, 12.87499999999999822 ) ;
#41726 = PLANE ( 'NONE',  #91032 ) ;
#41727 = DIRECTION ( 'NONE',  ( 0.000000000000000000, 0.2617529984164506107, 0.9651348961777299618 ) ) ;
#41728 = DIRECTION ( 'NONE',  ( 1.000000000000000000, 0.000000000000000000, 0.000000000000000000 ) ) ;
#41729 = DIRECTION ( 'NONE',  ( 0.000000000000000000, 0.9770955615653548199, 0.2128009952262535920 ) ) ;
#41731 = CARTESIAN_POINT ( 'NONE',  ( 18.57399277249656322, 65.66887361445355964, -130.9329845918269370 ) ) ;
#41730 = CARTESIAN_POINT ( 'NONE',  ( -20.64999999999999858, 2.000000000011154189, -87.77537807723795993 ) ) ;
#41732 = EDGE_CURVE ( 'NONE', #137094, #170116, #217797, .T. ) ;
#41733 = CARTESIAN_POINT ( 'NONE',  ( -23.25000000000000000, 10.33248238083634440, -173.0948465439131496 ) ) ;
#41735 = ORIENTED_EDGE ( 'NONE', *, *, #18937, .T. ) ;
#41734 = CARTESIAN_POINT ( 'NONE',  ( 20.77526135991770317, 67.06799098339173781, -128.0545389417991089 ) ) ;
#41737 = DIRECTION ( 'NONE',  ( -1.000000000000000000, 0.000000000000000000, 0.000000000000000000 ) ) ;
#41736 = LINE ( 'NONE', #82093, #220150 ) ;
#41738 = EDGE_LOOP ( 'NONE', ( #113672, #199204, #224684 ) ) ;
#41740 = ORIENTED_EDGE ( 'NONE', *, *, #86351, .T. ) ;
#41739 = CARTESIAN_POINT ( 'NONE',  ( -21.64999999999999858, 29.28400589394459175, -237.3759593473670293 ) ) ;
#41741 = EDGE_CURVE ( 'NONE', #95684, #258015, #102661, .T. ) ;
#41742 = VERTEX_POINT ( 'NONE', #200835 ) ;
#41743 = CARTESIAN_POINT ( 'NONE',  ( 18.59999999999999787, 87.75000000001176659, -78.17310748452423752 ) ) ;
#41745 = ADVANCED_FACE ( 'NONE', ( #221653 ), #101691, .T. ) ;
#41744 = EDGE_CURVE ( 'NONE', #208902, #71184, #198251, .T. ) ;
#41746 = DIRECTION ( 'NONE',  ( 0.000000000000000000, -0.9770955615653317272, -0.2128009952263598126 ) ) ;
#41747 = CARTESIAN_POINT ( 'NONE',  ( -23.25000000000000000, 68.31754949648690456, -231.8498166873408763 ) ) ;
#41748 = ORIENTED_EDGE ( 'NONE', *, *, #225442, .T. ) ;
#41749 = DIRECTION ( 'NONE',  ( -1.000000000000000000, 0.000000000000000000, 0.000000000000000000 ) ) ;
#41750 = CARTESIAN_POINT ( 'NONE',  ( -18.79999999999999716, 0.000000000000000000, 33.00000000000000000 ) ) ;
#41752 = EDGE_CURVE ( 'NONE', #145626, #23243, #247659, .T. ) ;
#41751 = DIRECTION ( 'NONE',  ( -1.000000000000000000, -0.000000000000000000, -0.000000000000000000 ) ) ;
#41753 = ORIENTED_EDGE ( 'NONE', *, *, #119145, .T. ) ;
#41754 = AXIS2_PLACEMENT_3D ( 'NONE', #60361, #221979, #257232 ) ;
#41755 = LINE ( 'NONE', #104247, #144171 ) ;
#41756 = EDGE_CURVE ( 'NONE', #142525, #12040, #112377, .T. ) ;
#41757 = AXIS2_PLACEMENT_3D ( 'NONE', #219132, #100457, #108202 ) ;
#41758 = DIRECTION ( 'NONE',  ( 0.000000000000000000, -0.4088369013363280513, 0.9126074666063769270 ) ) ;
#41759 = ORIENTED_EDGE ( 'NONE', *, *, #189167, .T. ) ;
#41760 = EDGE_LOOP ( 'NONE', ( #30262, #52266, #219377, #184826 ) ) ;
#41761 = DIRECTION ( 'NONE',  ( 1.000000000000000000, -0.000000000000000000, -0.000000000000000000 ) ) ;
#41762 = ADVANCED_FACE ( 'NONE', ( #89855 ), #258065, .T. ) ;
#41763 = EDGE_CURVE ( 'NONE', #217215, #137344, #20806, .T. ) ;
#41764 = AXIS2_PLACEMENT_3D ( 'NONE', #83273, #22067, #181140 ) ;
#41765 = ORIENTED_EDGE ( 'NONE', *, *, #61307, .T. ) ;
#41766 = ORIENTED_EDGE ( 'NONE', *, *, #21790, .T. ) ;
#41767 = LINE ( 'NONE', #121321, #217642 ) ;
#41768 = EDGE_CURVE ( 'NONE', #215370, #179506, #133214, .T. ) ;
#41769 = DIRECTION ( 'NONE',  ( 1.000000000000000000, 0.000000000000000000, 0.000000000000000000 ) ) ;
#41770 = DIRECTION ( 'NONE',  ( 1.000000000000000000, 0.000000000000000000, 0.000000000000000000 ) ) ;
#41771 = CARTESIAN_POINT ( 'NONE',  ( -21.08134388332232589, 30.84685005410138103, -252.0718209705130164 ) ) ;
#41772 = LINE ( 'NONE', #200828, #41385 ) ;
#41773 = VERTEX_POINT ( 'NONE', #205961 ) ;
#41774 = EDGE_CURVE ( 'NONE', #147541, #19150, #196012, .T. ) ;
#41775 = AXIS2_PLACEMENT_3D ( 'NONE', #254612, #232535, #94270 ) ;
#41776 = CIRCLE ( 'NONE', #187521, 0.09999999999998898659 ) ;
#41777 = ADVANCED_FACE ( 'NONE', ( #88562 ), #186419, .T. ) ;
#41778 = DIRECTION ( 'NONE',  ( 1.000000000000000000, 0.000000000000000000, 0.000000000000000000 ) ) ;
#41779 = CARTESIAN_POINT ( 'NONE',  ( 23.24999999999999645, -2.100000000000002309, -33.50000000000000000 ) ) ;
#41780 = FACE_OUTER_BOUND ( 'NONE', #6527, .T. ) ;
#41781 = EDGE_LOOP ( 'NONE', ( #93904, #64874, #178006, #257211 ) ) ;
#41784 = CARTESIAN_POINT ( 'NONE',  ( 22.49231231312462853, 64.35001509633487160, -136.5841603721257513 ) ) ;
#41783 = DIRECTION ( 'NONE',  ( 1.000000000000000000, 0.000000000000000000, 0.000000000000000000 ) ) ;
#41782 = CIRCLE ( 'NONE', #204055, 0.1000000000000028644 ) ;
#41785 = ORIENTED_EDGE ( 'NONE', *, *, #107211, .F. ) ;
#41788 = ORIENTED_EDGE ( 'NONE', *, *, #84327, .F. ) ;
#41787 = DIRECTION ( 'NONE',  ( 0.000000000000000000, 8.881784197000685330E-16, -1.000000000000000000 ) ) ;
#41786 = CARTESIAN_POINT ( 'NONE',  ( 20.73486653747088937, 63.06265453764984841, -221.6175843321023819 ) ) ;
#41789 = CIRCLE ( 'NONE', #91825, 7.900000000000003908 ) ;
#41790 = ORIENTED_EDGE ( 'NONE', *, *, #48770, .T. ) ;
#41791 = DIRECTION ( 'NONE',  ( 0.000000000000000000, 0.000000000000000000, 1.000000000000000000 ) ) ;
#41792 = DIRECTION ( 'NONE',  ( 1.000000000000000000, 0.000000000000000000, 0.000000000000000000 ) ) ;
#41793 = DIRECTION ( 'NONE',  ( 0.000000000000000000, 0.8814952561688428334, -0.4721928772777349570 ) ) ;
#41794 = ORIENTED_EDGE ( 'NONE', *, *, #170429, .T. ) ;
#41795 = CARTESIAN_POINT ( 'NONE',  ( -16.86578989773640913, 66.01519019875320282, -115.5584425979021432 ) ) ;
#41796 = EDGE_CURVE ( 'NONE', #16604, #76466, #129005, .T. ) ;
#41798 = CARTESIAN_POINT ( 'NONE',  ( -18.59999999999999787, 13.96869538424788004, -210.3925794786332233 ) ) ;
#41797 =( BOUNDED_SURFACE ( )  B_SPLINE_SURFACE ( 3, 2, ( 
 ( #14266, #212460, #155072 ),
 ( #15556, #71671, #10405 ),
 ( #234569, #151198, #173368 ),
 ( #70403, #91221, #190331 ) ),
 .UNSPECIFIED., .F., .F., .F. ) 
 B_SPLINE_SURFACE_WITH_KNOTS ( ( 4, 4 ),
 ( 3, 3 ),
 ( 4.282598581317742514E-18, 0.0003124336117480847335 ),
 ( 0.000000000000000000, 1.000000000000000000 ),
 .UNSPECIFIED. ) 
 GEOMETRIC_REPRESENTATION_ITEM ( )  RATIONAL_B_SPLINE_SURFACE ( (
 ( 1.000000000000000000, 0.7040654476015048013, 1.000000000000000000),
 ( 1.000000000000000000, 0.7039193538783653503, 1.000000000000000000),
 ( 1.000000000000000000, 0.7089171279144677040, 1.000000000000000000),
 ( 1.000000000000000000, 0.7071067811865137109, 1.000000000000000000) ) ) 
 REPRESENTATION_ITEM ( '' )  SURFACE ( )  );
#41800 = DIRECTION ( 'NONE',  ( 0.000000000000000000, 0.000000000000000000, 1.000000000000000000 ) ) ;
#41799 = DIRECTION ( 'NONE',  ( 1.000000000000000000, 0.000000000000000000, 0.000000000000000000 ) ) ;
#41802 = ORIENTED_EDGE ( 'NONE', *, *, #116143, .F. ) ;
#41801 = CARTESIAN_POINT ( 'NONE',  ( 21.17356465864818560, 0.09891124101387020751, 6.422803126241725558 ) ) ;
#41803 = TOROIDAL_SURFACE ( 'NONE', #108416, 11.65000000000000036, 0.1000000000000000056 ) ;
#41804 = AXIS2_PLACEMENT_3D ( 'NONE', #191578, #207280, #7785 ) ;
#41805 = EDGE_LOOP ( 'NONE', ( #176654, #82304, #164078, #63890 ) ) ;
#41806 = CARTESIAN_POINT ( 'NONE',  ( -18.35663730107557257, 11.47390742652235573, -176.7499999999999716 ) ) ;
#41807 = DIRECTION ( 'NONE',  ( 0.000000000000000000, -6.982962677686266711E-15, 1.000000000000000000 ) ) ;
#41808 = VERTEX_POINT ( 'NONE', #50709 ) ;
#41809 = DIRECTION ( 'NONE',  ( 1.000000000000000000, 0.000000000000000000, 0.000000000000000000 ) ) ;
#41810 = VERTEX_POINT ( 'NONE', #125157 ) ;
#41811 =( BOUNDED_SURFACE ( )  B_SPLINE_SURFACE ( 3, 2, ( 
 ( #236429, #98171, #56491 ),
 ( #156927, #158226, #21272 ),
 ( #175228, #78628, #100733 ),
 ( #138582, #59045, #61651 ),
 ( #38245, #180320, #139883 ),
 ( #115203, #18674, #1660 ),
 ( #136020, #177772, #57778 ),
 ( #81191, #239009, #95629 ) ),
 .UNSPECIFIED., .F., .F., .F. ) 
 B_SPLINE_SURFACE_WITH_KNOTS ( ( 4, 2, 2, 4 ),
 ( 3, 3 ),
 ( 0.0001723339234021429623, 0.0002782939632049932365, 0.0003842540030078435377, 0.0005961740826135441401 ),
 ( 0.000000000000000000, 1.000000000000000000 ),
 .UNSPECIFIED. ) 
 GEOMETRIC_REPRESENTATION_ITEM ( )  RATIONAL_B_SPLINE_SURFACE ( (
 ( 1.000000000000000000, 0.9504532311154358926, 1.000000000000000000),
 ( 1.000000000000000000, 0.9506023220705802634, 1.000000000000000000),
 ( 1.000000000000000000, 0.9395774818187462296, 1.000000000000000000),
 ( 1.000000000000000000, 0.9079328464641803764, 1.000000000000000000),
 ( 1.000000000000000000, 0.8875702416206912027, 1.000000000000000000),
 ( 1.000000000000000000, 0.8205919608037689494, 1.000000000000000000),
 ( 1.000000000000000000, 0.7666842783600247291, 1.000000000000000000),
 ( 1.000000000000000000, 0.7071067811865302533, 1.000000000000000000) ) ) 
 REPRESENTATION_ITEM ( '' )  SURFACE ( )  );
#41812 = DIRECTION ( 'NONE',  ( 1.000000000000000000, 0.000000000000000000, 0.000000000000000000 ) ) ;
#41813 = CARTESIAN_POINT ( 'NONE',  ( 22.40000000000010516, 76.00000000001296030, -114.7735403769832345 ) ) ;
#41814 = CARTESIAN_POINT ( 'NONE',  ( 21.05000000000000071, 64.25000000001219291, -143.5379132551784096 ) ) ;
#41815 = ORIENTED_EDGE ( 'NONE', *, *, #115717, .T. ) ;
#41816 = DIRECTION ( 'NONE',  ( 1.000000000000000000, 0.000000000000000000, 0.000000000000000000 ) ) ;
#41817 = AXIS2_PLACEMENT_3D ( 'NONE', #92700, #131835, #227076 ) ;
#41818 = EDGE_CURVE ( 'NONE', #237026, #58504, #162271, .T. ) ;
#41819 = CIRCLE ( 'NONE', #195932, 4.300000000000032685 ) ;
#41820 = TOROIDAL_SURFACE ( 'NONE', #21159, 12.97499999999999609, 0.1000000000000000056 ) ;
#41822 = EDGE_CURVE ( 'NONE', #116413, #220134, #257654, .T. ) ;
#41821 = DIRECTION ( 'NONE',  ( 0.000000000000000000, -1.000000000000000000, 0.000000000000000000 ) ) ;
#41823 =( BOUNDED_SURFACE ( )  B_SPLINE_SURFACE ( 3, 2, ( 
 ( #162837, #143239, #24620 ),
 ( #183673, #4995, #246207 ),
 ( #50539, #130094, #68868 ),
 ( #111836, #7590, #49278 ) ),
 .UNSPECIFIED., .F., .F., .F. ) 
 B_SPLINE_SURFACE_WITH_KNOTS ( ( 4, 4 ),
 ( 3, 3 ),
 ( -1.908195823574487804E-17, 0.001979672783031562362 ),
 ( 0.000000000000000000, 1.000000000000000000 ),
 .UNSPECIFIED. ) 
 GEOMETRIC_REPRESENTATION_ITEM ( )  RATIONAL_B_SPLINE_SURFACE ( (
 ( 1.000000000000000000, 0.7103081912008197829, 1.000000000000000000),
 ( 1.000000000000000000, 0.7104998333558621981, 1.000000000000000000),
 ( 1.000000000000000000, 0.7107238315755282088, 1.000000000000000000),
 ( 1.000000000000000000, 0.7110073749539377319, 1.000000000000000000) ) ) 
 REPRESENTATION_ITEM ( '' )  SURFACE ( )  );
#41824 = ORIENTED_EDGE ( 'NONE', *, *, #220625, .T. ) ;
#41825 = AXIS2_PLACEMENT_3D ( 'NONE', #137513, #38435, #120566 ) ;
#41826 = ORIENTED_EDGE ( 'NONE', *, *, #39111, .T. ) ;
#41827 = VERTEX_POINT ( 'NONE', #188972 ) ;
#41828 = ADVANCED_FACE ( 'NONE', ( #26058 ), #90566, .F. ) ;
#41829 = DIRECTION ( 'NONE',  ( -1.000000000000000000, -0.000000000000000000, 0.000000000000000000 ) ) ;
#41830 = ORIENTED_EDGE ( 'NONE', *, *, #33805, .T. ) ;
#41833 = ADVANCED_FACE ( 'NONE', ( #55840 ), #72907, .F. ) ;
#41832 = ORIENTED_EDGE ( 'NONE', *, *, #90309, .F. ) ;
#41831 = CARTESIAN_POINT ( 'NONE',  ( 20.95512820512820440, 65.37615131629968346, -57.37310748452439668 ) ) ;
#41834 = ORIENTED_EDGE ( 'NONE', *, *, #166418, .F. ) ;
#41835 = EDGE_CURVE ( 'NONE', #3044, #92153, #230676, .T. ) ;
#41836 = CIRCLE ( 'NONE', #241718, 0.1000000000000001305 ) ;
#41839 = EDGE_LOOP ( 'NONE', ( #113298, #18955, #116629, #120693 ) ) ;
#41838 = VERTEX_POINT ( 'NONE', #252776 ) ;
#41837 = DIRECTION ( 'NONE',  ( 1.000000000000000000, 0.000000000000000000, 0.000000000000000000 ) ) ;
#41840 = VECTOR ( 'NONE', #157361, 1000.000000000000000 ) ;
#41841 = ORIENTED_EDGE ( 'NONE', *, *, #204225, .F. ) ;
#41842 = DIRECTION ( 'NONE',  ( 0.000000000000000000, 0.9126074666063769270, 0.4088369013363280513 ) ) ;
#41843 = DIRECTION ( 'NONE',  ( -0.000000000000000000, 1.000000000000000000, -0.000000000000000000 ) ) ;
#41844 = EDGE_CURVE ( 'NONE', #218009, #20467, #53313, .T. ) ;
#41845 = FACE_OUTER_BOUND ( 'NONE', #105744, .T. ) ;
#41846 = VERTEX_POINT ( 'NONE', #172016 ) ;
#41847 = CARTESIAN_POINT ( 'NONE',  ( 23.24999999999999645, 5.650000000011139001, -113.1500000000000483 ) ) ;
#41849 = VERTEX_POINT ( 'NONE', #135395 ) ;
#41848 = CARTESIAN_POINT ( 'NONE',  ( -23.15000000000000213, 76.00000000001190870, -103.0231074845243029 ) ) ;
#41850 = CYLINDRICAL_SURFACE ( 'NONE', #217504, 0.09999999999999939493 ) ;
#41852 = ORIENTED_EDGE ( 'NONE', *, *, #61977, .F. ) ;
#41851 = CARTESIAN_POINT ( 'NONE',  ( 18.49999999999999645, 1.115600667400684642E-11, -167.5000000000000284 ) ) ;
#41853 = ORIENTED_EDGE ( 'NONE', *, *, #85058, .T. ) ;
#41854 = DIRECTION ( 'NONE',  ( 0.000000000000000000, 0.000000000000000000, -1.000000000000000000 ) ) ;
#41855 = CARTESIAN_POINT ( 'NONE',  ( 18.58685178364169133, 85.40673308381614959, -95.89868701543650786 ) ) ;
#41856 = ORIENTED_EDGE ( 'NONE', *, *, #15416, .F. ) ;
#41857 = EDGE_LOOP ( 'NONE', ( #140118, #167724, #110091, #29134, #29088, #27199, #229357, #238217, #240956, #136978 ) ) ;
#41859 = AXIS2_PLACEMENT_3D ( 'NONE', #147904, #252120, #130890 ) ;
#41858 = DIRECTION ( 'NONE',  ( 0.000000000000000000, -6.467318590049456648E-15, 1.000000000000000000 ) ) ;
#41860 = CARTESIAN_POINT ( 'NONE',  ( -21.44999999999999929, 68.65000000001261071, -191.1731074845243938 ) ) ;
#41861 = ADVANCED_FACE ( 'NONE', ( #71610 ), #113282, .T. ) ;
#41863 = ORIENTED_EDGE ( 'NONE', *, *, #85161, .T. ) ;
#41862 = ORIENTED_EDGE ( 'NONE', *, *, #39920, .F. ) ;
#41864 = ORIENTED_EDGE ( 'NONE', *, *, #258052, .T. ) ;
#41865 = CARTESIAN_POINT ( 'NONE',  ( 21.08832698747859169, 61.96276761393131238, -221.7557866019214998 ) ) ;
#41866 = ORIENTED_EDGE ( 'NONE', *, *, #143162, .T. ) ;
#41867 = ORIENTED_EDGE ( 'NONE', *, *, #72305, .F. ) ;
#41868 = CARTESIAN_POINT ( 'NONE',  ( -18.59999999999999787, 64.35000000001205933, -124.3731074845243825 ) ) ;
#41869 = VECTOR ( 'NONE', #15327, 1000.000000000000000 ) ;
#41870 = ORIENTED_EDGE ( 'NONE', *, *, #200893, .T. ) ;
#41871 = DIRECTION ( 'NONE',  ( -1.000000000000000000, -0.000000000000000000, -0.000000000000000000 ) ) ;
#41873 = CARTESIAN_POINT ( 'NONE',  ( -18.40000000000000213, 5.650000000011139001, -180.1499999999999773 ) ) ;
#41872 = SPHERICAL_SURFACE ( 'NONE', #257026, 0.1000000000000000056 ) ;
#41874 = ADVANCED_FACE ( 'NONE', ( #134109 ), #12609, .F. ) ;
#41875 = ORIENTED_EDGE ( 'NONE', *, *, #112567, .T. ) ;
#41876 = EDGE_CURVE ( 'NONE', #114288, #33031, #245819, .T. ) ;
#41878 = ORIENTED_EDGE ( 'NONE', *, *, #127673, .T. ) ;
#41877 = ORIENTED_EDGE ( 'NONE', *, *, #88840, .T. ) ;
#41879 = CARTESIAN_POINT ( 'NONE',  ( -16.94445028196808778, 66.00793639031412852, -90.41577730610593733 ) ) ;
#41880 = LINE ( 'NONE', #106948, #128634 ) ;
#41881 = ORIENTED_EDGE ( 'NONE', *, *, #36017, .T. ) ;
#41882 = AXIS2_PLACEMENT_3D ( 'NONE', #67379, #110349, #146888 ) ;
#41883 = EDGE_CURVE ( 'NONE', #1926, #250042, #93716, .T. ) ;
#41884 = DIRECTION ( 'NONE',  ( 1.000000000000000000, 0.000000000000000000, 0.000000000000000000 ) ) ;
#41885 = ORIENTED_EDGE ( 'NONE', *, *, #200702, .F. ) ;
#41886 = ORIENTED_EDGE ( 'NONE', *, *, #253274, .T. ) ;
#41887 = CIRCLE ( 'NONE', #50216, 0.1000000000000028644 ) ;
#41888 = CARTESIAN_POINT ( 'NONE',  ( 20.94999999999999929, 1.115624548013267999E-11, -132.1000000000000227 ) ) ;
#41890 = EDGE_CURVE ( 'NONE', #28763, #214793, #173312, .T. ) ;
#41889 = ORIENTED_EDGE ( 'NONE', *, *, #249074, .T. ) ;
#41891 = CARTESIAN_POINT ( 'NONE',  ( 23.14999999999999147, 71.85000000001166143, -69.52310748452434552 ) ) ;
#41892 = DIRECTION ( 'NONE',  ( -1.000000000000000000, -0.000000000000000000, -0.000000000000000000 ) ) ;
#41893 = ORIENTED_EDGE ( 'NONE', *, *, #138471, .F. ) ;
#41894 = ADVANCED_FACE ( 'NONE', ( #74198 ), #18978, .T. ) ;
#41895 = CARTESIAN_POINT ( 'NONE',  ( -22.50000000000000000, 75.90000000001199965, -110.8138870828977218 ) ) ;
#41897 = AXIS2_PLACEMENT_3D ( 'NONE', #131508, #114516, #55784 ) ;
#41896 = CARTESIAN_POINT ( 'NONE',  ( -23.25000000000000000, -8.596261682231835621, -42.95012751715027832 ) ) ;
#41899 = CARTESIAN_POINT ( 'NONE',  ( -21.05000000000000071, 6.258316057343178862, -66.93429838967794865 ) ) ;
#41898 = DIRECTION ( 'NONE',  ( -1.000000000000000000, 2.952720810173289112E-16, 2.061873921506763405E-30 ) ) ;
#41900 = CARTESIAN_POINT ( 'NONE',  ( -18.59999999999999787, 66.85000000001150511, -48.37310748452438247 ) ) ;
#41901 = DIRECTION ( 'NONE',  ( -1.000000000000000000, -0.000000000000000000, -0.000000000000000000 ) ) ;
#41902 = DIRECTION ( 'NONE',  ( 0.000000000000000000, -6.982962677686266711E-15, 1.000000000000000000 ) ) ;
#41904 = EDGE_CURVE ( 'NONE', #168456, #163852, #95769, .T. ) ;
#41903 = DIRECTION ( 'NONE',  ( 0.7071067811865388020, -0.7071067811865561215, 0.000000000000000000 ) ) ;
#41905 = CARTESIAN_POINT ( 'NONE',  ( 20.94999999999999929, 76.00000000001170974, -69.52310748452431710 ) ) ;
#41906 = ORIENTED_EDGE ( 'NONE', *, *, #241721, .T. ) ;
#41907 = AXIS2_PLACEMENT_3D ( 'NONE', #250099, #10217, #251371 ) ;
#41908 = AXIS2_PLACEMENT_3D ( 'NONE', #182527, #115095, #33041 ) ;
#41909 = VECTOR ( 'NONE', #153582, 1000.000000000000114 ) ;
#41910 = AXIS2_PLACEMENT_3D ( 'NONE', #199421, #76873, #58584 ) ;
#41912 = ORIENTED_EDGE ( 'NONE', *, *, #34071, .T. ) ;
#41911 = EDGE_LOOP ( 'NONE', ( #20504, #129857, #154406, #34367 ) ) ;
#41913 = ORIENTED_EDGE ( 'NONE', *, *, #70471, .F. ) ;
#41914 = ORIENTED_EDGE ( 'NONE', *, *, #40727, .F. ) ;
#41916 = EDGE_CURVE ( 'NONE', #144975, #98899, #66184, .T. ) ;
#41915 = FACE_OUTER_BOUND ( 'NONE', #88704, .T. ) ;
#41917 = DIRECTION ( 'NONE',  ( 0.000000000000000000, -0.1298341882519953583, -0.9915357197604862671 ) ) ;
#41919 = CARTESIAN_POINT ( 'NONE',  ( -14.45443560709636444, 9.450592112133699985, -15.05618831880839537 ) ) ;
#41918 = CARTESIAN_POINT ( 'NONE',  ( 20.85000000000000142, 87.65000000001170122, -69.52310748452423184 ) ) ;
#41920 = CARTESIAN_POINT ( 'NONE',  ( 20.94999999999999929, 67.07338541492521244, -161.5514244653012952 ) ) ;
#41921 = ORIENTED_EDGE ( 'NONE', *, *, #60769, .T. ) ;
#41922 = DIRECTION ( 'NONE',  ( 1.000000000000000000, 0.000000000000000000, 0.000000000000000000 ) ) ;
#41923 = TOROIDAL_SURFACE ( 'NONE', #104228, 4.149999999999999467, 0.1000000000000000056 ) ;
#41924 = DIRECTION ( 'NONE',  ( 0.000000000000000000, 0.1568667991644863147, -0.9876197685951252359 ) ) ;
#41925 = FACE_OUTER_BOUND ( 'NONE', #98545, .T. ) ;
#41926 = DIRECTION ( 'NONE',  ( 0.000000000000000000, -0.9770955615653316162, -0.2128009952263604232 ) ) ;
#41927 = ORIENTED_EDGE ( 'NONE', *, *, #191536, .T. ) ;
#41928 = CARTESIAN_POINT ( 'NONE',  ( 13.40000000000005898, 64.35000000001120668, -23.62310748452479103 ) ) ;
#41929 = CARTESIAN_POINT ( 'NONE',  ( 20.85000000000000142, 76.00000000001244871, -170.0231074845243597 ) ) ;
#41930 = ORIENTED_EDGE ( 'NONE', *, *, #35122, .T. ) ;
#41931 = DIRECTION ( 'NONE',  ( 0.000000000000000000, -0.9999631594459057471, 0.008583690987121077309 ) ) ;
#41932 = CARTESIAN_POINT ( 'NONE',  ( -23.15000000000000213, -8.663551401858004652, -110.0241011180673354 ) ) ;
#41933 = DIRECTION ( 'NONE',  ( 7.304098846218134667E-16, -1.000000000000000000, -6.982962677686267499E-15 ) ) ;
#41934 = CYLINDRICAL_SURFACE ( 'NONE', #154266, 0.9000000000000014655 ) ;
#41935 = ORIENTED_EDGE ( 'NONE', *, *, #137017, .F. ) ;
#41936 = DIRECTION ( 'NONE',  ( 0.000000000000000000, 0.000000000000000000, -1.000000000000000000 ) ) ;
#41937 = DIRECTION ( 'NONE',  ( -1.000000000000000000, 0.000000000000000000, -0.000000000000000000 ) ) ;
#41938 = TOROIDAL_SURFACE ( 'NONE', #79298, 0.2000000000000000111, 0.1000000000000000056 ) ;
#41939 = FACE_OUTER_BOUND ( 'NONE', #65859, .T. ) ;
#41941 = CARTESIAN_POINT ( 'NONE',  ( 18.60000000000000142, 9.122720154857409725, -245.4644708025847990 ) ) ;
#41940 = LINE ( 'NONE', #163163, #65875 ) ;
#41942 = DIRECTION ( 'NONE',  ( 0.000000000000000000, 0.2617529984165152257, 0.9651348961777124202 ) ) ;
#41943 = AXIS2_PLACEMENT_3D ( 'NONE', #122315, #61042, #181016 ) ;
#41944 = DIRECTION ( 'NONE',  ( -1.646408749285562691E-14, -1.000000000000000000, -6.982962677686266711E-15 ) ) ;
#41945 = DIRECTION ( 'NONE',  ( 0.000000000000000000, -0.2617529984165031243, -0.9651348961777158619 ) ) ;
#41946 = CARTESIAN_POINT ( 'NONE',  ( 18.49999999999999645, -9.419078080838366063, -207.8299253502082706 ) ) ;
#41949 = ORIENTED_EDGE ( 'NONE', *, *, #239089, .T. ) ;
#41948 = CIRCLE ( 'NONE', #46190, 12.97499999999999964 ) ;
#41947 = CARTESIAN_POINT ( 'NONE',  ( 20.94999999999999929, 5.400000000011154988, -124.1060308773475924 ) ) ;
#41950 = VERTEX_POINT ( 'NONE', #53085 ) ;
#41951 = VECTOR ( 'NONE', #67555, 1000.000000000000000 ) ;
#41952 = ADVANCED_FACE ( 'NONE', ( #235565 ), #173092, .T. ) ;
#41953 = FILL_AREA_STYLE_COLOUR ( '', #195254 ) ;
#41954 = CIRCLE ( 'NONE', #200153, 0.1000000000000124678 ) ;
#41955 = EDGE_CURVE ( 'NONE', #243771, #249368, #79202, .T. ) ;
#41956 = EDGE_CURVE ( 'NONE', #119060, #91291, #4201, .T. ) ;
#41957 = CARTESIAN_POINT ( 'NONE',  ( -20.94999999999999929, 11.65000000001115232, -167.5000000000000284 ) ) ;
#41958 = CARTESIAN_POINT ( 'NONE',  ( 15.75000000000000000, 9.350000000011142731, -150.5185689574027208 ) ) ;
#41959 = CIRCLE ( 'NONE', #21117, 0.09999999999998898659 ) ;
#41960 = ORIENTED_EDGE ( 'NONE', *, *, #191870, .T. ) ;
#41961 = LINE ( 'NONE', #120234, #209538 ) ;
#41962 = CARTESIAN_POINT ( 'NONE',  ( -18.59999999999999787, 78.52025535392039046, -230.5241873323956554 ) ) ;
#41964 = DIRECTION ( 'NONE',  ( -1.000000000000000000, 0.000000000000000000, 0.000000000000000000 ) ) ;
#41963 = AXIS2_PLACEMENT_3D ( 'NONE', #186828, #46008, #228521 ) ;
#41965 = DIRECTION ( 'NONE',  ( -1.000000000000000000, -0.000000000000000000, -0.000000000000000000 ) ) ;
#41967 = ORIENTED_EDGE ( 'NONE', *, *, #173643, .F. ) ;
#41966 = DIRECTION ( 'NONE',  ( -3.265361837132813093E-16, 1.000000000000000000, 0.000000000000000000 ) ) ;
#41969 = DIRECTION ( 'NONE',  ( 0.000000000000000000, 6.982962677686266711E-15, -1.000000000000000000 ) ) ;
#41968 = DIRECTION ( 'NONE',  ( -1.073024830501117725E-15, -0.000000000000000000, -1.000000000000000000 ) ) ;
#41970 = EDGE_CURVE ( 'NONE', #46643, #227800, #237446, .T. ) ;
#41971 = DIRECTION ( 'NONE',  ( 1.000000000000000000, 0.000000000000000000, 0.000000000000000000 ) ) ;
#41972 = DIRECTION ( 'NONE',  ( -0.000000000000000000, -0.8814952561688430555, 0.4721928772777346239 ) ) ;
#41973 = ORIENTED_EDGE ( 'NONE', *, *, #200462, .F. ) ;
#41974 = CARTESIAN_POINT ( 'NONE',  ( 0.000000000000000000, 0.000000000000000000, 0.000000000000000000 ) ) ;
#41975 = FACE_OUTER_BOUND ( 'NONE', #96161, .T. ) ;
#41976 = CARTESIAN_POINT ( 'NONE',  ( 23.14999999999999503, 61.90000000001218439, -142.1234050956638271 ) ) ;
#41977 = CIRCLE ( 'NONE', #50306, 0.1000000000000028644 ) ;
#41978 = ORIENTED_EDGE ( 'NONE', *, *, #184171, .F. ) ;
#41979 = CARTESIAN_POINT ( 'NONE',  ( -21.05000000000000071, 43.86852340793510763, -246.3213511806884810 ) ) ;
#41980 = DIRECTION ( 'NONE',  ( 0.000000000000000000, 0.000000000000000000, -1.000000000000000000 ) ) ;
#41981 = ORIENTED_EDGE ( 'NONE', *, *, #218304, .T. ) ;
#41982 = DIRECTION ( 'NONE',  ( 0.000000000000000000, -0.2605042016806740079, 0.9654727137038698892 ) ) ;
#41983 = CARTESIAN_POINT ( 'NONE',  ( -20.07928932188135107, 52.28206630536941901, -232.4484891355802461 ) ) ;
#41984 = DIRECTION ( 'NONE',  ( 0.000000000000000000, 0.9654727137038715545, -0.2605042016806676242 ) ) ;
#41985 = EDGE_CURVE ( 'NONE', #28439, #51036, #100036, .T. ) ;
#41986 = VERTEX_POINT ( 'NONE', #54368 ) ;
#41987 = ADVANCED_FACE ( 'NONE', ( #195199 ), #153529, .T. ) ;
#41988 = VERTEX_POINT ( 'NONE', #156076 ) ;
#41989 = CARTESIAN_POINT ( 'NONE',  ( 23.24999999999999289, 69.55000000001277272, -215.2731074845244166 ) ) ;
#41990 = DIRECTION ( 'NONE',  ( -1.000000000000000000, 0.000000000000000000, 0.000000000000000000 ) ) ;
#41991 = AXIS2_PLACEMENT_3D ( 'NONE', #64504, #144021, #223552 ) ;
#41992 = CYLINDRICAL_SURFACE ( 'NONE', #70320, 2.600000000000001421 ) ;
#41994 = CARTESIAN_POINT ( 'NONE',  ( -18.40000000000000213, 64.52683809664901560, -45.27310748452439526 ) ) ;
#41993 = AXIS2_PLACEMENT_3D ( 'NONE', #241113, #201972, #39061 ) ;
#41995 = EDGE_CURVE ( 'NONE', #207709, #206067, #16701, .T. ) ;
#41998 = CARTESIAN_POINT ( 'NONE',  ( -18.59999999999999787, 85.40000000001184333, -95.72584772486095517 ) ) ;
#41997 = TOROIDAL_SURFACE ( 'NONE', #116994, 11.70000000000000462, 0.1000000000000000056 ) ;
#41996 = CARTESIAN_POINT ( 'NONE',  ( -16.85939591225058720, 12.43626824939381770, -211.5553831086668026 ) ) ;
#41999 = CYLINDRICAL_SURFACE ( 'NONE', #115037, 0.1000000000000028644 ) ;
#42000 = DIRECTION ( 'NONE',  ( 0.000000000000000000, 0.000000000000000000, -1.000000000000000000 ) ) ;
#42001 = CYLINDRICAL_SURFACE ( 'NONE', #184520, 0.1000000000000028644 ) ;
#42002 = ORIENTED_EDGE ( 'NONE', *, *, #119535, .F. ) ;
#42003 = DIRECTION ( 'NONE',  ( 0.000000000000000000, 0.2128009952263485993, -0.9770955615653341697 ) ) ;
#42005 = ORIENTED_EDGE ( 'NONE', *, *, #68755, .T. ) ;
#42004 = DIRECTION ( 'NONE',  ( 1.000000000000000000, 0.000000000000000000, 0.000000000000000000 ) ) ;
#42006 = DIRECTION ( 'NONE',  ( 0.000000000000000000, -1.000000000000000000, 0.000000000000000000 ) ) ;
#42007 = DIRECTION ( 'NONE',  ( 1.000000000000000000, 0.000000000000000000, 0.000000000000000000 ) ) ;
#42009 = DIRECTION ( 'NONE',  ( 1.000000000000000000, 0.000000000000000000, 0.000000000000000000 ) ) ;
#42008 = CARTESIAN_POINT ( 'NONE',  ( -16.94445028196807002, 14.20918193489391790, -219.2878138714100373 ) ) ;
#42010 = VERTEX_POINT ( 'NONE', #72685 ) ;
#42012 = DIRECTION ( 'NONE',  ( 1.000000000000000000, 0.000000000000000000, 0.000000000000000000 ) ) ;
#42011 = CARTESIAN_POINT ( 'NONE',  ( -18.59999999999999787, 8.006782298343173565, -209.8034900594678618 ) ) ;
#42013 = CARTESIAN_POINT ( 'NONE',  ( 20.94999999999999929, 71.00000000001223555, -148.4283735034374843 ) ) ;
#42014 = DIRECTION ( 'NONE',  ( -1.000000000000000000, 2.849773892568378313E-16, -7.728835255496647986E-17 ) ) ;
#42015 = CARTESIAN_POINT ( 'NONE',  ( -21.05000000000000071, 28.58935552370083144, -258.2621935127861548 ) ) ;
#42016 = EDGE_LOOP ( 'NONE', ( #42909, #85309, #91659, #158564 ) ) ;
#42017 = DIRECTION ( 'NONE',  ( 1.000000000000000000, -0.000000000000000000, -0.000000000000000000 ) ) ;
#42019 = ORIENTED_EDGE ( 'NONE', *, *, #31208, .T. ) ;
#42018 = AXIS2_PLACEMENT_3D ( 'NONE', #216431, #135604, #172229 ) ;
#42020 = EDGE_CURVE ( 'NONE', #241077, #174819, #19090, .T. ) ;
#42021 = LINE ( 'NONE', #202356, #184339 ) ;
#42022 = ORIENTED_EDGE ( 'NONE', *, *, #127389, .F. ) ;
#42023 = DIRECTION ( 'NONE',  ( 0.000000000000000000, 0.000000000000000000, -1.000000000000000000 ) ) ;
#42024 = ORIENTED_EDGE ( 'NONE', *, *, #172856, .F. ) ;
#42025 = CARTESIAN_POINT ( 'NONE',  ( -21.05000000000000071, 87.65000000001172964, -72.42310748452422331 ) ) ;
#42026 = EDGE_CURVE ( 'NONE', #197787, #7520, #154298, .T. ) ;
#42027 = CARTESIAN_POINT ( 'NONE',  ( 18.60000000000000142, 85.40000000001204228, -129.2258477248609267 ) ) ;
#42028 = EDGE_LOOP ( 'NONE', ( #63165, #115313, #183566, #92146 ) ) ;
#42029 = CIRCLE ( 'NONE', #104341, 0.09999999999999543976 ) ;
#42030 = EDGE_CURVE ( 'NONE', #112737, #90934, #50009, .T. ) ;
#42032 = ADVANCED_FACE ( 'NONE', ( #96051 ), #193900, .T. ) ;
#42031 = DIRECTION ( 'NONE',  ( -1.000000000000000000, -0.000000000000000000, -0.000000000000000000 ) ) ;
#42033 = CARTESIAN_POINT ( 'NONE',  ( 22.47071067811865319, 68.27992525551410097, -136.6221999392269595 ) ) ;
#42034 = CARTESIAN_POINT ( 'NONE',  ( 20.85000000106584750, 11.75000000001115907, -160.6555046564734539 ) ) ;
#42035 = AXIS2_PLACEMENT_3D ( 'NONE', #64720, #84226, #166426 ) ;
#42036 = CARTESIAN_POINT ( 'NONE',  ( -23.15000000000000213, 1.115600667400684642E-11, -188.1249999999999716 ) ) ;
#42037 = CARTESIAN_POINT ( 'NONE',  ( 20.94999999999999929, 76.00000000001126921, -203.5231074845248997 ) ) ;
#42040 = CARTESIAN_POINT ( 'NONE',  ( 13.76927104934458335, 62.03428458984606664, -218.8918409208596074 ) ) ;
#42039 = CIRCLE ( 'NONE', #204507, 7.899999999999987921 ) ;
#42038 = ADVANCED_BREP_SHAPE_REPRESENTATION ( '', ( #21812, #2425 ), #94000 ) ;
#42041 = ORIENTED_EDGE ( 'NONE', *, *, #239190, .T. ) ;
#42042 = FACE_OUTER_BOUND ( 'NONE', #203761, .T. ) ;
#42043 = EDGE_LOOP ( 'NONE', ( #111940, #190056, #59931, #36495 ) ) ;
#42045 = ORIENTED_EDGE ( 'NONE', *, *, #123320, .F. ) ;
#42044 = CARTESIAN_POINT ( 'NONE',  ( -16.86757978335471719, 66.03434962097757932, -90.42510283135686677 ) ) ;
#42046 = EDGE_CURVE ( 'NONE', #156025, #13346, #174373, .T. ) ;
#42047 = ORIENTED_EDGE ( 'NONE', *, *, #167538, .T. ) ;
#42048 = FACE_OUTER_BOUND ( 'NONE', #172501, .T. ) ;
#42049 = EDGE_CURVE ( 'NONE', #91291, #23607, #183275, .T. ) ;
#42050 = FACE_OUTER_BOUND ( 'NONE', #27488, .T. ) ;
#42051 = CARTESIAN_POINT ( 'NONE',  ( 21.06280952165509746, 60.16910602115198969, -221.2948844812638924 ) ) ;
#42052 = CARTESIAN_POINT ( 'NONE',  ( -0.8999999999999993561, -11.75000000000000000, 26.00000000000000355 ) ) ;
#42053 = AXIS2_PLACEMENT_3D ( 'NONE', #23687, #121502, #125330 ) ;
#42054 = ORIENTED_EDGE ( 'NONE', *, *, #42262, .F. ) ;
#42055 = CARTESIAN_POINT ( 'NONE',  ( 22.10000000000000497, -11.65000000000000036, 12.09999999999999609 ) ) ;
#42057 = EDGE_CURVE ( 'NONE', #70458, #57517, #37398, .T. ) ;
#42056 = CARTESIAN_POINT ( 'NONE',  ( -16.83794237512073266, 66.07364077890480303, -157.2195653258254424 ) ) ;
#42058 = ORIENTED_EDGE ( 'NONE', *, *, #211006, .T. ) ;
#42059 = CARTESIAN_POINT ( 'NONE',  ( -20.89192007715127986, 10.32898536000685574, -39.08266832227643306 ) ) ;
#42060 = EDGE_CURVE ( 'NONE', #209479, #100484, #154787, .T. ) ;
#42061 = DIRECTION ( 'NONE',  ( 0.7071067811865388020, -0.7071067811865561215, 0.000000000000000000 ) ) ;
#42062 = AXIS2_PLACEMENT_3D ( 'NONE', #134998, #35947, #5764 ) ;
#42063 = ORIENTED_EDGE ( 'NONE', *, *, #187207, .T. ) ;
#42064 = CARTESIAN_POINT ( 'NONE',  ( -16.88783316861821859, 9.950000000011137047, -146.7522640419797995 ) ) ;
#42065 = ADVANCED_FACE ( 'NONE', ( #132637 ), #104154, .T. ) ;
#42067 = EDGE_CURVE ( 'NONE', #2443, #128224, #33577, .T. ) ;
#42066 = TOROIDAL_SURFACE ( 'NONE', #125251, 11.65000000000000036, 0.1000000000000000056 ) ;
#42068 = CIRCLE ( 'NONE', #175344, 11.79999999999999361 ) ;
#42069 = CARTESIAN_POINT ( 'NONE',  ( 20.96077737575347300, 64.37609936600719607, -109.8823155274179584 ) ) ;
#42070 = ORIENTED_EDGE ( 'NONE', *, *, #152175, .F. ) ;
#42071 = CARTESIAN_POINT ( 'NONE',  ( -20.94999999999999929, 77.13501884592227498, -128.8061306010920362 ) ) ;
#42072 = TOROIDAL_SURFACE ( 'NONE', #71286, 11.65000000000000036, 0.1000000000000000056 ) ;
#42073 = EDGE_CURVE ( 'NONE', #134077, #248044, #130671, .T. ) ;
#42074 = DIRECTION ( 'NONE',  ( 0.000000000000000000, 0.000000000000000000, 1.000000000000000000 ) ) ;
#42075 = DIRECTION ( 'NONE',  ( 1.000000000000000000, -7.304098846218134667E-16, -5.100424963727256530E-30 ) ) ;
#42076 = VECTOR ( 'NONE', #167900, 1000.000000000000000 ) ;
#42077 = AXIS2_PLACEMENT_3D ( 'NONE', #144312, #85613, #69966 ) ;
#42078 = CARTESIAN_POINT ( 'NONE',  ( 20.85000000000000142, 64.25000000001219291, -143.3069731475025321 ) ) ;
#42079 = ADVANCED_FACE ( 'NONE', ( #241990 ), #676, .T. ) ;
#42080 = EDGE_CURVE ( 'NONE', #191054, #201931, #183310, .T. ) ;
#42081 = ADVANCED_FACE ( 'NONE', ( #60775 ), #180747, .F. ) ;
#42082 = DIRECTION ( 'NONE',  ( 1.000000000000000000, 0.000000000000000000, 0.000000000000000000 ) ) ;
#42083 = DIRECTION ( 'NONE',  ( 0.000000000000000000, -0.8814952561688430555, 0.4721928772777346239 ) ) ;
#42084 = AXIS2_PLACEMENT_3D ( 'NONE', #117002, #98672, #223785 ) ;
#42085 = AXIS2_PLACEMENT_3D ( 'NONE', #90154, #171053, #71914 ) ;
#42086 = CIRCLE ( 'NONE', #79634, 0.2000000000000057288 ) ;
#42087 = ORIENTED_EDGE ( 'NONE', *, *, #37650, .F. ) ;
#42089 = FACE_OUTER_BOUND ( 'NONE', #112702, .T. ) ;
#42088 = VECTOR ( 'NONE', #133653, 1000.000000000000114 ) ;
#42090 = AXIS2_PLACEMENT_3D ( 'NONE', #156204, #113198, #14121 ) ;
#42091 = EDGE_LOOP ( 'NONE', ( #241259, #9184, #164050, #82562 ) ) ;
#42092 = CARTESIAN_POINT ( 'NONE',  ( -20.94999999999999929, -11.29603075032412995, -36.54789915966387071 ) ) ;
#42093 = CARTESIAN_POINT ( 'NONE',  ( 21.87500000000000355, 9.750000000011153745, -146.3500000000000227 ) ) ;
#42095 = VERTEX_POINT ( 'NONE', #124621 ) ;
#42094 = DIRECTION ( 'NONE',  ( -0.000000000000000000, 0.2128009952263604232, -0.9770955615653316162 ) ) ;
#42096 = CARTESIAN_POINT ( 'NONE',  ( 22.39999999999999858, 33.38250548509083870, -242.4821227592188961 ) ) ;
#42097 = EDGE_CURVE ( 'NONE', #243775, #22457, #79040, .T. ) ;
#42098 = SURFACE_SIDE_STYLE ('',( #61638 ) ) ;
#42099 = CARTESIAN_POINT ( 'NONE',  ( 21.12230431290520016, 75.99479014832300550, -109.4806741378173456 ) ) ;
#42100 = CARTESIAN_POINT ( 'NONE',  ( -16.81930730667006557, 9.936998068885204205, -79.72676773053824206 ) ) ;
#42101 = EDGE_CURVE ( 'NONE', #23723, #131609, #25529, .T. ) ;
#42102 = CARTESIAN_POINT ( 'NONE',  ( 20.90000000000000213, 11.49641995933507843, -1.885425182446133885 ) ) ;
#42103 = DIRECTION ( 'NONE',  ( 0.000000000000000000, -1.000000000000000000, 0.000000000000000000 ) ) ;
#42104 = CIRCLE ( 'NONE', #254429, 0.5000000000000004441 ) ;
#42106 = ORIENTED_EDGE ( 'NONE', *, *, #110975, .F. ) ;
#42105 = CARTESIAN_POINT ( 'NONE',  ( 21.05000000000000071, 67.22371710471982453, -157.8731074845244109 ) ) ;
#42107 = DIRECTION ( 'NONE',  ( -1.000000000000000000, 0.000000000000000000, 0.000000000000000000 ) ) ;
#42108 = ORIENTED_EDGE ( 'NONE', *, *, #117843, .T. ) ;
#42109 = ORIENTED_EDGE ( 'NONE', *, *, #228921, .T. ) ;
#42110 = CARTESIAN_POINT ( 'NONE',  ( -21.14999999999999858, 11.75000000001115552, -107.2838656629781866 ) ) ;
#42111 = PLANE ( 'NONE',  #184656 ) ;
#42112 = ORIENTED_EDGE ( 'NONE', *, *, #142596, .T. ) ;
#42113 = CARTESIAN_POINT ( 'NONE',  ( 18.59999999999999076, 10.20857864376269575, -21.25000000000000000 ) ) ;
#42114 = VECTOR ( 'NONE', #36372, 1000.000000000000000 ) ;
#42115 = CARTESIAN_POINT ( 'NONE',  ( -18.59999996769639097, 85.36327376984198168, -62.34161356905849516 ) ) ;
#42116 = ADVANCED_FACE ( 'NONE', ( #240716 ), #218559, .T. ) ;
#42117 = EDGE_LOOP ( 'NONE', ( #163401, #116206, #41719, #111509 ) ) ;
#42119 = EDGE_CURVE ( 'NONE', #179081, #196849, #32913, .T. ) ;
#42118 = CARTESIAN_POINT ( 'NONE',  ( -21.05000000000000071, 74.73821383144657204, -61.43660852097884373 ) ) ;
#42120 = B_SPLINE_CURVE_WITH_KNOTS ( 'NONE', 3,
 ( #258018, #222778, #102825, #162847, #104108, #182402 ),
 .UNSPECIFIED., .F., .F.,
 ( 4, 2, 4 ),
 ( 0.000000000000000000, 0.0001895189928937387276, 0.0003790379857874774552 ),
 .UNSPECIFIED. ) ;
#42121 = CARTESIAN_POINT ( 'NONE',  ( 20.94999999999999929, -12.41227409413852811, -164.5000000000000000 ) ) ;
#42123 = ORIENTED_EDGE ( 'NONE', *, *, #53023, .F. ) ;
#42122 = AXIS2_PLACEMENT_3D ( 'NONE', #110213, #208062, #108930 ) ;
#42124 = ORIENTED_EDGE ( 'NONE', *, *, #104048, .T. ) ;
#42125 = CARTESIAN_POINT ( 'NONE',  ( -21.14999999999999858, 7.128833340093095217, -233.7327013124392749 ) ) ;
#42126 = ORIENTED_EDGE ( 'NONE', *, *, #128289, .F. ) ;
#42127 = DIRECTION ( 'NONE',  ( 1.000000000000000000, 0.000000000000000000, 0.000000000000000000 ) ) ;
#42128 = EDGE_LOOP ( 'NONE', ( #66182, #226781, #145223, #39079 ) ) ;
#42130 = ORIENTED_EDGE ( 'NONE', *, *, #27115, .T. ) ;
#42129 = SPHERICAL_SURFACE ( 'NONE', #71839, 0.1000000000000000056 ) ;
#42131 = DIRECTION ( 'NONE',  ( 0.000000000000000000, -0.8660254037844468122, -0.4999999999999859557 ) ) ;
#42132 = ORIENTED_EDGE ( 'NONE', *, *, #62711, .T. ) ;
#42133 = CARTESIAN_POINT ( 'NONE',  ( -22.00411653889212005, 0.09903810579721090968, -93.24655713235959809 ) ) ;
#42134 = VERTEX_POINT ( 'NONE', #219856 ) ;
#42136 = ORIENTED_EDGE ( 'NONE', *, *, #49743, .T. ) ;
#42135 = EDGE_LOOP ( 'NONE', ( #56063, #62946, #93263, #193294 ) ) ;
#42137 = LINE ( 'NONE', #99493, #36205 ) ;
#42138 = ADVANCED_FACE ( 'NONE', ( #200304 ), #75154, .T. ) ;
#42139 = DIRECTION ( 'NONE',  ( 0.000000000000000000, 0.000000000000000000, -1.000000000000000000 ) ) ;
#42140 = EDGE_LOOP ( 'NONE', ( #152284, #192627, #114710, #63277, #162262 ) ) ;
#42141 = TOROIDAL_SURFACE ( 'NONE', #79516, 6.258578643762712446, 0.1000000000000000056 ) ;
#42142 = AXIS2_PLACEMENT_3D ( 'NONE', #55866, #238377, #157609 ) ;
#42143 = ORIENTED_EDGE ( 'NONE', *, *, #64497, .T. ) ;
#42144 = CARTESIAN_POINT ( 'NONE',  ( -18.59999999999999787, 61.41373750439892376, -221.5848334931070553 ) ) ;
#42145 = DIRECTION ( 'NONE',  ( 1.000000000000000000, -0.000000000000000000, -0.000000000000000000 ) ) ;
#42147 = ORIENTED_EDGE ( 'NONE', *, *, #71789, .T. ) ;
#42146 = CARTESIAN_POINT ( 'NONE',  ( -22.10000000000000497, 11.99999999999999822, 12.09999999999999964 ) ) ;
#42148 = CARTESIAN_POINT ( 'NONE',  ( -23.15000000000000213, 0.000000000000000000, 0.000000000000000000 ) ) ;
#42149 = ORIENTED_EDGE ( 'NONE', *, *, #127354, .F. ) ;
#42150 = FACE_OUTER_BOUND ( 'NONE', #36932, .T. ) ;
#42151 = LINE ( 'NONE', #85072, #156258 ) ;
#42152 = EDGE_LOOP ( 'NONE', ( #124855, #237150, #253469, #106676, #135474 ) ) ;
#42153 = CARTESIAN_POINT ( 'NONE',  ( -21.05000000000000426, -1.362148144022342189, -194.8444205686345754 ) ) ;
#42154 = PLANE ( 'NONE',  #44574 ) ;
#42155 = DIRECTION ( 'NONE',  ( 0.000000000000000000, 0.2617529984165033463, 0.9651348961777157509 ) ) ;
#42156 = VERTEX_POINT ( 'NONE', #102445 ) ;
#42157 = CARTESIAN_POINT ( 'NONE',  ( 20.94999999999999574, -11.74999999998883560, -170.5999999999999659 ) ) ;
#42158 = VERTEX_POINT ( 'NONE', #69797 ) ;
#42159 = ORIENTED_EDGE ( 'NONE', *, *, #225924, .T. ) ;
#42160 = ORIENTED_EDGE ( 'NONE', *, *, #152814, .F. ) ;
#42161 = ORIENTED_EDGE ( 'NONE', *, *, #126090, .F. ) ;
#42162 = CARTESIAN_POINT ( 'NONE',  ( -18.59999999999999787, 16.44800918141279311, -240.8068063186265135 ) ) ;
#42163 = ORIENTED_EDGE ( 'NONE', *, *, #50153, .T. ) ;
#42164 = CYLINDRICAL_SURFACE ( 'NONE', #59094, 0.09999999999999982514 ) ;
#42165 = ORIENTED_EDGE ( 'NONE', *, *, #111288, .T. ) ;
#42166 = DIRECTION ( 'NONE',  ( 0.000000000000000000, 0.000000000000000000, -1.000000000000000000 ) ) ;
#42167 = DIRECTION ( 'NONE',  ( 1.000000000000000000, 0.000000000000000000, 0.000000000000000000 ) ) ;
#42168 = ADVANCED_FACE ( 'NONE', ( #48919 ), #30679, .T. ) ;
#42169 = ORIENTED_EDGE ( 'NONE', *, *, #235174, .T. ) ;
#42170 = AXIS2_PLACEMENT_3D ( 'NONE', #124190, #147588, #162038 ) ;
#42171 = AXIS2_PLACEMENT_3D ( 'NONE', #90453, #132164, #170056 ) ;
#42172 = TOROIDAL_SURFACE ( 'NONE', #187915, 2.100000000000002309, 0.1000000000000000056 ) ;
#42173 = EDGE_CURVE ( 'NONE', #79959, #239049, #189728, .T. ) ;
#42174 = ORIENTED_EDGE ( 'NONE', *, *, #113665, .F. ) ;
#42175 = AXIS2_PLACEMENT_3D ( 'NONE', #199106, #36203, #59554 ) ;
#42176 = EDGE_LOOP ( 'NONE', ( #143607, #114057, #257289, #238476 ) ) ;
#42177 = ADVANCED_FACE ( 'NONE', ( #127189 ), #125885, .F. ) ;
#42178 = CARTESIAN_POINT ( 'NONE',  ( -22.45305610364634674, -0.1008583690875579503, -155.7504328765105583 ) ) ;
#42179 = ADVANCED_FACE ( 'NONE', ( #185867, #170217, #244551, #129748, #5926 ), #31962, .T. ) ;
#42180 = FACE_OUTER_BOUND ( 'NONE', #216843, .T. ) ;
#42181 = DIRECTION ( 'NONE',  ( 0.000000000000000000, 1.000000000000000000, 0.000000000000000000 ) ) ;
#42182 = CARTESIAN_POINT ( 'NONE',  ( 21.05000000000000071, 65.39167043205833352, -162.4314224712280748 ) ) ;
#42183 = AXIS2_PLACEMENT_3D ( 'NONE', #209717, #130163, #104175 ) ;
#42184 = CARTESIAN_POINT ( 'NONE',  ( -21.05000000000000071, 87.65000000001192859, -100.0231074845242318 ) ) ;
#42185 = DIRECTION ( 'NONE',  ( 1.000000000000000000, 0.000000000000000000, 0.000000000000000000 ) ) ;
#42187 = CARTESIAN_POINT ( 'NONE',  ( 21.09316766718127667, 6.370153312485567376, -100.4607365976853401 ) ) ;
#42186 = CYLINDRICAL_SURFACE ( 'NONE', #148745, 0.09999999999999939493 ) ;
#42188 = CARTESIAN_POINT ( 'NONE',  ( 18.49999999999999289, 69.35000000001180354, -81.87310748452435405 ) ) ;
#42189 = CARTESIAN_POINT ( 'NONE',  ( -23.25000000000000000, 77.85161776048127535, -158.4199177649206831 ) ) ;
#42190 = EDGE_CURVE ( 'NONE', #167418, #138366, #224402, .T. ) ;
#42191 = LINE ( 'NONE', #104679, #114426 ) ;
#42192 = DIRECTION ( 'NONE',  ( 0.000000000000000000, 0.000000000000000000, -1.000000000000000000 ) ) ;
#42193 = ORIENTED_EDGE ( 'NONE', *, *, #193338, .F. ) ;
#42195 = ORIENTED_EDGE ( 'NONE', *, *, #82631, .F. ) ;
#42194 = CARTESIAN_POINT ( 'NONE',  ( 23.24999999999999645, 1.115600667400684642E-11, -100.5000000000000284 ) ) ;
#42196 = ORIENTED_EDGE ( 'NONE', *, *, #117727, .T. ) ;
#42198 = EDGE_CURVE ( 'NONE', #80403, #62956, #3833, .T. ) ;
#42197 = CARTESIAN_POINT ( 'NONE',  ( -18.50000000000000000, 1.637172712981535883, -78.58215336547205254 ) ) ;
#42199 = DIRECTION ( 'NONE',  ( -1.000000000000000000, 0.000000000000000000, 0.000000000000000000 ) ) ;
#42200 = DIRECTION ( 'NONE',  ( 0.000000000000000000, -1.000000000000000000, -6.982962677686265922E-15 ) ) ;
#42201 = EDGE_LOOP ( 'NONE', ( #137794, #115569, #219154, #19189 ) ) ;
#42202 = CIRCLE ( 'NONE', #4750, 11.70000000000000639 ) ;
#42203 = CARTESIAN_POINT ( 'NONE',  ( 21.05000000000000071, 1.835341550224413698, -11.55515129256298401 ) ) ;
#42204 = AXIS2_PLACEMENT_3D ( 'NONE', #83083, #162675, #227767 ) ;
#42205 = DIRECTION ( 'NONE',  ( 2.915501640297156255E-16, 1.000000000000000000, 6.997203936713175802E-15 ) ) ;
#42206 = ORIENTED_EDGE ( 'NONE', *, *, #56353, .T. ) ;
#42207 = CARTESIAN_POINT ( 'NONE',  ( -21.05000000000000071, 11.63687328911514030, -140.8217592133249525 ) ) ;
#42208 = CARTESIAN_POINT ( 'NONE',  ( -20.64999999999999858, 85.00000000001207923, -126.6291383618717816 ) ) ;
#42209 = AXIS2_PLACEMENT_3D ( 'NONE', #76227, #153251, #52813 ) ;
#42210 = CARTESIAN_POINT ( 'NONE',  ( 16.87683809663749557, 51.61886293219124155, -231.9464690156495692 ) ) ;
#42211 = B_SPLINE_CURVE_WITH_KNOTS ( 'NONE', 3,
 ( #248041, #22924, #123288, #239381, #20354, #161132, #202813, #62037 ),
 .UNSPECIFIED., .F., .F.,
 ( 4, 2, 2, 4 ),
 ( 0.000000000000000000, 0.0001881495939909316674, 0.0002822243909863870115, 0.0003762991879818423013 ),
 .UNSPECIFIED. ) ;
#42212 = CIRCLE ( 'NONE', #187972, 0.09999999999999854838 ) ;
#42213 = FACE_OUTER_BOUND ( 'NONE', #180415, .T. ) ;
#42215 = ORIENTED_EDGE ( 'NONE', *, *, #48549, .F. ) ;
#42214 = CARTESIAN_POINT ( 'NONE',  ( -20.92356734117541706, 67.49293571122092317, -195.4648732548341741 ) ) ;
#42216 = CARTESIAN_POINT ( 'NONE',  ( 23.15000000000000213, 85.50000000001251976, -179.9170766071767389 ) ) ;
#42218 = EDGE_LOOP ( 'NONE', ( #54624, #128151, #210083, #70341 ) ) ;
#42217 = DIRECTION ( 'NONE',  ( -0.000000000000000000, 0.000000000000000000, 1.000000000000000000 ) ) ;
#42219 = DIRECTION ( 'NONE',  ( 1.000000000000000000, 0.000000000000000000, 0.000000000000000000 ) ) ;
#42221 = VECTOR ( 'NONE', #232716, 1000.000000000000000 ) ;
#42220 = DIRECTION ( 'NONE',  ( 0.000000000000000000, -0.1455152366551522025, -0.9893560106964505163 ) ) ;
#42222 = CARTESIAN_POINT ( 'NONE',  ( -16.93909480342659890, 66.00692163521075884, -157.4227604678520720 ) ) ;
#42223 = CARTESIAN_POINT ( 'NONE',  ( -12.93407622233968368, 9.417789466963364831, -182.8573845439768775 ) ) ;
#42225 = DIRECTION ( 'NONE',  ( 0.000000000000000000, 1.000000000000000000, 6.982962677686266711E-15 ) ) ;
#42224 = FACE_OUTER_BOUND ( 'NONE', #125149, .T. ) ;
#42226 = CARTESIAN_POINT ( 'NONE',  ( -16.89268316805466341, 66.04827818677041762, -190.8788599630699707 ) ) ;
#42227 = CARTESIAN_POINT ( 'NONE',  ( -21.05000000000000071, 67.23127455305841238, -235.8551265064783991 ) ) ;
#42228 = AXIS2_PLACEMENT_3D ( 'NONE', #164255, #45578, #65129 ) ;
#42229 = FACE_OUTER_BOUND ( 'NONE', #129654, .T. ) ;
#42230 = CARTESIAN_POINT ( 'NONE',  ( 21.07928932188134397, 10.02993822722304351, -228.1074463178677263 ) ) ;
#42231 = AXIS2_PLACEMENT_3D ( 'NONE', #165566, #63882, #45607 ) ;
#42232 = ORIENTED_EDGE ( 'NONE', *, *, #199238, .T. ) ;
#42233 = EDGE_CURVE ( 'NONE', #241870, #220791, #65929, .T. ) ;
#42234 = DIRECTION ( 'NONE',  ( -1.000000000000000000, -0.000000000000000000, -0.000000000000000000 ) ) ;
#42235 = ORIENTED_EDGE ( 'NONE', *, *, #179457, .T. ) ;
#42236 = ORIENTED_EDGE ( 'NONE', *, *, #22240, .T. ) ;
#42237 = FACE_OUTER_BOUND ( 'NONE', #222951, .T. ) ;
#42238 = LINE ( 'NONE', #124344, #173586 ) ;
#42239 = ORIENTED_EDGE ( 'NONE', *, *, #11716, .F. ) ;
#42241 = EDGE_CURVE ( 'NONE', #194487, #175937, #150606, .T. ) ;
#42240 = AXIS2_PLACEMENT_3D ( 'NONE', #125751, #5788, #227426 ) ;
#42242 = ORIENTED_EDGE ( 'NONE', *, *, #124785, .F. ) ;
#42243 = EDGE_CURVE ( 'NONE', #78058, #39695, #37164, .T. ) ;
#42244 = ADVANCED_FACE ( 'NONE', ( #149339 ), #182908, .T. ) ;
#42246 = ORIENTED_EDGE ( 'NONE', *, *, #96401, .F. ) ;
#42245 = AXIS2_PLACEMENT_3D ( 'NONE', #114179, #253678, #15094 ) ;
#42247 = CARTESIAN_POINT ( 'NONE',  ( 20.94999999999999574, 8.926614585098251453, -75.47168301922316402 ) ) ;
#42248 = AXIS2_PLACEMENT_3D ( 'NONE', #211106, #32510, #191569 ) ;
#42249 = VECTOR ( 'NONE', #96464, 1000.000000000000000 ) ;
#42250 = EDGE_LOOP ( 'NONE', ( #180563, #80778, #232506, #232971, #196091 ) ) ;
#42251 = VECTOR ( 'NONE', #235392, 999.9999999999998863 ) ;
#42252 = DIRECTION ( 'NONE',  ( -1.000000000000000000, -0.000000000000000000, -0.000000000000000000 ) ) ;
#42253 = FACE_OUTER_BOUND ( 'NONE', #58767, .T. ) ;
#42254 = LINE ( 'NONE', #22709, #49021 ) ;
#42255 = DIRECTION ( 'NONE',  ( -1.000000000000000000, 0.000000000000000000, 0.000000000000000000 ) ) ;
#42256 = PLANE ( 'NONE',  #12674 ) ;
#42257 = LINE ( 'NONE', #243005, #3633 ) ;
#42259 = VERTEX_POINT ( 'NONE', #226252 ) ;
#42258 = DIRECTION ( 'NONE',  ( 3.469446951953243109E-14, 0.4999999999999608646, 0.8660254037844612451 ) ) ;
#42261 = CARTESIAN_POINT ( 'NONE',  ( 21.14999999999999858, 69.45000000001259366, -191.1731074845243938 ) ) ;
#42260 = CARTESIAN_POINT ( 'NONE',  ( 20.95203847575071521, 65.49893946073758855, -61.95603613590083825 ) ) ;
#42262 = EDGE_CURVE ( 'NONE', #221067, #139739, #28109, .T. ) ;
#42263 = CARTESIAN_POINT ( 'NONE',  ( 18.49999999999999645, 1.115600667400684642E-11, -67.00000000000004263 ) ) ;
#42264 = EDGE_LOOP ( 'NONE', ( #100498, #110486, #236582, #243709, #161663 ) ) ;
#42265 = CARTESIAN_POINT ( 'NONE',  ( 18.59999999999999076, 6.650000000011155876, -121.6500000000000341 ) ) ;
#42267 = ADVANCED_FACE ( 'NONE', ( #8524 ), #88025, .F. ) ;
#42266 = DIRECTION ( 'NONE',  ( 1.000000000000000000, 0.000000000000000000, 0.000000000000000000 ) ) ;
#42268 = ORIENTED_EDGE ( 'NONE', *, *, #187879, .T. ) ;
#42270 = CARTESIAN_POINT ( 'NONE',  ( -20.64999999999999858, 1.115600667400684642E-11, -98.50000000000004263 ) ) ;
#42269 = DIRECTION ( 'NONE',  ( 0.000000000000000000, -0.8814952561688430555, 0.4721928772777346239 ) ) ;
#42271 = PRODUCT_DEFINITION ( 'UNKNOWN', '', #244573, #63507 ) ;
#42272 = CARTESIAN_POINT ( 'NONE',  ( -16.88705144915408951, 66.05000000001180638, -82.45408607923690170 ) ) ;
#42273 = ORIENTED_EDGE ( 'NONE', *, *, #152535, .F. ) ;
#42274 = CARTESIAN_POINT ( 'NONE',  ( 21.14999999999999858, 6.650000000011155876, -79.15000000000004832 ) ) ;
#42275 = CARTESIAN_POINT ( 'NONE',  ( -21.45000000000000284, 7.708578643773852157, -112.8500000000000369 ) ) ;
#42276 = EDGE_CURVE ( 'NONE', #49960, #213315, #103750, .T. ) ;
#42277 = CARTESIAN_POINT ( 'NONE',  ( -20.94999999999999929, 14.81796439977981272, -236.5325475414793743 ) ) ;
#42278 = CARTESIAN_POINT ( 'NONE',  ( -22.39999999999999858, -0.1008583690875575894, -122.2504328765106294 ) ) ;
#42279 = EDGE_CURVE ( 'NONE', #89984, #244131, #232801, .T. ) ;
#42280 = ORIENTED_EDGE ( 'NONE', *, *, #41535, .T. ) ;
#42281 = EDGE_CURVE ( 'NONE', #38619, #89486, #12235, .T. ) ;
#42282 = B_SPLINE_CURVE_WITH_KNOTS ( 'NONE', 3,
 ( #44992, #183222, #81507, #60675, #161097, #201480, #243176, #178099, #99792, #43705 ),
 .UNSPECIFIED., .F., .F.,
 ( 4, 3, 3, 4 ),
 ( 0.000000000000000000, 0.0002000000000008585893, 0.001000000000082977483, 0.001967863649483336721 ),
 .UNSPECIFIED. ) ;
#42283 = AXIS2_PLACEMENT_3D ( 'NONE', #80254, #159850, #17730 ) ;
#42284 = CARTESIAN_POINT ( 'NONE',  ( -17.11825945287481687, 66.05000000001255955, -182.6731074845244507 ) ) ;
#42285 = FACE_OUTER_BOUND ( 'NONE', #65027, .T. ) ;
#42286 = LINE ( 'NONE', #22739, #84050 ) ;
#42287 = LINE ( 'NONE', #21456, #99130 ) ;
#42288 = CARTESIAN_POINT ( 'NONE',  ( 20.94999999999999929, 1.115600667400684642E-11, -67.00000000000004263 ) ) ;
#42289 = CIRCLE ( 'NONE', #196395, 12.87499999999999822 ) ;
#42291 = VERTEX_POINT ( 'NONE', #50196 ) ;
#42290 = FACE_OUTER_BOUND ( 'NONE', #34264, .T. ) ;
#42292 = EDGE_CURVE ( 'NONE', #85480, #52627, #95408, .T. ) ;
#42293 = DIRECTION ( 'NONE',  ( 0.000000000000000000, 0.000000000000000000, 1.000000000000000000 ) ) ;
#42294 = PLANE ( 'NONE',  #13853 ) ;
#42295 = CYLINDRICAL_SURFACE ( 'NONE', #150579, 0.09999999999999933942 ) ;
#42297 = ORIENTED_EDGE ( 'NONE', *, *, #195, .T. ) ;
#42296 = CARTESIAN_POINT ( 'NONE',  ( 22.39999999999999503, 11.65000000001116298, -67.00000000000004263 ) ) ;
#42298 = DIRECTION ( 'NONE',  ( 1.000000000000000000, 0.000000000000000000, 0.000000000000000000 ) ) ;
#42299 = CARTESIAN_POINT ( 'NONE',  ( -16.87242674293849731, 63.08601772833120691, -213.1265693521094136 ) ) ;
#42300 = CARTESIAN_POINT ( 'NONE',  ( 20.93975676684922504, 67.49344847133114911, -195.4961807846321733 ) ) ;
#42301 = ORIENTED_EDGE ( 'NONE', *, *, #34109, .F. ) ;
#42302 = CARTESIAN_POINT ( 'NONE',  ( -13.77083647240105257, 66.54258906972208365, -151.5231915757781564 ) ) ;
#42303 = CARTESIAN_POINT ( 'NONE',  ( -23.15000000000000213, 76.00000000001170974, -69.52310748452431710 ) ) ;
#42304 = CARTESIAN_POINT ( 'NONE',  ( 20.85000000000000142, 11.65000000001115943, -167.5000000000000284 ) ) ;
#42305 = EDGE_CURVE ( 'NONE', #41194, #126005, #249553, .T. ) ;
#42307 = TOROIDAL_SURFACE ( 'NONE', #221338, 4.149999999999999467, 0.1000000000000000056 ) ;
#42306 = CARTESIAN_POINT ( 'NONE',  ( -23.15000000000000213, 68.18350826420393673, -222.4110246041809091 ) ) ;
#42309 = AXIS2_PLACEMENT_3D ( 'NONE', #66897, #164719, #27809 ) ;
#42308 = CARTESIAN_POINT ( 'NONE',  ( -16.84793658983420173, 9.950000000011138823, -87.76635332218982910 ) ) ;
#42310 = ORIENTED_EDGE ( 'NONE', *, *, #178339, .F. ) ;
#42311 = VERTEX_POINT ( 'NONE', #219232 ) ;
#42312 = AXIS2_PLACEMENT_3D ( 'NONE', #114801, #227820, #159086 ) ;
#42313 = DIRECTION ( 'NONE',  ( 1.000000000000000000, 0.000000000000000000, 0.000000000000000000 ) ) ;
#42314 = DIRECTION ( 'NONE',  ( 0.000000000000000000, -1.000000000000000000, -6.982962677686265922E-15 ) ) ;
#42315 = ADVANCED_FACE ( 'NONE', ( #40656 ), #94463, .F. ) ;
#42316 = DIRECTION ( 'NONE',  ( -0.000000000000000000, 6.982962677686266711E-15, -1.000000000000000000 ) ) ;
#42317 = CARTESIAN_POINT ( 'NONE',  ( -20.85000000000000142, 31.11065811373596190, -259.9087319612273177 ) ) ;
#42318 = VERTEX_POINT ( 'NONE', #114023 ) ;
#42319 = EDGE_CURVE ( 'NONE', #166243, #157545, #52764, .T. ) ;
#42320 = CARTESIAN_POINT ( 'NONE',  ( -23.25000000000000000, -11.64999999998884483, -103.6000000000000369 ) ) ;
#42321 = AXIS2_PLACEMENT_3D ( 'NONE', #53215, #31127, #248853 ) ;
#42322 = DIRECTION ( 'NONE',  ( 0.000000000000000000, -6.308085367188367561E-15, 1.000000000000000000 ) ) ;
#42323 = EDGE_CURVE ( 'NONE', #1463, #41556, #28958, .T. ) ;
#42324 = CARTESIAN_POINT ( 'NONE',  ( 20.95545211741311320, 10.58641331155510379, -108.0861468595883252 ) ) ;
#42325 = CARTESIAN_POINT ( 'NONE',  ( -20.07928932188135107, 9.220710678118654968, -12.34999999999999964 ) ) ;
#42326 = CARTESIAN_POINT ( 'NONE',  ( 18.59999999999999076, 6.450000000011156587, -88.15000000000004832 ) ) ;
#42327 = ORIENTED_EDGE ( 'NONE', *, *, #139074, .F. ) ;
#42329 = ORIENTED_EDGE ( 'NONE', *, *, #224395, .F. ) ;
#42328 = CARTESIAN_POINT ( 'NONE',  ( -20.85000000000000142, -11.64999999998884483, -97.60000000000005116 ) ) ;
#42330 = EDGE_CURVE ( 'NONE', #254440, #64828, #232721, .T. ) ;
#42331 = ORIENTED_EDGE ( 'NONE', *, *, #229821, .F. ) ;
#42332 = LINE ( 'NONE', #183138, #123711 ) ;
#42333 = EDGE_CURVE ( 'NONE', #100083, #254522, #245273, .T. ) ;
#42334 = ORIENTED_EDGE ( 'NONE', *, *, #175684, .F. ) ;
#42335 = CARTESIAN_POINT ( 'NONE',  ( -20.54999999999999716, 74.05981308412395947, -82.35222669557765585 ) ) ;
#42336 = CARTESIAN_POINT ( 'NONE',  ( 20.94999999999999929, 33.04479387145709524, -247.6151719044046899 ) ) ;
#42337 = CARTESIAN_POINT ( 'NONE',  ( -20.85000000000000142, 31.15787740146373608, -259.8205824356103903 ) ) ;
#42338 = VERTEX_POINT ( 'NONE', #174056 ) ;
#42339 = DIRECTION ( 'NONE',  ( 0.000000000000000000, 0.8700118002898357128, -0.4930308989875170633 ) ) ;
#42340 = CYLINDRICAL_SURFACE ( 'NONE', #101214, 4.049999999999995381 ) ;
#42341 = ORIENTED_EDGE ( 'NONE', *, *, #165761, .T. ) ;
#42342 = LINE ( 'NONE', #80137, #249802 ) ;
#42344 = EDGE_LOOP ( 'NONE', ( #139516, #92490, #145439, #92046 ) ) ;
#42343 = CARTESIAN_POINT ( 'NONE',  ( -23.15000000000000213, 42.94327155031035659, -233.8606566173841372 ) ) ;
#42345 = AXIS2_PLACEMENT_3D ( 'NONE', #225792, #202404, #147568 ) ;
#42346 = CIRCLE ( 'NONE', #96481, 0.09999999999999817368 ) ;
#42347 = CYLINDRICAL_SURFACE ( 'NONE', #73340, 0.09999999999999681366 ) ;
#42348 = CARTESIAN_POINT ( 'NONE',  ( 20.94999999999999929, 1.115600667400684642E-11, -134.0000000000000284 ) ) ;
#42349 = EDGE_CURVE ( 'NONE', #114076, #149886, #124636, .T. ) ;
#42350 = EDGE_CURVE ( 'NONE', #77018, #207338, #253607, .T. ) ;
#42351 = EDGE_LOOP ( 'NONE', ( #143890, #192807, #248057, #54736 ) ) ;
#42352 = LINE ( 'NONE', #98420, #64421 ) ;
#42353 = CARTESIAN_POINT ( 'NONE',  ( 21.05000000000000071, 76.00000000001190870, -103.0231074845243029 ) ) ;
#42354 = DIRECTION ( 'NONE',  ( 1.000000000000000000, 0.000000000000000000, 0.000000000000000000 ) ) ;
#42355 = ORIENTED_EDGE ( 'NONE', *, *, #182801, .F. ) ;
#42356 = LINE ( 'NONE', #120628, #142378 ) ;
#42357 = EDGE_CURVE ( 'NONE', #74489, #231873, #171482, .T. ) ;
#42358 = DIRECTION ( 'NONE',  ( 1.000000000000000000, -0.000000000000000000, 0.000000000000000000 ) ) ;
#42359 = FACE_OUTER_BOUND ( 'NONE', #149403, .T. ) ;
#42360 = VECTOR ( 'NONE', #148141, 1000.000000000000227 ) ;
#42361 = ORIENTED_EDGE ( 'NONE', *, *, #9904, .F. ) ;
#42362 = EDGE_CURVE ( 'NONE', #242182, #202321, #220538, .T. ) ;
#42363 = ORIENTED_EDGE ( 'NONE', *, *, #147036, .F. ) ;
#42364 = EDGE_CURVE ( 'NONE', #174276, #173665, #257851, .T. ) ;
#42365 = VERTEX_POINT ( 'NONE', #111474 ) ;
#42366 = CARTESIAN_POINT ( 'NONE',  ( 18.59117750673696179, 10.33248238082519066, -39.09484654391314962 ) ) ;
#42367 = CARTESIAN_POINT ( 'NONE',  ( 22.84999999999999787, 0.000000000000000000, -3.900000000000000355 ) ) ;
#42368 = CIRCLE ( 'NONE', #158923, 12.97499999999999964 ) ;
#42370 = ORIENTED_EDGE ( 'NONE', *, *, #25012, .T. ) ;
#42369 = LINE ( 'NONE', #104866, #200058 ) ;
#42371 = DIRECTION ( 'NONE',  ( -1.000000000000000000, 0.000000000000000000, 0.000000000000000000 ) ) ;
#42372 = CARTESIAN_POINT ( 'NONE',  ( -23.25000000000000000, -11.65000000000000036, -30.50000000000000000 ) ) ;
#42373 = CARTESIAN_POINT ( 'NONE',  ( -22.48660254037842066, 11.47023279864282941, -198.4507335280135294 ) ) ;
#42374 = DIRECTION ( 'NONE',  ( 0.000000000000000000, 0.8814952561688444987, -0.4721928772777320149 ) ) ;
#42375 = EDGE_CURVE ( 'NONE', #138430, #54663, #61456, .T. ) ;
#42376 = CARTESIAN_POINT ( 'NONE',  ( 20.94999999999999574, -11.74999999998883560, -70.10000000000005116 ) ) ;
#42377 = AXIS2_PLACEMENT_3D ( 'NONE', #225654, #47027, #126589 ) ;
#42378 = DIRECTION ( 'NONE',  ( -0.000000000000000000, 6.982962677686266711E-15, -1.000000000000000000 ) ) ;
#42380 = VERTEX_POINT ( 'NONE', #141009 ) ;
#42379 = CARTESIAN_POINT ( 'NONE',  ( 20.94999999999999574, -1.261786168553869603, -41.58649896354548048 ) ) ;
#42382 = ORIENTED_EDGE ( 'NONE', *, *, #56948, .F. ) ;
#42381 = LINE ( 'NONE', #84020, #27891 ) ;
#42383 = DIRECTION ( 'NONE',  ( -1.000000000000000000, 0.000000000000000000, 0.000000000000000000 ) ) ;
#42384 = ORIENTED_EDGE ( 'NONE', *, *, #217492, .F. ) ;
#42385 = ORIENTED_EDGE ( 'NONE', *, *, #43193, .T. ) ;
#42386 = CARTESIAN_POINT ( 'NONE',  ( 18.59999999999999076, 65.79142135624910281, -81.67310748452439384 ) ) ;
#42387 = VECTOR ( 'NONE', #96456, 1000.000000000000114 ) ;
#42388 = CARTESIAN_POINT ( 'NONE',  ( 23.25000000000000000, 82.09643798151613225, -215.4278993322501208 ) ) ;
#42389 = CARTESIAN_POINT ( 'NONE',  ( -18.59999999999999787, 11.65000000001115232, -112.6500000000000341 ) ) ;
#42390 = ADVANCED_FACE ( 'NONE', ( #211875 ), #55309, .T. ) ;
#42391 = CARTESIAN_POINT ( 'NONE',  ( -21.05000000000000071, 10.91926294161908295, -235.7631306847335395 ) ) ;
#42392 = CARTESIAN_POINT ( 'NONE',  ( -21.14999999999999858, 87.75000000001165290, -69.52310748452424605 ) ) ;
#42393 = AXIS2_PLACEMENT_3D ( 'NONE', #63701, #222767, #203216 ) ;
#42394 = VERTEX_POINT ( 'NONE', #54058 ) ;
#42395 = CARTESIAN_POINT ( 'NONE',  ( -18.59999999999999787, 66.85000000001200249, -115.3731074845243683 ) ) ;
#42396 = AXIS2_PLACEMENT_3D ( 'NONE', #184315, #168671, #68236 ) ;
#42397 = ORIENTED_EDGE ( 'NONE', *, *, #60668, .T. ) ;
#42398 = EDGE_LOOP ( 'NONE', ( #230348, #55523, #2406 ) ) ;
#42399 = CARTESIAN_POINT ( 'NONE',  ( -20.64999999999999858, 2.449293598294710359E-16, -35.50000000000000711 ) ) ;
#42400 = AXIS2_PLACEMENT_3D ( 'NONE', #139201, #98775, #40161 ) ;
#42401 = VERTEX_POINT ( 'NONE', #134854 ) ;
#42402 = AXIS2_PLACEMENT_3D ( 'NONE', #86953, #143087, #222616 ) ;
#42403 = CARTESIAN_POINT ( 'NONE',  ( -12.29659703204451660, 66.64411154550899141, -53.23446458774639467 ) ) ;
#42404 = CIRCLE ( 'NONE', #188166, 0.1000000000000060701 ) ;
#42405 = VERTEX_POINT ( 'NONE', #80995 ) ;
#42406 = EDGE_CURVE ( 'NONE', #130316, #43467, #250961, .T. ) ;
#42407 = DIRECTION ( 'NONE',  ( 1.000000000000000000, 0.000000000000000000, 0.000000000000000000 ) ) ;
#42408 = ORIENTED_EDGE ( 'NONE', *, *, #12975, .T. ) ;
#42410 = CIRCLE ( 'NONE', #129709, 0.5000000000000004441 ) ;
#42409 = DIRECTION ( 'NONE',  ( 1.000000000000000000, 1.836970198721029934E-16, 0.000000000000000000 ) ) ;
#42411 = ORIENTED_EDGE ( 'NONE', *, *, #76353, .T. ) ;
#42412 = CARTESIAN_POINT ( 'NONE',  ( -21.55000000000000426, 68.29142135624984178, -182.2731074845244166 ) ) ;
#42413 = LINE ( 'NONE', #84053, #134517 ) ;
#42414 = ORIENTED_EDGE ( 'NONE', *, *, #209217, .T. ) ;
#42415 = CARTESIAN_POINT ( 'NONE',  ( -23.25000000000000355, 64.25000000001210765, -127.2731074845243882 ) ) ;
#42417 = ORIENTED_EDGE ( 'NONE', *, *, #236978, .F. ) ;
#42416 = CARTESIAN_POINT ( 'NONE',  ( -18.59999999999999787, -1.835341550213255957, -145.6551512925629766 ) ) ;
#42418 = EDGE_CURVE ( 'NONE', #186897, #14594, #83985, .T. ) ;
#42419 = AXIS2_PLACEMENT_3D ( 'NONE', #47468, #210436, #87873 ) ;
#42420 = DIRECTION ( 'NONE',  ( 0.8049926720990051576, 0.5932847527679298016, -0.000000000000000000 ) ) ;
#42422 = VERTEX_POINT ( 'NONE', #185256 ) ;
#42421 = AXIS2_PLACEMENT_3D ( 'NONE', #123449, #42620, #243382 ) ;
#42423 = CIRCLE ( 'NONE', #188181, 11.75000000000001066 ) ;
#42424 = AXIS2_PLACEMENT_3D ( 'NONE', #221794, #223097, #163150 ) ;
#42425 = CARTESIAN_POINT ( 'NONE',  ( -16.97683809663752186, 66.05000000001261640, -190.1207434663279514 ) ) ;
#42426 = VERTEX_POINT ( 'NONE', #4042 ) ;
#42427 = CARTESIAN_POINT ( 'NONE',  ( -20.64999999999999858, 70.60814576644823148, -215.7631455941064189 ) ) ;
#42428 = CARTESIAN_POINT ( 'NONE',  ( -16.87683809663752399, 9.850000000011144508, -87.09763598180374800 ) ) ;
#42429 = DIRECTION ( 'NONE',  ( 0.000000000000000000, -0.9893560106964500722, 0.1455152366551550613 ) ) ;
#42430 = CARTESIAN_POINT ( 'NONE',  ( -12.93407622233968901, 66.58221053306039039, -188.1657229405475675 ) ) ;
#42431 = ORIENTED_EDGE ( 'NONE', *, *, #68313, .T. ) ;
#42432 = CARTESIAN_POINT ( 'NONE',  ( -23.25000000000000000, 1.115600667400684642E-11, -79.77500000000003411 ) ) ;
#42433 = DIRECTION ( 'NONE',  ( -1.836970198721029934E-16, 1.000000000000000000, 0.000000000000000000 ) ) ;
#42434 = DIRECTION ( 'NONE',  ( 0.000000000000000000, 0.000000000000000000, 1.000000000000000000 ) ) ;
#42435 = VERTEX_POINT ( 'NONE', #67868 ) ;
#42437 = CARTESIAN_POINT ( 'NONE',  ( -21.05000000000000071, 76.00000000001200817, -109.5637644362255401 ) ) ;
#42436 = CIRCLE ( 'NONE', #150595, 0.09999999999999939493 ) ;
#42438 = ORIENTED_EDGE ( 'NONE', *, *, #24617, .F. ) ;
#42439 = DIRECTION ( 'NONE',  ( -0.000000000000000000, 0.1350103645451876666, 0.9908441862701600211 ) ) ;
#42440 = VERTEX_POINT ( 'NONE', #82266 ) ;
#42441 = DIRECTION ( 'NONE',  ( 0.000000000000000000, 0.000000000000000000, 1.000000000000000000 ) ) ;
#42442 = CARTESIAN_POINT ( 'NONE',  ( 20.94999999999999574, 74.16465844978715438, -57.86795619196134766 ) ) ;
#42443 = ORIENTED_EDGE ( 'NONE', *, *, #170169, .T. ) ;
#42445 = ORIENTED_EDGE ( 'NONE', *, *, #146427, .F. ) ;
#42444 = DIRECTION ( 'NONE',  ( -0.000000000000000000, 0.000000000000000000, -1.000000000000000000 ) ) ;
#42446 = DIRECTION ( 'NONE',  ( 1.000000000000000000, 0.000000000000000000, 0.000000000000000000 ) ) ;
#42447 = ORIENTED_EDGE ( 'NONE', *, *, #77039, .T. ) ;
#42448 = DIRECTION ( 'NONE',  ( 1.000000000000000000, 0.000000000000000000, 0.000000000000000000 ) ) ;
#42449 = EDGE_CURVE ( 'NONE', #234552, #221499, #166185, .T. ) ;
#42450 = DIRECTION ( 'NONE',  ( -4.801466763864312543E-15, 0.7280513885558889120, -0.6855225566105335178 ) ) ;
#42451 = ORIENTED_EDGE ( 'NONE', *, *, #128832, .T. ) ;
#42452 = ORIENTED_EDGE ( 'NONE', *, *, #154702, .F. ) ;
#42453 = DIRECTION ( 'NONE',  ( 1.000000000000000000, 0.000000000000000000, -0.000000000000000000 ) ) ;
#42454 = CARTESIAN_POINT ( 'NONE',  ( -16.92778301347381742, 14.22548837169992630, -219.3209511219291699 ) ) ;
#42455 = CARTESIAN_POINT ( 'NONE',  ( 20.04142135623731136, 64.25000000001148237, -44.75595019699901655 ) ) ;
#42456 = ORIENTED_EDGE ( 'NONE', *, *, #14285, .T. ) ;
#42457 = VERTEX_POINT ( 'NONE', #62745 ) ;
#42458 = AXIS2_PLACEMENT_3D ( 'NONE', #183051, #66936, #185605 ) ;
#42459 = LINE ( 'NONE', #138963, #109762 ) ;
#42460 = EDGE_CURVE ( 'NONE', #230402, #29064, #191301, .T. ) ;
#42461 = APPLICATION_CONTEXT ( 'automotive_design' ) ;
#42462 = EDGE_CURVE ( 'NONE', #9026, #256883, #174577, .T. ) ;
#42464 = ORIENTED_EDGE ( 'NONE', *, *, #139361, .F. ) ;
#42463 = DIRECTION ( 'NONE',  ( 0.000000000000000000, -1.000000000000000000, -6.982962677686266711E-15 ) ) ;
#42465 = CARTESIAN_POINT ( 'NONE',  ( -18.59999999999999787, -10.74999999999999289, 32.89999999999999858 ) ) ;
#42466 = CARTESIAN_POINT ( 'NONE',  ( -22.50000000000000000, 75.90736249940226799, -81.17280469156507650 ) ) ;
#42467 = LINE ( 'NONE', #201540, #94292 ) ;
#42469 = DIRECTION ( 'NONE',  ( 0.000000000000000000, -1.000000000000000000, -0.000000000000000000 ) ) ;
#42468 = FACE_OUTER_BOUND ( 'NONE', #57541, .T. ) ;
#42470 = DIRECTION ( 'NONE',  ( 0.000000000000000000, 0.000000000000000000, -1.000000000000000000 ) ) ;
#42471 = CYLINDRICAL_SURFACE ( 'NONE', #56791, 0.09999999999999641120 ) ;
#42472 = CIRCLE ( 'NONE', #154944, 0.4000000000000114575 ) ;
#42473 = EDGE_CURVE ( 'NONE', #215522, #224607, #207873, .T. ) ;
#42474 = DIRECTION ( 'NONE',  ( 1.000000000000000000, 0.000000000000000000, 0.000000000000000000 ) ) ;
#42475 = AXIS2_PLACEMENT_3D ( 'NONE', #249536, #74779, #209106 ) ;
#42476 = ORIENTED_EDGE ( 'NONE', *, *, #168813, .T. ) ;
#42477 = ORIENTED_EDGE ( 'NONE', *, *, #209871, .F. ) ;
#42478 = CARTESIAN_POINT ( 'NONE',  ( -16.94107738177414291, 65.98576071487519812, -82.07310748452438531 ) ) ;
#42479 =( BOUNDED_CURVE ( )  B_SPLINE_CURVE ( 3, ( #226302, #45125, #23025, #145499 ),
 .UNSPECIFIED., .F., .F. ) 
 B_SPLINE_CURVE_WITH_KNOTS ( ( 4, 4 ),
 ( 0.3000847527772389500, 0.5517402753107879532 ),
 .UNSPECIFIED. ) 
 CURVE ( )  GEOMETRIC_REPRESENTATION_ITEM ( )  RATIONAL_B_SPLINE_CURVE ( ( 1.000000000000000000, 0.9947294176030464508, 0.9947294176030464508, 1.000000000000000000 ) ) 
 REPRESENTATION_ITEM ( '' )  );
#42480 = ORIENTED_EDGE ( 'NONE', *, *, #112968, .T. ) ;
#42481 = ADVANCED_FACE ( 'NONE', ( #87424 ), #70811, .F. ) ;
#42482 = ORIENTED_EDGE ( 'NONE', *, *, #249228, .F. ) ;
#42483 = EDGE_CURVE ( 'NONE', #124002, #139747, #224574, .T. ) ;
#42484 = CIRCLE ( 'NONE', #250786, 0.3999999999999926392 ) ;
#42485 = FILL_AREA_STYLE_COLOUR ( '', #31525 ) ;
#42486 = CARTESIAN_POINT ( 'NONE',  ( -21.05000000000000071, 69.74218538953626023, -170.1208977758331855 ) ) ;
#42487 = B_SPLINE_CURVE_WITH_KNOTS ( 'NONE', 3,
 ( #74879, #53991, #248341, #29334, #50129, #90538, #69722 ),
 .UNSPECIFIED., .F., .F.,
 ( 4, 3, 4 ),
 ( 0.000000000000000000, 0.0009834301579440000909, 0.001767853679402678867 ),
 .UNSPECIFIED. ) ;
#42489 = EDGE_LOOP ( 'NONE', ( #224382, #234129, #239447 ) ) ;
#42488 = EDGE_LOOP ( 'NONE', ( #57621, #148224, #70057, #99708 ) ) ;
#42490 = CARTESIAN_POINT ( 'NONE',  ( -20.64999999999999858, 2.739812813550878801, -213.5801053551551547 ) ) ;
#42491 = ORIENTED_EDGE ( 'NONE', *, *, #163048, .F. ) ;
#42492 = EDGE_LOOP ( 'NONE', ( #208957, #53599, #94322, #217022 ) ) ;
#42493 = DIRECTION ( 'NONE',  ( -1.000000000000000000, -0.000000000000000000, -0.000000000000000000 ) ) ;
#42494 = DIRECTION ( 'NONE',  ( 0.000000000000000000, 0.9908441862701596881, 0.1350103645451904977 ) ) ;
#42496 = ORIENTED_EDGE ( 'NONE', *, *, #26086, .T. ) ;
#42495 = CARTESIAN_POINT ( 'NONE',  ( 20.27550659511089037, 9.216043722519994930, -87.85000000000003695 ) ) ;
#42497 = CARTESIAN_POINT ( 'NONE',  ( 20.86036036209906186, 39.31301701234226442, -236.7240336282158353 ) ) ;
#42499 = ORIENTED_EDGE ( 'NONE', *, *, #169552, .F. ) ;
#42498 = CARTESIAN_POINT ( 'NONE',  ( -20.64999999999999858, 68.85000000001180354, -81.87310748452436826 ) ) ;
#42500 = CARTESIAN_POINT ( 'NONE',  ( 19.75857864376269291, 11.65000000001116476, -125.2500000000000568 ) ) ;
#42501 = ORIENTED_EDGE ( 'NONE', *, *, #65877, .F. ) ;
#42502 = CARTESIAN_POINT ( 'NONE',  ( -16.77683809663752257, 23.65833333334447985, -184.2499999999999716 ) ) ;
#42505 = ADVANCED_FACE ( 'NONE', ( #2748 ), #116272, .F. ) ;
#42504 = ORIENTED_EDGE ( 'NONE', *, *, #187590, .T. ) ;
#42503 = FACE_OUTER_BOUND ( 'NONE', #248735, .T. ) ;
#42506 = DIRECTION ( 'NONE',  ( 0.000000000000000000, 0.000000000000000000, 1.000000000000000000 ) ) ;
#42507 = CARTESIAN_POINT ( 'NONE',  ( -23.15000000000000213, 67.23127455305841238, -235.8551265064783991 ) ) ;
#42508 = AXIS2_PLACEMENT_3D ( 'NONE', #121319, #83399, #26040 ) ;
#42509 = AXIS2_PLACEMENT_3D ( 'NONE', #136234, #239217, #254865 ) ;
#42510 = FACE_OUTER_BOUND ( 'NONE', #227697, .T. ) ;
#42511 = AXIS2_PLACEMENT_3D ( 'NONE', #186972, #229925, #107397 ) ;
#42512 = VERTEX_POINT ( 'NONE', #126570 ) ;
#42514 = CARTESIAN_POINT ( 'NONE',  ( -21.07928932188134041, 69.67148334361938566, -203.6220026301787982 ) ) ;
#42513 = DIRECTION ( 'NONE',  ( 0.000000000000000000, 0.9126074666063745955, 0.4088369013363334359 ) ) ;
#42515 = CARTESIAN_POINT ( 'NONE',  ( -15.66061380678752535, 66.63927620602578372, -85.70918028991766846 ) ) ;
#42516 = DIRECTION ( 'NONE',  ( 1.000000000000000000, 0.000000000000000000, 0.000000000000000000 ) ) ;
#42517 = CARTESIAN_POINT ( 'NONE',  ( 21.05000000000000071, 1.835341550235569663, -179.0551512925629538 ) ) ;
#42518 = CARTESIAN_POINT ( 'NONE',  ( -17.01764560440450680, 44.22674245196203202, -235.2580479167952774 ) ) ;
#42519 = VERTEX_POINT ( 'NONE', #181425 ) ;
#42520 = ORIENTED_EDGE ( 'NONE', *, *, #145840, .T. ) ;
#42521 = VERTEX_POINT ( 'NONE', #86119 ) ;
#42522 = EDGE_CURVE ( 'NONE', #204034, #131851, #203537, .T. ) ;
#42523 = CARTESIAN_POINT ( 'NONE',  ( -18.69999999999999929, -8.250000000000005329, 5.900000000000002132 ) ) ;
#42524 = ORIENTED_EDGE ( 'NONE', *, *, #22333, .T. ) ;
#42525 = CYLINDRICAL_SURFACE ( 'NONE', #205973, 0.1000000000000052097 ) ;
#42526 = ORIENTED_EDGE ( 'NONE', *, *, #224276, .T. ) ;
#42527 = CARTESIAN_POINT ( 'NONE',  ( 18.52928932188133970, 10.27928932189249878, -91.70857864376273483 ) ) ;
#42528 = CARTESIAN_POINT ( 'NONE',  ( 20.94999999999999574, -11.48912529307605901, -2.900000000000003464 ) ) ;
#42529 = EDGE_CURVE ( 'NONE', #75238, #182666, #33106, .T. ) ;
#42530 = AXIS2_PLACEMENT_3D ( 'NONE', #42320, #236657, #121868 ) ;
#42531 = VERTEX_POINT ( 'NONE', #124011 ) ;
#42532 = DIRECTION ( 'NONE',  ( 1.000000000000000000, 0.000000000000000000, 0.000000000000000000 ) ) ;
#42533 = EDGE_CURVE ( 'NONE', #13290, #7110, #132840, .T. ) ;
#42534 = CIRCLE ( 'NONE', #63373, 0.5000000000000004441 ) ;
#42535 = ADVANCED_FACE ( 'NONE', ( #247791 ), #141202, .T. ) ;
#42536 = VERTEX_POINT ( 'NONE', #9183 ) ;
#42537 = VERTEX_POINT ( 'NONE', #228246 ) ;
#42538 = ORIENTED_EDGE ( 'NONE', *, *, #8267, .F. ) ;
#42539 = DIRECTION ( 'NONE',  ( 0.000000000000000000, 0.000000000000000000, -1.000000000000000000 ) ) ;
#42540 = DIRECTION ( 'NONE',  ( 1.000000000000000000, 0.000000000000000000, 0.000000000000000000 ) ) ;
#42541 = CARTESIAN_POINT ( 'NONE',  ( 21.05000000000005400, 82.74366731733570646, -26.36310895752070138 ) ) ;
#42542 = CARTESIAN_POINT ( 'NONE',  ( 21.05000000000000071, 1.115600667400684642E-11, -100.5000000000000284 ) ) ;
#42543 = CARTESIAN_POINT ( 'NONE',  ( -21.05000000000000071, 70.15000000001163016, -59.39061026024639744 ) ) ;
#42544 = CARTESIAN_POINT ( 'NONE',  ( 23.14999999999999858, 1.115600667400684642E-11, -100.5000000000000426 ) ) ;
#42545 = AXIS2_PLACEMENT_3D ( 'NONE', #173377, #153818, #172082 ) ;
#42546 = EDGE_CURVE ( 'NONE', #9803, #91270, #199488, .T. ) ;
#42548 = FACE_OUTER_BOUND ( 'NONE', #157993, .T. ) ;
#42547 = DIRECTION ( 'NONE',  ( 0.000000000000000000, 0.8814952561688430555, -0.4721928772777346239 ) ) ;
#42549 = DIRECTION ( 'NONE',  ( 1.000000000000000000, 0.000000000000000000, 0.000000000000000000 ) ) ;
#42551 = ORIENTED_EDGE ( 'NONE', *, *, #255603, .T. ) ;
#42550 = CARTESIAN_POINT ( 'NONE',  ( 20.94999999999999929, 74.16465844978819177, -191.9679561919613775 ) ) ;
#42552 = DIRECTION ( 'NONE',  ( -0.7071067811865389130, -5.024295867788141276E-15, 0.7071067811865561215 ) ) ;
#42553 = DIRECTION ( 'NONE',  ( 0.000000000000000000, -0.1350103645451945777, 0.9908441862701590219 ) ) ;
#42554 = EDGE_LOOP ( 'NONE', ( #107758, #228460, #141001, #160453 ) ) ;
#42555 = CARTESIAN_POINT ( 'NONE',  ( 21.14999999999999858, 81.77808381374873647, -227.1078217596952697 ) ) ;
#42556 = VECTOR ( 'NONE', #123722, 1000.000000000000000 ) ;
#42557 = CARTESIAN_POINT ( 'NONE',  ( -21.08479644141222664, 69.65496134227977620, -69.58166192708848996 ) ) ;
#42559 = EDGE_CURVE ( 'NONE', #165621, #9380, #190412, .T. ) ;
#42558 = DIRECTION ( 'NONE',  ( 0.000000000000000000, -7.086529944415886769E-15, 1.000000000000000000 ) ) ;
#42561 = EDGE_CURVE ( 'NONE', #166926, #247506, #7949, .T. ) ;
#42560 = ORIENTED_EDGE ( 'NONE', *, *, #31691, .T. ) ;
#42562 = TOROIDAL_SURFACE ( 'NONE', #26007, 0.4000000000000012990, 0.1000000000000000056 ) ;
#42563 = VECTOR ( 'NONE', #234896, 1000.000000000000000 ) ;
#42564 = CIRCLE ( 'NONE', #188312, 4.299999999999956302 ) ;
#42565 = CARTESIAN_POINT ( 'NONE',  ( 21.00000000000000000, 66.25000000001223555, -148.8731074845244393 ) ) ;
#42566 = CARTESIAN_POINT ( 'NONE',  ( -18.50000000000000000, 9.350000000011156942, -54.85000000000000142 ) ) ;
#42567 = CIRCLE ( 'NONE', #188314, 0.09999999999999939493 ) ;
#42568 = ORIENTED_EDGE ( 'NONE', *, *, #3930, .T. ) ;
#42569 = EDGE_LOOP ( 'NONE', ( #88999, #189318, #54057 ) ) ;
#42570 = EDGE_CURVE ( 'NONE', #198094, #90093, #168307, .T. ) ;
#42571 = CARTESIAN_POINT ( 'NONE',  ( 23.24999999999999289, 11.65000000001116298, -21.75000000000000355 ) ) ;
#42572 = ORIENTED_EDGE ( 'NONE', *, *, #141615, .F. ) ;
#42573 = CARTESIAN_POINT ( 'NONE',  ( 21.93340585971920120, 7.324147022865871826, -67.00000000000004263 ) ) ;
#42574 = DIRECTION ( 'NONE',  ( 0.000000000000000000, -1.387778780781454006E-13, -1.000000000000000000 ) ) ;
#42575 = CARTESIAN_POINT ( 'NONE',  ( -16.78493211734302903, 9.945835743215326374, -121.3360509808959904 ) ) ;
#42577 = EDGE_CURVE ( 'NONE', #257618, #79905, #211238, .T. ) ;
#42576 = CARTESIAN_POINT ( 'NONE',  ( 20.94999999999999929, 5.000000000011153745, -79.40526601891313874 ) ) ;
#42578 = ORIENTED_EDGE ( 'NONE', *, *, #106856, .T. ) ;
#42579 = EDGE_CURVE ( 'NONE', #226785, #19773, #91298, .T. ) ;
#42580 = CIRCLE ( 'NONE', #188322, 2.099999999999989875 ) ;
#42582 = AXIS2_PLACEMENT_3D ( 'NONE', #206158, #107038, #186609 ) ;
#42581 = DIRECTION ( 'NONE',  ( 1.000000000000000000, 0.000000000000000000, 0.000000000000000000 ) ) ;
#42583 = DIRECTION ( 'NONE',  ( 0.000000000000000000, 0.000000000000000000, 1.000000000000000000 ) ) ;
#42585 = DIRECTION ( 'NONE',  ( 1.000000000000000000, 0.000000000000000000, 0.000000000000000000 ) ) ;
#42584 = AXIS2_PLACEMENT_3D ( 'NONE', #38542, #118069, #155946 ) ;
#42586 = AXIS2_PLACEMENT_3D ( 'NONE', #73024, #53419, #195526 ) ;
#42587 = DIRECTION ( 'NONE',  ( 0.000000000000000000, -1.000000000000000000, -6.982962677686266711E-15 ) ) ;
#42588 = CIRCLE ( 'NONE', #138426, 0.09999999999999763245 ) ;
#42589 = ORIENTED_EDGE ( 'NONE', *, *, #212731, .F. ) ;
#42591 =( BOUNDED_CURVE ( )  B_SPLINE_CURVE ( 3, ( #23004, #42527, #204159, #65953 ),
 .UNSPECIFIED., .F., .F. ) 
 B_SPLINE_CURVE_WITH_KNOTS ( ( 4, 4 ),
 ( 3.141592653589793116, 4.712388980384689674 ),
 .UNSPECIFIED. ) 
 CURVE ( )  GEOMETRIC_REPRESENTATION_ITEM ( )  RATIONAL_B_SPLINE_CURVE ( ( 1.000000000000000000, 0.8047378541243649375, 0.8047378541243649375, 1.000000000000000000 ) ) 
 REPRESENTATION_ITEM ( '' )  );
#42590 = AXIS2_PLACEMENT_3D ( 'NONE', #52858, #230222, #50282 ) ;
#42593 = ORIENTED_EDGE ( 'NONE', *, *, #196269, .F. ) ;
#42592 = LINE ( 'NONE', #23058, #229285 ) ;
#42594 = EDGE_CURVE ( 'NONE', #34617, #156004, #195581, .T. ) ;
#42595 = CARTESIAN_POINT ( 'NONE',  ( -18.39999999999999858, 85.50000000001233502, -163.0238218066854472 ) ) ;
#42596 = CARTESIAN_POINT ( 'NONE',  ( -20.00857864376270001, 9.150000000011157653, -146.2500000000000284 ) ) ;
#42597 = EDGE_CURVE ( 'NONE', #38899, #94760, #58148, .T. ) ;
#42598 = AXIS2_PLACEMENT_3D ( 'NONE', #244315, #83920, #163513 ) ;
#42599 = DIRECTION ( 'NONE',  ( 0.000000000000000000, 1.734723475976817507E-14, -1.000000000000000000 ) ) ;
#42600 = DIRECTION ( 'NONE',  ( -0.000000000000000000, 0.000000000000000000, 1.000000000000000000 ) ) ;
#42601 = LINE ( 'NONE', #161283, #100640 ) ;
#42602 = DIRECTION ( 'NONE',  ( 0.000000000000000000, 0.000000000000000000, 1.000000000000000000 ) ) ;
#42603 = ORIENTED_EDGE ( 'NONE', *, *, #115456, .F. ) ;
#42604 = CARTESIAN_POINT ( 'NONE',  ( 21.13461538461538325, 61.88829803306103372, -221.6099259868126694 ) ) ;
#42605 = CARTESIAN_POINT ( 'NONE',  ( -22.45354308602459525, 2.198771867883399074E-07, 11.75043289045890127 ) ) ;
#42606 = CARTESIAN_POINT ( 'NONE',  ( 21.46681500593256331, 6.857511159395965450, -134.0000000000000000 ) ) ;
#42607 = EDGE_CURVE ( 'NONE', #118204, #249188, #158189, .T. ) ;
#42608 = DIRECTION ( 'NONE',  ( 1.000000000000000000, 0.000000000000000000, 0.000000000000000000 ) ) ;
#42609 = AXIS2_PLACEMENT_3D ( 'NONE', #193696, #157152, #155870 ) ;
#42610 = DIRECTION ( 'NONE',  ( 0.000000000000000000, -7.272083257015735086E-15, 1.000000000000000000 ) ) ;
#42611 = VECTOR ( 'NONE', #65756, 1000.000000000000000 ) ;
#42612 = VERTEX_POINT ( 'NONE', #212541 ) ;
#42613 = ORIENTED_EDGE ( 'NONE', *, *, #240506, .T. ) ;
#42614 = DIRECTION ( 'NONE',  ( -0.000000000000000000, -0.000000000000000000, -1.000000000000000000 ) ) ;
#42615 = CARTESIAN_POINT ( 'NONE',  ( -16.87683809663752399, 23.59405348476682107, -231.3784738672518415 ) ) ;
#42616 = CARTESIAN_POINT ( 'NONE',  ( -20.54999999999999716, 0.000000000000000000, 0.000000000000000000 ) ) ;
#42617 = CARTESIAN_POINT ( 'NONE',  ( 20.94999999999999929, 17.06838326776701109, -224.6250846885016870 ) ) ;
#42618 = ORIENTED_EDGE ( 'NONE', *, *, #88156, .F. ) ;
#42619 = LINE ( 'NONE', #142975, #172158 ) ;
#42620 = DIRECTION ( 'NONE',  ( -0.000000000000000000, -0.000000000000000000, 1.000000000000000000 ) ) ;
#42621 = ADVANCED_FACE ( 'NONE', ( #112162 ), #16500, .F. ) ;
#42622 = CARTESIAN_POINT ( 'NONE',  ( -18.59999999999999787, 66.65000000001187175, -90.87310748452436826 ) ) ;
#42623 = CARTESIAN_POINT ( 'NONE',  ( -20.54999999999999716, -8.999999999988844479, -157.6060308773475924 ) ) ;
#42624 = ADVANCED_FACE ( 'NONE', ( #28800 ), #150006, .T. ) ;
#42625 = B_SPLINE_CURVE_WITH_KNOTS ( 'NONE', 3,
 ( #217666, #239835, #40385, #100289, #119912, #233737, #14709, #173810, #80728, #179869 ),
 .UNSPECIFIED., .F., .F.,
 ( 4, 2, 2, 2, 4 ),
 ( 0.000000000000000000, 0.0001584437871624444667, 0.0002376656807436985214, 0.0002772766275343603246, 0.0003168875743250221277 ),
 .UNSPECIFIED. ) ;
#42626 = AXIS2_PLACEMENT_3D ( 'NONE', #45440, #8883, #128839 ) ;
#42627 = ORIENTED_EDGE ( 'NONE', *, *, #67596, .F. ) ;
#42628 = CARTESIAN_POINT ( 'NONE',  ( -20.94999999999999929, -4.714262876194486473, -233.3440214805475819 ) ) ;
#42629 = EDGE_CURVE ( 'NONE', #185777, #54825, #116458, .T. ) ;
#42630 = ORIENTED_EDGE ( 'NONE', *, *, #160764, .T. ) ;
#42631 = CARTESIAN_POINT ( 'NONE',  ( 21.04999999999999716, 69.55891531154070151, -170.0053880512155615 ) ) ;
#42632 = CARTESIAN_POINT ( 'NONE',  ( -21.07954640115394085, 10.05929242768339371, -228.1222958643088248 ) ) ;
#42633 = CARTESIAN_POINT ( 'NONE',  ( -1.820710678118657944, -4.435039894044390252, -227.2960777983303160 ) ) ;
#42634 = DIRECTION ( 'NONE',  ( -1.652117596168391306E-15, -0.9770955615653313941, -0.2128009952263603677 ) ) ;
#42636 = EDGE_CURVE ( 'NONE', #111464, #49762, #220506, .T. ) ;
#42635 = CARTESIAN_POINT ( 'NONE',  ( 23.24999999999999289, 69.35000000001156195, -57.37310748452436826 ) ) ;
#42637 = PLANE ( 'NONE',  #249614 ) ;
#42638 = DIRECTION ( 'NONE',  ( 0.000000000000000000, -0.9876197685951263461, 0.1568667991644794590 ) ) ;
#42639 = CARTESIAN_POINT ( 'NONE',  ( -22.00411653962179415, 7.253442868381127617, -66.90096189419944039 ) ) ;
#42640 = CYLINDRICAL_SURFACE ( 'NONE', #208845, 0.09999999999999939493 ) ;
#42641 = ADVANCED_FACE ( 'NONE', ( #11783 ), #92558, .T. ) ;
#42642 = CARTESIAN_POINT ( 'NONE',  ( 18.59999999999999787, 1.115600667400684642E-11, -134.0000000000000000 ) ) ;
#42643 = CARTESIAN_POINT ( 'NONE',  ( 18.50000000000000000, -9.399999999999998579, -40.38204184817267617 ) ) ;
#42644 = DIRECTION ( 'NONE',  ( 1.000000000000000000, -0.000000000000000000, 0.000000000000000000 ) ) ;
#42645 = CARTESIAN_POINT ( 'NONE',  ( -0.8999999999999437339, 67.75000000001118394, -12.62310748452478926 ) ) ;
#42646 = ADVANCED_FACE ( 'NONE', ( #230824 ), #87198, .T. ) ;
#42647 = AXIS2_PLACEMENT_3D ( 'NONE', #102237, #185675, #223497 ) ;
#42649 = ADVANCED_FACE ( 'NONE', ( #207405 ), #108076, .F. ) ;
#42648 = ADVANCED_FACE ( 'NONE', ( #48309 ), #41448, .T. ) ;
#42650 = ORIENTED_EDGE ( 'NONE', *, *, #227737, .T. ) ;
#42651 = DIRECTION ( 'NONE',  ( -1.000000000000000000, -0.000000000000000000, -0.000000000000000000 ) ) ;
#42652 = CARTESIAN_POINT ( 'NONE',  ( -20.64999999999999858, 73.50000000001205080, -123.2984855617622202 ) ) ;
#42653 = VERTEX_POINT ( 'NONE', #155153 ) ;
#42654 = CARTESIAN_POINT ( 'NONE',  ( 22.50000000000000000, 7.750000000011162626, -100.4000000000000341 ) ) ;
#42655 = LINE ( 'NONE', #158788, #147305 ) ;
#42656 = ORIENTED_EDGE ( 'NONE', *, *, #177110, .F. ) ;
#42657 = CARTESIAN_POINT ( 'NONE',  ( 21.30000000000002558, -0.8618440306552707098, -197.0427629756619297 ) ) ;
#42658 = CARTESIAN_POINT ( 'NONE',  ( 18.59999999999999076, 6.450000000011156587, -43.51702717044002355 ) ) ;
#42659 = CIRCLE ( 'NONE', #242568, 11.70000000000000284 ) ;
#42660 = EDGE_LOOP ( 'NONE', ( #101318, #199850, #192009, #168492, #239834 ) ) ;
#42661 = ADVANCED_FACE ( 'NONE', ( #78128 ), #232983, .F. ) ;
#42662 = ADVANCED_FACE ( 'NONE', ( #258012 ), #194272, .F. ) ;
#42663 = CIRCLE ( 'NONE', #96810, 0.09999999999999939493 ) ;
#42664 = EDGE_LOOP ( 'NONE', ( #13856, #88405, #42242, #255574 ) ) ;
#42665 = DIRECTION ( 'NONE',  ( 0.000000000000000000, -0.8814952561688413901, 0.4721928772777376215 ) ) ;
#42666 = VECTOR ( 'NONE', #200661, 1000.000000000000114 ) ;
#42667 = EDGE_CURVE ( 'NONE', #35453, #47428, #24889, .T. ) ;
#42668 = ORIENTED_EDGE ( 'NONE', *, *, #188970, .F. ) ;
#42669 = DIRECTION ( 'NONE',  ( 0.000000000000000000, 0.9126074666063844765, 0.4088369013363113980 ) ) ;
#42670 = EDGE_CURVE ( 'NONE', #161077, #13860, #83072, .T. ) ;
#42671 = DIRECTION ( 'NONE',  ( -1.000000000000000000, 0.000000000000000000, 0.000000000000000000 ) ) ;
#42673 = CARTESIAN_POINT ( 'NONE',  ( -20.64999999999999858, 76.00000000001243450, -168.0231074845243597 ) ) ;
#42672 = PRODUCT_DEFINITION_CONTEXT ( 'detailed design', #175775, 'design' ) ;
#42674 = DIRECTION ( 'NONE',  ( -1.000000000000000000, 3.265361837132813093E-16, 2.280189983783949500E-30 ) ) ;
#42675 = CYLINDRICAL_SURFACE ( 'NONE', #47532, 0.1000000000000028644 ) ;
#42676 = EDGE_CURVE ( 'NONE', #45367, #12292, #228870, .T. ) ;
#42677 = DIRECTION ( 'NONE',  ( 0.000000000000000000, 0.000000000000000000, -1.000000000000000000 ) ) ;
#42678 = VECTOR ( 'NONE', #137414, 999.9999999999998863 ) ;
#42679 = CARTESIAN_POINT ( 'NONE',  ( 21.05000000000000071, 1.115600667400684642E-11, -67.00000000000000000 ) ) ;
#42681 = CARTESIAN_POINT ( 'NONE',  ( 18.59999999999999432, 1.162701749949165642, -41.60000000000000142 ) ) ;
#42680 = AXIS2_PLACEMENT_3D ( 'NONE', #132884, #70364, #10374 ) ;
#42683 = EDGE_LOOP ( 'NONE', ( #76966, #19772, #7894, #96060, #195626, #106918, #113762, #132799, #44666 ) ) ;
#42682 = CARTESIAN_POINT ( 'NONE',  ( -18.58693740092145319, -9.406432150241794687, -40.62481645650139939 ) ) ;
#42684 = ORIENTED_EDGE ( 'NONE', *, *, #164339, .F. ) ;
#42686 = CARTESIAN_POINT ( 'NONE',  ( -21.05000000000000071, 2.923777413779037548, -208.5507632484912222 ) ) ;
#42685 = CARTESIAN_POINT ( 'NONE',  ( -21.65000000000000213, 45.23934133962703186, -237.7629717664446787 ) ) ;
#42688 = ORIENTED_EDGE ( 'NONE', *, *, #254388, .F. ) ;
#42687 = CARTESIAN_POINT ( 'NONE',  ( -16.87683809663750267, 61.13629130372253684, -220.3155949669961160 ) ) ;
#42689 = ORIENTED_EDGE ( 'NONE', *, *, #207552, .T. ) ;
#42690 = CARTESIAN_POINT ( 'NONE',  ( 23.14999999999999858, 5.000000000011153745, -88.09473398108696074 ) ) ;
#42691 = CARTESIAN_POINT ( 'NONE',  ( 20.54374330479337374, 10.50501031423420351, -175.2256836348880711 ) ) ;
#42692 = DIRECTION ( 'NONE',  ( 7.304098846218132695E-16, -0.4721928772777346794, -0.8814952561688431665 ) ) ;
#42693 = VECTOR ( 'NONE', #13206, 1000.000000000000227 ) ;
#42694 = CARTESIAN_POINT ( 'NONE',  ( -18.59999999999999787, 9.350000000011156942, -146.2500000000000284 ) ) ;
#42695 = EDGE_CURVE ( 'NONE', #254423, #99179, #68337, .T. ) ;
#42696 = CARTESIAN_POINT ( 'NONE',  ( -20.94999999999999929, -11.64999999998884306, -170.5999999999999659 ) ) ;
#42697 = FACE_OUTER_BOUND ( 'NONE', #50899, .T. ) ;
#42698 = VECTOR ( 'NONE', #166424, 1000.000000000000000 ) ;
#42699 = VECTOR ( 'NONE', #79242, 1000.000000000000000 ) ;
#42700 = VECTOR ( 'NONE', #67978, 1000.000000000000000 ) ;
#42702 = AXIS2_PLACEMENT_3D ( 'NONE', #135487, #54680, #252879 ) ;
#42701 = DIRECTION ( 'NONE',  ( -0.000000000000000000, -0.01283462868040327436, 0.9999176327611370985 ) ) ;
#42703 = EDGE_CURVE ( 'NONE', #183962, #249855, #149788, .T. ) ;
#42704 = ORIENTED_EDGE ( 'NONE', *, *, #88066, .F. ) ;
#42705 = ORIENTED_EDGE ( 'NONE', *, *, #48637, .T. ) ;
#42706 = CARTESIAN_POINT ( 'NONE',  ( 20.85000000000000142, 45.93315328338058379, -256.6017782078560003 ) ) ;
#42707 = ORIENTED_EDGE ( 'NONE', *, *, #214625, .F. ) ;
#42708 = DIRECTION ( 'NONE',  ( 1.000000000000000000, -0.000000000000000000, 0.000000000000000000 ) ) ;
#42709 = EDGE_LOOP ( 'NONE', ( #21661, #123575, #188696, #62281 ) ) ;
#42710 = DIRECTION ( 'NONE',  ( 1.284434275755705296E-16, -0.7071067811865471286, 0.7071067811865479058 ) ) ;
#42711 = CARTESIAN_POINT ( 'NONE',  ( -12.24999999999999822, 48.22810253856973617, -234.1229447132332382 ) ) ;
#42712 = EDGE_CURVE ( 'NONE', #68808, #207338, #37346, .T. ) ;
#42713 = FACE_OUTER_BOUND ( 'NONE', #35896, .T. ) ;
#42714 = CARTESIAN_POINT ( 'NONE',  ( -21.07971444708686093, 75.91217656369489930, -209.8528995661509100 ) ) ;
#42715 = VERTEX_POINT ( 'NONE', #119866 ) ;
#42716 = DIRECTION ( 'NONE',  ( 0.000000000000000000, 0.000000000000000000, 1.000000000000000000 ) ) ;
#42717 = ORIENTED_EDGE ( 'NONE', *, *, #209373, .F. ) ;
#42718 = DIRECTION ( 'NONE',  ( 0.000000000000000000, 1.000000000000000000, 6.982962677686266711E-15 ) ) ;
#42719 = DIRECTION ( 'NONE',  ( 0.000000000000000000, -0.8814952561688430555, 0.4721928772777346239 ) ) ;
#42720 = DIRECTION ( 'NONE',  ( 0.000000000000000000, 0.8814952561688437216, -0.4721928772777334582 ) ) ;
#42721 = CARTESIAN_POINT ( 'NONE',  ( 21.05000000000005400, 87.50449464844290048, -34.18759587077607165 ) ) ;
#42722 = ORIENTED_EDGE ( 'NONE', *, *, #170509, .F. ) ;
#42723 = AXIS2_PLACEMENT_3D ( 'NONE', #89616, #58179, #137721 ) ;
#42724 = CARTESIAN_POINT ( 'NONE',  ( -23.15000000000000213, 7.128833340094563376, -233.7327013124401276 ) ) ;
#42725 = ORIENTED_EDGE ( 'NONE', *, *, #173386, .F. ) ;
#42728 = VERTEX_POINT ( 'NONE', #79407 ) ;
#42727 = FACE_OUTER_BOUND ( 'NONE', #159331, .T. ) ;
#42726 = CARTESIAN_POINT ( 'NONE',  ( -22.49533356619858893, 64.34999999370857893, -203.5882300648471244 ) ) ;
#42729 = CIRCLE ( 'NONE', #17761, 0.09999999999998866740 ) ;
#42730 = EDGE_CURVE ( 'NONE', #13008, #204451, #124820, .T. ) ;
#42731 = CARTESIAN_POINT ( 'NONE',  ( -22.47071067811865319, 0.09909245471376171288, -159.7799252555019223 ) ) ;
#42732 = EDGE_LOOP ( 'NONE', ( #216306, #184945, #187242, #139078 ) ) ;
#42733 = DIRECTION ( 'NONE',  ( 0.000000000000000000, 0.9126074666063757057, 0.4088369013363309379 ) ) ;
#42734 = ORIENTED_EDGE ( 'NONE', *, *, #244057, .F. ) ;
#42735 = DIRECTION ( 'NONE',  ( 1.073024830501117528E-15, 0.8814952561688430555, -0.4721928772777346239 ) ) ;
#42736 = AXIS2_PLACEMENT_3D ( 'NONE', #188396, #89288, #47588 ) ;
#42737 = CARTESIAN_POINT ( 'NONE',  ( -16.93415306273742260, 9.995622260023671046, -54.41005694236041990 ) ) ;
#42738 = DIRECTION ( 'NONE',  ( -1.000000000000000000, -1.794895427898103559E-16, -3.909090864890002444E-17 ) ) ;
#42740 = ORIENTED_EDGE ( 'NONE', *, *, #107579, .T. ) ;
#42739 = LINE ( 'NONE', #182265, #122754 ) ;
#42741 = VECTOR ( 'NONE', #153272, 1000.000000000000000 ) ;
#42742 = DIRECTION ( 'NONE',  ( 0.000000000000000000, 1.000000000000000000, 0.000000000000000000 ) ) ;
#42743 = AXIS2_PLACEMENT_3D ( 'NONE', #6166, #85675, #1006 ) ;
#42744 = VERTEX_POINT ( 'NONE', #57272 ) ;
#42745 = TOROIDAL_SURFACE ( 'NONE', #34407, 0.2000000000000000111, 0.1000000000000000056 ) ;
#42746 = AXIS2_PLACEMENT_3D ( 'NONE', #221734, #198345, #163095 ) ;
#42747 = CARTESIAN_POINT ( 'NONE',  ( -23.25000000000000000, 7.128833340094563376, -233.7327013124401276 ) ) ;
#42748 = CARTESIAN_POINT ( 'NONE',  ( 18.57071067811864040, 10.17928932188134539, -21.35000000000000142 ) ) ;
#42749 = FACE_OUTER_BOUND ( 'NONE', #194374, .T. ) ;
#42750 = ORIENTED_EDGE ( 'NONE', *, *, #159260, .F. ) ;
#42751 = CARTESIAN_POINT ( 'NONE',  ( -18.59999999999999787, 12.87592094156238609, -205.3750039893633073 ) ) ;
#42753 = ORIENTED_EDGE ( 'NONE', *, *, #239243, .F. ) ;
#42752 = VECTOR ( 'NONE', #127288, 1000.000000000000114 ) ;
#42754 = DIRECTION ( 'NONE',  ( -1.000000000000000000, 0.000000000000000000, 0.000000000000000000 ) ) ;
#42755 = AXIS2_PLACEMENT_3D ( 'NONE', #222933, #2603, #242506 ) ;
#42756 = DIRECTION ( 'NONE',  ( 1.000000000000000000, 1.186688945009009831E-16, 0.000000000000000000 ) ) ;
#42757 = CARTESIAN_POINT ( 'NONE',  ( -21.05000000000000071, -1.835341550213255957, -179.0551512925629538 ) ) ;
#42759 = ORIENTED_EDGE ( 'NONE', *, *, #10597, .T. ) ;
#42758 = CARTESIAN_POINT ( 'NONE',  ( 20.12500000000000000, 9.750000000011153745, -142.1117712821142902 ) ) ;
#42760 = CYLINDRICAL_SURFACE ( 'NONE', #8773, 0.1000000000000056261 ) ;
#42761 = TOROIDAL_SURFACE ( 'NONE', #184406, 11.70000000000000462, 0.1000000000000000056 ) ;
#42762 = CARTESIAN_POINT ( 'NONE',  ( -22.39999999999999858, -0.09999999998884338825, -55.35042919245524473 ) ) ;
#42763 = CIRCLE ( 'NONE', #213446, 0.1000000000000017958 ) ;
#42764 = EDGE_CURVE ( 'NONE', #208002, #75479, #170664, .T. ) ;
#42765 = DIRECTION ( 'NONE',  ( 1.000000000000000000, 0.000000000000000000, 0.000000000000000000 ) ) ;
#42766 = ORIENTED_EDGE ( 'NONE', *, *, #147035, .F. ) ;
#42767 = AXIS2_PLACEMENT_3D ( 'NONE', #181957, #64561, #99809 ) ;
#42768 = DIRECTION ( 'NONE',  ( 0.000000000000000000, 0.000000000000000000, -1.000000000000000000 ) ) ;
#42769 = CARTESIAN_POINT ( 'NONE',  ( -21.14999999999994174, 83.90000000001120384, -37.18565239344504647 ) ) ;
#42770 = EDGE_LOOP ( 'NONE', ( #200309, #140821, #254104, #157909 ) ) ;
#42771 = CARTESIAN_POINT ( 'NONE',  ( 22.59999985501178799, 64.25013020700939137, -170.0887061543242567 ) ) ;
#42772 = AXIS2_PLACEMENT_3D ( 'NONE', #236150, #233595, #215300 ) ;
#42773 = ORIENTED_EDGE ( 'NONE', *, *, #115097, .T. ) ;
#42774 = VECTOR ( 'NONE', #77254, 1000.000000000000000 ) ;
#42775 = CARTESIAN_POINT ( 'NONE',  ( -20.94999999999999929, 1.835341550235569663, -179.0551512925629538 ) ) ;
#42776 = ORIENTED_EDGE ( 'NONE', *, *, #214270, .F. ) ;
#42778 = ORIENTED_EDGE ( 'NONE', *, *, #220191, .T. ) ;
#42777 = PLANE ( 'NONE',  #117962 ) ;
#42779 = ADVANCED_FACE ( 'NONE', ( #233395 ), #54726, .F. ) ;
#42780 = ADVANCED_FACE ( 'NONE', ( #213803 ), #62271, .T. ) ;
#42783 = EDGE_LOOP ( 'NONE', ( #193405, #115087, #143187, #186313 ) ) ;
#42782 = ORIENTED_EDGE ( 'NONE', *, *, #58949, .F. ) ;
#42781 = CARTESIAN_POINT ( 'NONE',  ( -11.59999999999994458, 64.35000000001120668, -21.02310748452479316 ) ) ;
#42784 = CARTESIAN_POINT ( 'NONE',  ( 20.94999999999999929, 68.22899648672319017, -213.7884437866858889 ) ) ;
#42785 = CARTESIAN_POINT ( 'NONE',  ( -20.94983749550516450, 65.70233904876961617, -30.54874109119683823 ) ) ;
#42786 = CARTESIAN_POINT ( 'NONE',  ( -23.15000000000000213, 76.00000000001189449, -101.0231074845243029 ) ) ;
#42788 = CARTESIAN_POINT ( 'NONE',  ( -16.89318236219975944, 9.951535257875127272, -20.85512963210584658 ) ) ;
#42787 = CARTESIAN_POINT ( 'NONE',  ( -20.64999999999999858, 1.115600667400684642E-11, -100.5000000000000426 ) ) ;
#42790 = EDGE_CURVE ( 'NONE', #14749, #243821, #189530, .T. ) ;
#42789 = VECTOR ( 'NONE', #47736, 1000.000000000000000 ) ;
#42791 = DIRECTION ( 'NONE',  ( 0.000000000000000000, 0.2716869542551192951, -0.9623856809447951521 ) ) ;
#42792 = CIRCLE ( 'NONE', #9468, 0.09999999999999982514 ) ;
#42793 = CARTESIAN_POINT ( 'NONE',  ( -20.65000000000000568, 11.52084357182974195, -219.8296352432475942 ) ) ;
#42796 = DIRECTION ( 'NONE',  ( 0.000000000000000000, 0.000000000000000000, 1.000000000000000000 ) ) ;
#42795 = FACE_OUTER_BOUND ( 'NONE', #148304, .T. ) ;
#42794 = CIRCLE ( 'NONE', #155262, 4.000000000000003553 ) ;
#42797 = ORIENTED_EDGE ( 'NONE', *, *, #75007, .F. ) ;
#42798 = EDGE_LOOP ( 'NONE', ( #210946, #243300, #119949, #218276 ) ) ;
#42799 = ADVANCED_FACE ( 'NONE', ( #121160 ), #45705, .T. ) ;
#42800 = CARTESIAN_POINT ( 'NONE',  ( -18.50000000000000000, 11.65000000001115232, -79.15000000000003411 ) ) ;
#42803 = ORIENTED_EDGE ( 'NONE', *, *, #20863, .T. ) ;
#42802 = ADVANCED_FACE ( 'NONE', ( #61146 ), #164110, .F. ) ;
#42801 = DIRECTION ( 'NONE',  ( 0.7071067811865463515, 0.7071067811865487940, 4.937700262164540154E-15 ) ) ;
#42804 = ORIENTED_EDGE ( 'NONE', *, *, #184521, .T. ) ;
#42805 = ORIENTED_EDGE ( 'NONE', *, *, #80041, .T. ) ;
#42806 = DIRECTION ( 'NONE',  ( 0.000000000000000000, 0.1455152366551700771, 0.9893560106964479628 ) ) ;
#42807 = EDGE_CURVE ( 'NONE', #249313, #197578, #84511, .T. ) ;
#42808 = ORIENTED_EDGE ( 'NONE', *, *, #204639, .T. ) ;
#42809 = EDGE_CURVE ( 'NONE', #109875, #138313, #191489, .T. ) ;
#42810 = FACE_OUTER_BOUND ( 'NONE', #8147, .T. ) ;
#42811 = CARTESIAN_POINT ( 'NONE',  ( -21.05000000000000071, 74.73821383144729680, -161.9366085209788935 ) ) ;
#42812 = AXIS2_PLACEMENT_3D ( 'NONE', #191052, #12412, #213149 ) ;
#42814 = ORIENTED_EDGE ( 'NONE', *, *, #96210, .T. ) ;
#42813 = ORIENTED_EDGE ( 'NONE', *, *, #240143, .F. ) ;
#42815 = ORIENTED_EDGE ( 'NONE', *, *, #218107, .T. ) ;
#42816 = CYLINDRICAL_SURFACE ( 'NONE', #123795, 11.74999999999999822 ) ;
#42818 = ORIENTED_EDGE ( 'NONE', *, *, #234152, .F. ) ;
#42817 = EDGE_CURVE ( 'NONE', #21663, #253988, #101519, .T. ) ;
#42819 = VERTEX_POINT ( 'NONE', #140682 ) ;
#42820 = DIRECTION ( 'NONE',  ( -5.603264701231743991E-32, 1.897661533703520143E-16, -1.000000000000000000 ) ) ;
#42821 = CIRCLE ( 'NONE', #150975, 0.09999999999999939493 ) ;
#42823 = ORIENTED_EDGE ( 'NONE', *, *, #238324, .F. ) ;
#42822 = DIRECTION ( 'NONE',  ( 0.000000000000000000, 0.9910465087640866200, -0.1335171055202867274 ) ) ;
#42824 = EDGE_CURVE ( 'NONE', #251013, #86684, #120557, .T. ) ;
#42826 = FACE_OUTER_BOUND ( 'NONE', #220946, .T. ) ;
#42825 = CARTESIAN_POINT ( 'NONE',  ( -22.50000000000000000, 1.115600667400684642E-11, -100.5000000000000284 ) ) ;
#42827 = DIRECTION ( 'NONE',  ( 1.000000000000000000, 0.000000000000000000, 0.000000000000000000 ) ) ;
#42828 = CARTESIAN_POINT ( 'NONE',  ( -18.59999999999999787, 77.83585931145526615, -58.01866831572577610 ) ) ;
#42829 = DIRECTION ( 'NONE',  ( 0.000000000000000000, 1.000000000000000000, 6.608470384673536824E-15 ) ) ;
#42830 = ORIENTED_EDGE ( 'NONE', *, *, #198237, .F. ) ;
#42832 = ADVANCED_FACE ( 'NONE', ( #144518 ), #123701, .T. ) ;
#42831 = VERTEX_POINT ( 'NONE', #145807 ) ;
#42833 = FACE_OUTER_BOUND ( 'NONE', #73963, .T. ) ;
#42834 = DIRECTION ( 'NONE',  ( 5.603264701231745086E-32, 7.172728831056619538E-15, -1.000000000000000000 ) ) ;
#42835 = ORIENTED_EDGE ( 'NONE', *, *, #74610, .F. ) ;
#42836 = CARTESIAN_POINT ( 'NONE',  ( 21.11344571971309136, 10.61787902352891066, -45.74602089239949265 ) ) ;
#42837 = AXIS2_PLACEMENT_3D ( 'NONE', #118986, #238926, #139799 ) ;
#42838 = DIRECTION ( 'NONE',  ( -1.000000000000000000, -7.049440681616513945E-16, 1.911869773728117920E-16 ) ) ;
#42839 = CARTESIAN_POINT ( 'NONE',  ( -18.59999999999999787, -1.135018845899022466, -141.7169768834323520 ) ) ;
#42840 = ORIENTED_EDGE ( 'NONE', *, *, #217316, .T. ) ;
#42841 = ORIENTED_EDGE ( 'NONE', *, *, #190632, .F. ) ;
#42842 = ADVANCED_FACE ( 'NONE', ( #181118 ), #239797, .F. ) ;
#42843 = DIRECTION ( 'NONE',  ( 0.000000000000000000, 0.2128009952263605342, -0.9770955615653315052 ) ) ;
#42844 = CARTESIAN_POINT ( 'NONE',  ( -21.14999999999999858, -3.187427350888460076, -228.3200064793908837 ) ) ;
#42845 = EDGE_LOOP ( 'NONE', ( #256675, #33731, #256195, #53328, #112366, #132750, #212571, #149961, #256215, #37005, #27756, #30000 ) ) ;
#42846 = CARTESIAN_POINT ( 'NONE',  ( -20.85000000000000142, 64.35000000001214460, -136.5231074845244166 ) ) ;
#42847 = ORIENTED_EDGE ( 'NONE', *, *, #172760, .T. ) ;
#42848 = DIRECTION ( 'NONE',  ( -1.000000000000000000, 0.000000000000000000, 0.000000000000000000 ) ) ;
#42849 = CYLINDRICAL_SURFACE ( 'NONE', #108072, 1.749999999999999778 ) ;
#42851 = DIRECTION ( 'NONE',  ( 4.504528286903032433E-15, -0.1298341882520124002, -0.9915357197604841577 ) ) ;
#42850 = CARTESIAN_POINT ( 'NONE',  ( -21.70464131381649509, 10.47921085838517463, -227.4781768778995570 ) ) ;
#42852 = DIRECTION ( 'NONE',  ( -1.000000000000000000, -0.000000000000000000, 0.000000000000000000 ) ) ;
#42853 = DIRECTION ( 'NONE',  ( 1.000000000000000000, 0.000000000000000000, -0.000000000000000000 ) ) ;
#42854 = ORIENTED_EDGE ( 'NONE', *, *, #24016, .F. ) ;
#42855 = AXIS2_PLACEMENT_3D ( 'NONE', #49017, #86841, #25617 ) ;
#42856 = CARTESIAN_POINT ( 'NONE',  ( -19.99999999999999645, 4.527376849368447864, 21.95857864376269220 ) ) ;
#42857 = CIRCLE ( 'NONE', #238487, 0.09999999999999810429 ) ;
#42858 = ADVANCED_FACE ( 'NONE', ( #81957 ), #124109, .T. ) ;
#42860 = ORIENTED_EDGE ( 'NONE', *, *, #151865, .T. ) ;
#42859 = ORIENTED_EDGE ( 'NONE', *, *, #79042, .F. ) ;
#42861 = ORIENTED_EDGE ( 'NONE', *, *, #145301, .T. ) ;
#42862 = VERTEX_POINT ( 'NONE', #242348 ) ;
#42863 = AXIS2_PLACEMENT_3D ( 'NONE', #13392, #214150, #154224 ) ;
#42864 = CARTESIAN_POINT ( 'NONE',  ( -21.05000000000000071, 87.65000000001144542, -38.92310748452424463 ) ) ;
#42865 = CARTESIAN_POINT ( 'NONE',  ( 21.05000000000000071, -3.187427350888460076, -228.3200064793908837 ) ) ;
#42866 = DIRECTION ( 'NONE',  ( 0.000000000000000000, 0.000000000000000000, -1.000000000000000000 ) ) ;
#42867 = DIRECTION ( 'NONE',  ( 1.000000000000000000, 0.000000000000000000, 0.000000000000000000 ) ) ;
#42868 = DIRECTION ( 'NONE',  ( 1.000000000000000000, 0.000000000000000000, 0.000000000000000000 ) ) ;
#42869 = EDGE_CURVE ( 'NONE', #86057, #222451, #258049, .T. ) ;
#42870 = CARTESIAN_POINT ( 'NONE',  ( -18.40000000000000213, 11.47316190337362762, -113.0500000000000398 ) ) ;
#42872 = EDGE_LOOP ( 'NONE', ( #33514, #212962, #80916, #208042 ) ) ;
#42871 = CARTESIAN_POINT ( 'NONE',  ( 18.37172112093938026, 77.36523961789227144, -241.8027249817224629 ) ) ;
#42873 = DIRECTION ( 'NONE',  ( 1.000000000000000000, 0.000000000000000000, 0.000000000000000000 ) ) ;
#42874 = ORIENTED_EDGE ( 'NONE', *, *, #241963, .T. ) ;
#42875 = DIRECTION ( 'NONE',  ( 0.000000000000000000, -1.000000000000000000, 0.000000000000000000 ) ) ;
#42876 = ORIENTED_EDGE ( 'NONE', *, *, #112527, .T. ) ;
#42877 = ORIENTED_EDGE ( 'NONE', *, *, #183711, .F. ) ;
#42878 = CARTESIAN_POINT ( 'NONE',  ( -21.05000000000000071, -1.835341550213255957, -179.0551512925629538 ) ) ;
#42880 = AXIS2_PLACEMENT_3D ( 'NONE', #213773, #76822, #195522 ) ;
#42879 = CARTESIAN_POINT ( 'NONE',  ( 22.47071067811865319, 0.09909245471376171288, -25.77992525550195424 ) ) ;
#42882 = EDGE_CURVE ( 'NONE', #240363, #170273, #99235, .T. ) ;
#42881 = DIRECTION ( 'NONE',  ( -1.000000000000000000, -3.265361837132813093E-16, 0.000000000000000000 ) ) ;
#42883 = CIRCLE ( 'NONE', #221907, 0.5000000000000004441 ) ;
#42884 = EDGE_CURVE ( 'NONE', #185772, #210485, #230499, .T. ) ;
#42885 = CARTESIAN_POINT ( 'NONE',  ( -23.15000000000000213, 71.65000000001228386, -157.6731074845243938 ) ) ;
#42886 = EDGE_CURVE ( 'NONE', #38614, #230960, #12755, .T. ) ;
#42887 = CYLINDRICAL_SURFACE ( 'NONE', #75935, 0.1000000000000054040 ) ;
#42888 = ORIENTED_EDGE ( 'NONE', *, *, #139178, .F. ) ;
#42889 = ORIENTED_EDGE ( 'NONE', *, *, #245805, .F. ) ;
#42890 = EDGE_CURVE ( 'NONE', #241094, #22343, #133194, .T. ) ;
#42891 = AXIS2_PLACEMENT_3D ( 'NONE', #7564, #104070, #204468 ) ;
#42892 = FACE_OUTER_BOUND ( 'NONE', #240091, .T. ) ;
#42893 = ORIENTED_EDGE ( 'NONE', *, *, #66187, .T. ) ;
#42894 = CARTESIAN_POINT ( 'NONE',  ( -20.94999999999999929, 74.16465844978715438, -57.96795619196134908 ) ) ;
#42895 = LINE ( 'NONE', #31065, #23638 ) ;
#42896 = CARTESIAN_POINT ( 'NONE',  ( 20.02499999999999858, 66.25000000001179501, -81.87310748452438247 ) ) ;
#42897 = CARTESIAN_POINT ( 'NONE',  ( -21.76363531954647357, 75.90099812571274640, -143.5360440323960347 ) ) ;
#42898 = CARTESIAN_POINT ( 'NONE',  ( -16.77732147278574715, 66.05403306743842506, -90.35959872764857437 ) ) ;
#42899 = CARTESIAN_POINT ( 'NONE',  ( -18.59999999999999787, 9.350000000011156942, -188.8499999999999659 ) ) ;
#42900 = AXIS2_PLACEMENT_3D ( 'NONE', #33044, #94241, #173843 ) ;
#42902 = PLANE ( 'NONE',  #95650 ) ;
#42901 = AXIS2_PLACEMENT_3D ( 'NONE', #186749, #159795, #8103 ) ;
#42903 = DIRECTION ( 'NONE',  ( -0.000000000000000000, -0.000000000000000000, -1.000000000000000000 ) ) ;
#42904 = VECTOR ( 'NONE', #171792, 1000.000000000000000 ) ;
#42905 = CARTESIAN_POINT ( 'NONE',  ( -21.05000000000000071, 6.108674899944905867, -199.6368316019445501 ) ) ;
#42906 = CARTESIAN_POINT ( 'NONE',  ( 18.59999999999997655, 76.00000000001190870, -103.0231074845243029 ) ) ;
#42907 = DIRECTION ( 'NONE',  ( -1.000000000000000000, -0.000000000000000000, -0.000000000000000000 ) ) ;
#42908 = EDGE_CURVE ( 'NONE', #237980, #100973, #246210, .T. ) ;
#42909 = ORIENTED_EDGE ( 'NONE', *, *, #284, .T. ) ;
#42910 = DIRECTION ( 'NONE',  ( 0.000000000000000000, -1.000000000000000000, 0.000000000000000000 ) ) ;
#42911 = EDGE_LOOP ( 'NONE', ( #37708, #203014, #146495, #101341 ) ) ;
#42912 = EDGE_CURVE ( 'NONE', #135120, #18374, #166359, .T. ) ;
#42913 = EDGE_CURVE ( 'NONE', #201784, #187652, #191676, .T. ) ;
#42914 = DIRECTION ( 'NONE',  ( 0.000000000000000000, 1.000000000000000000, -6.308085367188393199E-16 ) ) ;
#42915 = DIRECTION ( 'NONE',  ( 0.000000000000000000, 0.000000000000000000, -1.000000000000000000 ) ) ;
#42916 = DIRECTION ( 'NONE',  ( 1.000000000000000000, -0.000000000000000000, 0.000000000000000000 ) ) ;
#42917 = ORIENTED_EDGE ( 'NONE', *, *, #155150, .T. ) ;
#42918 = CARTESIAN_POINT ( 'NONE',  ( 20.99999999999999645, 19.88654501311280498, -229.5059066796121101 ) ) ;
#42919 = DIRECTION ( 'NONE',  ( 0.000000000000000000, -1.000000000000000000, -6.982962677686266711E-15 ) ) ;
#42921 = CIRCLE ( 'NONE', #167838, 0.6000000000000033085 ) ;
#42920 = PLANE ( 'NONE',  #250492 ) ;
#42922 = ADVANCED_FACE ( 'NONE', ( #109247 ), #169276, .T. ) ;
#42923 = DIRECTION ( 'NONE',  ( 1.000000000000000000, 7.136802563874195162E-16, 1.554319503706929005E-16 ) ) ;
#42924 = DIRECTION ( 'NONE',  ( 0.000000000000000000, -1.000000000000000000, 0.000000000000000000 ) ) ;
#42925 = CARTESIAN_POINT ( 'NONE',  ( 23.14999999999999858, 11.03721558635588806, -232.8814973315346890 ) ) ;
#42926 = ORIENTED_EDGE ( 'NONE', *, *, #632, .T. ) ;
#42927 = CYLINDRICAL_SURFACE ( 'NONE', #66567, 0.09999999999998898659 ) ;
#42929 = VERTEX_POINT ( 'NONE', #250057 ) ;
#42928 = CARTESIAN_POINT ( 'NONE',  ( -16.94445028196808778, 22.96031635112858282, -230.8778361528912058 ) ) ;
#42930 = VECTOR ( 'NONE', #118133, 1000.000000000000000 ) ;
#42931 = DIRECTION ( 'NONE',  ( 0.000000000000000000, 0.000000000000000000, -1.000000000000000000 ) ) ;
#42932 = TOROIDAL_SURFACE ( 'NONE', #30474, 0.2000000000000000111, 0.1000000000000000056 ) ;
#42933 = DIRECTION ( 'NONE',  ( 0.000000000000000000, 0.000000000000000000, -1.000000000000000000 ) ) ;
#42934 = CARTESIAN_POINT ( 'NONE',  ( -23.25000000000000000, 1.115600667400684642E-11, -100.5000000000000426 ) ) ;
#42935 = VERTEX_POINT ( 'NONE', #70164 ) ;
#42936 = LINE ( 'NONE', #200726, #97045 ) ;
#42937 = ITEM_DEFINED_TRANSFORMATION ( 'NONE', 'NONE', #194368,  #2425 ) ;
#42938 = EDGE_CURVE ( 'NONE', #53148, #129691, #232267, .T. ) ;
#42940 = CIRCLE ( 'NONE', #188669, 0.09999999999998898659 ) ;
#42939 = DIRECTION ( 'NONE',  ( 1.000000000000000000, -0.000000000000000000, -0.000000000000000000 ) ) ;
#42941 = ORIENTED_EDGE ( 'NONE', *, *, #224877, .T. ) ;
#42942 = CIRCLE ( 'NONE', #201150, 0.1000000000000000472 ) ;
#42943 = DIRECTION ( 'NONE',  ( 1.000000000000000000, 0.000000000000000000, 0.000000000000000000 ) ) ;
#42944 = CARTESIAN_POINT ( 'NONE',  ( -20.94999999999999929, 5.900000000011162093, -123.7809002353436654 ) ) ;
#42945 = AXIS2_PLACEMENT_3D ( 'NONE', #85752, #165336, #145750 ) ;
#42946 = DIRECTION ( 'NONE',  ( 1.000000000000000000, 0.000000000000000000, 0.000000000000000000 ) ) ;
#42947 = EDGE_LOOP ( 'NONE', ( #38929, #124642, #15564, #178574 ) ) ;
#42948 = ORIENTED_EDGE ( 'NONE', *, *, #233532, .T. ) ;
#42949 = DIRECTION ( 'NONE',  ( 0.000000000000000000, -1.000000000000000000, 0.000000000000000000 ) ) ;
#42951 = AXIS2_PLACEMENT_3D ( 'NONE', #165762, #26244, #129188 ) ;
#42950 = DIRECTION ( 'NONE',  ( -1.000000000000000000, 0.000000000000000000, 0.000000000000000000 ) ) ;
#42953 = VECTOR ( 'NONE', #158513, 1000.000000000000114 ) ;
#42952 = LINE ( 'NONE', #45515, #248695 ) ;
#42954 = CYLINDRICAL_SURFACE ( 'NONE', #131891, 0.1000000000000054040 ) ;
#42955 = ADVANCED_FACE ( 'NONE', ( #72735 ), #152267, .F. ) ;
#42956 = DIRECTION ( 'NONE',  ( 1.000000000000000000, 0.000000000000000000, 0.000000000000000000 ) ) ;
#42957 = CARTESIAN_POINT ( 'NONE',  ( -20.94999999999999929, 77.83534155023646406, -124.9679561919613064 ) ) ;
#42959 = CARTESIAN_POINT ( 'NONE',  ( -21.29999999999995808, 1.115650265596050101E-11, -163.4499999999999886 ) ) ;
#42958 = CARTESIAN_POINT ( 'NONE',  ( 22.39999999999999858, 7.790779598373385184, -1.572093150103981429E-15 ) ) ;
#42960 = AXIS2_PLACEMENT_3D ( 'NONE', #120106, #117504, #256958 ) ;
#42961 = DIRECTION ( 'NONE',  ( -1.000000000000000000, 0.000000000000000000, 0.000000000000000000 ) ) ;
#42962 = EDGE_CURVE ( 'NONE', #188456, #232621, #53134, .T. ) ;
#42963 = DIRECTION ( 'NONE',  ( 1.000000000000000000, 0.000000000000000000, 0.000000000000000000 ) ) ;
#42964 = DIRECTION ( 'NONE',  ( 0.000000000000000000, -1.000000000000000000, -6.982962677686266711E-15 ) ) ;
#42965 = DIRECTION ( 'NONE',  ( 1.000000000000000000, 0.000000000000000000, -0.000000000000000000 ) ) ;
#42966 = ORIENTED_EDGE ( 'NONE', *, *, #129954, .F. ) ;
#42967 = ORIENTED_EDGE ( 'NONE', *, *, #216949, .F. ) ;
#42968 = DIRECTION ( 'NONE',  ( 0.000000000000000000, 0.000000000000000000, -1.000000000000000000 ) ) ;
#42969 = AXIS2_PLACEMENT_3D ( 'NONE', #204399, #84417, #7493 ) ;
#42970 = CARTESIAN_POINT ( 'NONE',  ( -21.14999999999999858, 64.35000000001238618, -169.9231074845244507 ) ) ;
#42971 = CARTESIAN_POINT ( 'NONE',  ( 21.05281448260627641, 67.22398984147497458, -191.3495495727129878 ) ) ;
#42972 = CIRCLE ( 'NONE', #117963, 0.5000000000000004441 ) ;
#42973 = CIRCLE ( 'NONE', #155427, 0.2000000000000005107 ) ;
#42974 = EDGE_CURVE ( 'NONE', #64265, #132923, #31047, .T. ) ;
#42975 = VECTOR ( 'NONE', #228626, 1000.000000000000000 ) ;
#42976 = ADVANCED_FACE ( 'NONE', ( #226625 ), #167988, .F. ) ;
#42977 = DIRECTION ( 'NONE',  ( 1.000000000000000000, -0.000000000000000000, 0.000000000000000000 ) ) ;
#42978 = DIRECTION ( 'NONE',  ( 1.000000000000000000, 0.000000000000000000, 0.000000000000000000 ) ) ;
#42979 = DIRECTION ( 'NONE',  ( 1.000000000000000000, 1.734723475976817507E-14, 0.000000000000000000 ) ) ;
#42980 = ORIENTED_EDGE ( 'NONE', *, *, #241429, .F. ) ;
#42981 = DIRECTION ( 'NONE',  ( 0.000000000000000000, 0.9126074666063769270, 0.4088369013363283844 ) ) ;
#42982 = VERTEX_POINT ( 'NONE', #68871 ) ;
#42983 = CARTESIAN_POINT ( 'NONE',  ( -14.45422546970484312, 9.450602096088523751, -18.44389596309667922 ) ) ;
#42984 = VERTEX_POINT ( 'NONE', #149699 ) ;
#42985 = DIRECTION ( 'NONE',  ( -0.000000000000000000, -1.000000000000000000, -0.000000000000000000 ) ) ;
#42986 = VECTOR ( 'NONE', #26070, 1000.000000000000000 ) ;
#42987 = VECTOR ( 'NONE', #96227, 1000.000000000000114 ) ;
#42989 = EDGE_CURVE ( 'NONE', #17161, #254638, #190087, .T. ) ;
#42988 = VECTOR ( 'NONE', #93398, 1000.000000000000000 ) ;
#42990 = AXIS2_PLACEMENT_3D ( 'NONE', #105280, #206991, #164018 ) ;
#42991 = ADVANCED_FACE ( 'NONE', ( #133947 ), #234332, .T. ) ;
#42992 = CARTESIAN_POINT ( 'NONE',  ( 20.94999999999999929, 74.16465844978715438, -57.96795619196134908 ) ) ;
#42993 = ORIENTED_EDGE ( 'NONE', *, *, #233866, .F. ) ;
#42994 = DIRECTION ( 'NONE',  ( 1.000000000000000000, 0.000000000000000000, 0.000000000000000000 ) ) ;
#42995 = EDGE_LOOP ( 'NONE', ( #139803, #57980, #158477, #71939 ) ) ;
#42996 = FACE_OUTER_BOUND ( 'NONE', #11292, .T. ) ;
#42997 = DIRECTION ( 'NONE',  ( 1.000000000000000000, 0.000000000000000000, -0.000000000000000000 ) ) ;
#42998 = CARTESIAN_POINT ( 'NONE',  ( 23.14999999999999858, 71.00000000001199396, -115.4283735034374274 ) ) ;
#42999 = CARTESIAN_POINT ( 'NONE',  ( 21.14999999999999858, -11.74999999998884448, -79.25000000000004263 ) ) ;
#43000 = FACE_OUTER_BOUND ( 'NONE', #215298, .T. ) ;
#43001 = EDGE_CURVE ( 'NONE', #205178, #241214, #25077, .T. ) ;
#43003 = DIRECTION ( 'NONE',  ( 1.000000000000000000, 0.000000000000000000, 0.000000000000000000 ) ) ;
#43002 = PLANE ( 'NONE',  #83337 ) ;
#43004 = DIRECTION ( 'NONE',  ( 1.000000000000000000, 0.000000000000000000, 0.000000000000000000 ) ) ;
#43007 = ORIENTED_EDGE ( 'NONE', *, *, #45841, .T. ) ;
#43006 = EDGE_CURVE ( 'NONE', #55514, #199047, #139052, .T. ) ;
#43005 = CARTESIAN_POINT ( 'NONE',  ( 20.12518398540832010, 66.02491127934437998, -128.5264392320576405 ) ) ;
#43009 = CYLINDRICAL_SURFACE ( 'NONE', #60197, 0.09999999999999986677 ) ;
#43008 = CARTESIAN_POINT ( 'NONE',  ( 18.59999999999999787, -1.736705739456431807, -78.51742258762372728 ) ) ;
#43010 = ORIENTED_EDGE ( 'NONE', *, *, #13800, .F. ) ;
#43012 = ORIENTED_EDGE ( 'NONE', *, *, #181972, .T. ) ;
#43011 = DIRECTION ( 'NONE',  ( 0.000000000000000000, -6.467318590049456648E-15, 1.000000000000000000 ) ) ;
#43013 = ORIENTED_EDGE ( 'NONE', *, *, #91019, .T. ) ;
#43014 = CARTESIAN_POINT ( 'NONE',  ( -16.77683809663752257, 9.945835743215303282, -188.3360509808957488 ) ) ;
#43015 = CARTESIAN_POINT ( 'NONE',  ( 18.79999999999999716, 4.513204987021264714, 22.10000000000000142 ) ) ;
#43016 = DIRECTION ( 'NONE',  ( -0.000000000000000000, 6.982962677686266711E-15, -1.000000000000000000 ) ) ;
#43017 = AXIS2_PLACEMENT_3D ( 'NONE', #244375, #7054, #1904 ) ;
#43018 = ORIENTED_EDGE ( 'NONE', *, *, #121153, .F. ) ;
#43019 = CARTESIAN_POINT ( 'NONE',  ( -18.39999999999999858, 40.29670989715187090, -235.0462836312595130 ) ) ;
#43020 = CARTESIAN_POINT ( 'NONE',  ( 21.05000000000000071, 8.776282895303626930, -112.6500000000000341 ) ) ;
#43021 = CARTESIAN_POINT ( 'NONE',  ( 18.59999999999999432, -1.637172712959223952, -45.08215336547201701 ) ) ;
#43022 = EDGE_CURVE ( 'NONE', #68524, #222707, #226710, .T. ) ;
#43023 = PLANE ( 'NONE',  #132769 ) ;
#43024 = CARTESIAN_POINT ( 'NONE',  ( -20.64999999999999858, 76.00000000001179501, -82.39810748452430289 ) ) ;
#43025 = DIRECTION ( 'NONE',  ( 1.000000000000000000, -0.000000000000000000, -0.000000000000000000 ) ) ;
#43026 = EDGE_CURVE ( 'NONE', #167682, #40972, #173139, .T. ) ;
#43027 = VERTEX_POINT ( 'NONE', #236904 ) ;
#43028 = ORIENTED_EDGE ( 'NONE', *, *, #201011, .T. ) ;
#43029 = DIRECTION ( 'NONE',  ( 1.000000000000000000, -3.448943450116727019E-16, -6.438528483529604686E-16 ) ) ;
#43030 = AXIS2_PLACEMENT_3D ( 'NONE', #140850, #63877, #139543 ) ;
#43031 = CIRCLE ( 'NONE', #130494, 0.5999999999999894307 ) ;
#43032 = ORIENTED_EDGE ( 'NONE', *, *, #219311, .T. ) ;
#43033 = FACE_OUTER_BOUND ( 'NONE', #46591, .T. ) ;
#43034 = ORIENTED_EDGE ( 'NONE', *, *, #147994, .F. ) ;
#43035 = DIRECTION ( 'NONE',  ( 0.000000000000000000, -1.000000000000000000, -6.982962677686265922E-15 ) ) ;
#43036 = DIRECTION ( 'NONE',  ( 0.000000000000000000, -0.9964539953858966292, -0.08413937888696132461 ) ) ;
#43037 = CARTESIAN_POINT ( 'NONE',  ( -20.54999999999999716, 71.65000000001151648, -48.37310748452434694 ) ) ;
#43038 = EDGE_CURVE ( 'NONE', #36945, #9091, #166736, .T. ) ;
#43039 = CARTESIAN_POINT ( 'NONE',  ( 18.49999999999999645, 74.83729825007431202, -161.9231074845243654 ) ) ;
#43040 = CARTESIAN_POINT ( 'NONE',  ( 21.09551895715245706, 10.62143732718000244, -179.7371246658989037 ) ) ;
#43041 = ORIENTED_EDGE ( 'NONE', *, *, #246036, .T. ) ;
#43042 = DIRECTION ( 'NONE',  ( 0.000000000000000000, 0.8814952561688430555, -0.4721928772777346239 ) ) ;
#43044 = AXIS2_PLACEMENT_3D ( 'NONE', #121572, #237639, #19885 ) ;
#43043 = DIRECTION ( 'NONE',  ( 1.000000000000000000, 0.000000000000000000, 0.000000000000000000 ) ) ;
#43045 = CARTESIAN_POINT ( 'NONE',  ( -18.59999999999999787, 66.85000000001222986, -148.8731074845244393 ) ) ;
#43046 = VERTEX_POINT ( 'NONE', #235612 ) ;
#43048 = DIRECTION ( 'NONE',  ( -1.000000000000000000, -0.000000000000000000, -0.000000000000000000 ) ) ;
#43047 = CYLINDRICAL_SURFACE ( 'NONE', #108282, 0.09999999999999939493 ) ;
#43050 = EDGE_LOOP ( 'NONE', ( #33838, #2426, #106209, #178799 ) ) ;
#43049 = VECTOR ( 'NONE', #30863, 1000.000000000000000 ) ;
#43053 = VERTEX_POINT ( 'NONE', #135223 ) ;
#43052 = CARTESIAN_POINT ( 'NONE',  ( 23.24999999999999645, 71.00000000001186606, -90.61784146561124942 ) ) ;
#43051 = DIRECTION ( 'NONE',  ( -1.000000000000000000, -0.000000000000000000, 0.000000000000000000 ) ) ;
#43054 = ORIENTED_EDGE ( 'NONE', *, *, #73648, .F. ) ;
#43055 = CARTESIAN_POINT ( 'NONE',  ( -21.05000000000000071, 11.60000000001115517, -127.0717967697245143 ) ) ;
#43057 = DIRECTION ( 'NONE',  ( 0.000000000000000000, 0.000000000000000000, -1.000000000000000000 ) ) ;
#43056 = AXIS2_PLACEMENT_3D ( 'NONE', #211133, #16803, #131591 ) ;
#43058 = CARTESIAN_POINT ( 'NONE',  ( -20.94999999999999929, 7.120270961708750512, -70.65956304183931991 ) ) ;
#43059 = ORIENTED_EDGE ( 'NONE', *, *, #11665, .T. ) ;
#43060 = CARTESIAN_POINT ( 'NONE',  ( 19.80993210785516467, 16.75134015425318168, -222.6994291312944654 ) ) ;
#43061 = DIRECTION ( 'NONE',  ( 0.000000000000000000, 0.4721928772777330696, 0.8814952561688438326 ) ) ;
#43062 = FACE_BOUND ( 'NONE', #173109, .T. ) ;
#43064 = ORIENTED_EDGE ( 'NONE', *, *, #173494, .F. ) ;
#43063 = CARTESIAN_POINT ( 'NONE',  ( 23.14999999999999858, 7.128833340094563376, -233.7327013124401276 ) ) ;
#43065 = AXIS2_PLACEMENT_3D ( 'NONE', #101161, #2097, #256373 ) ;
#43066 = AXIS2_PLACEMENT_3D ( 'NONE', #56534, #78677, #55248 ) ;
#43067 = AXIS2_PLACEMENT_3D ( 'NONE', #115151, #113864, #117711 ) ;
#43068 = ORIENTED_EDGE ( 'NONE', *, *, #244944, .F. ) ;
#43069 = CARTESIAN_POINT ( 'NONE',  ( 21.13461538461538325, 67.11458296203740304, -90.67310748452436542 ) ) ;
#43070 = DIRECTION ( 'NONE',  ( 0.000000000000000000, -6.982962677686266711E-15, 1.000000000000000000 ) ) ;
#43071 = DIRECTION ( 'NONE',  ( 0.000000000000000000, 0.000000000000000000, -1.000000000000000000 ) ) ;
#43072 = ORIENTED_EDGE ( 'NONE', *, *, #190528, .F. ) ;
#43073 = DIRECTION ( 'NONE',  ( -1.000000000000000000, 0.000000000000000000, 0.000000000000000000 ) ) ;
#43074 = EDGE_LOOP ( 'NONE', ( #102996, #195395, #157314, #30128 ) ) ;
#43076 = AXIS2_PLACEMENT_3D ( 'NONE', #57916, #120509, #1796 ) ;
#43075 = CARTESIAN_POINT ( 'NONE',  ( 18.39999999999999147, 41.49355468354239207, -237.7178856438439141 ) ) ;
#43077 = CARTESIAN_POINT ( 'NONE',  ( -21.52071067811865746, 68.22071067813065781, -115.3731074845243540 ) ) ;
#43078 = CARTESIAN_POINT ( 'NONE',  ( 20.85000000000000142, 64.25000000001219291, -143.3069731475025321 ) ) ;
#43079 = ORIENTED_EDGE ( 'NONE', *, *, #123212, .F. ) ;
#43080 = CARTESIAN_POINT ( 'NONE',  ( -21.45000000000000284, 7.708578643773852157, -121.6500000000000341 ) ) ;
#43081 = AXIS2_PLACEMENT_3D ( 'NONE', #95227, #90073, #15726 ) ;
#43082 = CIRCLE ( 'NONE', #247060, 0.09999999999999939493 ) ;
#43083 = AXIS2_PLACEMENT_3D ( 'NONE', #56453, #134703, #96848 ) ;
#43084 = AXIS2_PLACEMENT_3D ( 'NONE', #240490, #63119, #179258 ) ;
#43085 = EDGE_CURVE ( 'NONE', #34631, #60110, #74025, .T. ) ;
#43086 = DIRECTION ( 'NONE',  ( 1.000000000000000000, 0.000000000000000000, 0.000000000000000000 ) ) ;
#43087 = ORIENTED_EDGE ( 'NONE', *, *, #140996, .T. ) ;
#43088 = ORIENTED_EDGE ( 'NONE', *, *, #37960, .F. ) ;
#43089 = VERTEX_POINT ( 'NONE', #193946 ) ;
#43090 = CARTESIAN_POINT ( 'NONE',  ( -20.54999999999999716, 1.115600667400684642E-11, -167.5000000000000284 ) ) ;
#43092 = EDGE_CURVE ( 'NONE', #146761, #133244, #16687, .T. ) ;
#43091 = ORIENTED_EDGE ( 'NONE', *, *, #87118, .T. ) ;
#43094 = ORIENTED_EDGE ( 'NONE', *, *, #103082, .F. ) ;
#43093 = CARTESIAN_POINT ( 'NONE',  ( 13.12229106158775060, 66.56936289831581632, -185.2548468664635379 ) ) ;
#43095 = EDGE_LOOP ( 'NONE', ( #14599, #3599, #107542, #27701 ) ) ;
#43096 = ADVANCED_FACE ( 'NONE', ( #19143 ), #253893, .F. ) ;
#43099 = VERTEX_POINT ( 'NONE', #158690 ) ;
#43098 = VERTEX_POINT ( 'NONE', #196488 ) ;
#43097 = CARTESIAN_POINT ( 'NONE',  ( -23.25000000000000000, 85.00000000001251976, -179.9170766071767389 ) ) ;
#43100 = CIRCLE ( 'NONE', #22265, 0.09999999999999691080 ) ;
#43101 = VECTOR ( 'NONE', #72055, 1000.000000000000000 ) ;
#43102 = EDGE_LOOP ( 'NONE', ( #33214, #176477, #201205 ) ) ;
#43103 = DIRECTION ( 'NONE',  ( 1.000000000000000000, -0.000000000000000000, -0.000000000000000000 ) ) ;
#43104 = AXIS2_PLACEMENT_3D ( 'NONE', #167135, #228365, #249212 ) ;
#43105 = CARTESIAN_POINT ( 'NONE',  ( 21.05000000000000071, 67.18479819544567988, -195.1025699878404112 ) ) ;
#43106 = CARTESIAN_POINT ( 'NONE',  ( -16.93710578446435022, 14.10179983278268523, -218.9924253766343156 ) ) ;
#43107 = ORIENTED_EDGE ( 'NONE', *, *, #194158, .F. ) ;
#43108 = AXIS2_PLACEMENT_3D ( 'NONE', #60412, #155705, #219484 ) ;
#43109 = EDGE_CURVE ( 'NONE', #186334, #180734, #153575, .T. ) ;
#43110 = DIRECTION ( 'NONE',  ( 0.000000000000000000, 0.000000000000000000, -1.000000000000000000 ) ) ;
#43111 = AXIS2_PLACEMENT_3D ( 'NONE', #225606, #144798, #27486 ) ;
#43114 = ORIENTED_EDGE ( 'NONE', *, *, #133837, .T. ) ;
#43113 = ADVANCED_FACE ( 'NONE', ( #233086 ), #91678, .F. ) ;
#43112 = FACE_OUTER_BOUND ( 'NONE', #156040, .T. ) ;
#43115 = DIRECTION ( 'NONE',  ( 0.7071067811865474617, 0.7071067811865474617, -0.000000000000000000 ) ) ;
#43117 = ORIENTED_EDGE ( 'NONE', *, *, #177579, .F. ) ;
#43116 = DIRECTION ( 'NONE',  ( 1.000000000000000000, 0.000000000000000000, 0.000000000000000000 ) ) ;
#43118 = ORIENTED_EDGE ( 'NONE', *, *, #141590, .F. ) ;
#43119 = AXIS2_PLACEMENT_3D ( 'NONE', #106739, #88444, #130158 ) ;
#43120 = EDGE_CURVE ( 'NONE', #43685, #127337, #174944, .T. ) ;
#43121 = DIRECTION ( 'NONE',  ( -0.7071067811865475727, 0.7071067811865475727, 4.937700262164531476E-15 ) ) ;
#43122 = AXIS2_PLACEMENT_3D ( 'NONE', #86389, #107264, #68147 ) ;
#43124 = ORIENTED_EDGE ( 'NONE', *, *, #64661, .T. ) ;
#43123 = AXIS2_PLACEMENT_3D ( 'NONE', #198168, #61229, #258096 ) ;
#43125 = ORIENTED_EDGE ( 'NONE', *, *, #66648, .F. ) ;
#43126 = AXIS2_PLACEMENT_3D ( 'NONE', #242635, #107942, #223075 ) ;
#43127 = CARTESIAN_POINT ( 'NONE',  ( -20.05000000000000426, 13.56015509305096778, -219.7948714774209691 ) ) ;
#43128 = CYLINDRICAL_SURFACE ( 'NONE', #11248, 0.09999999999999939493 ) ;
#43129 = AXIS2_PLACEMENT_3D ( 'NONE', #136708, #112043, #55872 ) ;
#43131 = ORIENTED_EDGE ( 'NONE', *, *, #254095, .F. ) ;
#43130 = ORIENTED_EDGE ( 'NONE', *, *, #118147, .F. ) ;
#43132 = ORIENTED_EDGE ( 'NONE', *, *, #68311, .F. ) ;
#43133 = CARTESIAN_POINT ( 'NONE',  ( -16.87683809663752399, 54.76195096157899656, -123.8731074845244393 ) ) ;
#43135 = EDGE_LOOP ( 'NONE', ( #65108, #70658, #28600, #80933 ) ) ;
#43134 = EDGE_CURVE ( 'NONE', #55107, #174088, #96096, .T. ) ;
#43136 = ORIENTED_EDGE ( 'NONE', *, *, #103639, .T. ) ;
#43137 = CARTESIAN_POINT ( 'NONE',  ( 18.47688499308726051, 85.46485595029653837, -163.3217597313869192 ) ) ;
#43139 = ORIENTED_EDGE ( 'NONE', *, *, #72524, .F. ) ;
#43138 = DIRECTION ( 'NONE',  ( 1.000000000000000000, 1.836970198721029934E-16, 3.186635328391151676E-31 ) ) ;
#43140 = DIRECTION ( 'NONE',  ( 1.734723475976817192E-14, 0.8814952561688430555, -0.4721928772777346239 ) ) ;
#43141 = AXIS2_PLACEMENT_3D ( 'NONE', #213854, #35250, #194320 ) ;
#43143 = CARTESIAN_POINT ( 'NONE',  ( 18.46082813847998949, -9.480749650896306946, -107.5843701027156811 ) ) ;
#43142 = CARTESIAN_POINT ( 'NONE',  ( -16.92132318717937522, 22.96133218596934000, -230.9078683685870317 ) ) ;
#43144 = ORIENTED_EDGE ( 'NONE', *, *, #38311, .F. ) ;
#43147 = EDGE_CURVE ( 'NONE', #248011, #50999, #45893, .T. ) ;
#43146 = ORIENTED_EDGE ( 'NONE', *, *, #170055, .F. ) ;
#43145 = ORIENTED_EDGE ( 'NONE', *, *, #47852, .T. ) ;
#43148 = LINE ( 'NONE', #240061, #194360 ) ;
#43149 = SURFACE_STYLE_USAGE ( .BOTH. , #182668 ) ;
#43150 = ORIENTED_EDGE ( 'NONE', *, *, #178085, .T. ) ;
#43151 = AXIS2_PLACEMENT_3D ( 'NONE', #201535, #97262, #60725 ) ;
#43152 = AXIS2_PLACEMENT_3D ( 'NONE', #134764, #133506, #137339 ) ;
#43153 =( GEOMETRIC_REPRESENTATION_CONTEXT ( 3 ) GLOBAL_UNCERTAINTY_ASSIGNED_CONTEXT ( ( #83108 ) ) GLOBAL_UNIT_ASSIGNED_CONTEXT ( ( #7985, #173199, #92315 ) ) REPRESENTATION_CONTEXT ( 'NONE', 'WORKASPACE' ) );
#43154 = FACE_OUTER_BOUND ( 'NONE', #234429, .T. ) ;
#43155 = EDGE_LOOP ( 'NONE', ( #81197, #225301, #216675, #213159 ) ) ;
#43156 = EDGE_LOOP ( 'NONE', ( #23325, #257247, #161749, #225030 ) ) ;
#43157 = CARTESIAN_POINT ( 'NONE',  ( -23.15000000000000213, -11.64999999998884483, -197.8999999999999773 ) ) ;
#43158 = VERTEX_POINT ( 'NONE', #116966 ) ;
#43159 = CARTESIAN_POINT ( 'NONE',  ( -18.59999999999999787, 77.16412189325360771, -162.1082593989527254 ) ) ;
#43160 = CARTESIAN_POINT ( 'NONE',  ( 22.47071067811865319, 1.115600667400684642E-11, -167.4999999999999716 ) ) ;
#43161 = ORIENTED_EDGE ( 'NONE', *, *, #152465, .F. ) ;
#43162 = DIRECTION ( 'NONE',  ( 0.000000000000000000, 0.000000000000000000, 1.000000000000000000 ) ) ;
#43164 = CARTESIAN_POINT ( 'NONE',  ( -20.54999999999999716, 68.75000000001158185, -57.27310748452437394 ) ) ;
#43163 = LINE ( 'NONE', #6588, #157158 ) ;
#43165 = FACE_BOUND ( 'NONE', #60408, .T. ) ;
#43166 = FACE_OUTER_BOUND ( 'NONE', #244326, .T. ) ;
#43167 = DIRECTION ( 'NONE',  ( 0.000000000000000000, -0.2617529984164856383, -0.9651348961777204138 ) ) ;
#43168 = CARTESIAN_POINT ( 'NONE',  ( -21.65000000000000213, 66.05000000001261640, -190.7731074845244166 ) ) ;
#43169 = DIRECTION ( 'NONE',  ( -1.000000000000000000, 0.000000000000000000, 0.000000000000000000 ) ) ;
#43171 = VERTEX_POINT ( 'NONE', #17847 ) ;
#43170 = AXIS2_PLACEMENT_3D ( 'NONE', #174226, #116772, #175487 ) ;
#43172 = AXIS2_PLACEMENT_3D ( 'NONE', #140210, #103649, #198919 ) ;
#43173 = EDGE_CURVE ( 'NONE', #246161, #78303, #176969, .T. ) ;
#43175 = VERTEX_POINT ( 'NONE', #45129 ) ;
#43174 = VERTEX_POINT ( 'NONE', #222449 ) ;
#43176 = ORIENTED_EDGE ( 'NONE', *, *, #251543, .T. ) ;
#43177 = EDGE_CURVE ( 'NONE', #229354, #72750, #37529, .T. ) ;
#43178 = CARTESIAN_POINT ( 'NONE',  ( -21.05000000000000071, -1.162701749926853712, -175.5999999999999659 ) ) ;
#43179 = CARTESIAN_POINT ( 'NONE',  ( -16.87786941232801041, 66.04184528586682745, -82.14592168473036793 ) ) ;
#43180 = EDGE_CURVE ( 'NONE', #70992, #59145, #122106, .T. ) ;
#43181 = ADVANCED_FACE ( 'NONE', ( #99936 ), #104136, .F. ) ;
#43183 = CARTESIAN_POINT ( 'NONE',  ( -13.54795643572458275, 9.450668889167525677, -15.05554649020735170 ) ) ;
#43182 = DIRECTION ( 'NONE',  ( 0.000000000000000000, 0.000000000000000000, 1.000000000000000000 ) ) ;
#43184 = CARTESIAN_POINT ( 'NONE',  ( -21.09813707148783735, 75.96864850048277162, -142.9081695902609681 ) ) ;
#43185 = EDGE_LOOP ( 'NONE', ( #256082, #191656, #99835, #63835 ) ) ;
#43186 = DIRECTION ( 'NONE',  ( 1.000000000000000000, 0.000000000000000000, 0.000000000000000000 ) ) ;
#43187 = DIRECTION ( 'NONE',  ( -1.000000000000000000, 0.000000000000000000, 0.000000000000000000 ) ) ;
#43188 = DIRECTION ( 'NONE',  ( 0.000000000000000000, -0.9651348961777157509, 0.2617529984165030132 ) ) ;
#43189 = EDGE_CURVE ( 'NONE', #215026, #34831, #77518, .T. ) ;
#43190 = DIRECTION ( 'NONE',  ( 1.000000000000000000, 0.000000000000000000, 0.000000000000000000 ) ) ;
#43191 = ORIENTED_EDGE ( 'NONE', *, *, #157121, .F. ) ;
#43192 = EDGE_CURVE ( 'NONE', #51707, #233834, #65976, .T. ) ;
#43194 = EDGE_CURVE ( 'NONE', #192087, #151216, #100021, .T. ) ;
#43193 = EDGE_CURVE ( 'NONE', #39697, #212805, #180798, .T. ) ;
#43195 = CARTESIAN_POINT ( 'NONE',  ( -23.15000000000000213, 64.25000000001173817, -81.27310748452440237 ) ) ;
#43196 = AXIS2_PLACEMENT_3D ( 'NONE', #150142, #88837, #229662 ) ;
#43197 = DIRECTION ( 'NONE',  ( 0.000000000000000000, -0.8430646840892555005, -0.5378121776619452232 ) ) ;
#43198 = ORIENTED_EDGE ( 'NONE', *, *, #242275, .F. ) ;
#43199 = DIRECTION ( 'NONE',  ( 1.000000000000000000, 0.000000000000000000, 0.000000000000000000 ) ) ;
#43200 = DIRECTION ( 'NONE',  ( 0.000000000000000000, -1.000000000000000000, 2.771150684185008344E-14 ) ) ;
#43201 = DIRECTION ( 'NONE',  ( 0.000000000000000000, -0.1350103645451876666, 0.9908441862701600211 ) ) ;
#43202 = CARTESIAN_POINT ( 'NONE',  ( -17.73285935861288110, 10.85798180379229372, -23.25856180978325938 ) ) ;
#43203 = ORIENTED_EDGE ( 'NONE', *, *, #189692, .T. ) ;
#43204 = DIRECTION ( 'NONE',  ( 1.000000000000000000, 0.000000000000000000, 0.000000000000000000 ) ) ;
#43205 = CARTESIAN_POINT ( 'NONE',  ( -20.94999999999999929, 67.65998959290219261, -227.8609496483021530 ) ) ;
#43206 = CARTESIAN_POINT ( 'NONE',  ( 21.05000000000000071, 11.84624361595474618, -206.1763227999733203 ) ) ;
#43207 = EDGE_CURVE ( 'NONE', #146298, #234584, #74362, .T. ) ;
#43209 = DIRECTION ( 'NONE',  ( 1.000000000000000000, 0.000000000000000000, 0.000000000000000000 ) ) ;
#43208 = CARTESIAN_POINT ( 'NONE',  ( -20.94999999999999929, 87.48912529308749697, -39.12310748452424747 ) ) ;
#43210 = CARTESIAN_POINT ( 'NONE',  ( -20.64999999999999858, 7.150000000011155876, -54.65000000000000568 ) ) ;
#43211 = CARTESIAN_POINT ( 'NONE',  ( 21.72449340488910607, 10.28395627750226815, -54.34999999999999432 ) ) ;
#43212 = CARTESIAN_POINT ( 'NONE',  ( -23.15000000000000213, 76.00000000001213607, -136.5231074845243313 ) ) ;
#43213 = EDGE_CURVE ( 'NONE', #183861, #83659, #208216, .T. ) ;
#43215 = EDGE_CURVE ( 'NONE', #143411, #107177, #184634, .T. ) ;
#43214 = VECTOR ( 'NONE', #231323, 1000.000000000000114 ) ;
#43216 = ORIENTED_EDGE ( 'NONE', *, *, #165366, .F. ) ;
#43217 = CIRCLE ( 'NONE', #255532, 0.09999999999998898659 ) ;
#43218 = AXIS2_PLACEMENT_3D ( 'NONE', #136457, #37403, #41265 ) ;
#43219 = ORIENTED_EDGE ( 'NONE', *, *, #209126, .T. ) ;
#43220 = ADVANCED_FACE ( 'NONE', ( #141657 ), #245803, .F. ) ;
#43221 = EDGE_CURVE ( 'NONE', #235820, #69009, #158353, .T. ) ;
#43222 = CARTESIAN_POINT ( 'NONE',  ( 22.42357213249528769, 7.672932386371071445, -100.4009130359984709 ) ) ;
#43224 = CARTESIAN_POINT ( 'NONE',  ( -18.53317502108577486, 65.67736539654895012, -30.46251168765719797 ) ) ;
#43223 = AXIS2_PLACEMENT_3D ( 'NONE', #22820, #7075, #24105 ) ;
#43225 = CARTESIAN_POINT ( 'NONE',  ( 14.77516762759920788, 9.436674251854004325, -149.1768619309991948 ) ) ;
#43226 = ORIENTED_EDGE ( 'NONE', *, *, #18866, .F. ) ;
#43227 = TOROIDAL_SURFACE ( 'NONE', #188974, 11.90000000000000213, 0.1000000000000000056 ) ;
#43228 = CARTESIAN_POINT ( 'NONE',  ( -23.15000000000000213, 1.115600667400684642E-11, -100.5000000000000426 ) ) ;
#43229 = CIRCLE ( 'NONE', #155685, 0.09999999999999939493 ) ;
#43230 = CARTESIAN_POINT ( 'NONE',  ( 20.95512820512820440, 65.37615131629968346, -57.37310748452439668 ) ) ;
#43231 = CARTESIAN_POINT ( 'NONE',  ( -18.59999999999999787, 67.85909929089923764, -227.8797997985275856 ) ) ;
#43232 = CIRCLE ( 'NONE', #39155, 0.09999999999999630018 ) ;
#43233 = ORIENTED_EDGE ( 'NONE', *, *, #222469, .T. ) ;
#43234 = DIRECTION ( 'NONE',  ( 0.000000000000000000, 1.000000000000000000, 0.000000000000000000 ) ) ;
#43236 = ORIENTED_EDGE ( 'NONE', *, *, #231159, .T. ) ;
#43235 = DIRECTION ( 'NONE',  ( -0.7071067811865456854, 0.7071067811865493491, 0.000000000000000000 ) ) ;
#43238 = DIRECTION ( 'NONE',  ( -0.000000000000000000, -0.000000000000000000, -1.000000000000000000 ) ) ;
#43237 = CARTESIAN_POINT ( 'NONE',  ( 20.94999999999999574, -1.835341550213255957, -78.55515129256302487 ) ) ;
#43239 = CARTESIAN_POINT ( 'NONE',  ( -18.59999999999999787, 0.000000000000000000, -33.50000000000000000 ) ) ;
#43240 = ORIENTED_EDGE ( 'NONE', *, *, #32420, .T. ) ;
#43241 = CIRCLE ( 'NONE', #251517, 12.87499999999999822 ) ;
#43242 =( LENGTH_UNIT ( ) NAMED_UNIT ( * ) SI_UNIT ( .MILLI., .METRE. ) );
#43244 = DIRECTION ( 'NONE',  ( 1.000000000000000000, 0.000000000000000000, 0.000000000000000000 ) ) ;
#43243 = AXIS2_PLACEMENT_3D ( 'NONE', #121082, #78057, #38957 ) ;
#43246 = CIRCLE ( 'NONE', #134970, 7.800000000000001599 ) ;
#43245 = FACE_OUTER_BOUND ( 'NONE', #152835, .T. ) ;
#43247 = ORIENTED_EDGE ( 'NONE', *, *, #150937, .F. ) ;
#43248 = DIRECTION ( 'NONE',  ( 0.000000000000000000, 0.4721928772777343464, 0.8814952561688431665 ) ) ;
#43249 = CARTESIAN_POINT ( 'NONE',  ( 18.49999999999999289, 55.06386612490207000, -230.0864074704206246 ) ) ;
#43250 = AXIS2_PLACEMENT_3D ( 'NONE', #138291, #62642, #22242 ) ;
#43251 = PLANE ( 'NONE',  #228326 ) ;
#43252 = CARTESIAN_POINT ( 'NONE',  ( 22.39999999999999858, 1.115600667400684642E-11, -167.4999999999999716 ) ) ;
#43253 = VERTEX_POINT ( 'NONE', #107662 ) ;
#43254 = ORIENTED_EDGE ( 'NONE', *, *, #41119, .T. ) ;
#43255 = VECTOR ( 'NONE', #245110, 1000.000000000000000 ) ;
#43256 = CARTESIAN_POINT ( 'NONE',  ( -23.25000000000000000, -8.999999999988844479, -124.1060308773475924 ) ) ;
#43257 = VECTOR ( 'NONE', #157877, 1000.000000000000114 ) ;
#43258 = VECTOR ( 'NONE', #61223, 1000.000000000000000 ) ;
#43259 = DIRECTION ( 'NONE',  ( -0.000000000000000000, 1.000000000000000000, 6.982962677686266711E-15 ) ) ;
#43260 = DIRECTION ( 'NONE',  ( -1.000000000000000000, 0.000000000000000000, 0.000000000000000000 ) ) ;
#43261 = EDGE_CURVE ( 'NONE', #83237, #173524, #224932, .T. ) ;
#43262 = DIRECTION ( 'NONE',  ( 1.000000000000000000, 0.000000000000000000, 0.000000000000000000 ) ) ;
#43263 = CARTESIAN_POINT ( 'NONE',  ( 18.69999999999999929, 1.350000000000000089, 16.39999999999999858 ) ) ;
#43265 = SURFACE_STYLE_USAGE ( .BOTH. , #144906 ) ;
#43264 = DIRECTION ( 'NONE',  ( 0.000000000000000000, -1.953992523340280244E-14, -1.000000000000000000 ) ) ;
#43266 = FACE_OUTER_BOUND ( 'NONE', #29968, .T. ) ;
#43267 = EDGE_CURVE ( 'NONE', #8263, #156110, #200017, .T. ) ;
#43268 = DIRECTION ( 'NONE',  ( 0.000000000000000000, 0.9126074666063768159, 0.4088369013363282178 ) ) ;
#43269 = CARTESIAN_POINT ( 'NONE',  ( 22.40000000000020819, 76.10085836911189006, -148.2726746080140003 ) ) ;
#43270 = VERTEX_POINT ( 'NONE', #146763 ) ;
#43271 = DIRECTION ( 'NONE',  ( -0.000000000000000000, 0.1350103645451876666, 0.9908441862701600211 ) ) ;
#43273 = ORIENTED_EDGE ( 'NONE', *, *, #237204, .T. ) ;
#43272 = FACE_OUTER_BOUND ( 'NONE', #34742, .T. ) ;
#43274 = FACE_OUTER_BOUND ( 'NONE', #209702, .T. ) ;
#43275 = DIRECTION ( 'NONE',  ( 0.000000000000000000, 0.000000000000000000, 1.000000000000000000 ) ) ;
#43277 = CYLINDRICAL_SURFACE ( 'NONE', #136716, 0.1000000000000028644 ) ;
#43276 = CARTESIAN_POINT ( 'NONE',  ( 21.00023020733502577, 76.00000000001200817, -109.4139767297926653 ) ) ;
#43278 = ADVANCED_FACE ( 'NONE', ( #185920 ), #189773, .F. ) ;
#43279 = EDGE_CURVE ( 'NONE', #215160, #172274, #90021, .T. ) ;
#43280 = EDGE_LOOP ( 'NONE', ( #5261, #162991, #164040, #222219 ) ) ;
#43282 = CARTESIAN_POINT ( 'NONE',  ( 20.94999999999999929, 67.92720994251783395, -214.1870976236629929 ) ) ;
#43281 = LINE ( 'NONE', #122829, #155864 ) ;
#43283 = LINE ( 'NONE', #67971, #149841 ) ;
#43284 = PLANE ( 'NONE',  #22140 ) ;
#43285 = DIRECTION ( 'NONE',  ( 1.000000000000000000, -0.000000000000000000, -0.000000000000000000 ) ) ;
#43286 = CARTESIAN_POINT ( 'NONE',  ( -23.25000000000000000, 76.00000000001237765, -170.0231074845243597 ) ) ;
#43287 = ORIENTED_EDGE ( 'NONE', *, *, #19168, .T. ) ;
#43288 = ORIENTED_EDGE ( 'NONE', *, *, #105078, .T. ) ;
#43289 = AXIS2_PLACEMENT_3D ( 'NONE', #109035, #88167, #86891 ) ;
#43290 = CIRCLE ( 'NONE', #147324, 4.049999999999994493 ) ;
#43291 = DIRECTION ( 'NONE',  ( 0.000000000000000000, -1.000000000000000000, 0.000000000000000000 ) ) ;
#43292 = VERTEX_POINT ( 'NONE', #149390 ) ;
#43293 = DIRECTION ( 'NONE',  ( 0.000000000000000000, 6.982962677686267499E-15, -1.000000000000000000 ) ) ;
#43294 = AXIS2_PLACEMENT_3D ( 'NONE', #199520, #20892, #179947 ) ;
#43295 = VERTEX_POINT ( 'NONE', #230178 ) ;
#43296 = EDGE_CURVE ( 'NONE', #182032, #129536, #105193, .T. ) ;
#43297 = LINE ( 'NONE', #65416, #130991 ) ;
#43298 = EDGE_CURVE ( 'NONE', #83188, #238889, #233177, .T. ) ;
#43299 = VECTOR ( 'NONE', #34039, 1000.000000000000000 ) ;
#43300 = CIRCLE ( 'NONE', #222309, 0.09999999999999062417 ) ;
#43301 = CARTESIAN_POINT ( 'NONE',  ( -21.65000000000000213, 7.708578643773852157, -179.7499999999999716 ) ) ;
#43302 = ORIENTED_EDGE ( 'NONE', *, *, #62490, .T. ) ;
#43303 =( BOUNDED_SURFACE ( )  B_SPLINE_SURFACE ( 3, 2, ( 
 ( #154896, #31105, #194008 ),
 ( #50608, #15372, #130154 ),
 ( #10231, #174484, #234386 ),
 ( #135278, #89739, #37498 ) ),
 .UNSPECIFIED., .F., .F., .F. ) 
 B_SPLINE_SURFACE_WITH_KNOTS ( ( 4, 4 ),
 ( 3, 3 ),
 ( 0.000000000000000000, 1.570796326794896558 ),
 ( 0.000000000000000000, 1.000000000000000000 ),
 .UNSPECIFIED. ) 
 GEOMETRIC_REPRESENTATION_ITEM ( )  RATIONAL_B_SPLINE_SURFACE ( (
 ( 1.000000000000000000, 0.6447402616205117898, 1.000000000000000000),
 ( 1.000000000000000000, 0.6438648806865400198, 1.000000000000000000),
 ( 1.000000000000000000, 0.6753870962079631113, 1.000000000000000000),
 ( 1.000000000000000000, 0.7071067811865505703, 1.000000000000000000) ) ) 
 REPRESENTATION_ITEM ( '' )  SURFACE ( )  );
#43304 = VECTOR ( 'NONE', #222516, 1000.000000000000000 ) ;
#43305 = CARTESIAN_POINT ( 'NONE',  ( -23.15000000000000213, 11.75000000001116263, -112.6500000000000341 ) ) ;
#43306 = CARTESIAN_POINT ( 'NONE',  ( -21.15000000000000213, 65.51923798433685420, -242.1677427744926092 ) ) ;
#43308 = CIRCLE ( 'NONE', #201497, 0.5999999999999894307 ) ;
#43307 = CARTESIAN_POINT ( 'NONE',  ( 20.85000000000000142, 7.070967871809997973, -137.7465642218683399 ) ) ;
#43310 = CIRCLE ( 'NONE', #193162, 4.049999999999998046 ) ;
#43309 = DIRECTION ( 'NONE',  ( 0.000000000000000000, 0.000000000000000000, -1.000000000000000000 ) ) ;
#43311 = ADVANCED_FACE ( 'NONE', ( #226306 ), #120747, .T. ) ;
#43312 = DIRECTION ( 'NONE',  ( 1.000000000000000000, 0.000000000000000000, -0.000000000000000000 ) ) ;
#43313 = CARTESIAN_POINT ( 'NONE',  ( 19.96984138294339317, 62.36267039717171201, -208.9169814761061730 ) ) ;
#43315 = ORIENTED_EDGE ( 'NONE', *, *, #197340, .T. ) ;
#43314 = EDGE_CURVE ( 'NONE', #149860, #146093, #129104, .T. ) ;
#43316 = DIRECTION ( 'NONE',  ( 0.000000000000000000, 1.000000000000000000, 0.000000000000000000 ) ) ;
#43317 = EDGE_LOOP ( 'NONE', ( #242473, #74468, #85881, #27864 ) ) ;
#43319 = ORIENTED_EDGE ( 'NONE', *, *, #36759, .T. ) ;
#43318 = SPHERICAL_SURFACE ( 'NONE', #98095, 0.1000000000000000056 ) ;
#43320 = VECTOR ( 'NONE', #53337, 1000.000000000000000 ) ;
#43321 = ORIENTED_EDGE ( 'NONE', *, *, #211440, .T. ) ;
#43322 = LINE ( 'NONE', #117709, #165597 ) ;
#43323 = LINE ( 'NONE', #122865, #242571 ) ;
#43324 =( BOUNDED_SURFACE ( )  B_SPLINE_SURFACE ( 3, 2, ( 
 ( #165173, #226402, #49069 ),
 ( #107761, #244693, #66065 ),
 ( #7375, #205562, #162618 ),
 ( #23119, #86893, #169066 ),
 ( #71229, #209425, #231576 ),
 ( #15097, #131173, #72509 ) ),
 .UNSPECIFIED., .F., .F., .F. ) 
 B_SPLINE_SURFACE_WITH_KNOTS ( ( 4, 2, 4 ),
 ( 3, 3 ),
 ( 0.0001381104793128029801, 0.0002947094729387742841, 0.0004513084665647455881 ),
 ( 0.000000000000000000, 1.000000000000000000 ),
 .UNSPECIFIED. ) 
 GEOMETRIC_REPRESENTATION_ITEM ( )  RATIONAL_B_SPLINE_SURFACE ( (
 ( 1.000000000000000000, 0.7071067811865601183, 1.000000000000000000),
 ( 1.000000000000000000, 0.6919563088096917225, 1.000000000000000000),
 ( 1.000000000000000000, 0.6959445945720270643, 1.000000000000000000),
 ( 1.000000000000000000, 0.7137882985309929040, 1.000000000000000000),
 ( 1.000000000000000000, 0.7257496306099716632, 1.000000000000000000),
 ( 1.000000000000000000, 0.7250110520819658122, 1.000000000000000000) ) ) 
 REPRESENTATION_ITEM ( '' )  SURFACE ( )  );
#43325 = DIRECTION ( 'NONE',  ( 1.000000000000000000, 0.000000000000000000, 0.000000000000000000 ) ) ;
#43326 = FACE_OUTER_BOUND ( 'NONE', #120707, .T. ) ;
#43327 = ORIENTED_EDGE ( 'NONE', *, *, #254991, .T. ) ;
#43328 = DIRECTION ( 'NONE',  ( 0.000000000000000000, -0.8660254037844411501, -0.4999999999999956146 ) ) ;
#43329 = AXIS2_PLACEMENT_3D ( 'NONE', #233440, #136880, #134295 ) ;
#43330 = ADVANCED_FACE ( 'NONE', ( #188484 ), #11141, .T. ) ;
#43331 = EDGE_LOOP ( 'NONE', ( #179017, #50843, #238934, #157987 ) ) ;
#43332 = EDGE_CURVE ( 'NONE', #120417, #56583, #229058, .T. ) ;
#43333 = CARTESIAN_POINT ( 'NONE',  ( 18.49999999999998579, -9.321008403350155902, -174.7359382490778046 ) ) ;
#43334 = VECTOR ( 'NONE', #44078, 1000.000000000000000 ) ;
#43335 = CARTESIAN_POINT ( 'NONE',  ( 21.05000000000000071, 76.00000000001170974, -69.52310748452431710 ) ) ;
#43336 = EDGE_CURVE ( 'NONE', #177661, #105159, #116620, .T. ) ;
#43337 = ORIENTED_EDGE ( 'NONE', *, *, #88053, .T. ) ;
#43338 = CARTESIAN_POINT ( 'NONE',  ( -18.59999999999999787, 64.35000000001234355, -163.0083017138704236 ) ) ;
#43339 = AXIS2_PLACEMENT_3D ( 'NONE', #204754, #163096, #175291 ) ;
#43340 =( BOUNDED_CURVE ( )  B_SPLINE_CURVE ( 3, ( #58768, #222992, #92, #24837 ),
 .UNSPECIFIED., .F., .F. ) 
 B_SPLINE_CURVE_WITH_KNOTS ( ( 4, 4 ),
 ( 0.000000000000000000, 1.570796326794896558 ),
 .UNSPECIFIED. ) 
 CURVE ( )  GEOMETRIC_REPRESENTATION_ITEM ( )  RATIONAL_B_SPLINE_CURVE ( ( 1.000000000000000000, 0.8047378541243649375, 0.8047378541243649375, 1.000000000000000000 ) ) 
 REPRESENTATION_ITEM ( '' )  );
#43341 = AXIS2_PLACEMENT_3D ( 'NONE', #8130, #107214, #135758 ) ;
#43342 = AXIS2_PLACEMENT_3D ( 'NONE', #197520, #35915, #236648 ) ;
#43343 = FACE_OUTER_BOUND ( 'NONE', #162496, .T. ) ;
#43344 = ORIENTED_EDGE ( 'NONE', *, *, #186719, .F. ) ;
#43345 = DIRECTION ( 'NONE',  ( 4.239556034732056743E-17, -0.1298341882520022694, -0.9915357197604852679 ) ) ;
#43346 = CARTESIAN_POINT ( 'NONE',  ( -23.15000000000000213, 1.115600667400684642E-11, -200.9999999999999432 ) ) ;
#43347 = DIRECTION ( 'NONE',  ( 0.000000000000000000, -1.000000000000000000, 0.000000000000000000 ) ) ;
#43348 = EDGE_CURVE ( 'NONE', #204472, #103006, #91951, .T. ) ;
#43349 = DIRECTION ( 'NONE',  ( 1.000000000000000000, -0.000000000000000000, -0.000000000000000000 ) ) ;
#43350 = EDGE_CURVE ( 'NONE', #127135, #53973, #107330, .T. ) ;
#43351 = AXIS2_PLACEMENT_3D ( 'NONE', #132191, #56483, #34402 ) ;
#43352 = CARTESIAN_POINT ( 'NONE',  ( 21.13736287352038445, 8.046642376395153562, -46.15000000000000568 ) ) ;
#43353 = DIRECTION ( 'NONE',  ( 1.000000000000000000, 0.000000000000000000, 0.000000000000000000 ) ) ;
#43354 = VECTOR ( 'NONE', #128658, 1000.000000000000000 ) ;
#43355 = CIRCLE ( 'NONE', #189101, 2.000000000000001776 ) ;
#43356 = CARTESIAN_POINT ( 'NONE',  ( 20.92356734117541706, 10.31973158071402175, -72.55053347133544150 ) ) ;
#43357 = VERTEX_POINT ( 'NONE', #151957 ) ;
#43359 = DIRECTION ( 'NONE',  ( 0.000000000000000000, 0.000000000000000000, -1.000000000000000000 ) ) ;
#43358 = FACE_OUTER_BOUND ( 'NONE', #149158, .T. ) ;
#43360 = ORIENTED_EDGE ( 'NONE', *, *, #211617, .T. ) ;
#43361 = DIRECTION ( 'NONE',  ( 0.000000000000000000, -1.000000000000000000, -6.982962677686265922E-15 ) ) ;
#43363 = EDGE_CURVE ( 'NONE', #64408, #111618, #104309, .T. ) ;
#43362 = DIRECTION ( 'NONE',  ( 0.000000000000000000, 6.982962677686267499E-15, -1.000000000000000000 ) ) ;
#43364 = ORIENTED_EDGE ( 'NONE', *, *, #66429, .T. ) ;
#43366 = ORIENTED_EDGE ( 'NONE', *, *, #71773, .T. ) ;
#43365 = LINE ( 'NONE', #169763, #170436 ) ;
#43367 = PRESENTATION_STYLE_ASSIGNMENT (( #143733 ) ) ;
#43368 = CARTESIAN_POINT ( 'NONE',  ( 23.40000000000005187, 79.78873604695631627, -7.297728304630792806 ) ) ;
#43369 = CARTESIAN_POINT ( 'NONE',  ( 18.59999999999999787, -8.150000000000007461, -15.00000000000000000 ) ) ;
#43370 = DIRECTION ( 'NONE',  ( 0.000000000000000000, 7.109473446599835262E-15, -1.000000000000000000 ) ) ;
#43372 = ORIENTED_EDGE ( 'NONE', *, *, #60513, .F. ) ;
#43371 = CARTESIAN_POINT ( 'NONE',  ( 21.12400222705963415, 67.22148809293508975, -157.7731074845244166 ) ) ;
#43373 = CARTESIAN_POINT ( 'NONE',  ( -21.65000000000000213, 68.75000000001182343, -82.17310748452436542 ) ) ;
#43374 = VERTEX_POINT ( 'NONE', #148084 ) ;
#43375 = ORIENTED_EDGE ( 'NONE', *, *, #61310, .F. ) ;
#43376 = CARTESIAN_POINT ( 'NONE',  ( -21.14999999999999503, 11.75000000001115019, -107.4191472459587828 ) ) ;
#43377 = PLANE ( 'NONE',  #1667 ) ;
#43378 = ORIENTED_EDGE ( 'NONE', *, *, #43396, .T. ) ;
#43379 = DIRECTION ( 'NONE',  ( 0.000000000000000000, -1.000000000000000000, 0.000000000000000000 ) ) ;
#43380 = DIRECTION ( 'NONE',  ( 0.000000000000000000, 0.000000000000000000, -1.000000000000000000 ) ) ;
#43381 = EDGE_LOOP ( 'NONE', ( #136192, #130700, #206779, #184489 ) ) ;
#43382 = DIRECTION ( 'NONE',  ( 0.000000000000000000, -1.000000000000000000, 0.000000000000000000 ) ) ;
#43383 = AXIS2_PLACEMENT_3D ( 'NONE', #128628, #208175, #129887 ) ;
#43384 = CIRCLE ( 'NONE', #59933, 0.09999999999999939493 ) ;
#43385 = DIRECTION ( 'NONE',  ( -1.000000000000000000, 0.000000000000000000, 0.000000000000000000 ) ) ;
#43386 = ORIENTED_EDGE ( 'NONE', *, *, #4631, .F. ) ;
#43387 = ORIENTED_EDGE ( 'NONE', *, *, #133304, .T. ) ;
#43388 = DIRECTION ( 'NONE',  ( -1.000000000000000000, -3.190570557967288949E-16, -6.948722487160392945E-17 ) ) ;
#43389 = EDGE_LOOP ( 'NONE', ( #171308, #148804 ) ) ;
#43390 = FACE_OUTER_BOUND ( 'NONE', #156948, .T. ) ;
#43392 = EDGE_CURVE ( 'NONE', #99184, #257935, #75138, .T. ) ;
#43391 = VERTEX_POINT ( 'NONE', #128520 ) ;
#43393 = ORIENTED_EDGE ( 'NONE', *, *, #99886, .F. ) ;
#43394 = DIRECTION ( 'NONE',  ( 1.000000000000000000, 0.000000000000000000, 0.000000000000000000 ) ) ;
#43395 = ORIENTED_EDGE ( 'NONE', *, *, #13559, .T. ) ;
#43396 = EDGE_CURVE ( 'NONE', #202583, #195513, #98326, .T. ) ;
#43397 = CARTESIAN_POINT ( 'NONE',  ( 22.45463910399148233, 1.026727559903827464E-11, -88.85042918981690718 ) ) ;
#43398 = EDGE_CURVE ( 'NONE', #59451, #105943, #125191, .T. ) ;
#43399 = ORIENTED_EDGE ( 'NONE', *, *, #148646, .T. ) ;
#43401 = ORIENTED_EDGE ( 'NONE', *, *, #184762, .T. ) ;
#43400 = ORIENTED_EDGE ( 'NONE', *, *, #231034, .F. ) ;
#43403 = LINE ( 'NONE', #239035, #148623 ) ;
#43402 = CIRCLE ( 'NONE', #26859, 0.09999999999998898659 ) ;
#43404 = CARTESIAN_POINT ( 'NONE',  ( -20.96428641294048489, 56.19879751616013408, -227.9223442982746803 ) ) ;
#43405 = VERTEX_POINT ( 'NONE', #136179 ) ;
#43406 = VECTOR ( 'NONE', #4727, 1000.000000000000114 ) ;
#43407 = AXIS2_PLACEMENT_3D ( 'NONE', #38555, #59357, #214609 ) ;
#43408 = CIRCLE ( 'NONE', #176702, 0.09999999999998898659 ) ;
#43409 = CIRCLE ( 'NONE', #126796, 0.09999999999999691080 ) ;
#43410 = VERTEX_POINT ( 'NONE', #234026 ) ;
#43411 = ADVANCED_FACE ( 'NONE', ( #253583 ), #17535, .F. ) ;
#43412 = CARTESIAN_POINT ( 'NONE',  ( 21.05000000000000071, 43.47002849391839874, -245.0086825852825143 ) ) ;
#43413 = DIRECTION ( 'NONE',  ( 1.000000000000000000, 0.000000000000000000, 0.000000000000000000 ) ) ;
#43415 = ORIENTED_EDGE ( 'NONE', *, *, #15899, .T. ) ;
#43414 = FACE_OUTER_BOUND ( 'NONE', #174579, .T. ) ;
#43416 = DIRECTION ( 'NONE',  ( 0.000000000000000000, -0.9999631594459053030, -0.008583690987162452199 ) ) ;
#43417 = ORIENTED_EDGE ( 'NONE', *, *, #49468, .F. ) ;
#43418 = CARTESIAN_POINT ( 'NONE',  ( -18.50211644919735932, 65.69792220476342948, -131.0335554128461979 ) ) ;
#43419 = CARTESIAN_POINT ( 'NONE',  ( -20.64999999999999858, 1.115600667400684642E-11, -102.4000000000000483 ) ) ;
#43420 = AXIS2_PLACEMENT_3D ( 'NONE', #183032, #245571, #83868 ) ;
#43421 = VERTEX_POINT ( 'NONE', #174109 ) ;
#43422 = TOROIDAL_SURFACE ( 'NONE', #189175, 7.800000000000000711, 0.1000000000000000056 ) ;
#43423 = DIRECTION ( 'NONE',  ( 0.000000000000000000, 0.6728388485993177515, -0.7397890806274072251 ) ) ;
#43424 = CARTESIAN_POINT ( 'NONE',  ( -23.25000000000000000, 23.40438595358395091, -253.3416554127419431 ) ) ;
#43425 = CIRCLE ( 'NONE', #168560, 0.1000000000000124678 ) ;
#43426 = ORIENTED_EDGE ( 'NONE', *, *, #18824, .F. ) ;
#43427 = CARTESIAN_POINT ( 'NONE',  ( -5.899999999999938183, 64.35000000001120668, -26.02310748452479316 ) ) ;
#43428 = EDGE_LOOP ( 'NONE', ( #228091, #230722, #29002, #206940, #25820 ) ) ;
#43429 = AXIS2_PLACEMENT_3D ( 'NONE', #44659, #240294, #124205 ) ;
#43432 = VERTEX_POINT ( 'NONE', #177927 ) ;
#43431 = ORIENTED_EDGE ( 'NONE', *, *, #102538, .T. ) ;
#43430 = AXIS2_PLACEMENT_3D ( 'NONE', #253757, #136356, #38581 ) ;
#43433 = ORIENTED_EDGE ( 'NONE', *, *, #130619, .T. ) ;
#43434 = DIRECTION ( 'NONE',  ( 1.000000000000000000, 0.000000000000000000, 0.000000000000000000 ) ) ;
#43435 = EDGE_CURVE ( 'NONE', #50174, #177630, #154536, .T. ) ;
#43436 = VERTEX_POINT ( 'NONE', #211921 ) ;
#43437 = EDGE_CURVE ( 'NONE', #16270, #28626, #29364, .T. ) ;
#43438 = CARTESIAN_POINT ( 'NONE',  ( -16.95709691156382348, 66.05000000001152216, -48.68316504703488334 ) ) ;
#43439 = ORIENTED_EDGE ( 'NONE', *, *, #1658, .F. ) ;
#43440 = DIRECTION ( 'NONE',  ( 0.000000000000000000, -0.9651348961777379554, 0.2617529984164210233 ) ) ;
#43441 = AXIS2_PLACEMENT_3D ( 'NONE', #80552, #160151, #100119 ) ;
#43442 = CIRCLE ( 'NONE', #143394, 0.2000000000000048683 ) ;
#43443 = DIRECTION ( 'NONE',  ( -0.5932847527679299127, 0.8049926720990051576, 6.366092712777055223E-16 ) ) ;
#43444 = AXIS2_PLACEMENT_3D ( 'NONE', #231875, #92335, #94893 ) ;
#43445 = VERTEX_POINT ( 'NONE', #153252 ) ;
#43447 = ADVANCED_FACE ( 'NONE', ( #217020 ), #18830, .T. ) ;
#43446 = ORIENTED_EDGE ( 'NONE', *, *, #109130, .T. ) ;
#43448 = ORIENTED_EDGE ( 'NONE', *, *, #209876, .F. ) ;
#43449 = CARTESIAN_POINT ( 'NONE',  ( -22.60000000000080789, 0.04781698047652397504, -155.7499775688472710 ) ) ;
#43450 = EDGE_LOOP ( 'NONE', ( #90150, #160060, #5104, #219725 ) ) ;
#43451 = PLANE ( 'NONE',  #16820 ) ;
#43452 = CARTESIAN_POINT ( 'NONE',  ( 21.14999999999999858, 87.75000000001229239, -157.7731074845242745 ) ) ;
#43453 = CARTESIAN_POINT ( 'NONE',  ( -21.05000000000000071, -11.29603075032412463, -130.9521008403361861 ) ) ;
#43454 = CARTESIAN_POINT ( 'NONE',  ( 21.05000000000000071, 65.51540711881798984, -162.5663939139407432 ) ) ;
#43455 = DIRECTION ( 'NONE',  ( 1.000000000000000000, 0.000000000000000000, 0.000000000000000000 ) ) ;
#43457 = EDGE_CURVE ( 'NONE', #170630, #251948, #241704, .T. ) ;
#43456 = DIRECTION ( 'NONE',  ( 0.000000000000000000, -0.8700118002898354908, 0.4930308989875170078 ) ) ;
#43458 = AXIS2_PLACEMENT_3D ( 'NONE', #77178, #177606, #257055 ) ;
#43460 = DIRECTION ( 'NONE',  ( 0.000000000000000000, 0.000000000000000000, 1.000000000000000000 ) ) ;
#43459 = DIRECTION ( 'NONE',  ( 0.000000000000000000, 8.881784197000778021E-16, -1.000000000000000000 ) ) ;
#43461 = DIRECTION ( 'NONE',  ( 0.000000000000000000, 0.000000000000000000, -1.000000000000000000 ) ) ;
#43462 = FACE_OUTER_BOUND ( 'NONE', #128236, .T. ) ;
#43463 = AXIS2_PLACEMENT_3D ( 'NONE', #217806, #40522, #1331 ) ;
#43464 = CARTESIAN_POINT ( 'NONE',  ( -22.39999999999999858, 7.040683814476209612, -233.6854820247115185 ) ) ;
#43466 = FACE_OUTER_BOUND ( 'NONE', #174926, .T. ) ;
#43465 = AXIS2_PLACEMENT_3D ( 'NONE', #105168, #51629, #86913 ) ;
#43467 = VERTEX_POINT ( 'NONE', #54104 ) ;
#43468 = AXIS2_PLACEMENT_3D ( 'NONE', #129003, #149859, #48162 ) ;
#43469 = B_SPLINE_CURVE_WITH_KNOTS ( 'NONE', 3,
 ( #124316, #63038, #128169, #123034, #25229, #66900, #26510, #65612, #164726, #205107 ),
 .UNSPECIFIED., .F., .F.,
 ( 4, 2, 2, 2, 4 ),
 ( 0.000000000000000000, 0.0003916577441626797819, 0.0005874866162440189410, 0.0006854010522846886019, 0.0007833154883253581544 ),
 .UNSPECIFIED. ) ;
#43470 = EDGE_CURVE ( 'NONE', #256377, #84395, #151915, .T. ) ;
#43471 = VECTOR ( 'NONE', #119524, 1000.000000000000000 ) ;
#43473 = VERTEX_POINT ( 'NONE', #236584 ) ;
#43472 = DIRECTION ( 'NONE',  ( 0.000000000000000000, 0.000000000000000000, 1.000000000000000000 ) ) ;
#43474 = EDGE_LOOP ( 'NONE', ( #196981, #31332 ) ) ;
#43475 = DIRECTION ( 'NONE',  ( 1.000000000000000000, -0.000000000000000000, -0.000000000000000000 ) ) ;
#43476 = CARTESIAN_POINT ( 'NONE',  ( 20.74897398619109268, 10.59569302167756888, -141.6793114562569542 ) ) ;
#43477 = AXIS2_PLACEMENT_3D ( 'NONE', #205220, #206525, #27922 ) ;
#43478 = ADVANCED_FACE ( 'NONE', ( #34570 ), #114074, .T. ) ;
#43479 = B_SPLINE_CURVE_WITH_KNOTS ( 'NONE', 3,
 ( #213786, #97663, #132985, #254179, #54709, #153870, #232089, #75589, #114687, #53431, #39017, #194255, #95124, #252906, #195537, #14334, #233381, #93834, #237210 ),
 .UNSPECIFIED., .F., .F.,
 ( 4, 3, 3, 3, 3, 3, 4 ),
 ( -2.000416914662652606E-06, 0.000000000000000000, 4.714008503744773841E-05, 9.979203887777149504E-05, 0.0001372215519229469133, 0.0001635031576220970250, 0.0001900083748504064938 ),
 .UNSPECIFIED. ) ;
#43480 = EDGE_CURVE ( 'NONE', #178121, #22846, #250092, .T. ) ;
#43481 = DIRECTION ( 'NONE',  ( 1.472176885922364728E-15, -0.9868171638914230437, 0.1618390714546045217 ) ) ;
#43482 = ORIENTED_EDGE ( 'NONE', *, *, #125220, .T. ) ;
#43483 = AXIS2_PLACEMENT_3D ( 'NONE', #24251, #107612, #103732 ) ;
#43484 = AXIS2_PLACEMENT_3D ( 'NONE', #79180, #3499, #219989 ) ;
#43485 = AXIS2_PLACEMENT_3D ( 'NONE', #206730, #249717, #247128 ) ;
#43486 = PRODUCT_DEFINITION_SHAPE ( 'NONE', 'NONE',  #258111 ) ;
#43487 = CARTESIAN_POINT ( 'NONE',  ( 20.94999999999999929, 1.115650877919449575E-11, -163.4000000000000341 ) ) ;
#43488 = ORIENTED_EDGE ( 'NONE', *, *, #242454, .F. ) ;
#43489 = EDGE_CURVE ( 'NONE', #209005, #112762, #129286, .T. ) ;
#43490 = CARTESIAN_POINT ( 'NONE',  ( 20.85000000000000142, 69.06610602788578035, -132.7374616501508342 ) ) ;
#43491 = DIRECTION ( 'NONE',  ( 1.000000000000000000, 0.000000000000000000, 0.000000000000000000 ) ) ;
#43492 = ADVANCED_FACE ( 'NONE', ( #16299 ), #137479, .T. ) ;
#43493 = CYLINDRICAL_SURFACE ( 'NONE', #172141, 0.1000000000000007827 ) ;
#43494 = DIRECTION ( 'NONE',  ( 0.000000000000000000, -6.982962677686266711E-15, 1.000000000000000000 ) ) ;
#43496 = VERTEX_POINT ( 'NONE', #175375 ) ;
#43495 = CARTESIAN_POINT ( 'NONE',  ( 21.05000000000000071, 16.50669723772569952, -240.7258389668962479 ) ) ;
#43498 = ADVANCED_FACE ( 'NONE', ( #196191 ), #176649, .T. ) ;
#43497 = CIRCLE ( 'NONE', #222534, 0.09999999999999817368 ) ;
#43499 = CARTESIAN_POINT ( 'NONE',  ( -18.59999999999999787, 64.35000000001174669, -81.27310748452440237 ) ) ;
#43501 = ORIENTED_EDGE ( 'NONE', *, *, #134438, .T. ) ;
#43500 = CARTESIAN_POINT ( 'NONE',  ( 21.05000000000000071, 4.813084112160684214, -189.0584822434761634 ) ) ;
#43502 = SPHERICAL_SURFACE ( 'NONE', #154172, 0.1000000000000000056 ) ;
#43503 = CARTESIAN_POINT ( 'NONE',  ( -20.54999999999999716, 4.349999999999999645, -21.25000000000000000 ) ) ;
#43504 = CARTESIAN_POINT ( 'NONE',  ( -16.93583594267724379, 65.99137656496009186, -157.4637166452036752 ) ) ;
#43505 = CARTESIAN_POINT ( 'NONE',  ( -23.25000000000000000, 71.85000000001178933, -81.77310748452433131 ) ) ;
#43506 = AXIS2_PLACEMENT_3D ( 'NONE', #202835, #224950, #124599 ) ;
#43507 = EDGE_CURVE ( 'NONE', #144682, #167762, #138740, .T. ) ;
#43509 = PLANE ( 'NONE',  #41156 ) ;
#43508 = CARTESIAN_POINT ( 'NONE',  ( -16.87036670365548474, 66.01058118071014746, -82.04354736722233099 ) ) ;
#43510 = FACE_OUTER_BOUND ( 'NONE', #6338, .T. ) ;
#43511 = CARTESIAN_POINT ( 'NONE',  ( 20.95289811251229750, 40.78188399555352817, -237.9593377293462027 ) ) ;
#43512 = CARTESIAN_POINT ( 'NONE',  ( -18.50000000000000000, 10.29288807858820398, -38.95800201601218049 ) ) ;
#43513 = DIRECTION ( 'NONE',  ( -0.000000000000000000, 0.000000000000000000, -1.000000000000000000 ) ) ;
#43514 = DIRECTION ( 'NONE',  ( 0.000000000000000000, 0.9579639084728133192, 0.2868887416116073785 ) ) ;
#43515 = EDGE_CURVE ( 'NONE', #185781, #253858, #20135, .T. ) ;
#43516 = EDGE_CURVE ( 'NONE', #113714, #22952, #12786, .T. ) ;
#43517 = TOROIDAL_SURFACE ( 'NONE', #14501, 0.2000000000000000111, 0.1000000000000000056 ) ;
#43519 = ORIENTED_EDGE ( 'NONE', *, *, #107150, .T. ) ;
#43518 = CIRCLE ( 'NONE', #160245, 0.09999999999999939493 ) ;
#43520 = CARTESIAN_POINT ( 'NONE',  ( 21.14999999999999858, 1.115600667400684642E-11, -26.95934304829875927 ) ) ;
#43521 = CIRCLE ( 'NONE', #247527, 4.000000000000000000 ) ;
#43522 = ORIENTED_EDGE ( 'NONE', *, *, #44656, .F. ) ;
#43523 = ORIENTED_EDGE ( 'NONE', *, *, #27419, .T. ) ;
#43524 = EDGE_CURVE ( 'NONE', #59101, #38092, #195935, .T. ) ;
#43525 = CARTESIAN_POINT ( 'NONE',  ( -21.05000000000000071, 11.74999999999999645, -26.65839931010294706 ) ) ;
#43526 = DIRECTION ( 'NONE',  ( -0.000000000000000000, 0.1350103645451859180, 0.9908441862701603542 ) ) ;
#43527 = EDGE_LOOP ( 'NONE', ( #81345, #161335, #29279 ) ) ;
#43528 = EDGE_CURVE ( 'NONE', #177002, #97776, #83456, .T. ) ;
#43529 = EDGE_CURVE ( 'NONE', #239691, #121353, #100892, .T. ) ;
#43530 = ORIENTED_EDGE ( 'NONE', *, *, #143591, .T. ) ;
#43531 =( LENGTH_UNIT ( ) NAMED_UNIT ( * ) SI_UNIT ( .MILLI., .METRE. ) );
#43532 = ADVANCED_FACE ( 'NONE', ( #180486 ), #21434, .T. ) ;
#43533 = ORIENTED_EDGE ( 'NONE', *, *, #175827, .F. ) ;
#43534 = PLANE ( 'NONE',  #125237 ) ;
#43535 = TOROIDAL_SURFACE ( 'NONE', #151719, 11.65000000000000036, 0.1000000000000000056 ) ;
#43536 = ORIENTED_EDGE ( 'NONE', *, *, #122993, .T. ) ;
#43537 = DIRECTION ( 'NONE',  ( 0.000000000000000000, 0.000000000000000000, -1.000000000000000000 ) ) ;
#43538 = LINE ( 'NONE', #195586, #215937 ) ;
#43539 = CYLINDRICAL_SURFACE ( 'NONE', #30308, 0.09999999999999543976 ) ;
#43540 = CARTESIAN_POINT ( 'NONE',  ( -16.87372397896795917, 29.73344917972452350, -234.6324668538658500 ) ) ;
#43541 = PLANE ( 'NONE',  #156888 ) ;
#43542 = AXIS2_PLACEMENT_3D ( 'NONE', #91030, #53184, #130144 ) ;
#43543 = FACE_OUTER_BOUND ( 'NONE', #151226, .T. ) ;
#43544 = DIRECTION ( 'NONE',  ( -1.000000000000000000, -0.000000000000000000, -0.000000000000000000 ) ) ;
#43546 = ORIENTED_EDGE ( 'NONE', *, *, #97325, .F. ) ;
#43545 = CARTESIAN_POINT ( 'NONE',  ( -23.15000000000000213, 11.65000000001115588, -126.9851942293460922 ) ) ;
#43548 = CARTESIAN_POINT ( 'NONE',  ( -23.25000000000000000, -4.892732937820631456, -233.2805462221312496 ) ) ;
#43547 = LINE ( 'NONE', #21433, #167148 ) ;
#43549 = EDGE_CURVE ( 'NONE', #81112, #39027, #71038, .T. ) ;
#43550 = PLANE ( 'NONE',  #198972 ) ;
#43551 = VERTEX_POINT ( 'NONE', #60510 ) ;
#43552 = CARTESIAN_POINT ( 'NONE',  ( -23.15000000000000213, 2.000000000011154189, -87.27537807723794572 ) ) ;
#43553 = LINE ( 'NONE', #24002, #125084 ) ;
#43554 = ORIENTED_EDGE ( 'NONE', *, *, #21238, .T. ) ;
#43556 = DIRECTION ( 'NONE',  ( 0.000000000000000000, 0.000000000000000000, -1.000000000000000000 ) ) ;
#43555 = FACE_OUTER_BOUND ( 'NONE', #212090, .T. ) ;
#43557 = DIRECTION ( 'NONE',  ( 0.000000000000000000, 6.982962677686266711E-15, -1.000000000000000000 ) ) ;
#43558 = VERTEX_POINT ( 'NONE', #158385 ) ;
#43559 = PRESENTATION_STYLE_ASSIGNMENT (( #85204 ) ) ;
#43560 = DIRECTION ( 'NONE',  ( -0.000000000000000000, 0.8660254037844383745, -0.5000000000000003331 ) ) ;
#43561 = CARTESIAN_POINT ( 'NONE',  ( -25.10847955711009760, 9.068702471349583405, 33.00000000000000000 ) ) ;
#43562 = ORIENTED_EDGE ( 'NONE', *, *, #178859, .T. ) ;
#43563 = DIRECTION ( 'NONE',  ( 0.000000000000000000, -0.3488585713686133682, -0.9371753822965315228 ) ) ;
#43564 = DIRECTION ( 'NONE',  ( 1.000000000000000000, 0.000000000000000000, 0.000000000000000000 ) ) ;
#43565 = EDGE_CURVE ( 'NONE', #4874, #221355, #37726, .T. ) ;
#43566 = DIRECTION ( 'NONE',  ( -0.000000000000000000, 6.982962677686266711E-15, -1.000000000000000000 ) ) ;
#43567 = DIRECTION ( 'NONE',  ( 0.000000000000000000, 0.000000000000000000, 1.000000000000000000 ) ) ;
#43568 = AXIS2_PLACEMENT_3D ( 'NONE', #240962, #62325, #141846 ) ;
#43569 = DIRECTION ( 'NONE',  ( 7.304098846218134667E-16, 1.000000000000000000, 6.982962677686267499E-15 ) ) ;
#43570 = EDGE_CURVE ( 'NONE', #36642, #108264, #58523, .T. ) ;
#43571 = VECTOR ( 'NONE', #236082, 1000.000000000000000 ) ;
#43572 = FACE_OUTER_BOUND ( 'NONE', #59838, .T. ) ;
#43573 = AXIS2_PLACEMENT_3D ( 'NONE', #20228, #61915, #218393 ) ;
#43575 = ORIENTED_EDGE ( 'NONE', *, *, #51067, .T. ) ;
#43574 = FACE_OUTER_BOUND ( 'NONE', #113045, .T. ) ;
#43576 = CARTESIAN_POINT ( 'NONE',  ( -23.25000000000000000, 79.15532900748003442, -196.2806010913881778 ) ) ;
#43577 = FACE_OUTER_BOUND ( 'NONE', #64575, .T. ) ;
#43578 = DIRECTION ( 'NONE',  ( -6.938893903907222856E-15, 1.000000000000000000, 0.000000000000000000 ) ) ;
#43580 = DIRECTION ( 'NONE',  ( 0.000000000000000000, 0.1568667991644863147, -0.9876197685951252359 ) ) ;
#43579 = MECHANICAL_DESIGN_GEOMETRIC_PRESENTATION_REPRESENTATION (  '', ( #185229 ), #214821 ) ;
#43581 = PLANE ( 'NONE',  #171459 ) ;
#43583 = ORIENTED_EDGE ( 'NONE', *, *, #120066, .F. ) ;
#43582 = DIRECTION ( 'NONE',  ( 0.000000000000000000, 0.8660254037844378194, 0.5000000000000016653 ) ) ;
#43584 = DIRECTION ( 'NONE',  ( 2.710505431213777355E-16, 0.9651348961777157509, -0.2617529984165031243 ) ) ;
#43585 = FACE_OUTER_BOUND ( 'NONE', #237500, .T. ) ;
#43586 = DIRECTION ( 'NONE',  ( 0.000000000000000000, 0.4721928772776973204, 0.8814952561688629284 ) ) ;
#43587 = EDGE_LOOP ( 'NONE', ( #192226, #211990, #32521, #25484, #208304 ) ) ;
#43588 = CARTESIAN_POINT ( 'NONE',  ( -14.11361717019514472, 66.54257354752336084, -151.5230656161243985 ) ) ;
#43589 = CARTESIAN_POINT ( 'NONE',  ( -18.50000000000000000, 64.35000000001157616, -57.37310748452440379 ) ) ;
#43590 = LINE ( 'NONE', #143958, #21199 ) ;
#43591 = AXIS2_PLACEMENT_3D ( 'NONE', #2604, #242507, #125146 ) ;
#43592 = CONTEXT_DEPENDENT_SHAPE_REPRESENTATION ( #72569, #16239 ) ;
#43593 = EDGE_CURVE ( 'NONE', #189189, #209120, #4396, .T. ) ;
#43594 = CARTESIAN_POINT ( 'NONE',  ( -18.50000000000000355, 78.21362219944487038, -231.2727646510690533 ) ) ;
#43595 = VECTOR ( 'NONE', #110496, 1000.000000000000000 ) ;
#43596 = EDGE_LOOP ( 'NONE', ( #10978, #127204, #147980, #209517, #248039 ) ) ;
#43597 = CARTESIAN_POINT ( 'NONE',  ( -16.88705144915409306, 9.950000000011138823, -87.56902140528751488 ) ) ;
#43598 = VERTEX_POINT ( 'NONE', #159638 ) ;
#43599 = VECTOR ( 'NONE', #47577, 1000.000000000000000 ) ;
#43600 = CARTESIAN_POINT ( 'NONE',  ( 21.07094088545368038, -1.248309276978959437, -194.8035479807908530 ) ) ;
#43602 = LINE ( 'NONE', #181824, #78939 ) ;
#43601 = VECTOR ( 'NONE', #152365, 1000.000000000000000 ) ;
#43603 = CARTESIAN_POINT ( 'NONE',  ( 18.60000000000000142, -9.321008403350125704, -174.7359382490778614 ) ) ;
#43604 = EDGE_LOOP ( 'NONE', ( #256595, #194482, #225425, #109662 ) ) ;
#43605 = CARTESIAN_POINT ( 'NONE',  ( 20.95325940946048249, 10.52339007070744614, -175.0644621292400416 ) ) ;
#43606 = AXIS2_PLACEMENT_3D ( 'NONE', #253992, #153684, #75401 ) ;
#43607 = VECTOR ( 'NONE', #127663, 1000.000000000000000 ) ;
#43608 = DIRECTION ( 'NONE',  ( 0.000000000000000000, -7.487053152578127080E-15, 1.000000000000000000 ) ) ;
#43609 = CIRCLE ( 'NONE', #197708, 11.75000000000001066 ) ;
#43610 = LINE ( 'NONE', #126994, #8305 ) ;
#43611 = CARTESIAN_POINT ( 'NONE',  ( 14.88075390448863722, 9.431689550524096077, -18.27929003223605875 ) ) ;
#43612 = CIRCLE ( 'NONE', #210221, 0.5999999999999998668 ) ;
#43613 = CARTESIAN_POINT ( 'NONE',  ( -16.88783316861815109, 9.949999999999983302, -20.74773595802023962 ) ) ;
#43614 = CARTESIAN_POINT ( 'NONE',  ( -23.25000000000000000, 1.910280373842930812, -154.8686321448010972 ) ) ;
#43615 = ORIENTED_EDGE ( 'NONE', *, *, #245377, .F. ) ;
#43617 = ORIENTED_EDGE ( 'NONE', *, *, #181619, .F. ) ;
#43616 = CARTESIAN_POINT ( 'NONE',  ( 18.49999999999999289, 69.15387683765879956, -32.28538121767450519 ) ) ;
#43618 = TOROIDAL_SURFACE ( 'NONE', #51969, 0.2000000000000000111, 0.1000000000000000056 ) ;
#43619 = ORIENTED_EDGE ( 'NONE', *, *, #45885, .T. ) ;
#43620 = DIRECTION ( 'NONE',  ( -0.7071067811865474617, 0.7071067811865474617, 4.937700262164531476E-15 ) ) ;
#43621 = ORIENTED_EDGE ( 'NONE', *, *, #6965, .F. ) ;
#43622 = DIRECTION ( 'NONE',  ( 0.000000000000000000, 0.000000000000000000, 1.000000000000000000 ) ) ;
#43623 = DIRECTION ( 'NONE',  ( 1.000000000000000000, 0.000000000000000000, 0.000000000000000000 ) ) ;
#43624 = CARTESIAN_POINT ( 'NONE',  ( -23.25000000000000000, -11.64999999998884483, -164.4000000000000057 ) ) ;
#43625 = ORIENTED_EDGE ( 'NONE', *, *, #93239, .T. ) ;
#43627 = VECTOR ( 'NONE', #64863, 1000.000000000000000 ) ;
#43626 = DIRECTION ( 'NONE',  ( 1.000000000000000000, 0.000000000000000000, 0.000000000000000000 ) ) ;
#43628 = DIRECTION ( 'NONE',  ( -0.000000000000000000, 0.000000000000000000, -1.000000000000000000 ) ) ;
#43629 = CIRCLE ( 'NONE', #85286, 0.1000000000000028644 ) ;
#43630 = EDGE_CURVE ( 'NONE', #146658, #16741, #179363, .T. ) ;
#43631 = ORIENTED_EDGE ( 'NONE', *, *, #119104, .T. ) ;
#43632 = CARTESIAN_POINT ( 'NONE',  ( -16.86733706339143524, 9.965990529650820662, -54.40311530199869594 ) ) ;
#43634 = VERTEX_POINT ( 'NONE', #42261 ) ;
#43633 = CYLINDRICAL_SURFACE ( 'NONE', #142382, 12.87499999999999822 ) ;
#43636 = EDGE_CURVE ( 'NONE', #91949, #6351, #98721, .T. ) ;
#43635 = CARTESIAN_POINT ( 'NONE',  ( -20.64999999999999858, 26.34635675162282098, -241.8429480539297174 ) ) ;
#43637 = SPHERICAL_SURFACE ( 'NONE', #147932, 0.1000000000000000056 ) ;
#43638 = VERTEX_POINT ( 'NONE', #162227 ) ;
#43639 = FACE_OUTER_BOUND ( 'NONE', #257634, .T. ) ;
#43641 = ADVANCED_FACE ( 'NONE', ( #222141 ), #269, .T. ) ;
#43640 = CARTESIAN_POINT ( 'NONE',  ( -18.59999999999999787, -9.399999999988787991, -141.2972597596633193 ) ) ;
#43642 = CARTESIAN_POINT ( 'NONE',  ( -21.65000000000000213, 9.950000000011138823, -146.7500000000000284 ) ) ;
#43643 = VERTEX_POINT ( 'NONE', #243009 ) ;
#43644 = CARTESIAN_POINT ( 'NONE',  ( 20.95000000000005258, 64.35000000001119247, -5.923107484524795296 ) ) ;
#43645 = EDGE_CURVE ( 'NONE', #209971, #56894, #171030, .T. ) ;
#43646 = DIRECTION ( 'NONE',  ( -0.000000000000000000, 0.1298341882520022694, 0.9915357197604853789 ) ) ;
#43647 = EDGE_CURVE ( 'NONE', #74878, #242431, #66916, .T. ) ;
#43648 = AXIS2_PLACEMENT_3D ( 'NONE', #59651, #135355, #94948 ) ;
#43649 = ORIENTED_EDGE ( 'NONE', *, *, #224337, .T. ) ;
#43650 = AXIS2_PLACEMENT_3D ( 'NONE', #63568, #143099, #146946 ) ;
#43651 = ADVANCED_FACE ( 'NONE', ( #125639 ), #91859, .F. ) ;
#43652 = AXIS2_PLACEMENT_3D ( 'NONE', #13534, #213004, #250834 ) ;
#43653 = ORIENTED_EDGE ( 'NONE', *, *, #200155, .T. ) ;
#43654 = TOROIDAL_SURFACE ( 'NONE', #151823, 0.2000000000000000111, 0.1000000000000000056 ) ;
#43655 = CIRCLE ( 'NONE', #172885, 0.09999999999999939493 ) ;
#43656 = VERTEX_POINT ( 'NONE', #147784 ) ;
#43657 = DIRECTION ( 'NONE',  ( 0.000000000000000000, 0.000000000000000000, -1.000000000000000000 ) ) ;
#43659 = EDGE_CURVE ( 'NONE', #64123, #230182, #30409, .T. ) ;
#43658 = DIRECTION ( 'NONE',  ( 0.000000000000000000, 0.1298341882519953583, 0.9915357197604862671 ) ) ;
#43661 = ORIENTED_EDGE ( 'NONE', *, *, #134171, .T. ) ;
#43660 = CARTESIAN_POINT ( 'NONE',  ( -16.81930730667006912, 9.936998068885202429, -146.7267677305382279 ) ) ;
#43662 = FACE_OUTER_BOUND ( 'NONE', #166540, .T. ) ;
#43663 = DIRECTION ( 'NONE',  ( 1.020425574104004196E-15, 1.210927747993693964E-31, -1.000000000000000000 ) ) ;
#43664 = FACE_OUTER_BOUND ( 'NONE', #256558, .T. ) ;
#43665 = FACE_OUTER_BOUND ( 'NONE', #102483, .T. ) ;
#43666 = CARTESIAN_POINT ( 'NONE',  ( -18.42554971533677133, 85.49715966944982881, -129.4832805709755803 ) ) ;
#43667 = CIRCLE ( 'NONE', #227004, 0.9000000000000014655 ) ;
#43668 = DIRECTION ( 'NONE',  ( 0.000000000000000000, 0.9126074666063781482, 0.4088369013363253313 ) ) ;
#43669 = CIRCLE ( 'NONE', #88862, 0.09999999999999344136 ) ;
#43671 = ORIENTED_EDGE ( 'NONE', *, *, #141263, .T. ) ;
#43670 = DIRECTION ( 'NONE',  ( -2.578261006436899437E-14, -0.1350103645451973811, 0.9908441862701586889 ) ) ;
#43672 = ORIENTED_EDGE ( 'NONE', *, *, #245097, .F. ) ;
#43673 = CARTESIAN_POINT ( 'NONE',  ( 22.39999999999999503, -0.1008583690875579364, -55.25043287651065782 ) ) ;
#43674 = CIRCLE ( 'NONE', #135416, 0.09999999999999939493 ) ;
#43675 = ORIENTED_EDGE ( 'NONE', *, *, #190528, .T. ) ;
#43676 = CARTESIAN_POINT ( 'NONE',  ( 21.13461538461538325, 65.38541703798632909, -90.67310748452437963 ) ) ;
#43677 = AXIS2_PLACEMENT_3D ( 'NONE', #110685, #190232, #171988 ) ;
#43678 = DIRECTION ( 'NONE',  ( 1.000000000000000000, -0.000000000000000000, -0.000000000000000000 ) ) ;
#43679 = FACE_OUTER_BOUND ( 'NONE', #166664, .T. ) ;
#43680 = DIRECTION ( 'NONE',  ( 1.000000000000000000, -0.000000000000000000, -0.000000000000000000 ) ) ;
#43681 = CIRCLE ( 'NONE', #189433, 0.9000000000000014655 ) ;
#43682 = CARTESIAN_POINT ( 'NONE',  ( 20.53930447208010790, 67.02285131248760308, -195.0806003429519535 ) ) ;
#43683 = VERTEX_POINT ( 'NONE', #210328 ) ;
#43684 = CYLINDRICAL_SURFACE ( 'NONE', #14803, 0.1000000000000013933 ) ;
#43685 = VERTEX_POINT ( 'NONE', #205156 ) ;
#43686 = PRESENTATION_STYLE_ASSIGNMENT (( #668 ) ) ;
#43687 = ORIENTED_EDGE ( 'NONE', *, *, #124429, .T. ) ;
#43688 = AXIS2_PLACEMENT_3D ( 'NONE', #65905, #163728, #204116 ) ;
#43690 = ADVANCED_FACE ( 'NONE', ( #89069 ), #69539, .T. ) ;
#43689 = CARTESIAN_POINT ( 'NONE',  ( 21.07016717457009847, 76.00000000001243450, -176.3440483226252411 ) ) ;
#43691 = AXIS2_PLACEMENT_3D ( 'NONE', #66711, #50963, #126677 ) ;
#43692 = DIRECTION ( 'NONE',  ( 1.000000000000000000, -0.000000000000000000, -0.000000000000000000 ) ) ;
#43693 = ORIENTED_EDGE ( 'NONE', *, *, #243235, .F. ) ;
#43694 = CARTESIAN_POINT ( 'NONE',  ( 23.14999999999999858, 67.23127455305841238, -235.8551265064783991 ) ) ;
#43695 = ORIENTED_EDGE ( 'NONE', *, *, #182156, .T. ) ;
#43697 = ADVANCED_FACE ( 'NONE', ( #169953 ), #26559, .T. ) ;
#43696 = DIRECTION ( 'NONE',  ( -0.000000000000000000, -0.9910827722268042983, 0.1332476588733650935 ) ) ;
#43698 = ORIENTED_EDGE ( 'NONE', *, *, #148768, .T. ) ;
#43699 = DIRECTION ( 'NONE',  ( -0.7071067811864846231, -0.2890913453341779626, 0.6453109281989296564 ) ) ;
#43700 = ADVANCED_FACE ( 'NONE', ( #109916 ), #180457, .F. ) ;
#43701 = DIRECTION ( 'NONE',  ( 0.000000000000000000, 0.9770955615653316162, 0.2128009952263597848 ) ) ;
#43702 = EDGE_CURVE ( 'NONE', #213681, #149981, #225109, .T. ) ;
#43703 = VERTEX_POINT ( 'NONE', #164773 ) ;
#43704 = CARTESIAN_POINT ( 'NONE',  ( 23.15000000000000213, 78.50726470275242264, -228.6618886302502176 ) ) ;
#43706 = VERTEX_POINT ( 'NONE', #206462 ) ;
#43705 = CARTESIAN_POINT ( 'NONE',  ( -22.47071067811865319, 7.720074744509219933, -100.4009075452974287 ) ) ;
#43707 = CARTESIAN_POINT ( 'NONE',  ( -22.50875500270927532, 76.10085791378739373, -215.2726746119222696 ) ) ;
#43708 = AXIS2_PLACEMENT_3D ( 'NONE', #217276, #116920, #39980 ) ;
#43709 = VERTEX_POINT ( 'NONE', #244290 ) ;
#43710 = AXIS2_PLACEMENT_3D ( 'NONE', #256807, #157816, #52227 ) ;
#43711 = EDGE_LOOP ( 'NONE', ( #194823, #36812, #179584, #125060 ) ) ;
#43712 = ADVANCED_FACE ( 'NONE', ( #128216 ), #41820, .F. ) ;
#43713 = CARTESIAN_POINT ( 'NONE',  ( 21.05000000000000071, -8.730841121484166578, -191.4019252810156217 ) ) ;
#43714 = LINE ( 'NONE', #41176, #132303 ) ;
#43715 = CYLINDRICAL_SURFACE ( 'NONE', #147872, 0.09999999999999939493 ) ;
#43716 = EDGE_CURVE ( 'NONE', #124908, #98885, #225987, .T. ) ;
#43717 = DIRECTION ( 'NONE',  ( 1.000000000000000000, 0.000000000000000000, 0.000000000000000000 ) ) ;
#43718 = DIRECTION ( 'NONE',  ( 1.000000000000000000, -0.000000000000000000, 0.000000000000000000 ) ) ;
#43719 = EDGE_LOOP ( 'NONE', ( #39971, #203583, #194083, #196701 ) ) ;
#43720 = CARTESIAN_POINT ( 'NONE',  ( 20.90000000000000213, 6.726092018229619995, 9.512212474619552438 ) ) ;
#43721 = CARTESIAN_POINT ( 'NONE',  ( -21.05000000000000071, 13.63177590472475487, -238.5351604075707144 ) ) ;
#43723 = DIRECTION ( 'NONE',  ( -0.000000000000000000, -0.000000000000000000, 1.000000000000000000 ) ) ;
#43722 = PRODUCT_RELATED_PRODUCT_CATEGORY ( 'part', '', ( #14100 ) ) ;
#43724 = FACE_OUTER_BOUND ( 'NONE', #246430, .T. ) ;
#43725 = ORIENTED_EDGE ( 'NONE', *, *, #39946, .T. ) ;
#43726 = CARTESIAN_POINT ( 'NONE',  ( -21.05000000000000071, 75.90220970870321082, -109.2809220950004203 ) ) ;
#43727 = EDGE_LOOP ( 'NONE', ( #179125, #122680, #218202, #132660 ) ) ;
#43728 = DIRECTION ( 'NONE',  ( 0.000000000000000000, -2.255140518769784599E-13, 1.000000000000000000 ) ) ;
#43729 = VERTEX_POINT ( 'NONE', #209032 ) ;
#43730 = CIRCLE ( 'NONE', #156188, 0.1000000000000028644 ) ;
#43731 = CARTESIAN_POINT ( 'NONE',  ( -21.14999999999994174, 77.16254490893143725, -43.92310748452479885 ) ) ;
#43732 = CARTESIAN_POINT ( 'NONE',  ( -17.27223548799954145, 65.65460260868350417, -181.3895013053292473 ) ) ;
#43733 = EDGE_CURVE ( 'NONE', #54640, #138432, #87748, .T. ) ;
#43734 = ORIENTED_EDGE ( 'NONE', *, *, #112123, .T. ) ;
#43736 = EDGE_LOOP ( 'NONE', ( #240023, #71699, #155675, #123802 ) ) ;
#43735 = DIRECTION ( 'NONE',  ( 0.000000000000000000, 0.000000000000000000, 1.000000000000000000 ) ) ;
#43737 = EDGE_CURVE ( 'NONE', #138262, #194835, #108438, .T. ) ;
#43738 = CARTESIAN_POINT ( 'NONE',  ( -20.65000000000000568, 70.35000000001187459, -90.37310748452433984 ) ) ;
#43739 = ORIENTED_EDGE ( 'NONE', *, *, #172205, .T. ) ;
#43740 = EDGE_CURVE ( 'NONE', #184576, #93118, #33014, .T. ) ;
#43741 = LINE ( 'NONE', #185815, #231251 ) ;
#43742 = DIRECTION ( 'NONE',  ( 0.000000000000000000, 0.000000000000000000, -1.000000000000000000 ) ) ;
#43743 = ORIENTED_EDGE ( 'NONE', *, *, #152411, .F. ) ;
#43744 = ORIENTED_EDGE ( 'NONE', *, *, #68585, .F. ) ;
#43745 = FACE_OUTER_BOUND ( 'NONE', #232720, .T. ) ;
#43746 = LINE ( 'NONE', #186805, #223429 ) ;
#43747 = CARTESIAN_POINT ( 'NONE',  ( -23.15000000000000213, 76.00000000001169553, -67.42310748452430857 ) ) ;
#43748 = VECTOR ( 'NONE', #79240, 1000.000000000000000 ) ;
#43749 = ORIENTED_EDGE ( 'NONE', *, *, #229863, .F. ) ;
#43750 = ORIENTED_EDGE ( 'NONE', *, *, #108712, .F. ) ;
#43751 = AXIS2_PLACEMENT_3D ( 'NONE', #213180, #189781, #115368 ) ;
#43752 = CIRCLE ( 'NONE', #48031, 0.09999999999999939493 ) ;
#43753 = DIRECTION ( 'NONE',  ( 0.000000000000000000, -6.982962677686267499E-15, 1.000000000000000000 ) ) ;
#43754 = STYLED_ITEM ( 'NONE', ( #108588 ), #200717 ) ;
#43756 = ORIENTED_EDGE ( 'NONE', *, *, #67311, .F. ) ;
#43755 = CARTESIAN_POINT ( 'NONE',  ( -16.81930730667006557, 9.936998068885202429, -46.22676773053819943 ) ) ;
#43757 = CARTESIAN_POINT ( 'NONE',  ( -23.25000000000000000, 77.73670573947921980, -58.00568489690056850 ) ) ;
#43758 = DIRECTION ( 'NONE',  ( 0.000000000000000000, 0.000000000000000000, 1.000000000000000000 ) ) ;
#43760 = EDGE_CURVE ( 'NONE', #217847, #211242, #137819, .T. ) ;
#43759 = CARTESIAN_POINT ( 'NONE',  ( 23.14999999999999858, 75.49601185175264106, -250.2710592679604531 ) ) ;
#43762 = CARTESIAN_POINT ( 'NONE',  ( -20.00857864376270001, 30.18746141061095045, -235.4776000216846796 ) ) ;
#43761 = DIRECTION ( 'NONE',  ( 0.7071067811865127117, 0.7071067811865821007, 0.000000000000000000 ) ) ;
#43763 = CARTESIAN_POINT ( 'NONE',  ( 21.04999999999963478, 10.54375127550701485, -108.0563878086650789 ) ) ;
#43764 = CARTESIAN_POINT ( 'NONE',  ( -23.15000000000000213, 2.000000000011154189, -53.77537807723790309 ) ) ;
#43765 = DIRECTION ( 'NONE',  ( 1.000000000000000000, 2.952720810173289112E-16, -0.000000000000000000 ) ) ;
#43766 = DIRECTION ( 'NONE',  ( 0.000000000000000000, -0.2617529984165031243, -0.9651348961777157509 ) ) ;
#43767 = VECTOR ( 'NONE', #106554, 1000.000000000000000 ) ;
#43768 = ORIENTED_EDGE ( 'NONE', *, *, #41676, .F. ) ;
#43769 = AXIS2_PLACEMENT_3D ( 'NONE', #252860, #175929, #157666 ) ;
#43770 = CIRCLE ( 'NONE', #160511, 11.65000000000000746 ) ;
#43771 = VERTEX_POINT ( 'NONE', #132061 ) ;
#43772 = EDGE_CURVE ( 'NONE', #219574, #249430, #37908, .T. ) ;
#43773 = CARTESIAN_POINT ( 'NONE',  ( -18.39999999999999858, -9.599999999988849453, -73.60018939122203108 ) ) ;
#43774 = ORIENTED_EDGE ( 'NONE', *, *, #2924, .F. ) ;
#43775 = DIRECTION ( 'NONE',  ( 0.000000000000000000, 1.897661533703519897E-16, -1.000000000000000000 ) ) ;
#43776 = AXIS2_PLACEMENT_3D ( 'NONE', #201106, #22498, #101976 ) ;
#43777 = ADVANCED_FACE ( 'NONE', ( #14713 ), #212888, .F. ) ;
#43778 = VECTOR ( 'NONE', #100701, 1000.000000000000000 ) ;
#43779 = AXIS2_PLACEMENT_3D ( 'NONE', #50146, #69741, #55260 ) ;
#43780 = ORIENTED_EDGE ( 'NONE', *, *, #225846, .F. ) ;
#43781 =( NAMED_UNIT ( * ) SI_UNIT ( $, .STERADIAN. ) SOLID_ANGLE_UNIT ( ) );
#43783 = ADVANCED_FACE ( 'NONE', ( #113773 ), #41997, .F. ) ;
#43782 = CARTESIAN_POINT ( 'NONE',  ( -21.05000000000000071, 69.74168394268035343, -170.0888090948464537 ) ) ;
#43784 = B_SPLINE_CURVE_WITH_KNOTS ( 'NONE', 3,
 ( #187658, #148516, #247605, #68996, #183786, #164233, #228050 ),
 .UNSPECIFIED., .F., .F.,
 ( 4, 3, 4 ),
 ( 0.000000000000000000, 4.520325912680430423E-05, 5.794988040901218388E-05 ),
 .UNSPECIFIED. ) ;
#43785 = ORIENTED_EDGE ( 'NONE', *, *, #242760, .T. ) ;
#43786 = CARTESIAN_POINT ( 'NONE',  ( -21.12230431290520016, 6.308551053831973121, -199.6207328664785052 ) ) ;
#43787 = ORIENTED_EDGE ( 'NONE', *, *, #72661, .T. ) ;
#43788 = EDGE_LOOP ( 'NONE', ( #118677, #243564, #11003 ) ) ;
#43789 = EDGE_CURVE ( 'NONE', #78058, #58451, #192057, .T. ) ;
#43791 = FACE_OUTER_BOUND ( 'NONE', #57093, .T. ) ;
#43790 = AXIS2_PLACEMENT_3D ( 'NONE', #62977, #81233, #1706 ) ;
#43792 = CARTESIAN_POINT ( 'NONE',  ( -21.09813707148783379, 75.96864850048257267, -109.4081695902609965 ) ) ;
#43795 = EDGE_CURVE ( 'NONE', #176943, #174581, #104485, .T. ) ;
#43794 = ORIENTED_EDGE ( 'NONE', *, *, #143561, .T. ) ;
#43793 = DIRECTION ( 'NONE',  ( -0.000000000000000000, -0.9126074666063771490, -0.4088369013363281623 ) ) ;
#43796 = CIRCLE ( 'NONE', #189562, 11.70000000000000462 ) ;
#43797 = CARTESIAN_POINT ( 'NONE',  ( -22.94999999999999929, 8.000000000000000000, 1.212568896937007867 ) ) ;
#43799 = ORIENTED_EDGE ( 'NONE', *, *, #190341, .T. ) ;
#43798 = DIRECTION ( 'NONE',  ( 1.000000000000000000, 0.000000000000000000, 0.000000000000000000 ) ) ;
#43800 = CARTESIAN_POINT ( 'NONE',  ( -21.07928932188134041, 0.09889514566555068775, -60.67148334360675221 ) ) ;
#43801 = VERTEX_POINT ( 'NONE', #75944 ) ;
#43802 = CIRCLE ( 'NONE', #168764, 0.09999999999998898659 ) ;
#43803 = DIRECTION ( 'NONE',  ( 1.000000000000000000, -0.000000000000000000, -0.000000000000000000 ) ) ;
#43805 = EDGE_LOOP ( 'NONE', ( #6550, #250061, #131199 ) ) ;
#43804 = DIRECTION ( 'NONE',  ( 0.000000000000000000, 1.000000000000000000, 6.982962677686267499E-15 ) ) ;
#43806 = CARTESIAN_POINT ( 'NONE',  ( 18.55121869061587958, 10.32747123227773400, -173.0774032850249569 ) ) ;
#43807 = CARTESIAN_POINT ( 'NONE',  ( -12.25000000000000178, 26.30888228346803714, -233.3999513616626587 ) ) ;
#43808 = CARTESIAN_POINT ( 'NONE',  ( 21.05000000000000426, 10.72371710471867878, -74.59441739161313478 ) ) ;
#43809 = ORIENTED_EDGE ( 'NONE', *, *, #82601, .F. ) ;
#43811 = CARTESIAN_POINT ( 'NONE',  ( 21.05000000000000071, 28.63831050940605394, -258.0693639473472558 ) ) ;
#43810 = CARTESIAN_POINT ( 'NONE',  ( -18.50000000000000000, 77.16412189325360771, -162.3082593989527425 ) ) ;
#43812 = CARTESIAN_POINT ( 'NONE',  ( -20.94999999999999929, 1.835341550235569663, -45.05515129256298223 ) ) ;
#43813 = LINE ( 'NONE', #123352, #47740 ) ;
#43814 = EDGE_CURVE ( 'NONE', #191967, #116906, #83627, .T. ) ;
#43815 = DIRECTION ( 'NONE',  ( 1.000000000000000000, 0.000000000000000000, 0.000000000000000000 ) ) ;
#43816 = DIRECTION ( 'NONE',  ( -0.000000000000000000, 0.8814952561688430555, -0.4721928772777346239 ) ) ;
#43817 = ADVANCED_FACE ( 'NONE', ( #154242 ), #127142, .T. ) ;
#43818 = VERTEX_POINT ( 'NONE', #91653 ) ;
#43819 = ORIENTED_EDGE ( 'NONE', *, *, #193202, .T. ) ;
#43820 = ORIENTED_EDGE ( 'NONE', *, *, #180419, .F. ) ;
#43821 = CARTESIAN_POINT ( 'NONE',  ( -33.72168855820451938, 66.05000000001254534, -182.6731074845243654 ) ) ;
#43822 = ORIENTED_EDGE ( 'NONE', *, *, #205097, .T. ) ;
#43823 = LINE ( 'NONE', #142890, #247477 ) ;
#43824 = ORIENTED_EDGE ( 'NONE', *, *, #209218, .F. ) ;
#43825 = EDGE_CURVE ( 'NONE', #188424, #12569, #46239, .T. ) ;
#43826 = CARTESIAN_POINT ( 'NONE',  ( 20.94999999999999929, -11.48912529306489994, -64.10000000000000853 ) ) ;
#43827 = CARTESIAN_POINT ( 'NONE',  ( -23.25000000000000000, 87.65000000001174385, -81.27310748452423184 ) ) ;
#43828 = AXIS2_PLACEMENT_3D ( 'NONE', #103294, #104569, #168481 ) ;
#43829 = ADVANCED_FACE ( 'NONE', ( #13410 ), #172527, .T. ) ;
#43830 = AXIS2_PLACEMENT_3D ( 'NONE', #188656, #72585, #232948 ) ;
#43831 = ORIENTED_EDGE ( 'NONE', *, *, #179370, .T. ) ;
#43832 = CARTESIAN_POINT ( 'NONE',  ( 12.42718393586866910, 9.370655051134638924, -151.5258232559808960 ) ) ;
#43833 = AXIS2_PLACEMENT_3D ( 'NONE', #188965, #15482, #37609 ) ;
#43834 = EDGE_CURVE ( 'NONE', #162728, #232247, #96751, .T. ) ;
#43835 = ORIENTED_EDGE ( 'NONE', *, *, #221673, .T. ) ;
#43836 = ORIENTED_EDGE ( 'NONE', *, *, #239552, .F. ) ;
#43837 = ORIENTED_EDGE ( 'NONE', *, *, #80950, .F. ) ;
#43838 = EDGE_CURVE ( 'NONE', #4264, #108752, #52507, .T. ) ;
#43839 = CARTESIAN_POINT ( 'NONE',  ( -23.15000000000000213, 76.00000000001165290, -69.52310748452431710 ) ) ;
#43840 = DIRECTION ( 'NONE',  ( -1.000000000000000000, 0.000000000000000000, 0.000000000000000000 ) ) ;
#43841 = AXIS2_PLACEMENT_3D ( 'NONE', #184965, #162859, #29781 ) ;
#43842 = DIRECTION ( 'NONE',  ( 1.000000000000000000, -0.000000000000000000, -0.000000000000000000 ) ) ;
#43843 = LINE ( 'NONE', #148077, #32304 ) ;
#43844 = CARTESIAN_POINT ( 'NONE',  ( 20.85000000000000142, 45.93315328338058379, -256.6017782078560003 ) ) ;
#43845 = CARTESIAN_POINT ( 'NONE',  ( -22.57320508075687115, 11.65000000001115588, -67.00000000000007105 ) ) ;
#43846 = CARTESIAN_POINT ( 'NONE',  ( -23.25000000000000000, -9.600000000000001421, -23.60603087734756045 ) ) ;
#43847 = CARTESIAN_POINT ( 'NONE',  ( -0.8999999999999437339, 67.75000000001118394, -10.02310748452479139 ) ) ;
#43849 = ORIENTED_EDGE ( 'NONE', *, *, #28189, .F. ) ;
#43848 = CARTESIAN_POINT ( 'NONE',  ( 23.15000000000000213, 87.65000000001215597, -139.6231074845242688 ) ) ;
#43851 = DIRECTION ( 'NONE',  ( -0.000000000000000000, 6.982962677686266711E-15, -1.000000000000000000 ) ) ;
#43850 = CARTESIAN_POINT ( 'NONE',  ( -20.97625342178428554, 11.60000000083159755, -40.42820322980187342 ) ) ;
#43852 = CARTESIAN_POINT ( 'NONE',  ( -22.39999999999999858, 64.25000000001237765, -170.0231074845244166 ) ) ;
#43853 = EDGE_CURVE ( 'NONE', #115361, #178200, #129467, .T. ) ;
#43854 = VERTEX_POINT ( 'NONE', #139741 ) ;
#43855 = CARTESIAN_POINT ( 'NONE',  ( -18.59999999999999787, -1.835859311432481045, -179.0044391687985410 ) ) ;
#43856 = VECTOR ( 'NONE', #91606, 1000.000000000000000 ) ;
#43857 = CARTESIAN_POINT ( 'NONE',  ( 22.49999999999999645, 64.25043287652256652, -103.1239658536230763 ) ) ;
#43858 = CARTESIAN_POINT ( 'NONE',  ( 19.87657994472038325, 64.25000000001148237, -44.75731935989819021 ) ) ;
#43859 = VERTEX_POINT ( 'NONE', #142318 ) ;
#43860 = CIRCLE ( 'NONE', #73115, 0.09999999999999820144 ) ;
#43861 = CARTESIAN_POINT ( 'NONE',  ( 21.08376601933332495, 69.65805272873703302, -203.5868834954544013 ) ) ;
#43862 = CARTESIAN_POINT ( 'NONE',  ( -20.94999999999999929, 74.75000000001159606, -61.52310748452433131 ) ) ;
#43863 = ORIENTED_EDGE ( 'NONE', *, *, #149847, .F. ) ;
#43864 = ORIENTED_EDGE ( 'NONE', *, *, #25214, .T. ) ;
#43865 = CARTESIAN_POINT ( 'NONE',  ( -21.98333005346336577, -1.569210568885923696, -193.7948237253318098 ) ) ;
#43866 = ORIENTED_EDGE ( 'NONE', *, *, #62086, .T. ) ;
#43867 = CARTESIAN_POINT ( 'NONE',  ( 18.59999999999999076, 43.16354019706792400, -239.5695141926698284 ) ) ;
#43868 = DIRECTION ( 'NONE',  ( 0.000000000000000000, 0.2617529984165152257, 0.9651348961777124202 ) ) ;
#43869 = VECTOR ( 'NONE', #30992, 1000.000000000000000 ) ;
#43870 = DIRECTION ( 'NONE',  ( 2.952720810173289112E-16, 0.9651348961777174162, -0.2617529984164969070 ) ) ;
#43871 = DIRECTION ( 'NONE',  ( -1.186688945009009831E-16, -0.4088369013363280513, 0.9126074666063770380 ) ) ;
#43872 = ORIENTED_EDGE ( 'NONE', *, *, #3752, .T. ) ;
#43873 = DIRECTION ( 'NONE',  ( -1.000000000000000000, 0.000000000000000000, 0.000000000000000000 ) ) ;
#43874 = DIRECTION ( 'NONE',  ( 0.000000000000000000, -1.176083712526648525E-14, 1.000000000000000000 ) ) ;
#43875 = CARTESIAN_POINT ( 'NONE',  ( -23.25000000000000000, 7.128833340094563376, -233.7327013124401276 ) ) ;
#43876 = DIRECTION ( 'NONE',  ( 1.000000000000000000, 0.000000000000000000, 0.000000000000000000 ) ) ;
#43877 = CIRCLE ( 'NONE', #39810, 0.4000000000000114575 ) ;
#43878 = ADVANCED_FACE ( 'NONE', ( #138449 ), #242127, .T. ) ;
#43879 = ORIENTED_EDGE ( 'NONE', *, *, #241293, .F. ) ;
#43880 = AXIS2_PLACEMENT_3D ( 'NONE', #51301, #248253, #245684 ) ;
#43882 = ORIENTED_EDGE ( 'NONE', *, *, #122672, .T. ) ;
#43881 = DIRECTION ( 'NONE',  ( 0.000000000000000000, 0.1568667991644355497, 0.9876197685951332295 ) ) ;
#43883 = CARTESIAN_POINT ( 'NONE',  ( 18.49999999999998934, 6.450000000011156587, -177.5170271704400022 ) ) ;
#43884 = CARTESIAN_POINT ( 'NONE',  ( 18.54147908293605695, 78.20968212019604948, -231.5289770586088309 ) ) ;
#43885 = LINE ( 'NONE', #6022, #246078 ) ;
#43886 = CARTESIAN_POINT ( 'NONE',  ( 20.94999999999999929, 76.00000000001213607, -136.5231074845243313 ) ) ;
#43887 = CARTESIAN_POINT ( 'NONE',  ( 22.39999999999999503, 10.80758397488569500, -226.8651660546161395 ) ) ;
#43888 = DIRECTION ( 'NONE',  ( -1.000000000000000000, 0.000000000000000000, 0.000000000000000000 ) ) ;
#43889 = ORIENTED_EDGE ( 'NONE', *, *, #225232, .T. ) ;
#43890 = CARTESIAN_POINT ( 'NONE',  ( -20.64999999999999858, 1.115600667400684642E-11, -100.5000000000000426 ) ) ;
#43891 = DIRECTION ( 'NONE',  ( -0.000000000000000000, -6.982962677686266711E-15, 1.000000000000000000 ) ) ;
#43892 = CARTESIAN_POINT ( 'NONE',  ( 14.88075390448863899, 9.431689550535253375, -51.77929003223604809 ) ) ;
#43893 = DIRECTION ( 'NONE',  ( 0.000000000000000000, 0.000000000000000000, 1.000000000000000000 ) ) ;
#43894 = EDGE_CURVE ( 'NONE', #126916, #133367, #25421, .T. ) ;
#43895 = AXIS2_PLACEMENT_3D ( 'NONE', #124624, #85451, #166347 ) ;
#43896 = CARTESIAN_POINT ( 'NONE',  ( 18.49999999999999289, 10.20857864377385127, -21.75000000000000355 ) ) ;
#43897 = FACE_OUTER_BOUND ( 'NONE', #41320, .T. ) ;
#43898 = ORIENTED_EDGE ( 'NONE', *, *, #139760, .T. ) ;
#43899 = ORIENTED_EDGE ( 'NONE', *, *, #181764, .F. ) ;
#43900 = FACE_OUTER_BOUND ( 'NONE', #190486, .T. ) ;
#43901 = CARTESIAN_POINT ( 'NONE',  ( -21.29999999999995808, 1.115600667400684642E-11, -104.5500000000000256 ) ) ;
#43903 = CARTESIAN_POINT ( 'NONE',  ( 20.94999999999999929, 87.65000000001144542, -39.02310748452423894 ) ) ;
#43902 = AXIS2_PLACEMENT_3D ( 'NONE', #59925, #179919, #143331 ) ;
#43904 = CARTESIAN_POINT ( 'NONE',  ( -23.15000000000000213, 76.00000000001173817, -73.42310748452430857 ) ) ;
#43905 = EDGE_LOOP ( 'NONE', ( #54589, #112405, #158293, #226881 ) ) ;
#43906 = CARTESIAN_POINT ( 'NONE',  ( -18.42554971533678909, 46.96631235741502053, -255.3402005058479460 ) ) ;
#43907 = CARTESIAN_POINT ( 'NONE',  ( -21.05000000000000071, 77.16270174995010223, -128.6231074845242972 ) ) ;
#43908 = DIRECTION ( 'NONE',  ( -4.408576920032448588E-17, 0.1350103645451876944, 0.9908441862701601321 ) ) ;
#43909 = CARTESIAN_POINT ( 'NONE',  ( -21.02374657821594894, 16.98881331262127503, -224.4946931421776810 ) ) ;
#43910 = CIRCLE ( 'NONE', #256223, 0.09999999999999939493 ) ;
#43911 = CIRCLE ( 'NONE', #206240, 11.80000000000000426 ) ;
#43912 = ORIENTED_EDGE ( 'NONE', *, *, #133728, .F. ) ;
#43913 = DIRECTION ( 'NONE',  ( -1.000000000000000000, -0.000000000000000000, -0.000000000000000000 ) ) ;
#43914 = ORIENTED_EDGE ( 'NONE', *, *, #234616, .F. ) ;
#43915 = CARTESIAN_POINT ( 'NONE',  ( -23.25000000000000355, 5.650000000011139001, -109.7500000000000426 ) ) ;
#43916 = CARTESIAN_POINT ( 'NONE',  ( -20.54999999999999716, 68.85000000001186038, -90.67310748452435121 ) ) ;
#43917 = LINE ( 'NONE', #219984, #145132 ) ;
#43918 = CARTESIAN_POINT ( 'NONE',  ( -23.49999999999994316, 77.83551161375991967, -47.62760213295649692 ) ) ;
#43919 = CARTESIAN_POINT ( 'NONE',  ( 23.14999999999999503, 69.45000000001252261, -182.3731074845244109 ) ) ;
#43920 = LINE ( 'NONE', #25647, #131095 ) ;
#43921 = CARTESIAN_POINT ( 'NONE',  ( -18.40000000000000213, -9.519327731092442235, -6.972976376559327782 ) ) ;
#43922 = CARTESIAN_POINT ( 'NONE',  ( 23.24999999999999289, 13.96869538424789070, -210.3925794786331949 ) ) ;
#43923 = CARTESIAN_POINT ( 'NONE',  ( -21.53699400380687834, 6.787711793201953725, -67.00000000000004263 ) ) ;
#43924 = DIRECTION ( 'NONE',  ( 0.000000000000000000, 0.000000000000000000, 1.000000000000000000 ) ) ;
#43926 = EDGE_CURVE ( 'NONE', #181257, #228369, #79555, .T. ) ;
#43925 = LINE ( 'NONE', #140447, #97853 ) ;
#43927 = CYLINDRICAL_SURFACE ( 'NONE', #39736, 1.500000000000001332 ) ;
#43928 = VECTOR ( 'NONE', #231373, 1000.000000000000000 ) ;
#43929 = CIRCLE ( 'NONE', #210530, 0.1999999999999987899 ) ;
#43930 = CARTESIAN_POINT ( 'NONE',  ( -21.05000000000000071, 69.72991413632250612, -69.55797548753746185 ) ) ;
#43932 = CARTESIAN_POINT ( 'NONE',  ( 21.05000000000000071, 8.815201804577398548, -175.9205374966817033 ) ) ;
#43931 = AXIS2_PLACEMENT_3D ( 'NONE', #68244, #104761, #107355 ) ;
#43933 = AXIS2_PLACEMENT_3D ( 'NONE', #223002, #204720, #26114 ) ;
#43934 = ORIENTED_EDGE ( 'NONE', *, *, #235378, .T. ) ;
#43935 = CARTESIAN_POINT ( 'NONE',  ( 20.85000000000000142, 76.00000000001126921, -203.5231074845248997 ) ) ;
#43936 = EDGE_CURVE ( 'NONE', #224430, #213545, #171207, .T. ) ;
#43937 = ORIENTED_EDGE ( 'NONE', *, *, #55379, .T. ) ;
#43939 = EDGE_CURVE ( 'NONE', #255163, #63952, #200384, .T. ) ;
#43938 = CARTESIAN_POINT ( 'NONE',  ( -22.47120815636973745, 0.02890382191504723905, -55.35006801124654885 ) ) ;
#43940 = DIRECTION ( 'NONE',  ( 1.000000000000000000, 0.000000000000000000, -0.000000000000000000 ) ) ;
#43941 = DIRECTION ( 'NONE',  ( 0.000000000000000000, 7.056502275159890043E-15, -1.000000000000000000 ) ) ;
#43942 = VERTEX_POINT ( 'NONE', #201027 ) ;
#43943 = DIRECTION ( 'NONE',  ( 0.000000000000000000, 0.9908441862701420355, 0.1350103645453197554 ) ) ;
#43944 = LINE ( 'NONE', #98743, #255719 ) ;
#43945 = EDGE_CURVE ( 'NONE', #56434, #126637, #221021, .T. ) ;
#43946 = ORIENTED_EDGE ( 'NONE', *, *, #148192, .F. ) ;
#43947 = AXIS2_PLACEMENT_3D ( 'NONE', #236778, #59397, #219784 ) ;
#43948 = AXIS2_PLACEMENT_3D ( 'NONE', #92191, #47926, #147022 ) ;
#43949 = EDGE_LOOP ( 'NONE', ( #237412, #235517, #217630, #51560 ) ) ;
#43950 = DIRECTION ( 'NONE',  ( 1.000000000000000000, 3.265361837132813093E-16, -0.000000000000000000 ) ) ;
#43951 = ORIENTED_EDGE ( 'NONE', *, *, #223325, .T. ) ;
#43952 = AXIS2_PLACEMENT_3D ( 'NONE', #65433, #27635, #50979 ) ;
#43954 = EDGE_CURVE ( 'NONE', #223215, #168134, #175288, .T. ) ;
#43953 = DIRECTION ( 'NONE',  ( 0.000000000000000000, 0.9994937237965558774, 0.03181660087586650476 ) ) ;
#43955 = CARTESIAN_POINT ( 'NONE',  ( 20.94999999999999929, 67.23127455305835554, -235.8551265064784559 ) ) ;
#43956 = CARTESIAN_POINT ( 'NONE',  ( -20.95000000000000284, 64.35000000001147669, -43.03791325517834565 ) ) ;
#43958 = CIRCLE ( 'NONE', #160711, 1.500000000000001332 ) ;
#43957 = CARTESIAN_POINT ( 'NONE',  ( -20.94999999999999929, 1.835341550224413698, -11.55515129256298046 ) ) ;
#43960 = LINE ( 'NONE', #158804, #100288 ) ;
#43959 = CIRCLE ( 'NONE', #85612, 0.5000000000000051070 ) ;
#43961 = AXIS2_PLACEMENT_3D ( 'NONE', #107255, #205052, #102094 ) ;
#43962 = LINE ( 'NONE', #80480, #214157 ) ;
#43963 = LINE ( 'NONE', #41419, #33525 ) ;
#43964 = DIRECTION ( 'NONE',  ( 0.000000000000000000, 0.000000000000000000, -1.000000000000000000 ) ) ;
#43965 = CARTESIAN_POINT ( 'NONE',  ( -20.94999999999999929, 44.10931966560507789, -259.0886734199950183 ) ) ;
#43967 = ORIENTED_EDGE ( 'NONE', *, *, #77049, .F. ) ;
#43966 = CARTESIAN_POINT ( 'NONE',  ( 18.33683296300310772, 86.98713236139516880, -199.3477403010566888 ) ) ;
#43968 = ORIENTED_EDGE ( 'NONE', *, *, #161303, .F. ) ;
#43969 = CARTESIAN_POINT ( 'NONE',  ( -23.15000000000000213, 64.25000000001193712, -106.1231074845243825 ) ) ;
#43971 = VERTEX_POINT ( 'NONE', #202309 ) ;
#43970 = CARTESIAN_POINT ( 'NONE',  ( -16.85697194749148764, 61.05396939583364002, -220.7775114784828361 ) ) ;
#43972 = ORIENTED_EDGE ( 'NONE', *, *, #130312, .T. ) ;
#43973 = FACE_OUTER_BOUND ( 'NONE', #56359, .T. ) ;
#43974 = DIRECTION ( 'NONE',  ( 0.000000000000000000, 1.000000000000000000, -6.308085367188393199E-16 ) ) ;
#43975 = B_SPLINE_CURVE_WITH_KNOTS ( 'NONE', 3,
 ( #212145, #162447, #59431, #118166 ),
 .UNSPECIFIED., .F., .F.,
 ( 4, 4 ),
 ( 0.000000000000000000, 7.713889350930393175E-05 ),
 .UNSPECIFIED. ) ;
#43976 = AXIS2_PLACEMENT_3D ( 'NONE', #89595, #252518, #32231 ) ;
#43977 = AXIS2_PLACEMENT_3D ( 'NONE', #86356, #44710, #25160 ) ;
#43978 = DIRECTION ( 'NONE',  ( 0.000000000000000000, -0.1298341882519953583, -0.9915357197604861561 ) ) ;
#43979 = LINE ( 'NONE', #23160, #94209 ) ;
#43980 = CARTESIAN_POINT ( 'NONE',  ( 21.14999999999999503, 65.59531831295525706, -241.8872196075891168 ) ) ;
#43981 = VECTOR ( 'NONE', #83608, 1000.000000000000000 ) ;
#43982 = DIRECTION ( 'NONE',  ( 0.000000000000000000, -0.8660254037844412611, -0.4999999999999956701 ) ) ;
#43983 = ADVANCED_FACE ( 'NONE', ( #160642 ), #158094, .T. ) ;
#43984 = DIRECTION ( 'NONE',  ( 1.000000000000000000, 0.000000000000000000, 0.000000000000000000 ) ) ;
#43985 = VERTEX_POINT ( 'NONE', #221838 ) ;
#43986 = ORIENTED_EDGE ( 'NONE', *, *, #195646, .T. ) ;
#43987 = CARTESIAN_POINT ( 'NONE',  ( 23.04999999999999716, 13.05738666989944363, -219.4949925395660557 ) ) ;
#43988 = VERTEX_POINT ( 'NONE', #23703 ) ;
#43989 = CARTESIAN_POINT ( 'NONE',  ( -21.14999999999999858, -11.74999999998884448, -167.4999999999999432 ) ) ;
#43990 = ORIENTED_EDGE ( 'NONE', *, *, #18403, .F. ) ;
#43991 = CARTESIAN_POINT ( 'NONE',  ( -16.87683809663752399, 9.850000000011144508, -154.0976359818037054 ) ) ;
#43992 = ADVANCED_FACE ( 'NONE', ( #103184 ), #240158, .F. ) ;
#43993 = CARTESIAN_POINT ( 'NONE',  ( 20.85000000000000142, 80.78317333349157536, -192.9003134612048882 ) ) ;
#43994 = DIRECTION ( 'NONE',  ( -1.000000000000000000, -0.000000000000000000, -0.000000000000000000 ) ) ;
#43995 = CARTESIAN_POINT ( 'NONE',  ( 18.49999999999999645, 42.92545512184477730, -254.1955779480491344 ) ) ;
#43996 = EDGE_LOOP ( 'NONE', ( #62289, #151888, #103339, #3681, #199751 ) ) ;
#43997 = APPLICATION_CONTEXT ( 'automotive_design' ) ;
#43999 = EDGE_CURVE ( 'NONE', #113100, #52139, #123726, .T. ) ;
#43998 = CARTESIAN_POINT ( 'NONE',  ( -20.97625342178427132, 11.60000000082050953, -6.928203229801833452 ) ) ;
#44000 = ORIENTED_EDGE ( 'NONE', *, *, #200424, .F. ) ;
#44001 = AXIS2_PLACEMENT_3D ( 'NONE', #102995, #182572, #85982 ) ;
#44002 = DIRECTION ( 'NONE',  ( 1.000000000000000000, 0.000000000000000000, 0.000000000000000000 ) ) ;
#44003 = CARTESIAN_POINT ( 'NONE',  ( -21.53752568622177677, 30.42476846892962072, -252.2355353702321850 ) ) ;
#44004 = AXIS2_PLACEMENT_3D ( 'NONE', #177804, #257261, #59074 ) ;
#44005 = CARTESIAN_POINT ( 'NONE',  ( 21.13736287352038445, 67.95335762362800835, -115.6731074845243654 ) ) ;
#44006 = DIRECTION ( 'NONE',  ( -0.000000000000000000, 0.9770955615653313941, 0.2128009952263603954 ) ) ;
#44007 = ADVANCED_FACE ( 'NONE', ( #44527 ), #197157, .T. ) ;
#44008 = CIRCLE ( 'NONE', #164829, 0.1000000000000028644 ) ;
#44009 = ORIENTED_EDGE ( 'NONE', *, *, #186560, .F. ) ;
#44010 = DIRECTION ( 'NONE',  ( 1.000000000000000000, -0.000000000000000000, -0.000000000000000000 ) ) ;
#44011 = ORIENTED_EDGE ( 'NONE', *, *, #110132, .F. ) ;
#44014 = ORIENTED_EDGE ( 'NONE', *, *, #9650, .T. ) ;
#44013 = DIRECTION ( 'NONE',  ( 0.000000000000000000, 1.000000000000000000, 6.688090509790097607E-15 ) ) ;
#44012 = CARTESIAN_POINT ( 'NONE',  ( -18.59999999999999787, 85.50000000001233502, -161.9231074845242802 ) ) ;
#44015 = LINE ( 'NONE', #45303, #152010 ) ;
#44016 = ORIENTED_EDGE ( 'NONE', *, *, #179289, .T. ) ;
#44017 = AXIS2_PLACEMENT_3D ( 'NONE', #10385, #229426, #248998 ) ;
#44018 = DIRECTION ( 'NONE',  ( -0.000000000000000000, 1.000000000000000000, -0.000000000000000000 ) ) ;
#44019 = ORIENTED_EDGE ( 'NONE', *, *, #57281, .T. ) ;
#44020 = CARTESIAN_POINT ( 'NONE',  ( -20.94999999999999929, 61.95000000001218154, -142.0368025552853624 ) ) ;
#44023 = EDGE_CURVE ( 'NONE', #11593, #231129, #89514, .T. ) ;
#44022 = DIRECTION ( 'NONE',  ( 0.000000000000000000, 1.000000000000000000, -1.224646799147353207E-16 ) ) ;
#44021 =( BOUNDED_SURFACE ( )  B_SPLINE_SURFACE ( 3, 2, ( 
 ( #243445, #63516, #20575 ),
 ( #197896, #199197, #222578 ),
 ( #179645, #43966, #123508 ),
 ( #24432, #19270, #103910 ),
 ( #950, #80487, #4810 ),
 ( #7395, #25692, #227730 ),
 ( #6105, #45250, #208193 ),
 ( #69973, #27001, #188604 ),
 ( #127358, #88195, #126053 ),
 ( #247288, #165199, #68673 ) ),
 .UNSPECIFIED., .F., .F., .F. ) 
 B_SPLINE_SURFACE_WITH_KNOTS ( ( 4, 2, 2, 2, 4 ),
 ( 3, 3 ),
 ( 0.0001701955120502368938, 0.0002247052511886077396, 0.0002792149903269785854, 0.0003882344686037202228, 0.0006062734251572035517 ),
 ( 0.000000000000000000, 1.000000000000000000 ),
 .UNSPECIFIED. ) 
 GEOMETRIC_REPRESENTATION_ITEM ( )  RATIONAL_B_SPLINE_SURFACE ( (
 ( 1.000000000000000000, 0.2966190024559618443, 1.000000000000000000),
 ( 1.000000000000000000, 0.2964522492724643299, 1.000000000000000000),
 ( 1.000000000000000000, 0.3059923531867425051, 1.000000000000000000),
 ( 1.000000000000000000, 0.3355751146960955222, 1.000000000000000000),
 ( 1.000000000000000000, 0.3550672384944031923, 1.000000000000000000),
 ( 1.000000000000000000, 0.4157034672218395399, 1.000000000000000000),
 ( 1.000000000000000000, 0.4588031877619547227, 1.000000000000000000),
 ( 1.000000000000000000, 0.5771441759730387977, 1.000000000000000000),
 ( 1.000000000000000000, 0.6469377121719541712, 1.000000000000000000),
 ( 1.000000000000000000, 0.7071067811865933139, 1.000000000000000000) ) ) 
 REPRESENTATION_ITEM ( '' )  SURFACE ( )  );
#44024 = CARTESIAN_POINT ( 'NONE',  ( -22.39999999999999858, -3.140208063160686791, -228.2318569537739847 ) ) ;
#44025 = CIRCLE ( 'NONE', #189776, 0.1000000000000013933 ) ;
#44026 = UNCERTAINTY_MEASURE_WITH_UNIT (LENGTH_MEASURE( 1.000000000000000082E-05 ), #28463, 'distance_accuracy_value', 'NONE');
#44027 = FACE_OUTER_BOUND ( 'NONE', #181000, .T. ) ;
#44028 = CIRCLE ( 'NONE', #177347, 14.30833333333333890 ) ;
#44029 = EDGE_CURVE ( 'NONE', #109797, #182432, #187742, .T. ) ;
#44030 = EDGE_CURVE ( 'NONE', #20048, #123690, #11503, .T. ) ;
#44031 = CARTESIAN_POINT ( 'NONE',  ( 18.59999999999999432, 1.162701749938009677, -8.099999999999999645 ) ) ;
#44032 = AXIS2_PLACEMENT_3D ( 'NONE', #154877, #234371, #118296 ) ;
#44033 = VERTEX_POINT ( 'NONE', #14069 ) ;
#44034 = DIRECTION ( 'NONE',  ( 1.000000000000000000, -0.000000000000000000, -0.000000000000000000 ) ) ;
#44035 = DIRECTION ( 'NONE',  ( 0.7071067811865388020, -0.7071067811865561215, 0.000000000000000000 ) ) ;
#44036 = CARTESIAN_POINT ( 'NONE',  ( -18.49372193242239959, -9.442484523346882597, -140.7647812600350505 ) ) ;
#44037 = ORIENTED_EDGE ( 'NONE', *, *, #179746, .T. ) ;
#44038 = CARTESIAN_POINT ( 'NONE',  ( -21.05000000000000426, 18.71344899777637494, -226.7788045585494103 ) ) ;
#44039 = ORIENTED_EDGE ( 'NONE', *, *, #107512, .T. ) ;
#44040 = DIRECTION ( 'NONE',  ( -0.000000000000000000, -0.9342891509276814999, -0.3565161741896601399 ) ) ;
#44041 = ADVANCED_FACE ( 'NONE', ( #184018 ), #12795, .T. ) ;
#44042 = FACE_OUTER_BOUND ( 'NONE', #253873, .T. ) ;
#44043 = PLANE ( 'NONE',  #239194 ) ;
#44045 = VERTEX_POINT ( 'NONE', #171883 ) ;
#44044 = DIRECTION ( 'NONE',  ( 1.000000000000000000, -0.000000000000000000, 0.000000000000000000 ) ) ;
#44046 = EDGE_CURVE ( 'NONE', #209410, #69800, #179555, .T. ) ;
#44047 = DIRECTION ( 'NONE',  ( -2.342056488767301376E-15, 0.1350103645451974088, -0.9908441862701587999 ) ) ;
#44048 = EDGE_CURVE ( 'NONE', #35701, #92871, #237796, .T. ) ;
#44049 = CARTESIAN_POINT ( 'NONE',  ( -15.31895204843006120, 62.84928511903725479, -216.1139082291015256 ) ) ;
#44050 = LINE ( 'NONE', #165275, #47804 ) ;
#44051 = ORIENTED_EDGE ( 'NONE', *, *, #31822, .F. ) ;
#44052 = CARTESIAN_POINT ( 'NONE',  ( 21.05000000000000071, -9.400000000000002132, -9.893969122652443104 ) ) ;
#44053 = DIRECTION ( 'NONE',  ( 0.000000000000000000, 0.01562499999998609446, -0.9998779222360101304 ) ) ;
#44054 = VERTEX_POINT ( 'NONE', #47063 ) ;
#44055 = DIRECTION ( 'NONE',  ( 1.000000000000000000, 0.000000000000000000, 0.000000000000000000 ) ) ;
#44056 = CIRCLE ( 'NONE', #139888, 4.049999999999998046 ) ;
#44057 = AXIS2_PLACEMENT_3D ( 'NONE', #183947, #5277, #165696 ) ;
#44058 = AXIS2_PLACEMENT_3D ( 'NONE', #247930, #169730, #171025 ) ;
#44059 = AXIS2_PLACEMENT_3D ( 'NONE', #92273, #174441, #256419 ) ;
#44060 = ORIENTED_EDGE ( 'NONE', *, *, #109471, .F. ) ;
#44061 = CARTESIAN_POINT ( 'NONE',  ( -16.78493832629888161, 44.14991418685006153, -235.2970290647050433 ) ) ;
#44063 = VERTEX_POINT ( 'NONE', #26252 ) ;
#44062 = CARTESIAN_POINT ( 'NONE',  ( -20.54999999999999716, -8.663551401858004652, -43.02410111806730697 ) ) ;
#44064 = EDGE_CURVE ( 'NONE', #152197, #53634, #125371, .T. ) ;
#44065 = EDGE_CURVE ( 'NONE', #101102, #65554, #225683, .T. ) ;
#44066 = B_SPLINE_CURVE_WITH_KNOTS ( 'NONE', 3,
 ( #9979, #149514, #192470, #93358, #54227, #89498, #210746 ),
 .UNSPECIFIED., .F., .F.,
 ( 4, 3, 4 ),
 ( 0.000000000000000000, 0.0009834301579440022593, 0.001767853679402679300 ),
 .UNSPECIFIED. ) ;
#44069 = EDGE_LOOP ( 'NONE', ( #195983, #206047, #54950 ) ) ;
#44068 = ORIENTED_EDGE ( 'NONE', *, *, #176450, .T. ) ;
#44067 = CARTESIAN_POINT ( 'NONE',  ( -20.94999999999994600, 66.25000000001119815, -4.623107484524796362 ) ) ;
#44070 = CARTESIAN_POINT ( 'NONE',  ( -21.14999999999999858, 30.68987205111127281, -252.2252246220829193 ) ) ;
#44071 = CARTESIAN_POINT ( 'NONE',  ( 23.14999999999999858, 71.00000000001151079, -48.42837350343745584 ) ) ;
#44073 = EDGE_CURVE ( 'NONE', #65920, #176003, #212862, .T. ) ;
#44072 = CARTESIAN_POINT ( 'NONE',  ( -27.30103769104855971, 12.19999999999999574, 33.00000000000000000 ) ) ;
#44075 = DIRECTION ( 'NONE',  ( -1.000000000000000000, 0.000000000000000000, 0.000000000000000000 ) ) ;
#44074 = CARTESIAN_POINT ( 'NONE',  ( 22.39999999999999503, 1.115600667400684642E-11, -88.85042919245522341 ) ) ;
#44076 = DIRECTION ( 'NONE',  ( 0.000000000000000000, 1.000000000000000000, 0.000000000000000000 ) ) ;
#44077 = VECTOR ( 'NONE', #48621, 1000.000000000000000 ) ;
#44078 = DIRECTION ( 'NONE',  ( 1.000000000000000000, 0.000000000000000000, 0.000000000000000000 ) ) ;
#44079 = CARTESIAN_POINT ( 'NONE',  ( -22.50000000000094147, 75.89914163091360422, -148.2726746080137161 ) ) ;
#44080 = ORIENTED_EDGE ( 'NONE', *, *, #5715, .F. ) ;
#44081 = ORIENTED_EDGE ( 'NONE', *, *, #159042, .T. ) ;
#44082 = CARTESIAN_POINT ( 'NONE',  ( -20.94999999999999929, 64.25000000001175238, -76.30697314750247529 ) ) ;
#44083 = VECTOR ( 'NONE', #253666, 1000.000000000000000 ) ;
#44085 = ORIENTED_EDGE ( 'NONE', *, *, #61038, .F. ) ;
#44084 = CARTESIAN_POINT ( 'NONE',  ( -18.50000000000000000, 1.866714910068465239, -112.2526752462820525 ) ) ;
#44086 = ORIENTED_EDGE ( 'NONE', *, *, #393, .F. ) ;
#44087 = CARTESIAN_POINT ( 'NONE',  ( -21.53699400380413564, 6.787711793193499155, -1.424708524881391155E-14 ) ) ;
#44088 = VERTEX_POINT ( 'NONE', #105741 ) ;
#44089 = CARTESIAN_POINT ( 'NONE',  ( -23.15000000000000213, 85.00000000001188027, -93.12913836187181005 ) ) ;
#44090 = EDGE_CURVE ( 'NONE', #208426, #116862, #158718, .T. ) ;
#44091 = ORIENTED_EDGE ( 'NONE', *, *, #11113, .T. ) ;
#44092 = DIRECTION ( 'NONE',  ( 0.000000000000000000, 0.000000000000000000, 1.000000000000000000 ) ) ;
#44094 = EDGE_CURVE ( 'NONE', #122253, #194728, #151004, .T. ) ;
#44093 = DIRECTION ( 'NONE',  ( -1.000000000000000000, 0.000000000000000000, 0.000000000000000000 ) ) ;
#44097 = ORIENTED_EDGE ( 'NONE', *, *, #89221, .T. ) ;
#44096 = VERTEX_POINT ( 'NONE', #185312 ) ;
#44095 = AXIS2_PLACEMENT_3D ( 'NONE', #181676, #206371, #107256 ) ;
#44098 = ORIENTED_EDGE ( 'NONE', *, *, #196337, .T. ) ;
#44099 = CARTESIAN_POINT ( 'NONE',  ( 21.07888907270776002, 10.72506921352637654, -45.72119358683318779 ) ) ;
#44100 = ORIENTED_EDGE ( 'NONE', *, *, #194811, .F. ) ;
#44101 = ORIENTED_EDGE ( 'NONE', *, *, #159015, .T. ) ;
#44102 = DIRECTION ( 'NONE',  ( -3.787827842127534447E-15, -0.7397360091702729346, -0.6728971962616859814 ) ) ;
#44103 = FACE_OUTER_BOUND ( 'NONE', #16362, .T. ) ;
#44106 = EDGE_CURVE ( 'NONE', #56611, #44045, #186612, .T. ) ;
#44105 = EDGE_LOOP ( 'NONE', ( #154387, #146732, #3000, #213187, #3996 ) ) ;
#44104 = CARTESIAN_POINT ( 'NONE',  ( 18.48413544395651442, -9.664304033616561540, -107.1831049930384125 ) ) ;
#44108 = CARTESIAN_POINT ( 'NONE',  ( -16.87487986503753845, 60.93934386241939904, -221.0417501376295775 ) ) ;
#44107 = LINE ( 'NONE', #243587, #49146 ) ;
#44109 = CARTESIAN_POINT ( 'NONE',  ( 21.09610168723073187, 0.03358950690265036926, -60.62104428477527307 ) ) ;
#44111 = ORIENTED_EDGE ( 'NONE', *, *, #224031, .T. ) ;
#44110 = CARTESIAN_POINT ( 'NONE',  ( 20.85000000000000142, 77.83585931145600512, -158.5186683157258187 ) ) ;
#44112 = CYLINDRICAL_SURFACE ( 'NONE', #38613, 0.09999999999999530098 ) ;
#44113 = EDGE_LOOP ( 'NONE', ( #193371, #216421, #105569, #71439, #233970 ) ) ;
#44114 = EDGE_CURVE ( 'NONE', #216369, #187259, #167096, .T. ) ;
#44115 = CARTESIAN_POINT ( 'NONE',  ( -21.05000000000000071, 1.116121084443477685E-11, -170.3999999999999488 ) ) ;
#44116 = ORIENTED_EDGE ( 'NONE', *, *, #224739, .F. ) ;
#44117 = FACE_OUTER_BOUND ( 'NONE', #46023, .T. ) ;
#44118 = CARTESIAN_POINT ( 'NONE',  ( 23.25000000000000000, 85.60000000001247145, -181.7731074845243029 ) ) ;
#44119 = ADVANCED_FACE ( 'NONE', ( #206161 ), #210973, .T. ) ;
#44120 = VECTOR ( 'NONE', #197190, 1000.000000000000000 ) ;
#44121 = VERTEX_POINT ( 'NONE', #133991 ) ;
#44122 = CARTESIAN_POINT ( 'NONE',  ( 21.12400247839509504, 10.72148804404154454, -45.75000000000000000 ) ) ;
#44123 = CIRCLE ( 'NONE', #77410, 0.1000000000000001305 ) ;
#44124 = TOROIDAL_SURFACE ( 'NONE', #152477, 11.70000000000000107, 0.1000000000000000056 ) ;
#44125 = AXIS2_PLACEMENT_3D ( 'NONE', #208608, #32559, #88614 ) ;
#44126 = EDGE_CURVE ( 'NONE', #171580, #206042, #75330, .T. ) ;
#44127 = DIRECTION ( 'NONE',  ( 0.000000000000000000, 0.000000000000000000, 1.000000000000000000 ) ) ;
#44128 = CARTESIAN_POINT ( 'NONE',  ( 21.05000000000000071, 18.94908112497232011, -227.8991131484155517 ) ) ;
#44129 = EDGE_CURVE ( 'NONE', #83250, #185463, #50325, .T. ) ;
#44130 = ORIENTED_EDGE ( 'NONE', *, *, #21874, .T. ) ;
#44131 = VERTEX_POINT ( 'NONE', #54455 ) ;
#44132 =( BOUNDED_SURFACE ( )  B_SPLINE_SURFACE ( 3, 2, ( 
 ( #48368, #243548, #104014 ),
 ( #221397, #226528, #62357 ),
 ( #63629, #67478, #246128 ),
 ( #42788, #162752, #4911 ) ),
 .UNSPECIFIED., .F., .F., .F. ) 
 B_SPLINE_SURFACE_WITH_KNOTS ( ( 4, 4 ),
 ( 3, 3 ),
 ( 0.0008258556059633722669, 0.0009616864997632808970 ),
 ( 0.000000000000000000, 1.000000000000000000 ),
 .UNSPECIFIED. ) 
 GEOMETRIC_REPRESENTATION_ITEM ( )  RATIONAL_B_SPLINE_SURFACE ( (
 ( 1.000000000000000000, 0.9152888060719368557, 1.000000000000000000),
 ( 1.000000000000000000, 0.9327727094138205111, 1.000000000000000000),
 ( 1.000000000000000000, 0.9369023509258461724, 1.000000000000000000),
 ( 1.000000000000000000, 0.9246339933864415883, 1.000000000000000000) ) ) 
 REPRESENTATION_ITEM ( '' )  SURFACE ( )  );
#44133 = DIRECTION ( 'NONE',  ( 1.000000000000000000, -0.000000000000000000, -0.000000000000000000 ) ) ;
#44134 = DIRECTION ( 'NONE',  ( -1.073024830501117725E-15, 0.000000000000000000, 1.000000000000000000 ) ) ;
#44135 = ORIENTED_EDGE ( 'NONE', *, *, #140931, .T. ) ;
#44136 = CARTESIAN_POINT ( 'NONE',  ( -20.85000000000000142, -1.249999999988843369, -74.80048075441509070 ) ) ;
#44137 = ORIENTED_EDGE ( 'NONE', *, *, #220646, .F. ) ;
#44138 = EDGE_CURVE ( 'NONE', #169096, #160332, #13132, .T. ) ;
#44139 = FACE_OUTER_BOUND ( 'NONE', #155613, .T. ) ;
#44140 = DIRECTION ( 'NONE',  ( 0.000000000000000000, -0.9651348961777157509, 0.2617529984165028467 ) ) ;
#44142 = DIRECTION ( 'NONE',  ( -1.000000000000000000, -1.394253735153569469E-16, -2.602809386958778209E-16 ) ) ;
#44141 = CARTESIAN_POINT ( 'NONE',  ( -11.59999999999994458, 67.75000000001118394, -21.02310748452479316 ) ) ;
#44143 = LINE ( 'NONE', #100226, #248932 ) ;
#44144 = CARTESIAN_POINT ( 'NONE',  ( 23.14999999999998437, -11.74999999998884448, -100.5000000000000284 ) ) ;
#44145 = ORIENTED_EDGE ( 'NONE', *, *, #136173, .T. ) ;
#44146 = FACE_OUTER_BOUND ( 'NONE', #7098, .T. ) ;
#44147 = EDGE_CURVE ( 'NONE', #62695, #155707, #37481, .T. ) ;
#44148 = EDGE_CURVE ( 'NONE', #221522, #64517, #154621, .T. ) ;
#44149 = CIRCLE ( 'NONE', #77266, 0.09999999999999939493 ) ;
#44151 = ORIENTED_EDGE ( 'NONE', *, *, #187693, .F. ) ;
#44150 = ORIENTED_EDGE ( 'NONE', *, *, #94197, .T. ) ;
#44152 = ORIENTED_EDGE ( 'NONE', *, *, #224428, .F. ) ;
#44153 = AXIS2_PLACEMENT_3D ( 'NONE', #123539, #25720, #64833 ) ;
#44154 = ORIENTED_EDGE ( 'NONE', *, *, #85818, .F. ) ;
#44155 = EDGE_CURVE ( 'NONE', #65207, #182460, #195283, .T. ) ;
#44156 = CARTESIAN_POINT ( 'NONE',  ( -18.50000000000000000, 46.45388641681647357, -243.1520440498138385 ) ) ;
#44157 = DIRECTION ( 'NONE',  ( 1.000000000000000000, -0.000000000000000000, -0.000000000000000000 ) ) ;
#44158 = CARTESIAN_POINT ( 'NONE',  ( -23.15000000000000213, 54.34471204062663219, -239.4366250215122420 ) ) ;
#44159 = CARTESIAN_POINT ( 'NONE',  ( -18.59999999999999787, 74.14897176987071248, -57.86919421510183525 ) ) ;
#44160 = VECTOR ( 'NONE', #157860, 1000.000000000000000 ) ;
#44161 = DIRECTION ( 'NONE',  ( 0.000000000000000000, 1.000000000000000000, 0.000000000000000000 ) ) ;
#44162 = CARTESIAN_POINT ( 'NONE',  ( 21.05000000000000071, 58.98867006934395363, -225.8934842717049492 ) ) ;
#44163 = ADVANCED_FACE ( 'NONE', ( #40067 ), #79137, .F. ) ;
#44165 = ORIENTED_EDGE ( 'NONE', *, *, #131190, .F. ) ;
#44164 = CARTESIAN_POINT ( 'NONE',  ( 18.50000000000000355, 77.44184265367995579, -241.6694879557322793 ) ) ;
#44166 = DIRECTION ( 'NONE',  ( -1.000000000000000000, 0.000000000000000000, -0.000000000000000000 ) ) ;
#44167 = ORIENTED_EDGE ( 'NONE', *, *, #227428, .F. ) ;
#44168 = AXIS2_PLACEMENT_3D ( 'NONE', #55806, #35039, #114539 ) ;
#44169 = CARTESIAN_POINT ( 'NONE',  ( -22.49999999999999645, 11.74956712350054744, -66.89914163090132604 ) ) ;
#44170 = CIRCLE ( 'NONE', #161048, 0.09999999999999939493 ) ;
#44171 = EDGE_CURVE ( 'NONE', #135978, #161523, #129640, .T. ) ;
#44172 = ORIENTED_EDGE ( 'NONE', *, *, #146107, .T. ) ;
#44173 = ORIENTED_EDGE ( 'NONE', *, *, #205971, .F. ) ;
#44174 = LINE ( 'NONE', #159005, #33611 ) ;
#44175 = CARTESIAN_POINT ( 'NONE',  ( -21.05000000000000071, -10.47749788991998088, -206.4278944321438587 ) ) ;
#44176 = CARTESIAN_POINT ( 'NONE',  ( -16.83558968593862915, 66.05000000001153637, -48.68541267214110491 ) ) ;
#44177 = CARTESIAN_POINT ( 'NONE',  ( 15.15590539855246277, 9.410682294279109072, -82.43114344194833620 ) ) ;
#44178 = AXIS2_PLACEMENT_3D ( 'NONE', #65888, #3324, #47592 ) ;
#44179 = CARTESIAN_POINT ( 'NONE',  ( -21.05000000000000071, -1.851028230129704522, -45.15391326942249606 ) ) ;
#44180 = VERTEX_POINT ( 'NONE', #197812 ) ;
#44181 = EDGE_LOOP ( 'NONE', ( #89470, #38835, #83219, #121920 ) ) ;
#44182 = AXIS2_PLACEMENT_3D ( 'NONE', #144913, #47090, #242733 ) ;
#44183 = DIRECTION ( 'NONE',  ( -0.000000000000000000, -0.000000000000000000, 1.000000000000000000 ) ) ;
#44185 = ADVANCED_FACE ( 'NONE', ( #160004 ), #174463, .T. ) ;
#44184 = ORIENTED_EDGE ( 'NONE', *, *, #257553, .F. ) ;
#44186 = CARTESIAN_POINT ( 'NONE',  ( 21.14999999999999858, 11.65000000001115943, -134.1000000000000227 ) ) ;
#44187 = CARTESIAN_POINT ( 'NONE',  ( -16.90257928357874917, 9.954106821116520010, -46.13628543011370198 ) ) ;
#44188 = DIRECTION ( 'NONE',  ( -1.000000000000000000, 0.000000000000000000, 0.000000000000000000 ) ) ;
#44189 = DIRECTION ( 'NONE',  ( -1.652117596168391306E-15, -0.9770955615653313941, -0.2128009952263603677 ) ) ;
#44190 = CIRCLE ( 'NONE', #131470, 2.000000000000001776 ) ;
#44191 = CARTESIAN_POINT ( 'NONE',  ( -20.54999999999999716, 7.814782362862218612, -216.4406663269861610 ) ) ;
#44192 = CARTESIAN_POINT ( 'NONE',  ( -16.78569801330232281, 66.05206626689836469, -90.36619457917686304 ) ) ;
#44193 = LINE ( 'NONE', #104128, #237702 ) ;
#44194 = FACE_OUTER_BOUND ( 'NONE', #60709, .T. ) ;
#44195 = CARTESIAN_POINT ( 'NONE',  ( -18.59999999999999787, -1.866714910057309273, -11.75267524628200633 ) ) ;
#44197 = ADVANCED_FACE ( 'NONE', ( #135263 ), #214811, .T. ) ;
#44196 = CARTESIAN_POINT ( 'NONE',  ( 18.52928932304156717, 65.72071067697093838, -178.8468540517211807 ) ) ;
#44198 = DIRECTION ( 'NONE',  ( -0.000000000000000000, -0.000000000000000000, 1.000000000000000000 ) ) ;
#44199 = AXIS2_PLACEMENT_3D ( 'NONE', #86362, #31595, #168558 ) ;
#44200 = FACE_OUTER_BOUND ( 'NONE', #175874, .T. ) ;
#44201 = VERTEX_POINT ( 'NONE', #175717 ) ;
#44203 = EDGE_CURVE ( 'NONE', #172081, #223901, #233877, .T. ) ;
#44202 = CARTESIAN_POINT ( 'NONE',  ( 13.40000000000000036, -12.24999999999999822, 15.00000000000000355 ) ) ;
#44204 = ORIENTED_EDGE ( 'NONE', *, *, #222285, .T. ) ;
#44205 = DIRECTION ( 'NONE',  ( 1.000000000000000000, 1.836970198721029934E-16, 0.000000000000000000 ) ) ;
#44206 = DIRECTION ( 'NONE',  ( 1.000000000000000000, 0.000000000000000000, 0.000000000000000000 ) ) ;
#44207 = CARTESIAN_POINT ( 'NONE',  ( -20.54999999999999716, 84.73084112150795022, -193.9250327655399531 ) ) ;
#44209 = ORIENTED_EDGE ( 'NONE', *, *, #144059, .F. ) ;
#44208 = VECTOR ( 'NONE', #103974, 1000.000000000000000 ) ;
#44210 = CARTESIAN_POINT ( 'NONE',  ( -18.40000000000000213, 5.650000000011139001, -124.7500000000000426 ) ) ;
#44211 = FACE_OUTER_BOUND ( 'NONE', #54607, .T. ) ;
#44212 = AXIS2_PLACEMENT_3D ( 'NONE', #162809, #64962, #238473 ) ;
#44213 = AXIS2_PLACEMENT_3D ( 'NONE', #129653, #106213, #245755 ) ;
#44214 = DIRECTION ( 'NONE',  ( 0.000000000000000000, -1.000000000000000000, 0.000000000000000000 ) ) ;
#44215 = DIRECTION ( 'NONE',  ( 0.000000000000000000, 0.2617529984165035128, 0.9651348961777155289 ) ) ;
#44216 = ADVANCED_FACE ( 'NONE', ( #256439 ), #236948, .F. ) ;
#44217 = DIRECTION ( 'NONE',  ( 0.000000000000000000, -0.9998779222360097974, 0.01562500000000363945 ) ) ;
#44218 = CARTESIAN_POINT ( 'NONE',  ( -23.25000000000000000, 17.11694853917243364, -224.3781540347815451 ) ) ;
#44219 = AXIS2_PLACEMENT_3D ( 'NONE', #179726, #194163, #18062 ) ;
#44220 = ORIENTED_EDGE ( 'NONE', *, *, #206958, .T. ) ;
#44221 = CARTESIAN_POINT ( 'NONE',  ( 20.85000000000000142, 11.75000000001115907, -167.5000000000000284 ) ) ;
#44223 = ORIENTED_EDGE ( 'NONE', *, *, #116114, .F. ) ;
#44222 = CARTESIAN_POINT ( 'NONE',  ( 22.49999999999999645, 11.64976291804307884, -167.4111900236130452 ) ) ;
#44224 = CARTESIAN_POINT ( 'NONE',  ( 22.40000000000020819, -0.1008583690885111045, -122.2504328765103168 ) ) ;
#44225 = CARTESIAN_POINT ( 'NONE',  ( -23.25000000000000000, 77.14957036958736580, -61.70719500002233815 ) ) ;
#44226 = CARTESIAN_POINT ( 'NONE',  ( -20.64999999999999858, 1.115600667400684642E-11, -79.97500000000005116 ) ) ;
#44227 = CIRCLE ( 'NONE', #98328, 0.1000000000000028644 ) ;
#44228 = ORIENTED_EDGE ( 'NONE', *, *, #253920, .T. ) ;
#44229 = CARTESIAN_POINT ( 'NONE',  ( -18.59999999999999787, 64.35000000001180354, -81.67310748452439384 ) ) ;
#44230 = CIRCLE ( 'NONE', #215089, 4.041421356237314022 ) ;
#44231 = DIRECTION ( 'NONE',  ( 0.000000000000000000, 8.023096076392503095E-14, 1.000000000000000000 ) ) ;
#44232 = AXIS2_PLACEMENT_3D ( 'NONE', #216745, #159367, #23727 ) ;
#44233 = VERTEX_POINT ( 'NONE', #77857 ) ;
#44234 = DIRECTION ( 'NONE',  ( -0.000000000000000000, -6.982962677686266711E-15, 1.000000000000000000 ) ) ;
#44235 = CARTESIAN_POINT ( 'NONE',  ( 17.23472005113827876, 22.09227994357196678, -230.0545770955219211 ) ) ;
#44236 = DIRECTION ( 'NONE',  ( 0.000000000000000000, 0.000000000000000000, 1.000000000000000000 ) ) ;
#44237 = ORIENTED_EDGE ( 'NONE', *, *, #160941, .T. ) ;
#44238 = VECTOR ( 'NONE', #243546, 999.9999999999998863 ) ;
#44239 = ORIENTED_EDGE ( 'NONE', *, *, #221267, .F. ) ;
#44240 = DIRECTION ( 'NONE',  ( 0.000000000000000000, 0.000000000000000000, -1.000000000000000000 ) ) ;
#44241 = DIRECTION ( 'NONE',  ( 0.000000000000000000, 1.000000000000000000, -1.224646799147353207E-16 ) ) ;
#44242 = DIRECTION ( 'NONE',  ( 0.000000000000000000, -7.086529944415894657E-15, 1.000000000000000000 ) ) ;
#44243 = CARTESIAN_POINT ( 'NONE',  ( -23.25000000000000000, 76.00000000001126921, -203.5231074845248997 ) ) ;
#44244 = LINE ( 'NONE', #88466, #228589 ) ;
#44245 = EDGE_CURVE ( 'NONE', #87569, #173980, #255166, .T. ) ;
#44246 = DIRECTION ( 'NONE',  ( 1.000000000000000000, 0.000000000000000000, 0.000000000000000000 ) ) ;
#44248 = FACE_OUTER_BOUND ( 'NONE', #165025, .T. ) ;
#44247 = CARTESIAN_POINT ( 'NONE',  ( 20.95265033839679347, 65.48774916754473452, -95.45734372849443616 ) ) ;
#44249 = DIRECTION ( 'NONE',  ( 0.000000000000000000, 0.000000000000000000, -1.000000000000000000 ) ) ;
#44250 = DIRECTION ( 'NONE',  ( 1.000000000000000000, 0.000000000000000000, 0.000000000000000000 ) ) ;
#44251 = DIRECTION ( 'NONE',  ( 0.000000000000000000, 0.000000000000000000, -1.000000000000000000 ) ) ;
#44252 = CARTESIAN_POINT ( 'NONE',  ( -20.65000000000000568, 70.35000000001232934, -160.7731074845243882 ) ) ;
#44253 = AXIS2_PLACEMENT_3D ( 'NONE', #207762, #29151, #27855 ) ;
#44254 = ORIENTED_EDGE ( 'NONE', *, *, #200564, .F. ) ;
#44255 = AXIS2_PLACEMENT_3D ( 'NONE', #244891, #27172, #42848 ) ;
#44256 = ORIENTED_EDGE ( 'NONE', *, *, #169123, .T. ) ;
#44257 = CIRCLE ( 'NONE', #85904, 0.09999999999999954758 ) ;
#44258 = LINE ( 'NONE', #143337, #85854 ) ;
#44259 = VECTOR ( 'NONE', #200650, 1000.000000000000227 ) ;
#44260 = CARTESIAN_POINT ( 'NONE',  ( 20.85000000000000142, -1.263275465206102233, -208.9018646667463770 ) ) ;
#44262 = CARTESIAN_POINT ( 'NONE',  ( -18.59999999999999787, 7.567413955921500346, -241.6205176796878504 ) ) ;
#44261 = FACE_OUTER_BOUND ( 'NONE', #12618, .T. ) ;
#44263 = FACE_OUTER_BOUND ( 'NONE', #241364, .T. ) ;
#44265 = ADVANCED_FACE ( 'NONE', ( #99971 ), #118294, .T. ) ;
#44264 = CARTESIAN_POINT ( 'NONE',  ( -23.39999999999994529, 77.25000000001119815, -43.82310748452479743 ) ) ;
#44266 = DIRECTION ( 'NONE',  ( 0.000000000000000000, 0.1568667991644863147, 0.9876197685951252359 ) ) ;
#44267 = DIRECTION ( 'NONE',  ( -1.000000000000000000, -0.000000000000000000, -0.000000000000000000 ) ) ;
#44268 = ORIENTED_EDGE ( 'NONE', *, *, #172451, .F. ) ;
#44269 = ADVANCED_FACE ( 'NONE', ( #257735 ), #80400, .T. ) ;
#44270 = DIRECTION ( 'NONE',  ( 1.186688945009010077E-16, 1.000000000000000000, 6.982962677686266711E-15 ) ) ;
#44271 = AXIS2_PLACEMENT_3D ( 'NONE', #242680, #124042, #104434 ) ;
#44272 = ORIENTED_EDGE ( 'NONE', *, *, #253362, .F. ) ;
#44273 = DIRECTION ( 'NONE',  ( 0.000000000000000000, 0.000000000000000000, 1.000000000000000000 ) ) ;
#44274 = CIRCLE ( 'NONE', #206573, 0.09999999999999939493 ) ;
#44275 = EDGE_CURVE ( 'NONE', #207698, #13242, #100572, .T. ) ;
#44276 = LINE ( 'NONE', #183779, #92305 ) ;
#44277 = ADVANCED_FACE ( 'NONE', ( #82970 ), #240807, .T. ) ;
#44278 = AXIS2_PLACEMENT_3D ( 'NONE', #184414, #202694, #27953 ) ;
#44279 = EDGE_CURVE ( 'NONE', #64541, #98189, #29721, .T. ) ;
#44280 = ORIENTED_EDGE ( 'NONE', *, *, #151923, .T. ) ;
#44281 = CARTESIAN_POINT ( 'NONE',  ( -18.50211644919735576, 18.36312997293285321, -236.9042258689304106 ) ) ;
#44282 = ORIENTED_EDGE ( 'NONE', *, *, #13395, .F. ) ;
#44283 = ADVANCED_FACE ( 'NONE', ( #103831 ), #85536, .F. ) ;
#44284 = LINE ( 'NONE', #125108, #66420 ) ;
#44285 = DIRECTION ( 'NONE',  ( 0.000000000000000000, -1.000000000000000000, -0.000000000000000000 ) ) ;
#44286 = CARTESIAN_POINT ( 'NONE',  ( -20.64999999999999858, -8.999999999988844479, -191.1060308773475356 ) ) ;
#44287 = CARTESIAN_POINT ( 'NONE',  ( -18.49999999999999289, 77.31516873553810854, -241.6587350081051113 ) ) ;
#44288 = LINE ( 'NONE', #65115, #109900 ) ;
#44289 = CARTESIAN_POINT ( 'NONE',  ( -17.04761207306817994, 10.02645087339777064, -20.85000000000000142 ) ) ;
#44290 = EDGE_CURVE ( 'NONE', #250175, #121523, #101234, .T. ) ;
#44291 = CARTESIAN_POINT ( 'NONE',  ( 18.59999999999999076, 64.25000000001161027, -61.42310748452440095 ) ) ;
#44292 = LINE ( 'NONE', #123825, #99634 ) ;
#44294 = EDGE_LOOP ( 'NONE', ( #207319, #35242, #114001, #234120 ) ) ;
#44293 = CARTESIAN_POINT ( 'NONE',  ( 21.05933563467872105, 65.27547528793127185, -191.3294597355684630 ) ) ;
#44296 = DIRECTION ( 'NONE',  ( 1.000000000000000000, 0.000000000000000000, 0.000000000000000000 ) ) ;
#44295 = CARTESIAN_POINT ( 'NONE',  ( -16.78805706634180339, 66.05174750694081354, -115.6789542764925045 ) ) ;
#44297 = ORIENTED_EDGE ( 'NONE', *, *, #92333, .F. ) ;
#44299 = ORIENTED_EDGE ( 'NONE', *, *, #44691, .F. ) ;
#44298 = LINE ( 'NONE', #87241, #227469 ) ;
#44300 = VECTOR ( 'NONE', #120142, 1000.000000000000000 ) ;
#44301 = ORIENTED_EDGE ( 'NONE', *, *, #58735, .F. ) ;
#44302 = CARTESIAN_POINT ( 'NONE',  ( 18.60000000000000142, 85.32100840337290037, -62.28716923544637041 ) ) ;
#44303 = PLANE ( 'NONE',  #138505 ) ;
#44304 = FACE_OUTER_BOUND ( 'NONE', #192833, .T. ) ;
#44305 = VERTEX_POINT ( 'NONE', #124710 ) ;
#44306 = DIRECTION ( 'NONE',  ( 1.000000000000000000, 0.000000000000000000, 0.000000000000000000 ) ) ;
#44307 = DIRECTION ( 'NONE',  ( 0.000000000000000000, 0.000000000000000000, 1.000000000000000000 ) ) ;
#44308 = CARTESIAN_POINT ( 'NONE',  ( 20.84999999999999787, 11.75000000001116085, -93.58085275404134507 ) ) ;
#44309 = ORIENTED_EDGE ( 'NONE', *, *, #76106, .F. ) ;
#44311 = ADVANCED_FACE ( 'NONE', ( #86837 ), #161280, .F. ) ;
#44310 = CARTESIAN_POINT ( 'NONE',  ( -18.50000324121759476, 46.33100819526732295, -243.0553980158188381 ) ) ;
#44313 = AXIS2_PLACEMENT_3D ( 'NONE', #118665, #36576, #216446 ) ;
#44312 = DIRECTION ( 'NONE',  ( 0.000000000000000000, 0.000000000000000000, -1.000000000000000000 ) ) ;
#44314 = EDGE_LOOP ( 'NONE', ( #238617, #220179, #105225, #232367 ) ) ;
#44315 = ORIENTED_EDGE ( 'NONE', *, *, #238079, .T. ) ;
#44316 = CARTESIAN_POINT ( 'NONE',  ( 19.95857864376269575, 4.513204987021262937, 22.00000000000000355 ) ) ;
#44317 = CIRCLE ( 'NONE', #190052, 4.049999999999998046 ) ;
#44318 = CIRCLE ( 'NONE', #27768, 6.258578643762724880 ) ;
#44319 = VERTEX_POINT ( 'NONE', #145538 ) ;
#44320 = LINE ( 'NONE', #221636, #21681 ) ;
#44321 = VERTEX_POINT ( 'NONE', #184667 ) ;
#44322 = CARTESIAN_POINT ( 'NONE',  ( -23.25000000000000000, 73.40000000001228386, -156.7984855617622770 ) ) ;
#44323 = EDGE_CURVE ( 'NONE', #216625, #50141, #620, .T. ) ;
#44324 = CARTESIAN_POINT ( 'NONE',  ( 23.14999999999999503, 11.75000000001116263, -122.2500000000000284 ) ) ;
#44325 = DIRECTION ( 'NONE',  ( 0.000000000000000000, 0.000000000000000000, 1.000000000000000000 ) ) ;
#44326 = CARTESIAN_POINT ( 'NONE',  ( -21.12757541349819590, 30.74915888275712206, -252.1930093910820290 ) ) ;
#44327 = DIRECTION ( 'NONE',  ( -0.000000000000000000, 0.000000000000000000, -1.000000000000000000 ) ) ;
#44328 = EDGE_LOOP ( 'NONE', ( #183189, #4589, #134813, #48225 ) ) ;
#44329 = DIRECTION ( 'NONE',  ( -1.000000000000000000, 0.000000000000000000, 0.000000000000000000 ) ) ;
#44330 = CARTESIAN_POINT ( 'NONE',  ( -16.86337532320261090, 66.02003279578819672, -182.5741830155416210 ) ) ;
#44331 = FACE_OUTER_BOUND ( 'NONE', #115367, .T. ) ;
#44332 = CARTESIAN_POINT ( 'NONE',  ( -20.54999999999999716, 1.115600667400684642E-11, -202.8999999999999773 ) ) ;
#44333 = ORIENTED_EDGE ( 'NONE', *, *, #221372, .F. ) ;
#44335 = CARTESIAN_POINT ( 'NONE',  ( 18.60000000000000142, -9.399999999988782662, -40.79725975966329798 ) ) ;
#44334 = CARTESIAN_POINT ( 'NONE',  ( 18.39999999999999858, -9.600000000000003197, -40.20018939122204671 ) ) ;
#44336 = AXIS2_PLACEMENT_3D ( 'NONE', #60541, #157109, #115385 ) ;
#44337 = ORIENTED_EDGE ( 'NONE', *, *, #207459, .T. ) ;
#44340 = ORIENTED_EDGE ( 'NONE', *, *, #173932, .T. ) ;
#44339 = SURFACE_SIDE_STYLE ('',( #26061 ) ) ;
#44338 = FILL_AREA_STYLE_COLOUR ( '', #69842 ) ;
#44341 = EDGE_CURVE ( 'NONE', #104038, #43171, #46437, .T. ) ;
#44342 = ORIENTED_EDGE ( 'NONE', *, *, #141917, .F. ) ;
#44343 = DIRECTION ( 'NONE',  ( 0.000000000000000000, 6.982962677686266711E-15, -1.000000000000000000 ) ) ;
#44344 = VECTOR ( 'NONE', #42407, 1000.000000000000000 ) ;
#44345 = DIRECTION ( 'NONE',  ( 0.000000000000000000, 0.9126074666063545004, 0.4088369013363783999 ) ) ;
#44346 = CYLINDRICAL_SURFACE ( 'NONE', #50133, 0.09999999999999939493 ) ;
#44347 = VERTEX_POINT ( 'NONE', #239524 ) ;
#44348 = CARTESIAN_POINT ( 'NONE',  ( -16.87036670365548474, 66.01058118071036063, -115.5435473672223168 ) ) ;
#44349 = AXIS2_PLACEMENT_3D ( 'NONE', #165530, #243770, #148527 ) ;
#44350 = EDGE_CURVE ( 'NONE', #24982, #156671, #26918, .T. ) ;
#44351 = TOROIDAL_SURFACE ( 'NONE', #210932, 12.77499999999999858, 0.1000000000000000056 ) ;
#44353 = CARTESIAN_POINT ( 'NONE',  ( -17.11825945287482753, 44.22674245267958781, -235.2580479164738279 ) ) ;
#44352 = DIRECTION ( 'NONE',  ( -1.000000000000000000, 0.000000000000000000, 0.000000000000000000 ) ) ;
#44354 = AXIS2_PLACEMENT_3D ( 'NONE', #208005, #226225, #45059 ) ;
#44356 = ORIENTED_EDGE ( 'NONE', *, *, #157656, .T. ) ;
#44355 = LINE ( 'NONE', #243819, #230710 ) ;
#44357 = EDGE_CURVE ( 'NONE', #209494, #99525, #45163, .T. ) ;
#44358 = EDGE_CURVE ( 'NONE', #92778, #212831, #108786, .T. ) ;
#44359 = ORIENTED_EDGE ( 'NONE', *, *, #184474, .F. ) ;
#44360 = FACE_OUTER_BOUND ( 'NONE', #224035, .T. ) ;
#44361 = CARTESIAN_POINT ( 'NONE',  ( -20.94999999999999929, -1.261786168553869603, -175.5864989635454378 ) ) ;
#44362 = CIRCLE ( 'NONE', #198279, 0.2000000000000048683 ) ;
#44363 = DIRECTION ( 'NONE',  ( 0.000000000000000000, 0.000000000000000000, -1.000000000000000000 ) ) ;
#44364 = VERTEX_POINT ( 'NONE', #162568 ) ;
#44366 = AXIS2_PLACEMENT_3D ( 'NONE', #42528, #162506, #85472 ) ;
#44365 = DIRECTION ( 'NONE',  ( -0.000000000000000000, -0.8660254037844468122, -0.4999999999999860112 ) ) ;
#44367 = ORIENTED_EDGE ( 'NONE', *, *, #162221, .T. ) ;
#44368 = CONICAL_SURFACE ( 'NONE', #248353, 6.250000000000000888, 0.7853981633974431720 ) ;
#44369 = ADVANCED_FACE ( 'NONE', ( #183403 ), #125980, .F. ) ;
#44370 = DIRECTION ( 'NONE',  ( 0.000000000000000000, -6.467318590049456648E-15, 1.000000000000000000 ) ) ;
#44371 = CARTESIAN_POINT ( 'NONE',  ( -21.14999999999999858, 11.75000000001115552, -100.6000000000000369 ) ) ;
#44372 = CARTESIAN_POINT ( 'NONE',  ( -21.05000000000000071, 76.10000000001203091, -114.6726782920691079 ) ) ;
#44374 = ORIENTED_EDGE ( 'NONE', *, *, #81196, .F. ) ;
#44373 = AXIS2_PLACEMENT_3D ( 'NONE', #247367, #144399, #67451 ) ;
#44375 = CARTESIAN_POINT ( 'NONE',  ( -20.54999999999999361, 11.65000000001115232, -88.35000000000003695 ) ) ;
#44376 = CIRCLE ( 'NONE', #131844, 0.1000000000000124678 ) ;
#44377 = DIRECTION ( 'NONE',  ( 1.000000000000000000, 0.000000000000000000, 0.000000000000000000 ) ) ;
#44378 = EDGE_LOOP ( 'NONE', ( #87354, #194189, #61152, #146985 ) ) ;
#44379 = EDGE_LOOP ( 'NONE', ( #89694, #160178, #165545, #11415 ) ) ;
#44380 = EDGE_LOOP ( 'NONE', ( #99270, #80910, #31225 ) ) ;
#44381 = DIRECTION ( 'NONE',  ( -1.000000000000000000, 0.000000000000000000, 0.000000000000000000 ) ) ;
#44382 = ORIENTED_EDGE ( 'NONE', *, *, #53541, .T. ) ;
#44384 = ORIENTED_EDGE ( 'NONE', *, *, #158548, .F. ) ;
#44383 = CARTESIAN_POINT ( 'NONE',  ( 15.07585980824111793, 66.58236703690626257, -185.3741590187921418 ) ) ;
#44385 = EDGE_CURVE ( 'NONE', #87224, #110507, #121491, .T. ) ;
#44386 = ADVANCED_FACE ( 'NONE', ( #163838 ), #64726, .F. ) ;
#44387 = EDGE_LOOP ( 'NONE', ( #148783, #78997, #143379, #241, #128822, #42108 ) ) ;
#44388 = AXIS2_PLACEMENT_3D ( 'NONE', #32176, #191250, #77669 ) ;
#44389 = AXIS2_PLACEMENT_3D ( 'NONE', #144082, #223619, #123259 ) ;
#44391 = VERTEX_POINT ( 'NONE', #105100 ) ;
#44390 = ORIENTED_EDGE ( 'NONE', *, *, #68038, .T. ) ;
#44392 = AXIS2_PLACEMENT_3D ( 'NONE', #9493, #89026, #168634 ) ;
#44393 = CIRCLE ( 'NONE', #190144, 0.09999999999999600875 ) ;
#44395 = EDGE_CURVE ( 'NONE', #206656, #115602, #106398, .T. ) ;
#44394 = CARTESIAN_POINT ( 'NONE',  ( -16.27683809663750480, 66.65000000001234071, -160.7731074845244166 ) ) ;
#44396 = VERTEX_POINT ( 'NONE', #200394 ) ;
#44397 = DIRECTION ( 'NONE',  ( 0.000000000000000000, 0.000000000000000000, -1.000000000000000000 ) ) ;
#44398 = CARTESIAN_POINT ( 'NONE',  ( -23.15000000000000213, 1.148907358139439339E-11, -201.0000000000015064 ) ) ;
#44399 = VECTOR ( 'NONE', #241934, 1000.000000000000000 ) ;
#44400 = CARTESIAN_POINT ( 'NONE',  ( -18.31572283045056437, 87.00870235977620837, -199.4106618404662754 ) ) ;
#44401 = EDGE_LOOP ( 'NONE', ( #149393, #59549, #55896 ) ) ;
#44402 = PLANE ( 'NONE',  #95550 ) ;
#44404 = ORIENTED_EDGE ( 'NONE', *, *, #66839, .T. ) ;
#44403 = DIRECTION ( 'NONE',  ( 1.186688945009010077E-16, -1.000000000000000000, -0.000000000000000000 ) ) ;
#44405 = DIRECTION ( 'NONE',  ( 2.952720810173289112E-16, -1.000000000000000000, 0.000000000000000000 ) ) ;
#44407 = ORIENTED_EDGE ( 'NONE', *, *, #225083, .T. ) ;
#44406 = DIRECTION ( 'NONE',  ( -1.000000000000000000, -1.836970198721029934E-16, -3.186635328391151676E-31 ) ) ;
#44408 = AXIS2_PLACEMENT_3D ( 'NONE', #130738, #233708, #55032 ) ;
#44409 = ORIENTED_EDGE ( 'NONE', *, *, #55888, .T. ) ;
#44410 = CIRCLE ( 'NONE', #6978, 11.64999999999998970 ) ;
#44411 = AXIS2_PLACEMENT_3D ( 'NONE', #219007, #156517, #121246 ) ;
#44412 = ORIENTED_EDGE ( 'NONE', *, *, #1584, .T. ) ;
#44413 = ORIENTED_EDGE ( 'NONE', *, *, #167454, .T. ) ;
#44414 = DIRECTION ( 'NONE',  ( -1.000000000000000000, -0.000000000000000000, -0.000000000000000000 ) ) ;
#44416 = ADVANCED_FACE ( 'NONE', ( #167711 ), #89416, .T. ) ;
#44415 = DIRECTION ( 'NONE',  ( 0.000000000000000000, -6.982962677686266711E-15, 1.000000000000000000 ) ) ;
#44418 = EDGE_LOOP ( 'NONE', ( #244373, #105267, #123980, #77305 ) ) ;
#44417 = ORIENTED_EDGE ( 'NONE', *, *, #130630, .T. ) ;
#44419 = ORIENTED_EDGE ( 'NONE', *, *, #159199, .F. ) ;
#44420 = CARTESIAN_POINT ( 'NONE',  ( -18.34374000495060386, 13.17878477875124688, -207.5966336730521391 ) ) ;
#44421 = EDGE_LOOP ( 'NONE', ( #104667, #242224, #191629, #155316 ) ) ;
#44422 = ORIENTED_EDGE ( 'NONE', *, *, #42262, .T. ) ;
#44423 = CARTESIAN_POINT ( 'NONE',  ( 6.100000000000061817, 64.35000000001120668, -22.12310748452479103 ) ) ;
#44424 = CIRCLE ( 'NONE', #198346, 0.09999999999999108213 ) ;
#44427 = ADVANCED_FACE ( 'NONE', ( #51548 ), #30766, .T. ) ;
#44426 = ORIENTED_EDGE ( 'NONE', *, *, #59909, .T. ) ;
#44425 = CARTESIAN_POINT ( 'NONE',  ( -23.25000000000000000, -1.851617760457748618, -112.1031897196037050 ) ) ;
#44428 = SPHERICAL_SURFACE ( 'NONE', #27625, 0.1000000000000000056 ) ;
#44430 = FACE_OUTER_BOUND ( 'NONE', #207425, .T. ) ;
#44429 = DIRECTION ( 'NONE',  ( 1.000000000000000000, 0.000000000000000000, 0.000000000000000000 ) ) ;
#44431 = EDGE_LOOP ( 'NONE', ( #156692, #168723, #5693, #97116 ) ) ;
#44432 = ADVANCED_FACE ( 'NONE', ( #29494 ), #247208, .F. ) ;
#44434 = ORIENTED_EDGE ( 'NONE', *, *, #22375, .F. ) ;
#44433 = ORIENTED_EDGE ( 'NONE', *, *, #254102, .T. ) ;
#44435 = DIRECTION ( 'NONE',  ( 0.000000000000000000, 0.000000000000000000, 1.000000000000000000 ) ) ;
#44436 = PRESENTATION_STYLE_ASSIGNMENT (( #43149 ) ) ;
#44437 = ADVANCED_FACE ( 'NONE', ( #152001 ), #227644, .T. ) ;
#44438 = ORIENTED_EDGE ( 'NONE', *, *, #163631, .T. ) ;
#44439 = AXIS2_PLACEMENT_3D ( 'NONE', #220870, #100885, #4388 ) ;
#44440 = VECTOR ( 'NONE', #193606, 1000.000000000000000 ) ;
#44441 = AXIS2_PLACEMENT_3D ( 'NONE', #176772, #198882, #151108 ) ;
#44442 = AXIS2_PLACEMENT_3D ( 'NONE', #31029, #231772, #90960 ) ;
#44443 = ADVANCED_FACE ( 'NONE', ( #111564 ), #129827, .F. ) ;
#44444 = DIRECTION ( 'NONE',  ( -1.000000000000000000, 0.000000000000000000, 0.000000000000000000 ) ) ;
#44445 = EDGE_CURVE ( 'NONE', #256245, #212201, #213024, .T. ) ;
#44446 = ORIENTED_EDGE ( 'NONE', *, *, #193634, .F. ) ;
#44447 = ORIENTED_EDGE ( 'NONE', *, *, #106016, .F. ) ;
#44448 = DIRECTION ( 'NONE',  ( 1.000000000000000000, 0.000000000000000000, 0.000000000000000000 ) ) ;
#44449 = VERTEX_POINT ( 'NONE', #148124 ) ;
#44450 = DIRECTION ( 'NONE',  ( -0.5932847527679299127, 0.8049926720990051576, 6.366092712777055223E-16 ) ) ;
#44451 = DIRECTION ( 'NONE',  ( 0.000000000000000000, 0.2617529984165083423, 0.9651348961777143076 ) ) ;
#44452 = VERTEX_POINT ( 'NONE', #245945 ) ;
#44453 = DIRECTION ( 'NONE',  ( 0.000000000000000000, 0.000000000000000000, 1.000000000000000000 ) ) ;
#44454 = DIRECTION ( 'NONE',  ( 0.000000000000000000, 0.000000000000000000, -1.000000000000000000 ) ) ;
#44456 = DIRECTION ( 'NONE',  ( -1.000000000000000000, 0.000000000000000000, 0.000000000000000000 ) ) ;
#44455 = CARTESIAN_POINT ( 'NONE',  ( -18.59999999999999787, 12.87592094156238609, -205.3750039893633073 ) ) ;
#44457 = DIRECTION ( 'NONE',  ( 0.000000000000000000, 0.000000000000000000, 1.000000000000000000 ) ) ;
#44458 = PLANE ( 'NONE',  #224158 ) ;
#44459 = LINE ( 'NONE', #82248, #36376 ) ;
#44460 = CARTESIAN_POINT ( 'NONE',  ( 23.14999999999999858, 4.813084112160680661, -179.4415177565237798 ) ) ;
#44461 = CIRCLE ( 'NONE', #202654, 0.2000000000000005107 ) ;
#44462 = AXIS2_PLACEMENT_3D ( 'NONE', #61167, #79427, #238518 ) ;
#44463 = AXIS2_PLACEMENT_3D ( 'NONE', #125166, #79582, #23524 ) ;
#44464 = ORIENTED_EDGE ( 'NONE', *, *, #6082, .F. ) ;
#44465 = EDGE_CURVE ( 'NONE', #252068, #81327, #127274, .T. ) ;
#44466 = EDGE_CURVE ( 'NONE', #107194, #151151, #154797, .T. ) ;
#44468 = ORIENTED_EDGE ( 'NONE', *, *, #250746, .F. ) ;
#44467 = ORIENTED_EDGE ( 'NONE', *, *, #148301, .T. ) ;
#44469 = ORIENTED_EDGE ( 'NONE', *, *, #231307, .T. ) ;
#44470 = EDGE_CURVE ( 'NONE', #73222, #184550, #166433, .T. ) ;
#44471 = CARTESIAN_POINT ( 'NONE',  ( -18.50000000000000000, 70.05000000001213323, -126.2174051794894893 ) ) ;
#44472 = DIRECTION ( 'NONE',  ( 1.000000000000000000, 0.000000000000000000, 0.000000000000000000 ) ) ;
#44474 = CARTESIAN_POINT ( 'NONE',  ( 21.14999999999999858, 6.540656951701244282, 0.000000000000000000 ) ) ;
#44473 = DIRECTION ( 'NONE',  ( 0.000000000000000000, 0.000000000000000000, 1.000000000000000000 ) ) ;
#44475 = DIRECTION ( 'NONE',  ( 0.000000000000000000, -5.204170427930272346E-14, -1.000000000000000000 ) ) ;
#44476 = ORIENTED_EDGE ( 'NONE', *, *, #87882, .F. ) ;
#44477 = DIRECTION ( 'NONE',  ( 0.000000000000000000, 1.072103779144463779E-14, -1.000000000000000000 ) ) ;
#44478 = EDGE_CURVE ( 'NONE', #199540, #64185, #171567, .T. ) ;
#44479 = CARTESIAN_POINT ( 'NONE',  ( -20.85000000000000142, 77.25000000001136868, -28.22262673010922995 ) ) ;
#44480 = CARTESIAN_POINT ( 'NONE',  ( -22.59999999999999787, 1.115600667400684642E-11, -67.00000000000004263 ) ) ;
#44481 = ADVANCED_FACE ( 'NONE', ( #208114 ), #88096, .T. ) ;
#44482 = DIRECTION ( 'NONE',  ( 1.000000000000000000, 0.000000000000000000, 0.000000000000000000 ) ) ;
#44483 = ORIENTED_EDGE ( 'NONE', *, *, #241530, .T. ) ;
#44484 = AXIS2_PLACEMENT_3D ( 'NONE', #33888, #114658, #14303 ) ;
#44485 = DIRECTION ( 'NONE',  ( 0.000000000000000000, 2.362176648138630895E-15, 1.000000000000000000 ) ) ;
#44486 = FACE_OUTER_BOUND ( 'NONE', #89155, .T. ) ;
#44487 = ORIENTED_EDGE ( 'NONE', *, *, #39021, .T. ) ;
#44488 = CARTESIAN_POINT ( 'NONE',  ( 18.50000000000000000, -11.78281952876889527, -191.5407366062592871 ) ) ;
#44489 = DIRECTION ( 'NONE',  ( 0.000000000000000000, 0.000000000000000000, 1.000000000000000000 ) ) ;
#44490 = LINE ( 'NONE', #165731, #186221 ) ;
#44491 = ADVANCED_FACE ( 'NONE', ( #50281 ), #160685, .F. ) ;
#44492 = CYLINDRICAL_SURFACE ( 'NONE', #31237, 0.09999999999999939493 ) ;
#44493 = CARTESIAN_POINT ( 'NONE',  ( -23.25000000000000000, -3.275978944802464099, -228.2735455795363748 ) ) ;
#44494 = AXIS2_PLACEMENT_3D ( 'NONE', #159349, #255812, #194635 ) ;
#44495 = ORIENTED_EDGE ( 'NONE', *, *, #4526, .F. ) ;
#44496 = DIRECTION ( 'NONE',  ( 0.000000000000000000, 0.000000000000000000, 1.000000000000000000 ) ) ;
#44497 = CARTESIAN_POINT ( 'NONE',  ( -18.50000000000000000, 5.950000000011100632, -77.30570230503489881 ) ) ;
#44498 = DIRECTION ( 'NONE',  ( 1.000000000000000000, 0.000000000000000000, 0.000000000000000000 ) ) ;
#44500 = CARTESIAN_POINT ( 'NONE',  ( 20.85000000000000142, 76.32388570108204817, -69.56551789521031992 ) ) ;
#44499 = DIRECTION ( 'NONE',  ( 1.000000000000000000, 0.000000000000000000, 0.000000000000000000 ) ) ;
#44501 = LINE ( 'NONE', #64049, #58087 ) ;
#44502 = AXIS2_PLACEMENT_3D ( 'NONE', #71197, #42961, #230245 ) ;
#44504 = EDGE_CURVE ( 'NONE', #53190, #163587, #129815, .T. ) ;
#44503 = DIRECTION ( 'NONE',  ( 0.000000000000000000, -1.000000000000000000, 0.000000000000000000 ) ) ;
#44505 = DIRECTION ( 'NONE',  ( -1.000000000000000000, -2.952720810173289112E-16, 0.000000000000000000 ) ) ;
#44506 = AXIS2_PLACEMENT_3D ( 'NONE', #67834, #88657, #187801 ) ;
#44508 = ORIENTED_EDGE ( 'NONE', *, *, #165027, .T. ) ;
#44507 = FACE_OUTER_BOUND ( 'NONE', #191956, .T. ) ;
#44509 = AXIS2_PLACEMENT_3D ( 'NONE', #216327, #115966, #96366 ) ;
#44510 = AXIS2_PLACEMENT_3D ( 'NONE', #39420, #40711, #22412 ) ;
#44511 = EDGE_CURVE ( 'NONE', #239535, #108899, #217284, .T. ) ;
#44512 = CIRCLE ( 'NONE', #190253, 0.09999999999999939493 ) ;
#44513 = CARTESIAN_POINT ( 'NONE',  ( -18.59999999999999787, 11.64999999999999680, -21.35000000000000142 ) ) ;
#44514 = DIRECTION ( 'NONE',  ( -1.000000000000000000, 0.000000000000000000, 0.000000000000000000 ) ) ;
#44515 = CARTESIAN_POINT ( 'NONE',  ( 13.12220780326572189, 9.430633469083952392, -149.2317657948241276 ) ) ;
#44516 = ORIENTED_EDGE ( 'NONE', *, *, #129794, .T. ) ;
#44517 = DIRECTION ( 'NONE',  ( 1.000000000000000000, -0.000000000000000000, 0.000000000000000000 ) ) ;
#44518 = VECTOR ( 'NONE', #11989, 1000.000000000000000 ) ;
#44519 = DIRECTION ( 'NONE',  ( -1.000000000000000000, 0.000000000000000000, 0.000000000000000000 ) ) ;
#44520 = CARTESIAN_POINT ( 'NONE',  ( -18.50000000000000000, 6.440012694424540385, -187.5719980452876712 ) ) ;
#44521 = ORIENTED_EDGE ( 'NONE', *, *, #71062, .F. ) ;
#44522 = DIRECTION ( 'NONE',  ( 1.000000000000000000, 0.000000000000000000, 0.000000000000000000 ) ) ;
#44525 = ORIENTED_EDGE ( 'NONE', *, *, #3196, .T. ) ;
#44524 = DIRECTION ( 'NONE',  ( -1.000000000000000000, 0.000000000000000000, 0.000000000000000000 ) ) ;
#44523 = AXIS2_PLACEMENT_3D ( 'NONE', #238990, #219397, #61626 ) ;
#44527 = FACE_OUTER_BOUND ( 'NONE', #109772, .T. ) ;
#44526 = DIRECTION ( 'NONE',  ( 0.000000000000000000, -0.3738317757009345654, 0.9274965247785492695 ) ) ;
#44528 = VECTOR ( 'NONE', #60033, 1000.000000000000000 ) ;
#44529 = CARTESIAN_POINT ( 'NONE',  ( 21.10000000000000142, -11.65000000000000036, 11.89999999999999680 ) ) ;
#44531 = ORIENTED_EDGE ( 'NONE', *, *, #167281, .T. ) ;
#44530 = AXIS2_PLACEMENT_3D ( 'NONE', #5600, #108584, #124304 ) ;
#44532 = DIRECTION ( 'NONE',  ( 1.000000000000000000, -0.000000000000000000, -0.000000000000000000 ) ) ;
#44533 = DIRECTION ( 'NONE',  ( 0.000000000000000000, 0.000000000000000000, 1.000000000000000000 ) ) ;
#44534 = DIRECTION ( 'NONE',  ( 0.000000000000000000, 0.000000000000000000, 1.000000000000000000 ) ) ;
#44535 = DIRECTION ( 'NONE',  ( 0.000000000000000000, 6.982962677686266711E-15, -1.000000000000000000 ) ) ;
#44536 = DIRECTION ( 'NONE',  ( 0.000000000000000000, -0.4999999999999689138, -0.8660254037844565822 ) ) ;
#44537 = EDGE_LOOP ( 'NONE', ( #51468, #82506, #168217, #104552 ) ) ;
#44538 = CARTESIAN_POINT ( 'NONE',  ( -18.50000000000000000, 64.25000000001229239, -157.8731074845244393 ) ) ;
#44539 = AXIS2_PLACEMENT_3D ( 'NONE', #52427, #248074, #9461 ) ;
#44540 = DIRECTION ( 'NONE',  ( 1.000000000000000000, 7.492892343619937423E-30, -1.073024830501117725E-15 ) ) ;
#44541 = AXIS2_PLACEMENT_3D ( 'NONE', #225964, #23975, #26536 ) ;
#44542 = AXIS2_PLACEMENT_3D ( 'NONE', #214530, #112877, #115432 ) ;
#44543 = CARTESIAN_POINT ( 'NONE',  ( 18.49999999999998934, 6.550000000011156231, -188.6499999999999488 ) ) ;
#44544 = DIRECTION ( 'NONE',  ( 0.000000000000000000, 0.000000000000000000, -1.000000000000000000 ) ) ;
#44545 = ORIENTED_EDGE ( 'NONE', *, *, #61847, .T. ) ;
#44546 = EDGE_LOOP ( 'NONE', ( #37727, #144223, #117202, #120218 ) ) ;
#44547 = DIRECTION ( 'NONE',  ( 1.000000000000000000, -7.304098846218134667E-16, -5.100424963727256530E-30 ) ) ;
#44548 = LINE ( 'NONE', #41989, #144425 ) ;
#44549 = CARTESIAN_POINT ( 'NONE',  ( 23.14999999999999858, 0.000000000000000000, -35.50000000000000711 ) ) ;
#44550 = DIRECTION ( 'NONE',  ( 0.000000000000000000, 6.982962677686266711E-15, -1.000000000000000000 ) ) ;
#44551 = EDGE_CURVE ( 'NONE', #177863, #144130, #39192, .T. ) ;
#44552 = TOROIDAL_SURFACE ( 'NONE', #144473, 11.70000000000000462, 0.1000000000000000056 ) ;
#44554 = CARTESIAN_POINT ( 'NONE',  ( 23.14999999999999503, 11.65000000001116298, -112.6500000000000341 ) ) ;
#44553 = CARTESIAN_POINT ( 'NONE',  ( 23.14999999999999858, 5.600000000011153389, -88.09473398108696074 ) ) ;
#44555 = DIRECTION ( 'NONE',  ( 1.000000000000000000, -0.000000000000000000, 0.000000000000000000 ) ) ;
#44556 = CARTESIAN_POINT ( 'NONE',  ( -16.78493832629887450, 66.05416425680742520, -56.85915846542017249 ) ) ;
#44557 = CYLINDRICAL_SURFACE ( 'NONE', #163878, 0.09999999999998898659 ) ;
#44558 = DIRECTION ( 'NONE',  ( 1.020425574104004196E-15, 6.982962677686266711E-15, -1.000000000000000000 ) ) ;
#44560 = ORIENTED_EDGE ( 'NONE', *, *, #2039, .F. ) ;
#44559 = DIRECTION ( 'NONE',  ( -1.000000000000000000, -7.304098846218134667E-16, 0.000000000000000000 ) ) ;
#44561 = CARTESIAN_POINT ( 'NONE',  ( 20.95496329884391784, 65.43256679391959096, -195.9487975522395971 ) ) ;
#44562 = LINE ( 'NONE', #142360, #232571 ) ;
#44563 = PLANE ( 'NONE',  #242716 ) ;
#44564 = ORIENTED_EDGE ( 'NONE', *, *, #180396, .F. ) ;
#44565 = CARTESIAN_POINT ( 'NONE',  ( -16.97683809663752186, 66.05000000001157900, -56.12074346632790878 ) ) ;
#44566 = CARTESIAN_POINT ( 'NONE',  ( 20.95512820512820085, 65.37615131630018084, -124.3229454650999486 ) ) ;
#44567 = DIRECTION ( 'NONE',  ( 1.000000000000000000, 0.000000000000000000, 0.000000000000000000 ) ) ;
#44568 = DIRECTION ( 'NONE',  ( 0.000000000000000000, -0.3350715337780675318, -0.9421926911474177713 ) ) ;
#44569 = ORIENTED_EDGE ( 'NONE', *, *, #215736, .T. ) ;
#44570 = AXIS2_PLACEMENT_3D ( 'NONE', #240617, #141511, #183221 ) ;
#44572 = EDGE_CURVE ( 'NONE', #133004, #168057, #225661, .T. ) ;
#44571 = EDGE_LOOP ( 'NONE', ( #186626, #80373, #13654 ) ) ;
#44573 = EDGE_CURVE ( 'NONE', #88949, #22117, #34613, .T. ) ;
#44574 = AXIS2_PLACEMENT_3D ( 'NONE', #141239, #219475, #62980 ) ;
#44575 = VECTOR ( 'NONE', #220549, 1000.000000000000000 ) ;
#44576 = VECTOR ( 'NONE', #150954, 1000.000000000000000 ) ;
#44577 = FACE_OUTER_BOUND ( 'NONE', #175414, .T. ) ;
#44578 = ORIENTED_EDGE ( 'NONE', *, *, #200265, .T. ) ;
#44579 = CARTESIAN_POINT ( 'NONE',  ( 18.69999999999999929, 11.75000000000000000, 16.39999999999999858 ) ) ;
#44580 = ORIENTED_EDGE ( 'NONE', *, *, #148183, .T. ) ;
#44581 = AXIS2_PLACEMENT_3D ( 'NONE', #149943, #131637, #52083 ) ;
#44582 = DIRECTION ( 'NONE',  ( 1.000000000000000000, 0.000000000000000000, 0.000000000000000000 ) ) ;
#44583 = DIRECTION ( 'NONE',  ( 0.000000000000000000, -2.428612866367527723E-14, -1.000000000000000000 ) ) ;
#44584 = EDGE_CURVE ( 'NONE', #151116, #80866, #38253, .T. ) ;
#44585 = ADVANCED_FACE ( 'NONE', ( #194970 ), #15045, .F. ) ;
#44586 = ORIENTED_EDGE ( 'NONE', *, *, #57388, .F. ) ;
#44587 = EDGE_CURVE ( 'NONE', #163063, #24254, #75034, .T. ) ;
#44588 = LINE ( 'NONE', #147532, #257518 ) ;
#44589 = CARTESIAN_POINT ( 'NONE',  ( -21.37071067811865532, 67.92928932189363422, -157.7731074845244166 ) ) ;
#44590 = DIRECTION ( 'NONE',  ( 0.000000000000000000, 1.000000000000000000, 6.982962677686266711E-15 ) ) ;
#44591 = AXIS2_PLACEMENT_3D ( 'NONE', #96478, #37842, #157808 ) ;
#44592 = CARTESIAN_POINT ( 'NONE',  ( 18.59999999999998721, 18.51212680383529374, -217.3114114048737520 ) ) ;
#44593 = DIRECTION ( 'NONE',  ( 1.000000000000000000, -0.000000000000000000, 0.000000000000000000 ) ) ;
#44594 = DIRECTION ( 'NONE',  ( 1.000000000000000000, 0.000000000000000000, 0.000000000000000000 ) ) ;
#44595 = ADVANCED_FACE ( 'NONE', ( #174147 ), #16333, .F. ) ;
#44596 = CARTESIAN_POINT ( 'NONE',  ( 21.10710606213542562, 11.18076043846704692, -211.0928915918022426 ) ) ;
#44597 = VERTEX_POINT ( 'NONE', #155844 ) ;
#44599 = CARTESIAN_POINT ( 'NONE',  ( -20.94999999999999929, 1.261786168565025568, -8.086498963545480478 ) ) ;
#44598 = DIRECTION ( 'NONE',  ( 0.000000000000000000, 0.9126074666063769270, 0.4088369013363280513 ) ) ;
#44600 = ORIENTED_EDGE ( 'NONE', *, *, #89681, .F. ) ;
#44602 = ORIENTED_EDGE ( 'NONE', *, *, #82280, .F. ) ;
#44601 = DIRECTION ( 'NONE',  ( -0.000000000000000000, 0.9770955615653313941, 0.2128009952263603954 ) ) ;
#44603 = AXIS2_PLACEMENT_3D ( 'NONE', #167442, #27938, #107437 ) ;
#44604 = ORIENTED_EDGE ( 'NONE', *, *, #231747, .T. ) ;
#44605 = CYLINDRICAL_SURFACE ( 'NONE', #115694, 0.09999999999999976963 ) ;
#44606 = ADVANCED_FACE ( 'NONE', ( #119277 ), #791, .F. ) ;
#44607 = DIRECTION ( 'NONE',  ( 0.000000000000000000, -1.000000000000000000, 0.000000000000000000 ) ) ;
#44608 = CYLINDRICAL_SURFACE ( 'NONE', #205533, 0.09999999999998898659 ) ;
#44609 = DIRECTION ( 'NONE',  ( 0.000000000000000000, -7.086529944415894657E-15, 1.000000000000000000 ) ) ;
#44610 = ORIENTED_EDGE ( 'NONE', *, *, #11079, .F. ) ;
#44611 = DIRECTION ( 'NONE',  ( 1.000000000000000000, -0.000000000000000000, -0.000000000000000000 ) ) ;
#44612 = LINE ( 'NONE', #162007, #102016 ) ;
#44613 = ORIENTED_EDGE ( 'NONE', *, *, #217459, .T. ) ;
#44615 = ADVANCED_FACE ( 'NONE', ( #93272 ), #88277, .T. ) ;
#44614 = DIRECTION ( 'NONE',  ( 1.000000000000000000, 0.000000000000000000, 0.000000000000000000 ) ) ;
#44616 = LINE ( 'NONE', #8064, #114164 ) ;
#44617 = VECTOR ( 'NONE', #124060, 1000.000000000000227 ) ;
#44618 = ORIENTED_EDGE ( 'NONE', *, *, #129281, .T. ) ;
#44619 = AXIS2_PLACEMENT_3D ( 'NONE', #246839, #12121, #130752 ) ;
#44620 = CARTESIAN_POINT ( 'NONE',  ( -16.87401514999234919, 9.950000000011137047, -146.7199820074679337 ) ) ;
#44621 = CIRCLE ( 'NONE', #15603, 0.09999999999999939493 ) ;
#44622 = TOROIDAL_SURFACE ( 'NONE', #240263, 0.2000000000000000111, 0.1000000000000000056 ) ;
#44623 = ORIENTED_EDGE ( 'NONE', *, *, #205890, .F. ) ;
#44624 = DIRECTION ( 'NONE',  ( -0.000000000000000000, 0.9983803033886520240, 0.05689261644170767740 ) ) ;
#44625 = EDGE_LOOP ( 'NONE', ( #203191, #58081, #207072, #28467 ) ) ;
#44626 = CARTESIAN_POINT ( 'NONE',  ( -23.15000000000000213, -11.48912529306489994, -164.4000000000000057 ) ) ;
#44627 = DIRECTION ( 'NONE',  ( 0.000000000000000000, -0.9955484899852913294, 0.09425075112701486457 ) ) ;
#44628 = CARTESIAN_POINT ( 'NONE',  ( 23.14999999999998437, 36.65892442174472876, -249.5511627012454596 ) ) ;
#44629 = CARTESIAN_POINT ( 'NONE',  ( -21.46681500593131275, 6.700443717232317020, -199.5407148005083116 ) ) ;
#44630 = CIRCLE ( 'NONE', #202292, 0.1000000000000028644 ) ;
#44631 = AXIS2_PLACEMENT_3D ( 'NONE', #246888, #29181, #31739 ) ;
#44632 = CARTESIAN_POINT ( 'NONE',  ( -20.64999999999999858, -9.399999999988846611, -191.1060308773475356 ) ) ;
#44633 = DIRECTION ( 'NONE',  ( -3.265361837132813093E-16, 1.000000000000000000, -0.000000000000000000 ) ) ;
#44634 = DIRECTION ( 'NONE',  ( 1.000000000000000000, 0.000000000000000000, 0.000000000000000000 ) ) ;
#44635 = ORIENTED_EDGE ( 'NONE', *, *, #30774, .T. ) ;
#44637 = CARTESIAN_POINT ( 'NONE',  ( 20.04999999999999716, 67.25000000001260503, -194.2731074845244166 ) ) ;
#44636 = CARTESIAN_POINT ( 'NONE',  ( -20.64999999999999858, 76.00000000001237765, -170.0231074845243597 ) ) ;
#44638 = EDGE_CURVE ( 'NONE', #12719, #203190, #214501, .T. ) ;
#44639 = VECTOR ( 'NONE', #234147, 1000.000000000000000 ) ;
#44640 = ADVANCED_FACE ( 'NONE', ( #198791 ), #158424, .T. ) ;
#44641 = ORIENTED_EDGE ( 'NONE', *, *, #178076, .F. ) ;
#44642 = DIRECTION ( 'NONE',  ( -0.8049926720990043805, -0.2801448344544986702, -0.5229776951222359083 ) ) ;
#44643 = CYLINDRICAL_SURFACE ( 'NONE', #42170, 0.5000000000000004441 ) ;
#44645 = VERTEX_POINT ( 'NONE', #217054 ) ;
#44644 = CARTESIAN_POINT ( 'NONE',  ( 21.13461538461538325, 10.61458296203669427, -146.3500000000000227 ) ) ;
#44647 = ORIENTED_EDGE ( 'NONE', *, *, #215653, .T. ) ;
#44646 = CARTESIAN_POINT ( 'NONE',  ( 21.05000000000000071, 67.22371711014383777, -57.34689234345615461 ) ) ;
#44649 = EDGE_CURVE ( 'NONE', #195497, #142060, #121655, .T. ) ;
#44648 = CARTESIAN_POINT ( 'NONE',  ( 18.52130828395272033, 46.94588606482535909, -255.3320774683811010 ) ) ;
#44650 = ADVANCED_FACE ( 'NONE', ( #117978 ), #159077, .F. ) ;
#44651 = CARTESIAN_POINT ( 'NONE',  ( -18.69999999999999929, 11.49641995933507843, 1.885425182446135661 ) ) ;
#44652 = CARTESIAN_POINT ( 'NONE',  ( 22.39999999999999503, 11.75000000001116263, -167.5999999999999659 ) ) ;
#44654 = VERTEX_POINT ( 'NONE', #73743 ) ;
#44653 = CARTESIAN_POINT ( 'NONE',  ( 21.05000000000000071, 67.22371711014456253, -157.8468923434562612 ) ) ;
#44655 = EDGE_CURVE ( 'NONE', #86816, #48432, #150676, .T. ) ;
#44656 = EDGE_CURVE ( 'NONE', #242308, #12289, #140088, .T. ) ;
#44657 = VECTOR ( 'NONE', #53746, 1000.000000000000000 ) ;
#44658 = ADVANCED_FACE ( 'NONE', ( #24037 ), #162263, .T. ) ;
#44659 = CARTESIAN_POINT ( 'NONE',  ( -23.15000000000000213, -8.999999999988844479, -57.10603087734755690 ) ) ;
#44660 = VERTEX_POINT ( 'NONE', #124410 ) ;
#44661 = VERTEX_POINT ( 'NONE', #142655 ) ;
#44662 = ADVANCED_FACE ( 'NONE', ( #203933 ), #80092, .T. ) ;
#44663 = DIRECTION ( 'NONE',  ( -0.000000000000000000, 7.272083257015735086E-15, -1.000000000000000000 ) ) ;
#44664 = DIRECTION ( 'NONE',  ( 0.000000000000000000, 0.000000000000000000, -1.000000000000000000 ) ) ;
#44665 = TOROIDAL_SURFACE ( 'NONE', #73911, 11.65000000000000036, 0.1000000000000000056 ) ;
#44666 = ORIENTED_EDGE ( 'NONE', *, *, #139703, .F. ) ;
#44667 = CARTESIAN_POINT ( 'NONE',  ( 20.94999999999999929, 68.87972903831409610, -65.86354444268503983 ) ) ;
#44668 = EDGE_CURVE ( 'NONE', #212825, #144138, #104846, .T. ) ;
#44669 = LINE ( 'NONE', #65495, #207413 ) ;
#44670 = AXIS2_PLACEMENT_3D ( 'NONE', #86551, #146534, #44894 ) ;
#44671 = VERTEX_POINT ( 'NONE', #201364 ) ;
#44672 = ADVANCED_FACE ( 'NONE', ( #222185 ), #83935, .T. ) ;
#44673 = EDGE_CURVE ( 'NONE', #171946, #132097, #196451, .T. ) ;
#44674 = AXIS2_PLACEMENT_3D ( 'NONE', #60969, #140498, #220055 ) ;
#44675 = AXIS2_PLACEMENT_3D ( 'NONE', #70129, #49246, #128800 ) ;
#44676 = CARTESIAN_POINT ( 'NONE',  ( 21.12757541349815682, 6.324013112643644519, -199.6174151709002444 ) ) ;
#44677 = CARTESIAN_POINT ( 'NONE',  ( 18.59999999999999076, 74.75000000001230660, -162.0231074845243597 ) ) ;
#44678 = PRODUCT_DEFINITION_FORMATION_WITH_SPECIFIED_SOURCE ( 'ANY', '', #209720, .NOT_KNOWN. ) ;
#44679 = EDGE_CURVE ( 'NONE', #165270, #133438, #171552, .T. ) ;
#44680 = ORIENTED_EDGE ( 'NONE', *, *, #175671, .F. ) ;
#44681 = ORIENTED_EDGE ( 'NONE', *, *, #113245, .T. ) ;
#44683 = SPHERICAL_SURFACE ( 'NONE', #52867, 0.1000000000000000056 ) ;
#44682 = CIRCLE ( 'NONE', #73926, 0.1999999999999987899 ) ;
#44684 = ORIENTED_EDGE ( 'NONE', *, *, #29103, .F. ) ;
#44685 = CARTESIAN_POINT ( 'NONE',  ( 23.25000000000000000, -11.38316329222462464, -203.4791315943886048 ) ) ;
#44686 = CIRCLE ( 'NONE', #232141, 0.09999999999999817368 ) ;
#44687 = VERTEX_POINT ( 'NONE', #179263 ) ;
#44689 = VERTEX_POINT ( 'NONE', #41034 ) ;
#44688 = CARTESIAN_POINT ( 'NONE',  ( 23.14999999999999858, 1.115600667400684642E-11, -167.5000000000000284 ) ) ;
#44690 = ADVANCED_FACE ( 'NONE', ( #104797 ), #184360, .F. ) ;
#44691 = EDGE_CURVE ( 'NONE', #97749, #204570, #183103, .T. ) ;
#44692 = CARTESIAN_POINT ( 'NONE',  ( -20.64999999999999858, 74.00000000001254818, -183.2477294072864709 ) ) ;
#44693 = ORIENTED_EDGE ( 'NONE', *, *, #123819, .T. ) ;
#44694 = CARTESIAN_POINT ( 'NONE',  ( -5.900000000000002132, -11.34999999999999964, 13.90000000000000213 ) ) ;
#44695 = ORIENTED_EDGE ( 'NONE', *, *, #116042, .F. ) ;
#44697 = ORIENTED_EDGE ( 'NONE', *, *, #40076, .T. ) ;
#44696 = EDGE_LOOP ( 'NONE', ( #79066, #39712, #74394, #240470 ) ) ;
#44698 = CARTESIAN_POINT ( 'NONE',  ( -18.79999999999999716, -10.13229168743236031, -1.028467303599445826 ) ) ;
#44699 = CARTESIAN_POINT ( 'NONE',  ( -16.94052228080551359, 14.20304230139262280, -219.2868029172807098 ) ) ;
#44701 = ORIENTED_EDGE ( 'NONE', *, *, #253984, .F. ) ;
#44700 = VECTOR ( 'NONE', #40724, 1000.000000000000000 ) ;
#44702 = TOROIDAL_SURFACE ( 'NONE', #3157, 0.2000000000000000111, 0.1000000000000000056 ) ;
#44703 = AXIS2_PLACEMENT_3D ( 'NONE', #143507, #126522, #87373 ) ;
#44704 = ORIENTED_EDGE ( 'NONE', *, *, #235285, .F. ) ;
#44705 = CIRCLE ( 'NONE', #61263, 0.09999999999999939493 ) ;
#44706 = DIRECTION ( 'NONE',  ( -1.000000000000000000, -0.000000000000000000, -0.000000000000000000 ) ) ;
#44707 = DIRECTION ( 'NONE',  ( -1.000000000000000000, 0.000000000000000000, 0.000000000000000000 ) ) ;
#44709 = ORIENTED_EDGE ( 'NONE', *, *, #223, .F. ) ;
#44708 = FACE_OUTER_BOUND ( 'NONE', #17400, .T. ) ;
#44710 = DIRECTION ( 'NONE',  ( 0.000000000000000000, 0.7674881895858254310, 0.6410630849193176273 ) ) ;
#44711 = VERTEX_POINT ( 'NONE', #102224 ) ;
#44712 = VECTOR ( 'NONE', #137969, 1000.000000000000000 ) ;
#44713 = CARTESIAN_POINT ( 'NONE',  ( 20.94999999999999929, 67.22371710471985295, -161.4644784893834810 ) ) ;
#44714 = DIRECTION ( 'NONE',  ( 0.000000000000000000, -0.9126074666063660468, -0.4088369013363524762 ) ) ;
#44715 = VERTEX_POINT ( 'NONE', #159684 ) ;
#44716 = DIRECTION ( 'NONE',  ( 1.000000000000000000, 0.000000000000000000, 0.000000000000000000 ) ) ;
#44717 = DIRECTION ( 'NONE',  ( -1.000000000000000000, 0.000000000000000000, -0.000000000000000000 ) ) ;
#44718 = ORIENTED_EDGE ( 'NONE', *, *, #111955, .T. ) ;
#44719 = DIRECTION ( 'NONE',  ( 0.000000000000000000, 0.000000000000000000, -1.000000000000000000 ) ) ;
#44720 = ORIENTED_EDGE ( 'NONE', *, *, #45774, .F. ) ;
#44721 = AXIS2_PLACEMENT_3D ( 'NONE', #116288, #34201, #236212 ) ;
#44722 = AXIS2_PLACEMENT_3D ( 'NONE', #247882, #129227, #208772 ) ;
#44724 = ORIENTED_EDGE ( 'NONE', *, *, #223017, .T. ) ;
#44723 = ORIENTED_EDGE ( 'NONE', *, *, #244606, .F. ) ;
#44725 = EDGE_LOOP ( 'NONE', ( #51780, #164781, #231790, #73583 ) ) ;
#44726 = CARTESIAN_POINT ( 'NONE',  ( 18.59999999999999076, 64.35000000001251408, -178.6731074845244507 ) ) ;
#44727 = ORIENTED_EDGE ( 'NONE', *, *, #88965, .F. ) ;
#44728 = FACE_OUTER_BOUND ( 'NONE', #89809, .T. ) ;
#44729 = VERTEX_POINT ( 'NONE', #145231 ) ;
#44730 = FACE_OUTER_BOUND ( 'NONE', #77515, .T. ) ;
#44731 = CARTESIAN_POINT ( 'NONE',  ( -23.25000000000000000, 1.115600667400684642E-11, -67.00000000000004263 ) ) ;
#44732 = ORIENTED_EDGE ( 'NONE', *, *, #57919, .T. ) ;
#44733 = VECTOR ( 'NONE', #121460, 1000.000000000000000 ) ;
#44734 = EDGE_CURVE ( 'NONE', #172220, #59001, #21684, .T. ) ;
#44735 = AXIS2_PLACEMENT_3D ( 'NONE', #4027, #83534, #242632 ) ;
#44736 = VERTEX_POINT ( 'NONE', #160974 ) ;
#44737 = EDGE_CURVE ( 'NONE', #236905, #217380, #92399, .T. ) ;
#44738 = ORIENTED_EDGE ( 'NONE', *, *, #42938, .T. ) ;
#44739 = AXIS2_PLACEMENT_3D ( 'NONE', #32234, #253809, #191320 ) ;
#44740 = ADVANCED_FACE ( 'NONE', ( #61864 ), #181806, .T. ) ;
#44741 = CARTESIAN_POINT ( 'NONE',  ( -22.50485643085239928, -0.07878633906603053905, -155.7502050608275965 ) ) ;
#44742 = ADVANCED_FACE ( 'NONE', ( #220910 ), #100928, .F. ) ;
#44743 = ORIENTED_EDGE ( 'NONE', *, *, #30093, .T. ) ;
#44744 = CARTESIAN_POINT ( 'NONE',  ( 23.24999999999999289, 14.06640494040442135, -210.3712993791105532 ) ) ;
#44745 = DIRECTION ( 'NONE',  ( -1.000000000000000000, -0.000000000000000000, 0.000000000000000000 ) ) ;
#44746 = CARTESIAN_POINT ( 'NONE',  ( -20.94999999999994600, 65.25000000001119815, -3.123107484524795474 ) ) ;
#44747 = FACE_OUTER_BOUND ( 'NONE', #158575, .T. ) ;
#44748 = DIRECTION ( 'NONE',  ( 0.000000000000000000, 0.000000000000000000, -1.000000000000000000 ) ) ;
#44749 = CARTESIAN_POINT ( 'NONE',  ( 21.04999999999999716, -0.08561306079281094661, -127.5862402661897050 ) ) ;
#44750 = CIRCLE ( 'NONE', #73429, 0.09999999999999130418 ) ;
#44751 = CARTESIAN_POINT ( 'NONE',  ( -18.44362607810620247, 85.49049615809748559, -196.4651536176772311 ) ) ;
#44753 = CARTESIAN_POINT ( 'NONE',  ( 21.08078803292165659, 6.333012964448271553, -100.4208140128422571 ) ) ;
#44752 = CARTESIAN_POINT ( 'NONE',  ( -16.77683809663752257, 66.05416425680809311, -149.1870565036286109 ) ) ;
#44755 = AXIS2_PLACEMENT_3D ( 'NONE', #15654, #35222, #153903 ) ;
#44754 = CARTESIAN_POINT ( 'NONE',  ( -23.25000000000000000, 66.17117490947157421, -239.7639228359981303 ) ) ;
#44756 = CARTESIAN_POINT ( 'NONE',  ( -20.94999999999999929, 1.115600667400684642E-11, -33.50000000000000000 ) ) ;
#44757 = DIRECTION ( 'NONE',  ( 0.000000000000000000, -0.8900778951570211817, -0.4558084472153261513 ) ) ;
#44758 = ORIENTED_EDGE ( 'NONE', *, *, #60994, .T. ) ;
#44759 = EDGE_CURVE ( 'NONE', #159790, #122938, #250617, .T. ) ;
#44761 = VERTEX_POINT ( 'NONE', #89123 ) ;
#44760 = CARTESIAN_POINT ( 'NONE',  ( -21.05000000000000071, 5.900000000011102586, -144.2190997646564483 ) ) ;
#44762 = ORIENTED_EDGE ( 'NONE', *, *, #220416, .T. ) ;
#44763 = DIRECTION ( 'NONE',  ( 1.000000000000000000, 0.000000000000000000, 0.000000000000000000 ) ) ;
#44764 = ORIENTED_EDGE ( 'NONE', *, *, #35255, .T. ) ;
#44765 = AXIS2_PLACEMENT_3D ( 'NONE', #192740, #53219, #49371 ) ;
#44766 =( LENGTH_UNIT ( ) NAMED_UNIT ( * ) SI_UNIT ( .MILLI., .METRE. ) );
#44767 = EDGE_CURVE ( 'NONE', #12756, #176282, #175633, .T. ) ;
#44768 = CARTESIAN_POINT ( 'NONE',  ( 23.14999999999999858, 5.500000000011153745, -88.09473398108696074 ) ) ;
#44769 = ADVANCED_FACE ( 'NONE', ( #47413 ), #168717, .F. ) ;
#44770 = CARTESIAN_POINT ( 'NONE',  ( 23.14999999999999858, 4.000000000011155521, -167.5000000000000284 ) ) ;
#44771 = ORIENTED_EDGE ( 'NONE', *, *, #37549, .F. ) ;
#44772 = AXIS2_PLACEMENT_3D ( 'NONE', #164557, #208809, #168452 ) ;
#44773 = CARTESIAN_POINT ( 'NONE',  ( -23.15000000000000213, -11.39257802169451139, -164.4260504201680817 ) ) ;
#44774 = CARTESIAN_POINT ( 'NONE',  ( 21.15000000000005187, 76.00000000001119815, -36.02310748452479316 ) ) ;
#44776 = ORIENTED_EDGE ( 'NONE', *, *, #38220, .T. ) ;
#44775 = DIRECTION ( 'NONE',  ( 0.000000000000000000, 0.2128009952263603954, -0.9770955615653315052 ) ) ;
#44777 = CARTESIAN_POINT ( 'NONE',  ( 22.39999999999999503, 31.80471377451587500, -238.9601694054147742 ) ) ;
#44778 = EDGE_CURVE ( 'NONE', #223079, #208058, #13311, .T. ) ;
#44780 = EDGE_LOOP ( 'NONE', ( #30655, #195036, #124952, #115502 ) ) ;
#44779 = DIRECTION ( 'NONE',  ( 0.7071067811865487940, 0.7071067811865462405, -7.215498431451186046E-16 ) ) ;
#44781 = CARTESIAN_POINT ( 'NONE',  ( 18.59999999999999076, 69.55000000001261640, -193.5060803140843859 ) ) ;
#44782 = CARTESIAN_POINT ( 'NONE',  ( 23.14999999999999503, 42.98415524044398950, -233.9519173640447889 ) ) ;
#44783 = ORIENTED_EDGE ( 'NONE', *, *, #18277, .F. ) ;
#44784 = CARTESIAN_POINT ( 'NONE',  ( -18.59999999999999787, -1.263275465206102233, -74.90186466674640542 ) ) ;
#44785 = ADVANCED_FACE ( 'NONE', ( #69581 ), #249499, .F. ) ;
#44786 = FACE_OUTER_BOUND ( 'NONE', #39043, .T. ) ;
#44788 = CARTESIAN_POINT ( 'NONE',  ( -18.69999999999999929, 8.000000000000000000, -1.212568896937008089 ) ) ;
#44787 = CARTESIAN_POINT ( 'NONE',  ( -16.94107738177414291, 65.98576071487519812, -82.07310748452438531 ) ) ;
#44789 = CYLINDRICAL_SURFACE ( 'NONE', #78760, 0.09999999999999939493 ) ;
#44790 = PLANE ( 'NONE',  #240908 ) ;
#44792 = EDGE_CURVE ( 'NONE', #14005, #3179, #209075, .T. ) ;
#44791 = SURFACE_STYLE_FILL_AREA ( #242978 ) ;
#44793 = DIRECTION ( 'NONE',  ( 0.000000000000000000, -0.2128009952263604232, 0.9770955615653316162 ) ) ;
#44794 = AXIS2_PLACEMENT_3D ( 'NONE', #199450, #177334, #239849 ) ;
#44795 = CIRCLE ( 'NONE', #94660, 0.1000000000000028644 ) ;
#44796 = VECTOR ( 'NONE', #143277, 1000.000000000000000 ) ;
#44797 = ORIENTED_EDGE ( 'NONE', *, *, #226161, .T. ) ;
#44798 = B_SPLINE_CURVE_WITH_KNOTS ( 'NONE', 3,
 ( #192600, #148336, #49229, #252553 ),
 .UNSPECIFIED., .F., .F.,
 ( 4, 4 ),
 ( 0.000000000000000000, 0.0002118541922231923684 ),
 .UNSPECIFIED. ) ;
#44799 = DIRECTION ( 'NONE',  ( 1.000000000000000000, 0.000000000000000000, 0.000000000000000000 ) ) ;
#44800 = VERTEX_POINT ( 'NONE', #52554 ) ;
#44801 = VERTEX_POINT ( 'NONE', #87814 ) ;
#44802 = DIRECTION ( 'NONE',  ( 0.000000000000000000, 0.000000000000000000, -1.000000000000000000 ) ) ;
#44803 = FACE_OUTER_BOUND ( 'NONE', #29001, .T. ) ;
#44804 = ORIENTED_EDGE ( 'NONE', *, *, #213651, .T. ) ;
#44805 = ADVANCED_FACE ( 'NONE', ( #30456 ), #138179, .T. ) ;
#44806 = ORIENTED_EDGE ( 'NONE', *, *, #84445, .F. ) ;
#44807 = EDGE_CURVE ( 'NONE', #230992, #10835, #75680, .T. ) ;
#44808 = AXIS2_PLACEMENT_3D ( 'NONE', #203322, #125073, #27285 ) ;
#44809 = VERTEX_POINT ( 'NONE', #29204 ) ;
#44810 = DIRECTION ( 'NONE',  ( 0.000000000000000000, 0.4721928772777343464, 0.8814952561688431665 ) ) ;
#44811 = ORIENTED_EDGE ( 'NONE', *, *, #137489, .F. ) ;
#44812 = LINE ( 'NONE', #46081, #167396 ) ;
#44813 = LINE ( 'NONE', #64379, #203496 ) ;
#44814 = VECTOR ( 'NONE', #190915, 1000.000000000000000 ) ;
#44815 = DIRECTION ( 'NONE',  ( 0.000000000000000000, 0.000000000000000000, -1.000000000000000000 ) ) ;
#44816 = CARTESIAN_POINT ( 'NONE',  ( -17.29158576265543346, 65.63525233399461456, -181.4403492397322566 ) ) ;
#44817 = CARTESIAN_POINT ( 'NONE',  ( -20.64999999999999858, 49.36776662947724503, -253.7196102226803021 ) ) ;
#44818 = CARTESIAN_POINT ( 'NONE',  ( 12.25000000000000000, 47.91805600923871822, -233.7139610577891631 ) ) ;
#44820 = EDGE_LOOP ( 'NONE', ( #39949, #228161, #10493 ) ) ;
#44819 = DIRECTION ( 'NONE',  ( -1.000000000000000000, 2.952720810173289112E-16, 2.061873921506763405E-30 ) ) ;
#44822 = CARTESIAN_POINT ( 'NONE',  ( 21.97500000000000497, 9.750000000011153745, -88.15000000000004832 ) ) ;
#44821 = CARTESIAN_POINT ( 'NONE',  ( 20.95568717954149562, 65.39800594611979534, -61.92059911625574387 ) ) ;
#44823 = DIRECTION ( 'NONE',  ( 0.000000000000000000, 1.734723475976997999E-14, -1.000000000000000000 ) ) ;
#44824 =( BOUNDED_SURFACE ( )  B_SPLINE_SURFACE ( 3, 2, ( 
 ( #210781, #189940, #11303 ),
 ( #248622, #72574, #32170 ),
 ( #208234, #90817, #28333 ),
 ( #50397, #171690, #112972 ) ),
 .UNSPECIFIED., .F., .F., .F. ) 
 B_SPLINE_SURFACE_WITH_KNOTS ( ( 4, 4 ),
 ( 3, 3 ),
 ( 0.0002700421466196717673, 0.0004789321604330994782 ),
 ( 0.000000000000000000, 1.000000000000000000 ),
 .UNSPECIFIED. ) 
 GEOMETRIC_REPRESENTATION_ITEM ( )  RATIONAL_B_SPLINE_SURFACE ( (
 ( 1.000000000000000000, 0.7071067811865475727, 1.000000000000000000),
 ( 1.000000000000000000, 0.7163411249511767442, 1.000000000000000000),
 ( 1.000000000000000000, 0.7221957104841900676, 1.000000000000000000),
 ( 1.000000000000000000, 0.7250110520819876836, 1.000000000000000000) ) ) 
 REPRESENTATION_ITEM ( '' )  SURFACE ( )  );
#44825 = ORIENTED_EDGE ( 'NONE', *, *, #67567, .F. ) ;
#44826 = CARTESIAN_POINT ( 'NONE',  ( -23.15000000000000213, 4.250000000000000000, -12.35000000000000142 ) ) ;
#44827 = CARTESIAN_POINT ( 'NONE',  ( 18.59999999999999076, 68.87972903831429505, -99.36354444268502561 ) ) ;
#44828 = ORIENTED_EDGE ( 'NONE', *, *, #104904, .T. ) ;
#44830 = CARTESIAN_POINT ( 'NONE',  ( -20.64999999999999858, 74.05981308412438580, -149.3522266955776843 ) ) ;
#44829 = CARTESIAN_POINT ( 'NONE',  ( -22.39999999999999858, 11.65000000001115588, -167.3999999999999773 ) ) ;
#44831 = CIRCLE ( 'NONE', #98966, 0.1000000000000028644 ) ;
#44832 = CARTESIAN_POINT ( 'NONE',  ( -16.93710578446422943, 66.05000000001182059, -82.44191146832372397 ) ) ;
#44833 = ORIENTED_EDGE ( 'NONE', *, *, #87933, .T. ) ;
#44834 = AXIS2_PLACEMENT_3D ( 'NONE', #64554, #144075, #5848 ) ;
#44835 =( NAMED_UNIT ( * ) SI_UNIT ( $, .STERADIAN. ) SOLID_ANGLE_UNIT ( ) );
#44836 = DIRECTION ( 'NONE',  ( 1.000000000000000000, 0.000000000000000000, 0.000000000000000000 ) ) ;
#44837 =( BOUNDED_CURVE ( )  B_SPLINE_CURVE ( 3, ( #183370, #8578, #146768, #144212 ),
 .UNSPECIFIED., .F., .F. ) 
 B_SPLINE_CURVE_WITH_KNOTS ( ( 4, 4 ),
 ( 1.570796326794895448, 3.141592653589791784 ),
 .UNSPECIFIED. ) 
 CURVE ( )  GEOMETRIC_REPRESENTATION_ITEM ( )  RATIONAL_B_SPLINE_CURVE ( ( 1.000000000000000000, 0.8047378541243650485, 0.8047378541243650485, 1.000000000000000000 ) ) 
 REPRESENTATION_ITEM ( '' )  );
#44838 = CARTESIAN_POINT ( 'NONE',  ( -18.40000000000000213, -0.6805341177324988333, -242.5179126613615495 ) ) ;
#44839 = DIRECTION ( 'NONE',  ( -0.000000000000000000, -0.9126074666063770380, -0.4088369013363281068 ) ) ;
#44840 = EDGE_LOOP ( 'NONE', ( #95796, #14639, #24792, #161158, #168774 ) ) ;
#44841 = AXIS2_PLACEMENT_3D ( 'NONE', #140090, #179266, #80095 ) ;
#44842 = ORIENTED_EDGE ( 'NONE', *, *, #120629, .T. ) ;
#44843 = AXIS2_PLACEMENT_3D ( 'NONE', #206231, #87545, #167138 ) ;
#44844 = DIRECTION ( 'NONE',  ( 1.000000000000000000, 0.000000000000000000, 0.000000000000000000 ) ) ;
#44845 = CARTESIAN_POINT ( 'NONE',  ( -20.64999999999999858, -8.999999999988844479, -91.10603087734760663 ) ) ;
#44846 = DIRECTION ( 'NONE',  ( 0.000000000000000000, -7.034366652768082711E-15, 1.000000000000000000 ) ) ;
#44847 = ADVANCED_FACE ( 'NONE', ( #169997, #167405 ), #245634, .T. ) ;
#44848 = VECTOR ( 'NONE', #243155, 1000.000000000000000 ) ;
#44850 = CARTESIAN_POINT ( 'NONE',  ( 12.25000000000000000, 26.30888228346803004, -233.3999513616626587 ) ) ;
#44849 = AXIS2_PLACEMENT_3D ( 'NONE', #17505, #136143, #97010 ) ;
#44851 = DIRECTION ( 'NONE',  ( -1.000000000000000000, -7.304098846218134667E-16, 0.000000000000000000 ) ) ;
#44852 = VECTOR ( 'NONE', #61939, 1000.000000000000000 ) ;
#44854 =( BOUNDED_CURVE ( )  B_SPLINE_CURVE ( 3, ( #138569, #39544, #110708, #103313 ),
 .UNSPECIFIED., .F., .F. ) 
 B_SPLINE_CURVE_WITH_KNOTS ( ( 4, 4 ),
 ( 0.5235987755983901870, 1.570796326794896558 ),
 .UNSPECIFIED. ) 
 CURVE ( )  GEOMETRIC_REPRESENTATION_ITEM ( )  RATIONAL_B_SPLINE_CURVE ( ( 1.000000000000000000, 0.9106836025229743115, 0.9106836025229743115, 1.000000000000000000 ) ) 
 REPRESENTATION_ITEM ( '' )  );
#44853 = DIRECTION ( 'NONE',  ( 1.000000000000000000, 0.000000000000000000, 0.000000000000000000 ) ) ;
#44856 = ORIENTED_EDGE ( 'NONE', *, *, #170723, .T. ) ;
#44855 = DIRECTION ( 'NONE',  ( 1.000000000000000000, 0.000000000000000000, 0.000000000000000000 ) ) ;
#44857 = CARTESIAN_POINT ( 'NONE',  ( -21.07954640115336531, 6.329287696035376776, -33.43399229286031726 ) ) ;
#44858 = AXIS2_PLACEMENT_3D ( 'NONE', #235244, #37081, #256038 ) ;
#44859 = FACE_OUTER_BOUND ( 'NONE', #62703, .T. ) ;
#44860 = CYLINDRICAL_SURFACE ( 'NONE', #233539, 0.09999999999999939493 ) ;
#44861 = DIRECTION ( 'NONE',  ( -0.000000000000000000, 6.982962677686266711E-15, -1.000000000000000000 ) ) ;
#44862 = AXIS2_PLACEMENT_3D ( 'NONE', #214774, #55664, #34896 ) ;
#44863 = ADVANCED_FACE ( 'NONE', ( #246903 ), #231229, .T. ) ;
#44864 = FACE_OUTER_BOUND ( 'NONE', #47912, .T. ) ;
#44866 = VERTEX_POINT ( 'NONE', #188228 ) ;
#44865 = CARTESIAN_POINT ( 'NONE',  ( -20.94999999999999929, -1.162701749926853712, -175.4999999999999716 ) ) ;
#44867 = CARTESIAN_POINT ( 'NONE',  ( -20.85000000000000142, 74.98773774893902555, -233.8732236541320333 ) ) ;
#44868 = CARTESIAN_POINT ( 'NONE',  ( 21.10642757222115051, 10.72315628916975250, -179.7406975237851725 ) ) ;
#44869 = DIRECTION ( 'NONE',  ( 0.000000000000000000, 0.9126074666063769270, 0.4088369013363280513 ) ) ;
#44870 = DIRECTION ( 'NONE',  ( 0.000000000000000000, -7.272083257015735086E-15, 1.000000000000000000 ) ) ;
#44871 = ORIENTED_EDGE ( 'NONE', *, *, #64860, .F. ) ;
#44872 = CARTESIAN_POINT ( 'NONE',  ( -20.94999999999999929, 14.05000000001115623, -106.0136950707610310 ) ) ;
#44873 = ADVANCED_FACE ( 'NONE', ( #185660 ), #146508, .F. ) ;
#44874 = ADVANCED_FACE ( 'NONE', ( #12185 ), #106091, .F. ) ;
#44875 = LINE ( 'NONE', #61873, #183474 ) ;
#44876 = FACE_OUTER_BOUND ( 'NONE', #218190, .T. ) ;
#44877 = AXIS2_PLACEMENT_3D ( 'NONE', #204578, #89762, #169357 ) ;
#44878 = ORIENTED_EDGE ( 'NONE', *, *, #11974, .F. ) ;
#44879 = CARTESIAN_POINT ( 'NONE',  ( -16.89155683852633416, 9.950000000011138823, -87.22262815045961304 ) ) ;
#44880 = AXIS2_PLACEMENT_3D ( 'NONE', #114957, #251894, #75833 ) ;
#44881 = ORIENTED_EDGE ( 'NONE', *, *, #163943, .F. ) ;
#44882 = VECTOR ( 'NONE', #128787, 1000.000000000000000 ) ;
#44883 = LINE ( 'NONE', #240510, #176623 ) ;
#44884 = AXIS2_PLACEMENT_3D ( 'NONE', #45984, #27748, #105936 ) ;
#44885 = CIRCLE ( 'NONE', #219652, 12.97499999999998721 ) ;
#44886 = ADVANCED_FACE ( 'NONE', ( #9580 ), #108690, .T. ) ;
#44887 = FACE_OUTER_BOUND ( 'NONE', #183879, .T. ) ;
#44888 = CARTESIAN_POINT ( 'NONE',  ( 18.52130828395270612, -9.481395502614638815, -174.5245067238836043 ) ) ;
#44889 = ORIENTED_EDGE ( 'NONE', *, *, #15718, .T. ) ;
#44890 = CIRCLE ( 'NONE', #153253, 0.09999999999999939493 ) ;
#44891 = FACE_OUTER_BOUND ( 'NONE', #218297, .T. ) ;
#44892 = DIRECTION ( 'NONE',  ( 0.000000000000000000, -0.000000000000000000, -1.000000000000000000 ) ) ;
#44893 = CARTESIAN_POINT ( 'NONE',  ( 23.14999999999999858, 4.775700934590591196, -122.1512318959540693 ) ) ;
#44894 = DIRECTION ( 'NONE',  ( 0.000000000000000000, 0.2818822000686317941, -0.9594490217226071538 ) ) ;
#44895 = AXIS2_PLACEMENT_3D ( 'NONE', #212522, #172135, #35191 ) ;
#44897 = AXIS2_PLACEMENT_3D ( 'NONE', #243582, #208330, #29703 ) ;
#44896 = DIRECTION ( 'NONE',  ( -1.646408749285562691E-14, 0.9770955615653315052, 0.2128009952263603954 ) ) ;
#44898 = AXIS2_PLACEMENT_3D ( 'NONE', #239509, #156144, #99957 ) ;
#44899 = ORIENTED_EDGE ( 'NONE', *, *, #29093, .T. ) ;
#44901 = VERTEX_POINT ( 'NONE', #68288 ) ;
#44900 = DIRECTION ( 'NONE',  ( 1.073024830501117725E-15, -6.982962677686266711E-15, 1.000000000000000000 ) ) ;
#44902 = VERTEX_POINT ( 'NONE', #117674 ) ;
#44903 = CARTESIAN_POINT ( 'NONE',  ( -16.83794479845801817, 9.926357419351495182, -20.69644470422230853 ) ) ;
#44904 = VERTEX_POINT ( 'NONE', #13452 ) ;
#44905 = EDGE_CURVE ( 'NONE', #144797, #63272, #123217, .T. ) ;
#44906 = CARTESIAN_POINT ( 'NONE',  ( 21.05000000000080718, 61.13731265359255929, -234.2555725237206445 ) ) ;
#44907 = CARTESIAN_POINT ( 'NONE',  ( 18.59999999999997655, 76.00000000001213607, -136.5231074845243313 ) ) ;
#44908 = EDGE_CURVE ( 'NONE', #61206, #42457, #255854, .T. ) ;
#44909 = CARTESIAN_POINT ( 'NONE',  ( 23.15000000000000213, 87.65000000001192859, -106.1231074845242262 ) ) ;
#44910 = ORIENTED_EDGE ( 'NONE', *, *, #54077, .F. ) ;
#44911 = FACE_OUTER_BOUND ( 'NONE', #12158, .T. ) ;
#44912 = DIRECTION ( 'NONE',  ( 0.000000000000000000, 0.4999999999999478195, 0.8660254037844686836 ) ) ;
#44913 = CARTESIAN_POINT ( 'NONE',  ( 20.12481660106788084, 9.526343992285099205, -41.72614166909304600 ) ) ;
#44914 = EDGE_LOOP ( 'NONE', ( #162155, #192806 ) ) ;
#44915 = CARTESIAN_POINT ( 'NONE',  ( -15.69373346032659100, 9.356790025057035720, -151.2048265086139054 ) ) ;
#44916 = CIRCLE ( 'NONE', #232185, 0.1000000000000000472 ) ;
#44918 = ORIENTED_EDGE ( 'NONE', *, *, #49663, .F. ) ;
#44917 = DIRECTION ( 'NONE',  ( 1.000000000000000000, 0.000000000000000000, 0.000000000000000000 ) ) ;
#44919 = CARTESIAN_POINT ( 'NONE',  ( 20.94999999999999574, -11.41227409413852989, -70.00000000000004263 ) ) ;
#44920 = AXIS2_PLACEMENT_3D ( 'NONE', #257993, #122393, #241070 ) ;
#44922 = EDGE_CURVE ( 'NONE', #57960, #31018, #257134, .T. ) ;
#44921 = LINE ( 'NONE', #222235, #47959 ) ;
#44923 = ORIENTED_EDGE ( 'NONE', *, *, #102055, .T. ) ;
#44924 = CIRCLE ( 'NONE', #65762, 0.1999999999999987899 ) ;
#44925 = LINE ( 'NONE', #167464, #89341 ) ;
#44926 = CARTESIAN_POINT ( 'NONE',  ( -15.75000000000000355, 66.65000000001204228, -119.7731074845243739 ) ) ;
#44927 = CARTESIAN_POINT ( 'NONE',  ( -22.59999999999999787, -3.180729737797944434, -228.0957332317254895 ) ) ;
#44928 = EDGE_LOOP ( 'NONE', ( #83807, #256650, #159313, #65950 ) ) ;
#44929 = DIRECTION ( 'NONE',  ( -0.000000000000000000, 1.000000000000000000, -0.000000000000000000 ) ) ;
#44930 = CARTESIAN_POINT ( 'NONE',  ( -22.16821283564876666, 7.558973340791935058, -100.5000000000000284 ) ) ;
#44931 = CIRCLE ( 'NONE', #115662, 11.64999999999999503 ) ;
#44932 = ORIENTED_EDGE ( 'NONE', *, *, #250721, .F. ) ;
#44933 = AXIS2_PLACEMENT_3D ( 'NONE', #251341, #113129, #72752 ) ;
#44934 = AXIS2_PLACEMENT_3D ( 'NONE', #85181, #8268, #44815 ) ;
#44935 = TOROIDAL_SURFACE ( 'NONE', #190713, 0.6000000000000004219, 0.1000000000000000056 ) ;
#44936 = EDGE_LOOP ( 'NONE', ( #89272, #197628, #256942, #162082 ) ) ;
#44937 = CARTESIAN_POINT ( 'NONE',  ( 21.06089410995835109, 65.27470446788900915, -191.3207267534812104 ) ) ;
#44938 = EDGE_CURVE ( 'NONE', #160483, #156337, #188445, .T. ) ;
#44939 = EDGE_CURVE ( 'NONE', #119072, #2821, #133398, .T. ) ;
#44940 = ORIENTED_EDGE ( 'NONE', *, *, #210132, .T. ) ;
#44941 = CARTESIAN_POINT ( 'NONE',  ( -20.54999999999999716, 78.89331866122350334, -228.7665898296168052 ) ) ;
#44942 = DIRECTION ( 'NONE',  ( 0.000000000000000000, 0.000000000000000000, -1.000000000000000000 ) ) ;
#44944 = VERTEX_POINT ( 'NONE', #215489 ) ;
#44943 = CARTESIAN_POINT ( 'NONE',  ( 12.25000000000000000, 26.30888228346803004, -233.3999513616626587 ) ) ;
#44945 = DIRECTION ( 'NONE',  ( 1.000000000000000000, 0.000000000000000000, 0.000000000000000000 ) ) ;
#44946 = DIRECTION ( 'NONE',  ( 0.000000000000000000, 0.9876197685951241256, 0.1568667991644932258 ) ) ;
#44947 = EDGE_CURVE ( 'NONE', #96616, #181669, #212930, .T. ) ;
#44948 = EDGE_CURVE ( 'NONE', #26849, #33224, #237632, .T. ) ;
#44949 = CARTESIAN_POINT ( 'NONE',  ( 18.39999999999999503, 5.650000000011139001, -146.6500000000000341 ) ) ;
#44950 = DIRECTION ( 'NONE',  ( 0.000000000000000000, -1.000000000000000000, 0.000000000000000000 ) ) ;
#44951 = AXIS2_PLACEMENT_3D ( 'NONE', #175448, #58017, #95868 ) ;
#44952 = CARTESIAN_POINT ( 'NONE',  ( 20.94999999999999574, 43.57281345108133053, -239.9888335660389487 ) ) ;
#44953 = DIRECTION ( 'NONE',  ( 0.000000000000000000, -6.982962677686266711E-15, 1.000000000000000000 ) ) ;
#44955 = ORIENTED_EDGE ( 'NONE', *, *, #121810, .T. ) ;
#44954 = DIRECTION ( 'NONE',  ( 0.000000000000000000, 6.982962677686266711E-15, -1.000000000000000000 ) ) ;
#44956 = FACE_OUTER_BOUND ( 'NONE', #48553, .T. ) ;
#44957 = EDGE_LOOP ( 'NONE', ( #59405, #46129, #116523, #81207 ) ) ;
#44958 = DIRECTION ( 'NONE',  ( -1.000000000000000000, 0.000000000000000000, 0.000000000000000000 ) ) ;
#44959 = TOROIDAL_SURFACE ( 'NONE', #190733, 0.4000000000000009104, 0.1000000000000000056 ) ;
#44960 = EDGE_CURVE ( 'NONE', #234897, #20839, #125894, .T. ) ;
#44962 = EDGE_CURVE ( 'NONE', #110731, #77018, #116405, .T. ) ;
#44961 = EDGE_CURVE ( 'NONE', #42311, #75854, #34318, .T. ) ;
#44963 = CARTESIAN_POINT ( 'NONE',  ( -16.94107738177415712, 65.98576071487597972, -190.9731074845244336 ) ) ;
#44964 = DIRECTION ( 'NONE',  ( 0.000000000000000000, 0.9915357197604804940, -0.1298341882520397950 ) ) ;
#44965 = EDGE_CURVE ( 'NONE', #66771, #153726, #250811, .T. ) ;
#44966 = CARTESIAN_POINT ( 'NONE',  ( 20.58091095332318332, 66.98152984665888710, -195.1044573023666544 ) ) ;
#44967 = ORIENTED_EDGE ( 'NONE', *, *, #237688, .F. ) ;
#44968 = EDGE_CURVE ( 'NONE', #109005, #214500, #88470, .T. ) ;
#44969 = DIRECTION ( 'NONE',  ( 2.952720810173289112E-16, 0.9651348961777157509, -0.2617529984165031243 ) ) ;
#44970 = AXIS2_PLACEMENT_3D ( 'NONE', #7334, #124720, #123435 ) ;
#44971 = AXIS2_PLACEMENT_3D ( 'NONE', #76247, #16310, #80067 ) ;
#44972 = ORIENTED_EDGE ( 'NONE', *, *, #64188, .T. ) ;
#44973 = EDGE_CURVE ( 'NONE', #35927, #105518, #105011, .T. ) ;
#44974 = AXIS2_PLACEMENT_3D ( 'NONE', #33660, #71475, #16626 ) ;
#44975 = EDGE_CURVE ( 'NONE', #174088, #38036, #200929, .T. ) ;
#44976 = DIRECTION ( 'NONE',  ( 0.000000000000000000, -8.881784197001644782E-16, -1.000000000000000000 ) ) ;
#44977 = CARTESIAN_POINT ( 'NONE',  ( -18.41418431465368855, 86.89640087696879789, -199.6396878666320447 ) ) ;
#44978 = EDGE_CURVE ( 'NONE', #35579, #216812, #175819, .T. ) ;
#44979 = VERTEX_POINT ( 'NONE', #176391 ) ;
#44980 = CARTESIAN_POINT ( 'NONE',  ( -16.93860193097148326, 66.00689223268298633, -149.1229691172175933 ) ) ;
#44981 = VERTEX_POINT ( 'NONE', #216769 ) ;
#44982 = CARTESIAN_POINT ( 'NONE',  ( -15.75000000000001066, 9.350000000011139178, -50.02151937182511432 ) ) ;
#44983 = ORIENTED_EDGE ( 'NONE', *, *, #110894, .F. ) ;
#44984 = EDGE_CURVE ( 'NONE', #188047, #124170, #50879, .T. ) ;
#44985 = CARTESIAN_POINT ( 'NONE',  ( 18.39999999999999503, 5.650000000011139001, -146.6500000000000341 ) ) ;
#44986 = CARTESIAN_POINT ( 'NONE',  ( -20.07928932188135107, 9.220710678118654968, -21.25000000000000000 ) ) ;
#44987 = AXIS2_PLACEMENT_3D ( 'NONE', #23188, #44006, #184795 ) ;
#44989 = ORIENTED_EDGE ( 'NONE', *, *, #79743, .F. ) ;
#44988 = ADVANCED_FACE ( 'NONE', ( #98077, #75986, #18584 ), #36895, .F. ) ;
#44991 = CARTESIAN_POINT ( 'NONE',  ( -20.64999999999999858, 73.60000000001180354, -82.74772940728642823 ) ) ;
#44990 = CIRCLE ( 'NONE', #78292, 4.150000000000001243 ) ;
#44993 = ORIENTED_EDGE ( 'NONE', *, *, #86112, .T. ) ;
#44992 = CARTESIAN_POINT ( 'NONE',  ( -21.07928932188134041, 6.328516656404449492, -100.4011048543456468 ) ) ;
#44994 = ORIENTED_EDGE ( 'NONE', *, *, #87991, .F. ) ;
#44995 = AXIS2_PLACEMENT_3D ( 'NONE', #30018, #75560, #169546 ) ;
#44996 = EDGE_LOOP ( 'NONE', ( #120232, #58011, #195421, #139897 ) ) ;
#44997 = ADVANCED_FACE ( 'NONE', ( #56400 ), #238914, .F. ) ;
#44998 = FACE_OUTER_BOUND ( 'NONE', #107788, .T. ) ;
#44999 = CARTESIAN_POINT ( 'NONE',  ( 22.45301702632625762, 26.02101828454447485, -254.3001460930269673 ) ) ;
#45000 = DIRECTION ( 'NONE',  ( -1.000000000000000000, -3.265361837132813093E-16, 0.000000000000000000 ) ) ;
#45001 = DIRECTION ( 'NONE',  ( -1.000000000000000000, 0.000000000000000000, 0.000000000000000000 ) ) ;
#45002 = DIRECTION ( 'NONE',  ( 0.000000000000000000, 0.000000000000000000, -1.000000000000000000 ) ) ;
#45003 = ORIENTED_EDGE ( 'NONE', *, *, #40851, .F. ) ;
#45004 = CARTESIAN_POINT ( 'NONE',  ( -23.15000000000000213, 84.59626168225486254, -93.57297996737396772 ) ) ;
#45005 = CARTESIAN_POINT ( 'NONE',  ( -23.25000000000000000, -1.835859311443637010, -45.10443916879852821 ) ) ;
#45006 = CYLINDRICAL_SURFACE ( 'NONE', #174497, 7.899999999999990585 ) ;
#45007 = CARTESIAN_POINT ( 'NONE',  ( -18.59999999999999787, -1.362429037182155023, -108.3888812479212476 ) ) ;
#45008 = TOROIDAL_SURFACE ( 'NONE', #240834, 0.2000000000000000111, 0.1000000000000000056 ) ;
#45009 = ORIENTED_EDGE ( 'NONE', *, *, #50197, .T. ) ;
#45010 = CARTESIAN_POINT ( 'NONE',  ( -21.09096482362058467, 75.96055172123791976, -109.3866518499287963 ) ) ;
#45011 = VERTEX_POINT ( 'NONE', #99371 ) ;
#45012 = CARTESIAN_POINT ( 'NONE',  ( 13.12220780326571301, 9.430633469083948839, -115.7317657948240850 ) ) ;
#45013 = CIRCLE ( 'NONE', #211621, 0.2000000000000057288 ) ;
#45014 = ORIENTED_EDGE ( 'NONE', *, *, #81113, .F. ) ;
#45015 = AXIS2_PLACEMENT_3D ( 'NONE', #88461, #115756, #216126 ) ;
#45016 = PLANE ( 'NONE',  #72166 ) ;
#45017 = DIRECTION ( 'NONE',  ( -0.000000000000000000, 0.8814952561688430555, -0.4721928772777346239 ) ) ;
#45018 = ORIENTED_EDGE ( 'NONE', *, *, #111677, .T. ) ;
#45020 = ORIENTED_EDGE ( 'NONE', *, *, #141113, .F. ) ;
#45019 = DIRECTION ( 'NONE',  ( 0.000000000000000000, 0.2128009952263603677, -0.9770955615653313941 ) ) ;
#45021 = DIRECTION ( 'NONE',  ( 0.000000000000000000, -1.000000000000000000, 0.000000000000000000 ) ) ;
#45022 = ORIENTED_EDGE ( 'NONE', *, *, #115614, .F. ) ;
#45023 = AXIS2_PLACEMENT_3D ( 'NONE', #238917, #236341, #195954 ) ;
#45024 = CARTESIAN_POINT ( 'NONE',  ( -22.48479450179659977, 0.04699158119804078271, -21.85000155374838826 ) ) ;
#45025 = CARTESIAN_POINT ( 'NONE',  ( -13.39999999999994529, 67.72071067812984779, -17.05239680640613642 ) ) ;
#45026 = ORIENTED_EDGE ( 'NONE', *, *, #66632, .F. ) ;
#45027 = EDGE_CURVE ( 'NONE', #18265, #210270, #21178, .T. ) ;
#45028 = CARTESIAN_POINT ( 'NONE',  ( -18.39999999999999858, -9.599999999988845900, -174.2001893912220680 ) ) ;
#45029 = FACE_OUTER_BOUND ( 'NONE', #11242, .T. ) ;
#45030 = CIRCLE ( 'NONE', #157303, 0.09999999999999986677 ) ;
#45031 = EDGE_CURVE ( 'NONE', #70728, #78387, #13504, .T. ) ;
#45033 = EDGE_LOOP ( 'NONE', ( #160107, #98866, #165113, #3381 ) ) ;
#45032 = VECTOR ( 'NONE', #193458, 999.9999999999998863 ) ;
#45034 = VERTEX_POINT ( 'NONE', #79806 ) ;
#45035 = DIRECTION ( 'NONE',  ( -1.000000000000000000, 0.000000000000000000, 0.000000000000000000 ) ) ;
#45036 = EDGE_CURVE ( 'NONE', #140605, #256115, #196633, .T. ) ;
#45037 = EDGE_CURVE ( 'NONE', #239889, #5246, #197205, .T. ) ;
#45039 = ORIENTED_EDGE ( 'NONE', *, *, #112042, .F. ) ;
#45038 = CARTESIAN_POINT ( 'NONE',  ( 23.15000000000000213, -8.663551401858002876, -110.0241011180673354 ) ) ;
#45040 = LINE ( 'NONE', #43757, #232994 ) ;
#45041 = CARTESIAN_POINT ( 'NONE',  ( -22.49072729836729678, 75.94351806727812004, -81.17311573367925348 ) ) ;
#45042 = FACE_OUTER_BOUND ( 'NONE', #17827, .T. ) ;
#45044 = CARTESIAN_POINT ( 'NONE',  ( -17.01473183483381391, 9.950000000011138823, -188.2499999999999716 ) ) ;
#45043 = FACE_OUTER_BOUND ( 'NONE', #80271, .T. ) ;
#45045 = CARTESIAN_POINT ( 'NONE',  ( 21.04999999999999716, 39.24426575657115279, -236.8395263841964038 ) ) ;
#45046 = CYLINDRICAL_SURFACE ( 'NONE', #106887, 0.09999999999999939493 ) ;
#45047 = VECTOR ( 'NONE', #177709, 1000.000000000000000 ) ;
#45048 = CARTESIAN_POINT ( 'NONE',  ( -21.05000000000000071, 65.49889199258218753, -241.8691648588935266 ) ) ;
#45049 = DIRECTION ( 'NONE',  ( 2.879366945564059217E-14, 0.2599159095383297702, -0.9656312546561770516 ) ) ;
#45050 = VECTOR ( 'NONE', #33879, 1000.000000000000000 ) ;
#45051 = EDGE_LOOP ( 'NONE', ( #2496, #73122, #224673 ) ) ;
#45052 = ADVANCED_FACE ( 'NONE', ( #220634 ), #63350, .T. ) ;
#45053 = AXIS2_PLACEMENT_3D ( 'NONE', #14648, #115005, #253221 ) ;
#45054 = CIRCLE ( 'NONE', #211678, 0.1999999999999987899 ) ;
#45055 = AXIS2_PLACEMENT_3D ( 'NONE', #100105, #80538, #61001 ) ;
#45056 = EDGE_LOOP ( 'NONE', ( #68100, #103137, #196764, #26420, #256378, #50145, #245394, #150291, #83760, #242914, #140395, #155187 ) ) ;
#45057 = DIRECTION ( 'NONE',  ( 0.000000000000000000, 0.000000000000000000, -1.000000000000000000 ) ) ;
#45058 = ORIENTED_EDGE ( 'NONE', *, *, #57682, .T. ) ;
#45059 = DIRECTION ( 'NONE',  ( 0.000000000000000000, 0.7216758089626587047, -0.6922311945860948335 ) ) ;
#45060 = ORIENTED_EDGE ( 'NONE', *, *, #253950, .F. ) ;
#45061 = PRODUCT ( 'Snap Open Cable Crossbars 8', 'Snap Open Cable Crossbars 8', '', ( #41670 ) ) ;
#45062 = ORIENTED_EDGE ( 'NONE', *, *, #159810, .T. ) ;
#45063 = EDGE_CURVE ( 'NONE', #9735, #192243, #218034, .T. ) ;
#45064 = CARTESIAN_POINT ( 'NONE',  ( -18.39999999999999858, 85.50000000001168132, -62.92291809330220786 ) ) ;
#45065 = VERTEX_POINT ( 'NONE', #120285 ) ;
#45066 = CIRCLE ( 'NONE', #170027, 0.09999999999999939493 ) ;
#45067 = AXIS2_PLACEMENT_3D ( 'NONE', #108662, #53826, #72120 ) ;
#45068 = VERTEX_POINT ( 'NONE', #2843 ) ;
#45069 = DIRECTION ( 'NONE',  ( 0.000000000000000000, -6.997203936713175802E-15, 1.000000000000000000 ) ) ;
#45070 = CARTESIAN_POINT ( 'NONE',  ( -21.07933241753356413, 75.90662040959273327, -109.3517534329040615 ) ) ;
#45072 = ORIENTED_EDGE ( 'NONE', *, *, #92427, .F. ) ;
#45071 = CARTESIAN_POINT ( 'NONE',  ( -18.59999999999999787, 18.81339837015603322, -226.7756228984618190 ) ) ;
#45073 = CYLINDRICAL_SURFACE ( 'NONE', #240999, 0.09999999999999939493 ) ;
#45075 = ORIENTED_EDGE ( 'NONE', *, *, #239080, .F. ) ;
#45074 = DIRECTION ( 'NONE',  ( 1.000000000000000000, 0.000000000000000000, 0.000000000000000000 ) ) ;
#45076 = CARTESIAN_POINT ( 'NONE',  ( 19.97071067695831559, 11.72071067696947644, -125.1762534328032217 ) ) ;
#45077 = EDGE_LOOP ( 'NONE', ( #29046, #13745, #188858, #79352 ) ) ;
#45078 = DIRECTION ( 'NONE',  ( 0.000000000000000000, 6.997203936713175802E-15, -1.000000000000000000 ) ) ;
#45079 = EDGE_CURVE ( 'NONE', #57491, #11139, #138359, .T. ) ;
#45081 = ORIENTED_EDGE ( 'NONE', *, *, #157731, .T. ) ;
#45080 = DIRECTION ( 'NONE',  ( 0.000000000000000000, -0.01562499999999307672, 0.9998779222360100194 ) ) ;
#45082 = AXIS2_PLACEMENT_3D ( 'NONE', #86789, #166385, #187217 ) ;
#45083 = DIRECTION ( 'NONE',  ( 0.000000000000000000, 0.2605042016806672911, -0.9654727137038716656 ) ) ;
#45084 = CARTESIAN_POINT ( 'NONE',  ( -12.68215100488890279, 27.35084141791446655, -233.9052011656355603 ) ) ;
#45085 = EDGE_CURVE ( 'NONE', #14142, #32896, #192554, .T. ) ;
#45086 = CARTESIAN_POINT ( 'NONE',  ( -16.97683809663753252, 12.54629451653078043, -211.8501780441710309 ) ) ;
#45087 = ORIENTED_EDGE ( 'NONE', *, *, #16744, .F. ) ;
#45089 = CARTESIAN_POINT ( 'NONE',  ( 20.22894356738321164, 9.278498222849551169, -108.7685229062446552 ) ) ;
#45088 = CARTESIAN_POINT ( 'NONE',  ( -20.85000000000000142, 68.97833521811233481, -166.1895420826271277 ) ) ;
#45090 = CARTESIAN_POINT ( 'NONE',  ( 23.14999999999998437, -0.8618440306552707098, -197.0427629756619297 ) ) ;
#45091 = AXIS2_PLACEMENT_3D ( 'NONE', #31751, #13446, #111259 ) ;
#45092 = DIRECTION ( 'NONE',  ( -0.000000000000000000, -0.9651348961777161950, 0.2617529984165015700 ) ) ;
#45093 = PLANE ( 'NONE',  #47493 ) ;
#45094 = DIRECTION ( 'NONE',  ( 1.000000000000000000, -0.000000000000000000, 0.000000000000000000 ) ) ;
#45095 = ORIENTED_EDGE ( 'NONE', *, *, #77527, .T. ) ;
#45096 = ORIENTED_EDGE ( 'NONE', *, *, #104125, .F. ) ;
#45098 = ORIENTED_EDGE ( 'NONE', *, *, #146597, .T. ) ;
#45097 = CIRCLE ( 'NONE', #190882, 2.000000000000001776 ) ;
#45099 = EDGE_CURVE ( 'NONE', #110678, #15317, #225833, .T. ) ;
#45100 = FACE_OUTER_BOUND ( 'NONE', #176688, .T. ) ;
#45101 = ORIENTED_EDGE ( 'NONE', *, *, #62654, .T. ) ;
#45102 = ORIENTED_EDGE ( 'NONE', *, *, #141554, .F. ) ;
#45103 = CARTESIAN_POINT ( 'NONE',  ( -22.00356870142647026, 7.254242362488315443, -100.5000000000000426 ) ) ;
#45104 = DIRECTION ( 'NONE',  ( 0.000000000000000000, -1.000000000000000000, -7.759275652592821052E-15 ) ) ;
#45105 = ADVANCED_FACE ( 'NONE', ( #221883 ), #109324, .F. ) ;
#45106 = EDGE_CURVE ( 'NONE', #153107, #44131, #171734, .T. ) ;
#45107 = CIRCLE ( 'NONE', #245023, 11.64999999999999680 ) ;
#45108 = AXIS2_PLACEMENT_3D ( 'NONE', #30401, #151649, #70827 ) ;
#45109 = EDGE_LOOP ( 'NONE', ( #95963, #108301, #6748, #111089, #182884, #201647, #232627, #103646, #116654, #101740, #25516, #62353, #223872, #12070, #167818, #197005, #102779, #32880 ) ) ;
#45110 = EDGE_CURVE ( 'NONE', #163777, #88476, #103225, .T. ) ;
#45111 = AXIS2_PLACEMENT_3D ( 'NONE', #84066, #119404, #198926 ) ;
#45112 = CARTESIAN_POINT ( 'NONE',  ( -17.11825945287481332, 30.11817903451004952, -234.7598257170722889 ) ) ;
#45113 = AXIS2_PLACEMENT_3D ( 'NONE', #58472, #138015, #3651 ) ;
#45114 = ORIENTED_EDGE ( 'NONE', *, *, #189441, .T. ) ;
#45115 = VERTEX_POINT ( 'NONE', #182808 ) ;
#45116 = ORIENTED_EDGE ( 'NONE', *, *, #232934, .T. ) ;
#45117 = DIRECTION ( 'NONE',  ( 0.000000000000000000, -1.000000000000000000, -6.982962677686266711E-15 ) ) ;
#45118 = CARTESIAN_POINT ( 'NONE',  ( 18.39999999999997371, 11.47316190337362940, -158.2500000000000284 ) ) ;
#45119 = CARTESIAN_POINT ( 'NONE',  ( -18.34374000495060386, 20.70020979027691155, -227.9869476361872103 ) ) ;
#45120 = CARTESIAN_POINT ( 'NONE',  ( 21.05000000000000071, 76.00000000001193712, -105.9231074845242944 ) ) ;
#45121 = FACE_OUTER_BOUND ( 'NONE', #187791, .T. ) ;
#45122 = EDGE_CURVE ( 'NONE', #37503, #250524, #83643, .T. ) ;
#45124 = DIRECTION ( 'NONE',  ( 1.000000000000000000, 0.000000000000000000, -0.000000000000000000 ) ) ;
#45123 = DIRECTION ( 'NONE',  ( 1.000000000000000000, 0.000000000000000000, 0.000000000000000000 ) ) ;
#45125 = CARTESIAN_POINT ( 'NONE',  ( -17.22361732159831504, 10.34515565861359043, -55.62921547413287726 ) ) ;
#45127 = EDGE_LOOP ( 'NONE', ( #116874, #103724, #91247, #22734 ) ) ;
#45126 = CARTESIAN_POINT ( 'NONE',  ( -20.90851465518105812, 10.32532329027886320, -139.5699343018359855 ) ) ;
#45129 = CARTESIAN_POINT ( 'NONE',  ( 18.59999999999999076, 6.650000000011155876, -54.75000000000000000 ) ) ;
#45128 = FACE_OUTER_BOUND ( 'NONE', #129484, .T. ) ;
#45130 = ORIENTED_EDGE ( 'NONE', *, *, #121237, .F. ) ;
#45131 = CARTESIAN_POINT ( 'NONE',  ( 20.94999999999999574, 8.926614585087095932, -8.471683019223121391 ) ) ;
#45132 = CIRCLE ( 'NONE', #65791, 0.09999999999999939493 ) ;
#45133 = CARTESIAN_POINT ( 'NONE',  ( 22.59999999999999432, 64.25043287652255231, -103.1239658536231047 ) ) ;
#45134 = CARTESIAN_POINT ( 'NONE',  ( 19.80993210785466374, 64.25000000001149658, -44.75598973563685234 ) ) ;
#45135 = ORIENTED_EDGE ( 'NONE', *, *, #76413, .T. ) ;
#45136 = DIRECTION ( 'NONE',  ( 0.000000000000000000, 0.000000000000000000, -1.000000000000000000 ) ) ;
#45137 = CARTESIAN_POINT ( 'NONE',  ( 20.95512820512820440, 10.62384868372303615, -108.1649135690876449 ) ) ;
#45138 = DIRECTION ( 'NONE',  ( 0.000000000000000000, 0.000000000000000000, -1.000000000000000000 ) ) ;
#45139 = EDGE_LOOP ( 'NONE', ( #166836, #43117, #133927 ) ) ;
#45140 = ORIENTED_EDGE ( 'NONE', *, *, #235445, .T. ) ;
#45141 = DIRECTION ( 'NONE',  ( -0.000000000000000000, -0.000000000000000000, 1.000000000000000000 ) ) ;
#45142 = EDGE_LOOP ( 'NONE', ( #31202, #163868, #210885, #212773 ) ) ;
#45143 = DIRECTION ( 'NONE',  ( 1.000000000000000000, 0.000000000000000000, 0.000000000000000000 ) ) ;
#45144 = CARTESIAN_POINT ( 'NONE',  ( -18.48408745364672967, -9.664322258652006781, -174.1830785333283416 ) ) ;
#45145 = DIRECTION ( 'NONE',  ( 0.000000000000000000, 0.4999999999999088507, -0.8660254037844913322 ) ) ;
#45146 = CARTESIAN_POINT ( 'NONE',  ( -23.49999999999994316, 74.25000000001119815, -47.64205752314703801 ) ) ;
#45147 = VERTEX_POINT ( 'NONE', #55944 ) ;
#45148 = CARTESIAN_POINT ( 'NONE',  ( -14.56336952470180002, 9.446645344706402270, -118.9108064561002323 ) ) ;
#45149 = DIRECTION ( 'NONE',  ( -0.000000000000000000, -0.1350103645451904977, 0.9908441862701596881 ) ) ;
#45150 = CARTESIAN_POINT ( 'NONE',  ( -17.11825945287481332, 63.05955705323258798, -213.2241350765465882 ) ) ;
#45151 = CIRCLE ( 'NONE', #165799, 11.75000000000001066 ) ;
#45152 = CARTESIAN_POINT ( 'NONE',  ( -18.50000000000000000, 64.35000000001268461, -203.4231074845244507 ) ) ;
#45153 = AXIS2_PLACEMENT_3D ( 'NONE', #231397, #112724, #137403 ) ;
#45154 = CIRCLE ( 'NONE', #49249, 0.1000000000000028644 ) ;
#45155 = EDGE_CURVE ( 'NONE', #171051, #212250, #46785, .T. ) ;
#45156 = ORIENTED_EDGE ( 'NONE', *, *, #30494, .T. ) ;
#45158 = ORIENTED_EDGE ( 'NONE', *, *, #40283, .T. ) ;
#45157 = DIRECTION ( 'NONE',  ( -1.000000000000000000, -7.304098846218134667E-16, 0.000000000000000000 ) ) ;
#45159 = DIRECTION ( 'NONE',  ( -1.000000000000000000, 7.304098846218134667E-16, 5.100424963727255829E-30 ) ) ;
#45160 = CARTESIAN_POINT ( 'NONE',  ( -23.15000000000000213, -9.600000000000004974, -9.893969122652444881 ) ) ;
#45161 = EDGE_CURVE ( 'NONE', #214271, #13299, #98912, .T. ) ;
#45162 = PLANE ( 'NONE',  #237867 ) ;
#45163 = LINE ( 'NONE', #3459, #167275 ) ;
#45164 = LINE ( 'NONE', #127275, #167340 ) ;
#45165 = CARTESIAN_POINT ( 'NONE',  ( -20.94999999999999929, 87.65000000001192859, -106.1231074845242262 ) ) ;
#45166 = ORIENTED_EDGE ( 'NONE', *, *, #251354, .T. ) ;
#45167 = CARTESIAN_POINT ( 'NONE',  ( -21.05000000000000071, 11.75000000000000000, -26.48519422934605316 ) ) ;
#45168 = EDGE_CURVE ( 'NONE', #155920, #90910, #221561, .T. ) ;
#45169 = CIRCLE ( 'NONE', #82546, 0.6000000000000033085 ) ;
#45170 = EDGE_CURVE ( 'NONE', #203104, #71443, #67648, .T. ) ;
#45171 = CARTESIAN_POINT ( 'NONE',  ( 16.27683809663750125, 9.349999999999983658, -9.250000000000001776 ) ) ;
#45172 = CIRCLE ( 'NONE', #70149, 0.1000000000000124678 ) ;
#45173 = CARTESIAN_POINT ( 'NONE',  ( -18.50000000000000000, -1.362429037193310988, -41.38888124792119783 ) ) ;
#45174 = DIRECTION ( 'NONE',  ( -1.000000000000000000, 0.000000000000000000, -0.000000000000000000 ) ) ;
#45175 = VECTOR ( 'NONE', #13976, 1000.000000000000000 ) ;
#45176 = ORIENTED_EDGE ( 'NONE', *, *, #30880, .F. ) ;
#45177 = ORIENTED_EDGE ( 'NONE', *, *, #32412, .F. ) ;
#45178 = CARTESIAN_POINT ( 'NONE',  ( 21.05000000000000071, 1.115600667400684642E-11, -79.87500000000004263 ) ) ;
#45179 = DIRECTION ( 'NONE',  ( 1.000000000000000000, 0.000000000000000000, 0.000000000000000000 ) ) ;
#45180 = CARTESIAN_POINT ( 'NONE',  ( 22.50000000000000000, 11.64957080754479968, 0.09999999999999592548 ) ) ;
#45181 = CARTESIAN_POINT ( 'NONE',  ( 22.39999999999999503, -3.140208063160686791, -228.2318569537739847 ) ) ;
#45182 = EDGE_CURVE ( 'NONE', #233399, #51812, #247440, .T. ) ;
#45183 = CARTESIAN_POINT ( 'NONE',  ( -23.15000000000000213, 78.50726470275243685, -228.6618886302502176 ) ) ;
#45184 = EDGE_CURVE ( 'NONE', #229783, #70381, #121829, .T. ) ;
#45185 = DIRECTION ( 'NONE',  ( 0.000000000000000000, 0.9868171638914228216, 0.1618390714546044939 ) ) ;
#45186 = FACE_OUTER_BOUND ( 'NONE', #93586, .T. ) ;
#45187 = DIRECTION ( 'NONE',  ( 1.000000000000000000, 0.000000000000000000, 0.000000000000000000 ) ) ;
#45188 = AXIS2_PLACEMENT_3D ( 'NONE', #163800, #142913, #184629 ) ;
#45189 = TOROIDAL_SURFACE ( 'NONE', #190973, 0.2000000000000000111, 0.1000000000000000056 ) ;
#45190 = AXIS2_PLACEMENT_3D ( 'NONE', #214538, #115438, #16370 ) ;
#45191 = ORIENTED_EDGE ( 'NONE', *, *, #24321, .T. ) ;
#45192 = CARTESIAN_POINT ( 'NONE',  ( 22.39999999999999858, 7.591056067193225232, -199.2444047917219052 ) ) ;
#45193 = EDGE_CURVE ( 'NONE', #3812, #74995, #155181, .T. ) ;
#45194 = EDGE_LOOP ( 'NONE', ( #228492, #39871, #75794, #65321 ) ) ;
#45195 = ADVANCED_FACE ( 'NONE', ( #38991 ), #157686, .T. ) ;
#45196 = CARTESIAN_POINT ( 'NONE',  ( -21.05000000000000071, 76.10000000001171827, -76.06376443622556849 ) ) ;
#45197 = EDGE_CURVE ( 'NONE', #189583, #150585, #117726, .T. ) ;
#45198 = LINE ( 'NONE', #4760, #145457 ) ;
#45199 = CARTESIAN_POINT ( 'NONE',  ( -21.04999999999897398, 10.05835145952827503, -228.1548128398107451 ) ) ;
#45200 = DIRECTION ( 'NONE',  ( 0.000000000000000000, 0.000000000000000000, 1.000000000000000000 ) ) ;
#45201 = DIRECTION ( 'NONE',  ( 0.000000000000000000, -0.2617529984165031243, -0.9651348961777157509 ) ) ;
#45202 = DIRECTION ( 'NONE',  ( 0.000000000000000000, -7.304098846218112382E-15, 1.000000000000000000 ) ) ;
#45203 = FACE_OUTER_BOUND ( 'NONE', #117382, .T. ) ;
#45204 = DIRECTION ( 'NONE',  ( 1.000000000000000000, 0.000000000000000000, 0.000000000000000000 ) ) ;
#45205 = FACE_OUTER_BOUND ( 'NONE', #69178, .T. ) ;
#45206 = CARTESIAN_POINT ( 'NONE',  ( -18.59999999999999787, 70.20041822846812352, -198.0817714174541493 ) ) ;
#45207 = LINE ( 'NONE', #249837, #44083 ) ;
#45209 = ADVANCED_FACE ( 'NONE', ( #115955 ), #22068, .T. ) ;
#45208 = DIRECTION ( 'NONE',  ( 0.000000000000000000, 0.9868171638914221555, 0.1618390714546086850 ) ) ;
#45210 = AXIS2_PLACEMENT_3D ( 'NONE', #203435, #224265, #24824 ) ;
#45211 = AXIS2_PLACEMENT_3D ( 'NONE', #95463, #56323, #173780 ) ;
#45212 = VECTOR ( 'NONE', #124700, 1000.000000000000000 ) ;
#45213 = CARTESIAN_POINT ( 'NONE',  ( 21.97500000000000497, 9.750000000011153745, -155.2500000000000000 ) ) ;
#45214 = DIRECTION ( 'NONE',  ( -1.000000000000000000, 2.952720810173289112E-16, 2.061873921506763405E-30 ) ) ;
#45215 = AXIS2_PLACEMENT_3D ( 'NONE', #18255, #116082, #117359 ) ;
#45216 = VERTEX_POINT ( 'NONE', #96358 ) ;
#45217 = CARTESIAN_POINT ( 'NONE',  ( -18.40000000000000213, 50.88295650978584206, -230.3037755757580953 ) ) ;
#45218 = DIRECTION ( 'NONE',  ( 1.000000000000000000, 0.000000000000000000, 0.000000000000000000 ) ) ;
#45219 = SHAPE_REPRESENTATION ( 'Injection Molded Chain Links 2', ( #2425 ), #35604 ) ;
#45220 = ORIENTED_EDGE ( 'NONE', *, *, #254847, .F. ) ;
#45221 = DIRECTION ( 'NONE',  ( 0.000000000000000000, 0.000000000000000000, -1.000000000000000000 ) ) ;
#45222 = CARTESIAN_POINT ( 'NONE',  ( 21.05000000000000071, 67.22371710471982453, -157.8731074845244109 ) ) ;
#45223 = CIRCLE ( 'NONE', #124346, 0.09999999999999939493 ) ;
#45224 = EDGE_CURVE ( 'NONE', #125446, #232714, #14306, .T. ) ;
#45225 = CARTESIAN_POINT ( 'NONE',  ( -17.22767730081687887, 10.34924421247923654, -189.6424286905727286 ) ) ;
#45226 = EDGE_LOOP ( 'NONE', ( #86052, #146347, #245129, #84604 ) ) ;
#45227 = CARTESIAN_POINT ( 'NONE',  ( 18.39999999999999858, -9.682403433465237796, -174.1568433774128266 ) ) ;
#45228 = PLANE ( 'NONE',  #239196 ) ;
#45229 = AXIS2_PLACEMENT_3D ( 'NONE', #176107, #17023, #118694 ) ;
#45230 = ORIENTED_EDGE ( 'NONE', *, *, #34705, .F. ) ;
#45231 = CIRCLE ( 'NONE', #107771, 11.80000000000000426 ) ;
#45232 = PRESENTATION_LAYER_ASSIGNMENT (  '', '', ( #120305 ) ) ;
#45233 = AXIS2_PLACEMENT_3D ( 'NONE', #19764, #241377, #118865 ) ;
#45234 = AXIS2_PLACEMENT_3D ( 'NONE', #150812, #191252, #30902 ) ;
#45235 = DIRECTION ( 'NONE',  ( -0.000000000000000000, -0.000000000000000000, 1.000000000000000000 ) ) ;
#45236 = ADVANCED_FACE ( 'NONE', ( #138056, #173406, #174689 ), #97635, .F. ) ;
#45237 = ORIENTED_EDGE ( 'NONE', *, *, #242448, .T. ) ;
#45238 = CIRCLE ( 'NONE', #136823, 0.2000000000000111688 ) ;
#45239 = DIRECTION ( 'NONE',  ( -0.5735764363510466035, 0.8191520442889914655, 0.000000000000000000 ) ) ;
#45240 = CARTESIAN_POINT ( 'NONE',  ( -0.8999999999999986899, -8.350000000000004974, 30.04142135623731136 ) ) ;
#45241 = DIRECTION ( 'NONE',  ( 1.000000000000000000, 0.000000000000000000, 0.000000000000000000 ) ) ;
#45243 = DIRECTION ( 'NONE',  ( 1.000000000000000000, 0.000000000000000000, 0.000000000000000000 ) ) ;
#45242 = PRODUCT_DEFINITION_CONTEXT ( 'detailed design', #242380, 'design' ) ;
#45244 = EDGE_CURVE ( 'NONE', #248091, #256994, #55319, .T. ) ;
#45245 = CARTESIAN_POINT ( 'NONE',  ( -21.46681500593004444, 69.14248884062553202, -203.5231074845244166 ) ) ;
#45246 = CARTESIAN_POINT ( 'NONE',  ( -16.93710578446436088, 66.05000000001230376, -157.1043035007245408 ) ) ;
#45247 = DIRECTION ( 'NONE',  ( 0.000000000000000000, 0.000000000000000000, -1.000000000000000000 ) ) ;
#45248 = FACE_OUTER_BOUND ( 'NONE', #98563, .T. ) ;
#45249 = DIRECTION ( 'NONE',  ( -1.000000000000000000, 0.000000000000000000, 0.000000000000000000 ) ) ;
#45251 = ORIENTED_EDGE ( 'NONE', *, *, #242449, .F. ) ;
#45250 = CARTESIAN_POINT ( 'NONE',  ( 18.37172112093625032, 87.02156976317876058, -199.4492670956951770 ) ) ;
#45252 = ORIENTED_EDGE ( 'NONE', *, *, #120119, .T. ) ;
#45254 = CARTESIAN_POINT ( 'NONE',  ( 23.14999999999999147, 4.149999999999999467, 5.082284216461513184E-16 ) ) ;
#45253 = FACE_OUTER_BOUND ( 'NONE', #193239, .T. ) ;
#45256 = VERTEX_POINT ( 'NONE', #254153 ) ;
#45255 = DIRECTION ( 'NONE',  ( -1.000000000000000000, 0.000000000000000000, -0.000000000000000000 ) ) ;
#45257 = ORIENTED_EDGE ( 'NONE', *, *, #214757, .F. ) ;
#45258 = CARTESIAN_POINT ( 'NONE',  ( 18.49999999999999645, -1.362429037182155023, -208.8888812479211765 ) ) ;
#45259 = AXIS2_PLACEMENT_3D ( 'NONE', #193044, #134319, #173523 ) ;
#45260 = DIRECTION ( 'NONE',  ( 2.694716079187273932E-16, 0.4088369013363286064, -0.9126074666063768159 ) ) ;
#45261 = EDGE_CURVE ( 'NONE', #155361, #26378, #9560, .T. ) ;
#45262 = EDGE_CURVE ( 'NONE', #212201, #245427, #177232, .T. ) ;
#45263 = CARTESIAN_POINT ( 'NONE',  ( -21.05000000000000071, -1.851028230129704522, -145.6539132694225032 ) ) ;
#45264 = CARTESIAN_POINT ( 'NONE',  ( 18.59999999999999076, 77.16412189325360771, -162.1082593989527254 ) ) ;
#45265 = CARTESIAN_POINT ( 'NONE',  ( -16.77683809663752257, 9.945835743215301505, -180.1639490191041943 ) ) ;
#45266 = CARTESIAN_POINT ( 'NONE',  ( -20.00857864376270001, 66.85000000001259934, -191.2731074845244166 ) ) ;
#45267 = CIRCLE ( 'NONE', #32848, 0.1000000000000028644 ) ;
#45268 = VECTOR ( 'NONE', #59719, 1000.000000000000000 ) ;
#45269 = CARTESIAN_POINT ( 'NONE',  ( -22.48660254037843487, 31.85034414784621148, -238.9397275603479898 ) ) ;
#45271 = VERTEX_POINT ( 'NONE', #161508 ) ;
#45270 = ADVANCED_FACE ( 'NONE', ( #198037 ), #44112, .T. ) ;
#45272 = EDGE_LOOP ( 'NONE', ( #240935, #108991 ) ) ;
#45273 = CARTESIAN_POINT ( 'NONE',  ( -20.94999999999999929, 63.58084468663284383, -237.4904741118237723 ) ) ;
#45274 = CIRCLE ( 'NONE', #95172, 0.1999999999999987899 ) ;
#45275 = ORIENTED_EDGE ( 'NONE', *, *, #233906, .F. ) ;
#45276 = CARTESIAN_POINT ( 'NONE',  ( 21.13435531349788832, 1.115486826172573664E-11, -27.00627893640781352 ) ) ;
#45278 = EDGE_CURVE ( 'NONE', #226695, #14872, #17737, .T. ) ;
#45277 = EDGE_LOOP ( 'NONE', ( #20672, #19950, #155217, #62661 ) ) ;
#45279 = CARTESIAN_POINT ( 'NONE',  ( 23.24999999999999645, 11.75000000001113953, -87.85000000000003695 ) ) ;
#45280 = AXIS2_PLACEMENT_3D ( 'NONE', #80331, #239450, #242003 ) ;
#45281 = DIRECTION ( 'NONE',  ( 1.000000000000000000, -0.000000000000000000, 0.000000000000000000 ) ) ;
#45282 = ADVANCED_FACE ( 'NONE', ( #201901 ), #243591, .T. ) ;
#45283 = CARTESIAN_POINT ( 'NONE',  ( 20.85000000000000142, -11.74999999998883560, -131.0000000000000284 ) ) ;
#45284 = CARTESIAN_POINT ( 'NONE',  ( -16.94107738177415712, 22.92025126680846725, -230.8312174982872307 ) ) ;
#45285 = ORIENTED_EDGE ( 'NONE', *, *, #138970, .F. ) ;
#45286 = CYLINDRICAL_SURFACE ( 'NONE', #250478, 11.80000000000000426 ) ;
#45287 = ORIENTED_EDGE ( 'NONE', *, *, #12893, .T. ) ;
#45288 = DIRECTION ( 'NONE',  ( 1.000000000000000000, 0.000000000000000000, 0.000000000000000000 ) ) ;
#45289 = CIRCLE ( 'NONE', #191063, 0.1000000000000024342 ) ;
#45291 = CARTESIAN_POINT ( 'NONE',  ( -21.46681500598551651, 30.40070853532066408, -252.3547663145424451 ) ) ;
#45290 = AXIS2_PLACEMENT_3D ( 'NONE', #170292, #16326, #193664 ) ;
#45292 = EDGE_CURVE ( 'NONE', #242521, #39555, #123657, .T. ) ;
#45293 = DIRECTION ( 'NONE',  ( 1.000000000000000000, 0.000000000000000000, 0.000000000000000000 ) ) ;
#45294 = AXIS2_PLACEMENT_3D ( 'NONE', #240340, #179106, #162093 ) ;
#45295 = DIRECTION ( 'NONE',  ( 4.026293107431335996E-15, 0.7106264324241517993, -0.7035695228903270371 ) ) ;
#45297 = VERTEX_POINT ( 'NONE', #203176 ) ;
#45296 = EDGE_CURVE ( 'NONE', #42435, #250411, #20714, .T. ) ;
#45298 = CARTESIAN_POINT ( 'NONE',  ( -23.25000000000000000, 70.05000000001251692, -180.3288097895592159 ) ) ;
#45299 = ORIENTED_EDGE ( 'NONE', *, *, #144136, .T. ) ;
#45302 = ORIENTED_EDGE ( 'NONE', *, *, #128756, .T. ) ;
#45301 = DIRECTION ( 'NONE',  ( 1.000000000000000000, -3.448943450116721596E-16, -6.438528483529603700E-16 ) ) ;
#45300 = FACE_OUTER_BOUND ( 'NONE', #246696, .T. ) ;
#45303 = CARTESIAN_POINT ( 'NONE',  ( -0.8999999999999993561, -8.250000000000005329, 23.40000000000000568 ) ) ;
#45304 = ORIENTED_EDGE ( 'NONE', *, *, #173356, .F. ) ;
#45305 = DIRECTION ( 'NONE',  ( 0.000000000000000000, 0.9126074666064696306, 0.4088369013361212723 ) ) ;
#45306 = ORIENTED_EDGE ( 'NONE', *, *, #22318, .T. ) ;
#45307 = DIRECTION ( 'NONE',  ( 1.000000000000000000, -0.000000000000000000, 0.000000000000000000 ) ) ;
#45308 = DIRECTION ( 'NONE',  ( 0.000000000000000000, 0.000000000000000000, -1.000000000000000000 ) ) ;
#45309 = EDGE_CURVE ( 'NONE', #204695, #131456, #51046, .T. ) ;
#45310 = FACE_OUTER_BOUND ( 'NONE', #99612, .T. ) ;
#45311 = EDGE_CURVE ( 'NONE', #179727, #248043, #155358, .T. ) ;
#45312 = CIRCLE ( 'NONE', #191088, 0.09999999999999939493 ) ;
#45313 = DIRECTION ( 'NONE',  ( 0.000000000000000000, 0.8814952561688476074, -0.4721928772777262417 ) ) ;
#45314 = ORIENTED_EDGE ( 'NONE', *, *, #41215, .F. ) ;
#45315 = DIRECTION ( 'NONE',  ( 0.000000000000000000, 0.2128009952263601734, -0.9770955615653316162 ) ) ;
#45316 =( LENGTH_UNIT ( ) NAMED_UNIT ( * ) SI_UNIT ( .MILLI., .METRE. ) );
#45317 = CARTESIAN_POINT ( 'NONE',  ( -18.44204374631830845, -9.491036389587215183, -140.6262012702210598 ) ) ;
#45318 = VERTEX_POINT ( 'NONE', #144466 ) ;
#45319 = CARTESIAN_POINT ( 'NONE',  ( -23.25000000000000000, -9.599999999988845900, -90.60603087734760663 ) ) ;
#45320 = VERTEX_POINT ( 'NONE', #122369 ) ;
#45321 = CARTESIAN_POINT ( 'NONE',  ( -21.05000000000000071, -0.09999999998884338825, -26.95934304829875927 ) ) ;
#45322 = DIRECTION ( 'NONE',  ( 0.000000000000000000, 0.000000000000000000, -1.000000000000000000 ) ) ;
#45323 = FACE_OUTER_BOUND ( 'NONE', #155671, .T. ) ;
#45325 = ORIENTED_EDGE ( 'NONE', *, *, #127665, .F. ) ;
#45324 = CARTESIAN_POINT ( 'NONE',  ( 20.84999999999998721, 42.20719072976272912, -239.1935934412594804 ) ) ;
#45326 = LINE ( 'NONE', #186121, #112826 ) ;
#45327 = CARTESIAN_POINT ( 'NONE',  ( -14.77538296656415362, 62.91973165888632735, -215.7008495347502617 ) ) ;
#45328 = CARTESIAN_POINT ( 'NONE',  ( 22.50000000000000000, 10.71943444926881561, -226.8179467668883547 ) ) ;
#45329 = ORIENTED_EDGE ( 'NONE', *, *, #20913, .T. ) ;
#45330 = CIRCLE ( 'NONE', #49434, 0.09999999999999939493 ) ;
#45332 = CIRCLE ( 'NONE', #178647, 0.1000000000000028644 ) ;
#45331 = FACE_OUTER_BOUND ( 'NONE', #204207, .T. ) ;
#45333 = CARTESIAN_POINT ( 'NONE',  ( -18.59999999999999787, -1.164121893230052995, -74.91484808557160591 ) ) ;
#45334 = EDGE_LOOP ( 'NONE', ( #132820, #13749, #163899, #223913 ) ) ;
#45335 = AXIS2_PLACEMENT_3D ( 'NONE', #246887, #24020, #223465 ) ;
#45336 = CARTESIAN_POINT ( 'NONE',  ( 18.59999999999999076, 80.80934863333322937, -192.8037999715871535 ) ) ;
#45337 = EDGE_CURVE ( 'NONE', #151819, #39792, #70122, .T. ) ;
#45338 = ORIENTED_EDGE ( 'NONE', *, *, #705, .F. ) ;
#45339 = DIRECTION ( 'NONE',  ( 1.000000000000000000, 0.000000000000000000, -0.000000000000000000 ) ) ;
#45340 = CIRCLE ( 'NONE', #224405, 0.09999999999999910349 ) ;
#45342 = ORIENTED_EDGE ( 'NONE', *, *, #250739, .F. ) ;
#45341 = DIRECTION ( 'NONE',  ( -1.000000000000000000, -0.000000000000000000, -0.000000000000000000 ) ) ;
#45345 = VERTEX_POINT ( 'NONE', #121112 ) ;
#45344 = VERTEX_POINT ( 'NONE', #24569 ) ;
#45343 = DIRECTION ( 'NONE',  ( -1.000000000000000000, 0.000000000000000000, 0.000000000000000000 ) ) ;
#45347 = CIRCLE ( 'NONE', #12061, 0.1000000000000124678 ) ;
#45346 = DIRECTION ( 'NONE',  ( 1.000000000000000000, 0.000000000000000000, 0.000000000000000000 ) ) ;
#45348 = AXIS2_PLACEMENT_3D ( 'NONE', #65300, #163138, #44472 ) ;
#45349 = DIRECTION ( 'NONE',  ( 1.000000000000000000, -2.952720810173289112E-16, -2.061873921506763405E-30 ) ) ;
#45350 = LINE ( 'NONE', #186147, #56657 ) ;
#45351 = VECTOR ( 'NONE', #226430, 1000.000000000000000 ) ;
#45353 = DIRECTION ( 'NONE',  ( 0.000000000000000000, 0.000000000000000000, -1.000000000000000000 ) ) ;
#45352 = CARTESIAN_POINT ( 'NONE',  ( -20.85000000000000142, 76.00000000001239187, -162.1231074845243825 ) ) ;
#45355 = ADVANCED_FACE ( 'NONE', ( #6247 ), #188831, .T. ) ;
#45354 = DIRECTION ( 'NONE',  ( 0.000000000000000000, 0.9910827722268055195, 0.1332476588733540468 ) ) ;
#45356 = CARTESIAN_POINT ( 'NONE',  ( -17.27223548802019693, 65.65460260862890607, -58.15671366372658468 ) ) ;
#45357 = DIRECTION ( 'NONE',  ( 0.000000000000000000, 0.000000000000000000, 1.000000000000000000 ) ) ;
#45358 = AXIS2_PLACEMENT_3D ( 'NONE', #30676, #231433, #148033 ) ;
#45359 = CARTESIAN_POINT ( 'NONE',  ( -22.59999970745345976, 76.00935637733975625, -148.2736206921935320 ) ) ;
#45360 = ORIENTED_EDGE ( 'NONE', *, *, #238209, .F. ) ;
#45361 = ORIENTED_EDGE ( 'NONE', *, *, #97611, .F. ) ;
#45362 = CARTESIAN_POINT ( 'NONE',  ( -20.94999999999999929, 76.00000000001169553, -65.42310748452432279 ) ) ;
#45364 = EDGE_LOOP ( 'NONE', ( #31665, #137170, #59008, #169476 ) ) ;
#45363 = DIRECTION ( 'NONE',  ( 0.000000000000000000, 0.8814952561688441657, -0.4721928772777325145 ) ) ;
#45365 = ORIENTED_EDGE ( 'NONE', *, *, #35300, .F. ) ;
#45366 = CARTESIAN_POINT ( 'NONE',  ( 20.94999999999999929, -8.999999999988844479, -43.39396912265245021 ) ) ;
#45367 = VERTEX_POINT ( 'NONE', #105322 ) ;
#45368 = CARTESIAN_POINT ( 'NONE',  ( -21.07928932188134041, 69.67148334361344553, -136.6220026301789972 ) ) ;
#45369 = ORIENTED_EDGE ( 'NONE', *, *, #137522, .F. ) ;
#45370 = DIRECTION ( 'NONE',  ( 0.000000000000000000, 0.000000000000000000, -1.000000000000000000 ) ) ;
#45371 = DIRECTION ( 'NONE',  ( 0.000000000000000000, 0.000000000000000000, -1.000000000000000000 ) ) ;
#45372 = VECTOR ( 'NONE', #55913, 1000.000000000000000 ) ;
#45373 = AXIS2_PLACEMENT_3D ( 'NONE', #187951, #45860, #204920 ) ;
#45375 = EDGE_LOOP ( 'NONE', ( #32256, #31580, #130456, #48097 ) ) ;
#45374 = ORIENTED_EDGE ( 'NONE', *, *, #161349, .F. ) ;
#45376 = EDGE_LOOP ( 'NONE', ( #173675, #60955, #130873, #47105 ) ) ;
#45377 = DIRECTION ( 'NONE',  ( 1.000000000000000000, -3.265361837132813093E-16, -2.280189983783949500E-30 ) ) ;
#45378 = EDGE_LOOP ( 'NONE', ( #50482, #230467, #127917, #197788 ) ) ;
#45379 = ORIENTED_EDGE ( 'NONE', *, *, #43314, .F. ) ;
#45380 = FACE_OUTER_BOUND ( 'NONE', #97727, .T. ) ;
#45381 = CARTESIAN_POINT ( 'NONE',  ( 18.58719872626879877, -9.566644397587475979, -73.82247819639700026 ) ) ;
#45383 = ORIENTED_EDGE ( 'NONE', *, *, #190761, .F. ) ;
#45382 = CARTESIAN_POINT ( 'NONE',  ( -18.50000000000000000, 65.70729864261028297, -131.0657455973724836 ) ) ;
#45384 = CIRCLE ( 'NONE', #95455, 2.100000000000004530 ) ;
#45385 = DIRECTION ( 'NONE',  ( 0.000000000000000000, -7.056502275159890832E-15, 1.000000000000000000 ) ) ;
#45386 = DIRECTION ( 'NONE',  ( 0.000000000000000000, 0.9910465087640866200, 0.1335171055202867274 ) ) ;
#45388 = ORIENTED_EDGE ( 'NONE', *, *, #22955, .T. ) ;
#45387 = CARTESIAN_POINT ( 'NONE',  ( -21.65000000000000213, 7.250000000011139534, -188.3499999999999659 ) ) ;
#45389 = DIRECTION ( 'NONE',  ( 1.000000000000000000, 0.000000000000000000, 0.000000000000000000 ) ) ;
#45390 = VERTEX_POINT ( 'NONE', #184898 ) ;
#45391 = FACE_OUTER_BOUND ( 'NONE', #109983, .T. ) ;
#45392 = EDGE_LOOP ( 'NONE', ( #9572, #119668, #58802, #180153 ) ) ;
#45393 = FACE_OUTER_BOUND ( 'NONE', #106753, .T. ) ;
#45394 = LINE ( 'NONE', #222734, #216285 ) ;
#45395 = EDGE_CURVE ( 'NONE', #131609, #193670, #165344, .T. ) ;
#45396 = ORIENTED_EDGE ( 'NONE', *, *, #33176, .F. ) ;
#45397 = CIRCLE ( 'NONE', #191168, 11.80000000000000959 ) ;
#45400 = DIRECTION ( 'NONE',  ( -1.000000000000000000, 0.000000000000000000, 0.000000000000000000 ) ) ;
#45399 = CARTESIAN_POINT ( 'NONE',  ( 21.09793522318416592, 10.72462451022393282, -45.73929087097716462 ) ) ;
#45398 = CIRCLE ( 'NONE', #141084, 0.09999999999999939493 ) ;
#45401 = DIRECTION ( 'NONE',  ( 2.952720810173289112E-16, 1.000000000000000000, 6.982962677686266711E-15 ) ) ;
#45402 = AXIS2_PLACEMENT_3D ( 'NONE', #10915, #74768, #55128 ) ;
#45403 = ORIENTED_EDGE ( 'NONE', *, *, #203792, .T. ) ;
#45404 = EDGE_LOOP ( 'NONE', ( #92987, #134621, #76804, #128507 ) ) ;
#45405 = EDGE_CURVE ( 'NONE', #227290, #158852, #250972, .T. ) ;
#45406 = DIRECTION ( 'NONE',  ( 1.000000000000000000, -0.000000000000000000, -0.000000000000000000 ) ) ;
#45407 = DIRECTION ( 'NONE',  ( 1.000000000000000000, -2.952720810173289112E-16, -2.061873921506763405E-30 ) ) ;
#45408 = EDGE_LOOP ( 'NONE', ( #41079, #52868, #161667, #51830 ) ) ;
#45409 = CYLINDRICAL_SURFACE ( 'NONE', #97421, 0.09999999999999817368 ) ;
#45410 = ORIENTED_EDGE ( 'NONE', *, *, #220105, .F. ) ;
#45411 = CARTESIAN_POINT ( 'NONE',  ( 23.14999999999999858, 1.115600667400684642E-11, -167.5000000000000284 ) ) ;
#45412 = EDGE_CURVE ( 'NONE', #109129, #88364, #5262, .T. ) ;
#45413 = VECTOR ( 'NONE', #220558, 1000.000000000000000 ) ;
#45414 = AXIS2_PLACEMENT_3D ( 'NONE', #168079, #106760, #243719 ) ;
#45415 = PLANE ( 'NONE',  #44920 ) ;
#45416 = DIRECTION ( 'NONE',  ( -3.265361837132813093E-16, -1.000000000000000000, -6.982962677686266711E-15 ) ) ;
#45417 = ORIENTED_EDGE ( 'NONE', *, *, #205499, .T. ) ;
#45419 = EDGE_CURVE ( 'NONE', #196915, #94787, #142814, .T. ) ;
#45418 = AXIS2_PLACEMENT_3D ( 'NONE', #97480, #118374, #157534 ) ;
#45420 = DIRECTION ( 'NONE',  ( -0.7071067811865487940, -0.7071067811865463515, -4.937700262164522799E-15 ) ) ;
#45422 = ORIENTED_EDGE ( 'NONE', *, *, #92443, .F. ) ;
#45421 = AXIS2_PLACEMENT_3D ( 'NONE', #152263, #109243, #14022 ) ;
#45423 = ORIENTED_EDGE ( 'NONE', *, *, #204635, .T. ) ;
#45424 = VECTOR ( 'NONE', #99047, 1000.000000000000000 ) ;
#45425 = VECTOR ( 'NONE', #22019, 1000.000000000000000 ) ;
#45426 = ORIENTED_EDGE ( 'NONE', *, *, #56936, .F. ) ;
#45427 = AXIS2_PLACEMENT_3D ( 'NONE', #50813, #148672, #74291 ) ;
#45428 = CARTESIAN_POINT ( 'NONE',  ( 21.76363531954645936, 7.012936547882880234, -33.40099812570054638 ) ) ;
#45429 = CYLINDRICAL_SURFACE ( 'NONE', #24087, 0.5000000000000004441 ) ;
#45430 = CARTESIAN_POINT ( 'NONE',  ( -18.50000000000000000, -1.736257131586239844, -45.06865232901750318 ) ) ;
#45431 = DIRECTION ( 'NONE',  ( 0.000000000000000000, 0.8814952561688430555, -0.4721928772777346239 ) ) ;
#45432 = SPHERICAL_SURFACE ( 'NONE', #155145, 0.1000000000000000056 ) ;
#45433 = EDGE_CURVE ( 'NONE', #163312, #37415, #30255, .T. ) ;
#45435 = CARTESIAN_POINT ( 'NONE',  ( 23.24999999999999289, 69.55000000001253113, -182.3731074845244109 ) ) ;
#45434 = CARTESIAN_POINT ( 'NONE',  ( 21.07928932188134397, 69.67148334361836248, -69.62200263017875557 ) ) ;
#45437 = ORIENTED_EDGE ( 'NONE', *, *, #165402, .F. ) ;
#45436 = CARTESIAN_POINT ( 'NONE',  ( 18.50000000000000355, 77.31102155260600739, -241.6627732871349963 ) ) ;
#45438 = CARTESIAN_POINT ( 'NONE',  ( -22.49806830649814060, 11.64988965485023620, -100.4225356836745249 ) ) ;
#45439 = ORIENTED_EDGE ( 'NONE', *, *, #242937, .F. ) ;
#45440 = CARTESIAN_POINT ( 'NONE',  ( -23.15000000000000213, 76.00000000001244871, -170.0231074845243597 ) ) ;
#45441 = ORIENTED_EDGE ( 'NONE', *, *, #151832, .T. ) ;
#45442 = ORIENTED_EDGE ( 'NONE', *, *, #55748, .F. ) ;
#45443 = CARTESIAN_POINT ( 'NONE',  ( -18.59999999999999787, 64.35000000001157616, -57.37310748452440379 ) ) ;
#45444 = LINE ( 'NONE', #7599, #26847 ) ;
#45445 = CARTESIAN_POINT ( 'NONE',  ( -16.87333278164147288, 66.11739021543263561, -49.15627529067739943 ) ) ;
#45446 = CARTESIAN_POINT ( 'NONE',  ( -23.25000000000000355, 70.35000000001230092, -157.3731074845244109 ) ) ;
#45447 = DIRECTION ( 'NONE',  ( -0.000000000000000000, 0.1686199900910312910, -0.9856811345164826488 ) ) ;
#45448 = ORIENTED_EDGE ( 'NONE', *, *, #69036, .T. ) ;
#45449 = ORIENTED_EDGE ( 'NONE', *, *, #184069, .F. ) ;
#45450 = DIRECTION ( 'NONE',  ( -0.000000000000000000, -0.000000000000000000, -1.000000000000000000 ) ) ;
#45451 = ORIENTED_EDGE ( 'NONE', *, *, #246410, .T. ) ;
#45452 = DIRECTION ( 'NONE',  ( 1.000000000000000000, 0.000000000000000000, 0.000000000000000000 ) ) ;
#45453 = DIRECTION ( 'NONE',  ( -1.000000000000000000, -0.000000000000000000, -0.000000000000000000 ) ) ;
#45454 = DIRECTION ( 'NONE',  ( -0.000000000000000000, -1.000000000000000000, -1.734723475976807292E-15 ) ) ;
#45455 = CARTESIAN_POINT ( 'NONE',  ( 22.24259225415828922, -1.497494999994575471, -193.6585794405570766 ) ) ;
#45456 = CARTESIAN_POINT ( 'NONE',  ( -17.01764560440453877, 66.05000000001209060, -123.7731074853111721 ) ) ;
#45457 = DIRECTION ( 'NONE',  ( 1.000000000000000000, 0.000000000000000000, 0.000000000000000000 ) ) ;
#45458 = EDGE_LOOP ( 'NONE', ( #234765, #50814, #188657, #212786, #76643, #147217, #244023, #254436, #209778, #126988, #106343, #65862, #93022 ) ) ;
#45459 = DIRECTION ( 'NONE',  ( -1.020425574104004196E-15, 0.2617529984165031243, 0.9651348961777157509 ) ) ;
#45460 = AXIS2_PLACEMENT_3D ( 'NONE', #215125, #54758, #134284 ) ;
#45461 = DIRECTION ( 'NONE',  ( 1.000000000000000000, 0.000000000000000000, 0.000000000000000000 ) ) ;
#45462 = LINE ( 'NONE', #125014, #133493 ) ;
#45463 = AXIS2_PLACEMENT_3D ( 'NONE', #222937, #204654, #127713 ) ;
#45464 = DIRECTION ( 'NONE',  ( 1.000000000000000000, 3.265361837132813093E-16, -0.000000000000000000 ) ) ;
#45465 = CYLINDRICAL_SURFACE ( 'NONE', #258062, 0.09999999999998898659 ) ;
#45466 = VECTOR ( 'NONE', #139151, 1000.000000000000000 ) ;
#45467 = CARTESIAN_POINT ( 'NONE',  ( 18.39999999999999858, 77.13860723519891849, -241.8264964602989266 ) ) ;
#45468 = VECTOR ( 'NONE', #8240, 1000.000000000000000 ) ;
#45469 = EDGE_CURVE ( 'NONE', #218153, #35062, #92207, .T. ) ;
#45470 = ORIENTED_EDGE ( 'NONE', *, *, #50223, .F. ) ;
#45471 = CARTESIAN_POINT ( 'NONE',  ( 18.54999999999999716, 67.25000000001155342, -56.87310748452438247 ) ) ;
#45472 = ORIENTED_EDGE ( 'NONE', *, *, #237291, .T. ) ;
#45473 = ADVANCED_FACE ( 'NONE', ( #226575 ), #12711, .T. ) ;
#45474 = DIRECTION ( 'NONE',  ( 0.000000000000000000, -1.000000000000000000, -2.891205793294679805E-16 ) ) ;
#45475 = DIRECTION ( 'NONE',  ( 0.000000000000000000, 0.9654727137038715545, 0.2605042016806676242 ) ) ;
#45476 = CARTESIAN_POINT ( 'NONE',  ( -23.15000000000000213, 64.35000000001228670, -157.8731074845244393 ) ) ;
#45477 = AXIS2_PLACEMENT_3D ( 'NONE', #24361, #4745, #32068 ) ;
#45478 = ORIENTED_EDGE ( 'NONE', *, *, #229119, .F. ) ;
#45479 = DIRECTION ( 'NONE',  ( -1.000000000000000000, 0.000000000000000000, 0.000000000000000000 ) ) ;
#45480 = AXIS2_PLACEMENT_3D ( 'NONE', #74572, #160513, #37998 ) ;
#45481 = DIRECTION ( 'NONE',  ( 0.000000000000000000, 0.4088369013363281068, -0.9126074666063770380 ) ) ;
#45482 = ADVANCED_FACE ( 'NONE', ( #247435 ), #26159, .T. ) ;
#45483 = ADVANCED_FACE ( 'NONE', ( #225284 ), #88335, .T. ) ;
#45484 = DIRECTION ( 'NONE',  ( 0.000000000000000000, 0.000000000000000000, -1.000000000000000000 ) ) ;
#45485 = DIRECTION ( 'NONE',  ( 0.000000000000000000, 0.000000000000000000, 1.000000000000000000 ) ) ;
#45486 = DIRECTION ( 'NONE',  ( 0.000000000000000000, -0.8068669527897506244, -0.5907332058516622242 ) ) ;
#45487 = AXIS2_PLACEMENT_3D ( 'NONE', #25104, #82448, #366 ) ;
#45488 = CARTESIAN_POINT ( 'NONE',  ( -21.44999999999999929, 7.350000000011155166, -121.7500000000000426 ) ) ;
#45489 = VERTEX_POINT ( 'NONE', #71394 ) ;
#45490 = DIRECTION ( 'NONE',  ( 1.000000000000000000, -2.952720810173289112E-16, -2.061873921506763405E-30 ) ) ;
#45492 = ORIENTED_EDGE ( 'NONE', *, *, #195482, .F. ) ;
#45491 = CARTESIAN_POINT ( 'NONE',  ( 22.39999999999999503, 11.75000000000000000, -3.469446951953614189E-15 ) ) ;
#45493 = CARTESIAN_POINT ( 'NONE',  ( -18.59999999999999787, 68.58368164137472434, -224.2353459317783120 ) ) ;
#45494 = EDGE_CURVE ( 'NONE', #60194, #45673, #148343, .T. ) ;
#45495 = DIRECTION ( 'NONE',  ( 1.000000000000000000, 0.000000000000000000, -0.000000000000000000 ) ) ;
#45496 = EDGE_CURVE ( 'NONE', #78009, #95420, #255020, .T. ) ;
#45497 = VERTEX_POINT ( 'NONE', #30998 ) ;
#45498 = FACE_OUTER_BOUND ( 'NONE', #17919, .T. ) ;
#45499 = EDGE_CURVE ( 'NONE', #100973, #137777, #229173, .T. ) ;
#45500 = DIRECTION ( 'NONE',  ( 0.000000000000000000, 0.000000000000000000, -1.000000000000000000 ) ) ;
#45501 = ORIENTED_EDGE ( 'NONE', *, *, #85096, .T. ) ;
#45502 = DIRECTION ( 'NONE',  ( -1.000000000000000000, 0.000000000000000000, 0.000000000000000000 ) ) ;
#45503 = CARTESIAN_POINT ( 'NONE',  ( 12.48201962039796342, 9.376659938544690931, -185.1281925482172426 ) ) ;
#45504 = CIRCLE ( 'NONE', #70664, 11.79999999999999716 ) ;
#45505 = EDGE_CURVE ( 'NONE', #238500, #23132, #130043, .T. ) ;
#45506 = CYLINDRICAL_SURFACE ( 'NONE', #245371, 4.000000000000002665 ) ;
#45507 = ORIENTED_EDGE ( 'NONE', *, *, #122087, .T. ) ;
#45508 = EDGE_CURVE ( 'NONE', #54287, #214183, #208339, .T. ) ;
#45509 = EDGE_LOOP ( 'NONE', ( #210578, #142761, #60880, #213064 ) ) ;
#45510 = EDGE_CURVE ( 'NONE', #67305, #135358, #192748, .T. ) ;
#45511 = CARTESIAN_POINT ( 'NONE',  ( 21.05000000000000071, 10.56271494673974232, -74.45680210564449908 ) ) ;
#45512 = EDGE_CURVE ( 'NONE', #43656, #115992, #184341, .T. ) ;
#45513 = CARTESIAN_POINT ( 'NONE',  ( -23.25000000000000000, -8.999999999988844479, -158.2060308773475867 ) ) ;
#45514 = CARTESIAN_POINT ( 'NONE',  ( -13.39999999999994529, 67.75000000001118394, -23.62310748452479103 ) ) ;
#45515 = CARTESIAN_POINT ( 'NONE',  ( -21.65000000000000213, 65.95000000001255103, -182.6731074845244223 ) ) ;
#45516 = DIRECTION ( 'NONE',  ( 0.000000000000000000, 0.2617529984165035684, 0.9651348961777156399 ) ) ;
#45517 = DIRECTION ( 'NONE',  ( 1.000000000000000000, 0.000000000000000000, 0.000000000000000000 ) ) ;
#45518 = LINE ( 'NONE', #11542, #109927 ) ;
#45520 = DIRECTION ( 'NONE',  ( 0.000000000000000000, 0.000000000000000000, -1.000000000000000000 ) ) ;
#45519 = CARTESIAN_POINT ( 'NONE',  ( -18.40000000000000213, 11.74999999999998224, -24.25000000000001066 ) ) ;
#45521 = AXIS2_PLACEMENT_3D ( 'NONE', #85583, #106441, #167760 ) ;
#45523 = CARTESIAN_POINT ( 'NONE',  ( 23.14999999999999503, 64.35000000001197407, -115.1731074845243796 ) ) ;
#45522 = AXIS2_PLACEMENT_3D ( 'NONE', #254175, #75585, #115982 ) ;
#45524 = DIRECTION ( 'NONE',  ( -1.000000000000000000, -0.000000000000000000, 0.000000000000000000 ) ) ;
#45525 = FACE_OUTER_BOUND ( 'NONE', #99402, .T. ) ;
#45526 = CIRCLE ( 'NONE', #166358, 0.2000000000000057288 ) ;
#45527 = AXIS2_PLACEMENT_3D ( 'NONE', #231436, #93183, #172776 ) ;
#45528 = ORIENTED_EDGE ( 'NONE', *, *, #110442, .F. ) ;
#45529 = VERTEX_POINT ( 'NONE', #106621 ) ;
#45530 = CARTESIAN_POINT ( 'NONE',  ( 23.14999999999998437, 1.115600667400684642E-11, -100.5000000000000284 ) ) ;
#45531 = DIRECTION ( 'NONE',  ( 0.000000000000000000, 0.000000000000000000, 1.000000000000000000 ) ) ;
#45533 = CARTESIAN_POINT ( 'NONE',  ( -12.48127053791145791, 12.91284736048185344, -216.2278651779593304 ) ) ;
#45532 = DIRECTION ( 'NONE',  ( 0.000000000000000000, 0.8814952561688429444, -0.4721928772777349015 ) ) ;
#45534 = CIRCLE ( 'NONE', #62104, 0.1000000000000028644 ) ;
#45535 = EDGE_CURVE ( 'NONE', #104826, #255232, #7545, .T. ) ;
#45536 = CARTESIAN_POINT ( 'NONE',  ( 20.95052659398289308, 39.28760495060160451, -236.8901595946551311 ) ) ;
#45538 = EDGE_CURVE ( 'NONE', #174969, #13316, #67515, .T. ) ;
#45537 = DIRECTION ( 'NONE',  ( 0.000000000000000000, 0.000000000000000000, 1.000000000000000000 ) ) ;
#45539 = CARTESIAN_POINT ( 'NONE',  ( -15.75000000000000355, 9.350000000011140955, -150.7500000000000284 ) ) ;
#45540 = DIRECTION ( 'NONE',  ( 0.000000000000000000, 6.982962677686266711E-15, -1.000000000000000000 ) ) ;
#45541 = ORIENTED_EDGE ( 'NONE', *, *, #28833, .F. ) ;
#45542 = AXIS2_PLACEMENT_3D ( 'NONE', #29668, #229126, #90888 ) ;
#45543 = AXIS2_PLACEMENT_3D ( 'NONE', #11814, #59867, #239829 ) ;
#45544 = ADVANCED_FACE ( 'NONE', ( #127498 ), #207038, .T. ) ;
#45546 = AXIS2_PLACEMENT_3D ( 'NONE', #21547, #101016, #26699 ) ;
#45545 = CARTESIAN_POINT ( 'NONE',  ( -20.94999999999999929, 4.384524567800934136, -245.2091454203640239 ) ) ;
#45547 = ORIENTED_EDGE ( 'NONE', *, *, #219347, .T. ) ;
#45548 = DIRECTION ( 'NONE',  ( 1.000000000000000000, 0.000000000000000000, -0.000000000000000000 ) ) ;
#45549 = AXIS2_PLACEMENT_3D ( 'NONE', #186871, #231140, #245551 ) ;
#45550 = DIRECTION ( 'NONE',  ( 0.000000000000000000, -0.4721928772777258532, -0.8814952561688478294 ) ) ;
#45551 = ORIENTED_EDGE ( 'NONE', *, *, #152843, .F. ) ;
#45552 = DIRECTION ( 'NONE',  ( -0.000000000000000000, -6.982962677686266711E-15, 1.000000000000000000 ) ) ;
#45553 =( BOUNDED_CURVE ( )  B_SPLINE_CURVE ( 3, ( #142690, #81418, #160998, #601 ),
 .UNSPECIFIED., .F., .F. ) 
 B_SPLINE_CURVE_WITH_KNOTS ( ( 4, 4 ),
 ( 1.570796326794908992, 2.617993877991515284 ),
 .UNSPECIFIED. ) 
 CURVE ( )  GEOMETRIC_REPRESENTATION_ITEM ( )  RATIONAL_B_SPLINE_CURVE ( ( 1.000000000000000000, 0.9106836025229576581, 0.9106836025229576581, 1.000000000000000000 ) ) 
 REPRESENTATION_ITEM ( '' )  );
#45554 = ORIENTED_EDGE ( 'NONE', *, *, #135235, .F. ) ;
#45555 = CARTESIAN_POINT ( 'NONE',  ( -18.54118089899631983, 85.46353763186043295, -162.9745298866561711 ) ) ;
#45556 = LINE ( 'NONE', #63839, #107581 ) ;
#45557 = DIRECTION ( 'NONE',  ( -1.000000000000000000, 0.000000000000000000, -0.000000000000000000 ) ) ;
#45558 = EDGE_CURVE ( 'NONE', #46643, #137948, #11412, .T. ) ;
#45559 = CARTESIAN_POINT ( 'NONE',  ( 18.52165635395197896, -9.481150711271054021, -141.0248375828624319 ) ) ;
#45560 = DIRECTION ( 'NONE',  ( 1.000000000000000000, -0.000000000000000000, 0.000000000000000000 ) ) ;
#45561 = CARTESIAN_POINT ( 'NONE',  ( -21.14999999999999858, 6.540656951712397138, -134.0000000000000000 ) ) ;
#45562 = CYLINDRICAL_SURFACE ( 'NONE', #34453, 0.1000000000000000472 ) ;
#45563 = DIRECTION ( 'NONE',  ( 0.000000000000000000, 0.000000000000000000, 1.000000000000000000 ) ) ;
#45564 = ADVANCED_FACE ( 'NONE', ( #146813 ), #128556, .T. ) ;
#45566 = EDGE_LOOP ( 'NONE', ( #12679, #101942, #7879, #60698 ) ) ;
#45565 = DIRECTION ( 'NONE',  ( 0.000000000000000000, -6.982962677686266711E-15, 1.000000000000000000 ) ) ;
#45568 = CYLINDRICAL_SURFACE ( 'NONE', #105970, 0.1000000000000046685 ) ;
#45567 = CARTESIAN_POINT ( 'NONE',  ( -16.78270389226384296, 66.05262738339500572, -115.6819004476129038 ) ) ;
#45569 = ORIENTED_EDGE ( 'NONE', *, *, #31430, .F. ) ;
#45571 = ORIENTED_EDGE ( 'NONE', *, *, #167142, .F. ) ;
#45570 = DIRECTION ( 'NONE',  ( 0.000000000000000000, 0.000000000000000000, -1.000000000000000000 ) ) ;
#45572 = AXIS2_PLACEMENT_3D ( 'NONE', #211052, #149812, #93662 ) ;
#45573 = VERTEX_POINT ( 'NONE', #33344 ) ;
#45574 = DIRECTION ( 'NONE',  ( 1.000000000000000000, -2.952720810173289112E-16, -2.061873921506763405E-30 ) ) ;
#45575 = CARTESIAN_POINT ( 'NONE',  ( -20.94999999999999929, -5.637547571910522137, -233.4427589080015650 ) ) ;
#45576 = EDGE_CURVE ( 'NONE', #243852, #109777, #205182, .T. ) ;
#45577 = ADVANCED_FACE ( 'NONE', ( #191121 ), #245942, .F. ) ;
#45578 = DIRECTION ( 'NONE',  ( -1.000000000000000000, 0.000000000000000000, -0.000000000000000000 ) ) ;
#45579 = CARTESIAN_POINT ( 'NONE',  ( -20.85000000000000142, 87.65000000001246860, -172.9231074845242802 ) ) ;
#45580 = VECTOR ( 'NONE', #17219, 1000.000000000000114 ) ;
#45581 = CARTESIAN_POINT ( 'NONE',  ( 23.24999999999999289, 6.450000000011156587, -88.75000000000004263 ) ) ;
#45582 = ADVANCED_FACE ( 'NONE', ( #226343 ), #51544, .T. ) ;
#45583 = ORIENTED_EDGE ( 'NONE', *, *, #25153, .F. ) ;
#45584 = CARTESIAN_POINT ( 'NONE',  ( -16.78805706634180694, 51.61424155150325532, -231.9504541878317809 ) ) ;
#45585 = DIRECTION ( 'NONE',  ( 7.304098846218134667E-16, 1.000000000000000000, 6.982962677686266711E-15 ) ) ;
#45586 = ORIENTED_EDGE ( 'NONE', *, *, #85648, .F. ) ;
#45587 = ORIENTED_EDGE ( 'NONE', *, *, #162436, .F. ) ;
#45588 = AXIS2_PLACEMENT_3D ( 'NONE', #194935, #115371, #218302 ) ;
#45589 = DIRECTION ( 'NONE',  ( 1.000000000000000000, 0.000000000000000000, 0.000000000000000000 ) ) ;
#45590 = VECTOR ( 'NONE', #121566, 1000.000000000000114 ) ;
#45591 = EDGE_CURVE ( 'NONE', #16939, #233320, #113625, .T. ) ;
#45592 = ORIENTED_EDGE ( 'NONE', *, *, #189092, .F. ) ;
#45593 = CARTESIAN_POINT ( 'NONE',  ( -23.25000000000000000, 2.600000000011156054, -53.77537807723790309 ) ) ;
#45596 = EDGE_CURVE ( 'NONE', #70740, #242169, #72449, .T. ) ;
#45595 = EDGE_LOOP ( 'NONE', ( #103415, #13057, #6830, #5122 ) ) ;
#45594 = CIRCLE ( 'NONE', #83136, 0.1999999999999987899 ) ;
#45597 = CARTESIAN_POINT ( 'NONE',  ( -20.64999999999999858, 4.662003332185090443, -213.0075696128765514 ) ) ;
#45598 = LINE ( 'NONE', #44324, #88525 ) ;
#45599 = DIRECTION ( 'NONE',  ( -0.000000000000000000, 0.2617529984165031243, 0.9651348961777157509 ) ) ;
#45600 = EDGE_CURVE ( 'NONE', #52358, #82377, #180276, .T. ) ;
#45601 = CARTESIAN_POINT ( 'NONE',  ( -20.94999999999999929, 1.115600667400684642E-11, -67.00000000000000000 ) ) ;
#45602 = CARTESIAN_POINT ( 'NONE',  ( 21.05000012384916275, 10.62872029888669978, -179.6779773300349632 ) ) ;
#45603 = EDGE_LOOP ( 'NONE', ( #248362, #105788 ) ) ;
#45604 = AXIS2_PLACEMENT_3D ( 'NONE', #30088, #130437, #147438 ) ;
#45605 = CIRCLE ( 'NONE', #133094, 0.1000000000000028644 ) ;
#45606 = CARTESIAN_POINT ( 'NONE',  ( 18.59999999999999076, 10.20857864377385127, -121.7500000000000426 ) ) ;
#45607 = DIRECTION ( 'NONE',  ( 0.000000000000000000, -0.1568667991644355497, 0.9876197685951332295 ) ) ;
#45608 = CARTESIAN_POINT ( 'NONE',  ( 21.05000000000000071, -0.9150442794618677267, -196.7984890852705746 ) ) ;
#45609 = DIRECTION ( 'NONE',  ( 1.000000000000000000, 0.000000000000000000, 0.000000000000000000 ) ) ;
#45611 = ORIENTED_EDGE ( 'NONE', *, *, #195879, .F. ) ;
#45610 = ADVANCED_FACE ( 'NONE', ( #231517 ), #122192, .F. ) ;
#45613 = DIRECTION ( 'NONE',  ( 1.000000000000000000, -0.000000000000000000, -0.000000000000000000 ) ) ;
#45612 = DIRECTION ( 'NONE',  ( 0.000000000000000000, -0.2128009952263604232, 0.9770955615653316162 ) ) ;
#45614 = ORIENTED_EDGE ( 'NONE', *, *, #40530, .T. ) ;
#45617 = ORIENTED_EDGE ( 'NONE', *, *, #128956, .T. ) ;
#45616 = CARTESIAN_POINT ( 'NONE',  ( -15.75000000000000355, 66.15000000001258229, -186.7731074845244166 ) ) ;
#45615 = SURFACE_STYLE_USAGE ( .BOTH. , #78299 ) ;
#45618 = VECTOR ( 'NONE', #69843, 1000.000000000000000 ) ;
#45619 = ORIENTED_EDGE ( 'NONE', *, *, #21143, .T. ) ;
#45620 = FACE_OUTER_BOUND ( 'NONE', #176601, .T. ) ;
#45621 = VECTOR ( 'NONE', #11226, 1000.000000000000000 ) ;
#45622 = CIRCLE ( 'NONE', #8030, 11.74999999999999645 ) ;
#45623 = AXIS2_PLACEMENT_3D ( 'NONE', #230454, #127504, #87065 ) ;
#45624 = CARTESIAN_POINT ( 'NONE',  ( -20.64999999999999858, 1.925233644870972816, -180.2302435331260995 ) ) ;
#45625 = ADVANCED_FACE ( 'NONE', ( #8611 ), #28205, .F. ) ;
#45626 = FACE_OUTER_BOUND ( 'NONE', #229785, .T. ) ;
#45627 = EDGE_LOOP ( 'NONE', ( #53257, #61398, #98764, #249649, #159832, #103194, #27542, #128745, #87260, #203777, #255056, #181368, #223270, #61473, #14296, #86027, #1330, #253553 ) ) ;
#45628 = DIRECTION ( 'NONE',  ( 0.000000000000000000, 0.000000000000000000, 1.000000000000000000 ) ) ;
#45629 = VECTOR ( 'NONE', #7557, 1000.000000000000000 ) ;
#45630 = EDGE_CURVE ( 'NONE', #173345, #105678, #52853, .T. ) ;
#45631 = CARTESIAN_POINT ( 'NONE',  ( -22.50014994444008209, 11.74971973189209606, 0.08308015671916883782 ) ) ;
#45632 = EDGE_CURVE ( 'NONE', #216543, #230388, #138703, .T. ) ;
#45634 = EDGE_LOOP ( 'NONE', ( #199665, #165807, #22808, #212676, #19617, #166538, #215244, #147861, #253144, #95436 ) ) ;
#45633 = LINE ( 'NONE', #83434, #134987 ) ;
#45635 = ORIENTED_EDGE ( 'NONE', *, *, #234865, .F. ) ;
#45636 = CARTESIAN_POINT ( 'NONE',  ( -18.59999999999999787, 1.115600667400684642E-11, -67.00000000000000000 ) ) ;
#45637 = VECTOR ( 'NONE', #80978, 1000.000000000000000 ) ;
#45638 = DIRECTION ( 'NONE',  ( -1.000000000000000000, -0.000000000000000000, 0.000000000000000000 ) ) ;
#45639 = DIRECTION ( 'NONE',  ( 0.000000000000000000, -6.982962677686266711E-15, 1.000000000000000000 ) ) ;
#45640 = ORIENTED_EDGE ( 'NONE', *, *, #178611, .T. ) ;
#45641 = CARTESIAN_POINT ( 'NONE',  ( -16.87683809663752754, 9.864913447291344895, -187.7242815513039602 ) ) ;
#45642 = ORIENTED_EDGE ( 'NONE', *, *, #76267, .T. ) ;
#45643 = CARTESIAN_POINT ( 'NONE',  ( -21.05000000000000071, 67.23127455305841238, -235.8551265064783991 ) ) ;
#45645 = EDGE_CURVE ( 'NONE', #77194, #71592, #155534, .T. ) ;
#45644 = DIRECTION ( 'NONE',  ( 0.000000000000000000, -8.881784197001832136E-16, -1.000000000000000000 ) ) ;
#45646 = DIRECTION ( 'NONE',  ( 1.000000000000000000, 7.492892343619937423E-30, -1.073024830501117725E-15 ) ) ;
#45647 = VERTEX_POINT ( 'NONE', #108975 ) ;
#45648 = DIRECTION ( 'NONE',  ( 0.000000000000000000, -0.2617529984165031243, -0.9651348961777157509 ) ) ;
#45649 = AXIS2_PLACEMENT_3D ( 'NONE', #3578, #205624, #200508 ) ;
#45650 = DIRECTION ( 'NONE',  ( 0.000000000000000000, 0.000000000000000000, -1.000000000000000000 ) ) ;
#45651 = ORIENTED_EDGE ( 'NONE', *, *, #256209, .T. ) ;
#45652 = EDGE_LOOP ( 'NONE', ( #198215, #182697, #10483, #25084 ) ) ;
#45653 =( BOUNDED_SURFACE ( )  B_SPLINE_SURFACE ( 3, 2, ( 
 ( #186967, #89118, #129541 ),
 ( #51248, #231224, #249495 ),
 ( #189519, #66988, #69576 ),
 ( #209071, #47409, #9576 ),
 ( #106087, #87810, #147825 ),
 ( #188223, #10880, #48701 ),
 ( #245631, #107392, #90396 ),
 ( #167402, #246899, #169992 ),
 ( #207817, #128258, #130812 ),
 ( #210366, #250757, #91691 ) ),
 .UNSPECIFIED., .F., .F., .T. ) 
 B_SPLINE_SURFACE_WITH_KNOTS ( ( 4, 2, 2, 2, 4 ),
 ( 3, 3 ),
 ( 0.002161241639767785133, 0.002579950749617447234, 0.002789305304542278284, 0.002893982582004694243, 0.002998659859467109768 ),
 ( 0.000000000000000000, 1.000000000000000000 ),
 .UNSPECIFIED. ) 
 GEOMETRIC_REPRESENTATION_ITEM ( )  RATIONAL_B_SPLINE_SURFACE ( (
 ( 1.000000000000000000, 0.7071067811864985009, 1.000000000000000000),
 ( 1.000000000000000000, 0.7632447400663812109, 1.000000000000000000),
 ( 1.000000000000000000, 0.8158073005109720555, 1.000000000000000000),
 ( 1.000000000000000000, 0.8906973462395535446, 1.000000000000000000),
 ( 1.000000000000000000, 0.9149408947797246228, 1.000000000000000000),
 ( 1.000000000000000000, 0.9493368785277208621, 1.000000000000000000),
 ( 1.000000000000000000, 0.9605194247156264575, 1.000000000000000000),
 ( 1.000000000000000000, 0.9803630264781529879, 1.000000000000000000),
 ( 1.000000000000000000, 0.9900844824270880196, 1.000000000000000000),
 ( 1.000000000000000000, 0.9894588281429241849, 1.000000000000000000) ) ) 
 REPRESENTATION_ITEM ( '' )  SURFACE ( )  );
#45654 = ORIENTED_EDGE ( 'NONE', *, *, #2280, .T. ) ;
#45655 = CARTESIAN_POINT ( 'NONE',  ( -22.39999999999999858, 26.02743912001966464, -254.3139371321002216 ) ) ;
#45656 = ADVANCED_FACE ( 'NONE', ( #89414 ), #143001, .F. ) ;
#45657 = ORIENTED_EDGE ( 'NONE', *, *, #193558, .F. ) ;
#45659 = ORIENTED_EDGE ( 'NONE', *, *, #150387, .T. ) ;
#45658 = CARTESIAN_POINT ( 'NONE',  ( 12.48201962039797763, 66.62334006147904120, -185.8949149363072024 ) ) ;
#45660 = ORIENTED_EDGE ( 'NONE', *, *, #177478, .F. ) ;
#45662 = ORIENTED_EDGE ( 'NONE', *, *, #65280, .T. ) ;
#45661 = ORIENTED_EDGE ( 'NONE', *, *, #174087, .F. ) ;
#45663 = AXIS2_PLACEMENT_3D ( 'NONE', #53375, #151203, #134182 ) ;
#45664 = DIRECTION ( 'NONE',  ( -0.000000000000000000, -0.4721928772777346239, -0.8814952561688430555 ) ) ;
#45665 = ORIENTED_EDGE ( 'NONE', *, *, #15821, .F. ) ;
#45666 = CYLINDRICAL_SURFACE ( 'NONE', #6512, 0.1000000000000028644 ) ;
#45667 = EDGE_CURVE ( 'NONE', #144818, #40557, #11178, .T. ) ;
#45668 = AXIS2_PLACEMENT_3D ( 'NONE', #237826, #37088, #257325 ) ;
#45669 = CARTESIAN_POINT ( 'NONE',  ( 21.04999999999999716, 67.10527618163501984, -195.0360231613764199 ) ) ;
#45670 = CARTESIAN_POINT ( 'NONE',  ( -18.36527282682019191, 86.98067533972476895, -199.3289536043583325 ) ) ;
#45671 = EDGE_LOOP ( 'NONE', ( #239280, #240975, #246468, #62200, #15139 ) ) ;
#45673 = VERTEX_POINT ( 'NONE', #170294 ) ;
#45672 = DIRECTION ( 'NONE',  ( 0.000000000000000000, -1.000000000000000000, 0.000000000000000000 ) ) ;
#45674 = LINE ( 'NONE', #125217, #209139 ) ;
#45676 = VERTEX_POINT ( 'NONE', #131111 ) ;
#45675 = FACE_OUTER_BOUND ( 'NONE', #202802, .T. ) ;
#45677 = VERTEX_POINT ( 'NONE', #171563 ) ;
#45678 = DIRECTION ( 'NONE',  ( 1.000000000000000000, -0.000000000000000000, 0.000000000000000000 ) ) ;
#45679 = ORIENTED_EDGE ( 'NONE', *, *, #193195, .F. ) ;
#45680 = ORIENTED_EDGE ( 'NONE', *, *, #129978, .T. ) ;
#45681 = AXIS2_PLACEMENT_3D ( 'NONE', #68672, #209453, #13830 ) ;
#45682 = DIRECTION ( 'NONE',  ( 1.000000000000000000, -0.000000000000000000, 0.000000000000000000 ) ) ;
#45683 = DIRECTION ( 'NONE',  ( -1.000000000000000000, 0.000000000000000000, 0.000000000000000000 ) ) ;
#45685 = ORIENTED_EDGE ( 'NONE', *, *, #219789, .F. ) ;
#45684 = ORIENTED_EDGE ( 'NONE', *, *, #156338, .F. ) ;
#45686 = VERTEX_POINT ( 'NONE', #251051 ) ;
#45687 = DIRECTION ( 'NONE',  ( -1.000000000000000000, 0.000000000000000000, 0.000000000000000000 ) ) ;
#45688 = VERTEX_POINT ( 'NONE', #132408 ) ;
#45689 = ORIENTED_EDGE ( 'NONE', *, *, #256763, .T. ) ;
#45690 = CARTESIAN_POINT ( 'NONE',  ( -20.54999999999999716, 9.350000000000001421, -21.25000000000000000 ) ) ;
#45692 = ORIENTED_EDGE ( 'NONE', *, *, #113535, .T. ) ;
#45691 = LINE ( 'NONE', #103075, #247524 ) ;
#45693 = FACE_OUTER_BOUND ( 'NONE', #170287, .T. ) ;
#45695 = CARTESIAN_POINT ( 'NONE',  ( -23.25000000000000355, 44.18585876254595490, -235.1667871698132046 ) ) ;
#45694 = CARTESIAN_POINT ( 'NONE',  ( -23.15000000000000213, 1.115600667400684642E-11, -96.50000000000004263 ) ) ;
#45696 = CARTESIAN_POINT ( 'NONE',  ( 23.14999999999999503, 69.35000000001151932, -48.17310748452437252 ) ) ;
#45697 = VERTEX_POINT ( 'NONE', #211957 ) ;
#45698 = EDGE_CURVE ( 'NONE', #191619, #231923, #213767, .T. ) ;
#45699 = ORIENTED_EDGE ( 'NONE', *, *, #24196, .F. ) ;
#45701 = AXIS2_PLACEMENT_3D ( 'NONE', #16368, #175445, #218377 ) ;
#45700 = DIRECTION ( 'NONE',  ( -0.000000000000000000, 0.9908441862701591329, 0.1350103645451946055 ) ) ;
#45702 = DIRECTION ( 'NONE',  ( 0.000000000000000000, -0.8660254037844411501, -0.4999999999999956146 ) ) ;
#45703 = VECTOR ( 'NONE', #66905, 1000.000000000000000 ) ;
#45704 = AXIS2_PLACEMENT_3D ( 'NONE', #209097, #253355, #113848 ) ;
#45705 = TOROIDAL_SURFACE ( 'NONE', #66565, 11.90000000000000391, 0.1000000000000000056 ) ;
#45706 = ORIENTED_EDGE ( 'NONE', *, *, #172243, .F. ) ;
#45707 = CIRCLE ( 'NONE', #8119, 2.000000000000001776 ) ;
#45708 = CARTESIAN_POINT ( 'NONE',  ( -20.64999999999999858, -9.500000000000003553, -9.893969122652444881 ) ) ;
#45709 = ORIENTED_EDGE ( 'NONE', *, *, #835, .F. ) ;
#45710 = ORIENTED_EDGE ( 'NONE', *, *, #186063, .T. ) ;
#45711 = EDGE_CURVE ( 'NONE', #96815, #244896, #34609, .T. ) ;
#45712 = CARTESIAN_POINT ( 'NONE',  ( -23.15000000000000213, 54.22301550979020845, -237.0256805049050115 ) ) ;
#45713 = B_SPLINE_CURVE_WITH_KNOTS ( 'NONE', 3,
 ( #52009, #69047, #148569, #246383, #168173, #205965, #172021 ),
 .UNSPECIFIED., .F., .F.,
 ( 4, 3, 4 ),
 ( 3.469446951953614189E-18, 3.882884552234413058E-05, 5.798605692158429121E-05 ),
 .UNSPECIFIED. ) ;
#45714 = ORIENTED_EDGE ( 'NONE', *, *, #76267, .F. ) ;
#45715 = CARTESIAN_POINT ( 'NONE',  ( -20.94999999999999929, 11.75000000001115197, -107.5148057706540357 ) ) ;
#45716 = CARTESIAN_POINT ( 'NONE',  ( -21.07946286933445279, 6.329037319018850916, -167.4233161567435673 ) ) ;
#45717 = VERTEX_POINT ( 'NONE', #76266 ) ;
#45718 = LINE ( 'NONE', #9165, #118910 ) ;
#45719 = DIRECTION ( 'NONE',  ( -1.000000000000000000, -0.000000000000000000, -0.000000000000000000 ) ) ;
#45721 = FACE_OUTER_BOUND ( 'NONE', #253781, .T. ) ;
#45720 = CARTESIAN_POINT ( 'NONE',  ( 20.90000000000000213, 6.336640076952988920, 12.03401928653448572 ) ) ;
#45722 = EDGE_CURVE ( 'NONE', #211171, #221991, #217837, .T. ) ;
#45723 = CARTESIAN_POINT ( 'NONE',  ( -16.87331047859651179, 60.93935776605891164, -221.0417277355860790 ) ) ;
#45725 = FACE_OUTER_BOUND ( 'NONE', #241970, .T. ) ;
#45724 = CIRCLE ( 'NONE', #133209, 0.1000000000000028644 ) ;
#45726 = FACE_OUTER_BOUND ( 'NONE', #252811, .T. ) ;
#45727 = VECTOR ( 'NONE', #50, 1000.000000000000000 ) ;
#45728 = DIRECTION ( 'NONE',  ( 1.000000000000000000, 0.000000000000000000, -0.000000000000000000 ) ) ;
#45729 = EDGE_CURVE ( 'NONE', #220255, #189976, #1362, .T. ) ;
#45730 = ORIENTED_EDGE ( 'NONE', *, *, #43630, .T. ) ;
#45731 = AXIS2_PLACEMENT_3D ( 'NONE', #139049, #80366, #219909 ) ;
#45733 = ORIENTED_EDGE ( 'NONE', *, *, #103222, .T. ) ;
#45732 = ORIENTED_EDGE ( 'NONE', *, *, #237083, .T. ) ;
#45734 = ORIENTED_EDGE ( 'NONE', *, *, #133590, .F. ) ;
#45735 = CARTESIAN_POINT ( 'NONE',  ( 22.39999999999999503, 1.115600667400684642E-11, -92.70922040162665212 ) ) ;
#45736 = CARTESIAN_POINT ( 'NONE',  ( -16.86379686415369150, 66.02478224075865398, -82.08971759543409519 ) ) ;
#45737 = EDGE_CURVE ( 'NONE', #208746, #176500, #209845, .T. ) ;
#45739 = CARTESIAN_POINT ( 'NONE',  ( -15.39946565075089779, 9.389534562346700142, -15.67480930438995479 ) ) ;
#45738 = DIRECTION ( 'NONE',  ( -1.000000000000000000, 0.000000000000000000, 0.000000000000000000 ) ) ;
#45740 = CARTESIAN_POINT ( 'NONE',  ( -21.45000000000000284, 44.68681448124952027, -237.5080042326551393 ) ) ;
#45741 = ORIENTED_EDGE ( 'NONE', *, *, #12250, .F. ) ;
#45742 = DIRECTION ( 'NONE',  ( 1.000000000000000000, 3.265361837132813093E-16, -0.000000000000000000 ) ) ;
#45743 = PLANE ( 'NONE',  #58473 ) ;
#45744 = EDGE_CURVE ( 'NONE', #220753, #92384, #134625, .T. ) ;
#45745 = CARTESIAN_POINT ( 'NONE',  ( -16.92989143108098204, 66.05000000001189164, -90.14062360976771515 ) ) ;
#45746 = DIRECTION ( 'NONE',  ( 0.000000000000000000, -0.9947597004326491632, 0.1022405907413782566 ) ) ;
#45747 = VERTEX_POINT ( 'NONE', #254853 ) ;
#45748 = AXIS2_PLACEMENT_3D ( 'NONE', #242149, #127345, #102611 ) ;
#45749 = CARTESIAN_POINT ( 'NONE',  ( 21.93642651522410603, 7.327166239336949438, -134.0000000000000000 ) ) ;
#45750 = DIRECTION ( 'NONE',  ( -0.000000000000000000, 0.8660254037844411501, 0.4999999999999956701 ) ) ;
#45751 = ORIENTED_EDGE ( 'NONE', *, *, #68313, .F. ) ;
#45752 = ORIENTED_EDGE ( 'NONE', *, *, #32918, .F. ) ;
#45753 = LINE ( 'NONE', #40669, #37192 ) ;
#45754 = CARTESIAN_POINT ( 'NONE',  ( -21.00000000000000000, -1.212568896937008089, -8.000000000000000000 ) ) ;
#45755 = CIRCLE ( 'NONE', #179064, 11.64999999999999325 ) ;
#45756 = CARTESIAN_POINT ( 'NONE',  ( -20.64999999999999858, 4.350000000011156054, -45.75000000000000711 ) ) ;
#45757 = DIRECTION ( 'NONE',  ( 1.000000000000000000, 0.000000000000000000, 0.000000000000000000 ) ) ;
#45758 = DIRECTION ( 'NONE',  ( 0.000000000000000000, 0.000000000000000000, -1.000000000000000000 ) ) ;
#45759 = DIRECTION ( 'NONE',  ( 0.000000000000000000, -0.1290532225515364506, -0.9916376685811525427 ) ) ;
#45760 = EDGE_LOOP ( 'NONE', ( #19396, #83261, #60030, #179653 ) ) ;
#45761 = CARTESIAN_POINT ( 'NONE',  ( -18.40000000000000213, 59.60579174656471224, -220.6800530043423976 ) ) ;
#45763 = EDGE_CURVE ( 'NONE', #162415, #14083, #22251, .T. ) ;
#45762 = FACE_OUTER_BOUND ( 'NONE', #134763, .T. ) ;
#45765 = DIRECTION ( 'NONE',  ( 2.952720810173289112E-16, 0.4088369013363281068, -0.9126074666063770380 ) ) ;
#45764 = FACE_OUTER_BOUND ( 'NONE', #21657, .T. ) ;
#45766 = CARTESIAN_POINT ( 'NONE',  ( 21.05000000000000071, 77.25000000001232081, -162.1231074845243540 ) ) ;
#45767 = DIRECTION ( 'NONE',  ( 1.000000000000000000, 0.000000000000000000, 0.000000000000000000 ) ) ;
#45768 = CYLINDRICAL_SURFACE ( 'NONE', #18089, 0.1000000000000028644 ) ;
#45769 = CARTESIAN_POINT ( 'NONE',  ( 18.39999999999999858, -9.499999999988842703, -207.6001893912220169 ) ) ;
#45770 = AXIS2_PLACEMENT_3D ( 'NONE', #103226, #26289, #108390 ) ;
#45772 = EDGE_LOOP ( 'NONE', ( #237236, #53437, #105927, #53514 ) ) ;
#45771 = PLANE ( 'NONE',  #157052 ) ;
#45773 = AXIS2_PLACEMENT_3D ( 'NONE', #234775, #56114, #37883 ) ;
#45774 = EDGE_CURVE ( 'NONE', #256115, #199490, #55499, .T. ) ;
#45775 = VECTOR ( 'NONE', #49952, 1000.000000000000000 ) ;
#45776 = CIRCLE ( 'NONE', #79070, 0.09999999999999080458 ) ;
#45778 = EDGE_CURVE ( 'NONE', #147787, #187556, #201282, .T. ) ;
#45777 = VECTOR ( 'NONE', #8038, 1000.000000000000227 ) ;
#45779 = LINE ( 'NONE', #146157, #195896 ) ;
#45780 = CARTESIAN_POINT ( 'NONE',  ( -18.59999999999999787, 77.16270174995034381, -161.9231074845243370 ) ) ;
#45781 = ADVANCED_FACE ( 'NONE', ( #172864 ), #88843, .T. ) ;
#45782 = DIRECTION ( 'NONE',  ( 1.000000000000000000, 7.049440681616511973E-16, -1.911869773728122111E-16 ) ) ;
#45783 = VERTEX_POINT ( 'NONE', #256128 ) ;
#45784 = EDGE_CURVE ( 'NONE', #121232, #189010, #75029, .T. ) ;
#45785 = AXIS2_PLACEMENT_3D ( 'NONE', #105048, #184628, #225018 ) ;
#45786 = FACE_OUTER_BOUND ( 'NONE', #57732, .T. ) ;
#45787 = VECTOR ( 'NONE', #173574, 1000.000000000000000 ) ;
#45788 = CARTESIAN_POINT ( 'NONE',  ( -20.94999999999999929, -11.48912529306490349, -137.0000000000000000 ) ) ;
#45789 = DIRECTION ( 'NONE',  ( 0.000000000000000000, 6.982962677686266711E-15, -1.000000000000000000 ) ) ;
#45790 = AXIS2_PLACEMENT_3D ( 'NONE', #20405, #84149, #179484 ) ;
#45791 = AXIS2_PLACEMENT_3D ( 'NONE', #244725, #188612, #54233 ) ;
#45792 = EDGE_LOOP ( 'NONE', ( #35826, #219848, #177981, #219915 ) ) ;
#45793 = CYLINDRICAL_SURFACE ( 'NONE', #53713, 0.09999999999999986677 ) ;
#45795 = ORIENTED_EDGE ( 'NONE', *, *, #67783, .F. ) ;
#45794 = CYLINDRICAL_SURFACE ( 'NONE', #21753, 0.09999999999999939493 ) ;
#45797 = DIRECTION ( 'NONE',  ( 1.000000000000000000, -0.000000000000000000, -0.000000000000000000 ) ) ;
#45796 = DIRECTION ( 'NONE',  ( 0.000000000000000000, -0.8814952561688476074, 0.4721928772777262417 ) ) ;
#45798 = CIRCLE ( 'NONE', #70771, 0.1000000000000013933 ) ;
#45799 = EDGE_CURVE ( 'NONE', #190938, #119358, #192929, .T. ) ;
#45800 = LINE ( 'NONE', #88755, #133449 ) ;
#45801 = EDGE_LOOP ( 'NONE', ( #79750, #250906, #20884, #16768 ) ) ;
#45802 = DIRECTION ( 'NONE',  ( 0.000000000000000000, 4.336808689942044242E-14, 1.000000000000000000 ) ) ;
#45803 = EDGE_CURVE ( 'NONE', #138430, #68978, #84541, .T. ) ;
#45804 = CARTESIAN_POINT ( 'NONE',  ( 0.000000000000000000, 0.000000000000000000, 0.000000000000000000 ) ) ;
#45805 = FACE_OUTER_BOUND ( 'NONE', #151199, .T. ) ;
#45806 = EDGE_CURVE ( 'NONE', #27688, #14341, #176191, .T. ) ;
#45807 = DIRECTION ( 'NONE',  ( 0.000000000000000000, 0.8660254037844420383, -0.4999999999999943379 ) ) ;
#45808 = DIRECTION ( 'NONE',  ( 4.336808689942128965E-15, -0.8660254037844367092, 0.5000000000000037748 ) ) ;
#45809 = ORIENTED_EDGE ( 'NONE', *, *, #200132, .T. ) ;
#45810 = DIRECTION ( 'NONE',  ( 2.952720810173289112E-16, -1.000000000000000000, 0.000000000000000000 ) ) ;
#45811 = CARTESIAN_POINT ( 'NONE',  ( 20.27550659511089037, 66.78395627750300889, -90.37310748452436826 ) ) ;
#45812 = EDGE_CURVE ( 'NONE', #225666, #107696, #57977, .T. ) ;
#45813 = CARTESIAN_POINT ( 'NONE',  ( -22.49072729836729678, 0.05648193274477466413, -122.3499917508450920 ) ) ;
#45814 = ORIENTED_EDGE ( 'NONE', *, *, #153372, .T. ) ;
#45815 = ORIENTED_EDGE ( 'NONE', *, *, #35205, .T. ) ;
#45816 = EDGE_CURVE ( 'NONE', #50778, #70322, #151242, .T. ) ;
#45817 = DIRECTION ( 'NONE',  ( 0.000000000000000000, 0.000000000000000000, 1.000000000000000000 ) ) ;
#45818 = AXIS2_PLACEMENT_3D ( 'NONE', #107190, #125483, #128054 ) ;
#45819 = LINE ( 'NONE', #4120, #102731 ) ;
#45820 = FACE_OUTER_BOUND ( 'NONE', #176904, .T. ) ;
#45821 = CARTESIAN_POINT ( 'NONE',  ( 21.05000000000000071, 10.72371681401022592, -141.5943992358848220 ) ) ;
#45822 = CARTESIAN_POINT ( 'NONE',  ( -21.05000000000000071, 1.115600667400684642E-11, -134.0000000000000284 ) ) ;
#45823 = AXIS2_PLACEMENT_3D ( 'NONE', #175892, #36384, #71651 ) ;
#45825 = CARTESIAN_POINT ( 'NONE',  ( -16.87331047859651179, 9.950000000011142376, -180.1499999999999773 ) ) ;
#45824 = DIRECTION ( 'NONE',  ( -1.000000000000000000, -0.000000000000000000, -0.000000000000000000 ) ) ;
#45826 = CARTESIAN_POINT ( 'NONE',  ( 5.899999999999996803, -11.65000000000000036, 13.90000000000000213 ) ) ;
#45827 = DIRECTION ( 'NONE',  ( 0.000000000000000000, 1.000000000000000000, 0.000000000000000000 ) ) ;
#45828 = LINE ( 'NONE', #27593, #255399 ) ;
#45829 = LINE ( 'NONE', #152342, #206479 ) ;
#45830 = AXIS2_PLACEMENT_3D ( 'NONE', #5327, #203562, #226977 ) ;
#45832 = VERTEX_POINT ( 'NONE', #218332 ) ;
#45831 = CARTESIAN_POINT ( 'NONE',  ( 18.52928932188133970, 10.27928932189250411, -125.1500000000000341 ) ) ;
#45833 = CARTESIAN_POINT ( 'NONE',  ( -21.14999999999999858, 64.25000000001209344, -129.7392418215462158 ) ) ;
#45834 = DIRECTION ( 'NONE',  ( 1.000000000000000000, -0.000000000000000000, -0.000000000000000000 ) ) ;
#45836 = LINE ( 'NONE', #125385, #32910 ) ;
#45835 = CARTESIAN_POINT ( 'NONE',  ( 21.07016717457010913, 76.00000000001200817, -109.3440483226251985 ) ) ;
#45837 = EDGE_CURVE ( 'NONE', #27007, #114076, #159976, .T. ) ;
#45838 = ORIENTED_EDGE ( 'NONE', *, *, #19256, .T. ) ;
#45839 = CARTESIAN_POINT ( 'NONE',  ( -23.15000000000000213, 28.58935552370083144, -258.2621935127861548 ) ) ;
#45841 = EDGE_CURVE ( 'NONE', #169290, #231688, #9747, .T. ) ;
#45840 = DIRECTION ( 'NONE',  ( 1.000000000000000000, 0.000000000000000000, -0.000000000000000000 ) ) ;
#45842 = DIRECTION ( 'NONE',  ( -1.000000000000000000, 2.952720810173289112E-16, 2.061873921506763405E-30 ) ) ;
#45843 = CARTESIAN_POINT ( 'NONE',  ( -21.05000000000000071, 8.366615838327078336, -209.3410474610450080 ) ) ;
#45844 = CARTESIAN_POINT ( 'NONE',  ( 23.24999999999999289, 42.98415524044398950, -233.9519173640447889 ) ) ;
#45845 = ORIENTED_EDGE ( 'NONE', *, *, #97186, .T. ) ;
#45847 = ORIENTED_EDGE ( 'NONE', *, *, #160066, .F. ) ;
#45846 = CIRCLE ( 'NONE', #224881, 2.099999999999995204 ) ;
#45848 = CIRCLE ( 'NONE', #33407, 0.1999999999999987899 ) ;
#45849 = EDGE_CURVE ( 'NONE', #187774, #164049, #251151, .T. ) ;
#45850 = DIRECTION ( 'NONE',  ( 0.000000000000000000, 0.000000000000000000, -1.000000000000000000 ) ) ;
#45851 = ORIENTED_EDGE ( 'NONE', *, *, #143489, .T. ) ;
#45852 = DIRECTION ( 'NONE',  ( -1.000000000000000000, 0.000000000000000000, 0.000000000000000000 ) ) ;
#45853 = CIRCLE ( 'NONE', #145792, 0.5000000000000004441 ) ;
#45854 = ORIENTED_EDGE ( 'NONE', *, *, #85600, .F. ) ;
#45855 = AXIS2_PLACEMENT_3D ( 'NONE', #240142, #234021, #55349 ) ;
#45856 = DIRECTION ( 'NONE',  ( 0.000000000000000000, 1.000000000000000000, 3.418575295766609984E-15 ) ) ;
#45857 = CARTESIAN_POINT ( 'NONE',  ( -18.59999999999999787, 9.350000000011156942, -155.2500000000000284 ) ) ;
#45858 = DIRECTION ( 'NONE',  ( 0.000000000000000000, 6.982962677686266711E-15, -1.000000000000000000 ) ) ;
#45859 = VERTEX_POINT ( 'NONE', #83929 ) ;
#45860 = DIRECTION ( 'NONE',  ( 0.000000000000000000, -1.000000000000000000, 0.000000000000000000 ) ) ;
#45861 = CARTESIAN_POINT ( 'NONE',  ( 21.53551880898957194, 69.21520223859582188, -136.6220772190960133 ) ) ;
#45862 = CARTESIAN_POINT ( 'NONE',  ( -21.05000000000000071, -1.835341550224411922, -11.55515129256297868 ) ) ;
#45863 = EDGE_CURVE ( 'NONE', #155258, #77947, #147475, .T. ) ;
#45864 = CARTESIAN_POINT ( 'NONE',  ( -16.78270389226385007, 30.19733697315739818, -234.8052090562477190 ) ) ;
#45865 = DIRECTION ( 'NONE',  ( 1.301042606982683734E-14, 0.8660254037844367092, -0.5000000000000037748 ) ) ;
#45867 = AXIS2_PLACEMENT_3D ( 'NONE', #41253, #19084, #3355 ) ;
#45866 = LINE ( 'NONE', #181550, #24777 ) ;
#45868 = CARTESIAN_POINT ( 'NONE',  ( 22.48660254037844197, 11.65000000001116298, -33.45000000000000995 ) ) ;
#45869 = ADVANCED_FACE ( 'NONE', ( #22753 ), #85231, .T. ) ;
#45870 = ORIENTED_EDGE ( 'NONE', *, *, #23916, .T. ) ;
#45872 = DIRECTION ( 'NONE',  ( -1.646408749285563007E-14, -0.9651348961777157509, 0.2617529984165031243 ) ) ;
#45871 = DIRECTION ( 'NONE',  ( 0.000000000000000000, 6.982962677686266711E-15, -1.000000000000000000 ) ) ;
#45873 = VERTEX_POINT ( 'NONE', #100924 ) ;
#45875 = ORIENTED_EDGE ( 'NONE', *, *, #147919, .T. ) ;
#45874 = DIRECTION ( 'NONE',  ( 0.000000000000000000, 1.000000000000000000, 6.982962677686266711E-15 ) ) ;
#45876 = ORIENTED_EDGE ( 'NONE', *, *, #79127, .T. ) ;
#45877 = DIRECTION ( 'NONE',  ( 0.000000000000000000, 0.000000000000000000, 1.000000000000000000 ) ) ;
#45878 = DIRECTION ( 'NONE',  ( 0.000000000000000000, 0.2617529984165026247, 0.9651348961777158619 ) ) ;
#45879 = CARTESIAN_POINT ( 'NONE',  ( 18.54999999999999716, 8.750000000000024869, -20.85000000000000142 ) ) ;
#45880 = PLANE ( 'NONE',  #141550 ) ;
#45881 = VERTEX_POINT ( 'NONE', #3139 ) ;
#45882 = EDGE_CURVE ( 'NONE', #127734, #234879, #76369, .T. ) ;
#45883 = CARTESIAN_POINT ( 'NONE',  ( 20.94999999999999929, 88.41227409416185878, -139.5231074845242745 ) ) ;
#45884 = CARTESIAN_POINT ( 'NONE',  ( -16.78493832629888516, 66.05416425680813575, -157.3591584654201938 ) ) ;
#45885 = EDGE_CURVE ( 'NONE', #122321, #105113, #143946, .T. ) ;
#45886 = ORIENTED_EDGE ( 'NONE', *, *, #129744, .F. ) ;
#45887 = CARTESIAN_POINT ( 'NONE',  ( 18.47073956224746993, -9.471729412460748065, -174.6086857528181326 ) ) ;
#45888 = AXIS2_PLACEMENT_3D ( 'NONE', #212967, #171329, #172608 ) ;
#45889 = AXIS2_PLACEMENT_3D ( 'NONE', #135853, #202274, #104423 ) ;
#45890 = EDGE_CURVE ( 'NONE', #143742, #206232, #72126, .T. ) ;
#45891 = CIRCLE ( 'NONE', #108258, 0.09999999999998898659 ) ;
#45893 = CIRCLE ( 'NONE', #216576, 0.09999999999999939493 ) ;
#45892 = FACE_OUTER_BOUND ( 'NONE', #223986, .T. ) ;
#45894 = ORIENTED_EDGE ( 'NONE', *, *, #251995, .F. ) ;
#45895 = CARTESIAN_POINT ( 'NONE',  ( -16.93710578446423654, 9.950000000011137047, -146.9188039837998758 ) ) ;
#45896 = ADVANCED_FACE ( 'NONE', ( #222180 ), #92947, .T. ) ;
#45897 = ORIENTED_EDGE ( 'NONE', *, *, #225357, .T. ) ;
#45898 = AXIS2_PLACEMENT_3D ( 'NONE', #192712, #36221, #115736 ) ;
#45899 = CARTESIAN_POINT ( 'NONE',  ( 21.14999999999999858, 59.16775194334852728, -221.0793150863668473 ) ) ;
#45902 = EDGE_CURVE ( 'NONE', #29706, #209835, #126275, .T. ) ;
#45901 = EDGE_CURVE ( 'NONE', #42426, #153822, #109701, .T. ) ;
#45900 = VERTEX_POINT ( 'NONE', #241765 ) ;
#45903 = DIRECTION ( 'NONE',  ( 0.000000000000000000, 0.9126074666063545004, 0.4088369013363783999 ) ) ;
#45904 = CARTESIAN_POINT ( 'NONE',  ( -16.94107738177415712, 44.01795756907898749, -235.2811900454759666 ) ) ;
#45905 =( REPRESENTATION_RELATIONSHIP ('NONE','NONE', #36900, #241717 ) REPRESENTATION_RELATIONSHIP_WITH_TRANSFORMATION ( #101584 )SHAPE_REPRESENTATION_RELATIONSHIP( ) );
#45906 = CARTESIAN_POINT ( 'NONE',  ( 21.05000000000000071, 85.50000000001197975, -112.9170766071766820 ) ) ;
#45907 = CIRCLE ( 'NONE', #249910, 11.80000000000000426 ) ;
#45908 = DIRECTION ( 'NONE',  ( 0.000000000000000000, 0.000000000000000000, -1.000000000000000000 ) ) ;
#45909 = CARTESIAN_POINT ( 'NONE',  ( -19.99016485861947601, 4.635725510443826636, 21.97684634237452528 ) ) ;
#45910 = ADVANCED_FACE ( 'NONE', ( #103525 ), #42294, .F. ) ;
#45912 = EDGE_CURVE ( 'NONE', #246412, #182351, #123120, .T. ) ;
#45911 = CARTESIAN_POINT ( 'NONE',  ( 23.14999999999999858, 76.00000000001213607, -136.5231074845243313 ) ) ;
#45913 = ORIENTED_EDGE ( 'NONE', *, *, #112848, .F. ) ;
#45915 = DIRECTION ( 'NONE',  ( -1.000000000000000000, 0.000000000000000000, 0.000000000000000000 ) ) ;
#45914 = CARTESIAN_POINT ( 'NONE',  ( -21.05000000000000071, 69.74218538953086011, -170.1208977758336118 ) ) ;
#45916 = CARTESIAN_POINT ( 'NONE',  ( -16.89797118371785700, 12.42123379871372890, -211.1519811452710940 ) ) ;
#45917 = EDGE_CURVE ( 'NONE', #192810, #122573, #255403, .T. ) ;
#45918 = CARTESIAN_POINT ( 'NONE',  ( 23.24999999999999645, 76.00000000001213607, -136.5231074845243313 ) ) ;
#45920 = ORIENTED_EDGE ( 'NONE', *, *, #177417, .T. ) ;
#45919 = CARTESIAN_POINT ( 'NONE',  ( -22.50000000000000000, 76.00000000001267608, -203.5231074845243597 ) ) ;
#45922 = ORIENTED_EDGE ( 'NONE', *, *, #187492, .F. ) ;
#45921 = DIRECTION ( 'NONE',  ( 0.000000000000000000, -1.000000000000000000, -6.982962677686265922E-15 ) ) ;
#45923 = CARTESIAN_POINT ( 'NONE',  ( -23.15000000000000213, 27.82649702422227733, -239.8850763025288870 ) ) ;
#45924 = CARTESIAN_POINT ( 'NONE',  ( 20.85000000000000142, 87.75000000001142553, -39.02310748452423894 ) ) ;
#45925 = CARTESIAN_POINT ( 'NONE',  ( 15.74999999999999645, 66.65000000001155911, -52.77310748452439526 ) ) ;
#45926 = CARTESIAN_POINT ( 'NONE',  ( 23.15000000000000213, 85.50000000001222134, -146.4170766071767389 ) ) ;
#45927 = ADVANCED_FACE ( 'NONE', ( #80087 ), #1852, .T. ) ;
#45929 = ORIENTED_EDGE ( 'NONE', *, *, #59149, .F. ) ;
#45928 = CARTESIAN_POINT ( 'NONE',  ( 21.06086055315980232, 67.22529248505607313, -157.8207853293704090 ) ) ;
#45930 = VECTOR ( 'NONE', #72226, 1000.000000000000000 ) ;
#45931 = DIRECTION ( 'NONE',  ( 0.000000000000000000, 0.9525900758537790836, -0.3042567129660269099 ) ) ;
#45932 = CARTESIAN_POINT ( 'NONE',  ( 22.59999999999999432, 75.90000000001202807, -114.6726782920691221 ) ) ;
#45933 = VERTEX_POINT ( 'NONE', #125675 ) ;
#45934 = CARTESIAN_POINT ( 'NONE',  ( 23.14999999999999858, 53.86595165227826243, -236.3638196928718855 ) ) ;
#45935 = EDGE_LOOP ( 'NONE', ( #55934, #131178, #219914, #231411, #184074 ) ) ;
#45936 = VECTOR ( 'NONE', #142600, 1000.000000000000000 ) ;
#45938 = EDGE_CURVE ( 'NONE', #185736, #242879, #30431, .T. ) ;
#45937 = DIRECTION ( 'NONE',  ( -1.000000000000000000, 4.625929269271478222E-14, 0.000000000000000000 ) ) ;
#45939 = CARTESIAN_POINT ( 'NONE',  ( 19.75857864376269291, 34.49410723828536618, -235.0619057650792740 ) ) ;
#45940 = VERTEX_POINT ( 'NONE', #239205 ) ;
#45941 = DIRECTION ( 'NONE',  ( 2.952720810173289112E-16, -1.000000000000000000, 0.000000000000000000 ) ) ;
#45942 = DIRECTION ( 'NONE',  ( 1.000000000000000000, 0.000000000000000000, 0.000000000000000000 ) ) ;
#45943 = EDGE_CURVE ( 'NONE', #160723, #32344, #130366, .T. ) ;
#45944 = ORIENTED_EDGE ( 'NONE', *, *, #82268, .F. ) ;
#45945 = AXIS2_PLACEMENT_3D ( 'NONE', #48094, #208483, #93647 ) ;
#45946 = CARTESIAN_POINT ( 'NONE',  ( 21.11101077988997332, 6.273301122770013727, -199.6180983270179468 ) ) ;
#45947 = AXIS2_PLACEMENT_3D ( 'NONE', #127353, #7392, #246021 ) ;
#45948 = VERTEX_POINT ( 'NONE', #206500 ) ;
#45949 = EDGE_LOOP ( 'NONE', ( #220138, #231610, #129435, #3235 ) ) ;
#45950 = CARTESIAN_POINT ( 'NONE',  ( 21.00000000000000000, 9.750000000011153745, -112.8500000000000369 ) ) ;
#45951 = CIRCLE ( 'NONE', #229319, 0.09999999999999976963 ) ;
#45952 = ORIENTED_EDGE ( 'NONE', *, *, #141192, .T. ) ;
#45954 = EDGE_CURVE ( 'NONE', #52860, #50099, #193117, .T. ) ;
#45953 = SPHERICAL_SURFACE ( 'NONE', #25585, 0.1000000000000000056 ) ;
#45955 = ORIENTED_EDGE ( 'NONE', *, *, #51871, .F. ) ;
#45957 = EDGE_LOOP ( 'NONE', ( #215532, #18714, #219963, #243119 ) ) ;
#45956 = DIRECTION ( 'NONE',  ( -1.000000000000000000, -0.000000000000000000, -0.000000000000000000 ) ) ;
#45958 = AXIS2_PLACEMENT_3D ( 'NONE', #34044, #14468, #122543 ) ;
#45959 = CARTESIAN_POINT ( 'NONE',  ( -21.03571358705762506, 11.75000000001115197, -73.82510682205845853 ) ) ;
#45960 = EDGE_LOOP ( 'NONE', ( #217867, #83058, #71350, #15126, #92098, #167251 ) ) ;
#45961 = LINE ( 'NONE', #198609, #197267 ) ;
#45962 = VERTEX_POINT ( 'NONE', #168714 ) ;
#45964 = ORIENTED_EDGE ( 'NONE', *, *, #232883, .F. ) ;
#45963 = ORIENTED_EDGE ( 'NONE', *, *, #150682, .F. ) ;
#45965 = DIRECTION ( 'NONE',  ( 1.000000000000000000, 0.000000000000000000, 0.000000000000000000 ) ) ;
#45966 = CARTESIAN_POINT ( 'NONE',  ( -20.94999999999999929, 56.27731819600170837, -227.9967441372480721 ) ) ;
#45967 = ORIENTED_EDGE ( 'NONE', *, *, #82177, .T. ) ;
#45968 = CIRCLE ( 'NONE', #237522, 0.2000000000000057288 ) ;
#45969 = AXIS2_PLACEMENT_3D ( 'NONE', #67901, #127886, #69214 ) ;
#45970 = AXIS2_PLACEMENT_3D ( 'NONE', #213138, #175331, #38364 ) ;
#45971 = AXIS2_PLACEMENT_3D ( 'NONE', #47028, #225655, #246526 ) ;
#45972 = ORIENTED_EDGE ( 'NONE', *, *, #253358, .T. ) ;
#45973 = CARTESIAN_POINT ( 'NONE',  ( 22.88900146558018989, 11.19647932930851120, -211.5080592518986862 ) ) ;
#45974 = CARTESIAN_POINT ( 'NONE',  ( -18.39999999999999858, -9.499999999988849808, -107.5320693966997112 ) ) ;
#45976 = ORIENTED_EDGE ( 'NONE', *, *, #32115, .T. ) ;
#45975 = DIRECTION ( 'NONE',  ( 0.000000000000000000, 0.000000000000000000, -1.000000000000000000 ) ) ;
#45977 = DIRECTION ( 'NONE',  ( 1.000000000000000000, -0.000000000000000000, -0.000000000000000000 ) ) ;
#45978 = ORIENTED_EDGE ( 'NONE', *, *, #101790, .F. ) ;
#45979 = DIRECTION ( 'NONE',  ( 1.000000000000000000, 0.000000000000000000, 0.000000000000000000 ) ) ;
#45980 = LINE ( 'NONE', #164659, #110423 ) ;
#45981 = ORIENTED_EDGE ( 'NONE', *, *, #125377, .F. ) ;
#45982 = DIRECTION ( 'NONE',  ( 0.000000000000000000, -1.000000000000000000, 0.000000000000000000 ) ) ;
#45983 = AXIS2_PLACEMENT_3D ( 'NONE', #126498, #127796, #120441 ) ;
#45984 = CARTESIAN_POINT ( 'NONE',  ( 18.59999999999998721, 70.37092869010230345, -198.1237041667535550 ) ) ;
#45985 = ORIENTED_EDGE ( 'NONE', *, *, #153999, .T. ) ;
#45986 = CARTESIAN_POINT ( 'NONE',  ( 18.39999999999997371, 11.47316190337362940, -124.7500000000000426 ) ) ;
#45987 = ORIENTED_EDGE ( 'NONE', *, *, #37411, .T. ) ;
#45989 = ORIENTED_EDGE ( 'NONE', *, *, #163051, .T. ) ;
#45988 = ORIENTED_EDGE ( 'NONE', *, *, #90139, .T. ) ;
#45990 = ORIENTED_EDGE ( 'NONE', *, *, #87384, .T. ) ;
#45991 = DIRECTION ( 'NONE',  ( 0.000000000000000000, 0.000000000000000000, -1.000000000000000000 ) ) ;
#45992 = EDGE_LOOP ( 'NONE', ( #17824, #195807, #138526, #51188 ) ) ;
#45993 = CARTESIAN_POINT ( 'NONE',  ( -17.01764560440427942, 66.05000000001153637, -48.77310748373898264 ) ) ;
#45994 = ORIENTED_EDGE ( 'NONE', *, *, #127616, .T. ) ;
#45995 = DIRECTION ( 'NONE',  ( 0.000000000000000000, 0.000000000000000000, -1.000000000000000000 ) ) ;
#45996 = AXIS2_PLACEMENT_3D ( 'NONE', #23554, #206000, #106885 ) ;
#45997 = VERTEX_POINT ( 'NONE', #30451 ) ;
#45998 = EDGE_CURVE ( 'NONE', #21929, #231005, #1543, .T. ) ;
#45999 = TOROIDAL_SURFACE ( 'NONE', #116738, 3.899999999999999467, 0.1000000000000000056 ) ;
#46000 = ORIENTED_EDGE ( 'NONE', *, *, #55409, .T. ) ;
#46001 = ORIENTED_EDGE ( 'NONE', *, *, #52662, .F. ) ;
#46002 = VECTOR ( 'NONE', #244942, 1000.000000000000000 ) ;
#46003 = CIRCLE ( 'NONE', #79310, 0.1000000000000021289 ) ;
#46004 = DIRECTION ( 'NONE',  ( 0.000000000000000000, -1.000000000000000000, -6.982962677686266711E-15 ) ) ;
#46005 = ORIENTED_EDGE ( 'NONE', *, *, #40306, .F. ) ;
#46006 = ADVANCED_FACE ( 'NONE', ( #8321 ), #45653, .F. ) ;
#46007 = DIRECTION ( 'NONE',  ( 1.000000000000000000, 0.000000000000000000, 0.000000000000000000 ) ) ;
#46009 = ORIENTED_EDGE ( 'NONE', *, *, #197227, .T. ) ;
#46008 = DIRECTION ( 'NONE',  ( -0.7071067811865456854, 0.3338907855510743206, 0.6233112732207635176 ) ) ;
#46010 = CARTESIAN_POINT ( 'NONE',  ( 19.97071067811865319, 64.27928932189384170, -178.8145288407617670 ) ) ;
#46011 = DIRECTION ( 'NONE',  ( 0.000000000000000000, 0.000000000000000000, -1.000000000000000000 ) ) ;
#46012 = CARTESIAN_POINT ( 'NONE',  ( -20.64999999999999858, 74.00000000001229239, -156.7984855617622770 ) ) ;
#46013 = SPHERICAL_SURFACE ( 'NONE', #210942, 0.1000000000000000056 ) ;
#46014 = EDGE_CURVE ( 'NONE', #952, #252597, #242973, .T. ) ;
#46015 = DIRECTION ( 'NONE',  ( 0.000000000000000000, -5.204170427930272346E-14, 1.000000000000000000 ) ) ;
#46016 = CIRCLE ( 'NONE', #121071, 0.09999999999999939493 ) ;
#46017 = CARTESIAN_POINT ( 'NONE',  ( 21.14250536705908345, 6.518172176891880554, -100.5000000000000284 ) ) ;
#46018 = CARTESIAN_POINT ( 'NONE',  ( 21.14999999999999858, 87.65000000001268177, -203.5231074845243029 ) ) ;
#46019 = CARTESIAN_POINT ( 'NONE',  ( 0.9000000000000547562, 67.72071067812984779, -10.02310748452479139 ) ) ;
#46020 = CARTESIAN_POINT ( 'NONE',  ( -20.54999999999999716, 87.75000000001183764, -86.27310748452423184 ) ) ;
#46021 = PLANE ( 'NONE',  #22046 ) ;
#46022 = TOROIDAL_SURFACE ( 'NONE', #183412, 11.90000000000000213, 0.1000000000000000056 ) ;
#46023 = EDGE_LOOP ( 'NONE', ( #22885, #75430, #227917, #145468 ) ) ;
#46024 = AXIS2_PLACEMENT_3D ( 'NONE', #66268, #67543, #85785 ) ;
#46025 = AXIS2_PLACEMENT_3D ( 'NONE', #143817, #25193, #145103 ) ;
#46026 = ADVANCED_FACE ( 'NONE', ( #248201 ), #64103, .F. ) ;
#46028 = ORIENTED_EDGE ( 'NONE', *, *, #156190, .F. ) ;
#46027 = CARTESIAN_POINT ( 'NONE',  ( 21.05000000000000426, 10.56275983746218472, -107.9568139579186692 ) ) ;
#46029 = ADVANCED_FACE ( 'NONE', ( #190828 ), #228656, .T. ) ;
#46030 = ORIENTED_EDGE ( 'NONE', *, *, #172178, .T. ) ;
#46031 = FACE_OUTER_BOUND ( 'NONE', #12801, .T. ) ;
#46032 = CARTESIAN_POINT ( 'NONE',  ( 20.75572585718235530, 8.882316728409755058, -142.4972583987020585 ) ) ;
#46033 = ADVANCED_FACE ( 'NONE', ( #151701 ), #227341, .F. ) ;
#46034 = CARTESIAN_POINT ( 'NONE',  ( 21.00000000000000000, 9.750000000011153745, -155.2500000000000284 ) ) ;
#46035 = ORIENTED_EDGE ( 'NONE', *, *, #28071, .T. ) ;
#46036 = SURFACE_STYLE_USAGE ( .BOTH. , #49893 ) ;
#46037 = DIRECTION ( 'NONE',  ( 0.000000000000000000, -7.124650136758292359E-15, 1.000000000000000000 ) ) ;
#46038 = EDGE_CURVE ( 'NONE', #13968, #51672, #255591, .T. ) ;
#46039 = AXIS2_PLACEMENT_3D ( 'NONE', #126433, #104285, #221665 ) ;
#46040 = CARTESIAN_POINT ( 'NONE',  ( 21.05000000000000071, 65.63240173135991995, -242.1325252935470189 ) ) ;
#46041 = VERTEX_POINT ( 'NONE', #160357 ) ;
#46042 = FACE_OUTER_BOUND ( 'NONE', #130943, .T. ) ;
#46043 = DIRECTION ( 'NONE',  ( 0.000000000000000000, 1.000000000000000000, 0.000000000000000000 ) ) ;
#46044 = EDGE_CURVE ( 'NONE', #190470, #70151, #113978, .T. ) ;
#46045 = CARTESIAN_POINT ( 'NONE',  ( 20.85000000000000142, 1.115600667400684642E-11, -100.5000000000000426 ) ) ;
#46046 = CARTESIAN_POINT ( 'NONE',  ( 18.52928932188134326, 15.30185809848915746, -222.9551995274939316 ) ) ;
#46048 = VERTEX_POINT ( 'NONE', #78210 ) ;
#46047 = CARTESIAN_POINT ( 'NONE',  ( -23.15000000000000213, 76.00000000001195133, -103.0231074845243171 ) ) ;
#46049 = CARTESIAN_POINT ( 'NONE',  ( -22.50000000000000000, 76.00000000001267608, -203.6231074845243540 ) ) ;
#46050 = CYLINDRICAL_SURFACE ( 'NONE', #231531, 0.09999999999999939493 ) ;
#46051 = DIRECTION ( 'NONE',  ( -1.000000000000000000, 0.000000000000000000, -0.000000000000000000 ) ) ;
#46052 = DIRECTION ( 'NONE',  ( 0.000000000000000000, 0.000000000000000000, -1.000000000000000000 ) ) ;
#46053 = EDGE_LOOP ( 'NONE', ( #132084, #214058, #179526, #196938, #192010 ) ) ;
#46054 = CARTESIAN_POINT ( 'NONE',  ( -16.94107738177415712, 65.98576071487568129, -157.4731074845244336 ) ) ;
#46056 = ADVANCED_FACE ( 'NONE', ( #2517 ), #116076, .F. ) ;
#46055 = FACE_OUTER_BOUND ( 'NONE', #149182, .T. ) ;
#46057 = VECTOR ( 'NONE', #126704, 1000.000000000000000 ) ;
#46060 = DIRECTION ( 'NONE',  ( 2.952720810173289112E-16, 0.4088369013363246096, -0.9126074666063785923 ) ) ;
#46059 = AXIS2_PLACEMENT_3D ( 'NONE', #7934, #87444, #112180 ) ;
#46058 = DIRECTION ( 'NONE',  ( 1.000000000000000000, 0.000000000000000000, 0.000000000000000000 ) ) ;
#46061 = DIRECTION ( 'NONE',  ( -1.000000000000000000, 0.000000000000000000, -0.000000000000000000 ) ) ;
#46062 = CARTESIAN_POINT ( 'NONE',  ( -16.97683809663752186, 9.950000000011137047, -53.59763598180368405 ) ) ;
#46063 = VECTOR ( 'NONE', #99624, 1000.000000000000000 ) ;
#46064 = DIRECTION ( 'NONE',  ( 1.000000000000000000, 0.000000000000000000, 0.000000000000000000 ) ) ;
#46065 = LINE ( 'NONE', #150328, #217281 ) ;
#46066 = CARTESIAN_POINT ( 'NONE',  ( -21.44999999999999929, 7.350000000011155166, -112.8500000000000369 ) ) ;
#46067 = ORIENTED_EDGE ( 'NONE', *, *, #189737, .T. ) ;
#46068 = CARTESIAN_POINT ( 'NONE',  ( -21.05000000000000071, 77.25000000001159606, -61.52310748452431710 ) ) ;
#46069 = CIRCLE ( 'NONE', #191862, 0.09999999999998916700 ) ;
#46070 = EDGE_LOOP ( 'NONE', ( #164667, #186472, #12732, #103200 ) ) ;
#46071 = VERTEX_POINT ( 'NONE', #179906 ) ;
#46072 = CARTESIAN_POINT ( 'NONE',  ( 18.59999999999999432, 1.162701749949165642, -41.50000000000000000 ) ) ;
#46073 = DIRECTION ( 'NONE',  ( 1.000000000000000000, 0.000000000000000000, 0.000000000000000000 ) ) ;
#46074 = VERTEX_POINT ( 'NONE', #18250 ) ;
#46075 = CONICAL_SURFACE ( 'NONE', #100225, 4.299999999999970512, 0.7853981633974466137 ) ;
#46076 = ORIENTED_EDGE ( 'NONE', *, *, #183453, .T. ) ;
#46077 = ORIENTED_EDGE ( 'NONE', *, *, #157505, .T. ) ;
#46078 = FACE_OUTER_BOUND ( 'NONE', #103282, .T. ) ;
#46079 = ORIENTED_EDGE ( 'NONE', *, *, #123838, .T. ) ;
#46080 = ADVANCED_FACE ( 'NONE', ( #59915 ), #19543, .T. ) ;
#46081 = CARTESIAN_POINT ( 'NONE',  ( 20.73486653747088582, 7.250000000011182166, -42.75000000000000000 ) ) ;
#46082 = DIRECTION ( 'NONE',  ( 0.000000000000000000, 0.9915357197604971473, -0.1298341882519111479 ) ) ;
#46083 = CARTESIAN_POINT ( 'NONE',  ( 21.14999999999999503, -1.330006220153263641, -194.8931527402181700 ) ) ;
#46084 = DIRECTION ( 'NONE',  ( 0.000000000000000000, -7.086529944415894657E-15, 1.000000000000000000 ) ) ;
#46085 = CARTESIAN_POINT ( 'NONE',  ( 23.14999999999999147, 67.23127455305841238, -235.8551265064783991 ) ) ;
#46086 = CARTESIAN_POINT ( 'NONE',  ( 21.05000000000000071, 76.00000000001260503, -190.6481074845243597 ) ) ;
#46087 = CYLINDRICAL_SURFACE ( 'NONE', #186824, 0.1000000000000050432 ) ;
#46089 = EDGE_LOOP ( 'NONE', ( #77570, #61552, #199715, #129280 ) ) ;
#46088 = DIRECTION ( 'NONE',  ( 0.000000000000000000, -7.056502275159894776E-15, 1.000000000000000000 ) ) ;
#46091 = CARTESIAN_POINT ( 'NONE',  ( 21.05000000000000071, 8.776282895303626930, -79.15000000000004832 ) ) ;
#46090 = CARTESIAN_POINT ( 'NONE',  ( 20.87155475150661132, 11.75000000000000355, -26.59558652915735522 ) ) ;
#46092 = EDGE_CURVE ( 'NONE', #152331, #135750, #136907, .T. ) ;
#46094 = CARTESIAN_POINT ( 'NONE',  ( -21.05000000000000071, 87.65000000001212754, -133.5231074845242176 ) ) ;
#46093 = VECTOR ( 'NONE', #140094, 1000.000000000000000 ) ;
#46095 = EDGE_CURVE ( 'NONE', #197589, #163018, #118081, .T. ) ;
#46096 = ORIENTED_EDGE ( 'NONE', *, *, #99391, .T. ) ;
#46097 = CARTESIAN_POINT ( 'NONE',  ( -20.85000000000000142, 87.75000000001246292, -170.0231074845242745 ) ) ;
#46098 = DIRECTION ( 'NONE',  ( -1.000000000000000000, 0.000000000000000000, 0.000000000000000000 ) ) ;
#46099 = ORIENTED_EDGE ( 'NONE', *, *, #154278, .T. ) ;
#46100 = CIRCLE ( 'NONE', #21203, 7.900000000000003908 ) ;
#46101 = EDGE_CURVE ( 'NONE', #223699, #227067, #184711, .T. ) ;
#46102 = CARTESIAN_POINT ( 'NONE',  ( 21.93340585898594597, 76.00000000001170974, -76.84725450665315805 ) ) ;
#46103 = EDGE_CURVE ( 'NONE', #12920, #194069, #181192, .T. ) ;
#46104 = AXIS2_PLACEMENT_3D ( 'NONE', #79254, #76700, #117131 ) ;
#46105 = EDGE_CURVE ( 'NONE', #70370, #92927, #176067, .T. ) ;
#46106 = CARTESIAN_POINT ( 'NONE',  ( -16.80621392010915471, 66.05779742250406628, -82.21269944994148204 ) ) ;
#46107 = EDGE_CURVE ( 'NONE', #216920, #150942, #199473, .T. ) ;
#46108 = ORIENTED_EDGE ( 'NONE', *, *, #166112, .F. ) ;
#46109 = CARTESIAN_POINT ( 'NONE',  ( -21.44999999999999929, 68.85000000001200249, -115.2731074845243455 ) ) ;
#46110 = ADVANCED_FACE ( 'NONE', ( #101592 ), #220311, .T. ) ;
#46112 = DIRECTION ( 'NONE',  ( 1.000000000000000000, 0.000000000000000000, -0.000000000000000000 ) ) ;
#46111 = AXIS2_PLACEMENT_3D ( 'NONE', #110897, #92600, #151330 ) ;
#46113 = CARTESIAN_POINT ( 'NONE',  ( -23.15000000000000213, 11.75000000001115552, -88.75000000000004263 ) ) ;
#46114 = ORIENTED_EDGE ( 'NONE', *, *, #214781, .T. ) ;
#46115 = ORIENTED_EDGE ( 'NONE', *, *, #219682, .F. ) ;
#46116 = B_SPLINE_CURVE_WITH_KNOTS ( 'NONE', 3,
 ( #148102, #249766, #172846, #227621, #112822, #211934, #90677, #33325, #69866, #149405, #13717, #188504, #111538, #29472, #71148, #110245, #88088, #248483, #129808 ),
 .UNSPECIFIED., .F., .F.,
 ( 4, 3, 3, 3, 3, 3, 4 ),
 ( 0.000000000000000000, 2.646747978908405501E-05, 5.271166642127181513E-05, 9.008788829882518278E-05, 0.0001426648776560658801, 0.0001897378458659452290, 0.0001917382627805908253 ),
 .UNSPECIFIED. ) ;
#46117 = CARTESIAN_POINT ( 'NONE',  ( -21.05000000000000071, 18.24178995542692050, -237.7003448530951459 ) ) ;
#46118 = FACE_OUTER_BOUND ( 'NONE', #115902, .T. ) ;
#46119 = FACE_OUTER_BOUND ( 'NONE', #162485, .T. ) ;
#46120 = AXIS2_PLACEMENT_3D ( 'NONE', #196585, #17946, #177059 ) ;
#46121 = CARTESIAN_POINT ( 'NONE',  ( 21.11927991906888025, 6.448493118502573118, -167.4909163205260541 ) ) ;
#46123 = LINE ( 'NONE', #147814, #159595 ) ;
#46122 = AXIS2_PLACEMENT_3D ( 'NONE', #124494, #204012, #11941 ) ;
#46124 = ORIENTED_EDGE ( 'NONE', *, *, #199590, .F. ) ;
#46125 = DIRECTION ( 'NONE',  ( 1.000000000000000000, 0.000000000000000000, 0.000000000000000000 ) ) ;
#46126 = EDGE_CURVE ( 'NONE', #159966, #196636, #196875, .T. ) ;
#46127 = AXIS2_PLACEMENT_3D ( 'NONE', #112607, #254645, #250818 ) ;
#46129 = ORIENTED_EDGE ( 'NONE', *, *, #154558, .T. ) ;
#46128 = FACE_OUTER_BOUND ( 'NONE', #180322, .T. ) ;
#46130 = DIRECTION ( 'NONE',  ( 0.000000000000000000, 0.000000000000000000, 1.000000000000000000 ) ) ;
#46131 = CARTESIAN_POINT ( 'NONE',  ( -16.77180007708460963, 66.05000000001187743, -90.38749336556955427 ) ) ;
#46132 = CARTESIAN_POINT ( 'NONE',  ( -21.09813707148783379, 75.96864850048226003, -75.90816959026101074 ) ) ;
#46133 = CIRCLE ( 'NONE', #108494, 0.1000000000000003525 ) ;
#46134 = DIRECTION ( 'NONE',  ( 0.000000000000000000, 1.000000000000000000, 0.000000000000000000 ) ) ;
#46135 = DIRECTION ( 'NONE',  ( 0.000000000000000000, 1.000000000000000000, 6.982962677686266711E-15 ) ) ;
#46136 = EDGE_CURVE ( 'NONE', #93310, #178218, #205548, .T. ) ;
#46138 = EDGE_LOOP ( 'NONE', ( #118964, #164037, #80537, #157527 ) ) ;
#46137 = CARTESIAN_POINT ( 'NONE',  ( 20.94999999999999929, 6.450000000011156587, -110.5170271704400591 ) ) ;
#46139 = DIRECTION ( 'NONE',  ( 1.734723475976817507E-14, 0.2128009952263604232, -0.9770955615653316162 ) ) ;
#46141 = ADVANCED_FACE ( 'NONE', ( #138170 ), #219004, .F. ) ;
#46140 = CARTESIAN_POINT ( 'NONE',  ( -18.50596464788227635, 65.69367753730709580, -164.5189238066348594 ) ) ;
#46142 = AXIS2_PLACEMENT_3D ( 'NONE', #123613, #225247, #181030 ) ;
#46143 = DIRECTION ( 'NONE',  ( 0.000000000000000000, -0.5774316882803290918, -0.8164390028469542537 ) ) ;
#46144 = LINE ( 'NONE', #166137, #211437 ) ;
#46145 = TOROIDAL_SURFACE ( 'NONE', #4442, 11.90000000000000213, 0.1000000000000000056 ) ;
#46146 = ORIENTED_EDGE ( 'NONE', *, *, #233872, .F. ) ;
#46147 = LINE ( 'NONE', #44872, #38949 ) ;
#46148 = DIRECTION ( 'NONE',  ( 0.000000000000000000, 0.8814952561688476074, -0.4721928772777262417 ) ) ;
#46149 = CARTESIAN_POINT ( 'NONE',  ( -21.05000000000000071, 1.750000000011155743, -78.66951155790169992 ) ) ;
#46150 = FACE_OUTER_BOUND ( 'NONE', #46340, .T. ) ;
#46151 = ORIENTED_EDGE ( 'NONE', *, *, #87384, .F. ) ;
#46153 = CARTESIAN_POINT ( 'NONE',  ( -16.85697194749126027, 9.908543714134777858, -87.56499573238625089 ) ) ;
#46152 = CIRCLE ( 'NONE', #245886, 0.09999999999999939493 ) ;
#46154 = TOROIDAL_SURFACE ( 'NONE', #183724, 0.4000000000000010214, 0.1000000000000000056 ) ;
#46155 = ORIENTED_EDGE ( 'NONE', *, *, #187128, .T. ) ;
#46156 = VECTOR ( 'NONE', #157421, 1000.000000000000000 ) ;
#46157 = CIRCLE ( 'NONE', #204364, 0.1000000000000028644 ) ;
#46158 = DIRECTION ( 'NONE',  ( -1.000000000000000000, 1.652117596168391700E-15, 0.000000000000000000 ) ) ;
#46159 = DIRECTION ( 'NONE',  ( 0.000000000000000000, 6.938893903907222067E-15, -1.000000000000000000 ) ) ;
#46160 = DIRECTION ( 'NONE',  ( 0.000000000000000000, -1.000000000000000000, 0.000000000000000000 ) ) ;
#46161 = DIRECTION ( 'NONE',  ( -0.000000000000000000, -1.265107689135680095E-16, 1.000000000000000000 ) ) ;
#46162 = ORIENTED_EDGE ( 'NONE', *, *, #60433, .F. ) ;
#46163 = DIRECTION ( 'NONE',  ( 0.000000000000000000, -7.116814260417668513E-15, 1.000000000000000000 ) ) ;
#46164 = CARTESIAN_POINT ( 'NONE',  ( -20.94999999999999929, -11.64999999998884483, -167.5000000000000000 ) ) ;
#46165 = CARTESIAN_POINT ( 'NONE',  ( 22.45305468355010348, -0.1008583690997046090, 11.74956712348972587 ) ) ;
#46166 = CARTESIAN_POINT ( 'NONE',  ( 21.05000000000000071, 11.60000000001116227, -160.5717967697245285 ) ) ;
#46167 = LINE ( 'NONE', #65738, #15801 ) ;
#46168 = ORIENTED_EDGE ( 'NONE', *, *, #92327, .T. ) ;
#46170 = EDGE_LOOP ( 'NONE', ( #102710, #197618, #223764, #158452 ) ) ;
#46169 = FACE_OUTER_BOUND ( 'NONE', #145158, .T. ) ;
#46171 = ORIENTED_EDGE ( 'NONE', *, *, #42607, .T. ) ;
#46172 = DIRECTION ( 'NONE',  ( -1.000000000000000000, -1.646408749285562691E-14, 0.000000000000000000 ) ) ;
#46173 = VERTEX_POINT ( 'NONE', #139461 ) ;
#46174 = CARTESIAN_POINT ( 'NONE',  ( 21.05000000000000071, 65.27628289530454708, -124.3731074845243825 ) ) ;
#46175 = DIRECTION ( 'NONE',  ( 0.000000000000000000, 6.982962677686267499E-15, -1.000000000000000000 ) ) ;
#46176 = CARTESIAN_POINT ( 'NONE',  ( 18.49999999999999289, 62.49201502323811752, -208.8221019049098857 ) ) ;
#46177 = EDGE_LOOP ( 'NONE', ( #247976, #159391, #101618, #71749 ) ) ;
#46178 = CARTESIAN_POINT ( 'NONE',  ( -20.94999999999999929, 74.63912941282058000, -195.4501095574334215 ) ) ;
#46179 = DIRECTION ( 'NONE',  ( 0.000000000000000000, -6.982962677686266711E-15, 1.000000000000000000 ) ) ;
#46180 = CARTESIAN_POINT ( 'NONE',  ( 21.05000000000000071, 0.3882413827466408840, -209.1776850584169551 ) ) ;
#46182 = ORIENTED_EDGE ( 'NONE', *, *, #141471, .T. ) ;
#46181 = AXIS2_PLACEMENT_3D ( 'NONE', #71638, #10381, #49494 ) ;
#46183 = CARTESIAN_POINT ( 'NONE',  ( 20.04999999999999716, 29.63969710739366548, -235.8648393122026334 ) ) ;
#46184 = ADVANCED_FACE ( 'NONE', ( #157805 ), #108856, .T. ) ;
#46186 = ORIENTED_EDGE ( 'NONE', *, *, #104008, .F. ) ;
#46185 = DIRECTION ( 'NONE',  ( 0.000000000000000000, 0.7035695228903320331, 0.7106264324241468033 ) ) ;
#46187 = DIRECTION ( 'NONE',  ( -1.000000000000000000, 0.000000000000000000, -0.000000000000000000 ) ) ;
#46188 = DIRECTION ( 'NONE',  ( 1.000000000000000000, 0.000000000000000000, 0.000000000000000000 ) ) ;
#46189 = EDGE_CURVE ( 'NONE', #104346, #23197, #83319, .T. ) ;
#46190 = AXIS2_PLACEMENT_3D ( 'NONE', #209207, #93112, #129676 ) ;
#46191 = ORIENTED_EDGE ( 'NONE', *, *, #35440, .T. ) ;
#46193 = EDGE_CURVE ( 'NONE', #76759, #38945, #134811, .T. ) ;
#46192 = CARTESIAN_POINT ( 'NONE',  ( -23.25000000000000355, 66.05000000001264482, -194.2731074845244166 ) ) ;
#46194 = AXIS2_PLACEMENT_3D ( 'NONE', #119538, #179515, #80359 ) ;
#46195 = CARTESIAN_POINT ( 'NONE',  ( -20.85000000000000142, 76.00000000001126921, -203.5231074845248997 ) ) ;
#46197 = EDGE_CURVE ( 'NONE', #220389, #11913, #105582, .T. ) ;
#46196 = EDGE_LOOP ( 'NONE', ( #214481, #80583, #36741, #223273 ) ) ;
#46198 = LINE ( 'NONE', #108748, #92484 ) ;
#46199 = CARTESIAN_POINT ( 'NONE',  ( -2.995603634470829482E-16, 6.650000000011155876, -88.25000000000005684 ) ) ;
#46200 = ORIENTED_EDGE ( 'NONE', *, *, #16982, .F. ) ;
#46201 = AXIS2_PLACEMENT_3D ( 'NONE', #149705, #87121, #148402 ) ;
#46202 = CIRCLE ( 'NONE', #33612, 0.1000000000000028644 ) ;
#46203 = EDGE_CURVE ( 'NONE', #123667, #133882, #104182, .T. ) ;
#46204 = ADVANCED_FACE ( 'NONE', ( #204575 ), #125061, .T. ) ;
#46206 = EDGE_LOOP ( 'NONE', ( #245760, #172074, #234604, #230713, #39431 ) ) ;
#46205 = CIRCLE ( 'NONE', #12938, 0.1000000000000032113 ) ;
#46207 = DIRECTION ( 'NONE',  ( -1.000000000000000000, -0.000000000000000000, -0.000000000000000000 ) ) ;
#46208 = ORIENTED_EDGE ( 'NONE', *, *, #69448, .F. ) ;
#46209 = DIRECTION ( 'NONE',  ( 0.000000000000000000, 0.9893560106964510714, -0.1455152366551481502 ) ) ;
#46210 = CARTESIAN_POINT ( 'NONE',  ( -16.84793658983456410, 66.05000000001253113, -182.7567541623338627 ) ) ;
#46212 = VERTEX_POINT ( 'NONE', #225410 ) ;
#46211 = CARTESIAN_POINT ( 'NONE',  ( -22.59999999999999787, 64.35042919246686210, -69.62310748452439668 ) ) ;
#46213 = FACE_OUTER_BOUND ( 'NONE', #130376, .T. ) ;
#46214 = LINE ( 'NONE', #127048, #49199 ) ;
#46215 = CARTESIAN_POINT ( 'NONE',  ( 19.97071067811864609, 64.27928932189314537, -81.67310748452439384 ) ) ;
#46216 = CYLINDRICAL_SURFACE ( 'NONE', #100462, 0.5000000000000004441 ) ;
#46217 = DIRECTION ( 'NONE',  ( 1.000000000000000000, 0.000000000000000000, 0.000000000000000000 ) ) ;
#46218 = LINE ( 'NONE', #31513, #208653 ) ;
#46219 = FACE_OUTER_BOUND ( 'NONE', #93541, .T. ) ;
#46221 = EDGE_CURVE ( 'NONE', #94746, #7823, #55689, .T. ) ;
#46220 = CARTESIAN_POINT ( 'NONE',  ( -18.60000000000000142, -9.321008403350123928, -107.7359382490779325 ) ) ;
#46223 = VERTEX_POINT ( 'NONE', #205862 ) ;
#46222 = DIRECTION ( 'NONE',  ( 0.000000000000000000, -0.3896596508880098009, -0.9209589331071360574 ) ) ;
#46224 = CARTESIAN_POINT ( 'NONE',  ( 20.84999999999998721, 72.03510814376021187, -246.5782642391033903 ) ) ;
#46225 = AXIS2_PLACEMENT_3D ( 'NONE', #108169, #53321, #187717 ) ;
#46226 = VERTEX_POINT ( 'NONE', #144591 ) ;
#46227 = EDGE_CURVE ( 'NONE', #17807, #76307, #48073, .T. ) ;
#46228 = CARTESIAN_POINT ( 'NONE',  ( -21.55000000000000071, 21.43869811404188752, -233.1734427395952025 ) ) ;
#46229 = CARTESIAN_POINT ( 'NONE',  ( 23.14999999999998792, 64.35000000001238618, -170.0231074845244166 ) ) ;
#46230 = CARTESIAN_POINT ( 'NONE',  ( -16.87683809663752399, 23.44353604138475689, -208.8407808817581781 ) ) ;
#46232 = EDGE_CURVE ( 'NONE', #7200, #179560, #26521, .T. ) ;
#46231 = DIRECTION ( 'NONE',  ( 0.000000000000000000, 0.000000000000000000, 1.000000000000000000 ) ) ;
#46233 = CARTESIAN_POINT ( 'NONE',  ( 20.94999999999999929, 1.115600667400684642E-11, -171.6000000000000227 ) ) ;
#46234 = EDGE_LOOP ( 'NONE', ( #96665, #179359, #112381, #17514 ) ) ;
#46235 = ADVANCED_FACE ( 'NONE', ( #46775 ), #14058, .T. ) ;
#46236 = DIRECTION ( 'NONE',  ( -3.265361837132813093E-16, -0.4088369013363281068, 0.9126074666063770380 ) ) ;
#46237 = VECTOR ( 'NONE', #11253, 1000.000000000000000 ) ;
#46238 = CIRCLE ( 'NONE', #54442, 0.1000000000000028644 ) ;
#46239 = CIRCLE ( 'NONE', #196106, 0.09999999999999939493 ) ;
#46240 = ADVANCED_FACE ( 'NONE', ( #222854 ), #163884, .T. ) ;
#46241 = ORIENTED_EDGE ( 'NONE', *, *, #255913, .F. ) ;
#46242 = FACE_OUTER_BOUND ( 'NONE', #66979, .T. ) ;
#46243 = CIRCLE ( 'NONE', #12968, 0.5000000000000004441 ) ;
#46244 = CARTESIAN_POINT ( 'NONE',  ( -18.49513951962168079, 86.88285858378623061, -199.4517059375024814 ) ) ;
#46245 = VERTEX_POINT ( 'NONE', #123772 ) ;
#46246 = CARTESIAN_POINT ( 'NONE',  ( -21.05000000000000071, 6.304961112695920633, -67.02138556593754970 ) ) ;
#46247 = ORIENTED_EDGE ( 'NONE', *, *, #180886, .F. ) ;
#46248 = ADVANCED_FACE ( 'NONE', ( #85887 ), #117249, .F. ) ;
#46249 = CARTESIAN_POINT ( 'NONE',  ( 20.84999999999998721, 46.46967969402478360, -243.0849751855955674 ) ) ;
#46250 = ORIENTED_EDGE ( 'NONE', *, *, #76402, .T. ) ;
#46251 = CIRCLE ( 'NONE', #137833, 11.75000000000000000 ) ;
#46252 = DIRECTION ( 'NONE',  ( 0.000000000000000000, -0.9126074666063770380, -0.4088369013363281068 ) ) ;
#46253 = EDGE_CURVE ( 'NONE', #77679, #2966, #234801, .T. ) ;
#46254 = CARTESIAN_POINT ( 'NONE',  ( 14.22821877134046886, 9.456028260519072859, -182.5111980350657177 ) ) ;
#46255 = ORIENTED_EDGE ( 'NONE', *, *, #124244, .T. ) ;
#46256 = DIRECTION ( 'NONE',  ( -1.000000000000000000, 0.000000000000000000, 0.000000000000000000 ) ) ;
#46258 = ORIENTED_EDGE ( 'NONE', *, *, #149898, .F. ) ;
#46257 = LINE ( 'NONE', #25437, #59887 ) ;
#46259 = CARTESIAN_POINT ( 'NONE',  ( -22.50000000000094147, 75.90000000001286651, -215.1726782920691790 ) ) ;
#46260 = EDGE_LOOP ( 'NONE', ( #177541, #106750, #251323, #184961 ) ) ;
#46261 =( BOUNDED_SURFACE ( )  B_SPLINE_SURFACE ( 3, 2, ( 
 ( #130827, #171296, #151714 ),
 ( #58962, #176400, #14767 ),
 ( #117684, #77263, #296 ),
 ( #98086, #235079, #55110 ) ),
 .UNSPECIFIED., .F., .F., .F. ) 
 B_SPLINE_SURFACE_WITH_KNOTS ( ( 4, 4 ),
 ( 3, 3 ),
 ( -1.044899843732904898E-17, 0.0003124336600439518762 ),
 ( 0.000000000000000000, 1.000000000000000000 ),
 .UNSPECIFIED. ) 
 GEOMETRIC_REPRESENTATION_ITEM ( )  RATIONAL_B_SPLINE_SURFACE ( (
 ( 1.000000000000000000, 0.7071067811864494290, 1.000000000000000000),
 ( 1.000000000000000000, 0.7089187706050879001, 1.000000000000000000),
 ( 1.000000000000000000, 0.7039288185050927016, 1.000000000000000000),
 ( 1.000000000000000000, 0.7040654476015839602, 1.000000000000000000) ) ) 
 REPRESENTATION_ITEM ( '' )  SURFACE ( )  );
#46262 = EDGE_LOOP ( 'NONE', ( #87935, #215426, #183338, #66768 ) ) ;
#46263 = DIRECTION ( 'NONE',  ( -0.000000000000000000, -0.000000000000000000, 1.000000000000000000 ) ) ;
#46265 = DIRECTION ( 'NONE',  ( 0.000000000000000000, -7.272083257015735086E-15, 1.000000000000000000 ) ) ;
#46264 = AXIS2_PLACEMENT_3D ( 'NONE', #3831, #46789, #222868 ) ;
#46266 = CARTESIAN_POINT ( 'NONE',  ( -16.80117486205003630, 9.949657268312314784, -20.84885487292548589 ) ) ;
#46267 = DIRECTION ( 'NONE',  ( 0.000000000000000000, 0.000000000000000000, -1.000000000000000000 ) ) ;
#46268 = SPHERICAL_SURFACE ( 'NONE', #25502, 0.1000000000000000056 ) ;
#46269 = VECTOR ( 'NONE', #82657, 1000.000000000000000 ) ;
#46270 = ORIENTED_EDGE ( 'NONE', *, *, #102453, .F. ) ;
#46271 = CARTESIAN_POINT ( 'NONE',  ( -23.15000000000000213, 64.25000000001199396, -115.1731074845243938 ) ) ;
#46272 = FACE_OUTER_BOUND ( 'NONE', #216034, .T. ) ;
#46273 = CARTESIAN_POINT ( 'NONE',  ( 20.95512820512820440, 67.12384868372396340, -127.9644784893834100 ) ) ;
#46274 = CARTESIAN_POINT ( 'NONE',  ( -20.64999999999999858, 85.00000000001222134, -146.4170766071767389 ) ) ;
#46275 = TOROIDAL_SURFACE ( 'NONE', #87956, 12.77500000000000036, 0.1000000000000000056 ) ;
#46276 = ORIENTED_EDGE ( 'NONE', *, *, #186307, .T. ) ;
#46277 = CARTESIAN_POINT ( 'NONE',  ( 20.92356734117541706, 68.07764576057049055, -224.1679995073710359 ) ) ;
#46278 = ORIENTED_EDGE ( 'NONE', *, *, #107512, .F. ) ;
#46279 = CARTESIAN_POINT ( 'NONE',  ( -18.50000000000000711, 12.97363049771892207, -205.3537238898406940 ) ) ;
#46280 = VERTEX_POINT ( 'NONE', #170649 ) ;
#46281 = CIRCLE ( 'NONE', #108830, 0.1000000000000033223 ) ;
#46282 = SPHERICAL_SURFACE ( 'NONE', #38832, 0.1000000000000000056 ) ;
#46283 = CYLINDRICAL_SURFACE ( 'NONE', #27223, 0.09999999999999939493 ) ;
#46284 = ORIENTED_EDGE ( 'NONE', *, *, #60034, .F. ) ;
#46285 = AXIS2_PLACEMENT_3D ( 'NONE', #151012, #208435, #67609 ) ;
#46286 = VERTEX_POINT ( 'NONE', #152346 ) ;
#46288 = ORIENTED_EDGE ( 'NONE', *, *, #202565, .T. ) ;
#46287 = CARTESIAN_POINT ( 'NONE',  ( -23.25000000000000000, 64.25000000001186606, -90.87310748452438247 ) ) ;
#46289 = DIRECTION ( 'NONE',  ( -0.000000000000000000, -0.000000000000000000, 1.000000000000000000 ) ) ;
#46290 = ORIENTED_EDGE ( 'NONE', *, *, #240199, .T. ) ;
#46291 = CARTESIAN_POINT ( 'NONE',  ( 23.14999999999999858, 78.00000000001142553, -36.02310748452431000 ) ) ;
#46292 = AXIS2_PLACEMENT_3D ( 'NONE', #26823, #5920, #183302 ) ;
#46293 = DIRECTION ( 'NONE',  ( 0.000000000000000000, -7.429790795770644761E-15, 1.000000000000000000 ) ) ;
#46294 = VERTEX_POINT ( 'NONE', #247562 ) ;
#46295 = CARTESIAN_POINT ( 'NONE',  ( -21.55000000000000071, 68.65000000001261071, -191.1731074845243938 ) ) ;
#46296 = ADVANCED_FACE ( 'NONE', ( #10249 ), #250136, .T. ) ;
#46297 = DIRECTION ( 'NONE',  ( 0.7071067811865476838, -0.3338907855510733769, -0.6233112732207617412 ) ) ;
#46298 = CIRCLE ( 'NONE', #250325, 0.09999999999998898659 ) ;
#46299 = AXIS2_PLACEMENT_3D ( 'NONE', #254058, #75466, #154999 ) ;
#46300 = EDGE_LOOP ( 'NONE', ( #173428, #33382, #153297 ) ) ;
#46301 = CARTESIAN_POINT ( 'NONE',  ( -21.05000000000000071, 87.65000000001172964, -72.52310748452423184 ) ) ;
#46302 = AXIS2_PLACEMENT_3D ( 'NONE', #159055, #40403, #80750 ) ;
#46303 = EDGE_CURVE ( 'NONE', #146129, #83517, #9933, .T. ) ;
#46304 = CIRCLE ( 'NONE', #217001, 0.4000000000000114575 ) ;
#46305 = CARTESIAN_POINT ( 'NONE',  ( -18.40000000000000213, 11.41458325961095177, -54.34999999999999432 ) ) ;
#46307 = ORIENTED_EDGE ( 'NONE', *, *, #190794, .T. ) ;
#46306 = CARTESIAN_POINT ( 'NONE',  ( 18.42555734704284731, 85.49715836194860685, -95.98327698678932052 ) ) ;
#46308 = EDGE_CURVE ( 'NONE', #212831, #35577, #233162, .T. ) ;
#46309 = DIRECTION ( 'NONE',  ( -0.000000000000000000, 0.000000000000000000, 1.000000000000000000 ) ) ;
#46310 = EDGE_CURVE ( 'NONE', #194502, #91478, #109878, .T. ) ;
#46311 = CARTESIAN_POINT ( 'NONE',  ( 18.39999999999997371, 40.29670989715187090, -235.0462836312595130 ) ) ;
#46312 = DIRECTION ( 'NONE',  ( -0.7070776581709311559, 4.937903618720164857E-15, -0.7071359030027479786 ) ) ;
#46314 = DIRECTION ( 'NONE',  ( 6.938893903907220489E-15, -0.4721928772777346239, -0.8814952561688430555 ) ) ;
#46313 = CARTESIAN_POINT ( 'NONE',  ( -23.25000000000000000, 7.575715430069919876, -235.7846019917273281 ) ) ;
#46315 = CARTESIAN_POINT ( 'NONE',  ( -20.94999999999999929, 65.70711192142420032, -164.5651054685122574 ) ) ;
#46316 = CARTESIAN_POINT ( 'NONE',  ( -23.15000000000000213, 76.00000000001139711, -32.02310748452432421 ) ) ;
#46317 = DIRECTION ( 'NONE',  ( 0.000000000000000000, -0.4088369013362748716, 0.9126074666064009078 ) ) ;
#46318 = AXIS2_PLACEMENT_3D ( 'NONE', #194966, #16330, #95819 ) ;
#46319 = LINE ( 'NONE', #127156, #242583 ) ;
#46320 = AXIS2_PLACEMENT_3D ( 'NONE', #233263, #255305, #134113 ) ;
#46322 = VERTEX_POINT ( 'NONE', #190170 ) ;
#46321 = CIRCLE ( 'NONE', #112985, 11.79999999999999716 ) ;
#46323 = ORIENTED_EDGE ( 'NONE', *, *, #128385, .F. ) ;
#46324 = EDGE_CURVE ( 'NONE', #83264, #209017, #200595, .T. ) ;
#46325 = DIRECTION ( 'NONE',  ( 0.000000000000000000, 0.2617529984165045120, 0.9651348961777153068 ) ) ;
#46326 = VERTEX_POINT ( 'NONE', #50624 ) ;
#46327 =( BOUNDED_SURFACE ( )  B_SPLINE_SURFACE ( 3, 2, ( 
 ( #129410, #249374, #107272 ),
 ( #130688, #227221, #85107 ),
 ( #86396, #66871, #126843 ),
 ( #166002, #69459, #47279 ) ),
 .UNSPECIFIED., .F., .F., .F. ) 
 B_SPLINE_SURFACE_WITH_KNOTS ( ( 4, 4 ),
 ( 3, 3 ),
 ( 4.712388980384689674, 5.765869716888459173 ),
 ( 0.000000000000000000, 1.000000000000000000 ),
 .UNSPECIFIED. ) 
 GEOMETRIC_REPRESENTATION_ITEM ( )  RATIONAL_B_SPLINE_SURFACE ( (
 ( 1.000000000000000000, 0.7071067811865795472, 1.000000000000000000),
 ( 1.000000000000000000, 0.7953136715913069477, 1.000000000000000000),
 ( 1.000000000000000000, 0.8646876308616193718, 1.000000000000000000),
 ( 1.000000000000000000, 0.8984936768950744224, 1.000000000000000000) ) ) 
 REPRESENTATION_ITEM ( '' )  SURFACE ( )  );
#46328 = CARTESIAN_POINT ( 'NONE',  ( -21.04386569057572132, 64.25000000001220712, -143.3802701327438740 ) ) ;
#46329 = ORIENTED_EDGE ( 'NONE', *, *, #6699, .F. ) ;
#46330 = CARTESIAN_POINT ( 'NONE',  ( 17.23472005113827166, 31.43009469574038661, -235.0565888300789936 ) ) ;
#46331 = DIRECTION ( 'NONE',  ( 0.000000000000000000, 1.000000000000000000, 6.982962677686266711E-15 ) ) ;
#46332 = ORIENTED_EDGE ( 'NONE', *, *, #220594, .T. ) ;
#46333 = DIRECTION ( 'NONE',  ( -3.265361837132813093E-16, 1.000000000000000000, 0.000000000000000000 ) ) ;
#46334 = ORIENTED_EDGE ( 'NONE', *, *, #173248, .F. ) ;
#46335 = ORIENTED_EDGE ( 'NONE', *, *, #220862, .F. ) ;
#46336 = B_SPLINE_CURVE_WITH_KNOTS ( 'NONE', 3,
 ( #13689, #194922, #252287, #254816, #54097, #236577, #134894, #74982, #215728, #76219, #232760, #116645, #253575, #196184, #133640, #154529, #17529, #97034, #57936, #234018, #137473, #217014, #34561, #38396, #197458, #18823 ),
 .UNSPECIFIED., .F., .F.,
 ( 4, 2, 2, 2, 2, 2, 2, 2, 2, 2, 2, 2, 4 ),
 ( 0.005476422646581347378, 0.006160811967703559190, 0.006845201288825771002, 0.007187395949386877342, 0.007529590609947982814, 0.007871785270509088286, 0.008213979931070194626, 0.008556174591631300966, 0.008898369252192407305, 0.009240563912753511910, 0.009582758573314618250, 0.01026714789443682746, 0.01095153721555903494 ),
 .UNSPECIFIED. ) ;
#46337 = CARTESIAN_POINT ( 'NONE',  ( 23.25000000000000000, -9.599999999988849453, -122.2500000000000284 ) ) ;
#46338 = FACE_OUTER_BOUND ( 'NONE', #27093, .T. ) ;
#46340 = EDGE_LOOP ( 'NONE', ( #22913, #200283, #237475, #8012, #133537 ) ) ;
#46339 = DIRECTION ( 'NONE',  ( 0.000000000000000000, 0.9126074666063844765, 0.4088369013363114535 ) ) ;
#46341 = ADVANCED_FACE ( 'NONE', ( #248852 ), #113187, .F. ) ;
#46342 = B_SPLINE_CURVE_WITH_KNOTS ( 'NONE', 3,
 ( #229632, #206216, #130516, #91408, #168426, #210078 ),
 .UNSPECIFIED., .F., .F.,
 ( 4, 2, 4 ),
 ( 0.000000000000000000, 0.0002113392456165905737, 0.0004226784912331811475 ),
 .UNSPECIFIED. ) ;
#46343 = CARTESIAN_POINT ( 'NONE',  ( 20.94999027547553894, 65.70673848566976005, -97.56382523348287350 ) ) ;
#46345 = ORIENTED_EDGE ( 'NONE', *, *, #123563, .T. ) ;
#46344 = CARTESIAN_POINT ( 'NONE',  ( -23.25000000000000000, 76.00000000001213607, -136.5231074845243313 ) ) ;
#46346 = CARTESIAN_POINT ( 'NONE',  ( 20.94999999999999929, 1.115625160336667635E-11, -132.0000000000000284 ) ) ;
#46347 = CARTESIAN_POINT ( 'NONE',  ( -21.14999999999994174, 74.26359666348515987, -47.54092689884382850 ) ) ;
#46348 = CIRCLE ( 'NONE', #196382, 0.09999999999999907574 ) ;
#46350 = ORIENTED_EDGE ( 'NONE', *, *, #218127, .T. ) ;
#46349 = CARTESIAN_POINT ( 'NONE',  ( -17.78043020864321022, 65.14640788800639370, -126.1861566502445697 ) ) ;
#46351 = CARTESIAN_POINT ( 'NONE',  ( -23.15000000000000213, -7.176961358819842651, -212.6889627706600834 ) ) ;
#46353 = ADVANCED_FACE ( 'NONE', ( #149773 ), #122373, .F. ) ;
#46352 = CARTESIAN_POINT ( 'NONE',  ( -23.25000000000000000, -0.8618440306552699326, -197.0427629756619297 ) ) ;
#46355 = CARTESIAN_POINT ( 'NONE',  ( -23.15000000000000213, 87.75000000001193712, -103.0231074845242318 ) ) ;
#46354 = DIRECTION ( 'NONE',  ( 0.000000000000000000, 0.000000000000000000, -1.000000000000000000 ) ) ;
#46356 = CARTESIAN_POINT ( 'NONE',  ( 20.94999999999999574, 79.07891399537199106, -236.0635483022085452 ) ) ;
#46357 = DIRECTION ( 'NONE',  ( -0.7071067811865475727, -0.7071067811865475727, -0.000000000000000000 ) ) ;
#46358 = CARTESIAN_POINT ( 'NONE',  ( 20.99999999999999645, 19.88654501311280498, -229.5059066796121101 ) ) ;
#46359 = ORIENTED_EDGE ( 'NONE', *, *, #178390, .T. ) ;
#46360 = ORIENTED_EDGE ( 'NONE', *, *, #89406, .F. ) ;
#46361 =( BOUNDED_SURFACE ( )  B_SPLINE_SURFACE ( 3, 2, ( 
 ( #162385, #247026, #222307 ),
 ( #164934, #24161, #43707 ),
 ( #22883, #103651, #5839 ),
 ( #46259, #184485, #144066 ) ),
 .UNSPECIFIED., .F., .F., .F. ) 
 B_SPLINE_SURFACE_WITH_KNOTS ( ( 4, 4 ),
 ( 3, 3 ),
 ( -5.692061405548898279E-19, 0.0003124336117481333599 ),
 ( 0.000000000000000000, 1.000000000000000000 ),
 .UNSPECIFIED. ) 
 GEOMETRIC_REPRESENTATION_ITEM ( )  RATIONAL_B_SPLINE_SURFACE ( (
 ( 1.000000000000000000, 0.7040654476014845953, 1.000000000000000000),
 ( 1.000000000000000000, 0.7039193538783811155, 1.000000000000000000),
 ( 1.000000000000000000, 0.7089171279145194404, 1.000000000000000000),
 ( 1.000000000000000000, 0.7071067811865509034, 1.000000000000000000) ) ) 
 REPRESENTATION_ITEM ( '' )  SURFACE ( )  );
#46362 = ORIENTED_EDGE ( 'NONE', *, *, #97929, .T. ) ;
#46364 = AXIS2_PLACEMENT_3D ( 'NONE', #54093, #93218, #232755 ) ;
#46363 = CARTESIAN_POINT ( 'NONE',  ( -20.54999999999999716, 1.115600667400684642E-11, -65.00000000000000000 ) ) ;
#46365 = VERTEX_POINT ( 'NONE', #194031 ) ;
#46366 = LINE ( 'NONE', #125908, #47536 ) ;
#46367 = ORIENTED_EDGE ( 'NONE', *, *, #205823, .F. ) ;
#46368 = CARTESIAN_POINT ( 'NONE',  ( -21.07016717456945898, 6.320940838111400950, -100.5000000000000426 ) ) ;
#46369 = DIRECTION ( 'NONE',  ( 0.000000000000000000, 0.9126074666063771490, 0.4088369013363281623 ) ) ;
#46370 = EDGE_CURVE ( 'NONE', #62193, #125, #97183, .T. ) ;
#46371 = ORIENTED_EDGE ( 'NONE', *, *, #105381, .T. ) ;
#46372 = SPHERICAL_SURFACE ( 'NONE', #256939, 0.1000000000000000056 ) ;
#46373 = AXIS2_PLACEMENT_3D ( 'NONE', #41313, #157419, #239492 ) ;
#46375 = ORIENTED_EDGE ( 'NONE', *, *, #22510, .T. ) ;
#46374 = VECTOR ( 'NONE', #4637, 1000.000000000000000 ) ;
#46376 = ORIENTED_EDGE ( 'NONE', *, *, #120018, .F. ) ;
#46377 = VERTEX_POINT ( 'NONE', #191475 ) ;
#46378 = CIRCLE ( 'NONE', #192169, 0.2000000000000057288 ) ;
#46379 = EDGE_CURVE ( 'NONE', #148174, #180506, #239081, .T. ) ;
#46380 = PLANE ( 'NONE',  #112834 ) ;
#46381 = DIRECTION ( 'NONE',  ( 1.000000000000000000, 0.000000000000000000, 0.000000000000000000 ) ) ;
#46382 = DIRECTION ( 'NONE',  ( -1.000000000000000000, 9.012599976028471648E-15, 6.882867235861662930E-14 ) ) ;
#46383 = ADVANCED_FACE ( 'NONE', ( #68949 ), #93317, .T. ) ;
#46384 = PLANE ( 'NONE',  #248764 ) ;
#46385 = FACE_OUTER_BOUND ( 'NONE', #27964, .T. ) ;
#46386 = LINE ( 'NONE', #41303, #146879 ) ;
#46388 = DIRECTION ( 'NONE',  ( 1.000000000000000000, 7.304098846218135653E-16, 0.000000000000000000 ) ) ;
#46387 = CARTESIAN_POINT ( 'NONE',  ( 20.94999999999999929, 6.650000000011155876, -43.51702717044002355 ) ) ;
#46389 = DIRECTION ( 'NONE',  ( 1.000000000000000000, -0.000000000000000000, 0.000000000000000000 ) ) ;
#46391 = EDGE_LOOP ( 'NONE', ( #231378, #116224, #150652, #257615 ) ) ;
#46390 = CARTESIAN_POINT ( 'NONE',  ( 20.95512820512820440, 10.62384868372303615, -112.6500000000000341 ) ) ;
#46393 = DIRECTION ( 'NONE',  ( -1.040834085586090694E-13, 0.1568667991644355497, 0.9876197685951332295 ) ) ;
#46392 = CARTESIAN_POINT ( 'NONE',  ( 20.87631937322879594, 10.47149503677605509, -74.57974587458122073 ) ) ;
#46394 = EDGE_CURVE ( 'NONE', #65298, #241398, #5816, .T. ) ;
#46395 = DIRECTION ( 'NONE',  ( 0.000000000000000000, -0.4999999999999689138, 0.8660254037844565822 ) ) ;
#46396 = ADVANCED_FACE ( 'NONE', ( #49367 ), #251412, .F. ) ;
#46397 = ORIENTED_EDGE ( 'NONE', *, *, #168069, .F. ) ;
#46398 = CARTESIAN_POINT ( 'NONE',  ( -20.65000000000000568, 62.65526179112262639, -225.0299194783148948 ) ) ;
#46399 = CARTESIAN_POINT ( 'NONE',  ( 22.59066674512252249, 64.25000000001193712, -103.0536116081550375 ) ) ;
#46400 = ORIENTED_EDGE ( 'NONE', *, *, #139284, .F. ) ;
#46401 = VECTOR ( 'NONE', #210183, 1000.000000000000000 ) ;
#46402 = EDGE_CURVE ( 'NONE', #197574, #18900, #188875, .T. ) ;
#46403 = DIRECTION ( 'NONE',  ( 0.000000000000000000, 0.3280696808754309246, 0.9446535261619960488 ) ) ;
#46404 = EDGE_CURVE ( 'NONE', #89936, #9735, #72494, .T. ) ;
#46405 = FACE_OUTER_BOUND ( 'NONE', #110173, .T. ) ;
#46406 = B_SPLINE_CURVE_WITH_KNOTS ( 'NONE', 3,
 ( #191523, #115807, #96228, #175798, #211059, #255257, #156246, #32454, #136633, #37567 ),
 .UNSPECIFIED., .F., .F.,
 ( 4, 2, 2, 2, 4 ),
 ( 0.000000000000000000, 3.990160268012908580E-05, 7.980320536025817160E-05, 0.0001596064107205132261, 0.0003192128214410382158 ),
 .UNSPECIFIED. ) ;
#46407 = DIRECTION ( 'NONE',  ( 1.020425574104004196E-15, 6.982962677686266711E-15, -1.000000000000000000 ) ) ;
#46409 = ADVANCED_FACE ( 'NONE', ( #137863 ), #75373, .F. ) ;
#46408 = EDGE_CURVE ( 'NONE', #120086, #47209, #122570, .T. ) ;
#46410 = ORIENTED_EDGE ( 'NONE', *, *, #157521, .F. ) ;
#46411 = ORIENTED_EDGE ( 'NONE', *, *, #228139, .T. ) ;
#46412 = CARTESIAN_POINT ( 'NONE',  ( -21.05000000000000071, 1.162701749949165642, -175.4999999999999716 ) ) ;
#46413 = EDGE_LOOP ( 'NONE', ( #162419, #123834, #21866 ) ) ;
#46414 = DIRECTION ( 'NONE',  ( 0.000000000000000000, 0.000000000000000000, -1.000000000000000000 ) ) ;
#46415 = CARTESIAN_POINT ( 'NONE',  ( -18.41809261886923466, -9.682403314745256395, -174.1568435500915086 ) ) ;
#46416 = DIRECTION ( 'NONE',  ( -1.000000000000000000, -1.836970198721029934E-16, 0.000000000000000000 ) ) ;
#46417 = CARTESIAN_POINT ( 'NONE',  ( 18.57071067811864040, 62.99531372641386895, -212.5850369713326131 ) ) ;
#46418 = ORIENTED_EDGE ( 'NONE', *, *, #50010, .F. ) ;
#46419 = CARTESIAN_POINT ( 'NONE',  ( -15.31895204843005232, 9.396533993965077158, -118.4059397791733375 ) ) ;
#46420 = EDGE_CURVE ( 'NONE', #227800, #127123, #58317, .T. ) ;
#46421 = AXIS2_PLACEMENT_3D ( 'NONE', #188815, #145826, #5017 ) ;
#46423 = DIRECTION ( 'NONE',  ( 0.000000000000000000, 6.938893903907270030E-14, -1.000000000000000000 ) ) ;
#46422 = CIRCLE ( 'NONE', #50504, 0.1000000000000028644 ) ;
#46424 = VECTOR ( 'NONE', #34936, 999.9999999999998863 ) ;
#46425 = CARTESIAN_POINT ( 'NONE',  ( 18.60000000000000142, -9.321008403350125704, -74.23593824907794669 ) ) ;
#46426 = CARTESIAN_POINT ( 'NONE',  ( 18.59999999999998366, 1.115600667400684642E-11, -134.0000000000000284 ) ) ;
#46427 = ADVANCED_FACE ( 'NONE', ( #253963 ), #76749, .F. ) ;
#46428 = ADVANCED_FACE ( 'NONE', ( #218683 ), #26713, .T. ) ;
#46429 = ORIENTED_EDGE ( 'NONE', *, *, #136672, .T. ) ;
#46430 = DIRECTION ( 'NONE',  ( 0.000000000000000000, 1.000000000000000000, 0.000000000000000000 ) ) ;
#46431 = EDGE_CURVE ( 'NONE', #121283, #191888, #118280, .T. ) ;
#46433 = EDGE_LOOP ( 'NONE', ( #234346, #164650, #109868, #63906 ) ) ;
#46432 = DIRECTION ( 'NONE',  ( 0.000000000000000000, 6.982962677686266711E-15, -1.000000000000000000 ) ) ;
#46434 = CARTESIAN_POINT ( 'NONE',  ( 23.24999999999999289, 64.35000000001156195, -57.37310748452439668 ) ) ;
#46435 = CARTESIAN_POINT ( 'NONE',  ( 18.40000000000000568, 78.23216008268646249, -231.5864513804630178 ) ) ;
#46436 = CARTESIAN_POINT ( 'NONE',  ( -16.90202395485779974, 9.965944544561983420, -87.90301372126040746 ) ) ;
#46437 = LINE ( 'NONE', #201667, #146371 ) ;
#46438 = ADVANCED_FACE ( 'NONE', ( #179598 ), #243160, .F. ) ;
#46439 = DIRECTION ( 'NONE',  ( 0.000000000000000000, -0.9976611540403004241, -0.06835365183350541884 ) ) ;
#46440 = DIRECTION ( 'NONE',  ( 0.000000000000000000, -1.000000000000000000, -6.982962677686266711E-15 ) ) ;
#46441 = CIRCLE ( 'NONE', #79746, 0.09999999999999939493 ) ;
#46442 = ORIENTED_EDGE ( 'NONE', *, *, #183670, .T. ) ;
#46443 = DIRECTION ( 'NONE',  ( 1.186688945009009831E-16, -1.000000000000000000, 0.000000000000000000 ) ) ;
#46444 = DIRECTION ( 'NONE',  ( 0.000000000000000000, -0.2617529984165031243, -0.9651348961777157509 ) ) ;
#46445 = CARTESIAN_POINT ( 'NONE',  ( -21.05000000000000071, -0.09999999999999939493, 11.64957080754479968 ) ) ;
#46446 = CARTESIAN_POINT ( 'NONE',  ( -23.15000000000000213, 70.60134440767090780, -223.4290147181903023 ) ) ;
#46447 = DIRECTION ( 'NONE',  ( 0.000000000000000000, 0.000000000000000000, 1.000000000000000000 ) ) ;
#46448 = ORIENTED_EDGE ( 'NONE', *, *, #232618, .F. ) ;
#46449 = ORIENTED_EDGE ( 'NONE', *, *, #50583, .T. ) ;
#46450 = DIRECTION ( 'NONE',  ( 0.000000000000000000, -0.8814952561688476074, 0.4721928772777262417 ) ) ;
#46451 = CARTESIAN_POINT ( 'NONE',  ( 22.47007471830798764, 1.115784145324971765E-11, -126.2792893480735330 ) ) ;
#46452 = CARTESIAN_POINT ( 'NONE',  ( -18.59999999999999787, 7.128833340093095217, -233.7327013124392749 ) ) ;
#46453 = AXIS2_PLACEMENT_3D ( 'NONE', #120116, #101759, #157968 ) ;
#46454 = DIRECTION ( 'NONE',  ( 1.000000000000000000, 0.000000000000000000, 0.000000000000000000 ) ) ;
#46455 = CARTESIAN_POINT ( 'NONE',  ( 21.00000000000000000, 63.35728523183471594, -212.8904317177587870 ) ) ;
#46456 = AXIS2_PLACEMENT_3D ( 'NONE', #170906, #15660, #73076 ) ;
#46457 = FACE_OUTER_BOUND ( 'NONE', #25357, .T. ) ;
#46458 = CARTESIAN_POINT ( 'NONE',  ( -20.87155475150660777, 17.14044013043752557, -224.4860178609578156 ) ) ;
#46459 = VECTOR ( 'NONE', #32721, 1000.000000000000000 ) ;
#46460 = AXIS2_PLACEMENT_3D ( 'NONE', #70533, #109615, #228300 ) ;
#46461 = EDGE_LOOP ( 'NONE', ( #4906, #7414, #96139, #237203 ) ) ;
#46462 = CARTESIAN_POINT ( 'NONE',  ( 18.59999999999999076, 65.79142135624927334, -111.8731074845243683 ) ) ;
#46463 = VECTOR ( 'NONE', #39088, 1000.000000000000000 ) ;
#46464 = EDGE_LOOP ( 'NONE', ( #101378, #82916, #23780, #253165 ) ) ;
#46465 = CARTESIAN_POINT ( 'NONE',  ( -16.87683809663752399, 44.13548170601895038, -235.2989316066074821 ) ) ;
#46466 = FACE_OUTER_BOUND ( 'NONE', #227400, .T. ) ;
#46467 = DIRECTION ( 'NONE',  ( 0.000000000000000000, 0.2128009952263603677, -0.9770955615653315052 ) ) ;
#46468 = DIRECTION ( 'NONE',  ( 0.000000000000000000, 0.9594490217226104845, 0.2818822000686205254 ) ) ;
#46469 = DIRECTION ( 'NONE',  ( -1.000000000000000000, 0.000000000000000000, 0.000000000000000000 ) ) ;
#46471 = CARTESIAN_POINT ( 'NONE',  ( -18.40000000000000213, -9.500000000000007105, -7.032069396699661468 ) ) ;
#46470 = VECTOR ( 'NONE', #167310, 1000.000000000000000 ) ;
#46472 = CARTESIAN_POINT ( 'NONE',  ( 18.59999999999999076, 55.07231556048840559, -230.1160242994351108 ) ) ;
#46473 = CARTESIAN_POINT ( 'NONE',  ( 21.93340585898357631, 1.115541036281197940E-11, -93.17585297786898479 ) ) ;
#46474 = EDGE_CURVE ( 'NONE', #11297, #52066, #55879, .T. ) ;
#46475 = DIRECTION ( 'NONE',  ( 0.000000000000000000, 0.3042567129659888292, 0.9525900758537912960 ) ) ;
#46476 = CARTESIAN_POINT ( 'NONE',  ( 21.05000000000000071, 69.35000000001159037, -59.50608031408435039 ) ) ;
#46477 = PLANE ( 'NONE',  #73074 ) ;
#46478 = AXIS2_PLACEMENT_3D ( 'NONE', #63857, #222916, #108120 ) ;
#46479 = EDGE_CURVE ( 'NONE', #1926, #85926, #110066, .T. ) ;
#46480 = CIRCLE ( 'NONE', #179794, 0.1999999999999997335 ) ;
#46481 = LINE ( 'NONE', #245992, #54014 ) ;
#46482 = CARTESIAN_POINT ( 'NONE',  ( 21.05000000000000071, 64.40000000001248281, -176.9513107147999449 ) ) ;
#46483 = ORIENTED_EDGE ( 'NONE', *, *, #80063, .T. ) ;
#46484 = CIRCLE ( 'NONE', #58948, 0.09999999999999990841 ) ;
#46485 = DIRECTION ( 'NONE',  ( 1.000000000000000000, 0.000000000000000000, 0.000000000000000000 ) ) ;
#46487 = EDGE_CURVE ( 'NONE', #195708, #34506, #180823, .T. ) ;
#46486 = DIRECTION ( 'NONE',  ( 0.000000000000000000, -8.232585987686539041E-15, 1.000000000000000000 ) ) ;
#46488 = EDGE_CURVE ( 'NONE', #247369, #147468, #172490, .T. ) ;
#46489 = VECTOR ( 'NONE', #77332, 1000.000000000000000 ) ;
#46490 = VERTEX_POINT ( 'NONE', #96171 ) ;
#46491 = FACE_OUTER_BOUND ( 'NONE', #195481, .T. ) ;
#46492 = DIRECTION ( 'NONE',  ( 0.000000000000000000, 0.000000000000000000, -1.000000000000000000 ) ) ;
#46493 = LINE ( 'NONE', #107764, #193115 ) ;
#46494 = VERTEX_POINT ( 'NONE', #76619 ) ;
#46495 = CARTESIAN_POINT ( 'NONE',  ( -23.25000000000000000, 31.44980407958350455, -233.5445995079518866 ) ) ;
#46496 = CARTESIAN_POINT ( 'NONE',  ( 18.59999999999999432, 1.162701749949165642, -75.10000000000003695 ) ) ;
#46497 = AXIS2_PLACEMENT_3D ( 'NONE', #42992, #226742, #48107 ) ;
#46498 = ORIENTED_EDGE ( 'NONE', *, *, #255873, .T. ) ;
#46499 = AXIS2_PLACEMENT_3D ( 'NONE', #162911, #42939, #5056 ) ;
#46500 = CIRCLE ( 'NONE', #196356, 6.258578643762696458 ) ;
#46501 = EDGE_CURVE ( 'NONE', #53074, #104197, #126641, .T. ) ;
#46502 = VECTOR ( 'NONE', #45750, 999.9999999999998863 ) ;
#46503 = EDGE_CURVE ( 'NONE', #231047, #200485, #255783, .T. ) ;
#46504 = DIRECTION ( 'NONE',  ( -1.000000000000000000, -3.448943450116723568E-16, -6.438528483529607644E-16 ) ) ;
#46505 = VERTEX_POINT ( 'NONE', #174505 ) ;
#46506 = CARTESIAN_POINT ( 'NONE',  ( -23.15000000000000213, -8.999999999988844479, -157.6060308773475924 ) ) ;
#46507 = DIRECTION ( 'NONE',  ( 0.000000000000000000, -7.056502275159890832E-15, 1.000000000000000000 ) ) ;
#46508 = DIRECTION ( 'NONE',  ( -0.000000000000000000, 0.9770955615653316162, 0.2128009952263604232 ) ) ;
#46509 = DIRECTION ( 'NONE',  ( -1.000000000000000000, 0.000000000000000000, 0.000000000000000000 ) ) ;
#46510 = DIRECTION ( 'NONE',  ( 0.000000000000000000, 3.552713678800509607E-15, 1.000000000000000000 ) ) ;
#46511 = DIRECTION ( 'NONE',  ( 0.000000000000000000, 0.000000000000000000, 1.000000000000000000 ) ) ;
#46512 = DIRECTION ( 'NONE',  ( -1.000000000000000000, 0.000000000000000000, -0.000000000000000000 ) ) ;
#46513 = LINE ( 'NONE', #205588, #13756 ) ;
#46514 = DIRECTION ( 'NONE',  ( 1.836970198721030427E-16, 0.4088369013363281623, -0.9126074666063771490 ) ) ;
#46517 = ORIENTED_EDGE ( 'NONE', *, *, #145313, .T. ) ;
#46516 = ADVANCED_FACE ( 'NONE', ( #135299 ), #230718, .T. ) ;
#46515 = CARTESIAN_POINT ( 'NONE',  ( -22.50000000000000000, 75.90000000001242597, -177.8138870828977360 ) ) ;
#46518 = VERTEX_POINT ( 'NONE', #201703 ) ;
#46520 = FACE_OUTER_BOUND ( 'NONE', #116178, .T. ) ;
#46519 = DIRECTION ( 'NONE',  ( -0.7071067811865474617, -0.7071067811865474617, -0.000000000000000000 ) ) ;
#46521 = ORIENTED_EDGE ( 'NONE', *, *, #81626, .F. ) ;
#46522 = ORIENTED_EDGE ( 'NONE', *, *, #73466, .F. ) ;
#46523 = EDGE_CURVE ( 'NONE', #7471, #44689, #218199, .T. ) ;
#46524 = PLANE ( 'NONE',  #104023 ) ;
#46525 = VECTOR ( 'NONE', #17214, 1000.000000000000000 ) ;
#46526 = DIRECTION ( 'NONE',  ( 0.000000000000000000, -0.9908441862701605762, -0.1350103645451835310 ) ) ;
#46527 = CARTESIAN_POINT ( 'NONE',  ( -20.85000000000000142, 76.32388570108204817, -69.56551789521031992 ) ) ;
#46528 = CARTESIAN_POINT ( 'NONE',  ( -20.93975676684922504, 10.31104185824063535, -173.0204516983106089 ) ) ;
#46529 = DIRECTION ( 'NONE',  ( 0.000000000000000000, -1.000000000000000000, -6.982962677686266711E-15 ) ) ;
#46531 = EDGE_CURVE ( 'NONE', #11593, #169411, #214137, .T. ) ;
#46530 = DIRECTION ( 'NONE',  ( -0.000000000000000000, 0.4791956752371485107, 0.8777080977375185666 ) ) ;
#46532 = EDGE_CURVE ( 'NONE', #210220, #26629, #122181, .T. ) ;
#46533 = DIRECTION ( 'NONE',  ( -3.265361837132813586E-16, 1.000000000000000000, 0.000000000000000000 ) ) ;
#46534 = ORIENTED_EDGE ( 'NONE', *, *, #42597, .F. ) ;
#46535 = ORIENTED_EDGE ( 'NONE', *, *, #211589, .T. ) ;
#46536 = CARTESIAN_POINT ( 'NONE',  ( 21.05000000000000071, 24.12844930803501242, -253.0488546976795021 ) ) ;
#46537 = EDGE_CURVE ( 'NONE', #42318, #163693, #85565, .T. ) ;
#46538 = ORIENTED_EDGE ( 'NONE', *, *, #214186, .F. ) ;
#46539 = CARTESIAN_POINT ( 'NONE',  ( 23.25000000000000000, 86.43238724539048690, -209.5644480942280836 ) ) ;
#46540 = ORIENTED_EDGE ( 'NONE', *, *, #86973, .T. ) ;
#46541 = CARTESIAN_POINT ( 'NONE',  ( -16.83199318825829494, 9.930646127992320160, -154.7275851882092184 ) ) ;
#46542 = EDGE_CURVE ( 'NONE', #212171, #117495, #23094, .T. ) ;
#46543 = VECTOR ( 'NONE', #196866, 1000.000000000000000 ) ;
#46544 = DIRECTION ( 'NONE',  ( 0.000000000000000000, -6.982962677686266711E-15, 1.000000000000000000 ) ) ;
#46545 = CARTESIAN_POINT ( 'NONE',  ( -23.15000000000000213, 4.349999999999999645, -12.35000000000000142 ) ) ;
#46546 = CARTESIAN_POINT ( 'NONE',  ( -16.92973740335385102, 22.94872168439534832, -230.8711258231723491 ) ) ;
#46547 = ORIENTED_EDGE ( 'NONE', *, *, #112083, .F. ) ;
#46548 = EDGE_CURVE ( 'NONE', #175208, #141902, #101669, .T. ) ;
#46549 = DIRECTION ( 'NONE',  ( -1.000000000000000000, 0.000000000000000000, 0.000000000000000000 ) ) ;
#46550 = ORIENTED_EDGE ( 'NONE', *, *, #1329, .F. ) ;
#46551 = DIRECTION ( 'NONE',  ( -1.000000000000000000, -0.000000000000000000, -0.000000000000000000 ) ) ;
#46552 = DIRECTION ( 'NONE',  ( 1.000000000000000000, 0.000000000000000000, 0.000000000000000000 ) ) ;
#46553 = CARTESIAN_POINT ( 'NONE',  ( -21.05000000000000071, 76.00000000001244871, -170.0231074845243597 ) ) ;
#46554 = ADVANCED_FACE ( 'NONE', ( #126009 ), #103863, .F. ) ;
#46555 = CARTESIAN_POINT ( 'NONE',  ( -22.50000000000000000, 64.35042919246716053, -103.1231074845243825 ) ) ;
#46556 = VERTEX_POINT ( 'NONE', #185996 ) ;
#46558 = LINE ( 'NONE', #225189, #219340 ) ;
#46557 = CIRCLE ( 'NONE', #250580, 0.09999999999999939493 ) ;
#46559 = ORIENTED_EDGE ( 'NONE', *, *, #201895, .T. ) ;
#46562 = ORIENTED_EDGE ( 'NONE', *, *, #13916, .F. ) ;
#46561 = CARTESIAN_POINT ( 'NONE',  ( -23.25000000000000000, -8.596261682231835621, -76.45012751715033517 ) ) ;
#46560 = CARTESIAN_POINT ( 'NONE',  ( 23.14999999999999858, 5.600000000011153389, -146.4052660189131245 ) ) ;
#46563 = CIRCLE ( 'NONE', #586, 0.09999999999998898659 ) ;
#46564 = DIRECTION ( 'NONE',  ( 3.469446951953514477E-14, 0.9999176327611370985, 0.01283462868040226822 ) ) ;
#46565 = EDGE_LOOP ( 'NONE', ( #208967, #15301, #205136, #130803, #232105, #136505, #195426, #164392, #25170, #214993, #48649, #106031 ) ) ;
#46566 = AXIS2_PLACEMENT_3D ( 'NONE', #61898, #108727, #43622 ) ;
#46567 = CARTESIAN_POINT ( 'NONE',  ( -21.05000000000000071, 4.481636728799211156, -245.1292951062512770 ) ) ;
#46568 = ORIENTED_EDGE ( 'NONE', *, *, #249066, .T. ) ;
#46569 = CARTESIAN_POINT ( 'NONE',  ( -1.739115166359751170E-14, 13.98997548377050748, -210.4902890347897255 ) ) ;
#46570 = EDGE_CURVE ( 'NONE', #16895, #71383, #86866, .T. ) ;
#46571 = DIRECTION ( 'NONE',  ( -0.000000000000000000, -0.000000000000000000, -1.000000000000000000 ) ) ;
#46572 = CYLINDRICAL_SURFACE ( 'NONE', #205224, 0.8750000000000007772 ) ;
#46573 = CARTESIAN_POINT ( 'NONE',  ( -18.44085059012131822, 54.07345485900965087, -229.1330576149768774 ) ) ;
#46574 = DIRECTION ( 'NONE',  ( 1.000000000000000000, 0.000000000000000000, 0.000000000000000000 ) ) ;
#46575 = AXIS2_PLACEMENT_3D ( 'NONE', #104183, #44241, #66361 ) ;
#46576 = ORIENTED_EDGE ( 'NONE', *, *, #45337, .T. ) ;
#46577 = CYLINDRICAL_SURFACE ( 'NONE', #198306, 2.000000000000001776 ) ;
#46578 = CARTESIAN_POINT ( 'NONE',  ( -14.77738660682464911, 66.56344716000788253, -154.8451520117641280 ) ) ;
#46579 = EDGE_LOOP ( 'NONE', ( #126097, #172052, #30972, #251760 ) ) ;
#46580 = DIRECTION ( 'NONE',  ( 0.000000000000000000, -1.411300455031978166E-14, 1.000000000000000000 ) ) ;
#46581 = ORIENTED_EDGE ( 'NONE', *, *, #230760, .T. ) ;
#46582 = CARTESIAN_POINT ( 'NONE',  ( -22.59999999999999787, 64.25043287652299284, -170.1239658536231616 ) ) ;
#46583 = CARTESIAN_POINT ( 'NONE',  ( -18.59999999999999787, 46.46967969402478360, -243.0849751855955674 ) ) ;
#46584 = DIRECTION ( 'NONE',  ( 0.000000000000000000, -6.454785026890406770E-15, 1.000000000000000000 ) ) ;
#46586 = ORIENTED_EDGE ( 'NONE', *, *, #70916, .T. ) ;
#46585 = CARTESIAN_POINT ( 'NONE',  ( -16.87333278164109629, 44.60397586039064066, -235.1628955916846166 ) ) ;
#46587 = CARTESIAN_POINT ( 'NONE',  ( -18.59999999999999787, 74.36282728704118483, -57.94095411905231430 ) ) ;
#46588 = CARTESIAN_POINT ( 'NONE',  ( 18.39999999999999503, 11.47316190337363828, -124.7500000000000426 ) ) ;
#46589 = CIRCLE ( 'NONE', #183993, 0.1000000000000028644 ) ;
#46590 = DIRECTION ( 'NONE',  ( 0.000000000000000000, -0.4999999999999949485, 0.8660254037844415942 ) ) ;
#46591 = EDGE_LOOP ( 'NONE', ( #11748, #49771, #109496 ) ) ;
#46592 = AXIS2_PLACEMENT_3D ( 'NONE', #72152, #129547, #248206 ) ;
#46593 = DIRECTION ( 'NONE',  ( 1.000000000000000000, 0.000000000000000000, 0.000000000000000000 ) ) ;
#46594 = DIRECTION ( 'NONE',  ( -1.000000000000000000, 0.000000000000000000, 0.000000000000000000 ) ) ;
#46595 = ORIENTED_EDGE ( 'NONE', *, *, #192635, .T. ) ;
#46596 = CARTESIAN_POINT ( 'NONE',  ( 22.49544290803777358, 64.25012976215509752, -170.0884194437818735 ) ) ;
#46597 = ADVANCED_FACE ( 'NONE', ( #182153 ), #145571, .F. ) ;
#46598 = ORIENTED_EDGE ( 'NONE', *, *, #171673, .T. ) ;
#46599 = CARTESIAN_POINT ( 'NONE',  ( -16.87683809663753465, 44.74130085420379999, -235.1207662860264520 ) ) ;
#46601 = VERTEX_POINT ( 'NONE', #47746 ) ;
#46600 = CARTESIAN_POINT ( 'NONE',  ( 21.05000000000000071, 6.350000000011161383, -143.8438220896831581 ) ) ;
#46602 = EDGE_CURVE ( 'NONE', #180750, #225961, #134991, .T. ) ;
#46603 = AXIS2_PLACEMENT_3D ( 'NONE', #213236, #52882, #132435 ) ;
#46606 = VERTEX_POINT ( 'NONE', #127305 ) ;
#46605 = ORIENTED_EDGE ( 'NONE', *, *, #242328, .T. ) ;
#46604 = DIRECTION ( 'NONE',  ( 1.000000000000000000, 0.000000000000000000, 0.000000000000000000 ) ) ;
#46607 = ADVANCED_FACE ( 'NONE', ( #206844 ), #101265, .T. ) ;
#46608 = DIRECTION ( 'NONE',  ( -1.073024830501117725E-15, 0.000000000000000000, -1.000000000000000000 ) ) ;
#46609 = EDGE_CURVE ( 'NONE', #166239, #92704, #83004, .T. ) ;
#46610 = DIRECTION ( 'NONE',  ( -1.000000000000000000, -0.000000000000000000, -0.000000000000000000 ) ) ;
#46611 = CARTESIAN_POINT ( 'NONE',  ( -20.85000000000000142, 11.65000000001115232, -134.0000000000000284 ) ) ;
#46613 = FACE_OUTER_BOUND ( 'NONE', #130348, .T. ) ;
#46612 = CARTESIAN_POINT ( 'NONE',  ( 20.94999675878240808, 46.33100819526731584, -243.0553980158188381 ) ) ;
#46614 = DIRECTION ( 'NONE',  ( 0.000000000000000000, 0.2128009952263603122, -0.9770955615653315052 ) ) ;
#46615 = CARTESIAN_POINT ( 'NONE',  ( 21.05000000000000071, 71.00000000001180922, -81.92837350343744163 ) ) ;
#46616 = CARTESIAN_POINT ( 'NONE',  ( -16.91247567987036504, 44.11235215177685376, -235.2993409081199445 ) ) ;
#46617 = DIRECTION ( 'NONE',  ( 0.000000000000000000, -1.000000000000000000, 0.000000000000000000 ) ) ;
#46618 = DIRECTION ( 'NONE',  ( 5.421010862427554711E-16, 1.000000000000000000, 1.023556919514279895E-14 ) ) ;
#46619 = VERTEX_POINT ( 'NONE', #63467 ) ;
#46620 = ORIENTED_EDGE ( 'NONE', *, *, #153324, .T. ) ;
#46621 = DIRECTION ( 'NONE',  ( -3.265361837132813093E-16, 1.000000000000000000, 0.000000000000000000 ) ) ;
#46623 = ORIENTED_EDGE ( 'NONE', *, *, #37238, .T. ) ;
#46622 = DIRECTION ( 'NONE',  ( 1.000000000000000000, 0.000000000000000000, 0.000000000000000000 ) ) ;
#46624 = ORIENTED_EDGE ( 'NONE', *, *, #207460, .T. ) ;
#46625 = ADVANCED_FACE ( 'NONE', ( #142989 ), #222531, .F. ) ;
#46627 = DIRECTION ( 'NONE',  ( 0.000000000000000000, 0.000000000000000000, -1.000000000000000000 ) ) ;
#46626 = VECTOR ( 'NONE', #257943, 1000.000000000000000 ) ;
#46628 = ORIENTED_EDGE ( 'NONE', *, *, #101064, .T. ) ;
#46629 = CARTESIAN_POINT ( 'NONE',  ( 20.84999999999998721, 64.25000000001142553, -36.02310748452440237 ) ) ;
#46630 = CIRCLE ( 'NONE', #71626, 0.5000000000000004441 ) ;
#46631 = ORIENTED_EDGE ( 'NONE', *, *, #233760, .F. ) ;
#46632 = AXIS2_PLACEMENT_3D ( 'NONE', #106866, #52018, #92433 ) ;
#46634 = CIRCLE ( 'NONE', #117397, 11.70000000000000284 ) ;
#46633 = CARTESIAN_POINT ( 'NONE',  ( -16.89208623190940273, 66.04842205103675212, -149.1678352813061394 ) ) ;
#46635 = CARTESIAN_POINT ( 'NONE',  ( -20.85000000000000142, -1.164121893230052995, -175.3148480855716400 ) ) ;
#46636 = VECTOR ( 'NONE', #172416, 999.9999999999998863 ) ;
#46638 = ORIENTED_EDGE ( 'NONE', *, *, #69103, .F. ) ;
#46637 = ORIENTED_EDGE ( 'NONE', *, *, #208165, .T. ) ;
#46639 = ORIENTED_EDGE ( 'NONE', *, *, #146606, .F. ) ;
#46641 = CARTESIAN_POINT ( 'NONE',  ( 21.11701782572533048, 10.72160911601861244, -45.74503742951121410 ) ) ;
#46640 = AXIS2_PLACEMENT_3D ( 'NONE', #216422, #147154, #224120 ) ;
#46642 = ORIENTED_EDGE ( 'NONE', *, *, #57104, .T. ) ;
#46643 = VERTEX_POINT ( 'NONE', #90729 ) ;
#46644 = CARTESIAN_POINT ( 'NONE',  ( -18.50000000000000000, 6.846123162363745074, -171.2377262668498759 ) ) ;
#46645 = DIRECTION ( 'NONE',  ( 0.000000000000000000, 0.000000000000000000, 1.000000000000000000 ) ) ;
#46646 = AXIS2_PLACEMENT_3D ( 'NONE', #165124, #60876, #103840 ) ;
#46648 = VERTEX_POINT ( 'NONE', #133716 ) ;
#46647 = CARTESIAN_POINT ( 'NONE',  ( -23.15000000000000213, 5.950000000011163692, -90.19429769496522908 ) ) ;
#46649 = ADVANCED_FACE ( 'NONE', ( #227677 ), #11217, .T. ) ;
#46650 = EDGE_CURVE ( 'NONE', #103845, #67554, #50312, .T. ) ;
#46651 = CARTESIAN_POINT ( 'NONE',  ( 21.05000000000000071, 0.9150442794848463457, -205.2015109147324665 ) ) ;
#46653 = ORIENTED_EDGE ( 'NONE', *, *, #243669, .F. ) ;
#46652 = DIRECTION ( 'NONE',  ( -0.000000000000000000, 1.000000000000000000, -0.000000000000000000 ) ) ;
#46654 = DIRECTION ( 'NONE',  ( 0.000000000000000000, 0.000000000000000000, -1.000000000000000000 ) ) ;
#46655 = ORIENTED_EDGE ( 'NONE', *, *, #105900, .F. ) ;
#46656 = DIRECTION ( 'NONE',  ( 0.000000000000000000, 0.000000000000000000, 1.000000000000000000 ) ) ;
#46657 = AXIS2_PLACEMENT_3D ( 'NONE', #44158, #124976, #244908 ) ;
#46658 = VERTEX_POINT ( 'NONE', #29522 ) ;
#46659 = CIRCLE ( 'NONE', #50747, 0.1000000000000026007 ) ;
#46660 = DIRECTION ( 'NONE',  ( 0.000000000000000000, 0.8814952561688437216, -0.4721928772777334582 ) ) ;
#46661 = CARTESIAN_POINT ( 'NONE',  ( -15.55912972643741199, 44.64076703536271395, -236.6714279798352152 ) ) ;
#46662 = ADVANCED_FACE ( 'NONE', ( #49046 ), #14242, .F. ) ;
#46664 = ORIENTED_EDGE ( 'NONE', *, *, #192188, .F. ) ;
#46663 = AXIS2_PLACEMENT_3D ( 'NONE', #81783, #242173, #103922 ) ;
#46666 = CARTESIAN_POINT ( 'NONE',  ( 23.15000000000000213, 41.42187432231295219, -260.1830396872097140 ) ) ;
#46665 = CARTESIAN_POINT ( 'NONE',  ( -20.64999999999999858, 71.65000000001199965, -115.3731074845243256 ) ) ;
#46667 = AXIS2_PLACEMENT_3D ( 'NONE', #159012, #4694, #223746 ) ;
#46668 = LINE ( 'NONE', #128803, #230294 ) ;
#46669 = FACE_OUTER_BOUND ( 'NONE', #99026, .T. ) ;
#46670 = ORIENTED_EDGE ( 'NONE', *, *, #24521, .T. ) ;
#46671 = ORIENTED_EDGE ( 'NONE', *, *, #32016, .F. ) ;
#46672 = AXIS2_PLACEMENT_3D ( 'NONE', #10219, #50592, #152312 ) ;
#46673 = DIRECTION ( 'NONE',  ( 0.000000000000000000, 1.000000000000000000, 0.000000000000000000 ) ) ;
#46674 = CARTESIAN_POINT ( 'NONE',  ( -20.12071067811865888, 22.41647294715246375, -231.3481210999354403 ) ) ;
#46675 = VERTEX_POINT ( 'NONE', #128593 ) ;
#46676 = DIRECTION ( 'NONE',  ( 0.000000000000000000, 0.9908441862701782288, 0.1350103645450542456 ) ) ;
#46677 = ORIENTED_EDGE ( 'NONE', *, *, #64609, .T. ) ;
#46678 = CARTESIAN_POINT ( 'NONE',  ( -20.64999999999999858, 76.00000000001190870, -103.0231074845243029 ) ) ;
#46679 = CIRCLE ( 'NONE', #192443, 12.87499999999999112 ) ;
#46680 = VERTEX_POINT ( 'NONE', #150725 ) ;
#46681 = DIRECTION ( 'NONE',  ( 0.000000000000000000, -0.9651348961777157509, 0.2617529984165031243 ) ) ;
#46682 = FACE_OUTER_BOUND ( 'NONE', #129381, .T. ) ;
#46683 = EDGE_CURVE ( 'NONE', #66247, #221268, #97386, .T. ) ;
#46684 = DIRECTION ( 'NONE',  ( -0.000000000000000000, 0.000000000000000000, -1.000000000000000000 ) ) ;
#46685 = ORIENTED_EDGE ( 'NONE', *, *, #190632, .T. ) ;
#46686 = DIRECTION ( 'NONE',  ( 6.938893903907991995E-14, 0.000000000000000000, 1.000000000000000000 ) ) ;
#46687 = CIRCLE ( 'NONE', #59134, 1.749999999999998002 ) ;
#46688 = AXIS2_PLACEMENT_3D ( 'NONE', #175743, #216115, #93614 ) ;
#46689 =( BOUNDED_SURFACE ( )  B_SPLINE_SURFACE ( 3, 2, ( 
 ( #222325, #142794, #102373 ),
 ( #198933, #157276, #98508 ),
 ( #181956, #97229, #19016 ),
 ( #20326, #159835, #118124 ),
 ( #161114, #217201, #257569 ),
 ( #78962, #158559, #60696 ) ),
 .UNSPECIFIED., .F., .F., .T. ) 
 B_SPLINE_SURFACE_WITH_KNOTS ( ( 4, 2, 4 ),
 ( 3, 3 ),
 ( 0.0001792624049599545865, 0.0003686986002124822948, 0.0005581347954650100031 ),
 ( 0.000000000000000000, 1.000000000000000000 ),
 .UNSPECIFIED. ) 
 GEOMETRIC_REPRESENTATION_ITEM ( )  RATIONAL_B_SPLINE_SURFACE ( (
 ( 1.000000000000000000, 0.9238795325112834078, 1.000000000000000000),
 ( 1.000000000000000000, 0.9229318695230264158, 1.000000000000000000),
 ( 1.000000000000000000, 0.8926288119241689856, 1.000000000000000000),
 ( 1.000000000000000000, 0.8123777807260450512, 1.000000000000000000),
 ( 1.000000000000000000, 0.7629087100939330179, 1.000000000000000000),
 ( 1.000000000000000000, 0.7071067811865966446, 1.000000000000000000) ) ) 
 REPRESENTATION_ITEM ( '' )  SURFACE ( )  );
#46690 = TOROIDAL_SURFACE ( 'NONE', #159170, 6.258578643762700899, 0.1000000000000000056 ) ;
#46691 = EDGE_LOOP ( 'NONE', ( #134503, #198780, #223081 ) ) ;
#46692 = ORIENTED_EDGE ( 'NONE', *, *, #120097, .F. ) ;
#46693 = ORIENTED_EDGE ( 'NONE', *, *, #187147, .T. ) ;
#46694 = B_SPLINE_CURVE_WITH_KNOTS ( 'NONE', 3,
 ( #6740, #27630, #187958, #26319, #86252, #5430, #203661, #163266, #65428, #64156, #48428, #44596, #224501, #108418, #165839, #129264 ),
 .UNSPECIFIED., .F., .F.,
 ( 4, 3, 3, 3, 3, 4 ),
 ( 0.000000000000000000, 2.372700795693673338E-05, 5.739057815866516020E-05, 9.073899019180219387E-05, 0.0001243544287365659932, 0.0001585386695601174523 ),
 .UNSPECIFIED. ) ;
#46695 = EDGE_CURVE ( 'NONE', #192087, #250224, #251537, .T. ) ;
#46696 = DIRECTION ( 'NONE',  ( 0.000000000000000000, 0.000000000000000000, 1.000000000000000000 ) ) ;
#46697 = CARTESIAN_POINT ( 'NONE',  ( 23.25000000000000000, -3.281532336344783030, -226.3283167004136942 ) ) ;
#46698 = DIRECTION ( 'NONE',  ( -1.000000000000000000, 0.000000000000000000, 0.000000000000000000 ) ) ;
#46699 = CYLINDRICAL_SURFACE ( 'NONE', #223597, 0.09999999999999939493 ) ;
#46700 = CYLINDRICAL_SURFACE ( 'NONE', #80047, 2.000000000000001776 ) ;
#46702 = CARTESIAN_POINT ( 'NONE',  ( 22.39999999999999503, 11.45959274888150681, -198.4018787499352641 ) ) ;
#46701 = FACE_OUTER_BOUND ( 'NONE', #70610, .T. ) ;
#46704 = EDGE_LOOP ( 'NONE', ( #164926, #145529, #112525, #149977 ) ) ;
#46703 = DIRECTION ( 'NONE',  ( 0.000000000000000000, 0.2617529984165030132, 0.9651348961777156399 ) ) ;
#46705 = DIRECTION ( 'NONE',  ( 0.000000000000000000, 0.000000000000000000, -1.000000000000000000 ) ) ;
#46706 = ORIENTED_EDGE ( 'NONE', *, *, #96198, .T. ) ;
#46707 = ADVANCED_FACE ( 'NONE', ( #231551 ), #72484, .F. ) ;
#46708 = EDGE_CURVE ( 'NONE', #50336, #110098, #163678, .T. ) ;
#46709 = VERTEX_POINT ( 'NONE', #52894 ) ;
#46710 = ORIENTED_EDGE ( 'NONE', *, *, #217162, .T. ) ;
#46711 = FACE_OUTER_BOUND ( 'NONE', #181529, .T. ) ;
#46712 = DIRECTION ( 'NONE',  ( 1.000000000000000000, 0.000000000000000000, 0.000000000000000000 ) ) ;
#46713 = DIRECTION ( 'NONE',  ( 0.000000000000000000, 0.2128009952263485993, -0.9770955615653341697 ) ) ;
#46714 = CARTESIAN_POINT ( 'NONE',  ( -23.15000000000000213, 11.65000000001115588, -93.48519422934609224 ) ) ;
#46715 = CIRCLE ( 'NONE', #200854, 0.1000000000000028644 ) ;
#46716 = ADVANCED_FACE ( 'NONE', ( #13778 ), #148148, .F. ) ;
#46717 = DIRECTION ( 'NONE',  ( -0.000000000000000000, 1.000000000000000000, -0.000000000000000000 ) ) ;
#46718 = ADVANCED_FACE ( 'NONE', ( #112879 ), #209403, .F. ) ;
#46719 = VERTEX_POINT ( 'NONE', #93307 ) ;
#46720 = ORIENTED_EDGE ( 'NONE', *, *, #142074, .F. ) ;
#46721 = CARTESIAN_POINT ( 'NONE',  ( -17.11825945287481332, 10.05000000001113847, -188.3499999999999659 ) ) ;
#46722 = ORIENTED_EDGE ( 'NONE', *, *, #172998, .T. ) ;
#46723 = CARTESIAN_POINT ( 'NONE',  ( 18.49999999999999645, -3.616484641954614165, -226.0163245033746477 ) ) ;
#46724 = DIRECTION ( 'NONE',  ( 0.000000000000000000, -0.4088369013363282178, 0.9126074666063770380 ) ) ;
#46725 = CARTESIAN_POINT ( 'NONE',  ( -21.05000000000000071, 74.25000000001205080, -124.8535959266226598 ) ) ;
#46727 = EDGE_CURVE ( 'NONE', #16782, #172822, #172899, .T. ) ;
#46726 = DIRECTION ( 'NONE',  ( -3.265361837132813093E-16, 1.000000000000000000, 0.000000000000000000 ) ) ;
#46728 = CARTESIAN_POINT ( 'NONE',  ( 23.14999999999999503, 69.35000000001254250, -182.3731074845244109 ) ) ;
#46729 = CARTESIAN_POINT ( 'NONE',  ( 20.94999999999999929, 6.450000000000001066, -10.01702717044001822 ) ) ;
#46730 = ORIENTED_EDGE ( 'NONE', *, *, #227513, .T. ) ;
#46731 = CARTESIAN_POINT ( 'NONE',  ( -23.15000000000000213, 4.250000000011156409, -179.7499999999999716 ) ) ;
#46732 = DIRECTION ( 'NONE',  ( 0.000000000000000000, 1.000000000000000000, 0.000000000000000000 ) ) ;
#46733 = DIRECTION ( 'NONE',  ( -0.000000000000000000, 1.000000000000000000, 6.982962677686266711E-15 ) ) ;
#46734 = DIRECTION ( 'NONE',  ( 0.000000000000000000, -1.000000000000000000, 5.551115123125768187E-14 ) ) ;
#46735 = ADVANCED_FACE ( 'NONE', ( #252365 ), #51581, .T. ) ;
#46736 = DIRECTION ( 'NONE',  ( -1.000000000000000000, -0.000000000000000000, -0.000000000000000000 ) ) ;
#46737 = LINE ( 'NONE', #126279, #190564 ) ;
#46738 = EDGE_CURVE ( 'NONE', #230960, #66524, #51217, .T. ) ;
#46739 = EDGE_CURVE ( 'NONE', #164082, #185160, #72691, .T. ) ;
#46741 = VERTEX_POINT ( 'NONE', #189847 ) ;
#46740 = AXIS2_PLACEMENT_3D ( 'NONE', #100939, #181818, #81392 ) ;
#46742 = EDGE_CURVE ( 'NONE', #221039, #220454, #134613, .T. ) ;
#46743 = CARTESIAN_POINT ( 'NONE',  ( -17.11825945287482753, 66.05000000001231797, -157.3731074845243825 ) ) ;
#46744 = ORIENTED_EDGE ( 'NONE', *, *, #10143, .T. ) ;
#46745 = CARTESIAN_POINT ( 'NONE',  ( 23.14999999999999503, 6.550000000000000711, -12.35000000000000320 ) ) ;
#46746 = EDGE_CURVE ( 'NONE', #237421, #194022, #111597, .T. ) ;
#46747 = CARTESIAN_POINT ( 'NONE',  ( -21.55000000000000071, 44.96555909964510533, -237.8856228368455845 ) ) ;
#46748 = CARTESIAN_POINT ( 'NONE',  ( 21.12400222705985797, 61.96530060562854203, -221.7344222149888822 ) ) ;
#46749 = EDGE_CURVE ( 'NONE', #109914, #233154, #114155, .T. ) ;
#46750 = EDGE_LOOP ( 'NONE', ( #27753, #113127, #127471, #147072, #20196, #79643, #36893 ) ) ;
#46751 = FACE_OUTER_BOUND ( 'NONE', #238283, .T. ) ;
#46752 = DIRECTION ( 'NONE',  ( 1.000000000000000000, 0.000000000000000000, 0.000000000000000000 ) ) ;
#46754 = EDGE_CURVE ( 'NONE', #23820, #142016, #72114, .T. ) ;
#46753 = CARTESIAN_POINT ( 'NONE',  ( -20.54999999999999716, 85.00000000001207923, -127.1291383618717816 ) ) ;
#46755 = CIRCLE ( 'NONE', #209253, 0.1000000000000013933 ) ;
#46756 = CARTESIAN_POINT ( 'NONE',  ( -21.12230431290519306, 69.54243334671936339, -170.0283173362134335 ) ) ;
#46757 = DIRECTION ( 'NONE',  ( 0.000000000000000000, 0.4999999999999966693, -0.8660254037844405950 ) ) ;
#46758 = VERTEX_POINT ( 'NONE', #254891 ) ;
#46759 = ORIENTED_EDGE ( 'NONE', *, *, #257302, .T. ) ;
#46760 = LINE ( 'NONE', #126301, #33464 ) ;
#46762 = ORIENTED_EDGE ( 'NONE', *, *, #246509, .F. ) ;
#46761 = FACE_OUTER_BOUND ( 'NONE', #196088, .T. ) ;
#46763 = CARTESIAN_POINT ( 'NONE',  ( -21.55000000000000426, 44.77807522791015060, -237.4671205425215135 ) ) ;
#46764 = CARTESIAN_POINT ( 'NONE',  ( 21.05000000000000071, 1.115600667400684642E-11, -200.9999999999999432 ) ) ;
#46765 = EDGE_CURVE ( 'NONE', #239334, #256668, #80426, .T. ) ;
#46766 = ORIENTED_EDGE ( 'NONE', *, *, #53008, .F. ) ;
#46767 = CYLINDRICAL_SURFACE ( 'NONE', #113843, 0.09999999999999982514 ) ;
#46768 = SPHERICAL_SURFACE ( 'NONE', #167533, 0.1000000000000000056 ) ;
#46769 = AXIS2_PLACEMENT_3D ( 'NONE', #195170, #230415, #16519 ) ;
#46770 = ORIENTED_EDGE ( 'NONE', *, *, #38189, .F. ) ;
#46771 = AXIS2_PLACEMENT_3D ( 'NONE', #36364, #115880, #195436 ) ;
#46772 = LINE ( 'NONE', #165466, #96312 ) ;
#46773 = VERTEX_POINT ( 'NONE', #38483 ) ;
#46774 = ORIENTED_EDGE ( 'NONE', *, *, #238373, .T. ) ;
#46775 = FACE_OUTER_BOUND ( 'NONE', #57775, .T. ) ;
#46776 = DIRECTION ( 'NONE',  ( 1.000000000000000000, 0.000000000000000000, 0.000000000000000000 ) ) ;
#46777 = DIRECTION ( 'NONE',  ( 0.000000000000000000, -1.000000000000000000, 0.000000000000000000 ) ) ;
#46778 = FACE_OUTER_BOUND ( 'NONE', #152929, .T. ) ;
#46779 = CARTESIAN_POINT ( 'NONE',  ( -18.34374000495059676, 11.47316190337362940, -191.7499999999999716 ) ) ;
#46781 = CARTESIAN_POINT ( 'NONE',  ( -18.50000000000000000, 74.13328508995527955, -191.7704322382423641 ) ) ;
#46780 = AXIS2_PLACEMENT_3D ( 'NONE', #135688, #75743, #155303 ) ;
#46782 = AXIS2_PLACEMENT_3D ( 'NONE', #75045, #9893, #228956 ) ;
#46783 = FACE_OUTER_BOUND ( 'NONE', #241974, .T. ) ;
#46786 = DIRECTION ( 'NONE',  ( 0.000000000000000000, 0.8814952561688430555, -0.4721928772777346239 ) ) ;
#46785 = CIRCLE ( 'NONE', #80075, 0.1000000000000009492 ) ;
#46784 = LINE ( 'NONE', #45519, #120279 ) ;
#46787 = EDGE_CURVE ( 'NONE', #30145, #114885, #242774, .T. ) ;
#46788 = LINE ( 'NONE', #126339, #23080 ) ;
#46789 = DIRECTION ( 'NONE',  ( 0.000000000000000000, -0.000000000000000000, 1.000000000000000000 ) ) ;
#46790 = FACE_OUTER_BOUND ( 'NONE', #98395, .T. ) ;
#46791 = EDGE_LOOP ( 'NONE', ( #223335, #249026, #176910, #200235 ) ) ;
#46792 = EDGE_CURVE ( 'NONE', #233728, #136029, #18906, .T. ) ;
#46793 = EDGE_LOOP ( 'NONE', ( #234619, #203746, #16300, #27935 ) ) ;
#46794 = DIRECTION ( 'NONE',  ( 0.000000000000000000, -1.000000000000000000, 0.000000000000000000 ) ) ;
#46795 = CARTESIAN_POINT ( 'NONE',  ( 18.49999999999999645, 76.00000000001244871, -170.0231074845243597 ) ) ;
#46797 = CARTESIAN_POINT ( 'NONE',  ( 22.39999999999999503, -1.657885652111590780, -193.3876638332971538 ) ) ;
#46796 = CARTESIAN_POINT ( 'NONE',  ( 18.50000000000000000, 85.40000000001160174, -62.22584772486096227 ) ) ;
#46798 = CARTESIAN_POINT ( 'NONE',  ( -20.94999999999999929, 76.00000000001190870, -103.0231074845243029 ) ) ;
#46799 = SPHERICAL_SURFACE ( 'NONE', #137504, 0.1000000000000000056 ) ;
#46800 = DIRECTION ( 'NONE',  ( 1.000000000000000000, 0.000000000000000000, 0.000000000000000000 ) ) ;
#46801 = ORIENTED_EDGE ( 'NONE', *, *, #116816, .F. ) ;
#46802 = ORIENTED_EDGE ( 'NONE', *, *, #196288, .T. ) ;
#46803 = DIRECTION ( 'NONE',  ( 0.000000000000000000, 1.000000000000000000, 0.000000000000000000 ) ) ;
#46804 = ORIENTED_EDGE ( 'NONE', *, *, #72263, .T. ) ;
#46805 = EDGE_CURVE ( 'NONE', #123266, #116784, #56716, .T. ) ;
#46806 = DIRECTION ( 'NONE',  ( 0.000000000000000000, -7.172728831056617961E-15, 1.000000000000000000 ) ) ;
#46807 = CIRCLE ( 'NONE', #67672, 11.75000000000000000 ) ;
#46808 = CIRCLE ( 'NONE', #25993, 0.09999999999999939493 ) ;
#46809 = PLANE ( 'NONE',  #158982 ) ;
#46810 = EDGE_LOOP ( 'NONE', ( #1386, #104350, #80862, #250026 ) ) ;
#46811 = CARTESIAN_POINT ( 'NONE',  ( -18.55121869061588669, 18.40663661316795796, -236.9846611508999388 ) ) ;
#46812 = TOROIDAL_SURFACE ( 'NONE', #30280, 0.6000000000000015321, 0.1000000000000000056 ) ;
#46813 = VERTEX_POINT ( 'NONE', #158456 ) ;
#46814 = FACE_OUTER_BOUND ( 'NONE', #50768, .T. ) ;
#46815 = DIRECTION ( 'NONE',  ( 0.000000000000000000, 2.168404344971021884E-15, 1.000000000000000000 ) ) ;
#46817 = TOROIDAL_SURFACE ( 'NONE', #125936, 0.2000000000000000111, 0.1000000000000000056 ) ;
#46816 = CARTESIAN_POINT ( 'NONE',  ( -23.15000000000000213, -8.999999999988846255, -76.89396912265249284 ) ) ;
#46818 = CYLINDRICAL_SURFACE ( 'NONE', #12662, 0.09999999999999892308 ) ;
#46819 = CARTESIAN_POINT ( 'NONE',  ( -21.05000000000000071, 64.35000000001195986, -110.0379132551783243 ) ) ;
#46820 = CARTESIAN_POINT ( 'NONE',  ( -20.94999999999999929, 77.83534155023700407, -191.8679561919613832 ) ) ;
#46821 = AXIS2_PLACEMENT_3D ( 'NONE', #24488, #124852, #40206 ) ;
#46822 = CARTESIAN_POINT ( 'NONE',  ( -22.39999999999999858, 75.90000000001199965, -110.8138870828977218 ) ) ;
#46823 = DIRECTION ( 'NONE',  ( 0.000000000000000000, 0.8814952561688476074, -0.4721928772777262417 ) ) ;
#46824 = TOROIDAL_SURFACE ( 'NONE', #171776, 12.77499999999999858, 0.1000000000000000056 ) ;
#46826 = ORIENTED_EDGE ( 'NONE', *, *, #112974, .F. ) ;
#46825 = CARTESIAN_POINT ( 'NONE',  ( -18.50000000000000000, 68.97833521811233481, -166.1895420826271277 ) ) ;
#46828 = CARTESIAN_POINT ( 'NONE',  ( -21.05000000000000071, 44.43513953521873106, -247.3415577889845736 ) ) ;
#46827 = DIRECTION ( 'NONE',  ( 0.000000000000000000, 0.9126074666063771490, 0.4088369013363276627 ) ) ;
#46829 = EDGE_LOOP ( 'NONE', ( #75098, #55327, #43866, #201098 ) ) ;
#46831 = EDGE_LOOP ( 'NONE', ( #249236, #151512, #151586, #100784 ) ) ;
#46830 = DIRECTION ( 'NONE',  ( 1.000000000000000000, 0.000000000000000000, 0.000000000000000000 ) ) ;
#46832 = ORIENTED_EDGE ( 'NONE', *, *, #91621, .T. ) ;
#46833 = DIRECTION ( 'NONE',  ( 0.000000000000000000, -0.7106264324241464703, 0.7035695228903323661 ) ) ;
#46834 = CIRCLE ( 'NONE', #210019, 0.09999999999998898659 ) ;
#46835 = DIRECTION ( 'NONE',  ( 0.000000000000000000, -1.000000000000000000, 0.000000000000000000 ) ) ;
#46836 = CIRCLE ( 'NONE', #184210, 0.5000000000000004441 ) ;
#46837 = DIRECTION ( 'NONE',  ( -3.035766082959430717E-14, 0.000000000000000000, -1.000000000000000000 ) ) ;
#46838 = CARTESIAN_POINT ( 'NONE',  ( 0.000000000000000000, 1.250000000000000000, 0.000000000000000000 ) ) ;
#46839 = DIRECTION ( 'NONE',  ( -2.915501640297153790E-16, 1.000000000000000000, 0.000000000000000000 ) ) ;
#46840 = CIRCLE ( 'NONE', #113495, 0.09999999999999939493 ) ;
#46841 = EDGE_CURVE ( 'NONE', #3248, #157975, #198831, .T. ) ;
#46842 = LINE ( 'NONE', #6444, #6822 ) ;
#46843 = CIRCLE ( 'NONE', #17620, 0.5000000000000004441 ) ;
#46844 = EDGE_CURVE ( 'NONE', #169064, #250549, #97120, .T. ) ;
#46845 = CARTESIAN_POINT ( 'NONE',  ( 21.08078803292166015, 69.66698703557503336, -136.6022934716821169 ) ) ;
#46846 = VERTEX_POINT ( 'NONE', #157169 ) ;
#46847 = EDGE_LOOP ( 'NONE', ( #97130, #106771, #205278, #206668 ) ) ;
#46848 = LINE ( 'NONE', #169426, #93813 ) ;
#46849 = AXIS2_PLACEMENT_3D ( 'NONE', #232495, #248189, #91677 ) ;
#46850 = ORIENTED_EDGE ( 'NONE', *, *, #215560, .T. ) ;
#46851 = CARTESIAN_POINT ( 'NONE',  ( 18.59999999999999076, 77.85161776048096272, -124.9199177649206689 ) ) ;
#46852 = EDGE_LOOP ( 'NONE', ( #130708, #7119, #25387, #137766 ) ) ;
#46854 = VECTOR ( 'NONE', #40856, 1000.000000000000000 ) ;
#46853 = FACE_OUTER_BOUND ( 'NONE', #145091, .T. ) ;
#46855 = TOROIDAL_SURFACE ( 'NONE', #163404, 0.2000000000000000111, 0.1000000000000000056 ) ;
#46856 = ADVANCED_FACE ( 'NONE', ( #118011 ), #235382, .T. ) ;
#46857 = CARTESIAN_POINT ( 'NONE',  ( -17.11825945287482753, 10.05000000001113847, -180.1499999999999773 ) ) ;
#46858 = CARTESIAN_POINT ( 'NONE',  ( -22.46246831459151494, -2.457692491805503643, -189.6123061134737497 ) ) ;
#46859 = CIRCLE ( 'NONE', #242508, 0.1000000000000000472 ) ;
#46860 = CARTESIAN_POINT ( 'NONE',  ( -23.25000000000000000, 76.00000000001170974, -69.52310748452431710 ) ) ;
#46861 = ADVANCED_FACE ( 'NONE', ( #195005 ), #179301, .F. ) ;
#46862 = CARTESIAN_POINT ( 'NONE',  ( 23.40000000000005542, 83.98667523412385094, -37.28476067066772970 ) ) ;
#46863 = ORIENTED_EDGE ( 'NONE', *, *, #103165, .F. ) ;
#46864 = FACE_OUTER_BOUND ( 'NONE', #79477, .T. ) ;
#46865 = LINE ( 'NONE', #108149, #142175 ) ;
#46866 = EDGE_CURVE ( 'NONE', #139023, #211977, #143885, .T. ) ;
#46867 = CARTESIAN_POINT ( 'NONE',  ( -18.79999999999999716, 1.250000000000000000, 21.90000000000000213 ) ) ;
#46868 = LINE ( 'NONE', #205958, #118312 ) ;
#46869 = ORIENTED_EDGE ( 'NONE', *, *, #87563, .T. ) ;
#46871 = DIRECTION ( 'NONE',  ( 0.000000000000000000, 0.2617529984164506107, 0.9651348961777299618 ) ) ;
#46870 = CARTESIAN_POINT ( 'NONE',  ( 23.14999999999999503, 64.35000000001146248, -43.03791325517834565 ) ) ;
#46872 = CIRCLE ( 'NONE', #105108, 0.1000000000000003803 ) ;
#46873 = VERTEX_POINT ( 'NONE', #193707 ) ;
#46876 = ORIENTED_EDGE ( 'NONE', *, *, #40341, .T. ) ;
#46875 = CARTESIAN_POINT ( 'NONE',  ( 21.05000000000000071, -11.64999999998883595, -198.0999999999999659 ) ) ;
#46874 = CARTESIAN_POINT ( 'NONE',  ( 23.25000000000000000, -9.599999999988842347, -90.60603087734760663 ) ) ;
#46877 = CIRCLE ( 'NONE', #134356, 0.5000000000000004441 ) ;
#46878 = ORIENTED_EDGE ( 'NONE', *, *, #80827, .T. ) ;
#46879 = CARTESIAN_POINT ( 'NONE',  ( 21.05000000000000071, 10.45765418377745526, -207.3040725013013912 ) ) ;
#46880 = CIRCLE ( 'NONE', #130083, 0.2000000000000057288 ) ;
#46881 = CARTESIAN_POINT ( 'NONE',  ( -23.15000000000000213, 1.115600667400684642E-11, -204.8999999999999488 ) ) ;
#46882 = CARTESIAN_POINT ( 'NONE',  ( -23.15000000000000213, 76.00000000001170974, -69.52310748452431710 ) ) ;
#46883 = ORIENTED_EDGE ( 'NONE', *, *, #12205, .F. ) ;
#46884 = CARTESIAN_POINT ( 'NONE',  ( -18.40000000000000213, 11.75000000001113953, -54.35000000000000142 ) ) ;
#46885 = ADVANCED_FACE ( 'NONE', ( #34649 ), #185093, .T. ) ;
#46886 = DIRECTION ( 'NONE',  ( -0.000000000000000000, -0.9651348961777157509, 0.2617529984165031243 ) ) ;
#46888 = CARTESIAN_POINT ( 'NONE',  ( -17.01473183483382101, 44.22674245267958781, -235.2580479164738279 ) ) ;
#46887 = CARTESIAN_POINT ( 'NONE',  ( 18.59999999999999432, 74.27191306321728348, -82.63867247935655769 ) ) ;
#46890 = ORIENTED_EDGE ( 'NONE', *, *, #162904, .T. ) ;
#46889 = DIRECTION ( 'NONE',  ( -0.000000000000000000, 1.000000000000000000, 0.000000000000000000 ) ) ;
#46891 = VERTEX_POINT ( 'NONE', #239254 ) ;
#46892 = DIRECTION ( 'NONE',  ( -1.000000000000000000, -0.000000000000000000, -0.000000000000000000 ) ) ;
#46893 = CIRCLE ( 'NONE', #67760, 0.09999999999999938105 ) ;
#46894 = FACE_OUTER_BOUND ( 'NONE', #12073, .T. ) ;
#46895 = CARTESIAN_POINT ( 'NONE',  ( -20.94999999999994600, 64.25000000001119815, -5.923107484524795296 ) ) ;
#46896 = ORIENTED_EDGE ( 'NONE', *, *, #249198, .T. ) ;
#46897 = CARTESIAN_POINT ( 'NONE',  ( 23.15000000000000213, 87.75000000001156764, -57.37310748452424036 ) ) ;
#46898 = ORIENTED_EDGE ( 'NONE', *, *, #95767, .F. ) ;
#46899 = CIRCLE ( 'NONE', #130112, 4.049999999999974953 ) ;
#46900 = DIRECTION ( 'NONE',  ( -1.000000000000000000, 0.000000000000000000, 0.000000000000000000 ) ) ;
#46901 = CARTESIAN_POINT ( 'NONE',  ( 22.00356870141551724, 7.254242362499355501, -33.50000000000000711 ) ) ;
#46902 = ORIENTED_EDGE ( 'NONE', *, *, #207289, .T. ) ;
#46903 = FACE_OUTER_BOUND ( 'NONE', #194082, .T. ) ;
#46904 = VERTEX_POINT ( 'NONE', #95863 ) ;
#46905 = CARTESIAN_POINT ( 'NONE',  ( 23.40000000000005542, 76.00000000001119815, -3.023107484524792277 ) ) ;
#46906 = DIRECTION ( 'NONE',  ( -0.000000000000000000, 0.4721928772777345684, 0.8814952561688429444 ) ) ;
#46907 = ADVANCED_FACE ( 'NONE', ( #15071 ), #72320, .T. ) ;
#46909 = VERTEX_POINT ( 'NONE', #240535 ) ;
#46908 = AXIS2_PLACEMENT_3D ( 'NONE', #151717, #172583, #9589 ) ;
#46910 = ORIENTED_EDGE ( 'NONE', *, *, #236469, .F. ) ;
#46911 = FACE_OUTER_BOUND ( 'NONE', #222239, .T. ) ;
#46912 = ORIENTED_EDGE ( 'NONE', *, *, #117350, .T. ) ;
#46914 = EDGE_LOOP ( 'NONE', ( #25785, #142589, #192617, #19726 ) ) ;
#46913 = PLANE ( 'NONE',  #221818 ) ;
#46915 = ADVANCED_FACE ( 'NONE', ( #81424 ), #105954, .T. ) ;
#46916 = EDGE_LOOP ( 'NONE', ( #97708, #203081, #201652, #42452 ) ) ;
#46918 = ORIENTED_EDGE ( 'NONE', *, *, #27307, .F. ) ;
#46917 = ORIENTED_EDGE ( 'NONE', *, *, #215303, .F. ) ;
#46919 = EDGE_CURVE ( 'NONE', #160725, #196143, #172669, .T. ) ;
#46920 = EDGE_CURVE ( 'NONE', #110550, #72537, #205936, .T. ) ;
#46921 = CARTESIAN_POINT ( 'NONE',  ( -18.52309608778539385, -9.642476320044121252, -107.2145963411695675 ) ) ;
#46922 = CIRCLE ( 'NONE', #105350, 0.1000000000000124678 ) ;
#46923 = ORIENTED_EDGE ( 'NONE', *, *, #206068, .T. ) ;
#46924 = DIRECTION ( 'NONE',  ( -1.000000000000000000, 0.000000000000000000, 0.000000000000000000 ) ) ;
#46925 = FACE_OUTER_BOUND ( 'NONE', #152446, .T. ) ;
#46926 = CARTESIAN_POINT ( 'NONE',  ( -20.94999999999999929, -1.135018845910178431, -41.21697688343231647 ) ) ;
#46927 = CIRCLE ( 'NONE', #22024, 0.1000000000000028644 ) ;
#46928 = CARTESIAN_POINT ( 'NONE',  ( -18.46919391072062311, 87.08044166374625661, -199.6133279112425214 ) ) ;
#46929 = VERTEX_POINT ( 'NONE', #141425 ) ;
#46930 = ORIENTED_EDGE ( 'NONE', *, *, #129732, .T. ) ;
#46931 = AXIS2_PLACEMENT_3D ( 'NONE', #163799, #244595, #184627 ) ;
#46932 = LINE ( 'NONE', #228171, #91460 ) ;
#46934 = ORIENTED_EDGE ( 'NONE', *, *, #16240, .T. ) ;
#46933 = CARTESIAN_POINT ( 'NONE',  ( -23.15000000000000213, 1.115600667400684642E-11, -180.2749999999999773 ) ) ;
#46935 = CARTESIAN_POINT ( 'NONE',  ( -16.78569801330232281, 9.947933733124651567, -180.1569129053474683 ) ) ;
#46937 = VERTEX_POINT ( 'NONE', #202683 ) ;
#46936 = DIRECTION ( 'NONE',  ( 0.000000000000000000, 0.2128009952263616722, -0.9770955615653312831 ) ) ;
#46938 = EDGE_CURVE ( 'NONE', #3738, #70370, #113785, .T. ) ;
#46939 = ORIENTED_EDGE ( 'NONE', *, *, #84627, .T. ) ;
#46940 = CARTESIAN_POINT ( 'NONE',  ( -17.11825945287482753, 10.05000000001113847, -79.65000000000004832 ) ) ;
#46941 = ADVANCED_FACE ( 'NONE', ( #143985 ), #7050, .F. ) ;
#46942 = CIRCLE ( 'NONE', #159411, 0.2000000000000005107 ) ;
#46943 = CIRCLE ( 'NONE', #126051, 0.1000000000000028644 ) ;
#46944 = VERTEX_POINT ( 'NONE', #142699 ) ;
#46945 = ORIENTED_EDGE ( 'NONE', *, *, #223149, .T. ) ;
#46946 = DIRECTION ( 'NONE',  ( 0.000000000000000000, -0.8814952561688438326, 0.4721928772777334582 ) ) ;
#46947 = CARTESIAN_POINT ( 'NONE',  ( 22.50000000000000000, 0.1000000000111554016, -59.20922040162665922 ) ) ;
#46949 = ORIENTED_EDGE ( 'NONE', *, *, #113626, .F. ) ;
#46948 = ORIENTED_EDGE ( 'NONE', *, *, #92709, .T. ) ;
#46950 = VERTEX_POINT ( 'NONE', #25362 ) ;
#46951 = CARTESIAN_POINT ( 'NONE',  ( -16.90138253750127006, 9.950000000011138823, -54.21156270790459075 ) ) ;
#46952 = EDGE_LOOP ( 'NONE', ( #220514, #137935, #173632, #164873 ) ) ;
#46953 = VERTEX_POINT ( 'NONE', #42336 ) ;
#46954 = EDGE_CURVE ( 'NONE', #168568, #164082, #138684, .T. ) ;
#46955 = CIRCLE ( 'NONE', #192734, 0.1000000000000054040 ) ;
#46957 = ORIENTED_EDGE ( 'NONE', *, *, #151356, .F. ) ;
#46956 = DIRECTION ( 'NONE',  ( 0.000000000000000000, 0.8814952561688437216, -0.4721928772777331806 ) ) ;
#46958 = EDGE_CURVE ( 'NONE', #219844, #127337, #59586, .T. ) ;
#46959 = DIRECTION ( 'NONE',  ( 0.000000000000000000, 0.000000000000000000, 1.000000000000000000 ) ) ;
#46960 = EDGE_CURVE ( 'NONE', #189027, #64247, #180565, .T. ) ;
#46962 = FACE_OUTER_BOUND ( 'NONE', #89533, .T. ) ;
#46961 = LINE ( 'NONE', #163099, #107225 ) ;
#46963 = CARTESIAN_POINT ( 'NONE',  ( 18.54147908293604985, 85.46326165794067720, -196.4741585877683860 ) ) ;
#46964 = DIRECTION ( 'NONE',  ( 1.000000000000000000, -0.000000000000000000, -0.000000000000000000 ) ) ;
#46965 = VERTEX_POINT ( 'NONE', #244371 ) ;
#46966 = AXIS2_PLACEMENT_3D ( 'NONE', #240914, #2275, #41450 ) ;
#46967 = AXIS2_PLACEMENT_3D ( 'NONE', #181530, #204907, #241491 ) ;
#46968 = ORIENTED_EDGE ( 'NONE', *, *, #236087, .F. ) ;
#46969 = AXIS2_PLACEMENT_3D ( 'NONE', #101462, #181072, #2391 ) ;
#46970 = DIRECTION ( 'NONE',  ( 0.000000000000000000, -1.156482317317873105E-15, -1.000000000000000000 ) ) ;
#46971 = ORIENTED_EDGE ( 'NONE', *, *, #102616, .F. ) ;
#46972 = CARTESIAN_POINT ( 'NONE',  ( -20.90000000000000213, 11.49641995933507843, -1.885425182446133885 ) ) ;
#46973 = ORIENTED_EDGE ( 'NONE', *, *, #36191, .F. ) ;
#46974 = ORIENTED_EDGE ( 'NONE', *, *, #221940, .F. ) ;
#46975 = CARTESIAN_POINT ( 'NONE',  ( -21.05000000000000071, 64.25000000001264766, -196.7392418215463010 ) ) ;
#46976 = CARTESIAN_POINT ( 'NONE',  ( -20.15000000000000568, 9.291421356237307805, -12.25000000000000000 ) ) ;
#46977 = EDGE_LOOP ( 'NONE', ( #120103, #178935, #103550, #126756 ) ) ;
#46978 = CARTESIAN_POINT ( 'NONE',  ( 21.72449340488910252, 10.28395627750227703, -79.65000000000004832 ) ) ;
#46979 = CARTESIAN_POINT ( 'NONE',  ( -18.50000000000000000, 85.40000000001191438, -95.72584772486095517 ) ) ;
#46980 = ORIENTED_EDGE ( 'NONE', *, *, #184480, .F. ) ;
#46981 = CARTESIAN_POINT ( 'NONE',  ( 19.83283456528359423, 64.25000000001220712, -145.1731074851066410 ) ) ;
#46982 = CARTESIAN_POINT ( 'NONE',  ( 20.94999999999999929, 87.48912529308822172, -139.6231074845242688 ) ) ;
#46984 = CARTESIAN_POINT ( 'NONE',  ( 23.24999999999999289, 70.05000000001251692, -180.3288097895592159 ) ) ;
#46983 = FACE_OUTER_BOUND ( 'NONE', #120728, .T. ) ;
#46985 = DIRECTION ( 'NONE',  ( 0.000000000000000000, 6.982962677686266711E-15, -1.000000000000000000 ) ) ;
#46986 = LINE ( 'NONE', #82247, #41023 ) ;
#46987 = CARTESIAN_POINT ( 'NONE',  ( -18.59999999999999787, 77.16270174995034381, -161.9231074845243370 ) ) ;
#46988 = ADVANCED_FACE ( 'NONE', ( #100966 ), #223518, .T. ) ;
#46989 = CARTESIAN_POINT ( 'NONE',  ( 23.14999999999999503, 64.35000000001178933, -81.67310748452439384 ) ) ;
#46990 = VECTOR ( 'NONE', #61620, 1000.000000000000114 ) ;
#46991 = ORIENTED_EDGE ( 'NONE', *, *, #248291, .T. ) ;
#46993 = EDGE_LOOP ( 'NONE', ( #21407, #103259, #247104, #193102 ) ) ;
#46992 = VERTEX_POINT ( 'NONE', #201397 ) ;
#46994 = ORIENTED_EDGE ( 'NONE', *, *, #235919, .F. ) ;
#46995 = ADVANCED_FACE ( 'NONE', ( #63163 ), #124450, .F. ) ;
#46996 = LINE ( 'NONE', #228240, #32278 ) ;
#46997 = AXIS2_PLACEMENT_3D ( 'NONE', #246776, #88978, #225905 ) ;
#46998 = FACE_OUTER_BOUND ( 'NONE', #215751, .T. ) ;
#47000 = CARTESIAN_POINT ( 'NONE',  ( -20.94999999999999929, 11.64999999999999680, -33.50000000000000000 ) ) ;
#46999 = FACE_OUTER_BOUND ( 'NONE', #195833, .T. ) ;
#47001 = DIRECTION ( 'NONE',  ( 0.000000000000000000, -0.9126074666063757057, -0.4088369013363309379 ) ) ;
#47002 = VERTEX_POINT ( 'NONE', #3183 ) ;
#47003 = VECTOR ( 'NONE', #91363, 1000.000000000000000 ) ;
#47004 = EDGE_CURVE ( 'NONE', #218009, #97734, #126256, .T. ) ;
#47005 = DIRECTION ( 'NONE',  ( -3.265361837132813093E-16, 1.000000000000000000, 0.000000000000000000 ) ) ;
#47006 = VECTOR ( 'NONE', #136358, 1000.000000000000000 ) ;
#47007 = DIRECTION ( 'NONE',  ( 0.000000000000000000, 0.9126074666063660468, 0.4088369013363524762 ) ) ;
#47008 = AXIS2_PLACEMENT_3D ( 'NONE', #238426, #18086, #59756 ) ;
#47009 = ADVANCED_FACE ( 'NONE', ( #125715 ), #47125, .T. ) ;
#47010 = AXIS2_PLACEMENT_3D ( 'NONE', #247424, #227870, #148334 ) ;
#47011 = DIRECTION ( 'NONE',  ( -1.000000000000000000, 0.000000000000000000, 0.000000000000000000 ) ) ;
#47012 = EDGE_LOOP ( 'NONE', ( #29974, #214878, #230422, #229886 ) ) ;
#47013 = TOROIDAL_SURFACE ( 'NONE', #246936, 0.2000000000000000111, 0.1000000000000000056 ) ;
#47014 = EDGE_CURVE ( 'NONE', #205943, #221081, #180427, .T. ) ;
#47015 = FACE_OUTER_BOUND ( 'NONE', #209224, .T. ) ;
#47016 = EDGE_CURVE ( 'NONE', #249207, #102678, #213739, .T. ) ;
#47017 = VERTEX_POINT ( 'NONE', #111304 ) ;
#47018 = ORIENTED_EDGE ( 'NONE', *, *, #58403, .F. ) ;
#47019 = CARTESIAN_POINT ( 'NONE',  ( -18.35235881385853318, 64.52658099229898880, -93.77310748452438816 ) ) ;
#47020 = CARTESIAN_POINT ( 'NONE',  ( 18.59999999999999787, 1.866714910068465239, -179.2526752462819672 ) ) ;
#47021 = DIRECTION ( 'NONE',  ( 1.000000000000000000, 0.000000000000000000, 0.000000000000000000 ) ) ;
#47022 = CARTESIAN_POINT ( 'NONE',  ( 22.39999999999999503, 64.35000000001237197, -169.9231074845244507 ) ) ;
#47023 = CARTESIAN_POINT ( 'NONE',  ( 20.90000000000000213, 1.899104650876408451, -11.59795743183152972 ) ) ;
#47025 = TOROIDAL_SURFACE ( 'NONE', #84397, 0.2000000000000000111, 0.1000000000000000056 ) ;
#47024 = FACE_OUTER_BOUND ( 'NONE', #131296, .T. ) ;
#47026 = ORIENTED_EDGE ( 'NONE', *, *, #123725, .T. ) ;
#47027 = DIRECTION ( 'NONE',  ( -1.000000000000000000, -0.000000000000000000, -0.000000000000000000 ) ) ;
#47028 = CARTESIAN_POINT ( 'NONE',  ( -22.39999999999999858, 29.50811709945089945, -252.6450601445781103 ) ) ;
#47029 = CIRCLE ( 'NONE', #180324, 0.09999999999999939493 ) ;
#47031 = DIRECTION ( 'NONE',  ( -0.000000000000000000, -6.982962677686266711E-15, 1.000000000000000000 ) ) ;
#47030 = CARTESIAN_POINT ( 'NONE',  ( -16.93234230245721861, 9.998107370558241058, -87.91769028166629596 ) ) ;
#47032 = CARTESIAN_POINT ( 'NONE',  ( -0.8999999999999437339, 64.35000000001120668, -7.423107484524793520 ) ) ;
#47033 = CARTESIAN_POINT ( 'NONE',  ( 22.48660254037844197, 64.35000000001213039, -136.5731074845243995 ) ) ;
#47034 = AXIS2_PLACEMENT_3D ( 'NONE', #24176, #4577, #5862 ) ;
#47035 = CARTESIAN_POINT ( 'NONE',  ( 23.24999999999997513, 11.65000000001116298, -160.4851942293460638 ) ) ;
#47036 = DIRECTION ( 'NONE',  ( 1.000000000000000000, 2.952720810173289112E-16, -0.000000000000000000 ) ) ;
#47038 = ORIENTED_EDGE ( 'NONE', *, *, #149215, .F. ) ;
#47037 = CARTESIAN_POINT ( 'NONE',  ( 21.53699400388664031, 30.46440795807615132, -252.3262297578936568 ) ) ;
#47039 = EDGE_CURVE ( 'NONE', #216685, #25616, #130855, .T. ) ;
#47040 = EDGE_CURVE ( 'NONE', #50465, #163390, #72189, .T. ) ;
#47041 = CIRCLE ( 'NONE', #105270, 0.1000000000000032391 ) ;
#47042 = CIRCLE ( 'NONE', #163588, 0.1000000000000060424 ) ;
#47043 = CIRCLE ( 'NONE', #134518, 1.900000000000005906 ) ;
#47044 = ADVANCED_FACE ( 'NONE', ( #48743 ), #50033, .T. ) ;
#47045 = LINE ( 'NONE', #107023, #20945 ) ;
#47046 = EDGE_CURVE ( 'NONE', #197646, #63374, #30496, .T. ) ;
#47047 = DIRECTION ( 'NONE',  ( -0.7071067811865474617, 0.6824534298470372740, -0.1850873201762209819 ) ) ;
#47048 = EDGE_CURVE ( 'NONE', #50040, #40157, #51391, .T. ) ;
#47049 = CARTESIAN_POINT ( 'NONE',  ( 14.56326696814970489, 9.446648990640015953, -149.0891632959232140 ) ) ;
#47050 = VERTEX_POINT ( 'NONE', #147868 ) ;
#47051 = AXIS2_PLACEMENT_3D ( 'NONE', #11264, #170385, #227727 ) ;
#47052 = CIRCLE ( 'NONE', #88744, 0.1000000000000090677 ) ;
#47054 = DIRECTION ( 'NONE',  ( 1.000000000000000000, 0.000000000000000000, 0.000000000000000000 ) ) ;
#47053 = CIRCLE ( 'NONE', #88745, 0.1000000000000028644 ) ;
#47055 = CARTESIAN_POINT ( 'NONE',  ( -20.64999999999999858, 68.85000000001200249, -115.3731074845243540 ) ) ;
#47056 = DIRECTION ( 'NONE',  ( 0.000000000000000000, 0.000000000000000000, -1.000000000000000000 ) ) ;
#47057 = ADVANCED_FACE ( 'NONE', ( #70919 ), #150741, .F. ) ;
#47058 = ORIENTED_EDGE ( 'NONE', *, *, #68582, .F. ) ;
#47059 = DIRECTION ( 'NONE',  ( 1.000000000000000000, 0.000000000000000000, 0.000000000000000000 ) ) ;
#47061 = ORIENTED_EDGE ( 'NONE', *, *, #177419, .F. ) ;
#47060 = DIRECTION ( 'NONE',  ( 0.000000000000000000, 0.5341055959866798375, -0.8454177738465836756 ) ) ;
#47063 = CARTESIAN_POINT ( 'NONE',  ( 21.05000000000000071, 45.73145985849338047, -239.4600911154851133 ) ) ;
#47062 = CARTESIAN_POINT ( 'NONE',  ( 21.05000000000000071, 71.93512633425886804, -225.1442869522136334 ) ) ;
#47064 =( BOUNDED_CURVE ( )  B_SPLINE_CURVE ( 3, ( #241397, #1478, #61464, #146128 ),
 .UNSPECIFIED., .F., .F. ) 
 B_SPLINE_CURVE_WITH_KNOTS ( ( 4, 4 ),
 ( 4.712388980384690562, 5.672655318024762749 ),
 .UNSPECIFIED. ) 
 CURVE ( )  GEOMETRIC_REPRESENTATION_ITEM ( )  RATIONAL_B_SPLINE_CURVE ( ( 1.000000000000000000, 0.9246222802177245237, 0.9246222802177245237, 1.000000000000000000 ) ) 
 REPRESENTATION_ITEM ( '' )  );
#47065 = DIRECTION ( 'NONE',  ( 0.000000000000000000, 0.8700118002898393765, -0.4930308989875104575 ) ) ;
#47066 = VERTEX_POINT ( 'NONE', #227384 ) ;
#47067 = CARTESIAN_POINT ( 'NONE',  ( -16.87683809663752399, 66.15000000001262492, -190.1207434663279514 ) ) ;
#47068 = ADVANCED_FACE ( 'NONE', ( #128304 ), #84711, .T. ) ;
#47069 = CARTESIAN_POINT ( 'NONE',  ( 0.000000000000000000, 0.000000000000000000, 0.000000000000000000 ) ) ;
#47070 = CARTESIAN_POINT ( 'NONE',  ( -21.05000000000000426, 69.74168394268011184, -136.5888090948464821 ) ) ;
#47071 = CARTESIAN_POINT ( 'NONE',  ( -20.54999999999999716, 2.500000000011156409, -147.2246219227621111 ) ) ;
#47072 = DIRECTION ( 'NONE',  ( 0.000000000000000000, -0.8660254037844411501, -0.4999999999999956146 ) ) ;
#47073 = ORIENTED_EDGE ( 'NONE', *, *, #34460, .F. ) ;
#47074 = CARTESIAN_POINT ( 'NONE',  ( -18.59999999999999787, 76.00000000001213607, -136.5231074845242745 ) ) ;
#47075 = FACE_OUTER_BOUND ( 'NONE', #161163, .T. ) ;
#47076 = CARTESIAN_POINT ( 'NONE',  ( -18.50000000000000000, 52.81534179157634412, -244.1198638051726277 ) ) ;
#47077 = CIRCLE ( 'NONE', #67943, 7.900000000000003908 ) ;
#47078 = CARTESIAN_POINT ( 'NONE',  ( 22.50000000000000000, 31.80488924422933295, -238.9605610896540213 ) ) ;
#47079 = ORIENTED_EDGE ( 'NONE', *, *, #17112, .F. ) ;
#47080 = ORIENTED_EDGE ( 'NONE', *, *, #151635, .T. ) ;
#47081 = DIRECTION ( 'NONE',  ( 0.000000000000000000, 0.2617529984165152257, 0.9651348961777124202 ) ) ;
#47082 = DIRECTION ( 'NONE',  ( 0.000000000000000000, -6.454785026890406770E-15, 1.000000000000000000 ) ) ;
#47083 = CARTESIAN_POINT ( 'NONE',  ( 21.07888907270776002, 13.08009968415031210, -210.6589686082192827 ) ) ;
#47084 = DIRECTION ( 'NONE',  ( 0.000000000000000000, 0.4999999999999543698, 0.8660254037844650199 ) ) ;
#47086 = DIRECTION ( 'NONE',  ( 1.000000000000000000, -0.000000000000000000, -0.000000000000000000 ) ) ;
#47085 = DIRECTION ( 'NONE',  ( 1.000000000000000000, 0.000000000000000000, 0.000000000000000000 ) ) ;
#47087 = CARTESIAN_POINT ( 'NONE',  ( -22.50000000000000000, 1.115600667400684642E-11, -55.35042919245524473 ) ) ;
#47088 = LINE ( 'NONE', #187921, #210146 ) ;
#47089 = CARTESIAN_POINT ( 'NONE',  ( -18.59999999999999787, 9.350000000011156942, -179.6499999999999773 ) ) ;
#47090 = DIRECTION ( 'NONE',  ( -1.000000000000000000, 2.952720810173289112E-16, 2.061873921506763405E-30 ) ) ;
#47091 = AXIS2_PLACEMENT_3D ( 'NONE', #21192, #86235, #42023 ) ;
#47093 = ORIENTED_EDGE ( 'NONE', *, *, #216367, .T. ) ;
#47092 = CARTESIAN_POINT ( 'NONE',  ( 14.88075390448863722, 62.91308081279556319, -215.7443727990306002 ) ) ;
#47094 = DIRECTION ( 'NONE',  ( 0.000000000000000000, 0.1335171055202901413, -0.9910465087640860649 ) ) ;
#47095 = CARTESIAN_POINT ( 'NONE',  ( 21.97500000000000497, 9.750000000011153745, -188.6499999999999488 ) ) ;
#47097 = DIRECTION ( 'NONE',  ( 0.000000000000000000, 0.000000000000000000, -1.000000000000000000 ) ) ;
#47096 = DIRECTION ( 'NONE',  ( 1.000000000000000000, 0.000000000000000000, 0.000000000000000000 ) ) ;
#47098 = EDGE_CURVE ( 'NONE', #38095, #194263, #59773, .T. ) ;
#47099 = ORIENTED_EDGE ( 'NONE', *, *, #97856, .T. ) ;
#47100 = CARTESIAN_POINT ( 'NONE',  ( 21.15000000000005187, 74.94272479589878344, -8.023107484524793165 ) ) ;
#47101 = CARTESIAN_POINT ( 'NONE',  ( -20.54999999999999716, 71.65000000001259650, -191.1731074845243654 ) ) ;
#47102 = DIRECTION ( 'NONE',  ( -1.000000000000000000, -0.000000000000000000, -0.000000000000000000 ) ) ;
#47103 = FACE_OUTER_BOUND ( 'NONE', #161036, .T. ) ;
#47104 = DIRECTION ( 'NONE',  ( 1.000000000000000000, 0.000000000000000000, 0.000000000000000000 ) ) ;
#47105 = ORIENTED_EDGE ( 'NONE', *, *, #45558, .F. ) ;
#47106 = ORIENTED_EDGE ( 'NONE', *, *, #56128, .F. ) ;
#47108 = AXIS2_PLACEMENT_3D ( 'NONE', #16045, #134651, #91702 ) ;
#47107 = LINE ( 'NONE', #27610, #1181 ) ;
#47109 = ORIENTED_EDGE ( 'NONE', *, *, #135821, .T. ) ;
#47110 = ADVANCED_FACE ( 'NONE', ( #108728 ), #90433, .F. ) ;
#47111 = CARTESIAN_POINT ( 'NONE',  ( -21.05000000000000071, -1.835341550213255957, -179.1551512925629197 ) ) ;
#47112 = ORIENTED_EDGE ( 'NONE', *, *, #102913, .F. ) ;
#47113 = AXIS2_PLACEMENT_3D ( 'NONE', #72546, #210752, #149521 ) ;
#47114 = DIRECTION ( 'NONE',  ( 0.000000000000000000, 0.000000000000000000, -1.000000000000000000 ) ) ;
#47115 = CARTESIAN_POINT ( 'NONE',  ( 22.60000000000000142, 36.65892442174472876, -249.5511627012454596 ) ) ;
#47116 = VERTEX_POINT ( 'NONE', #187005 ) ;
#47117 = B_SPLINE_CURVE_WITH_KNOTS ( 'NONE', 3,
 ( #8774, #85695, #88272, #68752, #146975, #208270, #105258, #248663, #244801, #25766, #226505, #6191, #148282, #47880, #227807, #124871, #49175, #45327, #27084, #29651, #109137, #44049, #184828, #169162, #123586, #66175, #145697, #164002, #106562, #203114 ),
 .UNSPECIFIED., .F., .F.,
 ( 4, 2, 2, 2, 2, 2, 2, 2, 2, 2, 2, 2, 2, 2, 4 ),
 ( 0.000000000000000000, 0.0003422764154113331811, 0.0006845528308226663623, 0.001026829246233999489, 0.001369105661645332725, 0.002053658492468004183, 0.002738211323290676291, 0.003080487738702012129, 0.003422764154113347532, 0.003765040569524683370, 0.004107316984936018774, 0.004449593400347354177, 0.004791869815758689581, 0.005134146231170025852, 0.005476422646581361256 ),
 .UNSPECIFIED. ) ;
#47118 = DIRECTION ( 'NONE',  ( 0.000000000000000000, 0.000000000000000000, 1.000000000000000000 ) ) ;
#47119 = LINE ( 'NONE', #244053, #196650 ) ;
#47120 = CARTESIAN_POINT ( 'NONE',  ( -18.50000000000000000, 5.341242990002803559, -23.69334979351197745 ) ) ;
#47121 = CIRCLE ( 'NONE', #55298, 0.1000000000000019901 ) ;
#47122 = LINE ( 'NONE', #169710, #158245 ) ;
#47123 = CARTESIAN_POINT ( 'NONE',  ( -23.25000000000000000, 77.16412189325330928, -128.6082593989527254 ) ) ;
#47125 = TOROIDAL_SURFACE ( 'NONE', #34700, 11.65000000000000036, 0.1000000000000000056 ) ;
#47124 = DIRECTION ( 'NONE',  ( -1.000000000000000000, 0.000000000000000000, 0.000000000000000000 ) ) ;
#47126 = B_SPLINE_CURVE_WITH_KNOTS ( 'NONE', 3,
 ( #247668, #166887, #31236, #190277, #11646, #32514, #250236, #91160, #71617, #87294 ),
 .UNSPECIFIED., .F., .F.,
 ( 4, 2, 2, 2, 4 ),
 ( 0.000000000000000000, 4.221631689686801018E-05, 8.443263379373602037E-05, 0.0001688652675874720407, 0.0003377305351749303663 ),
 .UNSPECIFIED. ) ;
#47127 = FACE_OUTER_BOUND ( 'NONE', #10642, .T. ) ;
#47128 = ORIENTED_EDGE ( 'NONE', *, *, #88420, .F. ) ;
#47130 = DIRECTION ( 'NONE',  ( 1.000000000000000000, 0.000000000000000000, 0.000000000000000000 ) ) ;
#47129 = LINE ( 'NONE', #144954, #32749 ) ;
#47131 = ORIENTED_EDGE ( 'NONE', *, *, #229262, .T. ) ;
#47133 = VERTEX_POINT ( 'NONE', #226073 ) ;
#47132 = CARTESIAN_POINT ( 'NONE',  ( 20.85000000000000142, 76.00000000001126921, -203.5231074845248997 ) ) ;
#47134 = ORIENTED_EDGE ( 'NONE', *, *, #188159, .T. ) ;
#47135 = DIRECTION ( 'NONE',  ( 0.000000000000000000, 0.000000000000000000, 1.000000000000000000 ) ) ;
#47136 = CARTESIAN_POINT ( 'NONE',  ( 18.50211644919734866, 10.30207779525984790, -72.48955207167824710 ) ) ;
#47137 = DIRECTION ( 'NONE',  ( 0.000000000000000000, 0.000000000000000000, 1.000000000000000000 ) ) ;
#47138 = CIRCLE ( 'NONE', #209661, 0.1999999999999929334 ) ;
#47139 = CARTESIAN_POINT ( 'NONE',  ( -20.65000000000000568, 7.250000000011138646, -154.8500000000000227 ) ) ;
#47140 = VERTEX_POINT ( 'NONE', #67035 ) ;
#47141 = CARTESIAN_POINT ( 'NONE',  ( -18.59999999999999787, 11.60000000001115872, -73.92820323027559937 ) ) ;
#47142 = FACE_BOUND ( 'NONE', #70018, .T. ) ;
#47143 = CIRCLE ( 'NONE', #151237, 0.1000000000000028644 ) ;
#47144 = ORIENTED_EDGE ( 'NONE', *, *, #202580, .F. ) ;
#47145 = CIRCLE ( 'NONE', #88653, 0.2000000000000057288 ) ;
#47147 = EDGE_CURVE ( 'NONE', #13016, #256646, #234585, .T. ) ;
#47146 = CIRCLE ( 'NONE', #192926, 0.1000000000000017680 ) ;
#47148 = DIRECTION ( 'NONE',  ( 2.952720810173289112E-16, -1.000000000000000000, 0.000000000000000000 ) ) ;
#47149 = AXIS2_PLACEMENT_3D ( 'NONE', #29492, #149423, #249785 ) ;
#47150 = EDGE_CURVE ( 'NONE', #50249, #9758, #126445, .T. ) ;
#47151 = CARTESIAN_POINT ( 'NONE',  ( -18.50000000000000000, 42.96960653111219131, -254.4772109693542745 ) ) ;
#47152 = ORIENTED_EDGE ( 'NONE', *, *, #239956, .T. ) ;
#47153 = CARTESIAN_POINT ( 'NONE',  ( -16.82055514392377304, 9.950000000011137047, -146.6767980745422619 ) ) ;
#47154 = ORIENTED_EDGE ( 'NONE', *, *, #240732, .F. ) ;
#47155 = DIRECTION ( 'NONE',  ( 0.000000000000000000, 0.000000000000000000, 1.000000000000000000 ) ) ;
#47156 = VERTEX_POINT ( 'NONE', #209107 ) ;
#47157 = FACE_OUTER_BOUND ( 'NONE', #104120, .T. ) ;
#47158 =( BOUNDED_SURFACE ( )  B_SPLINE_SURFACE ( 3, 2, ( 
 ( #215457, #98046, #36864 ),
 ( #74715, #116377, #195921 ),
 ( #177655, #158106, #43249 ),
 ( #141070, #118948, #202317 ),
 ( #64091, #143621, #201035 ),
 ( #124082, #223151, #256 ) ),
 .UNSPECIFIED., .F., .F., .T. ) 
 B_SPLINE_SURFACE_WITH_KNOTS ( ( 4, 2, 4 ),
 ( 3, 3 ),
 ( 3.141592653589804662, 3.926990816987256494, 4.712388980384708326 ),
 ( 0.000000000000000000, 1.000000000000000000 ),
 .UNSPECIFIED. ) 
 GEOMETRIC_REPRESENTATION_ITEM ( )  RATIONAL_B_SPLINE_SURFACE ( (
 ( 1.000000000000000000, 0.9238795325113159373, 1.000000000000000000),
 ( 1.000000000000000000, 0.9240297172245346413, 1.000000000000000000),
 ( 1.000000000000000000, 0.9038128468036756846, 1.000000000000000000),
 ( 1.000000000000000000, 0.8282379607651599862, 1.000000000000000000),
 ( 1.000000000000000000, 0.7727932973488951252, 1.000000000000000000),
 ( 1.000000000000000000, 0.7071067811865977548, 1.000000000000000000) ) ) 
 REPRESENTATION_ITEM ( '' )  SURFACE ( )  );
#47159 = EDGE_CURVE ( 'NONE', #238735, #24864, #55672, .T. ) ;
#47160 = DIRECTION ( 'NONE',  ( 1.000000000000000000, -0.000000000000000000, -0.000000000000000000 ) ) ;
#47161 = DIRECTION ( 'NONE',  ( -1.000000000000000000, 0.000000000000000000, 0.000000000000000000 ) ) ;
#47162 = EDGE_CURVE ( 'NONE', #99108, #86349, #97166, .T. ) ;
#47163 = CARTESIAN_POINT ( 'NONE',  ( 18.59999999999999432, 77.86671491006991630, -191.7704322382423356 ) ) ;
#47164 = CIRCLE ( 'NONE', #222122, 0.1000000000000033223 ) ;
#47165 = AXIS2_PLACEMENT_3D ( 'NONE', #56311, #249405, #13359 ) ;
#47166 = EDGE_CURVE ( 'NONE', #197693, #131787, #255378, .T. ) ;
#47167 = DIRECTION ( 'NONE',  ( 1.000000000000000000, 0.000000000000000000, 0.000000000000000000 ) ) ;
#47168 = DIRECTION ( 'NONE',  ( 0.000000000000000000, 0.4583618696494374256, 0.8887656589064814039 ) ) ;
#47169 = DIRECTION ( 'NONE',  ( 1.000000000000000000, 0.000000000000000000, 0.000000000000000000 ) ) ;
#47170 = ORIENTED_EDGE ( 'NONE', *, *, #36347, .F. ) ;
#47172 = CARTESIAN_POINT ( 'NONE',  ( -23.15000000000000213, -6.688413578037177842, -212.5825622730469036 ) ) ;
#47171 = DIRECTION ( 'NONE',  ( -0.000000000000000000, -1.265107689135680095E-16, 1.000000000000000000 ) ) ;
#47173 = EDGE_LOOP ( 'NONE', ( #63670, #217434, #99283, #227176 ) ) ;
#47174 = DIRECTION ( 'NONE',  ( 0.000000000000000000, 0.000000000000000000, 1.000000000000000000 ) ) ;
#47175 = CIRCLE ( 'NONE', #197023, 11.70000000000001528 ) ;
#47177 = B_SPLINE_CURVE_WITH_KNOTS ( 'NONE', 3,
 ( #255080, #174371, #251276, #71392 ),
 .UNSPECIFIED., .F., .F.,
 ( 4, 4 ),
 ( 0.000000000000000000, 7.713889350927705709E-05 ),
 .UNSPECIFIED. ) ;
#47176 = CARTESIAN_POINT ( 'NONE',  ( 23.24999999999999289, 6.450000000011156587, -55.25000000000004974 ) ) ;
#47178 = DIRECTION ( 'NONE',  ( -1.000000000000000000, -0.000000000000000000, -0.000000000000000000 ) ) ;
#47179 = VECTOR ( 'NONE', #18450, 1000.000000000000000 ) ;
#47181 = VERTEX_POINT ( 'NONE', #156876 ) ;
#47180 = CARTESIAN_POINT ( 'NONE',  ( -18.40000000000000213, -9.499999999988936850, -207.9221498493300828 ) ) ;
#47183 = ORIENTED_EDGE ( 'NONE', *, *, #52260, .F. ) ;
#47182 = PLANE ( 'NONE',  #70475 ) ;
#47184 = EDGE_CURVE ( 'NONE', #211780, #217631, #50911, .T. ) ;
#47185 = DIRECTION ( 'NONE',  ( 1.000000000000000000, 0.000000000000000000, 0.000000000000000000 ) ) ;
#47186 = CIRCLE ( 'NONE', #218057, 0.09999999999999693856 ) ;
#47188 = EDGE_LOOP ( 'NONE', ( #135178, #84263, #135071, #97048 ) ) ;
#47187 = CARTESIAN_POINT ( 'NONE',  ( 18.39999999999999503, 11.75000000001113953, -91.25000000000005684 ) ) ;
#47189 = AXIS2_PLACEMENT_3D ( 'NONE', #124247, #126799, #165953 ) ;
#47190 = CIRCLE ( 'NONE', #51275, 11.90000000000000746 ) ;
#47191 = CIRCLE ( 'NONE', #205402, 7.899999999999995914 ) ;
#47192 = AXIS2_PLACEMENT_3D ( 'NONE', #86715, #146687, #129721 ) ;
#47193 = PRODUCT_DEFINITION_SHAPE ( 'NONE', 'NONE',  #168000 ) ;
#47194 = AXIS2_PLACEMENT_3D ( 'NONE', #255955, #117782, #76085 ) ;
#47195 = DIRECTION ( 'NONE',  ( 0.000000000000000000, 0.000000000000000000, -1.000000000000000000 ) ) ;
#47196 = LINE ( 'NONE', #180635, #172113 ) ;
#47197 = ORIENTED_EDGE ( 'NONE', *, *, #164266, .T. ) ;
#47198 = CYLINDRICAL_SURFACE ( 'NONE', #234954, 12.87499999999999467 ) ;
#47199 = ORIENTED_EDGE ( 'NONE', *, *, #142546, .F. ) ;
#47200 = DIRECTION ( 'NONE',  ( 1.000000000000000000, -0.000000000000000000, -0.000000000000000000 ) ) ;
#47201 = LINE ( 'NONE', #105884, #18260 ) ;
#47202 = AXIS2_PLACEMENT_3D ( 'NONE', #31701, #211599, #188183 ) ;
#47203 = VERTEX_POINT ( 'NONE', #216806 ) ;
#47204 = CARTESIAN_POINT ( 'NONE',  ( 22.57320508075687115, 11.75000000001115552, -67.00000000000004263 ) ) ;
#47205 = EDGE_CURVE ( 'NONE', #150331, #222218, #14039, .T. ) ;
#47206 = CIRCLE ( 'NONE', #88721, 0.09999999999999939493 ) ;
#47207 = CARTESIAN_POINT ( 'NONE',  ( 23.50000000000005684, 76.00000000001119815, -36.02310748452479316 ) ) ;
#47208 = AXIS2_PLACEMENT_3D ( 'NONE', #180050, #19700, #99195 ) ;
#47209 = VERTEX_POINT ( 'NONE', #253370 ) ;
#47210 = DIRECTION ( 'NONE',  ( 0.000000000000000000, -0.8814952561688441657, 0.4721928772777327366 ) ) ;
#47211 = VECTOR ( 'NONE', #16506, 1000.000000000000000 ) ;
#47212 = AXIS2_PLACEMENT_3D ( 'NONE', #34982, #94899, #253969 ) ;
#47213 = CIRCLE ( 'NONE', #147199, 0.09999999999999939493 ) ;
#47214 = EDGE_CURVE ( 'NONE', #111790, #162078, #18619, .T. ) ;
#47215 = ORIENTED_EDGE ( 'NONE', *, *, #175980, .T. ) ;
#47216 = AXIS2_PLACEMENT_3D ( 'NONE', #175738, #179580, #38775 ) ;
#47217 = EDGE_LOOP ( 'NONE', ( #170117, #173078, #148880, #26466 ) ) ;
#47218 = CARTESIAN_POINT ( 'NONE',  ( -18.31572283045152361, -9.548437830874650700, -73.85062565105830856 ) ) ;
#47219 = ORIENTED_EDGE ( 'NONE', *, *, #100621, .T. ) ;
#47220 = CARTESIAN_POINT ( 'NONE',  ( 20.85000000000000142, 77.75000000001206502, -124.9041574459021007 ) ) ;
#47221 = ORIENTED_EDGE ( 'NONE', *, *, #84259, .F. ) ;
#47223 = VERTEX_POINT ( 'NONE', #98117 ) ;
#47222 = CARTESIAN_POINT ( 'NONE',  ( 23.14999999999999858, 5.600000000011153389, -79.40526601891313874 ) ) ;
#47224 = EDGE_CURVE ( 'NONE', #239420, #202942, #222083, .T. ) ;
#47225 = CARTESIAN_POINT ( 'NONE',  ( -21.05000000000000071, 11.65000000001115055, -73.78386566297820082 ) ) ;
#47226 = VERTEX_POINT ( 'NONE', #56442 ) ;
#47227 = CARTESIAN_POINT ( 'NONE',  ( -20.85000000000000142, 8.809961202382808665, -241.4517562488062481 ) ) ;
#47228 = ORIENTED_EDGE ( 'NONE', *, *, #58117, .F. ) ;
#47230 = ORIENTED_EDGE ( 'NONE', *, *, #107891, .F. ) ;
#47229 = EDGE_LOOP ( 'NONE', ( #238607, #174008, #158280 ) ) ;
#47231 = DIRECTION ( 'NONE',  ( 0.000000000000000000, -1.000000000000000000, 0.000000000000000000 ) ) ;
#47232 = EDGE_CURVE ( 'NONE', #208826, #80974, #230511, .T. ) ;
#47233 = DIRECTION ( 'NONE',  ( -0.000000000000000000, -0.9651348961777157509, 0.2617529984165031243 ) ) ;
#47235 = ORIENTED_EDGE ( 'NONE', *, *, #186030, .F. ) ;
#47234 = AXIS2_PLACEMENT_3D ( 'NONE', #1002, #238362, #38906 ) ;
#47236 = CIRCLE ( 'NONE', #80542, 0.1000000000000001860 ) ;
#47237 = VERTEX_POINT ( 'NONE', #34356 ) ;
#47238 = DIRECTION ( 'NONE',  ( 0.000000000000000000, 0.000000000000000000, -1.000000000000000000 ) ) ;
#47239 = SPHERICAL_SURFACE ( 'NONE', #126502, 0.1000000000000000056 ) ;
#47240 = EDGE_CURVE ( 'NONE', #164247, #167877, #5606, .T. ) ;
#47242 = ORIENTED_EDGE ( 'NONE', *, *, #129349, .T. ) ;
#47241 = CARTESIAN_POINT ( 'NONE',  ( 18.39999999999999147, 8.822561741677553471, -76.25000000000004263 ) ) ;
#47243 = DIRECTION ( 'NONE',  ( 1.000000000000000000, 0.000000000000000000, 0.000000000000000000 ) ) ;
#47244 = VERTEX_POINT ( 'NONE', #78580 ) ;
#47245 = DIRECTION ( 'NONE',  ( 0.000000000000000000, 0.000000000000000000, -1.000000000000000000 ) ) ;
#47247 = ORIENTED_EDGE ( 'NONE', *, *, #208484, .T. ) ;
#47246 = ADVANCED_FACE ( 'NONE', ( #252086 ), #255889, .F. ) ;
#47248 = EDGE_CURVE ( 'NONE', #121353, #100546, #38974, .T. ) ;
#47249 = DIRECTION ( 'NONE',  ( -0.000000000000000000, -0.000000000000000000, -1.000000000000000000 ) ) ;
#47250 = CARTESIAN_POINT ( 'NONE',  ( 20.73486653747090003, 7.250000000011182166, -87.85000000000003695 ) ) ;
#47251 = ORIENTED_EDGE ( 'NONE', *, *, #39273, .T. ) ;
#47252 = CARTESIAN_POINT ( 'NONE',  ( 20.01093837587850288, 54.44613876119747431, -228.7075138270121215 ) ) ;
#47253 = EDGE_CURVE ( 'NONE', #31313, #62035, #213928, .T. ) ;
#47255 = ORIENTED_EDGE ( 'NONE', *, *, #36906, .F. ) ;
#47254 = ORIENTED_EDGE ( 'NONE', *, *, #71138, .F. ) ;
#47256 = VECTOR ( 'NONE', #91440, 1000.000000000000114 ) ;
#47257 = ORIENTED_EDGE ( 'NONE', *, *, #181829, .F. ) ;
#47258 = FACE_OUTER_BOUND ( 'NONE', #38944, .T. ) ;
#47259 = ORIENTED_EDGE ( 'NONE', *, *, #256556, .F. ) ;
#47260 = CARTESIAN_POINT ( 'NONE',  ( -20.00857864376270001, 66.65000000001150227, -48.37310748452438958 ) ) ;
#47261 = ORIENTED_EDGE ( 'NONE', *, *, #144846, .F. ) ;
#47262 = ADVANCED_FACE ( 'NONE', ( #237668 ), #155600, .T. ) ;
#47263 = DIRECTION ( 'NONE',  ( 0.000000000000000000, -0.2128009952263602012, 0.9770955615653315052 ) ) ;
#47264 = EDGE_CURVE ( 'NONE', #246499, #51208, #101444, .T. ) ;
#47265 = CARTESIAN_POINT ( 'NONE',  ( 20.97224591636398827, 43.49434346882816271, -234.8463466113539653 ) ) ;
#47266 = VERTEX_POINT ( 'NONE', #116444 ) ;
#47267 = VERTEX_POINT ( 'NONE', #119015 ) ;
#47268 = AXIS2_PLACEMENT_3D ( 'NONE', #119700, #47508, #199233 ) ;
#47269 = ORIENTED_EDGE ( 'NONE', *, *, #229809, .F. ) ;
#47270 = AXIS2_PLACEMENT_3D ( 'NONE', #68984, #168107, #31158 ) ;
#47271 = CIRCLE ( 'NONE', #80586, 0.1000000000000048767 ) ;
#47272 = DIRECTION ( 'NONE',  ( -0.000000000000000000, 0.4721928772777347350, 0.8814952561688429444 ) ) ;
#47273 = EDGE_CURVE ( 'NONE', #68442, #203190, #195989, .T. ) ;
#47274 = ORIENTED_EDGE ( 'NONE', *, *, #80399, .T. ) ;
#47275 = EDGE_CURVE ( 'NONE', #79923, #31610, #9723, .T. ) ;
#47277 = ORIENTED_EDGE ( 'NONE', *, *, #79767, .F. ) ;
#47276 = CYLINDRICAL_SURFACE ( 'NONE', #229577, 11.80000000000000426 ) ;
#47278 = DIRECTION ( 'NONE',  ( 0.000000000000000000, 0.000000000000000000, 1.000000000000000000 ) ) ;
#47279 = CARTESIAN_POINT ( 'NONE',  ( -16.93388492042258875, 12.44093641839707054, -211.1852997975874757 ) ) ;
#47280 = CARTESIAN_POINT ( 'NONE',  ( 21.14999999999999858, 64.35000000001204512, -124.2731074845243739 ) ) ;
#47281 = CARTESIAN_POINT ( 'NONE',  ( -18.45068461519106151, 85.48650652910174585, -196.4543303156196146 ) ) ;
#47283 = CARTESIAN_POINT ( 'NONE',  ( 21.00000000000000000, 63.38346053167636995, -212.7939182281409956 ) ) ;
#47282 = DIRECTION ( 'NONE',  ( 0.000000000000000000, -1.000000000000000000, 0.000000000000000000 ) ) ;
#47284 = CARTESIAN_POINT ( 'NONE',  ( -18.59999999999999787, 76.00000000001267608, -203.5231074845243597 ) ) ;
#47285 = CARTESIAN_POINT ( 'NONE',  ( 18.37172112093865195, 38.14850358416990872, -261.2067334498989339 ) ) ;
#47286 = EDGE_CURVE ( 'NONE', #204366, #41069, #198532, .T. ) ;
#47287 = VECTOR ( 'NONE', #125737, 1000.000000000000114 ) ;
#47288 = CARTESIAN_POINT ( 'NONE',  ( -21.59142135623730852, 68.15000000001150227, -48.27310748452437394 ) ) ;
#47289 = AXIS2_PLACEMENT_3D ( 'NONE', #154873, #234367, #111881 ) ;
#47290 = ORIENTED_EDGE ( 'NONE', *, *, #235713, .T. ) ;
#47291 = CIRCLE ( 'NONE', #22398, 0.09999999999999834022 ) ;
#47292 = ORIENTED_EDGE ( 'NONE', *, *, #201184, .F. ) ;
#47294 = ORIENTED_EDGE ( 'NONE', *, *, #160418, .T. ) ;
#47293 = CARTESIAN_POINT ( 'NONE',  ( 20.94999999999999929, 5.000000000011153745, -88.49473398108695221 ) ) ;
#47295 = ORIENTED_EDGE ( 'NONE', *, *, #71953, .F. ) ;
#47296 = CARTESIAN_POINT ( 'NONE',  ( -17.80356949363740426, 65.12326860301199360, -92.73618050875685981 ) ) ;
#47297 = CARTESIAN_POINT ( 'NONE',  ( 20.22483756094572271, 9.501904678881089694, -142.1395391287154837 ) ) ;
#47299 =( NAMED_UNIT ( * ) PLANE_ANGLE_UNIT ( ) SI_UNIT ( $, .RADIAN. ) );
#47298 = CARTESIAN_POINT ( 'NONE',  ( -20.00857864376270001, 52.17883100310857003, -232.4626431718731396 ) ) ;
#47300 = VERTEX_POINT ( 'NONE', #1609 ) ;
#47301 = AXIS2_PLACEMENT_3D ( 'NONE', #255099, #97328, #113084 ) ;
#47302 = ADVANCED_FACE ( 'NONE', ( #242787 ), #44608, .T. ) ;
#47304 = CIRCLE ( 'NONE', #34903, 0.09999999999999344136 ) ;
#47303 =( LENGTH_UNIT ( ) NAMED_UNIT ( * ) SI_UNIT ( .MILLI., .METRE. ) );
#47306 = VECTOR ( 'NONE', #204937, 999.9999999999998863 ) ;
#47305 = CARTESIAN_POINT ( 'NONE',  ( 21.08489247129321242, 67.12232480914150301, -57.17310748452439384 ) ) ;
#47307 = ADVANCED_FACE ( 'NONE', ( #241516 ), #159770, .T. ) ;
#47308 = CARTESIAN_POINT ( 'NONE',  ( 21.05000000000000071, 64.25000000001219291, -143.5379132551784096 ) ) ;
#47309 = ORIENTED_EDGE ( 'NONE', *, *, #73362, .T. ) ;
#47310 = CARTESIAN_POINT ( 'NONE',  ( -13.40000000000000213, -11.75000000000000000, 12.30000000000000426 ) ) ;
#47311 = CARTESIAN_POINT ( 'NONE',  ( -16.78493832629887095, 9.945835743215301505, -180.1639490191041943 ) ) ;
#47312 = CARTESIAN_POINT ( 'NONE',  ( -18.39999999999999858, -11.68510997261236817, -191.5194565067366455 ) ) ;
#47313 = CARTESIAN_POINT ( 'NONE',  ( 21.05000000000000071, 65.51540711881749246, -62.06639391394066507 ) ) ;
#47314 = AXIS2_PLACEMENT_3D ( 'NONE', #63361, #124643, #85467 ) ;
#47315 = EDGE_CURVE ( 'NONE', #162422, #63327, #125430, .T. ) ;
#47316 = DIRECTION ( 'NONE',  ( 0.000000000000000000, -0.4999999999999608646, 0.8660254037844612451 ) ) ;
#47318 = ORIENTED_EDGE ( 'NONE', *, *, #61373, .F. ) ;
#47317 = DIRECTION ( 'NONE',  ( 1.073024830501117725E-15, -6.982962677686266711E-15, 1.000000000000000000 ) ) ;
#47319 = LINE ( 'NONE', #8230, #148628 ) ;
#47320 = LINE ( 'NONE', #224681, #73154 ) ;
#47322 = EDGE_CURVE ( 'NONE', #236908, #3727, #25064, .T. ) ;
#47321 = CARTESIAN_POINT ( 'NONE',  ( -21.14999999999999858, 64.25000000001237765, -169.9231074845244507 ) ) ;
#47323 = AXIS2_PLACEMENT_3D ( 'NONE', #61344, #220430, #80887 ) ;
#47325 = VERTEX_POINT ( 'NONE', #184102 ) ;
#47324 = VECTOR ( 'NONE', #165176, 1000.000000000000227 ) ;
#47326 = CARTESIAN_POINT ( 'NONE',  ( 15.75000000000000000, 66.65000000001185754, -86.15736431725046884 ) ) ;
#47327 = DIRECTION ( 'NONE',  ( -0.7070776581708965169, 0.6824815363281260261, -0.1850949428989399070 ) ) ;
#47328 = AXIS2_PLACEMENT_3D ( 'NONE', #182476, #27270, #44240 ) ;
#47330 = CARTESIAN_POINT ( 'NONE',  ( -16.94445028196808778, 66.00793639031432747, -123.9157773061059231 ) ) ;
#47329 = CARTESIAN_POINT ( 'NONE',  ( -21.05000000000000426, 11.60000000001115872, -107.4282032302755852 ) ) ;
#47332 = ADVANCED_FACE ( 'NONE', ( #121602 ), #193094, .T. ) ;
#47331 = FACE_OUTER_BOUND ( 'NONE', #214288, .T. ) ;
#47333 = CARTESIAN_POINT ( 'NONE',  ( 17.23472005113827876, 65.69211804551081002, -58.06968434459306394 ) ) ;
#47334 = CARTESIAN_POINT ( 'NONE',  ( -18.59999999999999787, 11.74999999999999645, -12.15000000000000036 ) ) ;
#47335 = FACE_OUTER_BOUND ( 'NONE', #8812, .T. ) ;
#47336 = CARTESIAN_POINT ( 'NONE',  ( 18.52130828395272388, 85.48139550263790909, -129.4986007606406133 ) ) ;
#47337 = CARTESIAN_POINT ( 'NONE',  ( -16.77683809663752257, 9.945835743215303282, -87.83605098089584828 ) ) ;
#47338 = ORIENTED_EDGE ( 'NONE', *, *, #160611, .F. ) ;
#47339 = EDGE_CURVE ( 'NONE', #29575, #180641, #226368, .T. ) ;
#47340 = CARTESIAN_POINT ( 'NONE',  ( -20.15000000000000568, 9.291421356237307805, -21.15000000000000213 ) ) ;
#47342 = ADVANCED_FACE ( 'NONE', ( #103262 ), #62875, .T. ) ;
#47341 = EDGE_CURVE ( 'NONE', #15594, #95642, #147292, .T. ) ;
#47343 = ORIENTED_EDGE ( 'NONE', *, *, #5359, .F. ) ;
#47344 = VERTEX_POINT ( 'NONE', #45879 ) ;
#47345 = CARTESIAN_POINT ( 'NONE',  ( 20.30531438145591139, 65.90309893892053594, -95.22708967725128559 ) ) ;
#47346 = CYLINDRICAL_SURFACE ( 'NONE', #61087, 0.09999999999998898659 ) ;
#47347 = ORIENTED_EDGE ( 'NONE', *, *, #110653, .T. ) ;
#47348 = VERTEX_POINT ( 'NONE', #180265 ) ;
#47349 = AXIS2_PLACEMENT_3D ( 'NONE', #106994, #69197, #228256 ) ;
#47350 = VERTEX_POINT ( 'NONE', #84973 ) ;
#47351 = VECTOR ( 'NONE', #10302, 1000.000000000000000 ) ;
#47352 = EDGE_CURVE ( 'NONE', #228403, #46643, #68183, .T. ) ;
#47353 = DIRECTION ( 'NONE',  ( 0.000000000000000000, 1.000000000000000000, 0.000000000000000000 ) ) ;
#47354 = EDGE_CURVE ( 'NONE', #132550, #21996, #247231, .T. ) ;
#47355 = ORIENTED_EDGE ( 'NONE', *, *, #210423, .F. ) ;
#47356 = DIRECTION ( 'NONE',  ( -1.836970198721029934E-16, -1.000000000000000000, -6.982962677686266711E-15 ) ) ;
#47357 = CARTESIAN_POINT ( 'NONE',  ( -16.93262454970419384, 30.29883458234789728, -234.7975840541324430 ) ) ;
#47358 = DIRECTION ( 'NONE',  ( 1.000000000000000000, 0.000000000000000000, 0.000000000000000000 ) ) ;
#47359 = CARTESIAN_POINT ( 'NONE',  ( 20.10000000000000497, 5.454087299794355914, 16.60000000000000142 ) ) ;
#47360 = AXIS2_PLACEMENT_3D ( 'NONE', #66766, #182878, #4204 ) ;
#47361 = ADVANCED_FACE ( 'NONE', ( #65439 ), #207126, .F. ) ;
#47362 = VECTOR ( 'NONE', #76831, 1000.000000000000000 ) ;
#47363 = CARTESIAN_POINT ( 'NONE',  ( 20.85000000000000142, 14.83511725869332132, -235.8887435844146978 ) ) ;
#47364 = CARTESIAN_POINT ( 'NONE',  ( -20.07928932188135107, 66.77928932189394118, -191.1731074845244223 ) ) ;
#47365 = ORIENTED_EDGE ( 'NONE', *, *, #215198, .F. ) ;
#47367 = CARTESIAN_POINT ( 'NONE',  ( -23.25000000000000000, 77.83585931145600512, -158.4186683157258244 ) ) ;
#47366 = DIRECTION ( 'NONE',  ( -1.000000000000000000, 0.000000000000000000, 0.000000000000000000 ) ) ;
#47368 = CARTESIAN_POINT ( 'NONE',  ( 21.05000000000000071, 53.66153320161009788, -235.9075159595686841 ) ) ;
#47369 = EDGE_CURVE ( 'NONE', #167778, #53080, #134793, .T. ) ;
#47370 = ORIENTED_EDGE ( 'NONE', *, *, #85271, .T. ) ;
#47371 = FACE_OUTER_BOUND ( 'NONE', #209935, .T. ) ;
#47372 = AXIS2_PLACEMENT_3D ( 'NONE', #201382, #121862, #80110 ) ;
#47373 = CARTESIAN_POINT ( 'NONE',  ( -15.75000000000001066, 9.350000000011140955, -117.0215193718251072 ) ) ;
#47374 = CARTESIAN_POINT ( 'NONE',  ( 21.05000000000000071, 0.09779029131994770863, -60.74218538952391810 ) ) ;
#47375 = ORIENTED_EDGE ( 'NONE', *, *, #17454, .T. ) ;
#47376 = EDGE_CURVE ( 'NONE', #51883, #90818, #10615, .T. ) ;
#47377 = TOROIDAL_SURFACE ( 'NONE', #126688, 0.2000000000000000111, 0.1000000000000000056 ) ;
#47378 = CARTESIAN_POINT ( 'NONE',  ( 21.07094088545369104, 75.90110629745947790, -75.84327470644146274 ) ) ;
#47379 = AXIS2_PLACEMENT_3D ( 'NONE', #74104, #72816, #153666 ) ;
#47380 = AXIS2_PLACEMENT_3D ( 'NONE', #118866, #219219, #139668 ) ;
#47381 = ORIENTED_EDGE ( 'NONE', *, *, #107381, .T. ) ;
#47382 = CARTESIAN_POINT ( 'NONE',  ( -20.64999999999999858, 71.65000000001199965, -115.2731074845243171 ) ) ;
#47383 = DIRECTION ( 'NONE',  ( 1.000000000000000000, -0.000000000000000000, -0.000000000000000000 ) ) ;
#47384 = DIRECTION ( 'NONE',  ( -3.469446951953635015E-14, 1.000000000000000000, 0.000000000000000000 ) ) ;
#47385 = CARTESIAN_POINT ( 'NONE',  ( -18.59999999999999787, 7.021664781911246322, -171.3335654018973173 ) ) ;
#47386 = ADVANCED_FACE ( 'NONE', ( #50984 ), #168189, .F. ) ;
#47387 = ORIENTED_EDGE ( 'NONE', *, *, #9229, .T. ) ;
#47388 = ADVANCED_FACE ( 'NONE', ( #86264 ), #88832, .F. ) ;
#47389 = AXIS2_PLACEMENT_3D ( 'NONE', #255495, #57323, #116055 ) ;
#47390 = ORIENTED_EDGE ( 'NONE', *, *, #204225, .T. ) ;
#47392 = ADVANCED_FACE ( 'NONE', ( #8052 ), #225778, .F. ) ;
#47391 = CARTESIAN_POINT ( 'NONE',  ( 21.13461538461538680, 67.11458296203740304, -90.67310748452436542 ) ) ;
#47394 = TOROIDAL_SURFACE ( 'NONE', #1618, 0.4000000000000012990, 0.1000000000000000056 ) ;
#47393 = CARTESIAN_POINT ( 'NONE',  ( 18.59999999999999076, 64.35000000001251408, -178.6731074845244507 ) ) ;
#47395 = DIRECTION ( 'NONE',  ( 1.000000000000000000, 3.265361837132813093E-16, -0.000000000000000000 ) ) ;
#47396 = LINE ( 'NONE', #126952, #165446 ) ;
#47397 = CARTESIAN_POINT ( 'NONE',  ( 21.09316766718127667, 6.370153312485570929, -167.4607365976852691 ) ) ;
#47398 = CARTESIAN_POINT ( 'NONE',  ( 22.39999999999999503, 11.75000000001116263, -66.90000000000004832 ) ) ;
#47399 = AXIS2_PLACEMENT_3D ( 'NONE', #108854, #188392, #7173 ) ;
#47400 = ORIENTED_EDGE ( 'NONE', *, *, #40622, .F. ) ;
#47401 = SPHERICAL_SURFACE ( 'NONE', #191013, 0.1000000000000000056 ) ;
#47402 = VECTOR ( 'NONE', #173971, 1000.000000000000000 ) ;
#47404 = VERTEX_POINT ( 'NONE', #168454 ) ;
#47403 = CARTESIAN_POINT ( 'NONE',  ( -20.85000000000000142, 87.65000000001245439, -170.0231074845242745 ) ) ;
#47405 = VECTOR ( 'NONE', #172884, 1000.000000000000000 ) ;
#47406 = CARTESIAN_POINT ( 'NONE',  ( -21.05000000000000071, 6.304961112695785630, -33.52138556593774155 ) ) ;
#47407 = DIRECTION ( 'NONE',  ( 0.000000000000000000, 0.000000000000000000, 1.000000000000000000 ) ) ;
#47408 = DIRECTION ( 'NONE',  ( 1.000000000000000000, 0.000000000000000000, 0.000000000000000000 ) ) ;
#47409 = CARTESIAN_POINT ( 'NONE',  ( -16.88705144915409662, 66.05000000001207638, -123.5921288898118036 ) ) ;
#47410 = EDGE_CURVE ( 'NONE', #211746, #17520, #68010, .T. ) ;
#47412 = ORIENTED_EDGE ( 'NONE', *, *, #59997, .T. ) ;
#47411 = DIRECTION ( 'NONE',  ( 0.000000000000000000, 0.000000000000000000, 1.000000000000000000 ) ) ;
#47413 = FACE_OUTER_BOUND ( 'NONE', #44069, .T. ) ;
#47414 = CARTESIAN_POINT ( 'NONE',  ( 18.49999999999999289, 52.81534179157633702, -244.1198638051726277 ) ) ;
#47415 = CARTESIAN_POINT ( 'NONE',  ( -23.15000000000000213, 8.980461154494397746, -187.0187154576991304 ) ) ;
#47416 = FACE_OUTER_BOUND ( 'NONE', #199726, .T. ) ;
#47417 = ORIENTED_EDGE ( 'NONE', *, *, #172587, .T. ) ;
#47418 = CARTESIAN_POINT ( 'NONE',  ( 18.50000000000000355, -7.664561988343767673, -210.0810037954756524 ) ) ;
#47419 = CARTESIAN_POINT ( 'NONE',  ( -16.87683809663752399, 66.15000000001201386, -116.4254715027206828 ) ) ;
#47420 = CARTESIAN_POINT ( 'NONE',  ( -20.94999999999999929, 1.851028230152016674, -45.15391326942249606 ) ) ;
#47421 = LINE ( 'NONE', #27913, #163335 ) ;
#47423 = ORIENTED_EDGE ( 'NONE', *, *, #2216, .F. ) ;
#47422 = CIRCLE ( 'NONE', #143295, 0.1999999999999987899 ) ;
#47424 = EDGE_CURVE ( 'NONE', #144016, #113568, #11916, .T. ) ;
#47425 = CARTESIAN_POINT ( 'NONE',  ( -16.77308656112214535, 9.950000000011135270, -87.84980680829774258 ) ) ;
#47426 = COLOUR_RGB ( '', 0.31764706, 0.68627451, 0.89019608) ;
#47427 = TOROIDAL_SURFACE ( 'NONE', #59888, 4.099999999999999645, 0.1000000000000000056 ) ;
#47428 = VERTEX_POINT ( 'NONE', #90122 ) ;
#47429 = PLANE ( 'NONE',  #55760 ) ;
#47430 = DIRECTION ( 'NONE',  ( 1.000000000000000000, 0.000000000000000000, 0.000000000000000000 ) ) ;
#47431 =( NAMED_UNIT ( * ) PLANE_ANGLE_UNIT ( ) SI_UNIT ( $, .RADIAN. ) );
#47432 = CARTESIAN_POINT ( 'NONE',  ( -23.15000000000000213, -11.74999999998884448, -167.4999999999999432 ) ) ;
#47433 = ORIENTED_EDGE ( 'NONE', *, *, #211360, .F. ) ;
#47434 = CARTESIAN_POINT ( 'NONE',  ( -20.64999999999999858, 82.09643798151613225, -215.4278993322501208 ) ) ;
#47435 = DIRECTION ( 'NONE',  ( 1.000000000000000000, 0.000000000000000000, 0.000000000000000000 ) ) ;
#47436 = DIRECTION ( 'NONE',  ( 0.000000000000000000, 0.3738317757009345654, 0.9274965247785492695 ) ) ;
#47437 = DIRECTION ( 'NONE',  ( -1.000000000000000000, 0.000000000000000000, 0.000000000000000000 ) ) ;
#47438 = DIRECTION ( 'NONE',  ( 0.000000000000000000, 0.2128009952263237581, -0.9770955615653394988 ) ) ;
#47439 = ORIENTED_EDGE ( 'NONE', *, *, #44350, .T. ) ;
#47441 = EDGE_LOOP ( 'NONE', ( #64825, #79544, #112385, #26806 ) ) ;
#47440 = CARTESIAN_POINT ( 'NONE',  ( 20.93975676684922504, 10.31104185824063180, -106.0204516983106231 ) ) ;
#47442 = ORIENTED_EDGE ( 'NONE', *, *, #107138, .T. ) ;
#47443 = VECTOR ( 'NONE', #151103, 1000.000000000000000 ) ;
#47444 = CARTESIAN_POINT ( 'NONE',  ( -20.64999999999999858, 73.60000000001224407, -149.7477294072864709 ) ) ;
#47445 = EDGE_LOOP ( 'NONE', ( #99182, #7597, #173079, #80956 ) ) ;
#47446 = CARTESIAN_POINT ( 'NONE',  ( 21.10642757222115407, 65.27684371085345560, -124.2824099607391730 ) ) ;
#47447 = DIRECTION ( 'NONE',  ( -1.000000000000000000, -0.000000000000000000, -0.000000000000000000 ) ) ;
#47448 = CARTESIAN_POINT ( 'NONE',  ( -18.59999999999999787, 1.115600667400684642E-11, -74.90000000000000568 ) ) ;
#47449 = VERTEX_POINT ( 'NONE', #249227 ) ;
#47450 = CARTESIAN_POINT ( 'NONE',  ( 23.14999999999999503, 14.05000000000000071, -27.98630492923908619 ) ) ;
#47451 = DIRECTION ( 'NONE',  ( 1.000000000000000000, -0.000000000000000000, 0.000000000000000000 ) ) ;
#47452 = FACE_OUTER_BOUND ( 'NONE', #254820, .T. ) ;
#47453 = VERTEX_POINT ( 'NONE', #69314 ) ;
#47454 = DIRECTION ( 'NONE',  ( 0.000000000000000000, -0.9915357197604792727, 0.1298341882520475943 ) ) ;
#47456 = EDGE_LOOP ( 'NONE', ( #84174, #155108, #65658, #227405, #235221 ) ) ;
#47455 = DIRECTION ( 'NONE',  ( -1.000000000000000000, -3.265361837132813093E-16, 0.000000000000000000 ) ) ;
#47457 = EDGE_CURVE ( 'NONE', #177284, #100958, #172465, .T. ) ;
#47458 = CARTESIAN_POINT ( 'NONE',  ( -23.39999999999994529, 64.25000000001119815, -3.123107484524795474 ) ) ;
#47459 = DIRECTION ( 'NONE',  ( 0.000000000000000000, 0.000000000000000000, -1.000000000000000000 ) ) ;
#47460 = AXIS2_PLACEMENT_3D ( 'NONE', #176185, #137038, #95343 ) ;
#47461 = AXIS2_PLACEMENT_3D ( 'NONE', #237022, #58348, #254000 ) ;
#47462 = EDGE_LOOP ( 'NONE', ( #254454, #195183, #246842, #48833 ) ) ;
#47463 = AXIS2_PLACEMENT_3D ( 'NONE', #254202, #192975, #75612 ) ;
#47464 = CARTESIAN_POINT ( 'NONE',  ( -18.59999999999999787, 44.14788529697245423, -236.0604079036328073 ) ) ;
#47465 = CARTESIAN_POINT ( 'NONE',  ( -14.87779219673429054, 66.56936653093923439, -121.2913416897003032 ) ) ;
#47466 = CARTESIAN_POINT ( 'NONE',  ( -21.14999999999999858, 76.10000000001174669, -81.17267829206912211 ) ) ;
#47467 = EDGE_LOOP ( 'NONE', ( #251401, #40877, #33894 ) ) ;
#47468 = CARTESIAN_POINT ( 'NONE',  ( 20.94999999999999574, 13.71992543034163958, -238.5823796952984992 ) ) ;
#47469 = ADVANCED_FACE ( 'NONE', ( #70614 ), #9319, .T. ) ;
#47470 = CYLINDRICAL_SURFACE ( 'NONE', #205519, 0.09999999999999817368 ) ;
#47471 = EDGE_CURVE ( 'NONE', #187409, #150205, #22592, .T. ) ;
#47472 = ORIENTED_EDGE ( 'NONE', *, *, #210310, .T. ) ;
#47473 = CIRCLE ( 'NONE', #193256, 0.1000000000000013933 ) ;
#47474 = ADVANCED_FACE ( 'NONE', ( #210108 ), #159977, .F. ) ;
#47475 = AXIS2_PLACEMENT_3D ( 'NONE', #73008, #250323, #174694 ) ;
#47476 = CIRCLE ( 'NONE', #164031, 0.09999999999998898659 ) ;
#47477 = VERTEX_POINT ( 'NONE', #148848 ) ;
#47478 = CARTESIAN_POINT ( 'NONE',  ( -22.10000000000000142, -11.65000000000000036, 12.09999999999999609 ) ) ;
#47479 = VECTOR ( 'NONE', #141551, 1000.000000000000000 ) ;
#47480 = ADVANCED_FACE ( 'NONE', ( #109690 ), #240605, .T. ) ;
#47481 = EDGE_LOOP ( 'NONE', ( #150356, #249660, #8212, #180630 ) ) ;
#47482 = EDGE_CURVE ( 'NONE', #67782, #214123, #30791, .T. ) ;
#47483 = CARTESIAN_POINT ( 'NONE',  ( 18.51024323315077069, 10.31104185822948338, -39.02045169831058757 ) ) ;
#47484 = CARTESIAN_POINT ( 'NONE',  ( -23.25000000000000000, 77.25000000001136868, -28.22262673010923351 ) ) ;
#47485 = ORIENTED_EDGE ( 'NONE', *, *, #204221, .F. ) ;
#47486 = DIRECTION ( 'NONE',  ( 1.020425574104004196E-15, -6.982962677686266711E-15, 1.000000000000000000 ) ) ;
#47487 = CARTESIAN_POINT ( 'NONE',  ( -20.64999999999999858, 68.75000000001223555, -148.7731074845244166 ) ) ;
#47488 = EDGE_CURVE ( 'NONE', #106308, #155405, #174868, .T. ) ;
#47489 = DIRECTION ( 'NONE',  ( -1.000000000000000000, 0.000000000000000000, 0.000000000000000000 ) ) ;
#47490 = DIRECTION ( 'NONE',  ( 0.000000000000000000, -0.8814952561688476074, 0.4721928772777262417 ) ) ;
#47491 = DIRECTION ( 'NONE',  ( -3.469446951953660258E-14, 0.5000000000000209832, 0.8660254037844264952 ) ) ;
#47492 = DIRECTION ( 'NONE',  ( 1.000000000000000000, 0.000000000000000000, 0.000000000000000000 ) ) ;
#47493 = AXIS2_PLACEMENT_3D ( 'NONE', #107626, #28124, #187193 ) ;
#47494 = CARTESIAN_POINT ( 'NONE',  ( -20.85000000000000142, -1.835859311432481045, -212.6044391687984785 ) ) ;
#47495 = CIRCLE ( 'NONE', #226549, 0.1000000000000009354 ) ;
#47496 = CARTESIAN_POINT ( 'NONE',  ( -18.51991288638537725, -9.392436789662212959, -107.6432664039581795 ) ) ;
#47498 = VERTEX_POINT ( 'NONE', #136965 ) ;
#47497 = CARTESIAN_POINT ( 'NONE',  ( -22.50000000000000000, 75.90736249940255220, -114.6728046915650765 ) ) ;
#47500 = DIRECTION ( 'NONE',  ( -1.000000000000000000, 0.000000000000000000, 0.000000000000000000 ) ) ;
#47499 = AXIS2_PLACEMENT_3D ( 'NONE', #156574, #15776, #152721 ) ;
#47501 = EDGE_CURVE ( 'NONE', #111920, #196020, #197350, .T. ) ;
#47502 = ORIENTED_EDGE ( 'NONE', *, *, #71685, .F. ) ;
#47503 = AXIS2_PLACEMENT_3D ( 'NONE', #151786, #192189, #189615 ) ;
#47504 = DIRECTION ( 'NONE',  ( 1.000000000000000000, 0.000000000000000000, 0.000000000000000000 ) ) ;
#47505 = CIRCLE ( 'NONE', #239068, 0.4000000000000097367 ) ;
#47506 = CARTESIAN_POINT ( 'NONE',  ( 23.24999999999999645, 5.650000000011139001, -180.1499999999999773 ) ) ;
#47507 = DIRECTION ( 'NONE',  ( 0.000000000000000000, 0.9126074666063660468, 0.4088369013363524762 ) ) ;
#47508 = DIRECTION ( 'NONE',  ( 1.000000000000000000, 1.394253735153569469E-16, 2.602809386958778209E-16 ) ) ;
#47509 = AXIS2_PLACEMENT_3D ( 'NONE', #212721, #14535, #155337 ) ;
#47511 = ORIENTED_EDGE ( 'NONE', *, *, #4342, .T. ) ;
#47510 = AXIS2_PLACEMENT_3D ( 'NONE', #25076, #184109, #162014 ) ;
#47512 = EDGE_CURVE ( 'NONE', #138960, #193873, #232245, .T. ) ;
#47513 = CARTESIAN_POINT ( 'NONE',  ( -22.50000000000000000, 64.35000000001217302, -136.5231074845243597 ) ) ;
#47514 = LINE ( 'NONE', #184465, #223168 ) ;
#47515 = ORIENTED_EDGE ( 'NONE', *, *, #134884, .F. ) ;
#47516 = CARTESIAN_POINT ( 'NONE',  ( -23.25000000000000000, 11.75000000001115552, -134.0000000000000284 ) ) ;
#47517 = LINE ( 'NONE', #86632, #59659 ) ;
#47518 = EDGE_CURVE ( 'NONE', #110550, #34172, #176124, .T. ) ;
#47519 = EDGE_LOOP ( 'NONE', ( #2363, #213518, #116344, #204562 ) ) ;
#47520 = DIRECTION ( 'NONE',  ( 0.000000000000000000, 1.000000000000000000, 6.982962677686266711E-15 ) ) ;
#47521 = ORIENTED_EDGE ( 'NONE', *, *, #43267, .T. ) ;
#47522 = CYLINDRICAL_SURFACE ( 'NONE', #67320, 0.09999999999999939493 ) ;
#47523 = ORIENTED_EDGE ( 'NONE', *, *, #254209, .T. ) ;
#47524 = DIRECTION ( 'NONE',  ( 4.336808689942128177E-15, 0.8660254037844330455, -0.5000000000000096589 ) ) ;
#47525 = CIRCLE ( 'NONE', #122588, 0.1000000000000028644 ) ;
#47526 = LINE ( 'NONE', #52671, #167885 ) ;
#47527 = ORIENTED_EDGE ( 'NONE', *, *, #122347, .F. ) ;
#47528 = ORIENTED_EDGE ( 'NONE', *, *, #125328, .T. ) ;
#47529 = CARTESIAN_POINT ( 'NONE',  ( 18.49999999999998934, 85.32100840337339775, -129.2871692354463562 ) ) ;
#47531 = ORIENTED_EDGE ( 'NONE', *, *, #141602, .F. ) ;
#47530 = CARTESIAN_POINT ( 'NONE',  ( 23.14999999999999858, -2.099999999988846344, -167.5000000000000284 ) ) ;
#47532 = AXIS2_PLACEMENT_3D ( 'NONE', #160084, #201746, #222574 ) ;
#47533 = CARTESIAN_POINT ( 'NONE',  ( 18.59999999999999787, 77.73670573947940454, -91.50568489690056140 ) ) ;
#47534 = ORIENTED_EDGE ( 'NONE', *, *, #210127, .F. ) ;
#47535 = ADVANCED_FACE ( 'NONE', ( #53588 ), #92699, .T. ) ;
#47536 = VECTOR ( 'NONE', #86772, 1000.000000000000000 ) ;
#47537 = ORIENTED_EDGE ( 'NONE', *, *, #236442, .F. ) ;
#47538 = CARTESIAN_POINT ( 'NONE',  ( -23.25000000000000000, 26.06832281015329755, -254.4051978787608732 ) ) ;
#47539 = DIRECTION ( 'NONE',  ( 1.000000000000000000, -0.000000000000000000, 0.000000000000000000 ) ) ;
#47540 = ADVANCED_FACE ( 'NONE', ( #58692 ), #195690, .T. ) ;
#47541 = CARTESIAN_POINT ( 'NONE',  ( -18.49513951962169145, 38.17733670730264350, -261.0710301328860510 ) ) ;
#47542 = AXIS2_PLACEMENT_3D ( 'NONE', #10905, #252067, #231247 ) ;
#47543 = CARTESIAN_POINT ( 'NONE',  ( -16.77683809663752257, 9.945835743204147761, -20.83605098089580210 ) ) ;
#47544 = FACE_OUTER_BOUND ( 'NONE', #104449, .T. ) ;
#47545 = LINE ( 'NONE', #84070, #225389 ) ;
#47546 = AXIS2_PLACEMENT_3D ( 'NONE', #123800, #42981, #143348 ) ;
#47548 = VERTEX_POINT ( 'NONE', #216503 ) ;
#47547 = EDGE_CURVE ( 'NONE', #153155, #89497, #72476, .T. ) ;
#47550 = EDGE_CURVE ( 'NONE', #194460, #243580, #57415, .T. ) ;
#47549 = CARTESIAN_POINT ( 'NONE',  ( 18.59999999999999076, 51.96945017402672562, -231.5060697639786440 ) ) ;
#47551 = AXIS2_PLACEMENT_3D ( 'NONE', #119001, #159413, #172907 ) ;
#47552 = CARTESIAN_POINT ( 'NONE',  ( -20.94999999999999929, 74.83729825007462466, -195.4231074845243654 ) ) ;
#47553 = LINE ( 'NONE', #127107, #166100 ) ;
#47555 = FACE_OUTER_BOUND ( 'NONE', #128314, .T. ) ;
#47554 = AXIS2_PLACEMENT_3D ( 'NONE', #154803, #135189, #77780 ) ;
#47556 = ORIENTED_EDGE ( 'NONE', *, *, #45063, .F. ) ;
#47557 = DIRECTION ( 'NONE',  ( 0.000000000000000000, 0.8814952561688429444, -0.4721928772777345684 ) ) ;
#47559 = EDGE_CURVE ( 'NONE', #171995, #6826, #201639, .T. ) ;
#47558 = ORIENTED_EDGE ( 'NONE', *, *, #61719, .F. ) ;
#47560 = CARTESIAN_POINT ( 'NONE',  ( 21.05000000000000071, -8.663551401858002876, -110.0241011180673354 ) ) ;
#47562 = EDGE_LOOP ( 'NONE', ( #167055, #49821, #93077, #37955, #21966 ) ) ;
#47561 = AXIS2_PLACEMENT_3D ( 'NONE', #138939, #218488, #162412 ) ;
#47563 = CARTESIAN_POINT ( 'NONE',  ( -15.39946565075089602, 25.37977472455730776, -232.8574044443168987 ) ) ;
#47564 = DIRECTION ( 'NONE',  ( 0.000000000000000000, -0.000000000000000000, 1.000000000000000000 ) ) ;
#47565 = EDGE_CURVE ( 'NONE', #182093, #200908, #218181, .T. ) ;
#47566 = ORIENTED_EDGE ( 'NONE', *, *, #97070, .F. ) ;
#47567 = ORIENTED_EDGE ( 'NONE', *, *, #166310, .F. ) ;
#47569 = ORIENTED_EDGE ( 'NONE', *, *, #155694, .T. ) ;
#47568 = PLANE ( 'NONE',  #90640 ) ;
#47570 = CYLINDRICAL_SURFACE ( 'NONE', #17349, 0.09999999999998898659 ) ;
#47571 = VERTEX_POINT ( 'NONE', #157866 ) ;
#47572 = AXIS2_PLACEMENT_3D ( 'NONE', #200079, #94542, #134933 ) ;
#47573 = DIRECTION ( 'NONE',  ( 0.000000000000000000, -0.8814952561688430555, 0.4721928772777346239 ) ) ;
#47574 = CARTESIAN_POINT ( 'NONE',  ( 21.05000000000000071, 76.00000000001213607, -136.5231074845242745 ) ) ;
#47575 = EDGE_LOOP ( 'NONE', ( #13801, #128302, #245357, #83041, #251564, #77260 ) ) ;
#47576 = AXIS2_PLACEMENT_3D ( 'NONE', #188408, #31935, #148006 ) ;
#47577 = DIRECTION ( 'NONE',  ( 1.000000000000000000, -0.000000000000000000, -0.000000000000000000 ) ) ;
#47578 = PLANE ( 'NONE',  #161661 ) ;
#47580 = ORIENTED_EDGE ( 'NONE', *, *, #34027, .F. ) ;
#47579 = VECTOR ( 'NONE', #43138, 1000.000000000000000 ) ;
#47581 = AXIS2_PLACEMENT_3D ( 'NONE', #131919, #211459, #35142 ) ;
#47582 = EDGE_CURVE ( 'NONE', #17664, #230778, #172297, .T. ) ;
#47583 = AXIS2_PLACEMENT_3D ( 'NONE', #158153, #155574, #38175 ) ;
#47584 = CARTESIAN_POINT ( 'NONE',  ( 18.59999999999999432, -1.162701749938009677, -8.099999999999999645 ) ) ;
#47585 = CARTESIAN_POINT ( 'NONE',  ( -16.80438519320023616, 22.97861394159803439, -230.9356067475303007 ) ) ;
#47586 = EDGE_CURVE ( 'NONE', #79203, #160294, #105751, .T. ) ;
#47587 = ADVANCED_FACE ( 'NONE', ( #13186 ), #32778, .T. ) ;
#47588 = DIRECTION ( 'NONE',  ( 0.000000000000000000, -6.688090509790120484E-15, 1.000000000000000000 ) ) ;
#47590 = EDGE_LOOP ( 'NONE', ( #33238, #39799, #79673, #195884 ) ) ;
#47589 = DIRECTION ( 'NONE',  ( 1.000000000000000000, 0.000000000000000000, 0.000000000000000000 ) ) ;
#47591 = CARTESIAN_POINT ( 'NONE',  ( 20.94999999999999929, 0.000000000000000000, -33.50000000000000000 ) ) ;
#47592 = DIRECTION ( 'NONE',  ( 0.000000000000000000, -0.9651348961777379554, 0.2617529984164210233 ) ) ;
#47593 = DIRECTION ( 'NONE',  ( -0.000000000000000000, 0.000000000000000000, -1.000000000000000000 ) ) ;
#47595 = CARTESIAN_POINT ( 'NONE',  ( -16.87036670365549540, 60.86740053880574663, -221.1564527318009539 ) ) ;
#47594 = DIRECTION ( 'NONE',  ( 1.000000000000000000, 3.265361837132813093E-16, -0.000000000000000000 ) ) ;
#47596 = CARTESIAN_POINT ( 'NONE',  ( -20.94999675878240808, 65.70692517833285251, -164.5644653378304270 ) ) ;
#47597 = DIRECTION ( 'NONE',  ( 1.000000000000000000, 0.000000000000000000, 0.000000000000000000 ) ) ;
#47598 = DIRECTION ( 'NONE',  ( 0.000000000000000000, 0.9126074666063660468, 0.4088369013363524762 ) ) ;
#47599 = CARTESIAN_POINT ( 'NONE',  ( 20.94999999999999929, 62.24653955602229161, -247.9500786234238490 ) ) ;
#47600 = CIRCLE ( 'NONE', #1809, 0.8750000000000007772 ) ;
#47601 = VERTEX_POINT ( 'NONE', #73183 ) ;
#47602 = ORIENTED_EDGE ( 'NONE', *, *, #242572, .F. ) ;
#47603 = VERTEX_POINT ( 'NONE', #93981 ) ;
#47604 = FACE_OUTER_BOUND ( 'NONE', #173037, .T. ) ;
#47606 = EDGE_CURVE ( 'NONE', #109848, #150544, #1713, .T. ) ;
#47605 = ORIENTED_EDGE ( 'NONE', *, *, #194625, .F. ) ;
#47607 = DIRECTION ( 'NONE',  ( 0.000000000000000000, -0.1495327102803689356, -0.9887567792719336168 ) ) ;
#47608 = CARTESIAN_POINT ( 'NONE',  ( 20.94999999999999574, 87.75000000001234923, -167.1231074845242688 ) ) ;
#47609 = ORIENTED_EDGE ( 'NONE', *, *, #207621, .T. ) ;
#47610 = CARTESIAN_POINT ( 'NONE',  ( 20.94999999999999929, -9.499999999988848032, -143.8939691226524644 ) ) ;
#47611 = ORIENTED_EDGE ( 'NONE', *, *, #68990, .F. ) ;
#47612 = EDGE_LOOP ( 'NONE', ( #141636, #93805, #173722, #213466, #48127, #98284, #42501 ) ) ;
#47613 = DIRECTION ( 'NONE',  ( -1.000000000000000000, 3.265361837132813093E-16, 2.280189983783949500E-30 ) ) ;
#47614 = CIRCLE ( 'NONE', #18616, 0.1000000000000124678 ) ;
#47615 = DIRECTION ( 'NONE',  ( 1.000000000000000000, -0.000000000000000000, -0.000000000000000000 ) ) ;
#47617 = ORIENTED_EDGE ( 'NONE', *, *, #5730, .T. ) ;
#47616 = CYLINDRICAL_SURFACE ( 'NONE', #141339, 0.09999999999999939493 ) ;
#47618 = EDGE_CURVE ( 'NONE', #105021, #76006, #9780, .T. ) ;
#47620 = ORIENTED_EDGE ( 'NONE', *, *, #14613, .T. ) ;
#47619 = DIRECTION ( 'NONE',  ( 0.000000000000000000, 0.000000000000000000, -1.000000000000000000 ) ) ;
#47621 = DIRECTION ( 'NONE',  ( 0.000000000000000000, 0.000000000000000000, 1.000000000000000000 ) ) ;
#47622 = CARTESIAN_POINT ( 'NONE',  ( -16.88328101497759448, 9.950352834230013599, -121.3511795149293135 ) ) ;
#47623 = EDGE_LOOP ( 'NONE', ( #161218, #137374, #203458, #31185, #67730 ) ) ;
#47624 = DIRECTION ( 'NONE',  ( 0.000000000000000000, 6.982962677686266711E-15, -1.000000000000000000 ) ) ;
#47626 = ADVANCED_FACE ( 'NONE', ( #40482 ), #179964, .F. ) ;
#47625 = CARTESIAN_POINT ( 'NONE',  ( -21.93642651522410247, 33.66330848088261263, -242.8643360821705528 ) ) ;
#47627 = CARTESIAN_POINT ( 'NONE',  ( -16.90137573187933739, 9.950000000011137047, -113.2884174240969344 ) ) ;
#47629 = CARTESIAN_POINT ( 'NONE',  ( -16.94107738177414291, 10.01423928513661998, -20.94999999999999929 ) ) ;
#47628 = CYLINDRICAL_SURFACE ( 'NONE', #132326, 0.1000000000000028644 ) ;
#47631 = EDGE_CURVE ( 'NONE', #67070, #174276, #155699, .T. ) ;
#47630 = CARTESIAN_POINT ( 'NONE',  ( 18.59999999999999076, 10.49142135624846617, -91.75000000000005684 ) ) ;
#47632 = AXIS2_PLACEMENT_3D ( 'NONE', #170772, #106882, #168198 ) ;
#47633 = CARTESIAN_POINT ( 'NONE',  ( 18.54271179734073982, 85.62408429011104261, -163.2821426318238593 ) ) ;
#47634 = VECTOR ( 'NONE', #201734, 1000.000000000000000 ) ;
#47635 = CYLINDRICAL_SURFACE ( 'NONE', #184873, 12.87499999999999822 ) ;
#47636 = CARTESIAN_POINT ( 'NONE',  ( -17.05016517656212116, 44.15619606664471775, -235.2896518282563818 ) ) ;
#47637 = EDGE_LOOP ( 'NONE', ( #37816, #210160, #247053, #120861 ) ) ;
#47639 = ORIENTED_EDGE ( 'NONE', *, *, #17270, .F. ) ;
#47638 = AXIS2_PLACEMENT_3D ( 'NONE', #140688, #46712, #64999 ) ;
#47640 = VERTEX_POINT ( 'NONE', #3879 ) ;
#47641 = CIRCLE ( 'NONE', #168345, 0.1000000000000124678 ) ;
#47642 = EDGE_CURVE ( 'NONE', #34916, #151221, #251519, .T. ) ;
#47643 = CARTESIAN_POINT ( 'NONE',  ( -17.01825945287481545, 66.05000000001255955, -182.7731074845244450 ) ) ;
#47644 = EDGE_CURVE ( 'NONE', #173596, #183385, #220373, .T. ) ;
#47645 = ORIENTED_EDGE ( 'NONE', *, *, #193984, .F. ) ;
#47646 = CARTESIAN_POINT ( 'NONE',  ( -21.05000000000000071, 69.08367151115869831, -247.5088222940653679 ) ) ;
#47648 = ORIENTED_EDGE ( 'NONE', *, *, #46746, .T. ) ;
#47647 = STYLED_ITEM ( 'NONE', ( #63027 ), #157027 ) ;
#47649 = CARTESIAN_POINT ( 'NONE',  ( -17.73285935862227802, 15.55873092870509034, -221.4152481787321278 ) ) ;
#47650 = ORIENTED_EDGE ( 'NONE', *, *, #178012, .F. ) ;
#47651 = CIRCLE ( 'NONE', #193445, 0.1999999999999987899 ) ;
#47652 = SURFACE_SIDE_STYLE ('',( #226287 ) ) ;
#47653 = TOROIDAL_SURFACE ( 'NONE', #56030, 3.899999999999999467, 0.1000000000000000056 ) ;
#47654 = ORIENTED_EDGE ( 'NONE', *, *, #57314, .T. ) ;
#47655 = EDGE_CURVE ( 'NONE', #14025, #239754, #122351, .T. ) ;
#47656 = ORIENTED_EDGE ( 'NONE', *, *, #11738, .F. ) ;
#47657 = EDGE_CURVE ( 'NONE', #165694, #59994, #184877, .T. ) ;
#47658 = ORIENTED_EDGE ( 'NONE', *, *, #108341, .T. ) ;
#47659 = CIRCLE ( 'NONE', #168359, 0.09999999999999939493 ) ;
#47660 = LINE ( 'NONE', #209313, #87870 ) ;
#47661 = CARTESIAN_POINT ( 'NONE',  ( -22.94999999999999929, 4.898587196589412829E-16, 4.000000000000000000 ) ) ;
#47662 = DIRECTION ( 'NONE',  ( 0.000000000000000000, 0.2128009952263601456, -0.9770955615653315052 ) ) ;
#47663 = TOROIDAL_SURFACE ( 'NONE', #64257, 4.149999999999999467, 0.1000000000000000056 ) ;
#47664 = CARTESIAN_POINT ( 'NONE',  ( -18.40000000000000213, 20.70659057908908096, -227.9750359040556873 ) ) ;
#47665 = CARTESIAN_POINT ( 'NONE',  ( -18.59999999999999787, -10.84999999999999076, 32.89999999999999858 ) ) ;
#47666 = CARTESIAN_POINT ( 'NONE',  ( -18.34374000495059676, 11.47316190337362940, -158.2500000000000284 ) ) ;
#47668 = CARTESIAN_POINT ( 'NONE',  ( 18.39999999999999503, 65.08943781962308606, -222.1672656287770451 ) ) ;
#47667 = CARTESIAN_POINT ( 'NONE',  ( -16.94445028196807002, 9.992063609708893068, -87.89266982158160602 ) ) ;
#47669 = CYLINDRICAL_SURFACE ( 'NONE', #174777, 0.09999999999999939493 ) ;
#47671 = EDGE_LOOP ( 'NONE', ( #201643, #123597, #170792, #74288 ) ) ;
#47670 = CARTESIAN_POINT ( 'NONE',  ( -18.50000000000000000, 77.16412189325305349, -95.10825939895268277 ) ) ;
#47673 = CARTESIAN_POINT ( 'NONE',  ( 21.56666275994540172, 1.115600667400684642E-11, -160.5426315931066483 ) ) ;
#47672 = CARTESIAN_POINT ( 'NONE',  ( 20.97217846901852312, 8.875441724720827708, -75.50122768393727313 ) ) ;
#47674 = CYLINDRICAL_SURFACE ( 'NONE', #7246, 0.09999999999999939493 ) ;
#47675 = EDGE_LOOP ( 'NONE', ( #53322, #84991, #37640, #21340 ) ) ;
#47676 = CARTESIAN_POINT ( 'NONE',  ( 20.84999999999999787, 11.75000000001116085, -160.5808527540413309 ) ) ;
#47677 = AXIS2_PLACEMENT_3D ( 'NONE', #161659, #2543, #20867 ) ;
#47679 = AXIS2_PLACEMENT_3D ( 'NONE', #225957, #223410, #86450 ) ;
#47678 = CARTESIAN_POINT ( 'NONE',  ( -20.94999999999999929, 72.02722222756958104, -225.1832529173024398 ) ) ;
#47680 = DIRECTION ( 'NONE',  ( 0.000000000000000000, 0.000000000000000000, 1.000000000000000000 ) ) ;
#47681 = CIRCLE ( 'NONE', #155872, 0.1000000000000028644 ) ;
#47682 = ORIENTED_EDGE ( 'NONE', *, *, #171027, .T. ) ;
#47683 = ADVANCED_FACE ( 'NONE', ( #120010 ), #1292, .T. ) ;
#47684 = AXIS2_PLACEMENT_3D ( 'NONE', #192455, #230284, #109050 ) ;
#47685 = DIRECTION ( 'NONE',  ( -0.000000000000000000, 0.5283051335749948674, -0.8490545835447252943 ) ) ;
#47686 = EDGE_CURVE ( 'NONE', #47453, #64807, #43246, .T. ) ;
#47687 = VECTOR ( 'NONE', #52331, 1000.000000000000114 ) ;
#47688 = DIRECTION ( 'NONE',  ( 0.000000000000000000, -0.2558827019434435912, 0.9667078373770033872 ) ) ;
#47689 = DIRECTION ( 'NONE',  ( 1.000000000000000000, 0.000000000000000000, -0.000000000000000000 ) ) ;
#47690 = VERTEX_POINT ( 'NONE', #63854 ) ;
#47691 = EDGE_LOOP ( 'NONE', ( #237598, #230914, #76016, #64885 ) ) ;
#47692 = VECTOR ( 'NONE', #146957, 1000.000000000000000 ) ;
#47693 = DIRECTION ( 'NONE',  ( 0.000000000000000000, 0.000000000000000000, -1.000000000000000000 ) ) ;
#47694 = EDGE_LOOP ( 'NONE', ( #33563, #163068, #105677, #154335 ) ) ;
#47695 = CARTESIAN_POINT ( 'NONE',  ( 22.47007471830798053, 7.720710651937614522, -67.00000000000004263 ) ) ;
#47696 = CARTESIAN_POINT ( 'NONE',  ( -18.39999999999999503, -9.499999999988849808, -174.4221498493304239 ) ) ;
#47697 = FACE_OUTER_BOUND ( 'NONE', #185435, .T. ) ;
#47699 = EDGE_CURVE ( 'NONE', #196043, #219593, #241224, .T. ) ;
#47698 = DIRECTION ( 'NONE',  ( 1.000000000000000000, 0.000000000000000000, 0.000000000000000000 ) ) ;
#47700 = EDGE_LOOP ( 'NONE', ( #41286, #65419, #30341, #155565 ) ) ;
#47701 = VECTOR ( 'NONE', #112031, 1000.000000000000000 ) ;
#47702 = CIRCLE ( 'NONE', #193476, 0.1000000000000025591 ) ;
#47703 = CARTESIAN_POINT ( 'NONE',  ( -15.69373346032659811, 9.356790025057039273, -117.7048265086139480 ) ) ;
#47704 = CARTESIAN_POINT ( 'NONE',  ( 23.14999999999999858, 76.00000000001142553, -36.02310748452432421 ) ) ;
#47706 = ADVANCED_FACE ( 'NONE', ( #44304 ), #80826, .T. ) ;
#47705 = CARTESIAN_POINT ( 'NONE',  ( -20.64999999999999858, 85.40000000001198543, -112.9170766071766820 ) ) ;
#47707 = CARTESIAN_POINT ( 'NONE',  ( 18.59999999999999076, 1.115600667400684642E-11, -67.00000000000000000 ) ) ;
#47708 = ORIENTED_EDGE ( 'NONE', *, *, #248501, .F. ) ;
#47709 = DIRECTION ( 'NONE',  ( 1.000000000000000000, 0.000000000000000000, -0.000000000000000000 ) ) ;
#47711 = VERTEX_POINT ( 'NONE', #160417 ) ;
#47710 = DIRECTION ( 'NONE',  ( 0.000000000000000000, 0.2128009952263603677, -0.9770955615653313941 ) ) ;
#47712 = CARTESIAN_POINT ( 'NONE',  ( -18.39999999999999858, 85.60000000001232934, -162.9910380878246201 ) ) ;
#47713 = CARTESIAN_POINT ( 'NONE',  ( 20.94999999999999929, 71.14953271029189352, -48.05737489352603120 ) ) ;
#47714 = CARTESIAN_POINT ( 'NONE',  ( 20.94999999999999929, 85.00000000001197975, -112.9170766071766820 ) ) ;
#47715 = EDGE_CURVE ( 'NONE', #198727, #39812, #239937, .T. ) ;
#47716 = CARTESIAN_POINT ( 'NONE',  ( -16.89797118371612683, 9.976380722655340705, -87.93729336755826864 ) ) ;
#47717 = DIRECTION ( 'NONE',  ( 0.5932847527679310229, -0.8049926720990042694, -6.366092712777067056E-16 ) ) ;
#47718 = CARTESIAN_POINT ( 'NONE',  ( 22.16821283564876666, 10.69812671114205394, -227.0695021710343156 ) ) ;
#47719 = VERTEX_POINT ( 'NONE', #140828 ) ;
#47720 = CARTESIAN_POINT ( 'NONE',  ( 23.14999999999999503, 14.05000000001115623, -94.98630492923912527 ) ) ;
#47721 = AXIS2_PLACEMENT_3D ( 'NONE', #62569, #85942, #41737 ) ;
#47722 = DIRECTION ( 'NONE',  ( 0.000000000000000000, 1.000000000000000000, 6.982962677686266711E-15 ) ) ;
#47724 = CIRCLE ( 'NONE', #193499, 0.1000000000000072220 ) ;
#47723 = CARTESIAN_POINT ( 'NONE',  ( -16.86733706339143524, 51.66079883479768853, -231.9101604434227113 ) ) ;
#47725 = VECTOR ( 'NONE', #100722, 1000.000000000000000 ) ;
#47726 = DIRECTION ( 'NONE',  ( 0.000000000000000000, -7.086529944415886769E-15, 1.000000000000000000 ) ) ;
#47727 = FACE_OUTER_BOUND ( 'NONE', #135397, .T. ) ;
#47728 = EDGE_LOOP ( 'NONE', ( #92932, #29697, #108879 ) ) ;
#47729 = ORIENTED_EDGE ( 'NONE', *, *, #185696, .F. ) ;
#47730 = CIRCLE ( 'NONE', #201867, 0.1000000000000028644 ) ;
#47731 = CARTESIAN_POINT ( 'NONE',  ( -18.69999999999999929, -6.162641848847272286, 0.4936627796039583793 ) ) ;
#47732 = CARTESIAN_POINT ( 'NONE',  ( 22.39999999999999503, 1.115541036281197940E-11, -126.2092204016266379 ) ) ;
#47733 = CIRCLE ( 'NONE', #85313, 0.09999999999999864553 ) ;
#47734 = CARTESIAN_POINT ( 'NONE',  ( -21.05000000000000071, 74.16465844978787914, -158.4679561919613775 ) ) ;
#47735 = DIRECTION ( 'NONE',  ( 1.000000000000000000, 0.000000000000000000, 0.000000000000000000 ) ) ;
#47737 = VECTOR ( 'NONE', #43798, 1000.000000000000000 ) ;
#47736 = DIRECTION ( 'NONE',  ( -0.000000000000000000, -6.982962677686266711E-15, 1.000000000000000000 ) ) ;
#47738 = CARTESIAN_POINT ( 'NONE',  ( -23.24999999999999645, 85.60000000001210196, -129.9229180933022576 ) ) ;
#47739 = AXIS2_PLACEMENT_3D ( 'NONE', #13169, #152706, #92685 ) ;
#47740 = VECTOR ( 'NONE', #184595, 1000.000000000000000 ) ;
#47741 = CARTESIAN_POINT ( 'NONE',  ( -20.94560253601877164, 17.12224500340141020, -224.4024732428971731 ) ) ;
#47742 = CIRCLE ( 'NONE', #43677, 0.09999999999999123479 ) ;
#47743 = ORIENTED_EDGE ( 'NONE', *, *, #126746, .T. ) ;
#47744 = DIRECTION ( 'NONE',  ( 2.259780016855445309E-14, 0.9875055080513753802, -0.1575844902526748192 ) ) ;
#47745 = ORIENTED_EDGE ( 'NONE', *, *, #174886, .F. ) ;
#47746 = CARTESIAN_POINT ( 'NONE',  ( -13.40000000000000036, -9.650000000000005684, 17.60000000000000497 ) ) ;
#47747 = CARTESIAN_POINT ( 'NONE',  ( -5.899999999999938183, 64.65000000001120384, -22.12310748452479103 ) ) ;
#47749 = VECTOR ( 'NONE', #233778, 1000.000000000000000 ) ;
#47748 = DIRECTION ( 'NONE',  ( 1.000000000000000000, -0.000000000000000000, -0.000000000000000000 ) ) ;
#47750 = FACE_OUTER_BOUND ( 'NONE', #148970, .T. ) ;
#47751 = DIRECTION ( 'NONE',  ( 1.000000000000000000, 0.000000000000000000, 0.000000000000000000 ) ) ;
#47752 = CARTESIAN_POINT ( 'NONE',  ( -18.43599941264911024, -9.519327428594779761, -6.972976789521343477 ) ) ;
#47753 = CARTESIAN_POINT ( 'NONE',  ( -16.87242674293849731, 66.05000000001182059, -82.17201723815203707 ) ) ;
#47754 = VERTEX_POINT ( 'NONE', #41747 ) ;
#47755 = CARTESIAN_POINT ( 'NONE',  ( -18.59999999999999787, 44.05662455031180968, -236.1012915937664616 ) ) ;
#47756 = DIRECTION ( 'NONE',  ( -0.000000000000000000, 0.8660254037844411501, 0.4999999999999956701 ) ) ;
#47757 = EDGE_CURVE ( 'NONE', #83423, #168199, #101658, .T. ) ;
#47758 = CARTESIAN_POINT ( 'NONE',  ( -18.40000000000000213, 11.75000000001113953, -124.7500000000000284 ) ) ;
#47759 = DIRECTION ( 'NONE',  ( 0.000000000000000000, 0.000000000000000000, 1.000000000000000000 ) ) ;
#47760 = CARTESIAN_POINT ( 'NONE',  ( 18.47149038651511432, 85.67145715801859751, -96.35032114978582740 ) ) ;
#47761 = CARTESIAN_POINT ( 'NONE',  ( 21.05000000000000071, 9.459578591139306880, -220.9384041938172345 ) ) ;
#47762 = AXIS2_PLACEMENT_3D ( 'NONE', #243565, #3663, #84442 ) ;
#47763 = AXIS2_PLACEMENT_3D ( 'NONE', #83656, #67984, #150116 ) ;
#47764 = EDGE_LOOP ( 'NONE', ( #178811, #159523, #163775, #175480 ) ) ;
#47765 = DIRECTION ( 'NONE',  ( 1.000000000000000000, 0.000000000000000000, 0.000000000000000000 ) ) ;
#47766 = VERTEX_POINT ( 'NONE', #68661 ) ;
#47767 = CARTESIAN_POINT ( 'NONE',  ( -16.90987985657661952, 51.63327247197580760, -231.9314585426081123 ) ) ;
#47768 = CARTESIAN_POINT ( 'NONE',  ( 21.09706851349341861, 67.22415748653889978, -157.7875412681247838 ) ) ;
#47769 = EDGE_CURVE ( 'NONE', #149928, #242592, #35769, .T. ) ;
#47770 = B_SPLINE_CURVE_WITH_KNOTS ( 'NONE', 3,
 ( #108077, #8966, #3834, #88475, #168087, #83332, #242430, #222869, #92347, #10262, #71534, #171935, #211023, #113200, #70259, #75387, #169367, #191490, #170665, #174522, #94907, #253981 ),
 .UNSPECIFIED., .F., .F.,
 ( 4, 3, 3, 3, 3, 3, 3, 4 ),
 ( 0.000000000000000000, 7.307836821075256540E-06, 4.161455748546809275E-05, 7.576591810647573624E-05, 0.0001098090429817548115, 0.0001438003617351177430, 0.0001777914035423749776, 0.0002117966137403039836 ),
 .UNSPECIFIED. ) ;
#47771 = DIRECTION ( 'NONE',  ( 1.000000000000000000, 0.000000000000000000, 0.000000000000000000 ) ) ;
#47772 = ORIENTED_EDGE ( 'NONE', *, *, #114256, .F. ) ;
#47773 = CARTESIAN_POINT ( 'NONE',  ( 20.96428641294107820, 64.25000000001146816, -42.84821430658371355 ) ) ;
#47774 = DIRECTION ( 'NONE',  ( 0.000000000000000000, -6.982962677686266711E-15, 1.000000000000000000 ) ) ;
#47775 = VERTEX_POINT ( 'NONE', #2580 ) ;
#47776 = CIRCLE ( 'NONE', #193561, 7.720710678118663850 ) ;
#47777 = CARTESIAN_POINT ( 'NONE',  ( 23.24999999999999289, 23.38726701055792745, -229.1122755113798348 ) ) ;
#47778 = ADVANCED_FACE ( 'NONE', ( #8679 ), #88182, .T. ) ;
#47779 = AXIS2_PLACEMENT_3D ( 'NONE', #152665, #232192, #211328 ) ;
#47780 =( BOUNDED_SURFACE ( )  B_SPLINE_SURFACE ( 3, 2, ( 
 ( #108908, #248430, #69810 ),
 ( #209294, #51477, #52776 ),
 ( #30693, #110188, #189741 ),
 ( #111485, #191050, #12410 ),
 ( #33273, #112773, #192313 ),
 ( #93196, #133608, #97014 ),
 ( #176616, #74958, #37110 ),
 ( #157047, #114037, #138710 ),
 ( #196155, #99593, #18794 ),
 ( #505, #257347, #216986 ) ),
 .UNSPECIFIED., .F., .F., .F. ) 
 B_SPLINE_SURFACE_WITH_KNOTS ( ( 4, 2, 2, 2, 4 ),
 ( 3, 3 ),
 ( 0.0001836757140119112878, 0.0004000170051583610588, 0.0005081876507315859172, 0.0005622729735181982921, 0.0006163582963048107755 ),
 ( 0.000000000000000000, 1.000000000000000000 ),
 .UNSPECIFIED. ) 
 GEOMETRIC_REPRESENTATION_ITEM ( )  RATIONAL_B_SPLINE_SURFACE ( (
 ( 1.000000000000000000, 0.7071067811865475727, 1.000000000000000000),
 ( 1.000000000000000000, 0.6461995200012254914, 1.000000000000000000),
 ( 1.000000000000000000, 0.5776453529573883916, 1.000000000000000000),
 ( 1.000000000000000000, 0.4585233068339760187, 1.000000000000000000),
 ( 1.000000000000000000, 0.4154092989943317660, 1.000000000000000000),
 ( 1.000000000000000000, 0.3550093145834672392, 1.000000000000000000),
 ( 1.000000000000000000, 0.3354498651689156175, 1.000000000000000000),
 ( 1.000000000000000000, 0.3060347992252056004, 1.000000000000000000),
 ( 1.000000000000000000, 0.2963555829629416771, 1.000000000000000000),
 ( 1.000000000000000000, 0.2966190024560776406, 1.000000000000000000) ) ) 
 REPRESENTATION_ITEM ( '' )  SURFACE ( )  );
#47781 = EDGE_LOOP ( 'NONE', ( #125482, #169566, #254018, #211583, #22556 ) ) ;
#47782 = EDGE_CURVE ( 'NONE', #245420, #190860, #99102, .T. ) ;
#47783 = DIRECTION ( 'NONE',  ( 0.000000000000000000, 0.03181660087583042945, -0.9994937237965569876 ) ) ;
#47784 = LINE ( 'NONE', #81760, #191530 ) ;
#47785 = DIRECTION ( 'NONE',  ( 1.000000000000000000, -0.000000000000000000, 0.000000000000000000 ) ) ;
#47787 = UNCERTAINTY_MEASURE_WITH_UNIT (LENGTH_MEASURE( 1.000000000000000082E-05 ), #23706, 'distance_accuracy_value', 'NONE');
#47786 = DIRECTION ( 'NONE',  ( 0.000000000000000000, 0.000000000000000000, -1.000000000000000000 ) ) ;
#47788 = EDGE_CURVE ( 'NONE', #255696, #88307, #115545, .T. ) ;
#47789 = DIRECTION ( 'NONE',  ( 0.000000000000000000, 0.1495327102803586661, -0.9887567792719350601 ) ) ;
#47790 = CARTESIAN_POINT ( 'NONE',  ( -16.77431908686106965, 66.05419424549431540, -157.3589467021746486 ) ) ;
#47791 = CARTESIAN_POINT ( 'NONE',  ( -16.77977881697926321, 66.05339806647970136, -190.8617289114093865 ) ) ;
#47792 = DIRECTION ( 'NONE',  ( 0.000000000000000000, -0.8814952561688430555, 0.4721928772777346239 ) ) ;
#47793 = CARTESIAN_POINT ( 'NONE',  ( -23.25000000000000000, 76.00000000001195133, -103.0231074845243171 ) ) ;
#47795 = ORIENTED_EDGE ( 'NONE', *, *, #76201, .F. ) ;
#47794 = CARTESIAN_POINT ( 'NONE',  ( -23.15000000000000213, 6.878457983866232972, -212.1414458560986986 ) ) ;
#47796 = ORIENTED_EDGE ( 'NONE', *, *, #177913, .F. ) ;
#47797 = CYLINDRICAL_SURFACE ( 'NONE', #61928, 0.1000000000000028644 ) ;
#47798 = EDGE_CURVE ( 'NONE', #206647, #102291, #222269, .T. ) ;
#47800 = ORIENTED_EDGE ( 'NONE', *, *, #205583, .T. ) ;
#47799 = CARTESIAN_POINT ( 'NONE',  ( 21.00000000000000000, 9.750000000011153745, -79.35000000000005116 ) ) ;
#47801 = ORIENTED_EDGE ( 'NONE', *, *, #169111, .T. ) ;
#47802 = CARTESIAN_POINT ( 'NONE',  ( -16.87683809663752399, 9.850000000011140955, -113.1500000000000341 ) ) ;
#47803 = DIRECTION ( 'NONE',  ( -1.000000000000000000, 0.000000000000000000, 0.000000000000000000 ) ) ;
#47804 = VECTOR ( 'NONE', #244803, 1000.000000000000114 ) ;
#47805 = CIRCLE ( 'NONE', #72804, 0.09999999999999950595 ) ;
#47806 = EDGE_CURVE ( 'NONE', #86798, #210461, #64086, .T. ) ;
#47807 = DIRECTION ( 'NONE',  ( 0.000000000000000000, 0.000000000000000000, -1.000000000000000000 ) ) ;
#47808 = CARTESIAN_POINT ( 'NONE',  ( 21.05000000000000071, 61.95000000001146390, -41.53680255528533394 ) ) ;
#47809 = DIRECTION ( 'NONE',  ( 1.000000000000000000, 0.000000000000000000, 0.000000000000000000 ) ) ;
#47810 = LINE ( 'NONE', #110366, #119691 ) ;
#47811 = ADVANCED_FACE ( 'NONE', ( #174215 ), #90765, .F. ) ;
#47812 = CARTESIAN_POINT ( 'NONE',  ( -23.15000000000000213, 74.00000000001199396, -116.2477294072864140 ) ) ;
#47813 = ORIENTED_EDGE ( 'NONE', *, *, #1896, .F. ) ;
#47814 = EDGE_LOOP ( 'NONE', ( #4668, #36540, #189453, #243950, #119582, #4876, #1693, #14777, #81039, #64571, #227862, #38893, #2093, #148009, #19068, #212946 ) ) ;
#47815 = DIRECTION ( 'NONE',  ( -0.000000000000000000, 1.000000000000000000, -0.000000000000000000 ) ) ;
#47816 = AXIS2_PLACEMENT_3D ( 'NONE', #201512, #179408, #64570 ) ;
#47817 = AXIS2_PLACEMENT_3D ( 'NONE', #247936, #71894, #31501 ) ;
#47818 = VERTEX_POINT ( 'NONE', #212032 ) ;
#47819 = LINE ( 'NONE', #10001, #34529 ) ;
#47820 = ORIENTED_EDGE ( 'NONE', *, *, #243430, .F. ) ;
#47821 = DIRECTION ( 'NONE',  ( 0.000000000000000000, -0.03181660087581233282, 0.9994937237965575427 ) ) ;
#47822 = TOROIDAL_SURFACE ( 'NONE', #226911, 0.2000000000000000111, 0.1000000000000000056 ) ;
#47823 = AXIS2_PLACEMENT_3D ( 'NONE', #163590, #183158, #82720 ) ;
#47824 = CARTESIAN_POINT ( 'NONE',  ( -21.52071067811865746, 62.95586049149184760, -221.8994582331316394 ) ) ;
#47825 = CARTESIAN_POINT ( 'NONE',  ( 18.49999999999987566, 65.62657994473185852, -44.75731935989774257 ) ) ;
#47826 = CARTESIAN_POINT ( 'NONE',  ( 21.05000000000000071, 61.88149656937974896, -248.1136133839584090 ) ) ;
#47827 = EDGE_LOOP ( 'NONE', ( #148577, #243529, #139538, #391 ) ) ;
#47828 = CARTESIAN_POINT ( 'NONE',  ( 20.94999999999999929, 1.835341550224413698, -11.55515129256298401 ) ) ;
#47829 = ORIENTED_EDGE ( 'NONE', *, *, #284, .F. ) ;
#47830 = CARTESIAN_POINT ( 'NONE',  ( -20.64999999999999858, 1.115600667400684642E-11, -134.0000000000000284 ) ) ;
#47831 = DIRECTION ( 'NONE',  ( -1.000000000000000000, 1.875376730785737719E-16, 1.309568571767809260E-30 ) ) ;
#47832 = CARTESIAN_POINT ( 'NONE',  ( 18.46082813848001436, 8.896929522169481075, -245.4351262571402970 ) ) ;
#47833 = SPHERICAL_SURFACE ( 'NONE', #44987, 0.1000000000000000056 ) ;
#47834 = ORIENTED_EDGE ( 'NONE', *, *, #196709, .T. ) ;
#47835 = CARTESIAN_POINT ( 'NONE',  ( 23.15000000000000213, -11.74999999999999289, -12.25000000000000000 ) ) ;
#47836 = ORIENTED_EDGE ( 'NONE', *, *, #93988, .T. ) ;
#47838 = EDGE_LOOP ( 'NONE', ( #48013, #35378, #104169, #246196, #127521, #32855, #134166, #150997, #179287, #29270, #239853, #59913, #243314, #129255 ) ) ;
#47837 = DIRECTION ( 'NONE',  ( 0.000000000000000000, -0.8660254037844412611, -0.4999999999999956701 ) ) ;
#47839 = CARTESIAN_POINT ( 'NONE',  ( -23.15000000000000213, 87.65000000001172964, -72.52310748452423184 ) ) ;
#47841 = ORIENTED_EDGE ( 'NONE', *, *, #188386, .T. ) ;
#47840 = AXIS2_PLACEMENT_3D ( 'NONE', #187734, #168195, #70366 ) ;
#47842 = VECTOR ( 'NONE', #185819, 1000.000000000000000 ) ;
#47843 = EDGE_CURVE ( 'NONE', #246499, #147363, #243147, .T. ) ;
#47844 = DIRECTION ( 'NONE',  ( 0.000000000000000000, 8.770518838402102073E-15, -1.000000000000000000 ) ) ;
#47845 = ORIENTED_EDGE ( 'NONE', *, *, #137375, .T. ) ;
#47847 = EDGE_CURVE ( 'NONE', #154949, #102316, #239237, .T. ) ;
#47846 = AXIS2_PLACEMENT_3D ( 'NONE', #20865, #119969, #142057 ) ;
#47848 = CARTESIAN_POINT ( 'NONE',  ( -21.44999999999999929, 68.85000000001156195, -57.27310748452436684 ) ) ;
#47849 = ADVANCED_FACE ( 'NONE', ( #191197 ), #155874, .F. ) ;
#47850 = CARTESIAN_POINT ( 'NONE',  ( 23.14999999999999147, 80.15000000001165859, -69.52310748452430289 ) ) ;
#47852 = EDGE_CURVE ( 'NONE', #40222, #782, #112915, .T. ) ;
#47851 =( BOUNDED_CURVE ( )  B_SPLINE_CURVE ( 3, ( #18377, #77059, #255657, #180034 ),
 .UNSPECIFIED., .F., .F. ) 
 B_SPLINE_CURVE_WITH_KNOTS ( ( 4, 4 ),
 ( 3.141592653589793116, 4.712388980384689674 ),
 .UNSPECIFIED. ) 
 CURVE ( )  GEOMETRIC_REPRESENTATION_ITEM ( )  RATIONAL_B_SPLINE_CURVE ( ( 1.000000000000000000, 0.8047378541243649375, 0.8047378541243649375, 1.000000000000000000 ) ) 
 REPRESENTATION_ITEM ( '' )  );
#47853 = DIRECTION ( 'NONE',  ( 0.000000000000000000, 1.000000000000000000, 0.000000000000000000 ) ) ;
#47854 = AXIS2_PLACEMENT_3D ( 'NONE', #29241, #189568, #231272 ) ;
#47855 = VECTOR ( 'NONE', #177075, 1000.000000000000000 ) ;
#47856 = CARTESIAN_POINT ( 'NONE',  ( -16.87851181299898684, 9.950042924007739487, -12.64985648463308365 ) ) ;
#47857 = AXIS2_PLACEMENT_3D ( 'NONE', #244107, #2923, #82444 ) ;
#47859 = EDGE_LOOP ( 'NONE', ( #88, #57658, #257367, #137807, #129739, #119793, #252679 ) ) ;
#47858 = EDGE_CURVE ( 'NONE', #171611, #42095, #193739, .T. ) ;
#47860 = DIRECTION ( 'NONE',  ( 0.000000000000000000, -1.000000000000000000, 0.000000000000000000 ) ) ;
#47861 = CARTESIAN_POINT ( 'NONE',  ( 20.94999999999999929, -8.999999999988842703, -57.10603087734755690 ) ) ;
#47862 = CARTESIAN_POINT ( 'NONE',  ( -21.05000000000000071, 74.16465844978787914, -158.4679561919613775 ) ) ;
#47863 = ADVANCED_FACE ( 'NONE', ( #72522 ), #152064, .T. ) ;
#47864 = ORIENTED_EDGE ( 'NONE', *, *, #10553, .T. ) ;
#47865 = DIRECTION ( 'NONE',  ( 2.952720810173289112E-16, -1.000000000000000000, -0.000000000000000000 ) ) ;
#47868 = ADVANCED_FACE ( 'NONE', ( #12553 ), #30980, .T. ) ;
#47867 = ADVANCED_FACE ( 'NONE', ( #34683 ), #32119, .F. ) ;
#47866 = VERTEX_POINT ( 'NONE', #213284 ) ;
#47869 = CARTESIAN_POINT ( 'NONE',  ( 21.08479644141222664, 30.84445554993508765, -252.0918114234447671 ) ) ;
#47870 = AXIS2_PLACEMENT_3D ( 'NONE', #101065, #67129, #245774 ) ;
#47871 = AXIS2_PLACEMENT_3D ( 'NONE', #105131, #66045, #46469 ) ;
#47872 = DIRECTION ( 'NONE',  ( -1.000000000000000000, -0.000000000000000000, 0.000000000000000000 ) ) ;
#47873 = FACE_OUTER_BOUND ( 'NONE', #143229, .T. ) ;
#47874 = EDGE_CURVE ( 'NONE', #179033, #185550, #202843, .T. ) ;
#47876 = VERTEX_POINT ( 'NONE', #71240 ) ;
#47875 = DIRECTION ( 'NONE',  ( -0.000000000000000000, 1.000000000000000000, -0.000000000000000000 ) ) ;
#47877 = DIRECTION ( 'NONE',  ( 1.000000000000000000, -0.000000000000000000, -0.000000000000000000 ) ) ;
#47878 = VECTOR ( 'NONE', #216592, 1000.000000000000000 ) ;
#47879 = TOROIDAL_SURFACE ( 'NONE', #193654, 11.65000000000000036, 0.1000000000000000056 ) ;
#47880 = CARTESIAN_POINT ( 'NONE',  ( -14.11361717019516071, 62.94602368561173478, -215.5245807872942976 ) ) ;
#47881 = EDGE_CURVE ( 'NONE', #113090, #153266, #255764, .T. ) ;
#47882 = CARTESIAN_POINT ( 'NONE',  ( -20.94999999999999929, 5.850000000011105428, -43.63249722427797650 ) ) ;
#47883 = VERTEX_POINT ( 'NONE', #131183 ) ;
#47884 = CARTESIAN_POINT ( 'NONE',  ( -20.54999999999999716, 71.65000000001199965, -115.3731074845243256 ) ) ;
#47885 = CARTESIAN_POINT ( 'NONE',  ( 18.52130828395273099, 85.48139550263810804, -162.9986007606406702 ) ) ;
#47887 = ORIENTED_EDGE ( 'NONE', *, *, #148497, .F. ) ;
#47886 = ADVANCED_FACE ( 'NONE', ( #171643 ), #176757, .F. ) ;
#47889 = ADVANCED_FACE ( 'NONE', ( #136296 ), #80168, .T. ) ;
#47888 = DIRECTION ( 'NONE',  ( 1.000000000000000000, 0.000000000000000000, 0.000000000000000000 ) ) ;
#47890 = VERTEX_POINT ( 'NONE', #39827 ) ;
#47891 =( BOUNDED_SURFACE ( )  B_SPLINE_SURFACE ( 3, 2, ( 
 ( #222969, #146004, #203427 ),
 ( #185141, #224255, #205988 ),
 ( #165594, #225518, #3937 ),
 ( #182591, #243822, #6490 ),
 ( #106872, #24816, #247682 ),
 ( #86003, #84713, #88585 ) ),
 .UNSPECIFIED., .F., .F., .F. ) 
 B_SPLINE_SURFACE_WITH_KNOTS ( ( 4, 2, 4 ),
 ( 3, 3 ),
 ( 4.712388980384689674, 5.497787143782137953, 6.283185307179586232 ),
 ( 0.000000000000000000, 1.000000000000000000 ),
 .UNSPECIFIED. ) 
 GEOMETRIC_REPRESENTATION_ITEM ( )  RATIONAL_B_SPLINE_SURFACE ( (
 ( 1.000000000000000000, 0.7071067811865475727, 1.000000000000000000),
 ( 1.000000000000000000, 0.7727932973487947610, 1.000000000000000000),
 ( 1.000000000000000000, 0.8282379607654274389, 1.000000000000000000),
 ( 1.000000000000000000, 0.9038128468035014906, 1.000000000000000000),
 ( 1.000000000000000000, 0.9240297172246950685, 1.000000000000000000),
 ( 1.000000000000000000, 0.9238795325112961754, 1.000000000000000000) ) ) 
 REPRESENTATION_ITEM ( '' )  SURFACE ( )  );
#47892 = ADVANCED_FACE ( 'NONE', ( #58050 ), #205911, .T. ) ;
#47893 = LINE ( 'NONE', #88285, #125134 ) ;
#47895 = ORIENTED_EDGE ( 'NONE', *, *, #155300, .F. ) ;
#47894 = CARTESIAN_POINT ( 'NONE',  ( -23.15000000000000213, 46.23295349378772556, -240.7147059833253309 ) ) ;
#47896 = EDGE_CURVE ( 'NONE', #131063, #46944, #200162, .T. ) ;
#47897 = EDGE_CURVE ( 'NONE', #193798, #107947, #43425, .T. ) ;
#47900 = ORIENTED_EDGE ( 'NONE', *, *, #218872, .F. ) ;
#47899 = ORIENTED_EDGE ( 'NONE', *, *, #193638, .T. ) ;
#47898 = LINE ( 'NONE', #83145, #180355 ) ;
#47901 = CIRCLE ( 'NONE', #193676, 0.09999999999998898659 ) ;
#47902 = DIRECTION ( 'NONE',  ( 1.000000000000000000, 0.000000000000000000, 0.000000000000000000 ) ) ;
#47903 = FACE_BOUND ( 'NONE', #97171, .T. ) ;
#47904 = CIRCLE ( 'NONE', #193681, 0.3999999999999890310 ) ;
#47905 = DIRECTION ( 'NONE',  ( 0.000000000000000000, 0.000000000000000000, 1.000000000000000000 ) ) ;
#47907 = CARTESIAN_POINT ( 'NONE',  ( 20.27550659511088682, 9.216043722520002035, -109.7500000000000426 ) ) ;
#47906 = CARTESIAN_POINT ( 'NONE',  ( -11.60000000000000320, -8.250000000000005329, 10.95857864376268864 ) ) ;
#47908 = DIRECTION ( 'NONE',  ( -1.000000000000000000, 0.000000000000000000, 0.000000000000000000 ) ) ;
#47909 = CARTESIAN_POINT ( 'NONE',  ( 23.15000000000000213, 28.06530170954950165, -259.0287255139427884 ) ) ;
#47910 = DIRECTION ( 'NONE',  ( -1.000000000000000000, 0.000000000000000000, 0.000000000000000000 ) ) ;
#47911 = CARTESIAN_POINT ( 'NONE',  ( -21.29999999999995808, 76.00000000001168132, -73.57310748452432847 ) ) ;
#47912 = EDGE_LOOP ( 'NONE', ( #179348, #93806, #52684, #152424 ) ) ;
#47914 = ORIENTED_EDGE ( 'NONE', *, *, #172092, .T. ) ;
#47913 = AXIS2_PLACEMENT_3D ( 'NONE', #232317, #251845, #91502 ) ;
#47915 = CARTESIAN_POINT ( 'NONE',  ( 18.59999999999999787, -1.835341550213255957, -112.0551512925630107 ) ) ;
#47916 = AXIS2_PLACEMENT_3D ( 'NONE', #12417, #89344, #29428 ) ;
#47918 = ORIENTED_EDGE ( 'NONE', *, *, #79356, .T. ) ;
#47917 = LINE ( 'NONE', #25800, #182769 ) ;
#47919 = EDGE_LOOP ( 'NONE', ( #29343, #9848, #104594, #257752 ) ) ;
#47920 = DIRECTION ( 'NONE',  ( 2.715809747126116015E-16, 0.9651348961777156399, -0.2617529984165029577 ) ) ;
#47921 = ORIENTED_EDGE ( 'NONE', *, *, #227679, .F. ) ;
#47922 = LINE ( 'NONE', #8816, #150244 ) ;
#47923 = AXIS2_PLACEMENT_3D ( 'NONE', #103436, #108597, #9491 ) ;
#47924 = EDGE_LOOP ( 'NONE', ( #174326, #54841, #193144, #18808 ) ) ;
#47925 = AXIS2_PLACEMENT_3D ( 'NONE', #241706, #26527, #5632 ) ;
#47926 = DIRECTION ( 'NONE',  ( 1.000000000000000000, 0.000000000000000000, 0.000000000000000000 ) ) ;
#47927 = DIRECTION ( 'NONE',  ( 1.000000000000000000, 0.000000000000000000, 0.000000000000000000 ) ) ;
#47928 = VECTOR ( 'NONE', #217463, 1000.000000000000000 ) ;
#47930 = EDGE_LOOP ( 'NONE', ( #182577, #20003, #215934, #249879 ) ) ;
#47929 = ORIENTED_EDGE ( 'NONE', *, *, #33728, .F. ) ;
#47931 = EDGE_LOOP ( 'NONE', ( #181341, #134228, #163971, #216047 ) ) ;
#47932 = DIRECTION ( 'NONE',  ( 0.000000000000000000, 0.4721928772778128947, 0.8814952561688012000 ) ) ;
#47933 = VERTEX_POINT ( 'NONE', #98435 ) ;
#47934 = EDGE_LOOP ( 'NONE', ( #41864, #249862, #172130 ) ) ;
#47935 = DIRECTION ( 'NONE',  ( 0.000000000000000000, 0.000000000000000000, 1.000000000000000000 ) ) ;
#47936 = DIRECTION ( 'NONE',  ( 1.000000000000000000, -0.000000000000000000, 0.000000000000000000 ) ) ;
#47937 = DIRECTION ( 'NONE',  ( 1.000000000000000000, 0.000000000000000000, 0.000000000000000000 ) ) ;
#47939 = ORIENTED_EDGE ( 'NONE', *, *, #101204, .F. ) ;
#47938 = CARTESIAN_POINT ( 'NONE',  ( 18.59999999999999076, -1.164121893230052995, -74.91484808557160591 ) ) ;
#47940 = CIRCLE ( 'NONE', #172902, 0.1000000000000026007 ) ;
#47941 = CARTESIAN_POINT ( 'NONE',  ( -23.25000000000000355, 11.74999999999998224, -9.250000000000001776 ) ) ;
#47942 = CARTESIAN_POINT ( 'NONE',  ( -18.40000000000000213, 11.74999999999998224, -20.85000000000000142 ) ) ;
#47944 = EDGE_LOOP ( 'NONE', ( #239636, #167197, #54004, #49061 ) ) ;
#47943 = DIRECTION ( 'NONE',  ( 0.000000000000000000, 0.3427706569149662763, -0.9394191166662954062 ) ) ;
#47945 = CARTESIAN_POINT ( 'NONE',  ( -18.50000000000000000, 11.65000000001115232, -146.2500000000000284 ) ) ;
#47946 = ORIENTED_EDGE ( 'NONE', *, *, #175147, .F. ) ;
#47947 = CARTESIAN_POINT ( 'NONE',  ( -16.89268316805466341, 60.93619025550653134, -221.0468289635910537 ) ) ;
#47948 = ORIENTED_EDGE ( 'NONE', *, *, #134216, .F. ) ;
#47949 = DIRECTION ( 'NONE',  ( 1.000000000000000000, 0.000000000000000000, 0.000000000000000000 ) ) ;
#47951 = EDGE_CURVE ( 'NONE', #192532, #21708, #189179, .T. ) ;
#47950 = DIRECTION ( 'NONE',  ( -1.000000000000000000, -3.265361837132813093E-16, 0.000000000000000000 ) ) ;
#47952 = EDGE_LOOP ( 'NONE', ( #255619, #228541, #258016, #234877 ) ) ;
#47954 = LINE ( 'NONE', #207048, #207946 ) ;
#47953 = CYLINDRICAL_SURFACE ( 'NONE', #123787, 0.1000000000000021844 ) ;
#47955 = EDGE_CURVE ( 'NONE', #70299, #158625, #135159, .T. ) ;
#47956 = FACE_OUTER_BOUND ( 'NONE', #91205, .T. ) ;
#47957 = VECTOR ( 'NONE', #101118, 1000.000000000000000 ) ;
#47958 = DIRECTION ( 'NONE',  ( 1.000000000000000000, 0.000000000000000000, 0.000000000000000000 ) ) ;
#47959 = VECTOR ( 'NONE', #25374, 1000.000000000000114 ) ;
#47960 = DIRECTION ( 'NONE',  ( 1.000000000000000000, -3.265361837132813093E-16, -2.280189983783949500E-30 ) ) ;
#47961 = VERTEX_POINT ( 'NONE', #257496 ) ;
#47962 = ORIENTED_EDGE ( 'NONE', *, *, #244745, .T. ) ;
#47963 = EDGE_CURVE ( 'NONE', #17316, #241355, #72172, .T. ) ;
#47964 = SPHERICAL_SURFACE ( 'NONE', #234401, 0.1000000000000000056 ) ;
#47966 = EDGE_CURVE ( 'NONE', #167063, #43942, #143371, .T. ) ;
#47965 = CARTESIAN_POINT ( 'NONE',  ( 21.05000000000000071, 9.290509600414956992, -221.0404682250134840 ) ) ;
#47967 = ORIENTED_EDGE ( 'NONE', *, *, #26440, .F. ) ;
#47968 = CARTESIAN_POINT ( 'NONE',  ( 20.94999999999999929, -1.162701749926853712, -41.40000000000000568 ) ) ;
#47969 = ORIENTED_EDGE ( 'NONE', *, *, #144972, .F. ) ;
#47970 = CARTESIAN_POINT ( 'NONE',  ( -20.94999999999999929, 74.73821383144657204, -61.43660852097884373 ) ) ;
#47971 = VERTEX_POINT ( 'NONE', #95902 ) ;
#47972 = DIRECTION ( 'NONE',  ( 1.000000000000000000, -1.772924042024179204E-16, 4.808324575169891715E-17 ) ) ;
#47973 = FACE_OUTER_BOUND ( 'NONE', #10314, .T. ) ;
#47974 = CARTESIAN_POINT ( 'NONE',  ( 21.05000000000000071, -11.39257802169451139, -164.4260504201680817 ) ) ;
#47975 = ORIENTED_EDGE ( 'NONE', *, *, #19029, .F. ) ;
#47976 = CARTESIAN_POINT ( 'NONE',  ( 18.60000000000000142, -9.480686695267790398, -207.9411151687578183 ) ) ;
#47977 = SURFACE_SIDE_STYLE ('',( #166686 ) ) ;
#47978 = VECTOR ( 'NONE', #90608, 1000.000000000000000 ) ;
#47979 = EDGE_CURVE ( 'NONE', #246766, #146445, #175476, .T. ) ;
#47980 = VERTEX_POINT ( 'NONE', #56752 ) ;
#47981 = VERTEX_POINT ( 'NONE', #158490 ) ;
#47982 = EDGE_CURVE ( 'NONE', #171414, #212664, #234136, .T. ) ;
#47983 = ORIENTED_EDGE ( 'NONE', *, *, #39965, .F. ) ;
#47984 = CARTESIAN_POINT ( 'NONE',  ( 22.49999999999999645, 64.35042919246734527, -136.6231074845243825 ) ) ;
#47985 = DIRECTION ( 'NONE',  ( 0.000000000000000000, -0.9651348961777157509, 0.2617529984165031243 ) ) ;
#47986 = CIRCLE ( 'NONE', #102122, 0.09999999999999939493 ) ;
#47987 = LINE ( 'NONE', #45430, #184040 ) ;
#47988 = DIRECTION ( 'NONE',  ( 0.000000000000000000, 0.000000000000000000, -1.000000000000000000 ) ) ;
#47989 = CARTESIAN_POINT ( 'NONE',  ( 20.94999999999999574, 14.00000000001115730, -139.4270925303825663 ) ) ;
#47991 = DIRECTION ( 'NONE',  ( 0.000000000000000000, -0.1332476588733589040, -0.9910827722268048534 ) ) ;
#47990 = CARTESIAN_POINT ( 'NONE',  ( -20.94999999999999929, 0.7653315920341953182, -212.6731560895497353 ) ) ;
#47993 = ORIENTED_EDGE ( 'NONE', *, *, #253079, .F. ) ;
#47992 = DIRECTION ( 'NONE',  ( -1.000000000000000000, 0.000000000000000000, 0.000000000000000000 ) ) ;
#47994 = CARTESIAN_POINT ( 'NONE',  ( 18.39999999999999503, 45.89348038176515843, -239.2231437130149061 ) ) ;
#47995 = ORIENTED_EDGE ( 'NONE', *, *, #226399, .F. ) ;
#47996 = DIRECTION ( 'NONE',  ( 0.000000000000000000, 0.000000000000000000, -1.000000000000000000 ) ) ;
#47997 = VERTEX_POINT ( 'NONE', #76332 ) ;
#47998 = VERTEX_POINT ( 'NONE', #237982 ) ;
#47999 = CARTESIAN_POINT ( 'NONE',  ( -23.25000000000000000, 11.75000000000000000, -33.50000000000000000 ) ) ;
#48000 = DIRECTION ( 'NONE',  ( -1.000000000000000000, 0.000000000000000000, -0.000000000000000000 ) ) ;
#48001 = EDGE_CURVE ( 'NONE', #35976, #109724, #180984, .T. ) ;
#48002 = DIRECTION ( 'NONE',  ( 0.000000000000000000, 0.000000000000000000, 1.000000000000000000 ) ) ;
#48003 = EDGE_CURVE ( 'NONE', #50777, #185233, #93474, .T. ) ;
#48004 = AXIS2_PLACEMENT_3D ( 'NONE', #158291, #115272, #56546 ) ;
#48005 = CIRCLE ( 'NONE', #114647, 0.1000000000000028644 ) ;
#48006 = CARTESIAN_POINT ( 'NONE',  ( -21.04999999999994387, 65.36599112033563586, -30.02023607076051803 ) ) ;
#48007 = ORIENTED_EDGE ( 'NONE', *, *, #23705, .F. ) ;
#48008 = ORIENTED_EDGE ( 'NONE', *, *, #15366, .T. ) ;
#48009 = LINE ( 'NONE', #106689, #82308 ) ;
#48010 = ORIENTED_EDGE ( 'NONE', *, *, #203075, .F. ) ;
#48011 = CARTESIAN_POINT ( 'NONE',  ( -23.49999999999994316, 84.00000000001119815, -37.18565239344504647 ) ) ;
#48012 = DIRECTION ( 'NONE',  ( 0.000000000000000000, 0.2128009952263618110, -0.9770955615653311721 ) ) ;
#48013 = ORIENTED_EDGE ( 'NONE', *, *, #122043, .F. ) ;
#48014 = CARTESIAN_POINT ( 'NONE',  ( -22.39999999999999858, 64.35000000001166143, -69.62310748452439668 ) ) ;
#48015 = DIRECTION ( 'NONE',  ( 0.000000000000000000, -0.1686199900910312910, 0.9856811345164826488 ) ) ;
#48016 = CARTESIAN_POINT ( 'NONE',  ( -16.87242674293850087, 66.05000000001209060, -123.8741977308967250 ) ) ;
#48018 = EDGE_CURVE ( 'NONE', #127278, #113415, #72663, .T. ) ;
#48017 = DIRECTION ( 'NONE',  ( 1.000000000000000000, 0.000000000000000000, 0.000000000000000000 ) ) ;
#48019 = VERTEX_POINT ( 'NONE', #214570 ) ;
#48020 = CARTESIAN_POINT ( 'NONE',  ( -11.60000000000000320, -11.65000000000000036, 15.00000000000000355 ) ) ;
#48021 = CARTESIAN_POINT ( 'NONE',  ( 18.79999999999999716, 11.49641995933507843, -1.885425182446133885 ) ) ;
#48022 = CARTESIAN_POINT ( 'NONE',  ( -23.15000000000000213, 60.15036700252697699, -246.1091865931380482 ) ) ;
#48023 = ADVANCED_FACE ( 'NONE', ( #35960 ), #24114, .F. ) ;
#48024 = DIRECTION ( 'NONE',  ( 1.000000000000000000, 0.000000000000000000, 0.000000000000000000 ) ) ;
#48025 = CARTESIAN_POINT ( 'NONE',  ( -20.85000000000000142, 11.75000000001115197, -160.6583993101029364 ) ) ;
#48026 = AXIS2_PLACEMENT_3D ( 'NONE', #217866, #61386, #140936 ) ;
#48027 = ADVANCED_FACE ( 'NONE', ( #61935 ), #67071, .F. ) ;
#48028 = CARTESIAN_POINT ( 'NONE',  ( 21.05000000000000071, 1.115600667400684642E-11, -67.00000000000004263 ) ) ;
#48029 = VECTOR ( 'NONE', #191546, 1000.000000000000000 ) ;
#48030 = AXIS2_PLACEMENT_3D ( 'NONE', #210332, #34284, #190791 ) ;
#48031 = AXIS2_PLACEMENT_3D ( 'NONE', #252933, #130425, #169609 ) ;
#48032 = ORIENTED_EDGE ( 'NONE', *, *, #193726, .T. ) ;
#48033 = CARTESIAN_POINT ( 'NONE',  ( 20.94999999999999929, 1.115600667400684642E-11, -200.9999999999999432 ) ) ;
#48034 = ORIENTED_EDGE ( 'NONE', *, *, #215391, .F. ) ;
#48035 = ADVANCED_FACE ( 'NONE', ( #164888 ), #104863, .T. ) ;
#48036 = DIRECTION ( 'NONE',  ( -2.952720810173289112E-16, -0.4088369013363282733, 0.9126074666063769270 ) ) ;
#48037 = DIRECTION ( 'NONE',  ( -1.000000000000000000, 0.000000000000000000, 0.000000000000000000 ) ) ;
#48038 = DIRECTION ( 'NONE',  ( 0.000000000000000000, 0.2617529984165030132, 0.9651348961777157509 ) ) ;
#48039 = FACE_OUTER_BOUND ( 'NONE', #21692, .T. ) ;
#48041 = VERTEX_POINT ( 'NONE', #44941 ) ;
#48040 = B_SPLINE_CURVE_WITH_KNOTS ( 'NONE', 3,
 ( #140441, #236997, #57034, #40107 ),
 .UNSPECIFIED., .F., .F.,
 ( 4, 4 ),
 ( 0.000000000000000000, 0.0002118541922231925311 ),
 .UNSPECIFIED. ) ;
#48042 = CARTESIAN_POINT ( 'NONE',  ( -20.64999999999999858, 1.148907358139439339E-11, -201.0000000000015064 ) ) ;
#48043 = EDGE_CURVE ( 'NONE', #209230, #86653, #226758, .T. ) ;
#48044 = DIRECTION ( 'NONE',  ( 0.000000000000000000, -1.000000000000000000, -6.982962677686265922E-15 ) ) ;
#48045 = CARTESIAN_POINT ( 'NONE',  ( 18.59999999999999076, 46.45388641681647357, -243.1520440498138385 ) ) ;
#48046 = DIRECTION ( 'NONE',  ( 3.469446951953515108E-14, -1.000000000000000000, 0.000000000000000000 ) ) ;
#48047 = CARTESIAN_POINT ( 'NONE',  ( -21.08479644141222664, 69.65496134228050096, -170.0816619270885610 ) ) ;
#48048 = CIRCLE ( 'NONE', #152125, 0.09999999999998898659 ) ;
#48049 = CARTESIAN_POINT ( 'NONE',  ( -2.995603634470884209E-16, -11.74999999998884448, -45.75000000000000711 ) ) ;
#48050 = CIRCLE ( 'NONE', #43769, 0.09999999999999939493 ) ;
#48051 = CIRCLE ( 'NONE', #235298, 12.97499999999998721 ) ;
#48052 = VERTEX_POINT ( 'NONE', #224845 ) ;
#48053 = ORIENTED_EDGE ( 'NONE', *, *, #111805, .T. ) ;
#48054 = CARTESIAN_POINT ( 'NONE',  ( -22.39999999999999858, 76.10000000001203091, -114.6726782920691079 ) ) ;
#48055 = CARTESIAN_POINT ( 'NONE',  ( -18.59999999999999787, 68.92903212821283887, -65.77654326265606244 ) ) ;
#48056 = CARTESIAN_POINT ( 'NONE',  ( 21.05000000000000071, 49.53130139001177668, -254.0846532093228802 ) ) ;
#48057 = CARTESIAN_POINT ( 'NONE',  ( 18.49999999999998934, 65.75000000001149658, -44.77310748452439526 ) ) ;
#48058 = CARTESIAN_POINT ( 'NONE',  ( -22.47007471830799474, 68.27928934808589645, -170.0231074845244450 ) ) ;
#48059 = EDGE_LOOP ( 'NONE', ( #248540, #156082, #246450, #214660 ) ) ;
#48060 = FACE_OUTER_BOUND ( 'NONE', #119101, .T. ) ;
#48061 = AXIS2_PLACEMENT_3D ( 'NONE', #108733, #228700, #90439 ) ;
#48062 = ITEM_DEFINED_TRANSFORMATION ( 'NONE', 'NONE', #144408,  #2425 ) ;
#48063 = VECTOR ( 'NONE', #176451, 1000.000000000000000 ) ;
#48064 = CIRCLE ( 'NONE', #27262, 0.3999999999999975797 ) ;
#48065 = CARTESIAN_POINT ( 'NONE',  ( 23.14999999999999858, -3.899999999988843502, -200.9999999999999432 ) ) ;
#48066 = ORIENTED_EDGE ( 'NONE', *, *, #161715, .F. ) ;
#48067 = CARTESIAN_POINT ( 'NONE',  ( 18.59999999999998366, 0.000000000000000000, -33.50000000000000000 ) ) ;
#48068 = CIRCLE ( 'NONE', #193826, 0.09999999999999939493 ) ;
#48069 = EDGE_LOOP ( 'NONE', ( #81869, #159733, #135842, #212602 ) ) ;
#48071 = ORIENTED_EDGE ( 'NONE', *, *, #148886, .T. ) ;
#48070 = AXIS2_PLACEMENT_3D ( 'NONE', #9411, #185495, #29032 ) ;
#48072 = ORIENTED_EDGE ( 'NONE', *, *, #212472, .T. ) ;
#48073 = LINE ( 'NONE', #147174, #101469 ) ;
#48074 = CARTESIAN_POINT ( 'NONE',  ( -18.59999999999999787, 9.250000000011157297, -45.75000000000000000 ) ) ;
#48075 = CYLINDRICAL_SURFACE ( 'NONE', #228376, 0.09999999999998898659 ) ;
#48076 = CIRCLE ( 'NONE', #252092, 0.09999999999999939493 ) ;
#48077 = CARTESIAN_POINT ( 'NONE',  ( -21.13614978966382196, 69.50089529817815048, -103.0231074845243739 ) ) ;
#48078 = CARTESIAN_POINT ( 'NONE',  ( -20.64999999999999858, 78.37638820354418101, -229.1444560783390898 ) ) ;
#48079 = CARTESIAN_POINT ( 'NONE',  ( -20.54999999999999716, 71.65000000001222702, -148.8731074845244109 ) ) ;
#48080 = LINE ( 'NONE', #127627, #34966 ) ;
#48082 = DIRECTION ( 'NONE',  ( 0.000000000000000000, 0.000000000000000000, -1.000000000000000000 ) ) ;
#48081 = CARTESIAN_POINT ( 'NONE',  ( 20.95556889135987788, 65.37805641227680553, -95.38071326266687322 ) ) ;
#48083 = DIRECTION ( 'NONE',  ( 0.000000000000000000, 0.9553114395362780620, -0.2956011730205483912 ) ) ;
#48084 = CARTESIAN_POINT ( 'NONE',  ( -16.88815647973234135, 9.950832619326892114, -113.1472170633260390 ) ) ;
#48085 = DIRECTION ( 'NONE',  ( 0.000000000000000000, 4.440892098500570153E-15, -1.000000000000000000 ) ) ;
#48086 = DIRECTION ( 'NONE',  ( 0.000000000000000000, 6.982962677686266711E-15, -1.000000000000000000 ) ) ;
#48087 = ORIENTED_EDGE ( 'NONE', *, *, #202822, .F. ) ;
#48088 = EDGE_LOOP ( 'NONE', ( #66403, #228808, #211333, #53364 ) ) ;
#48089 = LINE ( 'NONE', #63812, #60928 ) ;
#48090 = CARTESIAN_POINT ( 'NONE',  ( 20.85000000000000142, 11.65000000001115943, -100.5000000000000426 ) ) ;
#48092 = DIRECTION ( 'NONE',  ( -0.000000000000000000, 1.000000000000000000, 2.891205793294679805E-16 ) ) ;
#48091 = DIRECTION ( 'NONE',  ( 0.000000000000000000, 0.000000000000000000, -1.000000000000000000 ) ) ;
#48093 = LINE ( 'NONE', #187631, #251867 ) ;
#48094 = CARTESIAN_POINT ( 'NONE',  ( 20.94999999999999929, 76.00000000001190870, -103.0231074845243029 ) ) ;
#48096 = EDGE_CURVE ( 'NONE', #207310, #119594, #114334, .T. ) ;
#48095 = CARTESIAN_POINT ( 'NONE',  ( -20.54999999999999716, 36.65892442174935439, -249.5511627012433848 ) ) ;
#48097 = ORIENTED_EDGE ( 'NONE', *, *, #251535, .T. ) ;
#48098 = ORIENTED_EDGE ( 'NONE', *, *, #139375, .T. ) ;
#48099 = CIRCLE ( 'NONE', #39762, 0.1000000000000106498 ) ;
#48100 = EDGE_CURVE ( 'NONE', #79366, #46322, #125743, .T. ) ;
#48101 = EDGE_CURVE ( 'NONE', #88561, #200905, #146576, .T. ) ;
#48102 = CIRCLE ( 'NONE', #235353, 0.1000000000000028227 ) ;
#48103 = CARTESIAN_POINT ( 'NONE',  ( 18.79999999999999716, 11.49641995933507843, 1.885425182446133885 ) ) ;
#48104 = ORIENTED_EDGE ( 'NONE', *, *, #161592, .F. ) ;
#48105 = LINE ( 'NONE', #226739, #243108 ) ;
#48106 = AXIS2_PLACEMENT_3D ( 'NONE', #76382, #112971, #232938 ) ;
#48107 = DIRECTION ( 'NONE',  ( 1.000000000000000000, 0.000000000000000000, 0.000000000000000000 ) ) ;
#48108 = VECTOR ( 'NONE', #217839, 1000.000000000000000 ) ;
#48109 = AXIS2_PLACEMENT_3D ( 'NONE', #56001, #215107, #36499 ) ;
#48110 = VERTEX_POINT ( 'NONE', #85315 ) ;
#48111 = CARTESIAN_POINT ( 'NONE',  ( 18.59999999999997655, 8.809961202382808665, -241.4517562488062481 ) ) ;
#48112 = EDGE_CURVE ( 'NONE', #242376, #255891, #164239, .T. ) ;
#48113 = EDGE_LOOP ( 'NONE', ( #8678, #23738, #67150, #31602 ) ) ;
#48115 = VECTOR ( 'NONE', #100812, 1000.000000000000000 ) ;
#48114 = CARTESIAN_POINT ( 'NONE',  ( 20.04142135623730070, 61.57587952878035509, -212.2000740415318774 ) ) ;
#48116 = FACE_OUTER_BOUND ( 'NONE', #11567, .T. ) ;
#48117 = DIRECTION ( 'NONE',  ( 0.000000000000000000, 0.000000000000000000, 1.000000000000000000 ) ) ;
#48118 = DIRECTION ( 'NONE',  ( 0.000000000000000000, 0.3116596277708286733, 0.9501938099239273239 ) ) ;
#48119 = DIRECTION ( 'NONE',  ( 0.000000000000000000, 0.000000000000000000, 1.000000000000000000 ) ) ;
#48120 = CARTESIAN_POINT ( 'NONE',  ( 18.59999999999999432, 2.859758780633683273, -208.6670499591424459 ) ) ;
#48121 = DIRECTION ( 'NONE',  ( 1.000000000000000000, 0.000000000000000000, 0.000000000000000000 ) ) ;
#48122 = CARTESIAN_POINT ( 'NONE',  ( 20.27550659511088682, 9.216043722508844738, -9.250000000000001776 ) ) ;
#48124 = VERTEX_POINT ( 'NONE', #241844 ) ;
#48123 = CARTESIAN_POINT ( 'NONE',  ( 18.37172112093794851, -0.7723029343291464288, -242.4300124561790426 ) ) ;
#48126 = DIRECTION ( 'NONE',  ( 0.000000000000000000, 1.000000000000000000, 0.000000000000000000 ) ) ;
#48125 = CARTESIAN_POINT ( 'NONE',  ( -23.15000000000000213, 67.23127455305835554, -235.8551265064784559 ) ) ;
#48127 = ORIENTED_EDGE ( 'NONE', *, *, #47874, .F. ) ;
#48129 = ORIENTED_EDGE ( 'NONE', *, *, #68707, .T. ) ;
#48128 = CARTESIAN_POINT ( 'NONE',  ( -16.97683809663752186, 66.05000000001183480, -82.92547150272069700 ) ) ;
#48130 = ORIENTED_EDGE ( 'NONE', *, *, #190809, .F. ) ;
#48131 = LINE ( 'NONE', #243773, #99095 ) ;
#48132 = DIRECTION ( 'NONE',  ( 0.000000000000000000, 0.000000000000000000, -1.000000000000000000 ) ) ;
#48133 = EDGE_CURVE ( 'NONE', #108161, #132399, #51766, .T. ) ;
#48135 = EDGE_CURVE ( 'NONE', #68538, #257538, #150186, .T. ) ;
#48134 = CARTESIAN_POINT ( 'NONE',  ( 20.85000000000000142, 77.83585931145570669, -125.0186683157258045 ) ) ;
#48136 = DIRECTION ( 'NONE',  ( 0.000000000000000000, 0.000000000000000000, 1.000000000000000000 ) ) ;
#48138 = LINE ( 'NONE', #125130, #223020 ) ;
#48137 = CIRCLE ( 'NONE', #135611, 12.97499999999999076 ) ;
#48139 = CARTESIAN_POINT ( 'NONE',  ( -20.54999999999999716, 71.75000000001259082, -191.1731074845243654 ) ) ;
#48140 = CARTESIAN_POINT ( 'NONE',  ( 23.24999999999999645, 28.08470566095357057, -239.2860081655328770 ) ) ;
#48141 = DIRECTION ( 'NONE',  ( 0.000000000000000000, -0.08413937888704772772, 0.9964539953858893018 ) ) ;
#48142 = EDGE_CURVE ( 'NONE', #255181, #91499, #121917, .T. ) ;
#48143 = DIRECTION ( 'NONE',  ( 0.000000000000000000, 0.8814952561688429444, -0.4721928772777347350 ) ) ;
#48144 = VERTEX_POINT ( 'NONE', #162334 ) ;
#48145 = EDGE_LOOP ( 'NONE', ( #150547, #247648, #340, #47914 ) ) ;
#48146 = DIRECTION ( 'NONE',  ( 0.000000000000000000, -0.1350103645451974088, 0.9908441862701587999 ) ) ;
#48147 = CIRCLE ( 'NONE', #89832, 11.80000000000000426 ) ;
#48148 = ORIENTED_EDGE ( 'NONE', *, *, #167238, .F. ) ;
#48149 = VECTOR ( 'NONE', #168462, 1000.000000000000000 ) ;
#48150 = CARTESIAN_POINT ( 'NONE',  ( -18.50000000000000000, -1.164121893230052995, -108.2148480855716457 ) ) ;
#48151 = ORIENTED_EDGE ( 'NONE', *, *, #109051, .T. ) ;
#48152 = CARTESIAN_POINT ( 'NONE',  ( -23.25000000000000000, 59.16775194334852728, -221.0793150863668473 ) ) ;
#48153 = CARTESIAN_POINT ( 'NONE',  ( 22.39999999999999503, 11.65000000001116298, -134.1000000000000227 ) ) ;
#48154 = CARTESIAN_POINT ( 'NONE',  ( -22.39999999999999858, 1.115600667400684642E-11, -94.25000000000002842 ) ) ;
#48155 = DIRECTION ( 'NONE',  ( 0.000000000000000000, -1.000000000000000000, 0.000000000000000000 ) ) ;
#48156 = CARTESIAN_POINT ( 'NONE',  ( 21.13461538461538325, 43.58999342716158765, -234.8150793036844846 ) ) ;
#48157 = EDGE_LOOP ( 'NONE', ( #13081, #74460, #11329, #19681 ) ) ;
#48158 = EDGE_CURVE ( 'NONE', #144252, #150585, #89381, .T. ) ;
#48159 = DIRECTION ( 'NONE',  ( 0.000000000000000000, 0.000000000000000000, -1.000000000000000000 ) ) ;
#48160 = DIRECTION ( 'NONE',  ( -0.000000000000000000, 1.000000000000000000, -0.000000000000000000 ) ) ;
#48161 = CARTESIAN_POINT ( 'NONE',  ( 18.49351773456752213, 85.44302569515704704, -62.33778195849721016 ) ) ;
#48162 = DIRECTION ( 'NONE',  ( 1.000000000000000000, 1.159508501126949290E-16, 2.525285885220369759E-17 ) ) ;
#48163 = ORIENTED_EDGE ( 'NONE', *, *, #217152, .T. ) ;
#48164 = VECTOR ( 'NONE', #74660, 1000.000000000000000 ) ;
#48166 = CARTESIAN_POINT ( 'NONE',  ( -23.25000000000000000, 64.25000000001142553, -36.02310748452440237 ) ) ;
#48165 = CARTESIAN_POINT ( 'NONE',  ( 21.07928932188134397, 61.09751618602743406, -234.2940654522722639 ) ) ;
#48167 = EDGE_LOOP ( 'NONE', ( #255064, #182450, #109313 ) ) ;
#48170 = ORIENTED_EDGE ( 'NONE', *, *, #154682, .F. ) ;
#48169 = CARTESIAN_POINT ( 'NONE',  ( -16.79140778683514057, 51.60243904148639160, -231.9593695168616421 ) ) ;
#48168 = CARTESIAN_POINT ( 'NONE',  ( 22.16821283564876666, 68.44102665923118423, -103.0231074845243739 ) ) ;
#48171 = ORIENTED_EDGE ( 'NONE', *, *, #141247, .F. ) ;
#48172 = CARTESIAN_POINT ( 'NONE',  ( -16.92209698673559970, 9.950000000011138823, -113.2106355670527478 ) ) ;
#48173 = DIRECTION ( 'NONE',  ( 0.000000000000000000, -0.9126074666063767049, -0.4088369013363286619 ) ) ;
#48174 = EDGE_CURVE ( 'NONE', #38637, #196915, #214306, .T. ) ;
#48175 = CARTESIAN_POINT ( 'NONE',  ( -21.14999999999999858, 76.10000000001222986, -148.1726782920690937 ) ) ;
#48176 = AXIS2_PLACEMENT_3D ( 'NONE', #49055, #208159, #165162 ) ;
#48177 = ORIENTED_EDGE ( 'NONE', *, *, #130897, .F. ) ;
#48179 = EDGE_CURVE ( 'NONE', #203988, #61003, #223836, .T. ) ;
#48178 = DIRECTION ( 'NONE',  ( 0.000000000000000000, 0.8814952561688476074, -0.4721928772777262417 ) ) ;
#48180 = FACE_OUTER_BOUND ( 'NONE', #243054, .T. ) ;
#48181 = ADVANCED_FACE ( 'NONE', ( #149197 ), #10099, .F. ) ;
#48183 = CARTESIAN_POINT ( 'NONE',  ( 0.8999999999999993561, -11.65000000000000036, 26.00000000000000355 ) ) ;
#48182 = DIRECTION ( 'NONE',  ( -1.000000000000000000, 0.000000000000000000, 0.000000000000000000 ) ) ;
#48184 = EDGE_CURVE ( 'NONE', #176585, #9648, #50859, .T. ) ;
#48186 = EDGE_LOOP ( 'NONE', ( #209623, #250278, #238000, #8676 ) ) ;
#48185 = CARTESIAN_POINT ( 'NONE',  ( 20.87155475150661132, 11.75000000001115907, -93.59558652915731614 ) ) ;
#48187 = ORIENTED_EDGE ( 'NONE', *, *, #23916, .F. ) ;
#48188 = CARTESIAN_POINT ( 'NONE',  ( 18.39999999999999503, 45.89348038176515843, -239.2231437130149061 ) ) ;
#48189 = DIRECTION ( 'NONE',  ( -1.000000000000000000, 0.000000000000000000, 0.000000000000000000 ) ) ;
#48190 = EDGE_CURVE ( 'NONE', #219544, #30076, #101841, .T. ) ;
#48191 = AXIS2_PLACEMENT_3D ( 'NONE', #208929, #48566, #191966 ) ;
#48192 = AXIS2_PLACEMENT_3D ( 'NONE', #80406, #196537, #177017 ) ;
#48193 = DIRECTION ( 'NONE',  ( -0.000000000000000000, -0.2617529984165031243, -0.9651348961777157509 ) ) ;
#48195 = ADVANCED_FACE ( 'NONE', ( #89190 ), #218364, .T. ) ;
#48194 = VERTEX_POINT ( 'NONE', #9661 ) ;
#48196 = CARTESIAN_POINT ( 'NONE',  ( -16.87683809663752399, 9.850000000011144508, -187.5976359818036769 ) ) ;
#48197 = CARTESIAN_POINT ( 'NONE',  ( -21.65000000000000213, 7.249999999999983125, -9.250000000000001776 ) ) ;
#48198 = CYLINDRICAL_SURFACE ( 'NONE', #168511, 0.09999999999999939493 ) ;
#48199 = EDGE_CURVE ( 'NONE', #178423, #38202, #60347, .T. ) ;
#48200 = ORIENTED_EDGE ( 'NONE', *, *, #50731, .T. ) ;
#48201 = DIRECTION ( 'NONE',  ( 0.000000000000000000, -0.9908441862701605762, 0.1350103645451835310 ) ) ;
#48202 = ADVANCED_FACE ( 'NONE', ( #53925 ), #56238, .F. ) ;
#48203 = ORIENTED_EDGE ( 'NONE', *, *, #153343, .F. ) ;
#48204 = DIRECTION ( 'NONE',  ( -1.000000000000000000, -0.000000000000000000, -0.000000000000000000 ) ) ;
#48205 = SPHERICAL_SURFACE ( 'NONE', #227171, 0.1000000000000000056 ) ;
#48206 = AXIS2_PLACEMENT_3D ( 'NONE', #50378, #209480, #188630 ) ;
#48207 = EDGE_CURVE ( 'NONE', #194489, #77718, #10304, .T. ) ;
#48208 = EDGE_CURVE ( 'NONE', #166202, #42380, #52631, .T. ) ;
#48209 = VECTOR ( 'NONE', #162574, 1000.000000000000000 ) ;
#48210 = ORIENTED_EDGE ( 'NONE', *, *, #68832, .T. ) ;
#48211 = ORIENTED_EDGE ( 'NONE', *, *, #247706, .F. ) ;
#48212 =( GEOMETRIC_REPRESENTATION_CONTEXT ( 3 ) GLOBAL_UNCERTAINTY_ASSIGNED_CONTEXT ( ( #201743 ) ) GLOBAL_UNIT_ASSIGNED_CONTEXT ( ( #93212, #172805, #194912 ) ) REPRESENTATION_CONTEXT ( 'NONE', 'WORKASPACE' ) );
#48213 = ADVANCED_FACE ( 'NONE', ( #50069 ), #112622, .F. ) ;
#48214 = CARTESIAN_POINT ( 'NONE',  ( -23.25000000000000000, -1.149570369564537842, -141.8159124845019790 ) ) ;
#48215 = ORIENTED_EDGE ( 'NONE', *, *, #168013, .T. ) ;
#48217 = ORIENTED_EDGE ( 'NONE', *, *, #100480, .T. ) ;
#48216 = CARTESIAN_POINT ( 'NONE',  ( -21.78635804494510708, 7.035661485153180017, 0.09900506550767837477 ) ) ;
#48219 = EDGE_CURVE ( 'NONE', #227674, #179110, #43609, .T. ) ;
#48218 = VERTEX_POINT ( 'NONE', #129615 ) ;
#48220 = ADVANCED_FACE ( 'NONE', ( #13524 ), #39551, .F. ) ;
#48222 = ORIENTED_EDGE ( 'NONE', *, *, #175193, .F. ) ;
#48221 = ORIENTED_EDGE ( 'NONE', *, *, #146241, .T. ) ;
#48223 = ADVANCED_FACE ( 'NONE', ( #110042 ), #62409, .T. ) ;
#48224 = CARTESIAN_POINT ( 'NONE',  ( -18.31331870001056217, -9.536294719169665868, -107.3685786909854727 ) ) ;
#48225 = ORIENTED_EDGE ( 'NONE', *, *, #138443, .F. ) ;
#48226 = CARTESIAN_POINT ( 'NONE',  ( 21.08489247129321598, 22.20727474569241977, -231.7386547802595373 ) ) ;
#48227 = DIRECTION ( 'NONE',  ( -1.000000000000000000, 0.000000000000000000, -0.000000000000000000 ) ) ;
#48228 = DIRECTION ( 'NONE',  ( -0.000000000000000000, 0.000000000000000000, 1.000000000000000000 ) ) ;
#48229 =( BOUNDED_SURFACE ( )  B_SPLINE_SURFACE ( 3, 2, ( 
 ( #109913, #112509, #152944 ),
 ( #173812, #229879, #189473 ),
 ( #151655, #212885, #73402 ),
 ( #132058, #172524, #175086 ),
 ( #15992, #10834, #194631 ),
 ( #171235, #211604, #51203 ),
 ( #193327, #90350, #254538 ),
 ( #232466, #35555, #33011 ),
 ( #14711, #169950, #55061 ),
 ( #95493, #192055, #12140 ) ),
 .UNSPECIFIED., .F., .F., .T. ) 
 B_SPLINE_SURFACE_WITH_KNOTS ( ( 4, 2, 2, 2, 4 ),
 ( 3, 3 ),
 ( 0.002161241639767243466, 0.002579950749615821798, 0.002789305304540111181, 0.002893982582002256089, 0.002998659859464400564 ),
 ( 0.000000000000000000, 1.000000000000000000 ),
 .UNSPECIFIED. ) 
 GEOMETRIC_REPRESENTATION_ITEM ( )  RATIONAL_B_SPLINE_SURFACE ( (
 ( 1.000000000000000000, 0.7071067811865475727, 1.000000000000000000),
 ( 1.000000000000000000, 0.7632447400659836401, 1.000000000000000000),
 ( 1.000000000000000000, 0.8158073005114181431, 1.000000000000000000),
 ( 1.000000000000000000, 0.8906973462394581764, 1.000000000000000000),
 ( 1.000000000000000000, 0.9149408947801753733, 1.000000000000000000),
 ( 1.000000000000000000, 0.9493368785275054789, 1.000000000000000000),
 ( 1.000000000000000000, 0.9605194247162225363, 1.000000000000000000),
 ( 1.000000000000000000, 0.9803630264775601288, 1.000000000000000000),
 ( 1.000000000000000000, 0.9900844824275457645, 1.000000000000000000),
 ( 1.000000000000000000, 0.9894588281429267385, 1.000000000000000000) ) ) 
 REPRESENTATION_ITEM ( '' )  SURFACE ( )  );
#48230 =( GEOMETRIC_REPRESENTATION_CONTEXT ( 3 ) GLOBAL_UNCERTAINTY_ASSIGNED_CONTEXT ( ( #246015 ) ) GLOBAL_UNIT_ASSIGNED_CONTEXT ( ( #197710, #36094, #173072 ) ) REPRESENTATION_CONTEXT ( 'NONE', 'WORKASPACE' ) );
#48231 = DIRECTION ( 'NONE',  ( 1.000000000000000000, -0.000000000000000000, -0.000000000000000000 ) ) ;
#48232 = CIRCLE ( 'NONE', #202177, 0.1000000000000002554 ) ;
#48233 = ORIENTED_EDGE ( 'NONE', *, *, #196813, .F. ) ;
#48234 = EDGE_LOOP ( 'NONE', ( #240136, #81587, #236487, #207226, #165582, #35480, #249533, #57741, #240774, #204642, #86484, #67531, #184029, #124267, #25776, #46850, #199703, #55487, #180423, #12315, #63463, #153691, #29731, #81508, #128071, #88696, #219386 ) ) ;
#48235 = DIRECTION ( 'NONE',  ( 1.000000000000000000, 0.000000000000000000, 0.000000000000000000 ) ) ;
#48237 = ORIENTED_EDGE ( 'NONE', *, *, #231615, .T. ) ;
#48236 = CARTESIAN_POINT ( 'NONE',  ( 18.53691006697085797, 63.75418316127379370, -209.3175534518712766 ) ) ;
#48239 = DIRECTION ( 'NONE',  ( 0.000000000000000000, -0.1455152366551721865, -0.9893560106964475187 ) ) ;
#48238 = CIRCLE ( 'NONE', #6540, 0.09999999999998898659 ) ;
#48241 = ORIENTED_EDGE ( 'NONE', *, *, #229122, .F. ) ;
#48240 = LINE ( 'NONE', #208619, #189860 ) ;
#48242 = EDGE_CURVE ( 'NONE', #75851, #255897, #76918, .T. ) ;
#48243 = VERTEX_POINT ( 'NONE', #57760 ) ;
#48244 = LINE ( 'NONE', #166950, #237536 ) ;
#48245 = TOROIDAL_SURFACE ( 'NONE', #227306, 11.65000000000000036, 0.1000000000000000056 ) ;
#48246 = VECTOR ( 'NONE', #60003, 1000.000000000000114 ) ;
#48247 = ORIENTED_EDGE ( 'NONE', *, *, #181449, .T. ) ;
#48248 = CARTESIAN_POINT ( 'NONE',  ( -16.77180007708460252, 9.950000000011137047, -180.1356141189547770 ) ) ;
#48249 = CARTESIAN_POINT ( 'NONE',  ( 21.05000000000000071, 5.000000000011153745, -54.59473398108690390 ) ) ;
#48252 = ORIENTED_EDGE ( 'NONE', *, *, #178726, .F. ) ;
#48251 = ORIENTED_EDGE ( 'NONE', *, *, #75850, .F. ) ;
#48250 = VECTOR ( 'NONE', #249972, 1000.000000000000000 ) ;
#48253 = ORIENTED_EDGE ( 'NONE', *, *, #157233, .F. ) ;
#48254 = DIRECTION ( 'NONE',  ( 0.000000000000000000, 6.982962677686266711E-15, -1.000000000000000000 ) ) ;
#48255 = VERTEX_POINT ( 'NONE', #94323 ) ;
#48256 = AXIS2_PLACEMENT_3D ( 'NONE', #78527, #60248, #156828 ) ;
#48257 = ORIENTED_EDGE ( 'NONE', *, *, #256543, .T. ) ;
#48258 = CARTESIAN_POINT ( 'NONE',  ( 23.14999999999999503, 51.38014393322265505, -230.1906178717505327 ) ) ;
#48260 = ORIENTED_EDGE ( 'NONE', *, *, #20543, .F. ) ;
#48259 = CARTESIAN_POINT ( 'NONE',  ( -20.94999999999999929, 18.86061765788380740, -226.6874733728449485 ) ) ;
#48261 = CARTESIAN_POINT ( 'NONE',  ( -23.25000000000000000, 1.115600667400684642E-11, -33.50000000000000000 ) ) ;
#48262 = AXIS2_PLACEMENT_3D ( 'NONE', #188902, #204598, #246310 ) ;
#48263 = AXIS2_PLACEMENT_3D ( 'NONE', #28864, #91366, #69242 ) ;
#48265 = FACE_OUTER_BOUND ( 'NONE', #116256, .T. ) ;
#48264 = LINE ( 'NONE', #127813, #3160 ) ;
#48266 = CARTESIAN_POINT ( 'NONE',  ( -20.54999999999999716, 2.000000000011154189, -147.2246219227621111 ) ) ;
#48267 = CARTESIAN_POINT ( 'NONE',  ( -12.29659703204452370, 62.46518123923912214, -217.6854569796042540 ) ) ;
#48268 = ORIENTED_EDGE ( 'NONE', *, *, #187071, .F. ) ;
#48269 = ORIENTED_EDGE ( 'NONE', *, *, #93210, .T. ) ;
#48270 = DIRECTION ( 'NONE',  ( -0.000000000000000000, -6.982962677686266711E-15, 1.000000000000000000 ) ) ;
#48272 = EDGE_CURVE ( 'NONE', #127486, #45873, #136005, .T. ) ;
#48271 = CARTESIAN_POINT ( 'NONE',  ( -23.15000000000000213, 85.00000000001188027, -93.12913836187181005 ) ) ;
#48273 = EDGE_LOOP ( 'NONE', ( #249858, #34209 ) ) ;
#48274 = ADVANCED_FACE ( 'NONE', ( #18652 ), #17374, .F. ) ;
#48275 = LINE ( 'NONE', #14320, #84366 ) ;
#48276 = ORIENTED_EDGE ( 'NONE', *, *, #135447, .T. ) ;
#48277 = EDGE_LOOP ( 'NONE', ( #169431, #48310, #36365, #66969 ) ) ;
#48278 = EDGE_CURVE ( 'NONE', #64660, #158833, #181181, .T. ) ;
#48279 = LINE ( 'NONE', #69154, #209171 ) ;
#48281 = EDGE_CURVE ( 'NONE', #14558, #253941, #189361, .T. ) ;
#48280 = CARTESIAN_POINT ( 'NONE',  ( -21.05000000000000071, 78.93126476241668854, -235.8702625865613243 ) ) ;
#48282 = EDGE_LOOP ( 'NONE', ( #118221, #185413, #193918, #134767 ) ) ;
#48283 = DIRECTION ( 'NONE',  ( 0.000000000000000000, 0.000000000000000000, 1.000000000000000000 ) ) ;
#48284 = DIRECTION ( 'NONE',  ( -1.000000000000000000, -0.000000000000000000, -0.000000000000000000 ) ) ;
#48285 = ORIENTED_EDGE ( 'NONE', *, *, #64187, .F. ) ;
#48286 = CARTESIAN_POINT ( 'NONE',  ( -20.94999999999999929, -1.135018845899022466, -175.2169768834323520 ) ) ;
#48288 = DIRECTION ( 'NONE',  ( 0.000000000000000000, -6.982962677686266711E-15, 1.000000000000000000 ) ) ;
#48287 =( BOUNDED_CURVE ( )  B_SPLINE_CURVE ( 3, ( #195342, #174529, #94916, #118356 ),
 .UNSPECIFIED., .F., .F. ) 
 B_SPLINE_CURVE_WITH_KNOTS ( ( 4, 4 ),
 ( 3.752122642744585068, 4.712388980384675463 ),
 .UNSPECIFIED. ) 
 CURVE ( )  GEOMETRIC_REPRESENTATION_ITEM ( )  RATIONAL_B_SPLINE_CURVE ( ( 1.000000000000000000, 0.9246222802177217481, 0.9246222802177217481, 1.000000000000000000 ) ) 
 REPRESENTATION_ITEM ( '' )  );
#48290 = CARTESIAN_POINT ( 'NONE',  ( 21.72449340488909897, 65.71604372252068060, -82.17310748452439384 ) ) ;
#48289 = CARTESIAN_POINT ( 'NONE',  ( -20.94999999999999929, 87.75000000001192291, -99.92310748452422331 ) ) ;
#48291 = DIRECTION ( 'NONE',  ( -1.000000000000000000, -0.000000000000000000, -0.000000000000000000 ) ) ;
#48292 = AXIS2_PLACEMENT_3D ( 'NONE', #66455, #185120, #205962 ) ;
#48293 = DIRECTION ( 'NONE',  ( 0.000000000000000000, 0.2128009952263603677, -0.9770955615653313941 ) ) ;
#48294 = DIRECTION ( 'NONE',  ( 1.000000000000000000, -0.000000000000000000, -0.000000000000000000 ) ) ;
#48295 = DIRECTION ( 'NONE',  ( -1.836970198721029934E-16, -1.000000000000000000, -6.982962677686266711E-15 ) ) ;
#48296 = AXIS2_PLACEMENT_3D ( 'NONE', #62391, #63662, #101461 ) ;
#48297 = AXIS2_PLACEMENT_3D ( 'NONE', #226143, #47524, #207930 ) ;
#48298 = ORIENTED_EDGE ( 'NONE', *, *, #79784, .F. ) ;
#48299 = TOROIDAL_SURFACE ( 'NONE', #110838, 0.2000000000000000111, 0.1000000000000000056 ) ;
#48300 = ADVANCED_BREP_SHAPE_REPRESENTATION ( '', ( #24390, #2425 ), #106268 ) ;
#48302 = ORIENTED_EDGE ( 'NONE', *, *, #47482, .T. ) ;
#48301 = ORIENTED_EDGE ( 'NONE', *, *, #117874, .F. ) ;
#48303 = EDGE_LOOP ( 'NONE', ( #45417, #8251, #29288, #130669 ) ) ;
#48304 = LINE ( 'NONE', #106983, #149366 ) ;
#48305 = FACE_OUTER_BOUND ( 'NONE', #61971, .T. ) ;
#48306 = AXIS2_PLACEMENT_3D ( 'NONE', #103108, #22338, #206088 ) ;
#48308 = CARTESIAN_POINT ( 'NONE',  ( -22.49999999999999645, 11.74956712350054744, -33.39914163090129051 ) ) ;
#48307 = DIRECTION ( 'NONE',  ( 0.000000000000000000, 0.2617529984165152257, 0.9651348961777124202 ) ) ;
#48309 = FACE_OUTER_BOUND ( 'NONE', #147598, .T. ) ;
#48310 = ORIENTED_EDGE ( 'NONE', *, *, #141211, .T. ) ;
#48311 = CARTESIAN_POINT ( 'NONE',  ( -22.48660254037844197, 11.75000000001114842, -100.4500000000000313 ) ) ;
#48312 = DIRECTION ( 'NONE',  ( 1.734723475976823250E-13, 0.7899159663865635839, 0.6132151058540398214 ) ) ;
#48313 = AXIS2_PLACEMENT_3D ( 'NONE', #64411, #213523, #59555 ) ;
#48314 = DIRECTION ( 'NONE',  ( 0.000000000000000000, 0.000000000000000000, 1.000000000000000000 ) ) ;
#48315 = VERTEX_POINT ( 'NONE', #214289 ) ;
#48316 = EDGE_CURVE ( 'NONE', #156105, #201868, #96862, .T. ) ;
#48317 = DIRECTION ( 'NONE',  ( 0.000000000000000000, 0.000000000000000000, -1.000000000000000000 ) ) ;
#48318 = FACE_OUTER_BOUND ( 'NONE', #151530, .T. ) ;
#48319 = EDGE_LOOP ( 'NONE', ( #96769, #249618, #117830, #29257 ) ) ;
#48320 = ORIENTED_EDGE ( 'NONE', *, *, #234624, .T. ) ;
#48321 = CARTESIAN_POINT ( 'NONE',  ( -16.88328101497759448, 9.950352834230013599, -54.35117951492927801 ) ) ;
#48322 = CARTESIAN_POINT ( 'NONE',  ( 20.95512820512820440, 67.12384868372441815, -182.2731074845244166 ) ) ;
#48323 = VECTOR ( 'NONE', #223975, 1000.000000000000000 ) ;
#48324 = CARTESIAN_POINT ( 'NONE',  ( -20.65000000000000568, 70.35000000001264198, -194.2731074845243882 ) ) ;
#48325 = FACE_OUTER_BOUND ( 'NONE', #213160, .T. ) ;
#48326 = DIRECTION ( 'NONE',  ( 0.000000000000000000, -0.9868171638914228216, 0.1618390714546044939 ) ) ;
#48327 = CARTESIAN_POINT ( 'NONE',  ( -21.05000000000000071, 6.478078221094754063, -0.09999993530616047011 ) ) ;
#48328 = ORIENTED_EDGE ( 'NONE', *, *, #63203, .F. ) ;
#48330 = EDGE_CURVE ( 'NONE', #105040, #8189, #131086, .T. ) ;
#48329 = DIRECTION ( 'NONE',  ( 0.000000000000000000, 7.026728003956695223E-15, -1.000000000000000000 ) ) ;
#48331 = CARTESIAN_POINT ( 'NONE',  ( -21.05000000000000071, 1.261786168576181755, -75.08649896354552311 ) ) ;
#48333 = LINE ( 'NONE', #6634, #41519 ) ;
#48332 = CARTESIAN_POINT ( 'NONE',  ( -18.40000000000000213, 64.25000000001253397, -179.2731074845244450 ) ) ;
#48334 = LINE ( 'NONE', #127883, #162368 ) ;
#48335 = EDGE_CURVE ( 'NONE', #149025, #102673, #79875, .T. ) ;
#48336 = LINE ( 'NONE', #191737, #191758 ) ;
#48337 = DIRECTION ( 'NONE',  ( 1.000000000000000000, 0.000000000000000000, 0.000000000000000000 ) ) ;
#48338 = FACE_OUTER_BOUND ( 'NONE', #230796, .T. ) ;
#48339 = VECTOR ( 'NONE', #32000, 1000.000000000000000 ) ;
#48342 = VERTEX_POINT ( 'NONE', #95612 ) ;
#48341 = CIRCLE ( 'NONE', #2532, 0.09999999999999939493 ) ;
#48340 = DIRECTION ( 'NONE',  ( 0.000000000000000000, -0.9126074666063774821, -0.4088369013363273297 ) ) ;
#48343 = VECTOR ( 'NONE', #3887, 999.9999999999998863 ) ;
#48344 = AXIS2_PLACEMENT_3D ( 'NONE', #117635, #197159, #214171 ) ;
#48345 = EDGE_CURVE ( 'NONE', #204749, #76812, #250510, .T. ) ;
#48346 = EDGE_CURVE ( 'NONE', #227874, #30797, #97739, .T. ) ;
#48347 = ADVANCED_FACE ( 'NONE', ( #117746 ), #78610, .F. ) ;
#48348 = DIRECTION ( 'NONE',  ( 0.000000000000000000, 6.938893903907222067E-15, -1.000000000000000000 ) ) ;
#48349 = EDGE_CURVE ( 'NONE', #226515, #173747, #85261, .T. ) ;
#48350 = AXIS2_PLACEMENT_3D ( 'NONE', #194301, #162541, #57304 ) ;
#48351 = CARTESIAN_POINT ( 'NONE',  ( -23.15000000000000213, 20.06933876993645782, -235.7297789824848451 ) ) ;
#48352 = CIRCLE ( 'NONE', #165059, 0.3999999999999975797 ) ;
#48353 = EDGE_LOOP ( 'NONE', ( #220066, #63540, #239460, #81828 ) ) ;
#48354 = CARTESIAN_POINT ( 'NONE',  ( -18.59999999999999787, -7.558719773525646168, -210.9360835033311332 ) ) ;
#48355 = CARTESIAN_POINT ( 'NONE',  ( -23.25000000000000000, 76.00000000001216449, -140.6731074845242802 ) ) ;
#48356 = DIRECTION ( 'NONE',  ( 0.000000000000000000, 0.000000000000000000, 1.000000000000000000 ) ) ;
#48357 = AXIS2_PLACEMENT_3D ( 'NONE', #20222, #82713, #39807 ) ;
#48358 = VERTEX_POINT ( 'NONE', #218112 ) ;
#48359 = CARTESIAN_POINT ( 'NONE',  ( -16.87845715379269507, 12.41613630788209655, -211.2156174692765376 ) ) ;
#48361 = ORIENTED_EDGE ( 'NONE', *, *, #125775, .F. ) ;
#48360 = DIRECTION ( 'NONE',  ( 0.000000000000000000, 0.000000000000000000, -1.000000000000000000 ) ) ;
#48362 = DIRECTION ( 'NONE',  ( -1.000000000000000000, -0.000000000000000000, -0.000000000000000000 ) ) ;
#48363 = ADVANCED_FACE ( 'NONE', ( #119045 ), #106120, .T. ) ;
#48364 = LINE ( 'NONE', #228302, #150208 ) ;
#48365 = ORIENTED_EDGE ( 'NONE', *, *, #93162, .T. ) ;
#48366 = DIRECTION ( 'NONE',  ( 0.000000000000000000, 1.000000000000000000, 0.000000000000000000 ) ) ;
#48367 = CARTESIAN_POINT ( 'NONE',  ( 0.000000000000000000, 0.000000000000000000, 0.000000000000000000 ) ) ;
#48368 = CARTESIAN_POINT ( 'NONE',  ( -16.87036670365548474, 9.989418819301645769, -20.97956011730205006 ) ) ;
#48369 = DIRECTION ( 'NONE',  ( 0.000000000000000000, -2.428612866367527723E-14, -1.000000000000000000 ) ) ;
#48370 = CARTESIAN_POINT ( 'NONE',  ( 21.05000000000000071, 67.12338541492479749, -94.63802700567968884 ) ) ;
#48371 = ORIENTED_EDGE ( 'NONE', *, *, #86219, .T. ) ;
#48372 = CARTESIAN_POINT ( 'NONE',  ( -21.05000000000000071, 1.115600667400684642E-11, -33.50000000000000000 ) ) ;
#48373 = DIRECTION ( 'NONE',  ( 0.7071067811865475727, -0.7071067811865475727, 0.000000000000000000 ) ) ;
#48374 = VECTOR ( 'NONE', #49553, 1000.000000000000000 ) ;
#48375 = LINE ( 'NONE', #92634, #195128 ) ;
#48376 = VERTEX_POINT ( 'NONE', #233852 ) ;
#48377 = ORIENTED_EDGE ( 'NONE', *, *, #35575, .F. ) ;
#48378 = CARTESIAN_POINT ( 'NONE',  ( 18.50000000000000000, 85.40000000001185754, -96.14106563635155567 ) ) ;
#48379 = CARTESIAN_POINT ( 'NONE',  ( -23.15000000000000213, 4.350000000011156054, -45.65000000000000568 ) ) ;
#48380 = CARTESIAN_POINT ( 'NONE',  ( -20.94999999999999929, -12.41227409413852811, -97.50000000000004263 ) ) ;
#48381 = LINE ( 'NONE', #27586, #228411 ) ;
#48383 = CARTESIAN_POINT ( 'NONE',  ( -16.87036670365549895, 66.01058118071065905, -157.5026676018264880 ) ) ;
#48382 = VECTOR ( 'NONE', #143635, 1000.000000000000000 ) ;
#48384 = LINE ( 'NONE', #83629, #48382 ) ;
#48385 = DIRECTION ( 'NONE',  ( 0.7071067811865474617, 0.7071067811865474617, -0.000000000000000000 ) ) ;
#48386 = LINE ( 'NONE', #6698, #193112 ) ;
#48387 = TOROIDAL_SURFACE ( 'NONE', #110938, 2.100000000000002309, 0.1000000000000000056 ) ;
#48388 = CARTESIAN_POINT ( 'NONE',  ( 18.59999999999999076, 6.982009704867611077, -70.69615211825629331 ) ) ;
#48389 = CIRCLE ( 'NONE', #223173, 0.1000000000000028644 ) ;
#48390 = ADVANCED_FACE ( 'NONE', ( #198562 ), #133984, .T. ) ;
#48392 = ORIENTED_EDGE ( 'NONE', *, *, #120704, .T. ) ;
#48391 = DIRECTION ( 'NONE',  ( -1.000000000000000000, -2.952720810173289112E-16, 0.000000000000000000 ) ) ;
#48393 = DIRECTION ( 'NONE',  ( 1.000000000000000000, -0.000000000000000000, -0.000000000000000000 ) ) ;
#48394 = DIRECTION ( 'NONE',  ( 2.489438768765008884E-17, -0.1686199900910312910, 0.9856811345164826488 ) ) ;
#48396 = DIRECTION ( 'NONE',  ( 2.952720810173289112E-16, -1.000000000000000000, 0.000000000000000000 ) ) ;
#48395 = CARTESIAN_POINT ( 'NONE',  ( 20.94999999999999929, -8.999999999988842703, -157.6060308773475640 ) ) ;
#48397 = ORIENTED_EDGE ( 'NONE', *, *, #244532, .F. ) ;
#48398 = CYLINDRICAL_SURFACE ( 'NONE', #39345, 0.1000000000000028644 ) ;
#48399 = LINE ( 'NONE', #161963, #158231 ) ;
#48400 = CARTESIAN_POINT ( 'NONE',  ( 21.05000000000000071, 18.94908112497232366, -227.8991131484155517 ) ) ;
#48401 = DIRECTION ( 'NONE',  ( -1.020425574104003999E-15, -0.2128009952263603677, 0.9770955615653313941 ) ) ;
#48403 = EDGE_CURVE ( 'NONE', #127486, #217509, #114520, .T. ) ;
#48402 = CARTESIAN_POINT ( 'NONE',  ( -13.40000000000000213, -8.250000000000007105, 15.00000000000000355 ) ) ;
#48404 = EDGE_LOOP ( 'NONE', ( #187178, #4481, #210988, #114795 ) ) ;
#48405 = VERTEX_POINT ( 'NONE', #160763 ) ;
#48406 = ADVANCED_FACE ( 'NONE', ( #184132 ), #224546, .T. ) ;
#48407 = EDGE_CURVE ( 'NONE', #35875, #138363, #102006, .T. ) ;
#48408 = CARTESIAN_POINT ( 'NONE',  ( 21.05000000000000071, 6.477067021135911595, -100.6000000000000369 ) ) ;
#48409 = EDGE_LOOP ( 'NONE', ( #74583, #69396, #79937, #42684 ) ) ;
#48410 = FACE_OUTER_BOUND ( 'NONE', #43331, .T. ) ;
#48411 = VECTOR ( 'NONE', #223197, 1000.000000000000000 ) ;
#48412 = EDGE_LOOP ( 'NONE', ( #61327, #204588, #119800, #67886 ) ) ;
#48413 = CARTESIAN_POINT ( 'NONE',  ( 20.94999999999999574, 10.42338541492406279, -40.99205192387010044 ) ) ;
#48414 = VECTOR ( 'NONE', #254967, 1000.000000000000000 ) ;
#48415 = DIRECTION ( 'NONE',  ( 0.000000000000000000, 0.000000000000000000, -1.000000000000000000 ) ) ;
#48416 = FACE_OUTER_BOUND ( 'NONE', #96041, .T. ) ;
#48417 = ORIENTED_EDGE ( 'NONE', *, *, #152813, .F. ) ;
#48418 = ADVANCED_FACE ( 'NONE', ( #23821 ), #120358, .F. ) ;
#48419 = AXIS2_PLACEMENT_3D ( 'NONE', #196627, #74163, #156262 ) ;
#48420 = EDGE_CURVE ( 'NONE', #42512, #154148, #1637, .T. ) ;
#48421 = CARTESIAN_POINT ( 'NONE',  ( -20.64999999999999858, 74.00000000001156764, -56.29848556176223440 ) ) ;
#48422 = CIRCLE ( 'NONE', #194202, 0.1000000000000124678 ) ;
#48423 = CARTESIAN_POINT ( 'NONE',  ( -18.51697539158856998, 68.06642993404716435, -224.1774859612004036 ) ) ;
#48424 = CARTESIAN_POINT ( 'NONE',  ( 21.13461538461538325, 60.21941965847794620, -221.1573116214326831 ) ) ;
#48425 = CARTESIAN_POINT ( 'NONE',  ( -23.25000000000000355, 64.25000000001161027, -60.27310748452440947 ) ) ;
#48426 = PRODUCT_RELATED_PRODUCT_CATEGORY ( 'part', '', ( #149326 ) ) ;
#48427 = CARTESIAN_POINT ( 'NONE',  ( -23.15000000000000213, 2.000000000011154189, -147.2246219227621111 ) ) ;
#48428 = CARTESIAN_POINT ( 'NONE',  ( 21.09706851349341861, 11.17857743693056527, -211.0878094224673873 ) ) ;
#48429 = ORIENTED_EDGE ( 'NONE', *, *, #96181, .T. ) ;
#48431 = DIRECTION ( 'NONE',  ( 0.000000000000000000, -7.056502275159890043E-15, 1.000000000000000000 ) ) ;
#48430 = CARTESIAN_POINT ( 'NONE',  ( 18.52928932188133970, 63.78876043141220009, -209.2774030244867163 ) ) ;
#48432 = VERTEX_POINT ( 'NONE', #21253 ) ;
#48434 = ORIENTED_EDGE ( 'NONE', *, *, #9530, .T. ) ;
#48433 = DIRECTION ( 'NONE',  ( -1.000000000000000000, -0.000000000000000000, 0.000000000000000000 ) ) ;
#48435 = AXIS2_PLACEMENT_3D ( 'NONE', #249672, #150570, #91870 ) ;
#48436 = VERTEX_POINT ( 'NONE', #22524 ) ;
#48437 = DIRECTION ( 'NONE',  ( 0.000000000000000000, 0.9910465087640866200, 0.1335171055202867274 ) ) ;
#48438 = CIRCLE ( 'NONE', #35985, 0.09999999999999779898 ) ;
#48439 = CARTESIAN_POINT ( 'NONE',  ( 18.57399277249656322, 10.33112638556969820, -72.59012289269746532 ) ) ;
#48440 = CIRCLE ( 'NONE', #148412, 0.1000000000000028644 ) ;
#48441 = DIRECTION ( 'NONE',  ( 0.000000000000000000, 0.000000000000000000, 1.000000000000000000 ) ) ;
#48442 = EDGE_CURVE ( 'NONE', #60192, #105425, #27064, .T. ) ;
#48443 = CARTESIAN_POINT ( 'NONE',  ( 18.59999999999999076, 7.120270961708750512, -70.65956304183931991 ) ) ;
#48444 = ORIENTED_EDGE ( 'NONE', *, *, #81722, .T. ) ;
#48445 = ADVANCED_FACE ( 'NONE', ( #165889 ), #6790, .F. ) ;
#48446 = EDGE_CURVE ( 'NONE', #57698, #91491, #221953, .T. ) ;
#48447 = CARTESIAN_POINT ( 'NONE',  ( -18.37160782347004329, 40.40888803190161127, -235.2966881398250507 ) ) ;
#48448 = CARTESIAN_POINT ( 'NONE',  ( 18.59999999999999076, 10.49142135624846617, -158.7500000000000284 ) ) ;
#48449 = CIRCLE ( 'NONE', #152537, 0.1999999999999987899 ) ;
#48450 = ORIENTED_EDGE ( 'NONE', *, *, #257819, .T. ) ;
#48451 = CARTESIAN_POINT ( 'NONE',  ( -18.40000000000000213, 8.822561741677553471, -176.7499999999999716 ) ) ;
#48452 = AXIS2_PLACEMENT_3D ( 'NONE', #173694, #54946, #253163 ) ;
#48453 = EDGE_CURVE ( 'NONE', #66095, #142512, #103303, .T. ) ;
#48454 = DIRECTION ( 'NONE',  ( 0.000000000000000000, 1.224646799142015331E-16, 1.000000000000000000 ) ) ;
#48455 = ORIENTED_EDGE ( 'NONE', *, *, #99886, .T. ) ;
#48456 = FACE_OUTER_BOUND ( 'NONE', #76262, .T. ) ;
#48457 = EDGE_LOOP ( 'NONE', ( #15562, #177320, #162561 ) ) ;
#48458 = CARTESIAN_POINT ( 'NONE',  ( -20.94999999999999929, -11.48912529306490349, -69.90000000000004832 ) ) ;
#48459 = VERTEX_POINT ( 'NONE', #182885 ) ;
#48460 = CARTESIAN_POINT ( 'NONE',  ( 13.99999999999999822, 66.15000000001204228, -119.7731074845243739 ) ) ;
#48461 = DIRECTION ( 'NONE',  ( -0.000000000000000000, -1.000000000000000000, 6.308085367188393199E-16 ) ) ;
#48462 = CARTESIAN_POINT ( 'NONE',  ( 21.05000000000000782, 75.96513199699860763, -75.79319334821346388 ) ) ;
#48463 = LINE ( 'NONE', #128019, #149529 ) ;
#48464 = AXIS2_PLACEMENT_3D ( 'NONE', #105216, #141816, #200517 ) ;
#48465 = AXIS2_PLACEMENT_3D ( 'NONE', #249326, #150225, #229742 ) ;
#48466 = ADVANCED_FACE ( 'NONE', ( #122901 ), #61631, .F. ) ;
#48467 = AXIS2_PLACEMENT_3D ( 'NONE', #241059, #141933, #104071 ) ;
#48468 = AXIS2_PLACEMENT_3D ( 'NONE', #231342, #211768, #192214 ) ;
#48469 = DIRECTION ( 'NONE',  ( 0.000000000000000000, 0.7049548389605067023, -0.7092521942342977503 ) ) ;
#48470 = LINE ( 'NONE', #133155, #226413 ) ;
#48471 = ORIENTED_EDGE ( 'NONE', *, *, #215022, .T. ) ;
#48472 = CARTESIAN_POINT ( 'NONE',  ( 18.39999999999999858, 86.97871406799755789, -199.3361829075352603 ) ) ;
#48473 = ORIENTED_EDGE ( 'NONE', *, *, #10009, .F. ) ;
#48475 = DIRECTION ( 'NONE',  ( -1.000000000000000000, -0.000000000000000000, 0.000000000000000000 ) ) ;
#48474 = DIRECTION ( 'NONE',  ( -0.000000000000000000, 6.982962677686266711E-15, -1.000000000000000000 ) ) ;
#48476 = AXIS2_PLACEMENT_3D ( 'NONE', #172406, #71988, #94093 ) ;
#48477 = ORIENTED_EDGE ( 'NONE', *, *, #171094, .F. ) ;
#48478 = FACE_OUTER_BOUND ( 'NONE', #157079, .T. ) ;
#48479 = DIRECTION ( 'NONE',  ( 0.000000000000000000, -0.1290532225515364506, -0.9916376685811525427 ) ) ;
#48480 = EDGE_CURVE ( 'NONE', #63948, #257629, #119246, .T. ) ;
#48481 = CARTESIAN_POINT ( 'NONE',  ( 20.95265033839679347, 59.06589578572285859, -225.8015307137926015 ) ) ;
#48482 = ORIENTED_EDGE ( 'NONE', *, *, #79285, .T. ) ;
#48484 = EDGE_LOOP ( 'NONE', ( #95656, #198161, #122664 ) ) ;
#48483 = DIRECTION ( 'NONE',  ( 0.000000000000000000, 0.000000000000000000, -1.000000000000000000 ) ) ;
#48486 = CARTESIAN_POINT ( 'NONE',  ( -20.94999999999999929, -11.64999999999999858, -3.100000000000001865 ) ) ;
#48485 = VECTOR ( 'NONE', #48291, 1000.000000000000000 ) ;
#48487 = EDGE_CURVE ( 'NONE', #5980, #66070, #177437, .T. ) ;
#48489 = CARTESIAN_POINT ( 'NONE',  ( 18.56308993302889832, 15.40745845255181301, -222.9635632280946993 ) ) ;
#48488 = DIRECTION ( 'NONE',  ( 1.000000000000000000, 0.000000000000000000, 0.000000000000000000 ) ) ;
#48490 = AXIS2_PLACEMENT_3D ( 'NONE', #134938, #33347, #112843 ) ;
#48492 = ORIENTED_EDGE ( 'NONE', *, *, #202665, .F. ) ;
#48491 = DIRECTION ( 'NONE',  ( 0.000000000000000000, -2.775557561563196798E-13, -1.000000000000000000 ) ) ;
#48493 = CIRCLE ( 'NONE', #36033, 0.2000000000000048683 ) ;
#48494 = ORIENTED_EDGE ( 'NONE', *, *, #72723, .F. ) ;
#48496 = EDGE_CURVE ( 'NONE', #163018, #140720, #6171, .T. ) ;
#48495 = DIRECTION ( 'NONE',  ( 0.000000000000000000, -6.608470384673547079E-15, 1.000000000000000000 ) ) ;
#48497 = DIRECTION ( 'NONE',  ( 1.000000000000000000, 0.000000000000000000, 0.000000000000000000 ) ) ;
#48499 = EDGE_CURVE ( 'NONE', #217985, #211107, #135348, .T. ) ;
#48498 = ORIENTED_EDGE ( 'NONE', *, *, #23685, .T. ) ;
#48500 = CARTESIAN_POINT ( 'NONE',  ( -17.29158576265543346, 52.57432316029790087, -231.0639701379864448 ) ) ;
#48501 = ORIENTED_EDGE ( 'NONE', *, *, #237600, .F. ) ;
#48502 = CIRCLE ( 'NONE', #81784, 0.4000000000000114575 ) ;
#48503 = CARTESIAN_POINT ( 'NONE',  ( -18.49513951962167368, 85.43772502668907975, -29.24503490949512141 ) ) ;
#48504 = DIRECTION ( 'NONE',  ( 0.000000000000000000, 0.000000000000000000, -1.000000000000000000 ) ) ;
#48505 = ORIENTED_EDGE ( 'NONE', *, *, #247632, .T. ) ;
#48506 = CARTESIAN_POINT ( 'NONE',  ( 18.59999999999999432, 77.86671491006960366, -158.2704322382423356 ) ) ;
#48507 = CARTESIAN_POINT ( 'NONE',  ( -16.86578989773641979, 9.984809801269951990, -180.0353351133777551 ) ) ;
#48508 = ORIENTED_EDGE ( 'NONE', *, *, #221981, .F. ) ;
#48509 = CIRCLE ( 'NONE', #2711, 0.09999999999999963085 ) ;
#48510 = CIRCLE ( 'NONE', #85902, 0.09999999999999939493 ) ;
#48511 = CARTESIAN_POINT ( 'NONE',  ( 21.05000000000000071, 76.10000000001222986, -148.1726782920690937 ) ) ;
#48512 = CIRCLE ( 'NONE', #148488, 0.1000000000000013933 ) ;
#48513 = CIRCLE ( 'NONE', #194307, 0.4000000000000010214 ) ;
#48514 = EDGE_CURVE ( 'NONE', #114275, #253143, #87591, .T. ) ;
#48515 = ORIENTED_EDGE ( 'NONE', *, *, #178611, .F. ) ;
#48516 = ORIENTED_EDGE ( 'NONE', *, *, #165366, .T. ) ;
#48517 = CARTESIAN_POINT ( 'NONE',  ( -18.33682934331516279, -9.511185591082417901, -73.90565476867330119 ) ) ;
#48518 = EDGE_LOOP ( 'NONE', ( #204979, #52670, #193045, #181019, #813 ) ) ;
#48519 = ADVANCED_FACE ( 'NONE', ( #30223 ), #8089, .T. ) ;
#48520 = CARTESIAN_POINT ( 'NONE',  ( -16.87683809663752399, 23.59405348476682107, -231.3784738672518415 ) ) ;
#48521 = VERTEX_POINT ( 'NONE', #51018 ) ;
#48523 = ORIENTED_EDGE ( 'NONE', *, *, #19963, .T. ) ;
#48522 = DIRECTION ( 'NONE',  ( 1.000000000000000000, 0.000000000000000000, 0.000000000000000000 ) ) ;
#48524 = CARTESIAN_POINT ( 'NONE',  ( -21.12844524849339223, 11.75000000001115197, -73.90441347084285439 ) ) ;
#48525 = EDGE_LOOP ( 'NONE', ( #118592, #160817, #74484, #230094 ) ) ;
#48526 = CYLINDRICAL_SURFACE ( 'NONE', #59870, 0.09999999999998898659 ) ;
#48528 = ORIENTED_EDGE ( 'NONE', *, *, #38192, .T. ) ;
#48527 = ADVANCED_FACE ( 'NONE', ( #92737 ), #112329, .T. ) ;
#48531 = ORIENTED_EDGE ( 'NONE', *, *, #104701, .T. ) ;
#48530 = ORIENTED_EDGE ( 'NONE', *, *, #149164, .T. ) ;
#48529 = CYLINDRICAL_SURFACE ( 'NONE', #226969, 0.1000000000000026007 ) ;
#48532 = CARTESIAN_POINT ( 'NONE',  ( -20.64999999999999858, 76.00000000001126921, -203.5231074845248997 ) ) ;
#48533 = EDGE_CURVE ( 'NONE', #105425, #172898, #35451, .T. ) ;
#48534 = DIRECTION ( 'NONE',  ( 0.000000000000000000, -7.116814260417668513E-15, 1.000000000000000000 ) ) ;
#48535 = CIRCLE ( 'NONE', #56870, 0.09999999999998898659 ) ;
#48536 = AXIS2_PLACEMENT_3D ( 'NONE', #243811, #63898, #43057 ) ;
#48537 = ORIENTED_EDGE ( 'NONE', *, *, #246868, .T. ) ;
#48538 = AXIS2_PLACEMENT_3D ( 'NONE', #29881, #9004, #7732 ) ;
#48539 = ORIENTED_EDGE ( 'NONE', *, *, #47214, .F. ) ;
#48540 = CARTESIAN_POINT ( 'NONE',  ( 21.72449340488909897, 14.48530878454960735, -219.1840063279242088 ) ) ;
#48541 = CARTESIAN_POINT ( 'NONE',  ( 23.14999999999999858, 5.950000000011160139, -56.69429769496518645 ) ) ;
#48543 = ORIENTED_EDGE ( 'NONE', *, *, #129131, .F. ) ;
#48542 = CARTESIAN_POINT ( 'NONE',  ( -18.40000000000000213, 62.50563584222672375, -209.4474707446456421 ) ) ;
#48544 = FACE_OUTER_BOUND ( 'NONE', #206435, .T. ) ;
#48545 = ORIENTED_EDGE ( 'NONE', *, *, #214901, .T. ) ;
#48546 = EDGE_CURVE ( 'NONE', #74710, #151096, #102022, .T. ) ;
#48547 = CARTESIAN_POINT ( 'NONE',  ( 19.75857864376268935, 34.58225676390223668, -235.1091250528070589 ) ) ;
#48548 = FACE_OUTER_BOUND ( 'NONE', #17353, .T. ) ;
#48549 = EDGE_CURVE ( 'NONE', #250894, #156714, #13233, .T. ) ;
#48550 = ORIENTED_EDGE ( 'NONE', *, *, #91439, .T. ) ;
#48551 = CARTESIAN_POINT ( 'NONE',  ( -21.05000000000000071, -1.249999999999999334, -8.000000000000000000 ) ) ;
#48552 = FACE_OUTER_BOUND ( 'NONE', #42117, .T. ) ;
#48553 = EDGE_LOOP ( 'NONE', ( #155524, #67570, #88171, #106546, #130672, #117430 ) ) ;
#48555 = ORIENTED_EDGE ( 'NONE', *, *, #134458, .F. ) ;
#48554 = DIRECTION ( 'NONE',  ( 0.000000000000000000, 0.000000000000000000, -1.000000000000000000 ) ) ;
#48556 = AXIS2_PLACEMENT_3D ( 'NONE', #181069, #2388, #81907 ) ;
#48558 = VERTEX_POINT ( 'NONE', #168487 ) ;
#48557 = EDGE_LOOP ( 'NONE', ( #256331, #156146 ) ) ;
#48559 = EDGE_LOOP ( 'NONE', ( #98119, #70413 ) ) ;
#48560 = CARTESIAN_POINT ( 'NONE',  ( -20.64999999999999858, 23.49882452903949925, -253.1653563615082305 ) ) ;
#48561 = ORIENTED_EDGE ( 'NONE', *, *, #122571, .T. ) ;
#48562 = CARTESIAN_POINT ( 'NONE',  ( -18.59999999999999787, 69.15387683765983695, -166.2853812176745691 ) ) ;
#48563 = ORIENTED_EDGE ( 'NONE', *, *, #31822, .T. ) ;
#48564 = LINE ( 'NONE', #73303, #39896 ) ;
#48565 = AXIS2_PLACEMENT_3D ( 'NONE', #48664, #64391, #203887 ) ;
#48566 = DIRECTION ( 'NONE',  ( -0.000000000000000000, -6.982962677686266711E-15, 1.000000000000000000 ) ) ;
#48567 = ORIENTED_EDGE ( 'NONE', *, *, #155194, .F. ) ;
#48568 = ORIENTED_EDGE ( 'NONE', *, *, #240395, .T. ) ;
#48569 = CIRCLE ( 'NONE', #173533, 0.1000000000000028644 ) ;
#48570 = EDGE_LOOP ( 'NONE', ( #31686, #139272, #89239, #90857 ) ) ;
#48571 = AXIS2_PLACEMENT_3D ( 'NONE', #21032, #161830, #97943 ) ;
#48572 = TOROIDAL_SURFACE ( 'NONE', #165107, 0.2000000000000000111, 0.1000000000000000056 ) ;
#48573 = ADVANCED_FACE ( 'NONE', ( #247961 ), #52317, .F. ) ;
#48574 = B_SPLINE_CURVE_WITH_KNOTS ( 'NONE', 3,
 ( #115011, #194581, #112461, #255765 ),
 .UNSPECIFIED., .F., .F.,
 ( 4, 4 ),
 ( 0.000000000000000000, 0.0001048066582182452479 ),
 .UNSPECIFIED. ) ;
#48575 = COLOUR_RGB ( '', 0.40784314, 0.44705882, 0.49803922) ;
#48576 = DIRECTION ( 'NONE',  ( 0.000000000000000000, 0.000000000000000000, -1.000000000000000000 ) ) ;
#48577 = ORIENTED_EDGE ( 'NONE', *, *, #74999, .T. ) ;
#48578 = DIRECTION ( 'NONE',  ( -1.000000000000000000, -1.836970198721029934E-16, 0.000000000000000000 ) ) ;
#48580 = VERTEX_POINT ( 'NONE', #128034 ) ;
#48579 = DIRECTION ( 'NONE',  ( 1.000000000000000000, 0.000000000000000000, 0.000000000000000000 ) ) ;
#48581 = FACE_OUTER_BOUND ( 'NONE', #75793, .T. ) ;
#48582 = CYLINDRICAL_SURFACE ( 'NONE', #57783, 0.1000000000000028644 ) ;
#48583 = CARTESIAN_POINT ( 'NONE',  ( -21.14999999999999858, 6.540656951712397138, -134.0000000000000000 ) ) ;
#48584 = CARTESIAN_POINT ( 'NONE',  ( 20.94999999999999574, 65.52661458509899717, -95.44445302027583011 ) ) ;
#48586 = CARTESIAN_POINT ( 'NONE',  ( -18.39999999999999858, 37.94390843806124280, -261.1300795796834109 ) ) ;
#48585 = DIRECTION ( 'NONE',  ( 1.000000000000000000, 0.000000000000000000, 0.000000000000000000 ) ) ;
#48587 = CARTESIAN_POINT ( 'NONE',  ( 18.59999999999999076, 69.01799029515522932, -65.82695536626806643 ) ) ;
#48588 = CARTESIAN_POINT ( 'NONE',  ( 18.31572054635746838, 38.18894743439052064, -261.2028889386127730 ) ) ;
#48589 = DIRECTION ( 'NONE',  ( 0.000000000000000000, 0.000000000000000000, 1.000000000000000000 ) ) ;
#48590 = EDGE_CURVE ( 'NONE', #151632, #13430, #243507, .T. ) ;
#48591 = AXIS2_PLACEMENT_3D ( 'NONE', #150377, #9561, #111238 ) ;
#48592 = ORIENTED_EDGE ( 'NONE', *, *, #40377, .T. ) ;
#48593 = AXIS2_PLACEMENT_3D ( 'NONE', #192208, #57791, #233883 ) ;
#48594 = ORIENTED_EDGE ( 'NONE', *, *, #162324, .F. ) ;
#48596 = ORIENTED_EDGE ( 'NONE', *, *, #101465, .T. ) ;
#48595 = CARTESIAN_POINT ( 'NONE',  ( 23.40000000000005542, 74.73834681386826162, -44.00978271863746016 ) ) ;
#48597 = CIRCLE ( 'NONE', #52685, 0.1000000000000070832 ) ;
#48598 = ORIENTED_EDGE ( 'NONE', *, *, #100024, .T. ) ;
#48599 = DIRECTION ( 'NONE',  ( 0.000000000000000000, 0.1495327102803078179, 0.9887567792719429427 ) ) ;
#48600 =( BOUNDED_SURFACE ( )  B_SPLINE_SURFACE ( 3, 2, ( 
 ( #85191, #162228, #163488 ),
 ( #6972, #26560, #86483 ),
 ( #246860, #126931, #25277 ),
 ( #241736, #185619, #5663 ) ),
 .UNSPECIFIED., .F., .F., .F. ) 
 B_SPLINE_SURFACE_WITH_KNOTS ( ( 4, 4 ),
 ( 3, 3 ),
 ( 0.000000000000000000, 0.001979672783031562362 ),
 ( 0.000000000000000000, 1.000000000000000000 ),
 .UNSPECIFIED. ) 
 GEOMETRIC_REPRESENTATION_ITEM ( )  RATIONAL_B_SPLINE_SURFACE ( (
 ( 1.000000000000000000, 0.7103081912008383236, 1.000000000000000000),
 ( 1.000000000000000000, 0.7104998333558377732, 1.000000000000000000),
 ( 1.000000000000000000, 0.7107238315755368685, 1.000000000000000000),
 ( 1.000000000000000000, 0.7110073749539289611, 1.000000000000000000) ) ) 
 REPRESENTATION_ITEM ( '' )  SURFACE ( )  );
#48601 = CARTESIAN_POINT ( 'NONE',  ( 20.21567752745019320, 10.19811410124265905, -141.8826203476516810 ) ) ;
#48602 = VECTOR ( 'NONE', #135044, 1000.000000000000000 ) ;
#48603 = VECTOR ( 'NONE', #43775, 1000.000000000000000 ) ;
#48605 = FACE_OUTER_BOUND ( 'NONE', #181294, .T. ) ;
#48604 = DIRECTION ( 'NONE',  ( 1.000000000000000000, 0.000000000000000000, 0.000000000000000000 ) ) ;
#48606 = ORIENTED_EDGE ( 'NONE', *, *, #137167, .T. ) ;
#48607 = CARTESIAN_POINT ( 'NONE',  ( -20.15000000000000568, 9.291421356248463326, -121.6500000000000341 ) ) ;
#48608 = CYLINDRICAL_SURFACE ( 'NONE', #162299, 11.75000000000000000 ) ;
#48609 = EDGE_LOOP ( 'NONE', ( #114080, #17221, #94921, #28025 ) ) ;
#48611 = CYLINDRICAL_SURFACE ( 'NONE', #42309, 0.09999999999998898659 ) ;
#48610 = TOROIDAL_SURFACE ( 'NONE', #194400, 1.900000000000002576, 0.1000000000000000056 ) ;
#48612 = CARTESIAN_POINT ( 'NONE',  ( 18.49999999999999645, -1.835341550213255957, -179.0551512925629538 ) ) ;
#48613 = AXIS2_PLACEMENT_3D ( 'NONE', #112493, #52485, #92900 ) ;
#48614 = CYLINDRICAL_SURFACE ( 'NONE', #154031, 0.09999999999999939493 ) ;
#48615 = DIRECTION ( 'NONE',  ( 0.000000000000000000, 0.000000000000000000, 1.000000000000000000 ) ) ;
#48616 = VECTOR ( 'NONE', #175440, 1000.000000000000000 ) ;
#48617 = DIRECTION ( 'NONE',  ( -1.000000000000000000, 0.000000000000000000, -0.000000000000000000 ) ) ;
#48619 = ORIENTED_EDGE ( 'NONE', *, *, #171384, .F. ) ;
#48618 = DIRECTION ( 'NONE',  ( 0.000000000000000000, -6.982962677686266711E-15, 1.000000000000000000 ) ) ;
#48620 = DIRECTION ( 'NONE',  ( 0.000000000000000000, 0.9915357197604892647, -0.1298341882519715440 ) ) ;
#48621 = DIRECTION ( 'NONE',  ( -1.000000000000000000, 0.000000000000000000, 0.000000000000000000 ) ) ;
#48622 = LINE ( 'NONE', #207724, #208305 ) ;
#48623 = FACE_OUTER_BOUND ( 'NONE', #71615, .T. ) ;
#48624 = ORIENTED_EDGE ( 'NONE', *, *, #184003, .T. ) ;
#48625 = CARTESIAN_POINT ( 'NONE',  ( 14.45963434102924339, 66.54845833862631821, -84.56923198569378997 ) ) ;
#48626 = FACE_OUTER_BOUND ( 'NONE', #28898, .T. ) ;
#48627 = CARTESIAN_POINT ( 'NONE',  ( -20.94999999999999929, 87.41227409416215721, -172.9231074845242802 ) ) ;
#48629 = ADVANCED_FACE ( 'NONE', ( #228427 ), #77734, .F. ) ;
#48628 = CARTESIAN_POINT ( 'NONE',  ( -16.87401514999234209, 9.950000000011137047, -54.28001799253208759 ) ) ;
#48630 = CIRCLE ( 'NONE', #161075, 0.09999999999998904210 ) ;
#48631 = DIRECTION ( 'NONE',  ( -1.000000000000000000, -0.000000000000000000, 0.000000000000000000 ) ) ;
#48632 = DIRECTION ( 'NONE',  ( 1.000000000000000000, -0.000000000000000000, -0.000000000000000000 ) ) ;
#48633 = DIRECTION ( 'NONE',  ( 0.000000000000000000, 0.9908441862701782288, 0.1350103645450542456 ) ) ;
#48634 = ORIENTED_EDGE ( 'NONE', *, *, #10063, .T. ) ;
#48635 = EDGE_LOOP ( 'NONE', ( #89607, #123788, #226804, #102956 ) ) ;
#48636 = ORIENTED_EDGE ( 'NONE', *, *, #214730, .F. ) ;
#48637 = EDGE_CURVE ( 'NONE', #167224, #228476, #90210, .T. ) ;
#48638 = CARTESIAN_POINT ( 'NONE',  ( 20.21567752745066215, 65.80188589877991490, -95.14048713687273562 ) ) ;
#48639 = CARTESIAN_POINT ( 'NONE',  ( 18.59999999999999076, 6.450000000000001066, -10.01702717044001822 ) ) ;
#48640 = ORIENTED_EDGE ( 'NONE', *, *, #95572, .T. ) ;
#48641 = EDGE_CURVE ( 'NONE', #166675, #118383, #211418, .T. ) ;
#48642 = AXIS2_PLACEMENT_3D ( 'NONE', #44991, #204051, #104914 ) ;
#48643 = AXIS2_PLACEMENT_3D ( 'NONE', #19015, #178118, #39899 ) ;
#48644 = ORIENTED_EDGE ( 'NONE', *, *, #227533, .F. ) ;
#48645 = SURFACE_SIDE_STYLE ('',( #227285 ) ) ;
#48646 = VECTOR ( 'NONE', #91608, 1000.000000000000114 ) ;
#48647 = VECTOR ( 'NONE', #177273, 1000.000000000000000 ) ;
#48648 = EDGE_CURVE ( 'NONE', #223514, #4495, #27683, .T. ) ;
#48649 = ORIENTED_EDGE ( 'NONE', *, *, #59596, .T. ) ;
#48650 = DIRECTION ( 'NONE',  ( 0.000000000000000000, 0.8814952561688432775, -0.4721928772777344019 ) ) ;
#48651 = VERTEX_POINT ( 'NONE', #70654 ) ;
#48652 = VECTOR ( 'NONE', #232045, 1000.000000000000000 ) ;
#48653 = CARTESIAN_POINT ( 'NONE',  ( -20.94999999999999929, 87.65000000001212754, -133.6231074845242119 ) ) ;
#48654 = CARTESIAN_POINT ( 'NONE',  ( -16.93521499325732549, 30.27781715495975945, -234.7945324989871096 ) ) ;
#48655 = CARTESIAN_POINT ( 'NONE',  ( 23.25000000000000000, 52.55093873171406216, -255.3069320826340061 ) ) ;
#48656 = CARTESIAN_POINT ( 'NONE',  ( -21.11927991906891222, 1.448806495452435117, -230.6797615723483261 ) ) ;
#48657 = CARTESIAN_POINT ( 'NONE',  ( -21.70464131381649509, 7.095358018979010417, -67.00000000000004263 ) ) ;
#48658 = FACE_OUTER_BOUND ( 'NONE', #74185, .T. ) ;
#48660 = ORIENTED_EDGE ( 'NONE', *, *, #165404, .F. ) ;
#48659 = CARTESIAN_POINT ( 'NONE',  ( 21.09787244211748458, 44.24086307789509931, -236.5388354431762536 ) ) ;
#48662 = CARTESIAN_POINT ( 'NONE',  ( -6.000000000000003553, -11.25000000000000000, 10.00000000000000178 ) ) ;
#48661 = CARTESIAN_POINT ( 'NONE',  ( -20.15000000000000568, 22.31449321236291183, -231.3267202105024580 ) ) ;
#48663 = EDGE_CURVE ( 'NONE', #55464, #135449, #107168, .T. ) ;
#48664 = CARTESIAN_POINT ( 'NONE',  ( -20.54999999999999716, 85.00000000001232081, -160.1291383618718385 ) ) ;
#48665 = AXIS2_PLACEMENT_3D ( 'NONE', #63047, #215692, #116613 ) ;
#48666 = ORIENTED_EDGE ( 'NONE', *, *, #121730, .F. ) ;
#48667 = CARTESIAN_POINT ( 'NONE',  ( 15.06592377766031099, 66.58221053305985038, -121.1657229405474681 ) ) ;
#48668 = CARTESIAN_POINT ( 'NONE',  ( -21.05000000000000071, 87.22043517378990884, -209.5709486447514678 ) ) ;
#48669 = CARTESIAN_POINT ( 'NONE',  ( 21.05000000000000071, -0.09999999998884338825, -60.45934304829879835 ) ) ;
#48671 = ORIENTED_EDGE ( 'NONE', *, *, #56555, .F. ) ;
#48670 = CONICAL_SURFACE ( 'NONE', #190345, 4.049999999999998046, 0.7853981633974604915 ) ;
#48672 = CARTESIAN_POINT ( 'NONE',  ( -20.54999999999999716, 68.85000000001180354, -81.87310748452436826 ) ) ;
#48673 = LINE ( 'NONE', #89085, #206375 ) ;
#48674 = ORIENTED_EDGE ( 'NONE', *, *, #132492, .T. ) ;
#48675 = CARTESIAN_POINT ( 'NONE',  ( 18.49999999999999645, 74.83729825007408465, -128.4231074845243086 ) ) ;
#48676 = CARTESIAN_POINT ( 'NONE',  ( 23.24999999999999645, 76.00000000001213607, -136.5231074845243313 ) ) ;
#48677 = CARTESIAN_POINT ( 'NONE',  ( 18.52928932188133970, 10.27928932188134858, -21.35000000000000142 ) ) ;
#48678 = CARTESIAN_POINT ( 'NONE',  ( 22.39999999999999503, 11.36188319272497438, -198.4231588494578773 ) ) ;
#48679 = ORIENTED_EDGE ( 'NONE', *, *, #43570, .F. ) ;
#48680 = ORIENTED_EDGE ( 'NONE', *, *, #76762, .T. ) ;
#48681 = CARTESIAN_POINT ( 'NONE',  ( -21.65000000000000213, 9.949999999999983302, -12.75000000000000178 ) ) ;
#48682 = DIRECTION ( 'NONE',  ( -0.000000000000000000, 0.2617529984165031243, 0.9651348961777157509 ) ) ;
#48683 = LINE ( 'NONE', #108669, #145283 ) ;
#48684 = CARTESIAN_POINT ( 'NONE',  ( -23.25000000000000355, 70.35000000001255671, -182.6731074845243938 ) ) ;
#48685 = AXIS2_PLACEMENT_3D ( 'NONE', #90041, #206153, #125337 ) ;
#48686 = CIRCLE ( 'NONE', #61178, 4.049999999999998934 ) ;
#48687 = PLANE ( 'NONE',  #40922 ) ;
#48689 = AXIS2_PLACEMENT_3D ( 'NONE', #6801, #180308, #122914 ) ;
#48688 = FACE_OUTER_BOUND ( 'NONE', #249032, .T. ) ;
#48690 = CIRCLE ( 'NONE', #23801, 11.89999999999999325 ) ;
#48691 = DIRECTION ( 'NONE',  ( -1.000000000000000000, -0.000000000000000000, -0.000000000000000000 ) ) ;
#48692 = ORIENTED_EDGE ( 'NONE', *, *, #101979, .T. ) ;
#48693 = CARTESIAN_POINT ( 'NONE',  ( -20.94999675878240808, 65.70692517833232671, -97.56446533783034170 ) ) ;
#48694 = EDGE_CURVE ( 'NONE', #139578, #239511, #229701, .T. ) ;
#48696 = ORIENTED_EDGE ( 'NONE', *, *, #108463, .T. ) ;
#48695 = DIRECTION ( 'NONE',  ( -1.000000000000000000, -0.000000000000000000, -0.000000000000000000 ) ) ;
#48697 = DIRECTION ( 'NONE',  ( 0.000000000000000000, 0.000000000000000000, 1.000000000000000000 ) ) ;
#48698 = DIRECTION ( 'NONE',  ( -1.000000000000000000, 0.000000000000000000, 0.000000000000000000 ) ) ;
#48699 = DIRECTION ( 'NONE',  ( -0.000000000000000000, -6.982962677686266711E-15, 1.000000000000000000 ) ) ;
#48700 =( BOUNDED_SURFACE ( )  B_SPLINE_SURFACE ( 3, 2, ( 
 ( #249713, #54068, #189739 ),
 ( #191046, #231447, #11103 ),
 ( #91908, #71090, #150615 ),
 ( #206728, #29415, #167628 ),
 ( #112769, #89332, #28120 ),
 ( #230145, #107622, #72376 ) ),
 .UNSPECIFIED., .F., .F., .F. ) 
 B_SPLINE_SURFACE_WITH_KNOTS ( ( 4, 2, 4 ),
 ( 3, 3 ),
 ( 0.0001381104793128107321, 0.0002947094729387620326, 0.0004513084665647133873 ),
 ( 0.000000000000000000, 1.000000000000000000 ),
 .UNSPECIFIED. ) 
 GEOMETRIC_REPRESENTATION_ITEM ( )  RATIONAL_B_SPLINE_SURFACE ( (
 ( 1.000000000000000000, 0.7071067811865475727, 1.000000000000000000),
 ( 1.000000000000000000, 0.6919563088098478199, 1.000000000000000000),
 ( 1.000000000000000000, 0.6959445945718057969, 1.000000000000000000),
 ( 1.000000000000000000, 0.7137882985313904749, 1.000000000000000000),
 ( 1.000000000000000000, 0.7257496306095887473, 1.000000000000000000),
 ( 1.000000000000000000, 0.7250110520819876836, 1.000000000000000000) ) ) 
 REPRESENTATION_ITEM ( '' )  SURFACE ( )  );
#48701 = CARTESIAN_POINT ( 'NONE',  ( -16.83233564386414116, 66.06977820342736152, -123.7476281479999898 ) ) ;
#48703 = ORIENTED_EDGE ( 'NONE', *, *, #252854, .T. ) ;
#48702 = CARTESIAN_POINT ( 'NONE',  ( 20.94999999999999929, 75.24091630460340241, -206.3219986834402846 ) ) ;
#48704 = CARTESIAN_POINT ( 'NONE',  ( -18.50000000000000000, 65.70729864261058140, -164.5657455973725121 ) ) ;
#48705 = CARTESIAN_POINT ( 'NONE',  ( -18.40000000000000213, 5.650000000011139001, -121.3500000000000369 ) ) ;
#48706 = FACE_OUTER_BOUND ( 'NONE', #239439, .T. ) ;
#48707 = ADVANCED_FACE ( 'NONE', ( #60 ), #173630, .T. ) ;
#48708 = ORIENTED_EDGE ( 'NONE', *, *, #103401, .T. ) ;
#48709 = CARTESIAN_POINT ( 'NONE',  ( -15.73854595235691534, 66.64858632091087998, -153.0427639169753604 ) ) ;
#48710 = CARTESIAN_POINT ( 'NONE',  ( -23.15000000000000213, 31.49702336731127872, -233.4564499823349877 ) ) ;
#48711 = EDGE_LOOP ( 'NONE', ( #88570, #114411, #201732, #96954 ) ) ;
#48712 = DIRECTION ( 'NONE',  ( 1.000000000000000000, -0.000000000000000000, -0.000000000000000000 ) ) ;
#48713 = AXIS2_PLACEMENT_3D ( 'NONE', #178940, #257101, #160654 ) ;
#48714 = EDGE_CURVE ( 'NONE', #30797, #94319, #216546, .T. ) ;
#48715 = AXIS2_PLACEMENT_3D ( 'NONE', #107354, #186933, #8279 ) ;
#48717 = CIRCLE ( 'NONE', #227775, 0.09999999999999986677 ) ;
#48716 = CARTESIAN_POINT ( 'NONE',  ( -16.92209698673556062, 66.05000000001189164, -90.31247191747172565 ) ) ;
#48718 = EDGE_LOOP ( 'NONE', ( #67818, #38788, #220254, #51076 ) ) ;
#48719 = CARTESIAN_POINT ( 'NONE',  ( -20.94999999999999929, -1.835341550213255957, -78.55515129256303908 ) ) ;
#48720 = VERTEX_POINT ( 'NONE', #17087 ) ;
#48722 = CYLINDRICAL_SURFACE ( 'NONE', #64366, 0.9000000000000014655 ) ;
#48721 = AXIS2_PLACEMENT_3D ( 'NONE', #86916, #89494, #169090 ) ;
#48723 = DIRECTION ( 'NONE',  ( 0.000000000000000000, 1.000000000000000000, 2.891205793294679805E-16 ) ) ;
#48724 = ADVANCED_FACE ( 'NONE', ( #193149 ), #15233, .T. ) ;
#48725 = CARTESIAN_POINT ( 'NONE',  ( 20.84999999999999432, 77.16412189325360771, -162.1082593989527254 ) ) ;
#48726 = ORIENTED_EDGE ( 'NONE', *, *, #252576, .T. ) ;
#48727 = ADVANCED_FACE ( 'NONE', ( #74519 ), #248451, .T. ) ;
#48729 = EDGE_CURVE ( 'NONE', #183270, #91489, #252528, .T. ) ;
#48728 = CARTESIAN_POINT ( 'NONE',  ( -21.05000000000000071, 74.83729825007431202, -162.0231074845243597 ) ) ;
#48730 = CARTESIAN_POINT ( 'NONE',  ( 20.97468175916148780, 12.98972486229050993, -210.7130060050627094 ) ) ;
#48731 = CARTESIAN_POINT ( 'NONE',  ( 18.49999999999999645, 74.73788286442776041, -233.7359682632885267 ) ) ;
#48732 = CARTESIAN_POINT ( 'NONE',  ( 23.14999999999999858, 8.013878543493270001, -211.9507248933737458 ) ) ;
#48733 = AXIS2_PLACEMENT_3D ( 'NONE', #94149, #133291, #9478 ) ;
#48734 = CARTESIAN_POINT ( 'NONE',  ( -13.40000000000000036, -11.65000000000000036, 17.60000000000000497 ) ) ;
#48735 = ORIENTED_EDGE ( 'NONE', *, *, #68579, .F. ) ;
#48737 = ORIENTED_EDGE ( 'NONE', *, *, #99000, .F. ) ;
#48736 = CARTESIAN_POINT ( 'NONE',  ( -21.07016717456945543, 6.320940838111416049, -167.4999999999999432 ) ) ;
#48738 = EDGE_CURVE ( 'NONE', #133183, #16105, #27735, .T. ) ;
#48739 = ORIENTED_EDGE ( 'NONE', *, *, #28595, .F. ) ;
#48740 = FACE_OUTER_BOUND ( 'NONE', #104366, .T. ) ;
#48741 = ORIENTED_EDGE ( 'NONE', *, *, #181141, .T. ) ;
#48742 = DIRECTION ( 'NONE',  ( 1.000000000000000000, 2.952720810173289112E-16, -0.000000000000000000 ) ) ;
#48743 = FACE_OUTER_BOUND ( 'NONE', #13615, .T. ) ;
#48744 = CARTESIAN_POINT ( 'NONE',  ( -22.39999999999999858, 76.00000000001173817, -81.17267829206912211 ) ) ;
#48745 = ORIENTED_EDGE ( 'NONE', *, *, #36191, .T. ) ;
#48746 = ADVANCED_FACE ( 'NONE', ( #53630 ), #234832, .T. ) ;
#48747 = EDGE_CURVE ( 'NONE', #37986, #56908, #57459, .T. ) ;
#48748 = DIRECTION ( 'NONE',  ( 7.304098846218134667E-16, 1.000000000000000000, 6.982962677686267499E-15 ) ) ;
#48749 = DIRECTION ( 'NONE',  ( 2.952720810173289112E-16, -0.9770955615653316162, -0.2128009952263598403 ) ) ;
#48750 = CIRCLE ( 'NONE', #186122, 0.09999999999999939493 ) ;
#48751 = CARTESIAN_POINT ( 'NONE',  ( -18.59999999999999787, 64.35000000001205933, -124.3731074845243825 ) ) ;
#48752 = VERTEX_POINT ( 'NONE', #137012 ) ;
#48753 = CARTESIAN_POINT ( 'NONE',  ( -18.59999999999999787, -1.362429037182155023, -74.88888124792120493 ) ) ;
#48755 = ORIENTED_EDGE ( 'NONE', *, *, #25961, .T. ) ;
#48754 = CARTESIAN_POINT ( 'NONE',  ( -21.05000000000000071, 44.12194005689738674, -258.6913704466671788 ) ) ;
#48756 = FACE_OUTER_BOUND ( 'NONE', #256415, .T. ) ;
#48757 = CARTESIAN_POINT ( 'NONE',  ( -18.59999999999999787, 1.162701749949165642, -41.60000000000000142 ) ) ;
#48758 = AXIS2_PLACEMENT_3D ( 'NONE', #133422, #132135, #192130 ) ;
#48759 = AXIS2_PLACEMENT_3D ( 'NONE', #45266, #240906, #62263 ) ;
#48760 = VECTOR ( 'NONE', #119151, 1000.000000000000000 ) ;
#48761 = EDGE_LOOP ( 'NONE', ( #203010, #167751, #46863, #4171 ) ) ;
#48762 = VECTOR ( 'NONE', #128970, 1000.000000000000000 ) ;
#48763 = CARTESIAN_POINT ( 'NONE',  ( 18.49999999999999289, 63.83083047455526327, -209.3924252461221158 ) ) ;
#48764 = CARTESIAN_POINT ( 'NONE',  ( -13.12432614554023580, 66.56923500458974274, -121.2925700897739603 ) ) ;
#48765 = DIRECTION ( 'NONE',  ( 0.000000000000000000, 1.000000000000000000, 6.938893903907222067E-15 ) ) ;
#48767 = ORIENTED_EDGE ( 'NONE', *, *, #208335, .T. ) ;
#48766 = CIRCLE ( 'NONE', #61805, 3.999999999999996447 ) ;
#48768 = DIRECTION ( 'NONE',  ( 1.000000000000000000, 0.000000000000000000, 0.000000000000000000 ) ) ;
#48769 = ADVANCED_FACE ( 'NONE', ( #134419 ), #94318, .F. ) ;
#48770 = EDGE_CURVE ( 'NONE', #138858, #130839, #37937, .T. ) ;
#48771 = AXIS2_PLACEMENT_3D ( 'NONE', #214791, #133965, #213504 ) ;
#48772 = CARTESIAN_POINT ( 'NONE',  ( 20.85000000000000142, 78.45218979564165807, -232.7313097695096076 ) ) ;
#48773 = ORIENTED_EDGE ( 'NONE', *, *, #244847, .F. ) ;
#48774 = EDGE_CURVE ( 'NONE', #220166, #1095, #58730, .T. ) ;
#48775 = AXIS2_PLACEMENT_3D ( 'NONE', #196878, #114783, #212611 ) ;
#48776 = VECTOR ( 'NONE', #175562, 1000.000000000000000 ) ;
#48777 = EDGE_LOOP ( 'NONE', ( #209965, #242755, #169860, #186120 ) ) ;
#48778 = CARTESIAN_POINT ( 'NONE',  ( -22.39999999999999858, 68.20922040163873135, -136.6231074845243540 ) ) ;
#48779 = CIRCLE ( 'NONE', #32066, 0.09999999999999939493 ) ;
#48780 = ORIENTED_EDGE ( 'NONE', *, *, #60325, .T. ) ;
#48781 = CIRCLE ( 'NONE', #82076, 0.09999999999999939493 ) ;
#48782 = DIRECTION ( 'NONE',  ( -0.000000000000000000, -1.000000000000000000, -8.609265936414532828E-15 ) ) ;
#48783 = CARTESIAN_POINT ( 'NONE',  ( -16.87683809663752399, 66.15000000001255387, -183.4254715027207396 ) ) ;
#48785 = ORIENTED_EDGE ( 'NONE', *, *, #193382, .F. ) ;
#48784 = DIRECTION ( 'NONE',  ( 0.000000000000000000, 0.000000000000000000, -1.000000000000000000 ) ) ;
#48786 = PLANE ( 'NONE',  #16026 ) ;
#48788 = CIRCLE ( 'NONE', #102936, 0.1000000000000124678 ) ;
#48787 = DIRECTION ( 'NONE',  ( 0.000000000000000000, 0.000000000000000000, -1.000000000000000000 ) ) ;
#48789 = FACE_OUTER_BOUND ( 'NONE', #235280, .T. ) ;
#48790 = DIRECTION ( 'NONE',  ( -1.000000000000000000, 0.000000000000000000, 0.000000000000000000 ) ) ;
#48791 = FACE_OUTER_BOUND ( 'NONE', #90178, .T. ) ;
#48792 = ADVANCED_FACE ( 'NONE', ( #117460 ), #194444, .T. ) ;
#48793 = FACE_OUTER_BOUND ( 'NONE', #49462, .T. ) ;
#48794 = CARTESIAN_POINT ( 'NONE',  ( -18.47079683080347223, -9.471664105233722708, -107.6088605409924952 ) ) ;
#48796 = ORIENTED_EDGE ( 'NONE', *, *, #108872, .F. ) ;
#48795 = DIRECTION ( 'NONE',  ( -0.000000000000000000, 0.000000000000000000, -1.000000000000000000 ) ) ;
#48797 = DIRECTION ( 'NONE',  ( 0.000000000000000000, 1.000000000000000000, 0.000000000000000000 ) ) ;
#48798 = ADVANCED_FACE ( 'NONE', ( #217809, #176165 ), #255624, .T. ) ;
#48799 = AXIS2_PLACEMENT_3D ( 'NONE', #155441, #233663, #117552 ) ;
#48800 = CIRCLE ( 'NONE', #52890, 0.5000000000000004441 ) ;
#48802 = ADVANCED_FACE ( 'NONE', ( #19644 ), #39225, .T. ) ;
#48801 = DIRECTION ( 'NONE',  ( 1.000000000000000000, 0.000000000000000000, 0.000000000000000000 ) ) ;
#48803 = FACE_OUTER_BOUND ( 'NONE', #192019, .T. ) ;
#48804 = EDGE_CURVE ( 'NONE', #186173, #197247, #85921, .T. ) ;
#48805 = CARTESIAN_POINT ( 'NONE',  ( -23.49999999999994316, 79.88763423575340994, -7.282924647898262549 ) ) ;
#48806 = CYLINDRICAL_SURFACE ( 'NONE', #51534, 11.74999999999999645 ) ;
#48807 = EDGE_CURVE ( 'NONE', #148962, #77283, #181816, .T. ) ;
#48808 = EDGE_LOOP ( 'NONE', ( #207860, #219096, #256968 ) ) ;
#48809 = CARTESIAN_POINT ( 'NONE',  ( -16.87683809663752399, 23.65833333334447985, -117.2500000000000284 ) ) ;
#48810 = AXIS2_PLACEMENT_3D ( 'NONE', #128156, #169892, #188120 ) ;
#48811 = CARTESIAN_POINT ( 'NONE',  ( -21.07928932188134041, 6.328516656404449492, -100.4011048543456468 ) ) ;
#48812 = AXIS2_PLACEMENT_3D ( 'NONE', #244207, #245525, #65590 ) ;
#48813 = ORIENTED_EDGE ( 'NONE', *, *, #126569, .T. ) ;
#48815 = ADVANCED_FACE ( 'NONE', ( #101701 ), #120050, .F. ) ;
#48814 = DIRECTION ( 'NONE',  ( 0.000000000000000000, -3.469446951953515108E-14, 1.000000000000000000 ) ) ;
#48816 = EDGE_CURVE ( 'NONE', #201516, #168277, #227592, .T. ) ;
#48818 = DIRECTION ( 'NONE',  ( -1.000000000000000000, -3.265361837132813093E-16, 0.000000000000000000 ) ) ;
#48817 = AXIS2_PLACEMENT_3D ( 'NONE', #147003, #124901, #50458 ) ;
#48819 = ORIENTED_EDGE ( 'NONE', *, *, #178106, .T. ) ;
#48820 = CARTESIAN_POINT ( 'NONE',  ( -21.11825140030079240, 6.445407565431027663, -66.99279637936723475 ) ) ;
#48821 = ORIENTED_EDGE ( 'NONE', *, *, #253131, .T. ) ;
#48822 = EDGE_CURVE ( 'NONE', #217631, #239696, #2734, .T. ) ;
#48823 = CARTESIAN_POINT ( 'NONE',  ( -23.15000000000000213, -9.499999999988848032, -110.3939691226524786 ) ) ;
#48824 = ORIENTED_EDGE ( 'NONE', *, *, #46650, .F. ) ;
#48825 = AXIS2_PLACEMENT_3D ( 'NONE', #78035, #177180, #195452 ) ;
#48826 = LINE ( 'NONE', #85354, #60740 ) ;
#48827 = AXIS2_PLACEMENT_3D ( 'NONE', #55243, #244170, #100776 ) ;
#48828 = CARTESIAN_POINT ( 'NONE',  ( 20.94999999999999574, -1.736257131586239844, -179.0686523290174819 ) ) ;
#48829 = VECTOR ( 'NONE', #251318, 1000.000000000000000 ) ;
#48830 = ORIENTED_EDGE ( 'NONE', *, *, #195454, .F. ) ;
#48831 = VERTEX_POINT ( 'NONE', #159175 ) ;
#48832 = LINE ( 'NONE', #87936, #73805 ) ;
#48833 = ORIENTED_EDGE ( 'NONE', *, *, #68900, .T. ) ;
#48834 = EDGE_CURVE ( 'NONE', #36165, #110094, #131927, .T. ) ;
#48835 = LINE ( 'NONE', #232642, #181411 ) ;
#48836 = VERTEX_POINT ( 'NONE', #104284 ) ;
#48837 = CIRCLE ( 'NONE', #144696, 0.09999999999999939493 ) ;
#48838 = EDGE_CURVE ( 'NONE', #68130, #32779, #221664, .T. ) ;
#48839 = ORIENTED_EDGE ( 'NONE', *, *, #101499, .T. ) ;
#48840 = CARTESIAN_POINT ( 'NONE',  ( -18.40000000000000213, 11.41458325959978382, -12.65000000000000213 ) ) ;
#48841 = CARTESIAN_POINT ( 'NONE',  ( -18.40000000000000213, 5.650000000011139001, -113.1500000000000341 ) ) ;
#48843 = EDGE_CURVE ( 'NONE', #97363, #211140, #148506, .T. ) ;
#48842 = DIRECTION ( 'NONE',  ( 0.000000000000000000, 0.000000000000000000, 1.000000000000000000 ) ) ;
#48844 = DIRECTION ( 'NONE',  ( 0.000000000000000000, 0.000000000000000000, 1.000000000000000000 ) ) ;
#48845 = CIRCLE ( 'NONE', #177867, 0.09999999999999939493 ) ;
#48846 = CARTESIAN_POINT ( 'NONE',  ( 21.05000000000000071, 65.27628288308652316, -57.34686788338628105 ) ) ;
#48847 = EDGE_CURVE ( 'NONE', #9680, #159529, #152627, .T. ) ;
#48848 = CARTESIAN_POINT ( 'NONE',  ( -16.77683809663752257, 52.34166666667870516, -119.7731074845244592 ) ) ;
#48849 = AXIS2_PLACEMENT_3D ( 'NONE', #102577, #3496, #25646 ) ;
#48850 = EDGE_LOOP ( 'NONE', ( #181176, #99477, #60832, #146068, #102356 ) ) ;
#48851 = FACE_OUTER_BOUND ( 'NONE', #77091, .T. ) ;
#48852 = DIRECTION ( 'NONE',  ( -0.000000000000000000, -0.7397890806274223241, -0.6728388485993012091 ) ) ;
#48853 = CARTESIAN_POINT ( 'NONE',  ( 20.95083306685154056, 67.08315735812188052, -128.0457826312660075 ) ) ;
#48854 = CARTESIAN_POINT ( 'NONE',  ( 21.05000000000000071, 1.115600667400684642E-11, -100.5000000000000426 ) ) ;
#48855 = ORIENTED_EDGE ( 'NONE', *, *, #107595, .F. ) ;
#48856 = CARTESIAN_POINT ( 'NONE',  ( 22.45380639572154990, 1.426823211110743220E-07, -55.24956710889318146 ) ) ;
#48857 = ORIENTED_EDGE ( 'NONE', *, *, #231385, .F. ) ;
#48858 = DIRECTION ( 'NONE',  ( 1.000000000000000000, -0.000000000000000000, -0.000000000000000000 ) ) ;
#48860 = ORIENTED_EDGE ( 'NONE', *, *, #46738, .F. ) ;
#48859 = AXIS2_PLACEMENT_3D ( 'NONE', #91732, #212964, #253368 ) ;
#48861 = DIRECTION ( 'NONE',  ( 0.7071359030027766224, -0.7070776581709024011, 0.000000000000000000 ) ) ;
#48862 = CARTESIAN_POINT ( 'NONE',  ( -20.64999999999999858, -8.999999999988846255, -143.8939691226524644 ) ) ;
#48863 = VERTEX_POINT ( 'NONE', #219100 ) ;
#48864 = ORIENTED_EDGE ( 'NONE', *, *, #50047, .F. ) ;
#48866 = VERTEX_POINT ( 'NONE', #122604 ) ;
#48865 = DIRECTION ( 'NONE',  ( 0.000000000000000000, 1.000000000000000000, 0.000000000000000000 ) ) ;
#48867 = ADVANCED_FACE ( 'NONE', ( #144700 ), #163015, .T. ) ;
#48868 = DIRECTION ( 'NONE',  ( -3.265361837132813093E-16, 1.000000000000000000, 0.000000000000000000 ) ) ;
#48869 = ORIENTED_EDGE ( 'NONE', *, *, #43298, .F. ) ;
#48870 = CYLINDRICAL_SURFACE ( 'NONE', #218726, 0.09999999999999939493 ) ;
#48871 = CARTESIAN_POINT ( 'NONE',  ( -18.39999999999999858, -9.599999999988849453, -140.6001893912220737 ) ) ;
#48873 = ORIENTED_EDGE ( 'NONE', *, *, #136914, .F. ) ;
#48872 = EDGE_CURVE ( 'NONE', #104063, #250188, #169390, .T. ) ;
#48874 = CARTESIAN_POINT ( 'NONE',  ( 23.14999999999999858, 76.00000000001142553, -36.02310748452432421 ) ) ;
#48875 = DIRECTION ( 'NONE',  ( 0.000000000000000000, 0.8814952561688444987, -0.4721928772777320149 ) ) ;
#48876 = AXIS2_PLACEMENT_3D ( 'NONE', #242394, #63761, #143299 ) ;
#48877 = AXIS2_PLACEMENT_3D ( 'NONE', #130119, #31067, #110560 ) ;
#48878 = AXIS2_PLACEMENT_3D ( 'NONE', #109737, #207589, #228437 ) ;
#48879 = CIRCLE ( 'NONE', #103033, 0.1000000000000065836 ) ;
#48880 = VERTEX_POINT ( 'NONE', #45624 ) ;
#48881 = DIRECTION ( 'NONE',  ( 0.000000000000000000, -0.1350103645451945777, 0.9908441862701590219 ) ) ;
#48882 = EDGE_CURVE ( 'NONE', #26230, #237761, #200845, .T. ) ;
#48883 = CARTESIAN_POINT ( 'NONE',  ( -23.15000000000000213, -8.999999999988846255, -143.8939691226524644 ) ) ;
#48884 = DIRECTION ( 'NONE',  ( 0.000000000000000000, 0.000000000000000000, -1.000000000000000000 ) ) ;
#48886 = ORIENTED_EDGE ( 'NONE', *, *, #56690, .F. ) ;
#48885 = CARTESIAN_POINT ( 'NONE',  ( -23.15000000000000213, 76.00000000001190870, -103.0231074845243029 ) ) ;
#48887 = CARTESIAN_POINT ( 'NONE',  ( -18.59999999999999787, 0.8650195716890449749, -212.6652626294507229 ) ) ;
#48888 = CARTESIAN_POINT ( 'NONE',  ( -22.48660254037843487, 12.58580559757028183, -223.4396719342083770 ) ) ;
#48889 = CARTESIAN_POINT ( 'NONE',  ( -16.94878442675511465, 9.991729103002157331, -121.3882195756379048 ) ) ;
#48892 = CARTESIAN_POINT ( 'NONE',  ( 20.04142135623731136, 64.25000000001220712, -145.2559501969990663 ) ) ;
#48891 = AXIS2_PLACEMENT_3D ( 'NONE', #28965, #208836, #107158 ) ;
#48890 = DIRECTION ( 'NONE',  ( -3.265361837132813093E-16, 1.000000000000000000, 0.000000000000000000 ) ) ;
#48893 = CARTESIAN_POINT ( 'NONE',  ( 21.05000000000000071, 39.15968973805286168, -236.7234144681435453 ) ) ;
#48894 = DIRECTION ( 'NONE',  ( -1.000000000000000000, -7.304098846218163263E-16, 4.217023435051627211E-16 ) ) ;
#48895 = VECTOR ( 'NONE', #241803, 1000.000000000000000 ) ;
#48896 = CARTESIAN_POINT ( 'NONE',  ( -21.44999999999999929, 7.350000000011155166, -155.1500000000000057 ) ) ;
#48897 = ADVANCED_FACE ( 'NONE', ( #61331 ), #220415, .T. ) ;
#48898 = DIRECTION ( 'NONE',  ( 0.000000000000000000, 0.000000000000000000, -1.000000000000000000 ) ) ;
#48899 = ORIENTED_EDGE ( 'NONE', *, *, #99699, .F. ) ;
#48900 = AXIS2_PLACEMENT_3D ( 'NONE', #116486, #60343, #199888 ) ;
#48901 = ORIENTED_EDGE ( 'NONE', *, *, #105977, .T. ) ;
#48902 = VERTEX_POINT ( 'NONE', #183840 ) ;
#48903 = DIRECTION ( 'NONE',  ( -0.000000000000000000, 0.1350103645451945777, -0.9908441862701590219 ) ) ;
#48904 = DIRECTION ( 'NONE',  ( -1.000000000000000000, 0.000000000000000000, 0.000000000000000000 ) ) ;
#48905 = VERTEX_POINT ( 'NONE', #181296 ) ;
#48906 = FILL_AREA_STYLE_COLOUR ( '', #214276 ) ;
#48907 = DIRECTION ( 'NONE',  ( -0.000000000000000000, 0.8814952561688430555, -0.4721928772777346239 ) ) ;
#48908 = CARTESIAN_POINT ( 'NONE',  ( 20.87600722750343252, 10.33112638556969465, -206.5901228926974227 ) ) ;
#48909 = AXIS2_PLACEMENT_3D ( 'NONE', #180131, #96688, #215386 ) ;
#48910 = DIRECTION ( 'NONE',  ( -0.000000000000000000, 0.8660254037844502539, 0.4999999999999799050 ) ) ;
#48911 = EDGE_LOOP ( 'NONE', ( #181641, #32989, #130963, #151672, #159964 ) ) ;
#48912 = ORIENTED_EDGE ( 'NONE', *, *, #113325, .F. ) ;
#48913 = CARTESIAN_POINT ( 'NONE',  ( -16.88495309932522659, 9.954627058484012636, -46.13454867381192059 ) ) ;
#48914 = CYLINDRICAL_SURFACE ( 'NONE', #158765, 0.09999999999998898659 ) ;
#48915 = ORIENTED_EDGE ( 'NONE', *, *, #112688, .T. ) ;
#48916 = DIRECTION ( 'NONE',  ( 1.000000000000000000, 0.000000000000000000, 0.000000000000000000 ) ) ;
#48918 = EDGE_LOOP ( 'NONE', ( #165666, #30005 ) ) ;
#48917 = FACE_OUTER_BOUND ( 'NONE', #173664, .T. ) ;
#48919 = FACE_OUTER_BOUND ( 'NONE', #226416, .T. ) ;
#48921 = CARTESIAN_POINT ( 'NONE',  ( -21.05000000000000071, -1.835341550224411922, -11.55515129256297868 ) ) ;
#48920 = CIRCLE ( 'NONE', #107187, 0.6000000000000015321 ) ;
#48923 = ORIENTED_EDGE ( 'NONE', *, *, #231910, .T. ) ;
#48922 = DIRECTION ( 'NONE',  ( -1.000000000000000000, 0.000000000000000000, 0.000000000000000000 ) ) ;
#48924 = CARTESIAN_POINT ( 'NONE',  ( -18.51024323315077424, 10.31104185824062647, -72.52045169831058047 ) ) ;
#48925 = PLANE ( 'NONE',  #170660 ) ;
#48926 = EDGE_CURVE ( 'NONE', #106103, #250767, #202657, .T. ) ;
#48927 = DIRECTION ( 'NONE',  ( 0.000000000000000000, -1.000000000000000000, 0.000000000000000000 ) ) ;
#48928 = CARTESIAN_POINT ( 'NONE',  ( -16.86132326855787156, 12.42438317058102193, -211.2904107606333071 ) ) ;
#48929 = AXIS2_PLACEMENT_3D ( 'NONE', #24748, #147225, #125117 ) ;
#48931 = CARTESIAN_POINT ( 'NONE',  ( 18.59999999999999076, 43.12265650693429819, -239.4782534460092052 ) ) ;
#48930 = CARTESIAN_POINT ( 'NONE',  ( 21.05000000000000071, 85.00000000001222134, -146.0170766071767332 ) ) ;
#48932 = DIRECTION ( 'NONE',  ( -0.000000000000000000, -0.2605042016806452532, -0.9654727137038777718 ) ) ;
#48933 = DIRECTION ( 'NONE',  ( 0.000000000000000000, 0.000000000000000000, 1.000000000000000000 ) ) ;
#48934 = AXIS2_PLACEMENT_3D ( 'NONE', #140184, #123215, #202747 ) ;
#48935 = AXIS2_PLACEMENT_3D ( 'NONE', #95107, #174699, #254162 ) ;
#48936 = CARTESIAN_POINT ( 'NONE',  ( -23.25000000000000000, 1.115600667400684642E-11, -134.0000000000000000 ) ) ;
#48937 = DIRECTION ( 'NONE',  ( 0.000000000000000000, -1.000000000000000000, -6.860497997771531562E-15 ) ) ;
#48938 = ORIENTED_EDGE ( 'NONE', *, *, #72207, .F. ) ;
#48939 = ORIENTED_EDGE ( 'NONE', *, *, #88236, .F. ) ;
#48940 = DIRECTION ( 'NONE',  ( 1.000000000000000000, -0.000000000000000000, -0.000000000000000000 ) ) ;
#48941 = ORIENTED_EDGE ( 'NONE', *, *, #106331, .T. ) ;
#48942 = DIRECTION ( 'NONE',  ( -1.000000000000000000, 0.000000000000000000, 0.000000000000000000 ) ) ;
#48943 = VERTEX_POINT ( 'NONE', #241269 ) ;
#48944 = EDGE_CURVE ( 'NONE', #247446, #148383, #123551, .T. ) ;
#48945 = CARTESIAN_POINT ( 'NONE',  ( 21.05000000000000071, -11.48912529306489994, -97.60000000000005116 ) ) ;
#48946 = CARTESIAN_POINT ( 'NONE',  ( 20.94999999999999929, 11.65000000000000391, -26.71613433702190932 ) ) ;
#48947 = ADVANCED_FACE ( 'NONE', ( #105549 ), #244345, .T. ) ;
#48948 = ORIENTED_EDGE ( 'NONE', *, *, #52662, .T. ) ;
#48949 = FACE_OUTER_BOUND ( 'NONE', #122079, .T. ) ;
#48951 = EDGE_CURVE ( 'NONE', #215984, #71691, #52797, .T. ) ;
#48950 = VECTOR ( 'NONE', #11539, 1000.000000000000114 ) ;
#48952 = EDGE_LOOP ( 'NONE', ( #127912, #58749, #159541, #183712 ) ) ;
#48953 = ORIENTED_EDGE ( 'NONE', *, *, #72211, .F. ) ;
#48954 = AXIS2_PLACEMENT_3D ( 'NONE', #218490, #97241, #158571 ) ;
#48955 = ORIENTED_EDGE ( 'NONE', *, *, #112100, .F. ) ;
#48956 = EDGE_CURVE ( 'NONE', #73222, #51735, #247667, .T. ) ;
#48958 = CARTESIAN_POINT ( 'NONE',  ( -20.54999999999999716, -9.399999999988846611, -90.60603087734760663 ) ) ;
#48957 = AXIS2_PLACEMENT_3D ( 'NONE', #225589, #243892, #245191 ) ;
#48959 =( LENGTH_UNIT ( ) NAMED_UNIT ( * ) SI_UNIT ( .MILLI., .METRE. ) );
#48960 = CARTESIAN_POINT ( 'NONE',  ( -23.15000000000000213, 4.349999999999999645, -21.14999999999999858 ) ) ;
#48961 = AXIS2_PLACEMENT_3D ( 'NONE', #138633, #102083, #181660 ) ;
#48963 = EDGE_CURVE ( 'NONE', #201212, #42422, #91158, .T. ) ;
#48962 = CARTESIAN_POINT ( 'NONE',  ( 12.68104795156994591, 27.34981073572247823, -233.9047583970293260 ) ) ;
#48964 = FACE_OUTER_BOUND ( 'NONE', #223750, .T. ) ;
#48965 = AXIS2_PLACEMENT_3D ( 'NONE', #112322, #234824, #75761 ) ;
#48967 = CARTESIAN_POINT ( 'NONE',  ( 18.39999999999999858, 85.51932773110506503, -196.5501311079649724 ) ) ;
#48966 = DIRECTION ( 'NONE',  ( 0.000000000000000000, 0.000000000000000000, -1.000000000000000000 ) ) ;
#48968 = DIRECTION ( 'NONE',  ( -1.836970198721029934E-16, 1.000000000000000000, 0.000000000000000000 ) ) ;
#48970 = ORIENTED_EDGE ( 'NONE', *, *, #238869, .T. ) ;
#48969 = CARTESIAN_POINT ( 'NONE',  ( -18.59999999999999787, 68.97833521811159585, -65.68954208262705663 ) ) ;
#48972 = CARTESIAN_POINT ( 'NONE',  ( 21.05000000000000071, 11.75000000001116263, -126.9851942293460922 ) ) ;
#48971 = CARTESIAN_POINT ( 'NONE',  ( 20.97107704358301916, 8.875478152032441059, -75.55897322938929506 ) ) ;
#48973 = EDGE_CURVE ( 'NONE', #105209, #218153, #209833, .T. ) ;
#48974 = DIRECTION ( 'NONE',  ( 0.000000000000000000, 0.2617529984165031243, 0.9651348961777157509 ) ) ;
#48975 = ORIENTED_EDGE ( 'NONE', *, *, #238774, .T. ) ;
#48976 = CARTESIAN_POINT ( 'NONE',  ( 20.95035502843362707, 10.47763832678762164, -74.57629970873641412 ) ) ;
#48977 = CARTESIAN_POINT ( 'NONE',  ( -21.44999999999999929, 65.69978428250288971, -213.4221254243406065 ) ) ;
#48978 = CARTESIAN_POINT ( 'NONE',  ( -21.05000000000000071, -7.817436562502985353, -209.8389866834999395 ) ) ;
#48979 = ORIENTED_EDGE ( 'NONE', *, *, #199205, .F. ) ;
#48980 = EDGE_CURVE ( 'NONE', #231838, #71592, #236159, .T. ) ;
#48981 = DIRECTION ( 'NONE',  ( 0.000000000000000000, 0.4999999999999348299, -0.8660254037844762331 ) ) ;
#48982 = AXIS2_PLACEMENT_3D ( 'NONE', #170867, #208672, #250343 ) ;
#48983 = CARTESIAN_POINT ( 'NONE',  ( 20.46382478191414833, 10.59862044130854031, -108.1778144693454919 ) ) ;
#48984 = PLANE ( 'NONE',  #30168 ) ;
#48985 = CIRCLE ( 'NONE', #165535, 12.97499999999999964 ) ;
#48987 = ORIENTED_EDGE ( 'NONE', *, *, #31919, .T. ) ;
#48986 = AXIS2_PLACEMENT_3D ( 'NONE', #8591, #185939, #148104 ) ;
#48988 = EDGE_LOOP ( 'NONE', ( #180839, #58779, #30498, #195843, #63127, #177502, #147951 ) ) ;
#48989 = CARTESIAN_POINT ( 'NONE',  ( -21.04999999999994387, 77.16254490893143725, -43.82310748452479743 ) ) ;
#48990 = CARTESIAN_POINT ( 'NONE',  ( -16.97683809663752186, 66.05000000001203375, -116.4254715027206828 ) ) ;
#48991 = CARTESIAN_POINT ( 'NONE',  ( 18.59999999999999787, 77.73670573947995877, -158.5056848969006182 ) ) ;
#48992 = CARTESIAN_POINT ( 'NONE',  ( -20.92356734117541706, 10.31973158071402175, -206.5505334713353989 ) ) ;
#48993 = VERTEX_POINT ( 'NONE', #127731 ) ;
#48994 = EDGE_CURVE ( 'NONE', #97016, #102393, #223669, .T. ) ;
#48995 = CARTESIAN_POINT ( 'NONE',  ( -12.60829076262180592, 9.389529397477891948, -118.3171079128937322 ) ) ;
#48996 = CIRCLE ( 'NONE', #11607, 0.09999999999999875655 ) ;
#48997 = DIRECTION ( 'NONE',  ( 0.7071067811865474617, -0.7071067811865474617, -4.937700262164531476E-15 ) ) ;
#48998 = AXIS2_PLACEMENT_3D ( 'NONE', #103110, #80982, #163126 ) ;
#48999 = DIRECTION ( 'NONE',  ( 1.000000000000000000, -0.000000000000000000, -0.000000000000000000 ) ) ;
#49000 = CARTESIAN_POINT ( 'NONE',  ( -23.25000000000000355, 66.05000000001210481, -127.2731074845243597 ) ) ;
#49001 = AXIS2_PLACEMENT_3D ( 'NONE', #119271, #56674, #157120 ) ;
#49002 = EDGE_LOOP ( 'NONE', ( #208861, #246537, #88887, #214224 ) ) ;
#49003 = CARTESIAN_POINT ( 'NONE',  ( 20.91682497891422798, 10.32263460346243633, -39.06059579686719019 ) ) ;
#49004 = AXIS2_PLACEMENT_3D ( 'NONE', #50168, #52739, #110152 ) ;
#49005 = EDGE_CURVE ( 'NONE', #99065, #224509, #194492, .T. ) ;
#49007 = ORIENTED_EDGE ( 'NONE', *, *, #132643, .F. ) ;
#49006 = FACE_OUTER_BOUND ( 'NONE', #232360, .T. ) ;
#49008 = LINE ( 'NONE', #102867, #198844 ) ;
#49009 = DIRECTION ( 'NONE',  ( 1.000000000000000000, 0.000000000000000000, 0.000000000000000000 ) ) ;
#49010 = CARTESIAN_POINT ( 'NONE',  ( -22.94999999999999929, 5.586869315528661062, 16.41686199900910736 ) ) ;
#49011 = CARTESIAN_POINT ( 'NONE',  ( -21.05000000000000071, -10.74476030654554215, -206.4104182790846096 ) ) ;
#49012 = CARTESIAN_POINT ( 'NONE',  ( -21.05000000000000071, 69.60000000001207354, -126.5926828544627654 ) ) ;
#49013 = AXIS2_PLACEMENT_3D ( 'NONE', #80268, #159862, #60722 ) ;
#49014 = DIRECTION ( 'NONE',  ( 0.000000000000000000, 0.000000000000000000, 1.000000000000000000 ) ) ;
#49015 = DIRECTION ( 'NONE',  ( 2.952720810173289112E-16, 1.000000000000000000, 7.086529944415894657E-15 ) ) ;
#49016 = ORIENTED_EDGE ( 'NONE', *, *, #79236, .F. ) ;
#49017 = CARTESIAN_POINT ( 'NONE',  ( -20.94999999999999929, 76.00000000001126921, -203.5231074845248997 ) ) ;
#49018 = CARTESIAN_POINT ( 'NONE',  ( 20.94999999999999574, 10.42338541492406279, -107.9920519238701218 ) ) ;
#49019 = FACE_OUTER_BOUND ( 'NONE', #96455, .T. ) ;
#49020 = AXIS2_PLACEMENT_3D ( 'NONE', #205805, #246226, #90991 ) ;
#49021 = VECTOR ( 'NONE', #102179, 1000.000000000000000 ) ;
#49022 = DIRECTION ( 'NONE',  ( -0.000000000000000000, -0.8814952561688430555, 0.4721928772777346239 ) ) ;
#49023 = VECTOR ( 'NONE', #188596, 999.9999999999998863 ) ;
#49024 = ADVANCED_FACE ( 'NONE', ( #248964 ), #10358, .F. ) ;
#49025 = CARTESIAN_POINT ( 'NONE',  ( -20.54999999999999716, 87.75000000001186606, -90.67310748452422331 ) ) ;
#49026 = CIRCLE ( 'NONE', #219895, 0.1000000000000016293 ) ;
#49027 = EDGE_CURVE ( 'NONE', #109568, #240894, #86289, .T. ) ;
#49028 = EDGE_LOOP ( 'NONE', ( #169057, #223948, #67492, #23262 ) ) ;
#49029 = ORIENTED_EDGE ( 'NONE', *, *, #213092, .T. ) ;
#49030 = DIRECTION ( 'NONE',  ( 0.000000000000000000, -0.9126074666063660468, -0.4088369013363524762 ) ) ;
#49031 = LINE ( 'NONE', #191141, #34999 ) ;
#49032 = DIRECTION ( 'NONE',  ( 0.000000000000000000, -0.8814952561688431665, 0.4721928772777346794 ) ) ;
#49033 = EDGE_CURVE ( 'NONE', #177021, #48432, #50717, .T. ) ;
#49034 = CYLINDRICAL_SURFACE ( 'NONE', #76608, 0.1000000000000055844 ) ;
#49035 = CARTESIAN_POINT ( 'NONE',  ( 21.05000000000000071, 85.00000000001188027, -93.12913836187181005 ) ) ;
#49036 = AXIS2_PLACEMENT_3D ( 'NONE', #92027, #132444, #208150 ) ;
#49037 = EDGE_CURVE ( 'NONE', #47890, #162856, #61198, .T. ) ;
#49039 = ADVANCED_FACE ( 'NONE', ( #27381 ), #187716, .T. ) ;
#49038 = CARTESIAN_POINT ( 'NONE',  ( -20.54999999999999716, 19.91953773510093839, -237.8616849742533077 ) ) ;
#49040 = CARTESIAN_POINT ( 'NONE',  ( -16.94333152886235894, 9.990342011450481507, -12.60796846894558954 ) ) ;
#49041 = CIRCLE ( 'NONE', #232241, 0.09999999999999939493 ) ;
#49042 = ORIENTED_EDGE ( 'NONE', *, *, #223329, .T. ) ;
#49043 = DIRECTION ( 'NONE',  ( 0.000000000000000000, 6.982962677686266711E-15, -1.000000000000000000 ) ) ;
#49044 = ADVANCED_FACE ( 'NONE', ( #208561 ), #98929, .T. ) ;
#49045 = ORIENTED_EDGE ( 'NONE', *, *, #202432, .F. ) ;
#49046 = FACE_OUTER_BOUND ( 'NONE', #18364, .T. ) ;
#49047 = FACE_OUTER_BOUND ( 'NONE', #57468, .T. ) ;
#49048 = DIRECTION ( 'NONE',  ( 0.000000000000000000, -0.2617529984165031243, -0.9651348961777157509 ) ) ;
#49049 = CARTESIAN_POINT ( 'NONE',  ( 21.06600267594171783, 22.03040400259985176, -231.7602000086088765 ) ) ;
#49050 = DIRECTION ( 'NONE',  ( 0.000000000000000000, 0.1350103645451876666, 0.9908441862701600211 ) ) ;
#49051 = CARTESIAN_POINT ( 'NONE',  ( -21.44999999999999929, 21.30332930069722863, -233.2143729774842882 ) ) ;
#49052 = VERTEX_POINT ( 'NONE', #202945 ) ;
#49053 = DIRECTION ( 'NONE',  ( -1.000000000000000000, 0.000000000000000000, 0.000000000000000000 ) ) ;
#49054 = CARTESIAN_POINT ( 'NONE',  ( -20.94999999999999929, 43.39316802731212874, -245.2602608822587342 ) ) ;
#49055 = CARTESIAN_POINT ( 'NONE',  ( -23.15000000000000213, -11.65000000000000036, -30.39999999999999503 ) ) ;
#49056 = CARTESIAN_POINT ( 'NONE',  ( 18.50000000000000000, 84.35952707724818822, -212.2592855339655671 ) ) ;
#49057 = AXIS2_PLACEMENT_3D ( 'NONE', #187276, #88121, #202963 ) ;
#49058 = AXIS2_PLACEMENT_3D ( 'NONE', #140060, #114091, #193649 ) ;
#49059 = AXIS2_PLACEMENT_3D ( 'NONE', #59545, #60854, #21756 ) ;
#49060 = CARTESIAN_POINT ( 'NONE',  ( -22.50014994444008565, 11.74971973190334218, -167.4169198432813346 ) ) ;
#49061 = ORIENTED_EDGE ( 'NONE', *, *, #242474, .T. ) ;
#49062 = CARTESIAN_POINT ( 'NONE',  ( -20.54999999999999716, 0.000000000000000000, 0.000000000000000000 ) ) ;
#49063 = LINE ( 'NONE', #138839, #17117 ) ;
#49064 = VERTEX_POINT ( 'NONE', #86835 ) ;
#49065 = EDGE_CURVE ( 'NONE', #237934, #179358, #122141, .T. ) ;
#49066 = ADVANCED_FACE ( 'NONE', ( #225060 ), #85533, .F. ) ;
#49067 = ORIENTED_EDGE ( 'NONE', *, *, #4044, .T. ) ;
#49068 = CARTESIAN_POINT ( 'NONE',  ( -16.93935632781549572, 51.64085851770598623, -231.8985589246740631 ) ) ;
#49069 = CARTESIAN_POINT ( 'NONE',  ( 21.14999999999999858, 11.19216743630477673, -211.0996217964688526 ) ) ;
#49070 = CARTESIAN_POINT ( 'NONE',  ( 20.46382478191414478, 60.87711246931931441, -225.2773833193266171 ) ) ;
#49071 = ORIENTED_EDGE ( 'NONE', *, *, #19128, .T. ) ;
#49072 = DIRECTION ( 'NONE',  ( 0.000000000000000000, 6.505213034913742890E-15, 1.000000000000000000 ) ) ;
#49073 = CARTESIAN_POINT ( 'NONE',  ( -18.59999999999999787, -1.835859311432481045, -179.0044391687985410 ) ) ;
#49074 = EDGE_CURVE ( 'NONE', #77408, #194720, #157066, .T. ) ;
#49075 = CIRCLE ( 'NONE', #11687, 1.500000000000001332 ) ;
#49076 = EDGE_LOOP ( 'NONE', ( #53155, #134455, #156123, #255881 ) ) ;
#49077 = LINE ( 'NONE', #249857, #48063 ) ;
#49078 = EDGE_LOOP ( 'NONE', ( #175442, #57809, #139929, #131918, #55916 ) ) ;
#49079 = CARTESIAN_POINT ( 'NONE',  ( 21.05000000000000071, -12.41227409413852811, -197.9999999999999432 ) ) ;
#49080 = CARTESIAN_POINT ( 'NONE',  ( 21.14999999999999503, 87.65000000001245439, -181.7731074845242745 ) ) ;
#49082 = EDGE_LOOP ( 'NONE', ( #34022, #236839, #16387, #219436, #126342, #7928, #132008, #42759, #165319, #47442 ) ) ;
#49081 = DIRECTION ( 'NONE',  ( -0.000000000000000000, 0.8660254037844383745, -0.5000000000000003331 ) ) ;
#49083 = DIRECTION ( 'NONE',  ( 1.000000000000000000, -0.000000000000000000, 0.000000000000000000 ) ) ;
#49084 = LINE ( 'NONE', #213290, #232773 ) ;
#49085 = CARTESIAN_POINT ( 'NONE',  ( -20.94999999999999929, 4.184122562697133674, -245.3714803909117279 ) ) ;
#49086 = FACE_OUTER_BOUND ( 'NONE', #52711, .T. ) ;
#49087 = DIRECTION ( 'NONE',  ( -0.000000000000000000, 1.000000000000000000, 6.982962677686267499E-15 ) ) ;
#49088 = CARTESIAN_POINT ( 'NONE',  ( 23.24999999999999645, 72.10000000001214460, -136.5231074845243597 ) ) ;
#49089 = SPHERICAL_SURFACE ( 'NONE', #249872, 0.1000000000000000056 ) ;
#49091 = EDGE_LOOP ( 'NONE', ( #13266, #104463, #43693, #230926 ) ) ;
#49090 = CARTESIAN_POINT ( 'NONE',  ( 21.14999999999999858, -11.74999999998884448, -146.2500000000000284 ) ) ;
#49092 = ORIENTED_EDGE ( 'NONE', *, *, #199738, .T. ) ;
#49094 = DIRECTION ( 'NONE',  ( 0.000000000000000000, 1.000000000000000000, -0.000000000000000000 ) ) ;
#49093 = FACE_OUTER_BOUND ( 'NONE', #253752, .T. ) ;
#49096 = ORIENTED_EDGE ( 'NONE', *, *, #101630, .T. ) ;
#49095 = FACE_OUTER_BOUND ( 'NONE', #26720, .T. ) ;
#49097 = EDGE_CURVE ( 'NONE', #113536, #111115, #90410, .T. ) ;
#49098 = CIRCLE ( 'NONE', #115747, 0.1000000000000028644 ) ;
#49099 = VERTEX_POINT ( 'NONE', #66010 ) ;
#49100 = LINE ( 'NONE', #656, #172514 ) ;
#49102 = DIRECTION ( 'NONE',  ( 1.000000000000000000, 0.000000000000000000, 0.000000000000000000 ) ) ;
#49101 = AXIS2_PLACEMENT_3D ( 'NONE', #72279, #194809, #55235 ) ;
#49103 = PLANE ( 'NONE',  #92645 ) ;
#49104 = DIRECTION ( 'NONE',  ( -0.000000000000000000, 1.000000000000000000, 0.000000000000000000 ) ) ;
#49105 = ADVANCED_FACE ( 'NONE', ( #124708 ), #204229, .F. ) ;
#49107 = CARTESIAN_POINT ( 'NONE',  ( -20.94999999999999929, -0.2561057920810652089, -133.9651035583277121 ) ) ;
#49106 = CIRCLE ( 'NONE', #182218, 0.1000000000000020595 ) ;
#49108 = CARTESIAN_POINT ( 'NONE',  ( 20.85000000000000142, 69.15387683765909799, -65.78538121767449809 ) ) ;
#49109 = EDGE_CURVE ( 'NONE', #124485, #196062, #73691, .T. ) ;
#49110 = DIRECTION ( 'NONE',  ( 1.186688945009009831E-16, -1.000000000000000000, 0.000000000000000000 ) ) ;
#49111 = ORIENTED_EDGE ( 'NONE', *, *, #24067, .T. ) ;
#49112 = ORIENTED_EDGE ( 'NONE', *, *, #46708, .T. ) ;
#49113 = ADVANCED_FACE ( 'NONE', ( #63431 ), #187314, .T. ) ;
#49114 = CARTESIAN_POINT ( 'NONE',  ( -5.900000000000003020, -11.34999999999999964, 10.10000000000000142 ) ) ;
#49115 = TOROIDAL_SURFACE ( 'NONE', #103274, 0.6000000000000017542, 0.1000000000000000056 ) ;
#49116 = EDGE_LOOP ( 'NONE', ( #250804, #91037, #201564, #68220 ) ) ;
#49117 = FACE_OUTER_BOUND ( 'NONE', #95515, .T. ) ;
#49118 = VERTEX_POINT ( 'NONE', #7317 ) ;
#49120 = CARTESIAN_POINT ( 'NONE',  ( 22.39999999999999503, 76.10085836911147794, -215.2726746080137445 ) ) ;
#49119 = AXIS2_PLACEMENT_3D ( 'NONE', #129901, #8684, #188594 ) ;
#49121 = EDGE_CURVE ( 'NONE', #77509, #247780, #239522, .T. ) ;
#49124 = EDGE_CURVE ( 'NONE', #132941, #199601, #148701, .T. ) ;
#49123 = EDGE_CURVE ( 'NONE', #127664, #13761, #115350, .T. ) ;
#49122 = AXIS2_PLACEMENT_3D ( 'NONE', #63018, #202539, #109846 ) ;
#49125 = CARTESIAN_POINT ( 'NONE',  ( 23.14999999999999503, 11.65000000001116298, -179.6499999999999773 ) ) ;
#49126 = LINE ( 'NONE', #28326, #106655 ) ;
#49127 = DIRECTION ( 'NONE',  ( 0.000000000000000000, -6.853228547068871147E-15, 1.000000000000000000 ) ) ;
#49128 = ORIENTED_EDGE ( 'NONE', *, *, #61506, .T. ) ;
#49129 = FACE_OUTER_BOUND ( 'NONE', #244644, .T. ) ;
#49130 = ORIENTED_EDGE ( 'NONE', *, *, #75866, .F. ) ;
#49131 = DIRECTION ( 'NONE',  ( 0.000000000000000000, -0.9856811345164800953, -0.1686199900910462790 ) ) ;
#49132 = CARTESIAN_POINT ( 'NONE',  ( 18.50000000000000000, 85.50000000001136868, -29.42291809330221142 ) ) ;
#49133 = DIRECTION ( 'NONE',  ( 0.000000000000000000, -0.9579639084728133192, -0.2868887416116073785 ) ) ;
#49134 = ORIENTED_EDGE ( 'NONE', *, *, #253984, .T. ) ;
#49135 = CARTESIAN_POINT ( 'NONE',  ( -20.94999999999999929, 70.15000000001211333, -126.3906102602463619 ) ) ;
#49136 = AXIS2_PLACEMENT_3D ( 'NONE', #193408, #73473, #151726 ) ;
#49137 = EDGE_LOOP ( 'NONE', ( #110780, #186774, #95827, #124245, #238414 ) ) ;
#49140 = ORIENTED_EDGE ( 'NONE', *, *, #194516, .T. ) ;
#49139 = CARTESIAN_POINT ( 'NONE',  ( 18.50596464788227280, 46.37740828070798216, -243.0652246697500800 ) ) ;
#49138 = CARTESIAN_POINT ( 'NONE',  ( -16.27683809663750480, 60.62847850914943137, -224.4802381816402317 ) ) ;
#49141 = EDGE_CURVE ( 'NONE', #207603, #130702, #173683, .T. ) ;
#49142 = DIRECTION ( 'NONE',  ( 0.000000000000000000, 0.000000000000000000, -1.000000000000000000 ) ) ;
#49144 = EDGE_CURVE ( 'NONE', #211794, #116420, #15423, .T. ) ;
#49143 = CIRCLE ( 'NONE', #215722, 0.2000000000000057288 ) ;
#49145 = ORIENTED_EDGE ( 'NONE', *, *, #100524, .T. ) ;
#49146 = VECTOR ( 'NONE', #64940, 1000.000000000000000 ) ;
#49147 = CARTESIAN_POINT ( 'NONE',  ( -20.54999999999999716, 78.50726470275243685, -228.6618886302502176 ) ) ;
#49148 = ORIENTED_EDGE ( 'NONE', *, *, #204444, .T. ) ;
#49149 = AXIS2_PLACEMENT_3D ( 'NONE', #51345, #130922, #53947 ) ;
#49150 = CIRCLE ( 'NONE', #19951, 0.1000000000000028644 ) ;
#49151 = EDGE_CURVE ( 'NONE', #250043, #191668, #161155, .T. ) ;
#49152 = CARTESIAN_POINT ( 'NONE',  ( -20.54999999999999716, 85.40000000001221281, -146.4170766071767389 ) ) ;
#49153 = CIRCLE ( 'NONE', #228243, 4.300000000000032685 ) ;
#49154 = DIRECTION ( 'NONE',  ( 1.000000000000000000, 0.000000000000000000, 0.000000000000000000 ) ) ;
#49155 = FACE_OUTER_BOUND ( 'NONE', #188507, .T. ) ;
#49156 = DIRECTION ( 'NONE',  ( -1.000000000000000000, 0.000000000000000000, 0.000000000000000000 ) ) ;
#49157 = ADVANCED_FACE ( 'NONE', ( #171266 ), #19697, .F. ) ;
#49158 = VERTEX_POINT ( 'NONE', #168698 ) ;
#49160 = ADVANCED_FACE ( 'NONE', ( #6996 ), #206489, .F. ) ;
#49159 = CARTESIAN_POINT ( 'NONE',  ( -20.65000000000000568, 7.249999999999983125, -20.85000000000000142 ) ) ;
#49161 = CARTESIAN_POINT ( 'NONE',  ( 18.49999999999998934, 10.29288807859941457, -139.4580020160121876 ) ) ;
#49162 = EDGE_LOOP ( 'NONE', ( #97576, #221972, #47261, #21108 ) ) ;
#49163 = DIRECTION ( 'NONE',  ( 0.000000000000000000, -1.224646799142015331E-16, 1.000000000000000000 ) ) ;
#49165 = EDGE_LOOP ( 'NONE', ( #229805, #15581, #43372, #82638 ) ) ;
#49164 = AXIS2_PLACEMENT_3D ( 'NONE', #241575, #25121, #107192 ) ;
#49167 = TOROIDAL_SURFACE ( 'NONE', #3350, 12.97499999999999609, 0.1000000000000000056 ) ;
#49166 = DIRECTION ( 'NONE',  ( -1.073024830501117725E-15, -6.982962677686266711E-15, 1.000000000000000000 ) ) ;
#49168 = ORIENTED_EDGE ( 'NONE', *, *, #206645, .T. ) ;
#49169 = DIRECTION ( 'NONE',  ( 0.000000000000000000, 0.5000000000000144329, 0.8660254037844302699 ) ) ;
#49170 = DIRECTION ( 'NONE',  ( 0.000000000000000000, 0.000000000000000000, 1.000000000000000000 ) ) ;
#49172 = ORIENTED_EDGE ( 'NONE', *, *, #255430, .T. ) ;
#49171 = CARTESIAN_POINT ( 'NONE',  ( -16.87998658237752281, 44.33045077069872519, -235.2115878677316800 ) ) ;
#49173 = ADVANCED_FACE ( 'NONE', ( #30435 ), #226014, .T. ) ;
#49174 = DIRECTION ( 'NONE',  ( 0.000000000000000000, 6.982962677686266711E-15, -1.000000000000000000 ) ) ;
#49175 = CARTESIAN_POINT ( 'NONE',  ( -14.56336952470180179, 62.93307127222839625, -215.6135269849708607 ) ) ;
#49176 = VECTOR ( 'NONE', #16593, 1000.000000000000000 ) ;
#49177 = CARTESIAN_POINT ( 'NONE',  ( -20.94999999999999929, 28.51339163295720169, -258.4040038037771865 ) ) ;
#49178 = VECTOR ( 'NONE', #173435, 1000.000000000000000 ) ;
#49179 = ORIENTED_EDGE ( 'NONE', *, *, #173741, .F. ) ;
#49180 = EDGE_CURVE ( 'NONE', #116426, #152553, #48717, .T. ) ;
#49181 = DIRECTION ( 'NONE',  ( -1.000000000000000000, -7.304098846218134667E-16, 0.000000000000000000 ) ) ;
#49182 = VECTOR ( 'NONE', #201057, 1000.000000000000000 ) ;
#49183 = VERTEX_POINT ( 'NONE', #48684 ) ;
#49184 = DIRECTION ( 'NONE',  ( -1.000000000000000000, 0.000000000000000000, 0.000000000000000000 ) ) ;
#49185 = ORIENTED_EDGE ( 'NONE', *, *, #129223, .T. ) ;
#49186 = TOROIDAL_SURFACE ( 'NONE', #140783, 0.6000000000000009770, 0.1000000000000000056 ) ;
#49187 = CARTESIAN_POINT ( 'NONE',  ( 15.74999999999999645, 9.350000000011139178, -117.2500000000000284 ) ) ;
#49188 = DIRECTION ( 'NONE',  ( 0.000000000000000000, -0.9868171638914232657, 0.1618390714546023845 ) ) ;
#49189 = ADVANCED_FACE ( 'NONE', ( #46119 ), #210350, .F. ) ;
#49190 = AXIS2_PLACEMENT_3D ( 'NONE', #187135, #226197, #69747 ) ;
#49193 = VERTEX_POINT ( 'NONE', #51234 ) ;
#49192 = ORIENTED_EDGE ( 'NONE', *, *, #81195, .T. ) ;
#49191 = DIRECTION ( 'NONE',  ( 0.000000000000000000, 0.000000000000000000, -1.000000000000000000 ) ) ;
#49194 = DIRECTION ( 'NONE',  ( 1.000000000000000000, 0.000000000000000000, 0.000000000000000000 ) ) ;
#49195 = CIRCLE ( 'NONE', #157391, 0.1000000000000008937 ) ;
#49196 = LINE ( 'NONE', #11363, #48250 ) ;
#49197 = CIRCLE ( 'NONE', #224168, 0.09999999999998898659 ) ;
#49198 = DIRECTION ( 'NONE',  ( 0.000000000000000000, -0.4791956752371546169, -0.8777080977375152360 ) ) ;
#49199 = VECTOR ( 'NONE', #22836, 1000.000000000000000 ) ;
#49201 = CARTESIAN_POINT ( 'NONE',  ( 20.94999999999999574, 87.48912529308769592, -66.52310748452423184 ) ) ;
#49200 = DIRECTION ( 'NONE',  ( 0.000000000000000000, 0.000000000000000000, 1.000000000000000000 ) ) ;
#49202 = FACE_OUTER_BOUND ( 'NONE', #38986, .T. ) ;
#49203 = CARTESIAN_POINT ( 'NONE',  ( -23.25000000000000000, 7.128833340093095217, -233.7327013124392749 ) ) ;
#49204 = DIRECTION ( 'NONE',  ( 1.000000000000000000, 0.000000000000000000, 0.000000000000000000 ) ) ;
#49205 = TOROIDAL_SURFACE ( 'NONE', #41048, 0.2000000000000000111, 0.1000000000000000056 ) ;
#49206 = CARTESIAN_POINT ( 'NONE',  ( 20.95512820512820440, 8.876151316299271343, -179.6499999999999773 ) ) ;
#49207 = EDGE_LOOP ( 'NONE', ( #14278, #69401, #96800, #57535 ) ) ;
#49208 = ORIENTED_EDGE ( 'NONE', *, *, #219471, .T. ) ;
#49209 = CARTESIAN_POINT ( 'NONE',  ( -18.50000000000000000, 77.16412189325360771, -162.1082593989527254 ) ) ;
#49211 = ORIENTED_EDGE ( 'NONE', *, *, #39372, .F. ) ;
#49210 = CARTESIAN_POINT ( 'NONE',  ( -23.25000000000000000, 64.35000000001222986, -148.2731074845243882 ) ) ;
#49212 = VERTEX_POINT ( 'NONE', #149100 ) ;
#49213 = DIRECTION ( 'NONE',  ( 0.000000000000000000, 0.8814952561688476074, -0.4721928772777262417 ) ) ;
#49214 = ORIENTED_EDGE ( 'NONE', *, *, #142696, .T. ) ;
#49215 = DIRECTION ( 'NONE',  ( -1.000000000000000000, -0.000000000000000000, -0.000000000000000000 ) ) ;
#49216 = CIRCLE ( 'NONE', #215797, 0.1000000000000106498 ) ;
#49217 = ORIENTED_EDGE ( 'NONE', *, *, #96471, .T. ) ;
#49218 = CARTESIAN_POINT ( 'NONE',  ( -16.88853107394619357, 66.04912151666525233, -149.1701711376321953 ) ) ;
#49219 = CARTESIAN_POINT ( 'NONE',  ( -23.25000000000000000, 76.00000000001170974, -69.52310748452431710 ) ) ;
#49220 = AXIS2_PLACEMENT_3D ( 'NONE', #118711, #225468, #27336 ) ;
#49222 = ORIENTED_EDGE ( 'NONE', *, *, #107691, .T. ) ;
#49221 = VERTEX_POINT ( 'NONE', #90379 ) ;
#49223 = ORIENTED_EDGE ( 'NONE', *, *, #49394, .F. ) ;
#49224 = DIRECTION ( 'NONE',  ( 0.000000000000000000, 1.000000000000000000, 2.891205793294679805E-16 ) ) ;
#49225 = VERTEX_POINT ( 'NONE', #228641 ) ;
#49226 = VERTEX_POINT ( 'NONE', #49976 ) ;
#49227 = CARTESIAN_POINT ( 'NONE',  ( -20.01715728752537515, 4.611773100472912112, 22.11686199900910665 ) ) ;
#49228 = CARTESIAN_POINT ( 'NONE',  ( 18.39999999999999858, -9.682403433465241349, -73.65684337741279819 ) ) ;
#49229 = CARTESIAN_POINT ( 'NONE',  ( 21.05000000000000071, 8.815452279208699338, -75.42039255261430242 ) ) ;
#49231 = EDGE_LOOP ( 'NONE', ( #76206, #163142 ) ) ;
#49230 = DIRECTION ( 'NONE',  ( 0.000000000000000000, -0.5000000000000275335, -0.8660254037844228314 ) ) ;
#49232 = DIRECTION ( 'NONE',  ( 0.000000000000000000, 0.000000000000000000, 1.000000000000000000 ) ) ;
#49233 = CARTESIAN_POINT ( 'NONE',  ( 22.39999999999999858, 7.790779598384538041, -167.4999999999999432 ) ) ;
#49235 = VERTEX_POINT ( 'NONE', #189500 ) ;
#49234 = CARTESIAN_POINT ( 'NONE',  ( 21.05000000000000071, 76.00000000001186606, -90.14810748452431710 ) ) ;
#49236 = CARTESIAN_POINT ( 'NONE',  ( -21.45000000000000284, 7.708578643773852157, -188.7499999999999716 ) ) ;
#49237 = ORIENTED_EDGE ( 'NONE', *, *, #194218, .F. ) ;
#49238 = CARTESIAN_POINT ( 'NONE',  ( -1.820710678118658388, 85.92928932189310842, -78.37310748452424036 ) ) ;
#49239 = ORIENTED_EDGE ( 'NONE', *, *, #255314, .F. ) ;
#49240 = FACE_OUTER_BOUND ( 'NONE', #13249, .T. ) ;
#49241 = CARTESIAN_POINT ( 'NONE',  ( -16.92570016628983254, 30.23634993850275521, -234.8131561248061701 ) ) ;
#49242 = EDGE_CURVE ( 'NONE', #147359, #48110, #250741, .T. ) ;
#49243 = ORIENTED_EDGE ( 'NONE', *, *, #58339, .T. ) ;
#49244 = AXIS2_PLACEMENT_3D ( 'NONE', #92967, #120282, #142362 ) ;
#49245 = AXIS2_PLACEMENT_3D ( 'NONE', #87790, #112523, #69553 ) ;
#49248 = CARTESIAN_POINT ( 'NONE',  ( 22.39999999999999503, 11.65000000000000746, 0.09999999999999592548 ) ) ;
#49247 = CIRCLE ( 'NONE', #115895, 0.2000000000000057288 ) ;
#49246 = DIRECTION ( 'NONE',  ( 1.000000000000000000, 0.000000000000000000, 0.000000000000000000 ) ) ;
#49249 = AXIS2_PLACEMENT_3D ( 'NONE', #72437, #33334, #11165 ) ;
#49250 = CARTESIAN_POINT ( 'NONE',  ( 20.94999999999999929, 28.43730376342110944, -239.4748853164439879 ) ) ;
#49251 = DIRECTION ( 'NONE',  ( -0.000000000000000000, 0.2128009952263604232, -0.9770955615653316162 ) ) ;
#49252 = LINE ( 'NONE', #144479, #130869 ) ;
#49253 = ORIENTED_EDGE ( 'NONE', *, *, #114664, .T. ) ;
#49254 = VERTEX_POINT ( 'NONE', #129523 ) ;
#49255 = FACE_OUTER_BOUND ( 'NONE', #15127, .T. ) ;
#49256 = ORIENTED_EDGE ( 'NONE', *, *, #97630, .T. ) ;
#49257 = DIRECTION ( 'NONE',  ( 0.000000000000000000, 0.7397360091702755991, -0.6728971962616832059 ) ) ;
#49258 = EDGE_LOOP ( 'NONE', ( #107562, #185036, #152079, #224520, #135766, #42370, #51250, #186445, #182657, #166634, #154376, #190901, #247545, #15387, #151696, #185396, #227966, #181924 ) ) ;
#49259 = EDGE_CURVE ( 'NONE', #115014, #5081, #244523, .T. ) ;
#49260 = CARTESIAN_POINT ( 'NONE',  ( -22.50875500270928598, -0.1008579137641426871, -55.25043287260216118 ) ) ;
#49261 = DIRECTION ( 'NONE',  ( 0.000000000000000000, 0.2128009952263603677, -0.9770955615653313941 ) ) ;
#49262 = EDGE_CURVE ( 'NONE', #49118, #121114, #209056, .T. ) ;
#49263 = CARTESIAN_POINT ( 'NONE',  ( -18.50000000000000000, 77.13501884592203339, -95.30613060109196510 ) ) ;
#49264 = AXIS2_PLACEMENT_3D ( 'NONE', #27890, #184346, #4424 ) ;
#49265 = ORIENTED_EDGE ( 'NONE', *, *, #38189, .T. ) ;
#49266 = CARTESIAN_POINT ( 'NONE',  ( 18.33683296300592147, -9.511149971122062396, -207.9057074127082956 ) ) ;
#49267 =( NAMED_UNIT ( * ) PLANE_ANGLE_UNIT ( ) SI_UNIT ( $, .RADIAN. ) );
#49268 = ORIENTED_EDGE ( 'NONE', *, *, #107633, .T. ) ;
#49269 = AXIS2_PLACEMENT_3D ( 'NONE', #71391, #148340, #209600 ) ;
#49270 = EDGE_LOOP ( 'NONE', ( #89828, #134132, #173243, #223578 ) ) ;
#49271 = EDGE_LOOP ( 'NONE', ( #182364, #133661, #72347, #203382 ) ) ;
#49272 = EDGE_CURVE ( 'NONE', #10605, #123853, #47396, .T. ) ;
#49273 = DIRECTION ( 'NONE',  ( 1.000000000000000000, 0.000000000000000000, 0.000000000000000000 ) ) ;
#49274 = CARTESIAN_POINT ( 'NONE',  ( -23.15000000000000213, 31.44980407958351165, -233.5445995079518866 ) ) ;
#49276 = ADVANCED_FACE ( 'NONE', ( #167390, #190812, #128243 ), #12166, .F. ) ;
#49275 = DIRECTION ( 'NONE',  ( -1.000000000000000000, 0.000000000000000000, 0.000000000000000000 ) ) ;
#49277 = DIRECTION ( 'NONE',  ( 0.000000000000000000, -1.000000000000000000, 0.000000000000000000 ) ) ;
#49278 = CARTESIAN_POINT ( 'NONE',  ( -21.00023020733502932, 1.115541036281197940E-11, -161.1091307547316376 ) ) ;
#49280 = ORIENTED_EDGE ( 'NONE', *, *, #114406, .F. ) ;
#49279 = CARTESIAN_POINT ( 'NONE',  ( -21.05000000000000071, 61.06354069362765813, -234.0936775124800704 ) ) ;
#49281 = DIRECTION ( 'NONE',  ( -0.000000000000000000, 1.000000000000000000, -0.000000000000000000 ) ) ;
#49282 = ORIENTED_EDGE ( 'NONE', *, *, #23406, .F. ) ;
#49283 = EDGE_CURVE ( 'NONE', #240428, #246816, #173833, .T. ) ;
#49284 = CARTESIAN_POINT ( 'NONE',  ( -20.64999999999999858, 2.000000000011154189, -46.72462192276210402 ) ) ;
#49285 = ORIENTED_EDGE ( 'NONE', *, *, #1060, .F. ) ;
#49286 = ORIENTED_EDGE ( 'NONE', *, *, #230286, .F. ) ;
#49287 = DIRECTION ( 'NONE',  ( -0.7071067811865474617, 0.7071067811865474617, 0.000000000000000000 ) ) ;
#49288 = CARTESIAN_POINT ( 'NONE',  ( -18.39999999999999858, 64.25000000001233502, -160.7731074845244450 ) ) ;
#49289 = CARTESIAN_POINT ( 'NONE',  ( -16.94445028196807002, 66.00793639031378746, -48.63043766294283898 ) ) ;
#49290 = CYLINDRICAL_SURFACE ( 'NONE', #112592, 0.09999999999998898659 ) ;
#49291 = ADVANCED_FACE ( 'NONE', ( #195933 ), #23813, .F. ) ;
#49292 = CIRCLE ( 'NONE', #253289, 4.149999999999996803 ) ;
#49293 = AXIS2_PLACEMENT_3D ( 'NONE', #10410, #9121, #226872 ) ;
#49294 = AXIS2_PLACEMENT_3D ( 'NONE', #209727, #231878, #31128 ) ;
#49295 = DIRECTION ( 'NONE',  ( 0.000000000000000000, -0.4930308989875575865, -0.8700118002898125091 ) ) ;
#49296 = ORIENTED_EDGE ( 'NONE', *, *, #247327, .F. ) ;
#49298 = ORIENTED_EDGE ( 'NONE', *, *, #9631, .F. ) ;
#49297 = ADVANCED_FACE ( 'NONE', ( #155538 ), #119651, .T. ) ;
#49299 = FACE_OUTER_BOUND ( 'NONE', #71276, .T. ) ;
#49300 = ORIENTED_EDGE ( 'NONE', *, *, #104701, .F. ) ;
#49301 = DIRECTION ( 'NONE',  ( 1.000000000000000000, 0.000000000000000000, 0.000000000000000000 ) ) ;
#49302 = ORIENTED_EDGE ( 'NONE', *, *, #78739, .F. ) ;
#49304 = LINE ( 'NONE', #114419, #207122 ) ;
#49303 = AXIS2_PLACEMENT_3D ( 'NONE', #61563, #100648, #257136 ) ;
#49305 = CARTESIAN_POINT ( 'NONE',  ( -17.71734398241074260, 53.42160327193604985, -230.1610529824684193 ) ) ;
#49306 = FACE_BOUND ( 'NONE', #75797, .T. ) ;
#49307 = DIRECTION ( 'NONE',  ( 0.000000000000000000, 0.000000000000000000, -1.000000000000000000 ) ) ;
#49308 = EDGE_LOOP ( 'NONE', ( #238676, #131710, #141585, #83052, #229085, #27460 ) ) ;
#49309 = DIRECTION ( 'NONE',  ( 0.000000000000000000, -0.9594490217226103734, -0.2818822000686205254 ) ) ;
#49310 = CARTESIAN_POINT ( 'NONE',  ( 22.39999999999999503, 11.65000000001116298, -33.40000000000000568 ) ) ;
#49311 = DIRECTION ( 'NONE',  ( 0.000000000000000000, -1.000000000000000000, 0.000000000000000000 ) ) ;
#49312 = ADVANCED_FACE ( 'NONE', ( #57663 ), #240273, .F. ) ;
#49313 = CARTESIAN_POINT ( 'NONE',  ( 20.85000000000000142, -1.835859311432481045, -179.0044391687985410 ) ) ;
#49314 = CARTESIAN_POINT ( 'NONE',  ( 20.73486653747090003, 7.250000000011182166, -54.35000000000000142 ) ) ;
#49315 = CIRCLE ( 'NONE', #215699, 0.8750000000000007772 ) ;
#49316 = FACE_OUTER_BOUND ( 'NONE', #237659, .T. ) ;
#49317 = VECTOR ( 'NONE', #207730, 1000.000000000000000 ) ;
#49318 = AXIS2_PLACEMENT_3D ( 'NONE', #227423, #44945, #249577 ) ;
#49319 = VERTEX_POINT ( 'NONE', #252026 ) ;
#49320 = VECTOR ( 'NONE', #69257, 1000.000000000000000 ) ;
#49321 = CARTESIAN_POINT ( 'NONE',  ( 23.14999999999999147, 9.088433780795693195, -230.0744959993385805 ) ) ;
#49322 = ORIENTED_EDGE ( 'NONE', *, *, #140112, .T. ) ;
#49323 = CARTESIAN_POINT ( 'NONE',  ( -18.40000000000000213, 11.41458325961095177, -121.3500000000000227 ) ) ;
#49324 = DIRECTION ( 'NONE',  ( 1.000000000000000000, 0.000000000000000000, -0.000000000000000000 ) ) ;
#49325 = CARTESIAN_POINT ( 'NONE',  ( 18.59999999999999432, 74.83729825007431202, -161.9231074845243654 ) ) ;
#49326 = LINE ( 'NONE', #22408, #107005 ) ;
#49327 = CIRCLE ( 'NONE', #195093, 14.30833333333333890 ) ;
#49328 = ORIENTED_EDGE ( 'NONE', *, *, #24179, .T. ) ;
#49329 = FACE_OUTER_BOUND ( 'NONE', #243486, .T. ) ;
#49330 = CARTESIAN_POINT ( 'NONE',  ( 23.24999999999999645, 71.00000000001223555, -148.9283735034374843 ) ) ;
#49331 = DIRECTION ( 'NONE',  ( -1.000000000000000000, 3.265361837132813093E-16, 2.280189983783949500E-30 ) ) ;
#49332 = DIRECTION ( 'NONE',  ( -1.000000000000000000, 1.387778780781454006E-13, 0.000000000000000000 ) ) ;
#49333 = LINE ( 'NONE', #105420, #144552 ) ;
#49334 = EDGE_CURVE ( 'NONE', #224010, #56398, #92952, .T. ) ;
#49335 = CIRCLE ( 'NONE', #224115, 0.09999999999999939493 ) ;
#49336 = CIRCLE ( 'NONE', #195107, 0.1000000000000033223 ) ;
#49338 = ORIENTED_EDGE ( 'NONE', *, *, #174541, .T. ) ;
#49337 = CIRCLE ( 'NONE', #7657, 0.09999999999999939493 ) ;
#49339 = ORIENTED_EDGE ( 'NONE', *, *, #23161, .T. ) ;
#49340 = CARTESIAN_POINT ( 'NONE',  ( -16.94107738177415712, 12.45552124806248706, -211.1315092113344463 ) ) ;
#49342 = DIRECTION ( 'NONE',  ( 0.000000000000000000, -1.000000000000000000, -6.982962677686265922E-15 ) ) ;
#49341 = AXIS2_PLACEMENT_3D ( 'NONE', #49138, #128697, #208240 ) ;
#49343 = DIRECTION ( 'NONE',  ( 0.000000000000000000, 0.000000000000000000, 1.000000000000000000 ) ) ;
#49344 = CARTESIAN_POINT ( 'NONE',  ( 11.60000000000000320, -11.75000000000000000, 12.30000000000000426 ) ) ;
#49345 =( BOUNDED_SURFACE ( )  B_SPLINE_SURFACE ( 3, 2, ( 
 ( #148752, #32688, #110893 ),
 ( #129183, #229569, #150041 ),
 ( #210006, #53490, #251685 ),
 ( #93890, #172206, #133038 ) ),
 .UNSPECIFIED., .F., .F., .F. ) 
 B_SPLINE_SURFACE_WITH_KNOTS ( ( 4, 4 ),
 ( 3, 3 ),
 ( 0.0006461284895274040097, 0.0007503702773986319378 ),
 ( 0.000000000000000000, 1.000000000000000000 ),
 .UNSPECIFIED. ) 
 GEOMETRIC_REPRESENTATION_ITEM ( )  RATIONAL_B_SPLINE_SURFACE ( (
 ( 1.000000000000000000, 0.7071067811865471286, 1.000000000000000000),
 ( 1.000000000000000000, 0.7076476444648849284, 1.000000000000000000),
 ( 1.000000000000000000, 0.7075727925191714895, 1.000000000000000000),
 ( 1.000000000000000000, 0.7071067811865475727, 1.000000000000000000) ) ) 
 REPRESENTATION_ITEM ( '' )  SURFACE ( )  );
#49346 = CARTESIAN_POINT ( 'NONE',  ( 22.59999999999999432, 11.74987124438766273, -33.43457040898632471 ) ) ;
#49347 = VECTOR ( 'NONE', #243231, 999.9999999999998863 ) ;
#49348 = EDGE_CURVE ( 'NONE', #117400, #130735, #73427, .T. ) ;
#49349 = EDGE_CURVE ( 'NONE', #83073, #140260, #186093, .T. ) ;
#49350 = VERTEX_POINT ( 'NONE', #75968 ) ;
#49351 = DIRECTION ( 'NONE',  ( -1.000000000000000000, 0.000000000000000000, 0.000000000000000000 ) ) ;
#49352 = CONTEXT_DEPENDENT_SHAPE_REPRESENTATION ( #5890, #139123 ) ;
#49353 = DIRECTION ( 'NONE',  ( -0.000000000000000000, -0.000000000000000000, 1.000000000000000000 ) ) ;
#49354 = EDGE_CURVE ( 'NONE', #83776, #187034, #36275, .T. ) ;
#49355 = VERTEX_POINT ( 'NONE', #232494 ) ;
#49356 = DIRECTION ( 'NONE',  ( 0.000000000000000000, 0.000000000000000000, 1.000000000000000000 ) ) ;
#49357 = PRODUCT ( 'Snap Open Cable Crossbars 11', 'Snap Open Cable Crossbars 11', '', ( #173516 ) ) ;
#49358 = EDGE_CURVE ( 'NONE', #144142, #55598, #156819, .T. ) ;
#49360 = EDGE_CURVE ( 'NONE', #196735, #27978, #49327, .T. ) ;
#49359 = AXIS2_PLACEMENT_3D ( 'NONE', #222647, #80559, #3611 ) ;
#49361 = VECTOR ( 'NONE', #50921, 1000.000000000000000 ) ;
#49362 = CLOSED_SHELL ( 'NONE', ( #250430, #92543, #2477, #12966, #239687, #126683, #163600, #226910, #94229, #216332, #185328, #40272, #206463, #231341, #191825, #130510, #47392, #91707, #57887, #193128, #42315, #157460, #68631, #20255, #137924, #126022, #123603, #2568, #185082, #206354, #159569, #254867, #161591, #191092, #37022, #256040, #64070, #115225, #193009, #56992, #88417, #89308, #94726, #96986, #215951, #17265, #49381, #245747, #249818, #160442, #166099, #89587, #19490 ) ) ;
#49363 = VERTEX_POINT ( 'NONE', #132087 ) ;
#49364 = ORIENTED_EDGE ( 'NONE', *, *, #250849, .F. ) ;
#49365 = EDGE_CURVE ( 'NONE', #158454, #216204, #96775, .T. ) ;
#49366 = EDGE_LOOP ( 'NONE', ( #162713, #122274, #50244, #138814, #41239 ) ) ;
#49367 = FACE_OUTER_BOUND ( 'NONE', #192602, .T. ) ;
#49368 = CARTESIAN_POINT ( 'NONE',  ( 22.39999999999999503, 11.75000000000000711, -0.1000000000000028644 ) ) ;
#49369 = CARTESIAN_POINT ( 'NONE',  ( 21.05000000000000071, 10.72371711693665652, -112.6762396011380218 ) ) ;
#49370 = FACE_OUTER_BOUND ( 'NONE', #3526, .T. ) ;
#49372 = AXIS2_PLACEMENT_3D ( 'NONE', #179213, #76216, #239161 ) ;
#49371 = DIRECTION ( 'NONE',  ( 0.000000000000000000, -6.938893903907222067E-15, 1.000000000000000000 ) ) ;
#49373 = DIRECTION ( 'NONE',  ( 1.000000000000000000, 0.000000000000000000, 0.000000000000000000 ) ) ;
#49374 = LINE ( 'NONE', #145888, #243193 ) ;
#49375 = AXIS2_PLACEMENT_3D ( 'NONE', #228573, #167331, #246829 ) ;
#49377 = DIRECTION ( 'NONE',  ( 0.000000000000000000, -0.5826443254700256480, -0.8127272543710952757 ) ) ;
#49376 = DIRECTION ( 'NONE',  ( 0.000000000000000000, 0.000000000000000000, -1.000000000000000000 ) ) ;
#49378 = FACE_OUTER_BOUND ( 'NONE', #126303, .T. ) ;
#49379 = VECTOR ( 'NONE', #157822, 1000.000000000000000 ) ;
#49381 = ADVANCED_FACE ( 'NONE', ( #112533 ), #9096, .T. ) ;
#49380 = CARTESIAN_POINT ( 'NONE',  ( 20.27550659511089037, 9.216043722508848290, -12.65000000000000391 ) ) ;
#49382 = LINE ( 'NONE', #209739, #163020 ) ;
#49383 = DIRECTION ( 'NONE',  ( -3.265361837132813093E-16, -1.000000000000000000, -6.982962677686266711E-15 ) ) ;
#49384 = VERTEX_POINT ( 'NONE', #38139 ) ;
#49385 = ORIENTED_EDGE ( 'NONE', *, *, #201857, .F. ) ;
#49386 = CARTESIAN_POINT ( 'NONE',  ( -20.54999999999999716, 6.878457983866232972, -212.1414458560986986 ) ) ;
#49387 = DIRECTION ( 'NONE',  ( 0.000000000000000000, 0.000000000000000000, 1.000000000000000000 ) ) ;
#49388 = FACE_OUTER_BOUND ( 'NONE', #112711, .T. ) ;
#49389 = AXIS2_PLACEMENT_3D ( 'NONE', #256369, #161196, #238144 ) ;
#49390 = EDGE_CURVE ( 'NONE', #37051, #101165, #19476, .T. ) ;
#49391 = CARTESIAN_POINT ( 'NONE',  ( 20.95265033839679347, 39.26570085966146451, -236.8644406904388404 ) ) ;
#49392 = CARTESIAN_POINT ( 'NONE',  ( -20.54999999999999716, 85.00000000001222134, -146.4170766071767389 ) ) ;
#49393 = CARTESIAN_POINT ( 'NONE',  ( -22.16821283564876666, 7.385839301279057523, -199.3914429501938343 ) ) ;
#49394 = EDGE_CURVE ( 'NONE', #54600, #140913, #184045, .T. ) ;
#49395 = ADVANCED_FACE ( 'NONE', ( #4123 ), #64108, .F. ) ;
#49396 = ORIENTED_EDGE ( 'NONE', *, *, #246489, .F. ) ;
#49397 = ORIENTED_EDGE ( 'NONE', *, *, #38942, .T. ) ;
#49398 = VECTOR ( 'NONE', #215752, 1000.000000000000000 ) ;
#49399 = CIRCLE ( 'NONE', #41043, 0.8750000000000007772 ) ;
#49400 = DIRECTION ( 'NONE',  ( 0.000000000000000000, 0.000000000000000000, 1.000000000000000000 ) ) ;
#49401 = ORIENTED_EDGE ( 'NONE', *, *, #168005, .F. ) ;
#49402 = DIRECTION ( 'NONE',  ( 0.000000000000000000, -0.2128009952263604232, 0.9770955615653316162 ) ) ;
#49403 = DIRECTION ( 'NONE',  ( -3.787827842127535236E-15, 0.7397360091702777085, 0.6728971962616808744 ) ) ;
#49404 = ORIENTED_EDGE ( 'NONE', *, *, #131432, .T. ) ;
#49405 = DIRECTION ( 'NONE',  ( -1.000000000000000000, 0.000000000000000000, 0.000000000000000000 ) ) ;
#49406 = EDGE_LOOP ( 'NONE', ( #35832, #119218, #185011, #74697 ) ) ;
#49407 = DIRECTION ( 'NONE',  ( 4.239556034732056743E-17, -0.1298341882520022972, -0.9915357197604853789 ) ) ;
#49408 = LINE ( 'NONE', #29873, #3131 ) ;
#49410 = FACE_OUTER_BOUND ( 'NONE', #221320, .T. ) ;
#49409 = AXIS2_PLACEMENT_3D ( 'NONE', #184740, #146885, #247279 ) ;
#49411 = CARTESIAN_POINT ( 'NONE',  ( -21.05000000000000071, 61.17710000698043871, -234.1095691268366465 ) ) ;
#49412 = CARTESIAN_POINT ( 'NONE',  ( -23.15000000000000213, 74.97916330618690495, -207.2871335796180006 ) ) ;
#49413 = CARTESIAN_POINT ( 'NONE',  ( 20.46382478191414833, 10.51603790215317602, -207.4557705628764666 ) ) ;
#49414 = DIRECTION ( 'NONE',  ( -1.000000000000000000, 2.952720810173289112E-16, 2.061873921506763405E-30 ) ) ;
#49415 = CARTESIAN_POINT ( 'NONE',  ( -22.59999999999999787, 64.05844819680034163, -247.1686437718134073 ) ) ;
#49417 = ORIENTED_EDGE ( 'NONE', *, *, #154083, .T. ) ;
#49416 = DIRECTION ( 'NONE',  ( -3.469446951953426755E-14, -0.2128009952263403282, 0.9770955615653358350 ) ) ;
#49419 = PLANE ( 'NONE',  #251751 ) ;
#49418 = CARTESIAN_POINT ( 'NONE',  ( -18.59999999999999787, 68.48451787451661232, -224.2224406095231757 ) ) ;
#49420 = ORIENTED_EDGE ( 'NONE', *, *, #114088, .T. ) ;
#49422 = EDGE_LOOP ( 'NONE', ( #195189, #60233, #14027, #174332 ) ) ;
#49421 = CARTESIAN_POINT ( 'NONE',  ( 18.49999999999999289, 11.75000000001115552, -192.3499999999999659 ) ) ;
#49423 = ORIENTED_EDGE ( 'NONE', *, *, #225077, .T. ) ;
#49424 = CARTESIAN_POINT ( 'NONE',  ( 18.39999999999999858, 46.91436717984746707, -255.3877622108296634 ) ) ;
#49425 = CYLINDRICAL_SURFACE ( 'NONE', #151195, 0.09999999999999939493 ) ;
#49426 = LINE ( 'NONE', #91117, #150557 ) ;
#49427 = DIRECTION ( 'NONE',  ( 0.000000000000000000, -0.2617529984164955192, -0.9651348961777178603 ) ) ;
#49428 = CARTESIAN_POINT ( 'NONE',  ( 18.59999999999999076, 39.24721131055453327, -235.5164460677962666 ) ) ;
#49429 = DIRECTION ( 'NONE',  ( 1.000000000000000000, 0.000000000000000000, 0.000000000000000000 ) ) ;
#49430 = DIRECTION ( 'NONE',  ( -1.000000000000000000, 0.000000000000000000, -0.000000000000000000 ) ) ;
#49431 = CARTESIAN_POINT ( 'NONE',  ( -16.81744102076748959, 51.61886293219124155, -231.9464690156495692 ) ) ;
#49432 = EDGE_CURVE ( 'NONE', #206936, #44660, #236744, .T. ) ;
#49433 = CARTESIAN_POINT ( 'NONE',  ( 20.04142135623730070, 64.25000000001202238, -114.7731074845243882 ) ) ;
#49434 = AXIS2_PLACEMENT_3D ( 'NONE', #93946, #76948, #156534 ) ;
#49435 = ORIENTED_EDGE ( 'NONE', *, *, #227212, .F. ) ;
#49436 = ORIENTED_EDGE ( 'NONE', *, *, #239023, .F. ) ;
#49437 = EDGE_CURVE ( 'NONE', #100605, #91770, #125611, .T. ) ;
#49438 = CARTESIAN_POINT ( 'NONE',  ( -21.55000000000000071, 29.24307565605548120, -237.2405905340223455 ) ) ;
#49439 = CIRCLE ( 'NONE', #116088, 0.1000000000000050987 ) ;
#49440 = VERTEX_POINT ( 'NONE', #124093 ) ;
#49441 = DIRECTION ( 'NONE',  ( 0.000000000000000000, 0.2617529984164856383, 0.9651348961777204138 ) ) ;
#49442 = ORIENTED_EDGE ( 'NONE', *, *, #515, .T. ) ;
#49443 = CARTESIAN_POINT ( 'NONE',  ( -20.94999999999999929, 87.48912529308822172, -139.5231074845243029 ) ) ;
#49444 =( BOUNDED_SURFACE ( )  B_SPLINE_SURFACE ( 3, 2, ( 
 ( #41013, #164791, #63100 ),
 ( #121823, #162240, #24012 ),
 ( #1834, #100908, #66966 ),
 ( #3120, #85207, #120547 ) ),
 .UNSPECIFIED., .F., .F., .F. ) 
 B_SPLINE_SURFACE_WITH_KNOTS ( ( 4, 4 ),
 ( 3, 3 ),
 ( -1.355252715606880543E-20, 0.0003124336117481267463 ),
 ( 0.000000000000000000, 1.000000000000000000 ),
 .UNSPECIFIED. ) 
 GEOMETRIC_REPRESENTATION_ITEM ( )  RATIONAL_B_SPLINE_SURFACE ( (
 ( 1.000000000000000000, 0.7040654476016099395, 1.000000000000000000),
 ( 1.000000000000000000, 0.7039193538781852721, 1.000000000000000000),
 ( 1.000000000000000000, 0.7089171279145316529, 1.000000000000000000),
 ( 1.000000000000000000, 0.7071067811865506814, 1.000000000000000000) ) ) 
 REPRESENTATION_ITEM ( '' )  SURFACE ( )  );
#49445 = ADVANCED_FACE ( 'NONE', ( #163216 ), #143632, .T. ) ;
#49446 = CIRCLE ( 'NONE', #57790, 0.8750000000000007772 ) ;
#49447 = EDGE_CURVE ( 'NONE', #194632, #75205, #182784, .T. ) ;
#49448 = FACE_OUTER_BOUND ( 'NONE', #38655, .T. ) ;
#49449 = DIRECTION ( 'NONE',  ( -0.000000000000000000, 1.000000000000000000, -0.000000000000000000 ) ) ;
#49450 = DIRECTION ( 'NONE',  ( -1.000000000000000000, -0.000000000000000000, -0.000000000000000000 ) ) ;
#49451 = CARTESIAN_POINT ( 'NONE',  ( 23.15000000000000213, 88.41227409416184457, -139.5231074845242745 ) ) ;
#49452 = ORIENTED_EDGE ( 'NONE', *, *, #98376, .T. ) ;
#49453 = DIRECTION ( 'NONE',  ( -0.000000000000000000, -6.982962677686266711E-15, 1.000000000000000000 ) ) ;
#49454 = AXIS2_PLACEMENT_3D ( 'NONE', #240348, #61697, #222024 ) ;
#49455 = CIRCLE ( 'NONE', #228532, 0.5999999999999894307 ) ;
#49457 = TOROIDAL_SURFACE ( 'NONE', #141045, 0.2000000000000000111, 0.1000000000000000056 ) ;
#49456 = CARTESIAN_POINT ( 'NONE',  ( -20.54999999999999716, 1.115600667400684642E-11, -134.0000000000000284 ) ) ;
#49458 = CARTESIAN_POINT ( 'NONE',  ( -18.50000000000000000, 77.16270174994961906, -61.42310748452431568 ) ) ;
#49459 = DIRECTION ( 'NONE',  ( -1.000000000000000000, 2.952720810173289112E-16, 2.061873921506763405E-30 ) ) ;
#49460 = ORIENTED_EDGE ( 'NONE', *, *, #150054, .F. ) ;
#49461 = CARTESIAN_POINT ( 'NONE',  ( -16.87683809663752399, 66.05000000001157900, -56.87310748452438958 ) ) ;
#49462 = EDGE_LOOP ( 'NONE', ( #86598, #87138, #52229, #114977 ) ) ;
#49465 = ORIENTED_EDGE ( 'NONE', *, *, #148630, .T. ) ;
#49464 = DIRECTION ( 'NONE',  ( 0.000000000000000000, 0.9889818879709272315, 0.1480365673253073999 ) ) ;
#49463 = DIRECTION ( 'NONE',  ( 0.000000000000000000, 0.000000000000000000, -1.000000000000000000 ) ) ;
#49466 = ADVANCED_FACE ( 'NONE', ( #221864 ), #157712, .F. ) ;
#49467 = DIRECTION ( 'NONE',  ( 0.000000000000000000, -0.1575844902526579161, -0.9875055080513779338 ) ) ;
#49468 = EDGE_CURVE ( 'NONE', #212214, #37875, #166066, .T. ) ;
#49469 = CARTESIAN_POINT ( 'NONE',  ( -21.09107601085565875, 34.02126425780384267, -243.7595103637841305 ) ) ;
#49470 = FACE_OUTER_BOUND ( 'NONE', #217586, .T. ) ;
#49471 = ORIENTED_EDGE ( 'NONE', *, *, #116741, .F. ) ;
#49472 = DIRECTION ( 'NONE',  ( 0.000000000000000000, 0.9908441862701596881, -0.1350103645451904977 ) ) ;
#49473 = LINE ( 'NONE', #191583, #236417 ) ;
#49475 = CARTESIAN_POINT ( 'NONE',  ( -18.39999999999999858, 11.47316190336247388, -9.325946066807970780 ) ) ;
#49474 = CARTESIAN_POINT ( 'NONE',  ( -22.50000000000000000, 11.64957080754479968, 0.09999999999999571731 ) ) ;
#49477 = ORIENTED_EDGE ( 'NONE', *, *, #211752, .T. ) ;
#49476 = DIRECTION ( 'NONE',  ( 1.000000000000000000, 0.000000000000000000, 0.000000000000000000 ) ) ;
#49478 = ADVANCED_FACE ( 'NONE', ( #240186 ), #170176, .T. ) ;
#49479 = ORIENTED_EDGE ( 'NONE', *, *, #102530, .F. ) ;
#49480 = AXIS2_PLACEMENT_3D ( 'NONE', #208069, #225019, #106355 ) ;
#49482 = EDGE_CURVE ( 'NONE', #156141, #10283, #140915, .T. ) ;
#49481 = FACE_OUTER_BOUND ( 'NONE', #115612, .T. ) ;
#49483 = DIRECTION ( 'NONE',  ( 0.000000000000000000, 0.1678971852675816834, 0.9858045116447902156 ) ) ;
#49484 = AXIS2_PLACEMENT_3D ( 'NONE', #130331, #112085, #115925 ) ;
#49485 = AXIS2_PLACEMENT_3D ( 'NONE', #103865, #200428, #83006 ) ;
#49486 = DIRECTION ( 'NONE',  ( 5.603264701231745086E-32, -1.897661533703520636E-16, 1.000000000000000000 ) ) ;
#49487 = ORIENTED_EDGE ( 'NONE', *, *, #65169, .T. ) ;
#49488 = CARTESIAN_POINT ( 'NONE',  ( -16.81453563122428108, 9.939100205448106351, -188.2882586606452833 ) ) ;
#49489 = DIRECTION ( 'NONE',  ( 0.000000000000000000, 0.000000000000000000, 1.000000000000000000 ) ) ;
#49490 = DIRECTION ( 'NONE',  ( 0.000000000000000000, 0.2128009952263678062, -0.9770955615653298398 ) ) ;
#49491 = AXIS2_PLACEMENT_3D ( 'NONE', #126202, #247438, #8838 ) ;
#49492 = ORIENTED_EDGE ( 'NONE', *, *, #216147, .T. ) ;
#49493 = EDGE_CURVE ( 'NONE', #253814, #65805, #141079, .T. ) ;
#49494 = DIRECTION ( 'NONE',  ( -1.000000000000000000, 0.000000000000000000, 0.000000000000000000 ) ) ;
#49495 = ADVANCED_FACE ( 'NONE', ( #121544 ), #201045, .T. ) ;
#49496 = ORIENTED_EDGE ( 'NONE', *, *, #114145, .T. ) ;
#49497 = EDGE_CURVE ( 'NONE', #166883, #59365, #203612, .T. ) ;
#49498 = AXIS2_PLACEMENT_3D ( 'NONE', #83447, #87314, #246409 ) ;
#49500 = AXIS2_PLACEMENT_3D ( 'NONE', #31384, #90018, #169618 ) ;
#49499 = DIRECTION ( 'NONE',  ( 0.000000000000000000, 0.000000000000000000, -1.000000000000000000 ) ) ;
#49501 = DIRECTION ( 'NONE',  ( 1.000000000000000000, 0.000000000000000000, 0.000000000000000000 ) ) ;
#49502 = AXIS2_PLACEMENT_3D ( 'NONE', #4721, #125963, #28194 ) ;
#49503 = ORIENTED_EDGE ( 'NONE', *, *, #66261, .T. ) ;
#49504 = ORIENTED_EDGE ( 'NONE', *, *, #246068, .T. ) ;
#49505 = VECTOR ( 'NONE', #598, 1000.000000000000114 ) ;
#49506 = DIRECTION ( 'NONE',  ( -1.000000000000000000, 0.000000000000000000, 0.000000000000000000 ) ) ;
#49507 = VERTEX_POINT ( 'NONE', #43263 ) ;
#49509 = EDGE_LOOP ( 'NONE', ( #31014, #147591, #70686, #120474 ) ) ;
#49508 = CARTESIAN_POINT ( 'NONE',  ( -21.22070241538126112, 6.469946272869613324, 0.09891903053502529297 ) ) ;
#49510 = EDGE_CURVE ( 'NONE', #129272, #49816, #178973, .T. ) ;
#49511 = ORIENTED_EDGE ( 'NONE', *, *, #224691, .T. ) ;
#49512 = VECTOR ( 'NONE', #193592, 1000.000000000000000 ) ;
#49513 = CIRCLE ( 'NONE', #141109, 0.09999999999998898659 ) ;
#49516 = ORIENTED_EDGE ( 'NONE', *, *, #10049, .T. ) ;
#49515 = ORIENTED_EDGE ( 'NONE', *, *, #244160, .T. ) ;
#49514 = DIRECTION ( 'NONE',  ( -1.000000000000000000, 0.000000000000000000, 0.000000000000000000 ) ) ;
#49517 = EDGE_CURVE ( 'NONE', #213934, #4326, #53429, .T. ) ;
#49518 = CARTESIAN_POINT ( 'NONE',  ( -18.46154800491018477, -9.480206274230813079, -107.1574508383815214 ) ) ;
#49519 = ORIENTED_EDGE ( 'NONE', *, *, #135607, .T. ) ;
#49520 = DIRECTION ( 'NONE',  ( 0.000000000000000000, 1.000000000000000000, -6.308085367188393199E-16 ) ) ;
#49521 = CARTESIAN_POINT ( 'NONE',  ( -20.54999999999999716, 84.73084112150753811, -146.1211822035086243 ) ) ;
#49522 = CIRCLE ( 'NONE', #195297, 0.09999999999998898659 ) ;
#49523 = VECTOR ( 'NONE', #204583, 1000.000000000000000 ) ;
#49524 = TOROIDAL_SURFACE ( 'NONE', #82788, 11.65000000000000036, 0.1000000000000000056 ) ;
#49525 = VERTEX_POINT ( 'NONE', #109636 ) ;
#49526 = VECTOR ( 'NONE', #129101, 1000.000000000000114 ) ;
#49527 = ORIENTED_EDGE ( 'NONE', *, *, #211051, .F. ) ;
#49528 = CARTESIAN_POINT ( 'NONE',  ( -21.14999999999999858, 0.09779029131994770863, -60.74218538952393232 ) ) ;
#49530 = EDGE_LOOP ( 'NONE', ( #176223, #235542, #37231, #79658 ) ) ;
#49529 = CARTESIAN_POINT ( 'NONE',  ( 18.49999999999962697, 63.80058314495188654, -209.3457071354949619 ) ) ;
#49531 = CARTESIAN_POINT ( 'NONE',  ( -23.49999999999994316, 77.25000000001119815, -43.92310748452479885 ) ) ;
#49533 = ORIENTED_EDGE ( 'NONE', *, *, #89401, .T. ) ;
#49532 = FACE_OUTER_BOUND ( 'NONE', #156248, .T. ) ;
#49534 = AXIS2_PLACEMENT_3D ( 'NONE', #39641, #93150, #154457 ) ;
#49535 = ORIENTED_EDGE ( 'NONE', *, *, #144792, .T. ) ;
#49536 = CARTESIAN_POINT ( 'NONE',  ( -18.59999999999999787, 9.350000000011156942, -121.6500000000000341 ) ) ;
#49537 = EDGE_LOOP ( 'NONE', ( #7780, #24315, #113264, #107744 ) ) ;
#49538 = CARTESIAN_POINT ( 'NONE',  ( -16.85722902420155833, 9.950000000011137047, -180.2655474737702548 ) ) ;
#49539 = CARTESIAN_POINT ( 'NONE',  ( 21.05000000000000071, 10.72371710471867701, -100.5000000000000284 ) ) ;
#49540 = AXIS2_PLACEMENT_3D ( 'NONE', #192535, #170449, #34770 ) ;
#49541 = AXIS2_PLACEMENT_3D ( 'NONE', #94572, #114136, #33370 ) ;
#49543 = ORIENTED_EDGE ( 'NONE', *, *, #191094, .T. ) ;
#49542 = ORIENTED_EDGE ( 'NONE', *, *, #214841, .F. ) ;
#49544 = ORIENTED_EDGE ( 'NONE', *, *, #257622, .F. ) ;
#49545 = CARTESIAN_POINT ( 'NONE',  ( 21.05000000000000426, 6.413826288824131083, -33.58574093703341390 ) ) ;
#49546 = ORIENTED_EDGE ( 'NONE', *, *, #156998, .F. ) ;
#49547 = VERTEX_POINT ( 'NONE', #126645 ) ;
#49548 = CARTESIAN_POINT ( 'NONE',  ( 20.85000000000000142, -1.749999999988843813, -112.1189500386223017 ) ) ;
#49550 = ORIENTED_EDGE ( 'NONE', *, *, #110613, .T. ) ;
#49549 = CARTESIAN_POINT ( 'NONE',  ( 23.14999999999999858, 72.10000000001170406, -69.52310748452433131 ) ) ;
#49551 = CARTESIAN_POINT ( 'NONE',  ( 20.94999999999999929, 82.09643798151613225, -215.4278993322501208 ) ) ;
#49553 = DIRECTION ( 'NONE',  ( 0.000000000000000000, -0.1350103645451876666, -0.9908441862701600211 ) ) ;
#49552 = DIRECTION ( 'NONE',  ( 0.000000000000000000, -0.2128009952263603954, 0.9770955615653315052 ) ) ;
#49554 = DIRECTION ( 'NONE',  ( 1.000000000000000000, -0.000000000000000000, -0.000000000000000000 ) ) ;
#49555 = FACE_OUTER_BOUND ( 'NONE', #6523, .T. ) ;
#49556 = ORIENTED_EDGE ( 'NONE', *, *, #100642, .T. ) ;
#49557 = AXIS2_PLACEMENT_3D ( 'NONE', #161275, #122138, #19179 ) ;
#49558 = ORIENTED_EDGE ( 'NONE', *, *, #26483, .T. ) ;
#49559 = FACE_OUTER_BOUND ( 'NONE', #156576, .T. ) ;
#49560 = FACE_OUTER_BOUND ( 'NONE', #179884, .T. ) ;
#49561 = EDGE_CURVE ( 'NONE', #76080, #204167, #11938, .T. ) ;
#49562 = CIRCLE ( 'NONE', #195332, 4.049999999999998046 ) ;
#49563 = ORIENTED_EDGE ( 'NONE', *, *, #28230, .F. ) ;
#49564 = AXIS2_PLACEMENT_3D ( 'NONE', #153211, #136145, #30692 ) ;
#49565 = DIRECTION ( 'NONE',  ( 0.000000000000000000, 0.000000000000000000, -1.000000000000000000 ) ) ;
#49566 = ORIENTED_EDGE ( 'NONE', *, *, #106138, .F. ) ;
#49567 = ORIENTED_EDGE ( 'NONE', *, *, #209613, .T. ) ;
#49568 = CYLINDRICAL_SURFACE ( 'NONE', #30140, 11.75000000000000000 ) ;
#49569 = EDGE_CURVE ( 'NONE', #100199, #71987, #86706, .T. ) ;
#49570 = CARTESIAN_POINT ( 'NONE',  ( -18.34804628011471195, 64.52683809664971193, -127.2731074845243882 ) ) ;
#49571 = VERTEX_POINT ( 'NONE', #127936 ) ;
#49572 = CARTESIAN_POINT ( 'NONE',  ( -20.94999999999999929, 0.2428138352382497867, -200.9114032742886309 ) ) ;
#49573 = DIRECTION ( 'NONE',  ( 0.5932847527679296906, -0.7865547670005542669, -0.1713032417725948720 ) ) ;
#49574 = ORIENTED_EDGE ( 'NONE', *, *, #162849, .F. ) ;
#49575 = CARTESIAN_POINT ( 'NONE',  ( 18.50000000000000355, -9.480686695267811714, -140.9411151687578467 ) ) ;
#49576 = CARTESIAN_POINT ( 'NONE',  ( -20.85000000000000142, 68.87972903831429505, -99.36354444268502561 ) ) ;
#49578 = CARTESIAN_POINT ( 'NONE',  ( -21.05000000000000426, 6.270085863700299633, -66.96513199698695473 ) ) ;
#49577 = CARTESIAN_POINT ( 'NONE',  ( 23.25000000000000000, 78.47509609352879068, -238.9045489380306435 ) ) ;
#49579 = CARTESIAN_POINT ( 'NONE',  ( -23.15000000000000213, 4.250000000011156409, -121.6500000000000341 ) ) ;
#49580 = ADVANCED_FACE ( 'NONE', ( #168395 ), #249171, .F. ) ;
#49583 = EDGE_CURVE ( 'NONE', #212825, #198468, #48381, .T. ) ;
#49582 = CIRCLE ( 'NONE', #120351, 0.09999999999999022171 ) ;
#49581 = CARTESIAN_POINT ( 'NONE',  ( -20.85000000000000142, -4.352039508298082282, -236.2331130063498676 ) ) ;
#49584 = FACE_OUTER_BOUND ( 'NONE', #247336, .T. ) ;
#49585 = DIRECTION ( 'NONE',  ( 0.000000000000000000, 0.000000000000000000, -1.000000000000000000 ) ) ;
#49586 = CIRCLE ( 'NONE', #57756, 0.09999999999999939493 ) ;
#49587 = VERTEX_POINT ( 'NONE', #107071 ) ;
#49588 = AXIS2_PLACEMENT_3D ( 'NONE', #194231, #96361, #254156 ) ;
#49590 = ORIENTED_EDGE ( 'NONE', *, *, #234927, .T. ) ;
#49589 = ORIENTED_EDGE ( 'NONE', *, *, #219270, .F. ) ;
#49591 = ORIENTED_EDGE ( 'NONE', *, *, #130400, .T. ) ;
#49592 = EDGE_CURVE ( 'NONE', #26849, #47325, #146197, .T. ) ;
#49593 = CARTESIAN_POINT ( 'NONE',  ( -21.05000000000000071, 76.00000000001149658, -47.82310748452432847 ) ) ;
#49594 = CARTESIAN_POINT ( 'NONE',  ( -2.995603634470891112E-16, 66.34920340998563404, -213.7018660128499334 ) ) ;
#49596 = CYLINDRICAL_SURFACE ( 'NONE', #140691, 0.09999999999999939493 ) ;
#49595 = DIRECTION ( 'NONE',  ( 0.000000000000000000, -0.1350103645451876666, -0.9908441862701600211 ) ) ;
#49597 = DIRECTION ( 'NONE',  ( -0.000000000000000000, 6.982962677686266711E-15, -1.000000000000000000 ) ) ;
#49598 = EDGE_LOOP ( 'NONE', ( #136639, #192983, #238778, #10896, #176252 ) ) ;
#49599 = CARTESIAN_POINT ( 'NONE',  ( -20.54999999999999716, 26.29846678923107817, -241.7324770631975639 ) ) ;
#49600 = ORIENTED_EDGE ( 'NONE', *, *, #247474, .F. ) ;
#49601 = DIRECTION ( 'NONE',  ( 0.000000000000000000, 0.000000000000000000, -1.000000000000000000 ) ) ;
#49602 = CARTESIAN_POINT ( 'NONE',  ( -22.50000000000000000, 0.1000000000111554016, -88.85042919245522341 ) ) ;
#49603 = VERTEX_POINT ( 'NONE', #5381 ) ;
#49604 = CARTESIAN_POINT ( 'NONE',  ( -18.59999999999999787, 64.21185867012613357, -224.4479740254296303 ) ) ;
#49605 = DIRECTION ( 'NONE',  ( 0.000000000000000000, -0.4088369013363280513, 0.9126074666063769270 ) ) ;
#49606 = ORIENTED_EDGE ( 'NONE', *, *, #231117, .T. ) ;
#49608 = ORIENTED_EDGE ( 'NONE', *, *, #86269, .T. ) ;
#49607 = EDGE_CURVE ( 'NONE', #183161, #44671, #220010, .T. ) ;
#49609 = LINE ( 'NONE', #126582, #145669 ) ;
#49610 = CARTESIAN_POINT ( 'NONE',  ( -23.15000000000000213, 11.65000000001115588, -93.48519422934610645 ) ) ;
#49611 = CYLINDRICAL_SURFACE ( 'NONE', #123867, 0.1000000000000028644 ) ;
#49612 = DIRECTION ( 'NONE',  ( -1.000000000000000000, 0.000000000000000000, -0.000000000000000000 ) ) ;
#49613 = FACE_OUTER_BOUND ( 'NONE', #212026, .T. ) ;
#49614 = CARTESIAN_POINT ( 'NONE',  ( -18.59999999999999787, 77.73625713160897988, -57.95445515550681392 ) ) ;
#49615 = EDGE_LOOP ( 'NONE', ( #214324, #20921, #58372, #18389 ) ) ;
#49616 = DIRECTION ( 'NONE',  ( 0.000000000000000000, -0.2128009952263604232, 0.9770955615653316162 ) ) ;
#49617 = CARTESIAN_POINT ( 'NONE',  ( -20.94999999999999929, 36.65892442174935439, -249.5511627012433848 ) ) ;
#49619 = CARTESIAN_POINT ( 'NONE',  ( -21.03571358705729111, 11.75000000001115197, -174.3251068220585580 ) ) ;
#49618 = CARTESIAN_POINT ( 'NONE',  ( -16.94445028196807002, 9.992063609708893068, -87.89266982158160602 ) ) ;
#49620 = DIRECTION ( 'NONE',  ( 0.000000000000000000, 0.000000000000000000, 1.000000000000000000 ) ) ;
#49621 = EDGE_CURVE ( 'NONE', #154576, #36482, #84913, .T. ) ;
#49622 = CARTESIAN_POINT ( 'NONE',  ( 23.14999999999999503, 11.75000000001116263, -55.25000000000004974 ) ) ;
#49623 = AXIS2_PLACEMENT_3D ( 'NONE', #211523, #12058, #17189 ) ;
#49624 = DIRECTION ( 'NONE',  ( 1.000000000000000000, 0.000000000000000000, 0.000000000000000000 ) ) ;
#49625 = CARTESIAN_POINT ( 'NONE',  ( 20.89192007715127986, 10.32898536001801304, -139.5826683222764757 ) ) ;
#49626 = AXIS2_PLACEMENT_3D ( 'NONE', #182146, #2195, #3484 ) ;
#49627 = VECTOR ( 'NONE', #12395, 1000.000000000000000 ) ;
#49629 = ORIENTED_EDGE ( 'NONE', *, *, #255596, .F. ) ;
#49628 = CARTESIAN_POINT ( 'NONE',  ( -20.94999999999999929, 76.00000000001222134, -148.2231074845243199 ) ) ;
#49630 = AXIS2_PLACEMENT_3D ( 'NONE', #203584, #41965, #164470 ) ;
#49631 = CARTESIAN_POINT ( 'NONE',  ( -18.36973785203556275, 54.09804631718828460, -229.1642379400122138 ) ) ;
#49632 = AXIS2_PLACEMENT_3D ( 'NONE', #64901, #242254, #165296 ) ;
#49633 = AXIS2_PLACEMENT_3D ( 'NONE', #252947, #170912, #153917 ) ;
#49635 = CIRCLE ( 'NONE', #145483, 0.09999999999999939493 ) ;
#49634 = FACE_OUTER_BOUND ( 'NONE', #182064, .T. ) ;
#49636 = FACE_OUTER_BOUND ( 'NONE', #62383, .T. ) ;
#49637 = ORIENTED_EDGE ( 'NONE', *, *, #248639, .T. ) ;
#49638 = TOROIDAL_SURFACE ( 'NONE', #91351, 0.2000000000000000111, 0.1000000000000000056 ) ;
#49639 = CARTESIAN_POINT ( 'NONE',  ( -21.05000000000000071, 1.835341550224411922, -11.55515129256298046 ) ) ;
#49640 = DIRECTION ( 'NONE',  ( 0.000000000000000000, -0.000000000000000000, 1.000000000000000000 ) ) ;
#49641 = DIRECTION ( 'NONE',  ( -0.000000000000000000, -6.982962677686266711E-15, 1.000000000000000000 ) ) ;
#49642 = EDGE_CURVE ( 'NONE', #133463, #247150, #88777, .T. ) ;
#49643 = ADVANCED_FACE ( 'NONE', ( #69255 ), #100455, .F. ) ;
#49644 = ORIENTED_EDGE ( 'NONE', *, *, #22727, .F. ) ;
#49645 = CARTESIAN_POINT ( 'NONE',  ( -23.30000000000000426, 3.332938107839114927, -347.0000000000001137 ) ) ;
#49647 = VERTEX_POINT ( 'NONE', #67953 ) ;
#49646 = DIRECTION ( 'NONE',  ( 0.000000000000000000, -0.000000000000000000, -1.000000000000000000 ) ) ;
#49648 = CARTESIAN_POINT ( 'NONE',  ( 21.09610168723073542, -1.324627966594374540, -194.7600028027378869 ) ) ;
#49650 = EDGE_CURVE ( 'NONE', #103069, #187669, #45223, .T. ) ;
#49649 = DIRECTION ( 'NONE',  ( 0.000000000000000000, 0.000000000000000000, -1.000000000000000000 ) ) ;
#49651 = EDGE_CURVE ( 'NONE', #54193, #67239, #210052, .T. ) ;
#49652 = ORIENTED_EDGE ( 'NONE', *, *, #60205, .T. ) ;
#49653 = DIRECTION ( 'NONE',  ( 0.000000000000000000, 0.000000000000000000, -1.000000000000000000 ) ) ;
#49654 = APPLICATION_PROTOCOL_DEFINITION ( 'draft international standard', 'automotive_design', 1998, #250762 ) ;
#49655 = LINE ( 'NONE', #169654, #129549 ) ;
#49656 = DIRECTION ( 'NONE',  ( 0.000000000000000000, -0.9915357197604982575, 0.1298341882519033486 ) ) ;
#49657 = CARTESIAN_POINT ( 'NONE',  ( 22.50000000000000000, 64.35042919246686210, -69.62310748452439668 ) ) ;
#49658 = EDGE_CURVE ( 'NONE', #41070, #60897, #95123, .T. ) ;
#49659 = ORIENTED_EDGE ( 'NONE', *, *, #252492, .T. ) ;
#49660 = CARTESIAN_POINT ( 'NONE',  ( 23.14999999999999858, 76.00000000001244871, -170.0231074845243597 ) ) ;
#49661 = CARTESIAN_POINT ( 'NONE',  ( 18.59999999999999076, 6.450000000011156587, -77.01702717044007329 ) ) ;
#49662 = CIRCLE ( 'NONE', #62142, 11.64999999999999325 ) ;
#49663 = EDGE_CURVE ( 'NONE', #218579, #40869, #120096, .T. ) ;
#49665 = EDGE_CURVE ( 'NONE', #202789, #9029, #61799, .T. ) ;
#49664 = EDGE_CURVE ( 'NONE', #116440, #22716, #111887, .T. ) ;
#49666 = DIRECTION ( 'NONE',  ( 1.000000000000000000, 0.000000000000000000, 0.000000000000000000 ) ) ;
#49667 = VERTEX_POINT ( 'NONE', #37843 ) ;
#49668 = EDGE_CURVE ( 'NONE', #123863, #167063, #136911, .T. ) ;
#49669 = ORIENTED_EDGE ( 'NONE', *, *, #220698, .F. ) ;
#49670 = DIRECTION ( 'NONE',  ( -0.000000000000000000, -0.000000000000000000, 1.000000000000000000 ) ) ;
#49671 = DIRECTION ( 'NONE',  ( 0.000000000000000000, 0.9651348961777157509, -0.2617529984165031243 ) ) ;
#49672 = DIRECTION ( 'NONE',  ( 1.000000000000000000, 0.000000000000000000, 0.000000000000000000 ) ) ;
#49673 = EDGE_CURVE ( 'NONE', #157880, #71756, #224288, .T. ) ;
#49674 = DIRECTION ( 'NONE',  ( -1.000000000000000000, -1.541880601228652843E-16, -2.878400969107353907E-16 ) ) ;
#49676 = DIRECTION ( 'NONE',  ( -0.000000000000000000, 1.000000000000000000, 6.982962677686266711E-15 ) ) ;
#49675 = CARTESIAN_POINT ( 'NONE',  ( -18.59999999999999787, 11.75000000000000000, 5.900000000000001243 ) ) ;
#49678 = DIRECTION ( 'NONE',  ( 0.000000000000000000, 0.1332476588733589318, 0.9910827722268049644 ) ) ;
#49677 = CIRCLE ( 'NONE', #207917, 11.70000000000000817 ) ;
#49680 = EDGE_CURVE ( 'NONE', #161202, #94122, #257544, .T. ) ;
#49679 = DIRECTION ( 'NONE',  ( 1.040834085586108490E-13, -0.9742838591452925856, -0.2253241261138180518 ) ) ;
#49682 = ADVANCED_FACE ( 'NONE', ( #11858 ), #233783, .T. ) ;
#49681 = CARTESIAN_POINT ( 'NONE',  ( -22.59066674512272144, 64.25000000001213607, -136.5536116081548244 ) ) ;
#49684 = EDGE_LOOP ( 'NONE', ( #232364, #140022, #243425, #136516 ) ) ;
#49683 = CARTESIAN_POINT ( 'NONE',  ( 21.05000000000000071, -1.360870587180885716, -108.5729979270909951 ) ) ;
#49685 = DIRECTION ( 'NONE',  ( 0.000000000000000000, 1.000000000000000000, 0.000000000000000000 ) ) ;
#49686 = CIRCLE ( 'NONE', #195456, 12.87499999999999822 ) ;
#49687 = CARTESIAN_POINT ( 'NONE',  ( -20.85000000000000142, -1.164121893230052995, -108.4148480855716485 ) ) ;
#49689 = LINE ( 'NONE', #69270, #157622 ) ;
#49688 = CARTESIAN_POINT ( 'NONE',  ( 23.24999999999999289, 6.650000000011155876, -146.1500000000000341 ) ) ;
#49690 = EDGE_CURVE ( 'NONE', #47548, #186482, #7644, .T. ) ;
#49691 = EDGE_LOOP ( 'NONE', ( #53695, #153234, #242903, #132535 ) ) ;
#49692 = CARTESIAN_POINT ( 'NONE',  ( -23.25000000000000000, -1.736705739456431807, -112.0174225876237699 ) ) ;
#49693 = LINE ( 'NONE', #129237, #249775 ) ;
#49694 = DIRECTION ( 'NONE',  ( -1.000000000000000000, 0.000000000000000000, 0.000000000000000000 ) ) ;
#49695 = CARTESIAN_POINT ( 'NONE',  ( 22.49231231312462853, 11.64998490368843953, -133.9389471123986368 ) ) ;
#49696 = DIRECTION ( 'NONE',  ( 0.000000000000000000, 0.000000000000000000, 1.000000000000000000 ) ) ;
#49697 = VERTEX_POINT ( 'NONE', #54795 ) ;
#49698 = ADVANCED_FACE ( 'NONE', ( #134327 ), #170961, .F. ) ;
#49699 = CIRCLE ( 'NONE', #195463, 0.1000000000000134115 ) ;
#49700 = AXIS2_PLACEMENT_3D ( 'NONE', #239563, #60907, #58323 ) ;
#49701 = ORIENTED_EDGE ( 'NONE', *, *, #15857, .T. ) ;
#49702 = ADVANCED_FACE ( 'NONE', ( #191786 ), #16987, .T. ) ;
#49703 = DIRECTION ( 'NONE',  ( 0.000000000000000000, 0.000000000000000000, -1.000000000000000000 ) ) ;
#49704 = EDGE_LOOP ( 'NONE', ( #256476, #193398, #90804, #136158 ) ) ;
#49705 = DIRECTION ( 'NONE',  ( 0.000000000000000000, 0.000000000000000000, 1.000000000000000000 ) ) ;
#49706 = ORIENTED_EDGE ( 'NONE', *, *, #73019, .T. ) ;
#49707 = DIRECTION ( 'NONE',  ( -0.7071067811865546782, -0.6824534298470523730, 0.1850873201761376874 ) ) ;
#49709 = CIRCLE ( 'NONE', #91411, 0.09999999999999939493 ) ;
#49708 = DIRECTION ( 'NONE',  ( 1.000000000000000000, 0.000000000000000000, 0.000000000000000000 ) ) ;
#49710 = AXIS2_PLACEMENT_3D ( 'NONE', #118542, #134212, #213769 ) ;
#49711 = DIRECTION ( 'NONE',  ( -6.938893903907222067E-15, 1.000000000000000000, 0.000000000000000000 ) ) ;
#49712 = ORIENTED_EDGE ( 'NONE', *, *, #125508, .T. ) ;
#49713 = EDGE_CURVE ( 'NONE', #45676, #229726, #162452, .T. ) ;
#49714 = AXIS2_PLACEMENT_3D ( 'NONE', #246175, #147051, #240082 ) ;
#49715 = DIRECTION ( 'NONE',  ( -0.000000000000000000, 0.000000000000000000, 1.000000000000000000 ) ) ;
#49716 = CARTESIAN_POINT ( 'NONE',  ( -18.54148534481894472, 68.09306500613196533, -224.1549646960459086 ) ) ;
#49717 = LINE ( 'NONE', #148833, #45777 ) ;
#49718 = DIRECTION ( 'NONE',  ( 1.000000000000000000, 0.000000000000000000, 0.000000000000000000 ) ) ;
#49719 = CARTESIAN_POINT ( 'NONE',  ( -23.15000000000000213, 11.75000000001115552, -155.3500000000000227 ) ) ;
#49720 = CYLINDRICAL_SURFACE ( 'NONE', #44843, 0.1000000000000028644 ) ;
#49721 = ORIENTED_EDGE ( 'NONE', *, *, #125859, .T. ) ;
#49723 = DIRECTION ( 'NONE',  ( -1.000000000000000000, 0.000000000000000000, 0.000000000000000000 ) ) ;
#49722 = FACE_OUTER_BOUND ( 'NONE', #29964, .T. ) ;
#49724 = AXIS2_PLACEMENT_3D ( 'NONE', #185682, #25344, #67013 ) ;
#49725 = ORIENTED_EDGE ( 'NONE', *, *, #257404, .T. ) ;
#49727 = ORIENTED_EDGE ( 'NONE', *, *, #24359, .F. ) ;
#49726 = DIRECTION ( 'NONE',  ( 0.000000000000000000, 0.000000000000000000, 1.000000000000000000 ) ) ;
#49728 = EDGE_LOOP ( 'NONE', ( #212446, #219053, #32588, #60217 ) ) ;
#49729 = CARTESIAN_POINT ( 'NONE',  ( -21.14999999999999858, 11.65000000001115232, -67.00000000000004263 ) ) ;
#49730 = LINE ( 'NONE', #171017, #105155 ) ;
#49731 = CARTESIAN_POINT ( 'NONE',  ( -20.54999999999999716, 87.75000000001199396, -115.3731074845242119 ) ) ;
#49732 = DIRECTION ( 'NONE',  ( 0.000000000000000000, -7.272083257015735086E-15, 1.000000000000000000 ) ) ;
#49733 = ORIENTED_EDGE ( 'NONE', *, *, #67164, .T. ) ;
#49734 = DIRECTION ( 'NONE',  ( 0.000000000000000000, 7.056502275159894776E-15, -1.000000000000000000 ) ) ;
#49735 = FACE_OUTER_BOUND ( 'NONE', #248586, .T. ) ;
#49736 = EDGE_LOOP ( 'NONE', ( #199599, #775, #114087, #73608 ) ) ;
#49737 = VECTOR ( 'NONE', #132851, 1000.000000000000000 ) ;
#49738 = CARTESIAN_POINT ( 'NONE',  ( -16.91776028072577631, 9.963400393640901243, -154.8750240147021486 ) ) ;
#49739 = ADVANCED_FACE ( 'NONE', ( #156518 ), #92642, .T. ) ;
#49740 = AXIS2_PLACEMENT_3D ( 'NONE', #116001, #30361, #68188 ) ;
#49741 = CYLINDRICAL_SURFACE ( 'NONE', #214133, 0.1000000000000028644 ) ;
#49742 = EDGE_LOOP ( 'NONE', ( #258013, #24460, #142901, #75698 ) ) ;
#49743 = EDGE_CURVE ( 'NONE', #226489, #254689, #133072, .T. ) ;
#49744 = DIRECTION ( 'NONE',  ( 1.000000000000000000, -1.836970198721029934E-16, -1.282749433769087582E-30 ) ) ;
#49745 = CIRCLE ( 'NONE', #24832, 11.90000000000000213 ) ;
#49746 = ORIENTED_EDGE ( 'NONE', *, *, #59327, .F. ) ;
#49747 = CARTESIAN_POINT ( 'NONE',  ( 21.05000000000000071, 65.65271564877468791, -222.5736063831752176 ) ) ;
#49748 = ORIENTED_EDGE ( 'NONE', *, *, #190658, .F. ) ;
#49749 = DIRECTION ( 'NONE',  ( 0.5932847527679310229, 0.8049926720990042694, 6.257843056355992909E-15 ) ) ;
#49750 = EDGE_CURVE ( 'NONE', #213316, #257624, #74314, .T. ) ;
#49751 = EDGE_CURVE ( 'NONE', #208072, #116233, #155232, .T. ) ;
#49752 = DIRECTION ( 'NONE',  ( -1.000000000000000000, 0.000000000000000000, -0.000000000000000000 ) ) ;
#49753 = LINE ( 'NONE', #112309, #114125 ) ;
#49754 = CARTESIAN_POINT ( 'NONE',  ( 21.00000000000000000, 30.46448808713892831, -235.1722212069449256 ) ) ;
#49755 = EDGE_CURVE ( 'NONE', #187906, #71369, #174271, .T. ) ;
#49756 = CIRCLE ( 'NONE', #3964, 0.09999999999999939493 ) ;
#49757 = DIRECTION ( 'NONE',  ( -1.000000000000000000, 0.000000000000000000, 0.000000000000000000 ) ) ;
#49758 = DIRECTION ( 'NONE',  ( 0.000000000000000000, -6.982962677686266711E-15, 1.000000000000000000 ) ) ;
#49759 = ORIENTED_EDGE ( 'NONE', *, *, #204528, .F. ) ;
#49761 = CARTESIAN_POINT ( 'NONE',  ( -23.15000000000000213, 2.000000000011154189, -120.7753780772379315 ) ) ;
#49760 = AXIS2_PLACEMENT_3D ( 'NONE', #93171, #73647, #111458 ) ;
#49762 = VERTEX_POINT ( 'NONE', #122500 ) ;
#49765 =( BOUNDED_CURVE ( )  B_SPLINE_CURVE ( 3, ( #251706, #95204, #211301, #254254 ),
 .UNSPECIFIED., .F., .T. ) 
 B_SPLINE_CURVE_WITH_KNOTS ( ( 4, 4 ),
 ( 3.141592653589793116, 4.712388980384689674 ),
 .UNSPECIFIED. ) 
 CURVE ( )  GEOMETRIC_REPRESENTATION_ITEM ( )  RATIONAL_B_SPLINE_CURVE ( ( 1.000000000000000000, 0.8047378541243649375, 0.8047378541243649375, 1.000000000000000000 ) ) 
 REPRESENTATION_ITEM ( '' )  );
#49764 = DIRECTION ( 'NONE',  ( 0.000000000000000000, -1.000000000000000000, -6.982962677686266711E-15 ) ) ;
#49763 = CARTESIAN_POINT ( 'NONE',  ( 18.59999999999999076, 64.25000000001220712, -148.2731074845243882 ) ) ;
#49766 = ADVANCED_FACE ( 'NONE', ( #181199 ), #116167, .F. ) ;
#49767 = ORIENTED_EDGE ( 'NONE', *, *, #245208, .F. ) ;
#49768 = CARTESIAN_POINT ( 'NONE',  ( 21.14999999999999858, 11.65000000001116298, -146.2500000000000284 ) ) ;
#49769 = CARTESIAN_POINT ( 'NONE',  ( -23.39999999999994529, 76.00000000001119815, -36.02310748452479316 ) ) ;
#49770 = FACE_OUTER_BOUND ( 'NONE', #118096, .T. ) ;
#49771 = ORIENTED_EDGE ( 'NONE', *, *, #214107, .T. ) ;
#49773 = ORIENTED_EDGE ( 'NONE', *, *, #49074, .T. ) ;
#49772 = DIRECTION ( 'NONE',  ( -1.000000000000000000, 0.000000000000000000, 4.336808689942017736E-16 ) ) ;
#49774 = CARTESIAN_POINT ( 'NONE',  ( -21.05000000000000071, 70.15000000001211333, -126.3906102602463619 ) ) ;
#49776 = CARTESIAN_POINT ( 'NONE',  ( 18.50000000000000000, 15.30611090022306620, -222.9706416475797255 ) ) ;
#49775 = DIRECTION ( 'NONE',  ( 1.000000000000000000, -0.000000000000000000, -0.000000000000000000 ) ) ;
#49778 = ORIENTED_EDGE ( 'NONE', *, *, #53486, .T. ) ;
#49777 = DIRECTION ( 'NONE',  ( 1.000000000000000000, -0.000000000000000000, 0.000000000000000000 ) ) ;
#49779 = AXIS2_PLACEMENT_3D ( 'NONE', #134069, #109366, #151088 ) ;
#49780 = ORIENTED_EDGE ( 'NONE', *, *, #55809, .F. ) ;
#49781 = ADVANCED_FACE ( 'NONE', ( #199477 ), #101596, .T. ) ;
#49782 = DIRECTION ( 'NONE',  ( 1.000000000000000000, 0.000000000000000000, -0.000000000000000000 ) ) ;
#49783 = FACE_OUTER_BOUND ( 'NONE', #72412, .T. ) ;
#49784 = ORIENTED_EDGE ( 'NONE', *, *, #146215, .T. ) ;
#49785 = CARTESIAN_POINT ( 'NONE',  ( -23.15000000000000213, 11.65000000000000036, -21.35000000000000142 ) ) ;
#49786 = ORIENTED_EDGE ( 'NONE', *, *, #163022, .T. ) ;
#49787 = CARTESIAN_POINT ( 'NONE',  ( 22.50000000000000000, 75.90000000001276703, -215.1726782920691505 ) ) ;
#49788 = CARTESIAN_POINT ( 'NONE',  ( 23.14999999999999503, 11.65000000000000746, -21.35000000000000142 ) ) ;
#49789 = VERTEX_POINT ( 'NONE', #58638 ) ;
#49790 = EDGE_CURVE ( 'NONE', #70706, #142483, #3714, .T. ) ;
#49791 = DIRECTION ( 'NONE',  ( 0.000000000000000000, 0.000000000000000000, -1.000000000000000000 ) ) ;
#49792 = ADVANCED_FACE ( 'NONE', ( #242420 ), #27413, .T. ) ;
#49793 = CIRCLE ( 'NONE', #249710, 4.000000000000006217 ) ;
#49794 = AXIS2_PLACEMENT_3D ( 'NONE', #92538, #96380, #93830 ) ;
#49795 = EDGE_LOOP ( 'NONE', ( #62641, #62940, #26299, #240070 ) ) ;
#49796 = CIRCLE ( 'NONE', #12408, 0.09999999999998898659 ) ;
#49797 = AXIS2_PLACEMENT_3D ( 'NONE', #15640, #217627, #75605 ) ;
#49798 = CARTESIAN_POINT ( 'NONE',  ( -20.64999999999999858, 1.115600667400684642E-11, -67.00000000000000000 ) ) ;
#49799 = EDGE_CURVE ( 'NONE', #3259, #176509, #199568, .T. ) ;
#49800 = ORIENTED_EDGE ( 'NONE', *, *, #149989, .T. ) ;
#49801 = AXIS2_PLACEMENT_3D ( 'NONE', #67925, #88750, #206157 ) ;
#49802 = VERTEX_POINT ( 'NONE', #99043 ) ;
#49803 = CARTESIAN_POINT ( 'NONE',  ( -18.58744394320938653, -9.566385154537710989, -73.82284805387557469 ) ) ;
#49804 = ORIENTED_EDGE ( 'NONE', *, *, #235973, .T. ) ;
#49805 = FACE_OUTER_BOUND ( 'NONE', #42995, .T. ) ;
#49806 = ORIENTED_EDGE ( 'NONE', *, *, #108880, .F. ) ;
#49808 = ORIENTED_EDGE ( 'NONE', *, *, #20571, .F. ) ;
#49807 = DIRECTION ( 'NONE',  ( -1.000000000000000000, 1.836970198721029934E-16, 1.282749433769087757E-30 ) ) ;
#49809 = EDGE_CURVE ( 'NONE', #254925, #75581, #16214, .T. ) ;
#49810 = EDGE_CURVE ( 'NONE', #86511, #5771, #204037, .T. ) ;
#49811 = ORIENTED_EDGE ( 'NONE', *, *, #15256, .T. ) ;
#49812 = CARTESIAN_POINT ( 'NONE',  ( 18.59999999999999076, 74.16465844978715438, -57.96795619196135618 ) ) ;
#49813 = CIRCLE ( 'NONE', #195592, 0.09999999999999761857 ) ;
#49814 = ORIENTED_EDGE ( 'NONE', *, *, #146413, .F. ) ;
#49817 = EDGE_LOOP ( 'NONE', ( #41478, #96927, #106977, #140142 ) ) ;
#49816 = VERTEX_POINT ( 'NONE', #140767 ) ;
#49815 = CARTESIAN_POINT ( 'NONE',  ( 23.14999999999999858, 9.480858690661944976, -221.0361137499737936 ) ) ;
#49818 = DIRECTION ( 'NONE',  ( 0.000000000000000000, 6.982962677686266711E-15, -1.000000000000000000 ) ) ;
#49819 = ADVANCED_FACE ( 'NONE', ( #117357 ), #236953, .T. ) ;
#49820 = DIRECTION ( 'NONE',  ( -0.000000000000000000, 0.07893460099012301889, -0.9968797965484754720 ) ) ;
#49821 = ORIENTED_EDGE ( 'NONE', *, *, #44551, .T. ) ;
#49822 = AXIS2_PLACEMENT_3D ( 'NONE', #152597, #137787, #257690 ) ;
#49823 = VERTEX_POINT ( 'NONE', #78215 ) ;
#49824 = CARTESIAN_POINT ( 'NONE',  ( -21.04999999999999716, 69.70076908992041353, -203.6215449845247178 ) ) ;
#49825 = EDGE_CURVE ( 'NONE', #110943, #108582, #179911, .T. ) ;
#49826 = DIRECTION ( 'NONE',  ( 0.000000000000000000, 0.2617529984165031243, 0.9651348961777157509 ) ) ;
#49828 = ORIENTED_EDGE ( 'NONE', *, *, #40418, .F. ) ;
#49827 = DIRECTION ( 'NONE',  ( 0.000000000000000000, 0.000000000000000000, -1.000000000000000000 ) ) ;
#49829 = CARTESIAN_POINT ( 'NONE',  ( -23.15000000000000213, 1.999999999999998224, -20.27537807723789953 ) ) ;
#49830 = ORIENTED_EDGE ( 'NONE', *, *, #17995, .T. ) ;
#49831 = LINE ( 'NONE', #189354, #195227 ) ;
#49832 = CARTESIAN_POINT ( 'NONE',  ( 18.56308993302904042, 65.61930884468790737, -111.7838848455857601 ) ) ;
#49833 = ORIENTED_EDGE ( 'NONE', *, *, #60513, .T. ) ;
#49834 = DIRECTION ( 'NONE',  ( 0.000000000000000000, 0.9126074666064696306, 0.4088369013361213278 ) ) ;
#49835 = ORIENTED_EDGE ( 'NONE', *, *, #227825, .T. ) ;
#49837 = ORIENTED_EDGE ( 'NONE', *, *, #52531, .T. ) ;
#49836 = CARTESIAN_POINT ( 'NONE',  ( -21.05000000000000071, 4.288595810029049993, -211.9930862808554934 ) ) ;
#49838 = AXIS2_PLACEMENT_3D ( 'NONE', #169397, #130206, #132809 ) ;
#49839 = LINE ( 'NONE', #140252, #148454 ) ;
#49841 = VERTEX_POINT ( 'NONE', #1232 ) ;
#49840 = ORIENTED_EDGE ( 'NONE', *, *, #153041, .F. ) ;
#49842 = ORIENTED_EDGE ( 'NONE', *, *, #129144, .F. ) ;
#49843 = CARTESIAN_POINT ( 'NONE',  ( -20.64999999999999858, 11.50825441376376901, -220.2417535673963300 ) ) ;
#49844 = ORIENTED_EDGE ( 'NONE', *, *, #135624, .F. ) ;
#49845 = EDGE_LOOP ( 'NONE', ( #22026, #53683, #250638, #171721 ) ) ;
#49846 = DIRECTION ( 'NONE',  ( 1.000000000000000000, 0.000000000000000000, 0.000000000000000000 ) ) ;
#49847 = AXIS2_PLACEMENT_3D ( 'NONE', #58866, #178882, #257042 ) ;
#49848 = ORIENTED_EDGE ( 'NONE', *, *, #70443, .T. ) ;
#49849 = CARTESIAN_POINT ( 'NONE',  ( -22.47071067811865319, 7.720074744509219933, -100.4009075452974287 ) ) ;
#49850 = CARTESIAN_POINT ( 'NONE',  ( -23.25000000000000000, 76.00000000001213607, -136.5231074845243313 ) ) ;
#49851 = EDGE_LOOP ( 'NONE', ( #151656, #58255, #198581, #52046 ) ) ;
#49852 = ORIENTED_EDGE ( 'NONE', *, *, #231528, .F. ) ;
#49853 = DIRECTION ( 'NONE',  ( 0.000000000000000000, -1.734723475983309083E-15, 1.000000000000000000 ) ) ;
#49855 = ORIENTED_EDGE ( 'NONE', *, *, #156202, .F. ) ;
#49854 = AXIS2_PLACEMENT_3D ( 'NONE', #223182, #86223, #241482 ) ;
#49856 = EDGE_CURVE ( 'NONE', #192844, #143815, #107763, .T. ) ;
#49857 = TOROIDAL_SURFACE ( 'NONE', #195642, 0.2000000000000000111, 0.1000000000000000056 ) ;
#49858 = CARTESIAN_POINT ( 'NONE',  ( -18.59999999999999787, 85.32100840337338354, -129.2871692354463562 ) ) ;
#49859 = VERTEX_POINT ( 'NONE', #46781 ) ;
#49860 = CARTESIAN_POINT ( 'NONE',  ( -18.59999999999999787, 1.162701749949165642, -41.60000000000000142 ) ) ;
#49861 = EDGE_CURVE ( 'NONE', #247898, #120029, #91208, .T. ) ;
#49863 = ORIENTED_EDGE ( 'NONE', *, *, #235477, .F. ) ;
#49862 = CYLINDRICAL_SURFACE ( 'NONE', #187715, 0.1000000000000124678 ) ;
#49864 = CARTESIAN_POINT ( 'NONE',  ( 23.14999999999999858, 36.65892442174935439, -249.5511627012433848 ) ) ;
#49865 = DIRECTION ( 'NONE',  ( -1.000000000000000000, 2.952720810173289112E-16, 2.061873921506763405E-30 ) ) ;
#49866 = AXIS2_PLACEMENT_3D ( 'NONE', #164139, #141984, #162868 ) ;
#49868 = AXIS2_PLACEMENT_3D ( 'NONE', #91420, #129258, #187953 ) ;
#49867 = DIRECTION ( 'NONE',  ( 0.000000000000000000, 0.4088369013363281068, -0.9126074666063770380 ) ) ;
#49869 = CARTESIAN_POINT ( 'NONE',  ( -21.07946286933445279, 6.329037319018852692, -133.9233161567436525 ) ) ;
#49870 = DIRECTION ( 'NONE',  ( 0.000000000000000000, -0.01283462868041947667, -0.9999176327611367654 ) ) ;
#49871 = EDGE_CURVE ( 'NONE', #16586, #162715, #128624, .T. ) ;
#49872 = DIRECTION ( 'NONE',  ( 0.000000000000000000, 0.000000000000000000, -1.000000000000000000 ) ) ;
#49874 = EDGE_CURVE ( 'NONE', #65743, #258063, #195288, .T. ) ;
#49873 = CARTESIAN_POINT ( 'NONE',  ( 20.94999999999999929, -1.164121893230052995, -175.4148480855716059 ) ) ;
#49875 = FACE_OUTER_BOUND ( 'NONE', #191954, .T. ) ;
#49876 = FACE_OUTER_BOUND ( 'NONE', #120161, .T. ) ;
#49877 = ORIENTED_EDGE ( 'NONE', *, *, #45763, .T. ) ;
#49878 = AXIS2_PLACEMENT_3D ( 'NONE', #90652, #231478, #8570 ) ;
#49879 = AXIS2_PLACEMENT_3D ( 'NONE', #244677, #183446, #41387 ) ;
#49880 = CIRCLE ( 'NONE', #120641, 0.4000000000000086264 ) ;
#49881 = AXIS2_PLACEMENT_3D ( 'NONE', #8703, #64814, #85627 ) ;
#49882 = ORIENTED_EDGE ( 'NONE', *, *, #193512, .T. ) ;
#49884 = EDGE_LOOP ( 'NONE', ( #251231, #139758, #7825, #232240, #49828 ) ) ;
#49883 = CARTESIAN_POINT ( 'NONE',  ( -23.15000000000000213, 4.349999999999999645, -21.35000000000000142 ) ) ;
#49885 = ORIENTED_EDGE ( 'NONE', *, *, #13706, .T. ) ;
#49886 = EDGE_CURVE ( 'NONE', #115014, #186169, #226707, .T. ) ;
#49887 = AXIS2_PLACEMENT_3D ( 'NONE', #54380, #10130, #150922 ) ;
#49888 = DIRECTION ( 'NONE',  ( 0.000000000000000000, 0.000000000000000000, 1.000000000000000000 ) ) ;
#49890 = CARTESIAN_POINT ( 'NONE',  ( 21.14999999999999858, 1.363275264940682741, -230.6442496871288483 ) ) ;
#49889 = DIRECTION ( 'NONE',  ( -0.9880948137434723000, -0.1538461538461483591, -1.074301950413233512E-15 ) ) ;
#49891 = EDGE_LOOP ( 'NONE', ( #15915, #30487, #171675, #21980 ) ) ;
#49892 = ORIENTED_EDGE ( 'NONE', *, *, #194937, .F. ) ;
#49893 = SURFACE_SIDE_STYLE ('',( #245541 ) ) ;
#49894 = CARTESIAN_POINT ( 'NONE',  ( 18.50000000000000000, -9.399999999988823518, -40.79725975966326246 ) ) ;
#49895 = FACE_OUTER_BOUND ( 'NONE', #43095, .T. ) ;
#49896 = ORIENTED_EDGE ( 'NONE', *, *, #211636, .T. ) ;
#49897 = ORIENTED_EDGE ( 'NONE', *, *, #240088, .T. ) ;
#49898 = CARTESIAN_POINT ( 'NONE',  ( -16.83794237512073977, 9.926359221118634224, -180.3035421586989457 ) ) ;
#49899 = DIRECTION ( 'NONE',  ( -0.000000000000000000, -6.982962677686266711E-15, 1.000000000000000000 ) ) ;
#49900 = DIRECTION ( 'NONE',  ( 0.000000000000000000, 0.000000000000000000, -1.000000000000000000 ) ) ;
#49901 = ADVANCED_FACE ( 'NONE', ( #109322 ), #126333, .F. ) ;
#49902 = CARTESIAN_POINT ( 'NONE',  ( 20.94999999999999574, 62.00000000001233502, -164.5960149541419071 ) ) ;
#49904 = ORIENTED_EDGE ( 'NONE', *, *, #232856, .T. ) ;
#49903 = DIRECTION ( 'NONE',  ( 0.000000000000000000, 0.9126074666063660468, 0.4088369013363524762 ) ) ;
#49905 = ADVANCED_FACE ( 'NONE', ( #24700 ), #124528, .T. ) ;
#49906 = FACE_OUTER_BOUND ( 'NONE', #36452, .T. ) ;
#49907 = SPHERICAL_SURFACE ( 'NONE', #189828, 0.1000000000000000056 ) ;
#49908 = CARTESIAN_POINT ( 'NONE',  ( 23.40000000000005542, 64.35000000001120668, -3.123107484524795474 ) ) ;
#49909 = CARTESIAN_POINT ( 'NONE',  ( 18.58703555225010007, 85.40633674080056892, -95.89816284327731921 ) ) ;
#49910 = ORIENTED_EDGE ( 'NONE', *, *, #91163, .T. ) ;
#49911 = CARTESIAN_POINT ( 'NONE',  ( -20.64999999999999858, 45.00644278977874535, -237.9768835835062077 ) ) ;
#49912 = AXIS2_PLACEMENT_3D ( 'NONE', #88229, #173951, #167830 ) ;
#49913 = CARTESIAN_POINT ( 'NONE',  ( -23.15000000000000213, 76.00000000001193712, -107.0231074845243029 ) ) ;
#49915 = CARTESIAN_POINT ( 'NONE',  ( -17.71734398241073905, 65.15764277154742956, -113.2979692315187918 ) ) ;
#49914 = CARTESIAN_POINT ( 'NONE',  ( -23.15000000000000213, 11.65000000000000036, 11.75000000000000000 ) ) ;
#49916 = SPHERICAL_SURFACE ( 'NONE', #203857, 0.1000000000000000056 ) ;
#49917 = CIRCLE ( 'NONE', #216514, 0.1000000000000028644 ) ;
#49918 = CARTESIAN_POINT ( 'NONE',  ( -16.77431908686106254, 9.945805754529134290, -54.33583921765023916 ) ) ;
#49919 = EDGE_CURVE ( 'NONE', #21362, #187411, #68956, .T. ) ;
#49920 = DIRECTION ( 'NONE',  ( 0.000000000000000000, -7.086529944415894657E-15, 1.000000000000000000 ) ) ;
#49921 = CARTESIAN_POINT ( 'NONE',  ( -16.78805706634180339, 66.05174750694033037, -48.67895427649254003 ) ) ;
#49922 = DIRECTION ( 'NONE',  ( 1.000000000000000000, -0.000000000000000000, -0.000000000000000000 ) ) ;
#49923 = DIRECTION ( 'NONE',  ( -1.000000000000000000, -0.000000000000000000, -0.000000000000000000 ) ) ;
#49925 = ORIENTED_EDGE ( 'NONE', *, *, #146996, .F. ) ;
#49924 = TOROIDAL_SURFACE ( 'NONE', #166667, 2.100000000000002309, 0.1000000000000000056 ) ;
#49926 = ORIENTED_EDGE ( 'NONE', *, *, #236764, .F. ) ;
#49927 = ORIENTED_EDGE ( 'NONE', *, *, #95246, .T. ) ;
#49928 = CARTESIAN_POINT ( 'NONE',  ( 20.59588692710267921, 65.63127657884309940, -95.38402639001375860 ) ) ;
#49929 = CARTESIAN_POINT ( 'NONE',  ( 20.09999999999999787, 9.750000000011137757, -79.65000000000004832 ) ) ;
#49930 = ORIENTED_EDGE ( 'NONE', *, *, #122078, .F. ) ;
#49932 = EDGE_CURVE ( 'NONE', #208853, #238489, #44244, .T. ) ;
#49931 = ORIENTED_EDGE ( 'NONE', *, *, #111803, .T. ) ;
#49933 = AXIS2_PLACEMENT_3D ( 'NONE', #1072, #257939, #118501 ) ;
#49934 = ORIENTED_EDGE ( 'NONE', *, *, #63382, .T. ) ;
#49935 = CARTESIAN_POINT ( 'NONE',  ( 21.95218792049437795, 7.201507561257818324, -66.90097156020011937 ) ) ;
#49936 = CIRCLE ( 'NONE', #141515, 11.70000000000000284 ) ;
#49937 = ORIENTED_EDGE ( 'NONE', *, *, #147521, .F. ) ;
#49938 = DIRECTION ( 'NONE',  ( 0.5000000000001141309, -6.047423072554455661E-15, 0.8660254037843729824 ) ) ;
#49939 = CARTESIAN_POINT ( 'NONE',  ( -21.05000000000000071, -1.162701749926853712, -175.5999999999999659 ) ) ;
#49940 = DIRECTION ( 'NONE',  ( -1.000000000000000000, 0.000000000000000000, -0.000000000000000000 ) ) ;
#49941 = EDGE_CURVE ( 'NONE', #130548, #44866, #253501, .T. ) ;
#49942 = CARTESIAN_POINT ( 'NONE',  ( 18.49999999999998934, 30.62437029989165893, -230.5032680968432715 ) ) ;
#49943 = DIRECTION ( 'NONE',  ( 0.000000000000000000, -0.5826443254699743557, -0.8127272543711318020 ) ) ;
#49945 = ORIENTED_EDGE ( 'NONE', *, *, #211029, .T. ) ;
#49944 = CARTESIAN_POINT ( 'NONE',  ( 21.05000000000000071, 76.10000000001203091, -114.6726782920691079 ) ) ;
#49947 = CARTESIAN_POINT ( 'NONE',  ( 21.00000000000000000, 43.94346684630428967, -235.6041041703296344 ) ) ;
#49946 = CARTESIAN_POINT ( 'NONE',  ( 20.95556889135987788, 65.37805641227650710, -61.88071326266687322 ) ) ;
#49948 = CARTESIAN_POINT ( 'NONE',  ( -17.01764560440441088, 9.949999999999983302, -20.75000000078611251 ) ) ;
#49949 = ORIENTED_EDGE ( 'NONE', *, *, #235914, .F. ) ;
#49950 = CARTESIAN_POINT ( 'NONE',  ( 13.12220780326572012, 66.56936653093924861, -121.2913416897002890 ) ) ;
#49951 = DIRECTION ( 'NONE',  ( 1.000000000000000000, 0.000000000000000000, 0.000000000000000000 ) ) ;
#49953 = EDGE_CURVE ( 'NONE', #139879, #166580, #153619, .T. ) ;
#49952 = DIRECTION ( 'NONE',  ( 3.265361837132813093E-16, -1.000000000000000000, -0.000000000000000000 ) ) ;
#49954 = ADVANCED_FACE ( 'NONE', ( #228007 ), #65076, .F. ) ;
#49955 = ORIENTED_EDGE ( 'NONE', *, *, #86201, .F. ) ;
#49956 = DIRECTION ( 'NONE',  ( 1.000000000000000000, 0.000000000000000000, 0.000000000000000000 ) ) ;
#49957 = AXIS2_PLACEMENT_3D ( 'NONE', #230297, #30851, #112930 ) ;
#49958 = VECTOR ( 'NONE', #39536, 1000.000000000000000 ) ;
#49959 = CARTESIAN_POINT ( 'NONE',  ( -18.59999999999999787, 85.50000000001263345, -195.4231074845242802 ) ) ;
#49960 = VERTEX_POINT ( 'NONE', #85893 ) ;
#49961 = ADVANCED_FACE ( 'NONE', ( #183750 ), #128914, .F. ) ;
#49962 = DIRECTION ( 'NONE',  ( -1.000000000000000000, -2.952720810173289112E-16, 0.000000000000000000 ) ) ;
#49964 = ADVANCED_FACE ( 'NONE', ( #105452 ), #191181, .T. ) ;
#49963 = SPHERICAL_SURFACE ( 'NONE', #32865, 0.1000000000000000056 ) ;
#49965 = CARTESIAN_POINT ( 'NONE',  ( 22.59999999999999432, 64.25012875563515991, -69.58853707553808476 ) ) ;
#49966 = DIRECTION ( 'NONE',  ( -6.938893903907222067E-15, 1.000000000000000000, 2.891205793294679805E-16 ) ) ;
#49967 = ORIENTED_EDGE ( 'NONE', *, *, #251446, .F. ) ;
#49968 = EDGE_CURVE ( 'NONE', #167954, #23326, #7827, .T. ) ;
#49969 = ORIENTED_EDGE ( 'NONE', *, *, #179024, .F. ) ;
#49970 = DIRECTION ( 'NONE',  ( 0.000000000000000000, 0.9651348961777163060, -0.2617529984165013479 ) ) ;
#49971 = CARTESIAN_POINT ( 'NONE',  ( 21.05000000000000426, 10.56275983746218117, -40.95681395791864077 ) ) ;
#49972 = VECTOR ( 'NONE', #150445, 1000.000000000000000 ) ;
#49973 = EDGE_CURVE ( 'NONE', #401, #245998, #78705, .T. ) ;
#49974 = FACE_OUTER_BOUND ( 'NONE', #98947, .T. ) ;
#49976 = CARTESIAN_POINT ( 'NONE',  ( -18.50000000000000000, 66.65000000001187175, -90.87310748452436826 ) ) ;
#49975 = CONICAL_SURFACE ( 'NONE', #95746, 7.750000000000020428, 0.7853981633974531640 ) ;
#49977 = TOROIDAL_SURFACE ( 'NONE', #20978, 11.65000000000000036, 0.1000000000000000056 ) ;
#49980 = CARTESIAN_POINT ( 'NONE',  ( -21.05000000000000071, 75.74389420792046224, -203.5580039261966760 ) ) ;
#49979 = AXIS2_PLACEMENT_3D ( 'NONE', #170263, #12443, #125932 ) ;
#49978 = CARTESIAN_POINT ( 'NONE',  ( 21.14999999999999503, -11.74999999998883560, -88.75000000000004263 ) ) ;
#49981 = DIRECTION ( 'NONE',  ( 0.000000000000000000, -6.938893903907270030E-14, 1.000000000000000000 ) ) ;
#49983 = EDGE_CURVE ( 'NONE', #185852, #119534, #212021, .T. ) ;
#49982 = DIRECTION ( 'NONE',  ( 0.000000000000000000, -0.1290532225515392262, -0.9916376685811522096 ) ) ;
#49985 = EDGE_CURVE ( 'NONE', #150648, #248438, #89764, .T. ) ;
#49984 = DIRECTION ( 'NONE',  ( -2.940209281316621016E-16, -1.000000000000000000, -7.056502275159890832E-15 ) ) ;
#49986 = ORIENTED_EDGE ( 'NONE', *, *, #8735, .T. ) ;
#49987 = CARTESIAN_POINT ( 'NONE',  ( 21.05000000000000071, -9.499999999988844479, -124.1060308773475924 ) ) ;
#49989 = VERTEX_POINT ( 'NONE', #211016 ) ;
#49988 = DIRECTION ( 'NONE',  ( 1.713247197920696616E-14, 0.9876197685951252359, -0.1568667991644863424 ) ) ;
#49990 = AXIS2_PLACEMENT_3D ( 'NONE', #174482, #173196, #57011 ) ;
#49991 = DIRECTION ( 'NONE',  ( -1.000000000000000000, 2.849773892568378313E-16, -7.728835255496647986E-17 ) ) ;
#49992 = CARTESIAN_POINT ( 'NONE',  ( 23.04999999999999716, 19.44861527341281615, -230.3234391047226666 ) ) ;
#49993 = CARTESIAN_POINT ( 'NONE',  ( -20.94999999999999929, 11.65000000001115232, -100.5000000000000426 ) ) ;
#49994 = CARTESIAN_POINT ( 'NONE',  ( 21.05000000000000071, -11.48912529306490349, -170.5999999999999659 ) ) ;
#49995 = EDGE_CURVE ( 'NONE', #171330, #73607, #182816, .T. ) ;
#49996 = DIRECTION ( 'NONE',  ( 0.000000000000000000, 0.2617529984165174461, 0.9651348961777118651 ) ) ;
#49998 = EDGE_LOOP ( 'NONE', ( #134251, #2974, #222966 ) ) ;
#49997 = DIRECTION ( 'NONE',  ( 0.000000000000000000, -6.982962677686266711E-15, 1.000000000000000000 ) ) ;
#49999 = CARTESIAN_POINT ( 'NONE',  ( -22.39999999999999858, 68.20922040163824818, -69.62310748452438247 ) ) ;
#50000 = CYLINDRICAL_SURFACE ( 'NONE', #216258, 0.09999999999999939493 ) ;
#50001 = CARTESIAN_POINT ( 'NONE',  ( 18.79999999999999716, 1.212568896937007645, -7.900000000000000355 ) ) ;
#50002 = DIRECTION ( 'NONE',  ( 1.000000000000000000, 0.000000000000000000, 0.000000000000000000 ) ) ;
#50003 = ORIENTED_EDGE ( 'NONE', *, *, #67045, .F. ) ;
#50004 = DIRECTION ( 'NONE',  ( 1.000000000000000000, 0.000000000000000000, 0.000000000000000000 ) ) ;
#50005 = EDGE_CURVE ( 'NONE', #111912, #13073, #76626, .T. ) ;
#50007 = ORIENTED_EDGE ( 'NONE', *, *, #21284, .T. ) ;
#50006 = CIRCLE ( 'NONE', #99, 0.1000000000000002554 ) ;
#50008 = EDGE_CURVE ( 'NONE', #120817, #70703, #99542, .T. ) ;
#50009 = CIRCLE ( 'NONE', #116636, 0.1000000000000001860 ) ;
#50010 = EDGE_CURVE ( 'NONE', #239754, #52643, #157895, .T. ) ;
#50011 = ORIENTED_EDGE ( 'NONE', *, *, #61961, .F. ) ;
#50012 = DIRECTION ( 'NONE',  ( 0.000000000000000000, 0.8814952561688429444, -0.4721928772777348460 ) ) ;
#50013 = ORIENTED_EDGE ( 'NONE', *, *, #146857, .F. ) ;
#50014 = DIRECTION ( 'NONE',  ( 1.000000000000000000, 0.000000000000000000, 0.000000000000000000 ) ) ;
#50015 = DIRECTION ( 'NONE',  ( 1.000000000000000000, 0.000000000000000000, 0.000000000000000000 ) ) ;
#50016 = CARTESIAN_POINT ( 'NONE',  ( 21.05000000000000071, 1.115600667400684642E-11, -104.5000000000000568 ) ) ;
#50017 = ORIENTED_EDGE ( 'NONE', *, *, #233545, .F. ) ;
#50018 = EDGE_CURVE ( 'NONE', #179078, #224002, #32407, .T. ) ;
#50019 = EDGE_CURVE ( 'NONE', #75576, #222999, #49513, .T. ) ;
#50020 = DIRECTION ( 'NONE',  ( -1.000000000000000000, 0.000000000000000000, 0.000000000000000000 ) ) ;
#50021 = DIRECTION ( 'NONE',  ( -0.000000000000000000, 1.000000000000000000, -0.000000000000000000 ) ) ;
#50022 = DIRECTION ( 'NONE',  ( -0.000000000000000000, 6.982962677686266711E-15, -1.000000000000000000 ) ) ;
#50023 = DIRECTION ( 'NONE',  ( 0.000000000000000000, 6.853228547068871147E-15, -1.000000000000000000 ) ) ;
#50025 = CYLINDRICAL_SURFACE ( 'NONE', #182036, 0.09999999999999781286 ) ;
#50024 = TOROIDAL_SURFACE ( 'NONE', #16727, 0.4000000000000003553, 0.1000000000000000056 ) ;
#50026 = DIRECTION ( 'NONE',  ( 0.000000000000000000, 6.982962677686266711E-15, -1.000000000000000000 ) ) ;
#50027 = ORIENTED_EDGE ( 'NONE', *, *, #232325, .T. ) ;
#50029 = EDGE_LOOP ( 'NONE', ( #157967, #132686, #189311, #27754 ) ) ;
#50028 = PLANE ( 'NONE',  #127752 ) ;
#50030 = ORIENTED_EDGE ( 'NONE', *, *, #143859, .T. ) ;
#50031 = CARTESIAN_POINT ( 'NONE',  ( 21.05000000000000071, 76.00000000001195133, -103.0231074845243171 ) ) ;
#50032 = EDGE_LOOP ( 'NONE', ( #107967, #257405, #41509, #125930 ) ) ;
#50033 = CYLINDRICAL_SURFACE ( 'NONE', #151795, 0.09999999999999939493 ) ;
#50034 = DIRECTION ( 'NONE',  ( -0.000000000000000000, -1.000000000000000000, 0.000000000000000000 ) ) ;
#50035 = AXIS2_PLACEMENT_3D ( 'NONE', #141015, #41926, #121469 ) ;
#50036 = VERTEX_POINT ( 'NONE', #93629 ) ;
#50037 = DIRECTION ( 'NONE',  ( 2.557131231893036985E-16, -0.8660254037844383745, 0.5000000000000003331 ) ) ;
#50038 = CARTESIAN_POINT ( 'NONE',  ( 18.49999999999999289, 11.75000000001115907, -88.75000000000004263 ) ) ;
#50039 = CARTESIAN_POINT ( 'NONE',  ( 18.39999999999999858, -9.682403433465241349, -140.6568433774128266 ) ) ;
#50040 = VERTEX_POINT ( 'NONE', #209732 ) ;
#50042 = VERTEX_POINT ( 'NONE', #130173 ) ;
#50041 = CARTESIAN_POINT ( 'NONE',  ( -17.11825945287482753, 65.95000000001186891, -90.27310748452438816 ) ) ;
#50043 = CARTESIAN_POINT ( 'NONE',  ( -25.10847955711010115, 9.068702471349579852, -347.0000000000001137 ) ) ;
#50044 = CARTESIAN_POINT ( 'NONE',  ( 21.05000000000000071, 0.000000000000000000, -33.50000000000000000 ) ) ;
#50045 = EDGE_CURVE ( 'NONE', #81897, #51105, #220215, .T. ) ;
#50046 = AXIS2_PLACEMENT_3D ( 'NONE', #20866, #196900, #216460 ) ;
#50047 = EDGE_CURVE ( 'NONE', #53080, #7765, #191480, .T. ) ;
#50048 = CIRCLE ( 'NONE', #79057, 0.1000000000000028644 ) ;
#50049 = ORIENTED_EDGE ( 'NONE', *, *, #40804, .F. ) ;
#50050 = DIRECTION ( 'NONE',  ( -1.000000000000000000, -1.875376730785737719E-16, -0.000000000000000000 ) ) ;
#50051 = CARTESIAN_POINT ( 'NONE',  ( -21.14999999999999858, 87.75000000001237765, -170.0231074845242745 ) ) ;
#50052 = DIRECTION ( 'NONE',  ( 0.000000000000000000, 0.000000000000000000, -1.000000000000000000 ) ) ;
#50053 = ORIENTED_EDGE ( 'NONE', *, *, #135861, .F. ) ;
#50054 = DIRECTION ( 'NONE',  ( 0.000000000000000000, -0.5000000000000209832, 0.8660254037844264952 ) ) ;
#50055 = AXIS2_PLACEMENT_3D ( 'NONE', #85195, #143915, #142619 ) ;
#50056 = CARTESIAN_POINT ( 'NONE',  ( -21.14999999999999858, -0.09999999998884338825, -155.8504291924551808 ) ) ;
#50057 = AXIS2_PLACEMENT_3D ( 'NONE', #10203, #144547, #45461 ) ;
#50058 = VECTOR ( 'NONE', #14159, 1000.000000000000000 ) ;
#50059 = EDGE_LOOP ( 'NONE', ( #226317, #84254, #31123, #118779 ) ) ;
#50060 = EDGE_CURVE ( 'NONE', #56225, #209971, #28711, .T. ) ;
#50061 = VECTOR ( 'NONE', #134895, 1000.000000000000000 ) ;
#50062 = CIRCLE ( 'NONE', #116703, 0.1000000000000070832 ) ;
#50063 = CIRCLE ( 'NONE', #8385, 0.09999999999998898659 ) ;
#50064 = EDGE_LOOP ( 'NONE', ( #70393, #217263, #194947, #42132 ) ) ;
#50066 = DIRECTION ( 'NONE',  ( 0.2834754621636439431, 0.9519569026850353000, 0.1158435055642859091 ) ) ;
#50065 = VECTOR ( 'NONE', #117286, 1000.000000000000000 ) ;
#50067 = AXIS2_PLACEMENT_3D ( 'NONE', #86143, #64046, #83574 ) ;
#50068 = ORIENTED_EDGE ( 'NONE', *, *, #127798, .T. ) ;
#50069 = FACE_OUTER_BOUND ( 'NONE', #8122, .T. ) ;
#50070 = CARTESIAN_POINT ( 'NONE',  ( 21.05000000000000071, 5.500000000011153745, -45.90526601891310321 ) ) ;
#50072 = ORIENTED_EDGE ( 'NONE', *, *, #214933, .F. ) ;
#50071 = CARTESIAN_POINT ( 'NONE',  ( 15.70340296795548873, 25.90497867185233360, -233.1769111789295721 ) ) ;
#50073 = CARTESIAN_POINT ( 'NONE',  ( -22.47071067811865319, 68.27992525551462677, -203.6221999392270448 ) ) ;
#50074 = CARTESIAN_POINT ( 'NONE',  ( 21.05193202509564543, 65.27606398031439028, -57.35057288119863728 ) ) ;
#50075 = DIRECTION ( 'NONE',  ( -1.000000000000000000, -0.000000000000000000, -0.000000000000000000 ) ) ;
#50076 = LINE ( 'NONE', #129623, #92110 ) ;
#50077 = CARTESIAN_POINT ( 'NONE',  ( -18.50000000000000000, 5.950000000011100632, -177.8057023050348278 ) ) ;
#50078 = LINE ( 'NONE', #8401, #201547 ) ;
#50079 = CARTESIAN_POINT ( 'NONE',  ( -18.45037301276681418, -9.490200447530819261, -107.5126741364140912 ) ) ;
#50080 = AXIS2_PLACEMENT_3D ( 'NONE', #170153, #250910, #210521 ) ;
#50082 = ORIENTED_EDGE ( 'NONE', *, *, #47369, .T. ) ;
#50081 = CARTESIAN_POINT ( 'NONE',  ( -22.45372860728439690, 75.98507938046353161, -114.6729046192281913 ) ) ;
#50083 = FACE_OUTER_BOUND ( 'NONE', #156282, .T. ) ;
#50084 = DIRECTION ( 'NONE',  ( 1.000000000000000000, 0.000000000000000000, 0.000000000000000000 ) ) ;
#50085 = CARTESIAN_POINT ( 'NONE',  ( 22.49436431346199683, 11.64995094766461392, -66.93309647027778908 ) ) ;
#50086 = DIRECTION ( 'NONE',  ( 1.000000000000000000, -0.000000000000000000, -0.000000000000000000 ) ) ;
#50087 = DIRECTION ( 'NONE',  ( -1.000000000000000000, 2.849773892568378313E-16, -7.728835255496647986E-17 ) ) ;
#50088 = ORIENTED_EDGE ( 'NONE', *, *, #163175, .T. ) ;
#50089 = ADVANCED_FACE ( 'NONE', ( #54495 ), #190175, .T. ) ;
#50090 = DIRECTION ( 'NONE',  ( 0.000000000000000000, -1.000000000000000000, 0.000000000000000000 ) ) ;
#50091 = CARTESIAN_POINT ( 'NONE',  ( 23.14999999999999503, 11.65000000001116298, -88.35000000000003695 ) ) ;
#50092 = EDGE_CURVE ( 'NONE', #205047, #57915, #95302, .T. ) ;
#50093 = CARTESIAN_POINT ( 'NONE',  ( 20.94999999999999574, 1.250000000011155299, -175.3999999999999773 ) ) ;
#50094 = ORIENTED_EDGE ( 'NONE', *, *, #40939, .T. ) ;
#50095 = CIRCLE ( 'NONE', #12724, 0.1999999999999987899 ) ;
#50096 = FACE_OUTER_BOUND ( 'NONE', #131603, .T. ) ;
#50097 = CARTESIAN_POINT ( 'NONE',  ( -21.53699400377577433, 60.68021703623777796, -234.0784225921609050 ) ) ;
#50098 = ADVANCED_FACE ( 'NONE', ( #212312 ), #11541, .T. ) ;
#50099 = VERTEX_POINT ( 'NONE', #114475 ) ;
#50100 = CARTESIAN_POINT ( 'NONE',  ( -21.13435531349821872, 6.493721063603322463, -67.00000000000004263 ) ) ;
#50101 = ORIENTED_EDGE ( 'NONE', *, *, #212169, .T. ) ;
#50102 = PLANE ( 'NONE',  #184030 ) ;
#50103 = ORIENTED_EDGE ( 'NONE', *, *, #82679, .F. ) ;
#50104 = EDGE_CURVE ( 'NONE', #59781, #65824, #116350, .T. ) ;
#50105 = LINE ( 'NONE', #170112, #252459 ) ;
#50106 = VERTEX_POINT ( 'NONE', #252686 ) ;
#50107 = AXIS2_PLACEMENT_3D ( 'NONE', #105962, #186827, #8187 ) ;
#50108 = DIRECTION ( 'NONE',  ( 1.000000000000000000, 0.000000000000000000, 0.000000000000000000 ) ) ;
#50109 = EDGE_LOOP ( 'NONE', ( #152524, #219159, #41967, #205414 ) ) ;
#50110 = ORIENTED_EDGE ( 'NONE', *, *, #121789, .T. ) ;
#50111 = CARTESIAN_POINT ( 'NONE',  ( -20.94999999999999929, -11.74999999998884448, -136.9000000000000341 ) ) ;
#50112 = EDGE_CURVE ( 'NONE', #114130, #252230, #45605, .T. ) ;
#50114 = EDGE_LOOP ( 'NONE', ( #151505, #125442, #105612, #114920 ) ) ;
#50113 = SURFACE_STYLE_FILL_AREA ( #110090 ) ;
#50115 = FACE_OUTER_BOUND ( 'NONE', #191404, .T. ) ;
#50116 = AXIS2_PLACEMENT_3D ( 'NONE', #199712, #164421, #142273 ) ;
#50117 = ORIENTED_EDGE ( 'NONE', *, *, #163596, .F. ) ;
#50118 = CIRCLE ( 'NONE', #75101, 0.09999999999999939493 ) ;
#50119 = EDGE_LOOP ( 'NONE', ( #203781, #18516, #57789, #247404 ) ) ;
#50120 = CARTESIAN_POINT ( 'NONE',  ( 20.85000000000000142, 42.15997144203495139, -239.2817429668763793 ) ) ;
#50121 = ADVANCED_FACE ( 'NONE', ( #233167 ), #253970, .F. ) ;
#50122 = LINE ( 'NONE', #30593, #113660 ) ;
#50123 =( BOUNDED_SURFACE ( )  B_SPLINE_SURFACE ( 3, 2, ( 
 ( #64750, #245970, #25633 ),
 ( #146838, #6054, #89443 ),
 ( #85557, #226369, #46458 ),
 ( #225087, #244664, #47741 ),
 ( #43909, #26947, #66033 ),
 ( #145565, #103858, #28232 ) ),
 .UNSPECIFIED., .F., .F., .F. ) 
 B_SPLINE_SURFACE_WITH_KNOTS ( ( 4, 2, 4 ),
 ( 3, 3 ),
 ( 1.570796326794897668, 2.356194490192346169, 3.141592653589794448 ),
 ( 0.000000000000000000, 1.000000000000000000 ),
 .UNSPECIFIED. ) 
 GEOMETRIC_REPRESENTATION_ITEM ( )  RATIONAL_B_SPLINE_SURFACE ( (
 ( 1.000000000000000000, 0.7071067811865806574, 1.000000000000000000),
 ( 1.000000000000000000, 0.6611148371769989263, 1.000000000000000000),
 ( 1.000000000000000000, 0.6092287576708182995, 1.000000000000000000),
 ( 1.000000000000000000, 0.5278258667044445351, 1.000000000000000000),
 ( 1.000000000000000000, 0.4993418825344856371, 1.000000000000000000),
 ( 1.000000000000000000, 0.5000000000000655032, 1.000000000000000000) ) ) 
 REPRESENTATION_ITEM ( '' )  SURFACE ( )  );
#50124 = ORIENTED_EDGE ( 'NONE', *, *, #6521, .T. ) ;
#50125 = CARTESIAN_POINT ( 'NONE',  ( -21.55000000000000426, 68.29142135624930177, -115.3731074845243540 ) ) ;
#50126 = CARTESIAN_POINT ( 'NONE',  ( -18.42609945526390902, -9.499999710479540838, -73.99936249024790413 ) ) ;
#50127 = DIRECTION ( 'NONE',  ( 0.000000000000000000, -0.1298341882520079038, -0.9915357197604846018 ) ) ;
#50128 = EDGE_LOOP ( 'NONE', ( #38941, #194109, #155629 ) ) ;
#50129 = CARTESIAN_POINT ( 'NONE',  ( -21.51976009735018636, 60.56174996242723552, -234.0462932889414560 ) ) ;
#50130 = FACE_OUTER_BOUND ( 'NONE', #231101, .T. ) ;
#50131 = CARTESIAN_POINT ( 'NONE',  ( -18.40000000000000213, 11.75000000001113953, -46.15000000000000568 ) ) ;
#50132 = LINE ( 'NONE', #51392, #130241 ) ;
#50133 = AXIS2_PLACEMENT_3D ( 'NONE', #82145, #203416, #85992 ) ;
#50134 = ORIENTED_EDGE ( 'NONE', *, *, #179428, .F. ) ;
#50135 = CARTESIAN_POINT ( 'NONE',  ( 20.85000000000000142, 7.804459559388681633, -245.4620200072988325 ) ) ;
#50136 = ORIENTED_EDGE ( 'NONE', *, *, #17054, .F. ) ;
#50137 = EDGE_LOOP ( 'NONE', ( #257336, #75929, #51102, #168855 ) ) ;
#50138 = CARTESIAN_POINT ( 'NONE',  ( -14.23072895065542376, 24.82647667088539478, -232.4856315176583905 ) ) ;
#50139 = CARTESIAN_POINT ( 'NONE',  ( 23.24999999999999645, 1.115600667400684642E-11, -167.4999999999999716 ) ) ;
#50140 = EDGE_LOOP ( 'NONE', ( #202935, #155893, #28745, #120860 ) ) ;
#50141 = VERTEX_POINT ( 'NONE', #36249 ) ;
#50143 = ORIENTED_EDGE ( 'NONE', *, *, #35571, .T. ) ;
#50142 = DIRECTION ( 'NONE',  ( 1.000000000000000000, 0.000000000000000000, 0.000000000000000000 ) ) ;
#50144 = DIRECTION ( 'NONE',  ( 0.000000000000000000, 0.000000000000000000, 1.000000000000000000 ) ) ;
#50145 = ORIENTED_EDGE ( 'NONE', *, *, #235077, .T. ) ;
#50146 = CARTESIAN_POINT ( 'NONE',  ( 23.14999999999999858, 9.125777775466493935, -211.6520035670780544 ) ) ;
#50147 = CARTESIAN_POINT ( 'NONE',  ( 20.85000000000000142, 1.115600667400684642E-11, -167.5000000000000284 ) ) ;
#50148 = ORIENTED_EDGE ( 'NONE', *, *, #90762, .T. ) ;
#50149 = AXIS2_PLACEMENT_3D ( 'NONE', #86907, #167785, #127344 ) ;
#50150 = AXIS2_PLACEMENT_3D ( 'NONE', #126587, #147433, #125309 ) ;
#50151 = AXIS2_PLACEMENT_3D ( 'NONE', #218293, #123085, #239171 ) ;
#50152 = EDGE_LOOP ( 'NONE', ( #34097, #130540, #187396, #181433 ) ) ;
#50153 = EDGE_CURVE ( 'NONE', #116247, #213696, #115760, .T. ) ;
#50154 = AXIS2_PLACEMENT_3D ( 'NONE', #239537, #40081, #222508 ) ;
#50155 = DIRECTION ( 'NONE',  ( 1.000000000000000000, -0.000000000000000000, -0.000000000000000000 ) ) ;
#50156 = CARTESIAN_POINT ( 'NONE',  ( -23.25000000000000000, 64.35000000001146248, -43.03791325517835276 ) ) ;
#50157 = EDGE_CURVE ( 'NONE', #102599, #223523, #79179, .T. ) ;
#50158 = DIRECTION ( 'NONE',  ( 1.000000000000000000, 0.000000000000000000, 0.000000000000000000 ) ) ;
#50160 = EDGE_LOOP ( 'NONE', ( #34725, #121665, #193949, #64705 ) ) ;
#50159 = DIRECTION ( 'NONE',  ( 0.000000000000000000, 0.2128009952263605342, -0.9770955615653315052 ) ) ;
#50161 = CARTESIAN_POINT ( 'NONE',  ( -20.94999999999999929, 7.021664781911246322, -171.3335654018973173 ) ) ;
#50162 = CIRCLE ( 'NONE', #191869, 0.09999999999999971412 ) ;
#50163 = CARTESIAN_POINT ( 'NONE',  ( 20.94999999999999929, 61.88149656937974896, -248.1136133839584090 ) ) ;
#50164 = CARTESIAN_POINT ( 'NONE',  ( 18.79999999999999716, 4.513204987021263825, 22.10000000000000142 ) ) ;
#50165 = EDGE_CURVE ( 'NONE', #210784, #9389, #97447, .T. ) ;
#50167 = PLANE ( 'NONE',  #16064 ) ;
#50166 = FACE_OUTER_BOUND ( 'NONE', #84171, .T. ) ;
#50169 = EDGE_CURVE ( 'NONE', #85465, #52763, #166437, .T. ) ;
#50168 = CARTESIAN_POINT ( 'NONE',  ( 21.05000000000000071, 87.75000000001172396, -72.42310748452422331 ) ) ;
#50170 = LINE ( 'NONE', #170182, #111187 ) ;
#50171 = DIRECTION ( 'NONE',  ( 0.000000000000000000, -0.9908441862701605762, -0.1350103645451835310 ) ) ;
#50172 = DIRECTION ( 'NONE',  ( 1.000000000000000000, 0.000000000000000000, 0.000000000000000000 ) ) ;
#50173 = ORIENTED_EDGE ( 'NONE', *, *, #98270, .T. ) ;
#50174 = VERTEX_POINT ( 'NONE', #3498 ) ;
#50175 = ORIENTED_EDGE ( 'NONE', *, *, #52992, .T. ) ;
#50176 = ADVANCED_FACE ( 'NONE', ( #120924 ), #42637, .F. ) ;
#50177 = DIRECTION ( 'NONE',  ( 0.000000000000000000, -0.9651348961777379554, 0.2617529984164210233 ) ) ;
#50178 = ADVANCED_FACE ( 'NONE', ( #21806 ), #91402, .T. ) ;
#50179 = CARTESIAN_POINT ( 'NONE',  ( -23.15000000000000213, 36.65892442174472876, -249.5511627012454596 ) ) ;
#50180 = ORIENTED_EDGE ( 'NONE', *, *, #43267, .F. ) ;
#50181 = DIRECTION ( 'NONE',  ( 0.000000000000000000, -0.3488585713686311318, -0.9371753822965249725 ) ) ;
#50182 = CARTESIAN_POINT ( 'NONE',  ( -16.88328101497759448, 63.08570056202644594, -213.1263908404952474 ) ) ;
#50183 = AXIS2_PLACEMENT_3D ( 'NONE', #46211, #183180, #200165 ) ;
#50184 = DIRECTION ( 'NONE',  ( 0.000000000000000000, 0.000000000000000000, -1.000000000000000000 ) ) ;
#50185 = ORIENTED_EDGE ( 'NONE', *, *, #39440, .T. ) ;
#50186 = ORIENTED_EDGE ( 'NONE', *, *, #134126, .T. ) ;
#50187 = CYLINDRICAL_SURFACE ( 'NONE', #13276, 0.1000000000000055705 ) ;
#50188 = DIRECTION ( 'NONE',  ( -0.000000000000000000, -0.000000000000000000, -1.000000000000000000 ) ) ;
#50189 = VERTEX_POINT ( 'NONE', #158766 ) ;
#50190 = EDGE_CURVE ( 'NONE', #251279, #77493, #87273, .T. ) ;
#50191 = AXIS2_PLACEMENT_3D ( 'NONE', #67574, #247497, #66300 ) ;
#50192 = ADVANCED_FACE ( 'NONE', ( #38801 ), #161321, .T. ) ;
#50193 = LINE ( 'NONE', #111471, #157838 ) ;
#50195 = EDGE_LOOP ( 'NONE', ( #29904, #82099, #12766, #146319 ) ) ;
#50194 = CARTESIAN_POINT ( 'NONE',  ( -16.94445028196807002, 66.00793639031407167, -82.13043766294282477 ) ) ;
#50196 = CARTESIAN_POINT ( 'NONE',  ( 21.05000000000000071, 77.16270174994961906, -61.62310748452431142 ) ) ;
#50197 = EDGE_CURVE ( 'NONE', #209005, #98180, #53961, .T. ) ;
#50198 = CARTESIAN_POINT ( 'NONE',  ( -21.05000000000000071, 1.115600667400684642E-11, -33.50000000000000000 ) ) ;
#50200 = EDGE_LOOP ( 'NONE', ( #104220, #50981, #97996, #175103 ) ) ;
#50199 = CARTESIAN_POINT ( 'NONE',  ( 21.13736287352038445, 8.046642376395153562, -143.2500000000000284 ) ) ;
#50201 = CARTESIAN_POINT ( 'NONE',  ( -16.97683809663752186, 9.950000000011138823, -87.09763598180373378 ) ) ;
#50202 = DIRECTION ( 'NONE',  ( 0.000000000000000000, 1.000000000000000000, 1.224646799147353207E-16 ) ) ;
#50203 = CARTESIAN_POINT ( 'NONE',  ( -16.94225986326250677, 9.950000000011137047, -113.4467193756079268 ) ) ;
#50205 = DIRECTION ( 'NONE',  ( 1.000000000000000000, 0.000000000000000000, 0.000000000000000000 ) ) ;
#50204 = CYLINDRICAL_SURFACE ( 'NONE', #215700, 0.1000000000000018374 ) ;
#50206 = CARTESIAN_POINT ( 'NONE',  ( 18.53691006697098942, 10.30215155716143016, -91.70219871729851491 ) ) ;
#50207 = CIRCLE ( 'NONE', #143, 0.1000000000000028644 ) ;
#50208 = CARTESIAN_POINT ( 'NONE',  ( -11.60000000000000320, -11.65000000000000036, 15.00000000000000355 ) ) ;
#50209 = PLANE ( 'NONE',  #201635 ) ;
#50210 = CARTESIAN_POINT ( 'NONE',  ( -20.65000000000000568, 68.75000000001263345, -194.2731074845244166 ) ) ;
#50211 = CIRCLE ( 'NONE', #112602, 0.1000000000000028644 ) ;
#50212 = VERTEX_POINT ( 'NONE', #118341 ) ;
#50213 = ORIENTED_EDGE ( 'NONE', *, *, #134950, .F. ) ;
#50215 = VERTEX_POINT ( 'NONE', #2210 ) ;
#50214 = ADVANCED_FACE ( 'NONE', ( #156200 ), #57036, .T. ) ;
#50217 = FACE_OUTER_BOUND ( 'NONE', #242898, .T. ) ;
#50216 = AXIS2_PLACEMENT_3D ( 'NONE', #229584, #186613, #49649 ) ;
#50218 = ORIENTED_EDGE ( 'NONE', *, *, #200022, .T. ) ;
#50219 = CYLINDRICAL_SURFACE ( 'NONE', #60976, 0.1000000000000098310 ) ;
#50220 = DIRECTION ( 'NONE',  ( 1.000000000000000000, 0.000000000000000000, 0.000000000000000000 ) ) ;
#50221 = AXIS2_PLACEMENT_3D ( 'NONE', #109926, #52517, #248169 ) ;
#50223 = EDGE_CURVE ( 'NONE', #185777, #228133, #3908, .T. ) ;
#50222 = ORIENTED_EDGE ( 'NONE', *, *, #24791, .T. ) ;
#50224 = DIRECTION ( 'NONE',  ( -1.000000000000000000, 0.000000000000000000, 0.000000000000000000 ) ) ;
#50226 = ORIENTED_EDGE ( 'NONE', *, *, #219810, .T. ) ;
#50225 = CIRCLE ( 'NONE', #171106, 12.77500000000000036 ) ;
#50227 = VERTEX_POINT ( 'NONE', #81727 ) ;
#50228 = CIRCLE ( 'NONE', #183350, 0.5000000000000009992 ) ;
#50229 = EDGE_LOOP ( 'NONE', ( #179297, #85356, #28393, #128488 ) ) ;
#50230 = AXIS2_PLACEMENT_3D ( 'NONE', #76858, #159007, #217635 ) ;
#50231 = AXIS2_PLACEMENT_3D ( 'NONE', #48020, #150987, #10202 ) ;
#50232 = CARTESIAN_POINT ( 'NONE',  ( 21.05000000000000071, 67.23127455305835554, -235.8551265064784559 ) ) ;
#50233 = CARTESIAN_POINT ( 'NONE',  ( 21.05000000000000071, 10.56271494673968725, -40.95680210564469803 ) ) ;
#50234 = CARTESIAN_POINT ( 'NONE',  ( 21.14999999999999858, 22.98593783141595992, -230.0732594427593938 ) ) ;
#50235 = FACE_OUTER_BOUND ( 'NONE', #179675, .T. ) ;
#50236 = ADVANCED_FACE ( 'NONE', ( #201710 ), #178329, .F. ) ;
#50237 = DIRECTION ( 'NONE',  ( 7.304098846218134667E-16, -1.000000000000000000, 0.000000000000000000 ) ) ;
#50238 = DIRECTION ( 'NONE',  ( 0.000000000000000000, 0.000000000000000000, 1.000000000000000000 ) ) ;
#50240 = ORIENTED_EDGE ( 'NONE', *, *, #56634, .F. ) ;
#50239 = CARTESIAN_POINT ( 'NONE',  ( -20.94983749550516450, 10.29766095125282810, -139.4743663933276139 ) ) ;
#50242 = CARTESIAN_POINT ( 'NONE',  ( 22.39999999999999503, 1.115600667400684642E-11, -159.7092204016265669 ) ) ;
#50241 = CARTESIAN_POINT ( 'NONE',  ( -19.99999999999999645, 1.350000000000000089, 21.90000000000000213 ) ) ;
#50243 = CARTESIAN_POINT ( 'NONE',  ( -20.64999999999999858, 68.59518897103603763, -214.2073844195901131 ) ) ;
#50244 = ORIENTED_EDGE ( 'NONE', *, *, #204998, .T. ) ;
#50245 = CARTESIAN_POINT ( 'NONE',  ( 20.94999999999999574, 10.47338541492405994, -74.57865446424858646 ) ) ;
#50246 = DIRECTION ( 'NONE',  ( 0.000000000000000000, 0.000000000000000000, -1.000000000000000000 ) ) ;
#50248 = EDGE_CURVE ( 'NONE', #229678, #250282, #257780, .T. ) ;
#50247 = DIRECTION ( 'NONE',  ( -0.000000000000000000, 0.9770955615653315052, 0.2128009952263602844 ) ) ;
#50249 = VERTEX_POINT ( 'NONE', #139139 ) ;
#50250 = AXIS2_PLACEMENT_3D ( 'NONE', #69112, #45678, #26129 ) ;
#50251 = DIRECTION ( 'NONE',  ( -1.000000000000000000, -0.000000000000000000, 0.000000000000000000 ) ) ;
#50252 = EDGE_CURVE ( 'NONE', #191338, #231430, #99732, .T. ) ;
#50253 = CARTESIAN_POINT ( 'NONE',  ( 18.39999999999999503, 67.17743825834537574, -78.77310748452437394 ) ) ;
#50254 = LINE ( 'NONE', #153262, #142552 ) ;
#50255 = VERTEX_POINT ( 'NONE', #37521 ) ;
#50256 = VERTEX_POINT ( 'NONE', #102579 ) ;
#50257 = EDGE_CURVE ( 'NONE', #122787, #232039, #112260, .T. ) ;
#50259 = EDGE_CURVE ( 'NONE', #15820, #203639, #12298, .T. ) ;
#50258 = DIRECTION ( 'NONE',  ( -1.000000000000000000, -0.000000000000000000, -0.000000000000000000 ) ) ;
#50260 = CARTESIAN_POINT ( 'NONE',  ( -21.05000000000000071, 77.85102823015243700, -57.86919421510181394 ) ) ;
#50261 = CARTESIAN_POINT ( 'NONE',  ( -20.85000000000000142, 43.02787096365918984, -254.3959382439171577 ) ) ;
#50262 = CARTESIAN_POINT ( 'NONE',  ( 21.05000000000000071, 76.00000000001170974, -69.52310748452431710 ) ) ;
#50263 = ORIENTED_EDGE ( 'NONE', *, *, #204497, .F. ) ;
#50264 = AXIS2_PLACEMENT_3D ( 'NONE', #236137, #99169, #237426 ) ;
#50265 = CARTESIAN_POINT ( 'NONE',  ( 21.14999999999999858, -11.74999999998884448, -45.75000000000000711 ) ) ;
#50266 = DIRECTION ( 'NONE',  ( 0.000000000000000000, 0.000000000000000000, 1.000000000000000000 ) ) ;
#50267 = CARTESIAN_POINT ( 'NONE',  ( 22.24259225415828212, 0.09906588346399246292, -126.5080621294346059 ) ) ;
#50268 = CARTESIAN_POINT ( 'NONE',  ( -5.900000000000003020, -11.34999999999999964, 10.00000000000000178 ) ) ;
#50269 = AXIS2_PLACEMENT_3D ( 'NONE', #207954, #218178, #216907 ) ;
#50270 = EDGE_CURVE ( 'NONE', #54789, #111107, #907, .T. ) ;
#50271 = ORIENTED_EDGE ( 'NONE', *, *, #53881, .F. ) ;
#50273 = ADVANCED_FACE ( 'NONE', ( #45203 ), #54018, .T. ) ;
#50272 = LINE ( 'NONE', #29486, #67829 ) ;
#50274 = TOROIDAL_SURFACE ( 'NONE', #21109, 0.2000000000000000111, 0.1000000000000000056 ) ;
#50276 = EDGE_LOOP ( 'NONE', ( #204316, #221502, #76163, #50213, #158239 ) ) ;
#50275 = DIRECTION ( 'NONE',  ( -1.000000000000000000, 0.000000000000000000, 0.000000000000000000 ) ) ;
#50277 = DIRECTION ( 'NONE',  ( 0.000000000000000000, -0.7071067811865479058, 0.7071067811865472397 ) ) ;
#50278 = DIRECTION ( 'NONE',  ( 0.000000000000000000, 6.982962677686266711E-15, -1.000000000000000000 ) ) ;
#50279 = EDGE_CURVE ( 'NONE', #228033, #78723, #163881, .T. ) ;
#50280 = LINE ( 'NONE', #128558, #54525 ) ;
#50281 = FACE_OUTER_BOUND ( 'NONE', #236247, .T. ) ;
#50282 = DIRECTION ( 'NONE',  ( 0.000000000000000000, -0.2617529984164856383, -0.9651348961777204138 ) ) ;
#50283 = DIRECTION ( 'NONE',  ( 0.000000000000000000, 0.4088369013363281623, -0.9126074666063771490 ) ) ;
#50284 = ORIENTED_EDGE ( 'NONE', *, *, #215019, .T. ) ;
#50285 = CIRCLE ( 'NONE', #220980, 0.09999999999999939493 ) ;
#50286 = DIRECTION ( 'NONE',  ( 0.000000000000000000, 0.4721928772777346239, 0.8814952561688430555 ) ) ;
#50287 = DIRECTION ( 'NONE',  ( 0.000000000000000000, -0.9910465087640866200, -0.1335171055202867274 ) ) ;
#50288 = EDGE_CURVE ( 'NONE', #248274, #25370, #89045, .T. ) ;
#50289 = DIRECTION ( 'NONE',  ( -1.000000000000000000, 0.000000000000000000, 0.000000000000000000 ) ) ;
#50290 = EDGE_CURVE ( 'NONE', #139686, #72782, #244675, .T. ) ;
#50292 = AXIS2_PLACEMENT_3D ( 'NONE', #104107, #143248, #178568 ) ;
#50291 = CARTESIAN_POINT ( 'NONE',  ( 21.09096482362069835, 6.363544365415760851, -167.4605517212258974 ) ) ;
#50294 = CARTESIAN_POINT ( 'NONE',  ( 12.42718393586867087, 9.370655051134642477, -185.0258232559808960 ) ) ;
#50293 = VECTOR ( 'NONE', #124961, 1000.000000000000000 ) ;
#50295 = ORIENTED_EDGE ( 'NONE', *, *, #4902, .T. ) ;
#50296 = ORIENTED_EDGE ( 'NONE', *, *, #173239, .F. ) ;
#50297 = CIRCLE ( 'NONE', #108578, 0.1000000000000002554 ) ;
#50298 = DIRECTION ( 'NONE',  ( -0.000000000000000000, 1.000000000000000000, -0.000000000000000000 ) ) ;
#50299 = EDGE_CURVE ( 'NONE', #80879, #68170, #243401, .T. ) ;
#50300 = CARTESIAN_POINT ( 'NONE',  ( -17.29158576265544411, 63.00812307438908988, -211.8292821411627074 ) ) ;
#50301 = DIRECTION ( 'NONE',  ( -3.469446951953749873E-14, -0.4088369013363783999, 0.9126074666063545004 ) ) ;
#50302 = DIRECTION ( 'NONE',  ( 0.000000000000000000, 1.000000000000000000, 0.000000000000000000 ) ) ;
#50303 = EDGE_CURVE ( 'NONE', #182491, #162495, #78886, .T. ) ;
#50304 = CARTESIAN_POINT ( 'NONE',  ( 21.53551880898956838, 6.784797761416324846, 0.09896973457166428900 ) ) ;
#50305 = DIRECTION ( 'NONE',  ( 0.000000000000000000, 6.938893903907222067E-15, -1.000000000000000000 ) ) ;
#50306 = AXIS2_PLACEMENT_3D ( 'NONE', #180972, #203086, #121024 ) ;
#50307 = DIRECTION ( 'NONE',  ( -0.000000000000000000, 1.000000000000000000, 2.891205793294679805E-16 ) ) ;
#50308 = CARTESIAN_POINT ( 'NONE',  ( -23.15000000000000213, 64.35000000001203091, -114.7731074845243882 ) ) ;
#50309 = ORIENTED_EDGE ( 'NONE', *, *, #234533, .T. ) ;
#50310 = DIRECTION ( 'NONE',  ( 1.000000000000000000, 0.000000000000000000, 0.000000000000000000 ) ) ;
#50311 = ORIENTED_EDGE ( 'NONE', *, *, #227660, .T. ) ;
#50312 = LINE ( 'NONE', #107736, #22614 ) ;
#50313 = CARTESIAN_POINT ( 'NONE',  ( 21.05000000000000071, 10.72371710470752504, -7.664913569087607570 ) ) ;
#50314 = CARTESIAN_POINT ( 'NONE',  ( 21.08832698747859169, 8.775364393428372267, -79.22871746646418956 ) ) ;
#50315 = DIRECTION ( 'NONE',  ( -1.000000000000000000, 2.952720810173289112E-16, 2.061873921506763405E-30 ) ) ;
#50316 = LINE ( 'NONE', #131156, #120459 ) ;
#50317 = CARTESIAN_POINT ( 'NONE',  ( 21.14999999999999858, 64.35000000001156195, -57.37310748452439668 ) ) ;
#50318 = ORIENTED_EDGE ( 'NONE', *, *, #2086, .T. ) ;
#50319 = DIRECTION ( 'NONE',  ( 1.000000000000000000, 1.836970198721029934E-16, -0.000000000000000000 ) ) ;
#50320 = VECTOR ( 'NONE', #170374, 1000.000000000000000 ) ;
#50321 = CARTESIAN_POINT ( 'NONE',  ( -21.05000000000000071, 87.48912529308798014, -99.92310748452423752 ) ) ;
#50322 = VECTOR ( 'NONE', #147111, 1000.000000000000227 ) ;
#50323 = CARTESIAN_POINT ( 'NONE',  ( 20.94999999999999574, 44.49901850127302083, -247.5171717259850652 ) ) ;
#50324 = DIRECTION ( 'NONE',  ( 0.000000000000000000, 0.000000000000000000, -1.000000000000000000 ) ) ;
#50325 = CIRCLE ( 'NONE', #125546, 0.5000000000000004441 ) ;
#50326 = CARTESIAN_POINT ( 'NONE',  ( -18.40000000000000213, 11.47316190337364183, -158.1740539331920559 ) ) ;
#50327 = VECTOR ( 'NONE', #180525, 1000.000000000000000 ) ;
#50328 = ORIENTED_EDGE ( 'NONE', *, *, #187437, .F. ) ;
#50329 = CARTESIAN_POINT ( 'NONE',  ( -23.25000000000000000, 85.00000000001149658, -45.91707660717669626 ) ) ;
#50330 = DIRECTION ( 'NONE',  ( -1.000000000000000000, -0.000000000000000000, -0.000000000000000000 ) ) ;
#50331 = ADVANCED_FACE ( 'NONE', ( #146849 ), #70579, .F. ) ;
#50332 = VERTEX_POINT ( 'NONE', #167749 ) ;
#50333 = ORIENTED_EDGE ( 'NONE', *, *, #133464, .T. ) ;
#50334 = CARTESIAN_POINT ( 'NONE',  ( -16.94165728009537020, 51.64084748583298534, -231.8951239911713174 ) ) ;
#50335 = CARTESIAN_POINT ( 'NONE',  ( -23.25000000000000000, 76.10085836911045476, -81.27267460801371612 ) ) ;
#50336 = VERTEX_POINT ( 'NONE', #208152 ) ;
#50337 = CARTESIAN_POINT ( 'NONE',  ( 20.94560253601876809, 64.25000000001146816, -43.01302397200912964 ) ) ;
#50338 = CARTESIAN_POINT ( 'NONE',  ( 21.05000000000000071, 69.35000000001262777, -193.5060803140843859 ) ) ;
#50339 = ADVANCED_FACE ( 'NONE', ( #103869 ), #148152, .F. ) ;
#50340 = ORIENTED_EDGE ( 'NONE', *, *, #153064, .T. ) ;
#50341 = CARTESIAN_POINT ( 'NONE',  ( 23.14999999999998437, 80.05000000001165006, -69.52310748452430289 ) ) ;
#50342 = VERTEX_POINT ( 'NONE', #128600 ) ;
#50343 = DIRECTION ( 'NONE',  ( -1.000000000000000000, 0.000000000000000000, 0.000000000000000000 ) ) ;
#50344 = CARTESIAN_POINT ( 'NONE',  ( 21.30000000000002558, 40.35498466150055918, -247.8953732508333587 ) ) ;
#50345 = AXIS2_PLACEMENT_3D ( 'NONE', #46149, #68296, #233478 ) ;
#50347 = VERTEX_POINT ( 'NONE', #188564 ) ;
#50346 = DIRECTION ( 'NONE',  ( 0.000000000000000000, -0.9126074666063545004, -0.4088369013363783999 ) ) ;
#50348 = SPHERICAL_SURFACE ( 'NONE', #223895, 0.1000000000000000056 ) ;
#50350 = LINE ( 'NONE', #29566, #153702 ) ;
#50349 = UNCERTAINTY_MEASURE_WITH_UNIT (LENGTH_MEASURE( 1.000000000000000082E-05 ), #161166, 'distance_accuracy_value', 'NONE');
#50351 = DIRECTION ( 'NONE',  ( 0.000000000000000000, -0.4088369013363281623, 0.9126074666063771490 ) ) ;
#50352 = CARTESIAN_POINT ( 'NONE',  ( -16.85722902420150504, 66.05000000001230376, -157.2575600107541050 ) ) ;
#50353 = CARTESIAN_POINT ( 'NONE',  ( -16.78055652883087134, 66.05322308388724650, -190.8623156469320179 ) ) ;
#50354 = VECTOR ( 'NONE', #98668, 1000.000000000000000 ) ;
#50355 = CARTESIAN_POINT ( 'NONE',  ( -20.64999999999999858, 2.000000000011154189, -53.77537807723790309 ) ) ;
#50356 = DIRECTION ( 'NONE',  ( 0.000000000000000000, -6.982962677686266711E-15, 1.000000000000000000 ) ) ;
#50358 = ORIENTED_EDGE ( 'NONE', *, *, #152381, .T. ) ;
#50357 = CARTESIAN_POINT ( 'NONE',  ( 23.24999999999999289, 11.65000000001116298, -160.4851942293460922 ) ) ;
#50359 = ORIENTED_EDGE ( 'NONE', *, *, #94742, .T. ) ;
#50361 = CARTESIAN_POINT ( 'NONE',  ( -12.48127053791145258, 9.376580978055097049, -84.62694624701198620 ) ) ;
#50360 = FACE_OUTER_BOUND ( 'NONE', #99781, .T. ) ;
#50362 = B_SPLINE_CURVE_WITH_KNOTS ( 'NONE', 3,
 ( #103340, #87631, #124225, #83755, #244140, #128068, #66807, #107205 ),
 .UNSPECIFIED., .F., .F.,
 ( 4, 2, 2, 4 ),
 ( 0.000000000000000000, 0.0002181133598168996678, 0.0003271700397253495289, 0.0004362267196337993357 ),
 .UNSPECIFIED. ) ;
#50364 = EDGE_LOOP ( 'NONE', ( #38056, #202097, #109521, #34394 ) ) ;
#50363 = DIRECTION ( 'NONE',  ( 1.000000000000000000, 0.000000000000000000, 0.000000000000000000 ) ) ;
#50365 = TOROIDAL_SURFACE ( 'NONE', #166956, 0.9750000000000019762, 0.1000000000000000056 ) ;
#50366 = ORIENTED_EDGE ( 'NONE', *, *, #53445, .T. ) ;
#50367 = CARTESIAN_POINT ( 'NONE',  ( -20.64999999999999858, 68.85000000001222986, -148.7731074845244166 ) ) ;
#50368 = CARTESIAN_POINT ( 'NONE',  ( 20.97239005616515684, 67.12515615866173846, -90.77295468237119280 ) ) ;
#50369 = DIRECTION ( 'NONE',  ( 1.000000000000000000, 0.000000000000000000, 0.000000000000000000 ) ) ;
#50370 = TOROIDAL_SURFACE ( 'NONE', #54487, 0.2000000000000000111, 0.1000000000000000056 ) ;
#50371 = CARTESIAN_POINT ( 'NONE',  ( -20.94983749550516450, 10.29766095125295244, -172.9743663933275855 ) ) ;
#50372 = DIRECTION ( 'NONE',  ( 1.000000000000000000, 7.304098846218133681E-16, 5.311601492717083645E-30 ) ) ;
#50373 = DIRECTION ( 'NONE',  ( 0.000000000000000000, 0.8814952561688438326, -0.4721928772777330696 ) ) ;
#50374 = ADVANCED_FACE ( 'NONE', ( #83011 ), #137177, .T. ) ;
#50375 = FACE_OUTER_BOUND ( 'NONE', #236672, .T. ) ;
#50376 = ORIENTED_EDGE ( 'NONE', *, *, #49447, .F. ) ;
#50377 = VERTEX_POINT ( 'NONE', #63473 ) ;
#50378 = CARTESIAN_POINT ( 'NONE',  ( 23.14999999999998792, 11.65000000000000036, 0.000000000000000000 ) ) ;
#50379 = CIRCLE ( 'NONE', #83689, 0.09999999999999939493 ) ;
#50380 = ORIENTED_EDGE ( 'NONE', *, *, #53819, .F. ) ;
#50381 = CARTESIAN_POINT ( 'NONE',  ( -20.94999999999999929, -11.64999999998884483, -200.9999999999999432 ) ) ;
#50383 = ORIENTED_EDGE ( 'NONE', *, *, #53963, .T. ) ;
#50382 = VECTOR ( 'NONE', #75753, 1000.000000000000000 ) ;
#50384 = DIRECTION ( 'NONE',  ( 0.000000000000000000, 6.982962677686266711E-15, -1.000000000000000000 ) ) ;
#50385 = CIRCLE ( 'NONE', #104373, 0.1000000000000028644 ) ;
#50386 = CIRCLE ( 'NONE', #246055, 0.09999999999999990841 ) ;
#50387 = LINE ( 'NONE', #248615, #1222 ) ;
#50388 = EDGE_CURVE ( 'NONE', #82237, #59204, #252372, .T. ) ;
#50389 = FACE_OUTER_BOUND ( 'NONE', #64470, .T. ) ;
#50390 = ORIENTED_EDGE ( 'NONE', *, *, #69148, .T. ) ;
#50391 = CIRCLE ( 'NONE', #216999, 11.75000000000000000 ) ;
#50393 = CIRCLE ( 'NONE', #83703, 0.1000000000000028644 ) ;
#50392 = DIRECTION ( 'NONE',  ( 1.000000000000000000, -1.476360405086644309E-16, 0.000000000000000000 ) ) ;
#50394 = ORIENTED_EDGE ( 'NONE', *, *, #50584, .T. ) ;
#50395 = ADVANCED_FACE ( 'NONE', ( #249830 ), #153339, .T. ) ;
#50396 = DIRECTION ( 'NONE',  ( 0.000000000000000000, 0.000000000000000000, 1.000000000000000000 ) ) ;
#50397 = CARTESIAN_POINT ( 'NONE',  ( 21.05000000000000071, 8.776282895303630482, -109.0586289951409924 ) ) ;
#50398 = ORIENTED_EDGE ( 'NONE', *, *, #145404, .T. ) ;
#50399 = LINE ( 'NONE', #109103, #169320 ) ;
#50400 = ADVANCED_FACE ( 'NONE', ( #51587 ), #231556, .F. ) ;
#50401 = ORIENTED_EDGE ( 'NONE', *, *, #150216, .F. ) ;
#50404 = ORIENTED_EDGE ( 'NONE', *, *, #221842, .T. ) ;
#50403 = CARTESIAN_POINT ( 'NONE',  ( 18.50211644919735221, 46.36250628750310909, -243.0620573837409779 ) ) ;
#50402 = CARTESIAN_POINT ( 'NONE',  ( 20.85000000000000142, 76.00000000001170974, -69.52310748452431710 ) ) ;
#50405 = AXIS2_PLACEMENT_3D ( 'NONE', #174144, #90699, #170296 ) ;
#50406 = CARTESIAN_POINT ( 'NONE',  ( -21.52071067811865746, 68.22071067813071465, -124.1731074845243512 ) ) ;
#50407 = AXIS2_PLACEMENT_3D ( 'NONE', #35380, #79577, #194438 ) ;
#50409 = ORIENTED_EDGE ( 'NONE', *, *, #257819, .F. ) ;
#50408 = CIRCLE ( 'NONE', #21420, 11.69999999999999396 ) ;
#50410 = TOROIDAL_SURFACE ( 'NONE', #192118, 0.6000000000000004219, 0.1000000000000000056 ) ;
#50411 = DIRECTION ( 'NONE',  ( -1.000000000000000000, 2.952720810173289112E-16, 2.061873921506763405E-30 ) ) ;
#50412 = ORIENTED_EDGE ( 'NONE', *, *, #72617, .T. ) ;
#50413 = DIRECTION ( 'NONE',  ( 1.000000000000000000, 0.000000000000000000, 0.000000000000000000 ) ) ;
#50414 = CARTESIAN_POINT ( 'NONE',  ( 21.05000000000000071, 18.81018314204461817, -229.8995852278561642 ) ) ;
#50415 = EDGE_CURVE ( 'NONE', #196072, #182596, #24786, .T. ) ;
#50416 = CARTESIAN_POINT ( 'NONE',  ( -18.59999999999999787, 74.83729825007462466, -195.4231074845243654 ) ) ;
#50417 = CARTESIAN_POINT ( 'NONE',  ( -21.14999999999994174, 83.80000000001119531, -37.18565239344504647 ) ) ;
#50418 = CARTESIAN_POINT ( 'NONE',  ( -16.86445178670652467, 66.03778837089606668, -123.9138849226416568 ) ) ;
#50419 = AXIS2_PLACEMENT_3D ( 'NONE', #190343, #131632, #135469 ) ;
#50420 = ADVANCED_FACE ( 'NONE', ( #9929 ), #2223, .T. ) ;
#50421 = EDGE_LOOP ( 'NONE', ( #217848, #147207, #89159, #75857 ) ) ;
#50422 = CYLINDRICAL_SURFACE ( 'NONE', #102794, 0.09999999999999939493 ) ;
#50423 = CARTESIAN_POINT ( 'NONE',  ( 18.50596464788227280, 10.30632246271648889, -139.5041836778896425 ) ) ;
#50424 = ORIENTED_EDGE ( 'NONE', *, *, #99782, .F. ) ;
#50425 = DIRECTION ( 'NONE',  ( 0.000000000000000000, 0.000000000000000000, 1.000000000000000000 ) ) ;
#50426 = ORIENTED_EDGE ( 'NONE', *, *, #46787, .T. ) ;
#50427 = DIRECTION ( 'NONE',  ( 0.000000000000000000, -6.467318590049456648E-15, 1.000000000000000000 ) ) ;
#50428 = ORIENTED_EDGE ( 'NONE', *, *, #85563, .F. ) ;
#50429 = DIRECTION ( 'NONE',  ( 4.336808689942128177E-15, 0.8660254037844330455, -0.5000000000000096589 ) ) ;
#50430 = LINE ( 'NONE', #251207, #51915 ) ;
#50432 = ORIENTED_EDGE ( 'NONE', *, *, #214466, .T. ) ;
#50431 = CARTESIAN_POINT ( 'NONE',  ( 18.52928932188133970, 10.27928932189249878, -58.20857864376269930 ) ) ;
#50433 = FACE_OUTER_BOUND ( 'NONE', #187122, .T. ) ;
#50434 = ORIENTED_EDGE ( 'NONE', *, *, #252724, .F. ) ;
#50435 = CIRCLE ( 'NONE', #62938, 0.09999999999999971412 ) ;
#50436 = EDGE_CURVE ( 'NONE', #111358, #237092, #50316, .T. ) ;
#50437 = DIRECTION ( 'NONE',  ( 0.000000000000000000, 1.000000000000000000, 0.000000000000000000 ) ) ;
#50438 = CARTESIAN_POINT ( 'NONE',  ( -20.85000000000000142, 7.070967871809997973, -104.2465642218683541 ) ) ;
#50439 = EDGE_LOOP ( 'NONE', ( #217475, #235929, #190404, #97950 ) ) ;
#50440 = CARTESIAN_POINT ( 'NONE',  ( -2.995603634470891112E-16, 87.75000000001156764, -57.27310748452423894 ) ) ;
#50441 = LINE ( 'NONE', #187426, #235724 ) ;
#50442 = ORIENTED_EDGE ( 'NONE', *, *, #78351, .F. ) ;
#50443 = DIRECTION ( 'NONE',  ( 1.186688945009010077E-16, -1.000000000000000000, -0.000000000000000000 ) ) ;
#50444 = ORIENTED_EDGE ( 'NONE', *, *, #224934, .T. ) ;
#50445 = EDGE_CURVE ( 'NONE', #47498, #100761, #145542, .T. ) ;
#50447 = CARTESIAN_POINT ( 'NONE',  ( 15.57250062127604373, 9.370689921613767126, -118.0264651266610798 ) ) ;
#50446 = VECTOR ( 'NONE', #216039, 1000.000000000000000 ) ;
#50448 = DIRECTION ( 'NONE',  ( 1.000000000000000000, 0.000000000000000000, 0.000000000000000000 ) ) ;
#50449 = EDGE_CURVE ( 'NONE', #140091, #83237, #178912, .T. ) ;
#50452 = EDGE_LOOP ( 'NONE', ( #169785, #227032, #171685, #148168, #193428 ) ) ;
#50451 = VERTEX_POINT ( 'NONE', #12522 ) ;
#50450 = DIRECTION ( 'NONE',  ( 0.000000000000000000, 0.000000000000000000, -1.000000000000000000 ) ) ;
#50453 = CARTESIAN_POINT ( 'NONE',  ( -18.59999999999999787, 48.04585786805223080, -246.4610531646956417 ) ) ;
#50454 = DIRECTION ( 'NONE',  ( -1.000000000000000000, -0.000000000000000000, -0.000000000000000000 ) ) ;
#50455 = DIRECTION ( 'NONE',  ( 0.000000000000000000, -1.000000000000000000, 0.000000000000000000 ) ) ;
#50457 = CARTESIAN_POINT ( 'NONE',  ( -15.75000000000000355, 66.65000000001155911, -52.77310748452439526 ) ) ;
#50456 = DIRECTION ( 'NONE',  ( -0.000000000000000000, -0.000000000000000000, 1.000000000000000000 ) ) ;
#50459 = ADVANCED_FACE ( 'NONE', ( #92028 ), #171609, .T. ) ;
#50458 = DIRECTION ( 'NONE',  ( 0.000000000000000000, 0.000000000000000000, -1.000000000000000000 ) ) ;
#50460 = CARTESIAN_POINT ( 'NONE',  ( 18.59999999999999432, -1.866714910046153308, -145.7526752462820241 ) ) ;
#50461 = AXIS2_PLACEMENT_3D ( 'NONE', #66297, #224064, #166708 ) ;
#50462 = CARTESIAN_POINT ( 'NONE',  ( -20.94999999999999929, -1.736257131586239844, -78.56865232901753870 ) ) ;
#50463 = CARTESIAN_POINT ( 'NONE',  ( -21.05000000000000071, 76.00000000001247713, -174.0231074845243882 ) ) ;
#50465 = VERTEX_POINT ( 'NONE', #58019 ) ;
#50464 = VECTOR ( 'NONE', #41488, 1000.000000000000000 ) ;
#50466 = ORIENTED_EDGE ( 'NONE', *, *, #144014, .F. ) ;
#50467 = DIRECTION ( 'NONE',  ( 1.000000000000000000, 0.000000000000000000, 0.000000000000000000 ) ) ;
#50469 = ORIENTED_EDGE ( 'NONE', *, *, #253576, .F. ) ;
#50468 = CARTESIAN_POINT ( 'NONE',  ( 21.05000000000000071, 10.72371710471867701, -175.1649135690875880 ) ) ;
#50470 = ORIENTED_EDGE ( 'NONE', *, *, #117106, .F. ) ;
#50471 = CARTESIAN_POINT ( 'NONE',  ( -23.25000000000000000, -8.999999999988844479, -124.7060308773475867 ) ) ;
#50472 = EDGE_CURVE ( 'NONE', #169534, #152480, #16391, .T. ) ;
#50473 = VERTEX_POINT ( 'NONE', #163262 ) ;
#50474 = DIRECTION ( 'NONE',  ( 0.000000000000000000, -0.1575844902526579161, -0.9875055080513779338 ) ) ;
#50475 = ADVANCED_FACE ( 'NONE', ( #77580 ), #161990, .T. ) ;
#50476 = ADVANCED_FACE ( 'NONE', ( #16374, #137561, #164544 ), #38489, .F. ) ;
#50477 = EDGE_LOOP ( 'NONE', ( #52053, #20018, #185270, #21315 ) ) ;
#50478 = AXIS2_PLACEMENT_3D ( 'NONE', #224584, #223293, #186767 ) ;
#50479 = DIRECTION ( 'NONE',  ( 0.000000000000000000, 0.000000000000000000, -1.000000000000000000 ) ) ;
#50480 = DIRECTION ( 'NONE',  ( 0.000000000000000000, -0.9770955615653315052, -0.2128009952263607008 ) ) ;
#50482 = ORIENTED_EDGE ( 'NONE', *, *, #202366, .T. ) ;
#50481 = EDGE_LOOP ( 'NONE', ( #142133, #61938, #124676, #89845, #144966, #72186, #200143, #232018, #180418 ) ) ;
#50483 = ORIENTED_EDGE ( 'NONE', *, *, #62331, .F. ) ;
#50484 = VERTEX_POINT ( 'NONE', #136267 ) ;
#50485 = ORIENTED_EDGE ( 'NONE', *, *, #247532, .F. ) ;
#50486 = EDGE_CURVE ( 'NONE', #63323, #162761, #28905, .T. ) ;
#50487 = DIRECTION ( 'NONE',  ( -0.000000000000000000, -0.1350103645451876666, 0.9908441862701600211 ) ) ;
#50488 = LINE ( 'NONE', #153521, #153263 ) ;
#50489 = CARTESIAN_POINT ( 'NONE',  ( -12.42749937872396870, 9.370689921613765350, -185.0264651266610088 ) ) ;
#50491 = ORIENTED_EDGE ( 'NONE', *, *, #113275, .F. ) ;
#50490 = DIRECTION ( 'NONE',  ( 0.000000000000000000, 0.9126074666063844765, 0.4088369013363114535 ) ) ;
#50492 = CARTESIAN_POINT ( 'NONE',  ( 23.24999999999999645, 76.00000000001190870, -103.0231074845243029 ) ) ;
#50493 = EDGE_CURVE ( 'NONE', #252057, #198528, #56722, .T. ) ;
#50494 = CARTESIAN_POINT ( 'NONE',  ( 21.05000000000000071, 11.83110912403452097, -206.0549139711134785 ) ) ;
#50496 = ORIENTED_EDGE ( 'NONE', *, *, #54484, .T. ) ;
#50495 = DIRECTION ( 'NONE',  ( -1.000000000000000000, 0.000000000000000000, 0.000000000000000000 ) ) ;
#50497 = DIRECTION ( 'NONE',  ( 0.000000000000000000, -0.4088369013363280513, 0.9126074666063769270 ) ) ;
#50499 = ADVANCED_FACE ( 'NONE', ( #254898 ), #29069, .T. ) ;
#50498 = ORIENTED_EDGE ( 'NONE', *, *, #167446, .F. ) ;
#50500 = DIRECTION ( 'NONE',  ( 0.000000000000000000, 0.000000000000000000, -1.000000000000000000 ) ) ;
#50501 = ORIENTED_EDGE ( 'NONE', *, *, #159332, .T. ) ;
#50502 = CARTESIAN_POINT ( 'NONE',  ( 20.94999999999999929, 78.89331866122350334, -228.7665898296168052 ) ) ;
#50503 = VECTOR ( 'NONE', #48015, 1000.000000000000227 ) ;
#50504 = AXIS2_PLACEMENT_3D ( 'NONE', #29552, #9953, #149489 ) ;
#50505 = AXIS2_PLACEMENT_3D ( 'NONE', #188526, #88109, #108978 ) ;
#50506 = ORIENTED_EDGE ( 'NONE', *, *, #234695, .T. ) ;
#50508 = DIRECTION ( 'NONE',  ( 1.000000000000000000, 0.000000000000000000, 0.000000000000000000 ) ) ;
#50507 = CARTESIAN_POINT ( 'NONE',  ( -21.53752568622148900, 75.90102553874208979, -210.3099153590730168 ) ) ;
#50509 = CYLINDRICAL_SURFACE ( 'NONE', #189048, 0.5000000000000004441 ) ;
#50510 = DIRECTION ( 'NONE',  ( 0.000000000000000000, -1.000000000000000000, 0.000000000000000000 ) ) ;
#50511 = CARTESIAN_POINT ( 'NONE',  ( -20.64999999999999858, 73.60000000001224407, -149.7477294072864709 ) ) ;
#50512 = ORIENTED_EDGE ( 'NONE', *, *, #15550, .T. ) ;
#50513 = ORIENTED_EDGE ( 'NONE', *, *, #96556, .F. ) ;
#50514 = B_SPLINE_CURVE_WITH_KNOTS ( 'NONE', 3,
 ( #250816, #35666, #209123, #55156, #214273, #10946, #133446, #52618, #233836, #12241, #149181, #111323, #173907, #253390, #228716, #91754, #72208, #53912, #231282 ),
 .UNSPECIFIED., .F., .F.,
 ( 4, 3, 3, 3, 3, 3, 4 ),
 ( -2.000416914658646987E-06, 0.000000000000000000, 4.714008503743518199E-05, 9.979203887776679231E-05, 0.0001372215519229392155, 0.0001635031576220894356, 0.0001900083748504071714 ),
 .UNSPECIFIED. ) ;
#50515 = CARTESIAN_POINT ( 'NONE',  ( 23.14999999999999858, -1.999999999988846699, -167.5000000000000284 ) ) ;
#50516 = DIRECTION ( 'NONE',  ( -0.000000000000000000, -0.000000000000000000, -1.000000000000000000 ) ) ;
#50518 = ORIENTED_EDGE ( 'NONE', *, *, #128569, .F. ) ;
#50517 = EDGE_CURVE ( 'NONE', #15975, #91559, #62350, .T. ) ;
#50519 = CARTESIAN_POINT ( 'NONE',  ( 20.94999999999999929, 67.23127455305835554, -235.8551265064784559 ) ) ;
#50520 = ORIENTED_EDGE ( 'NONE', *, *, #112739, .F. ) ;
#50521 = EDGE_CURVE ( 'NONE', #162149, #86723, #70754, .T. ) ;
#50522 = CARTESIAN_POINT ( 'NONE',  ( -20.65000000000000568, 7.250000000011138646, -79.65000000000004832 ) ) ;
#50523 = CARTESIAN_POINT ( 'NONE',  ( -18.59999999999999787, 1.162701749949165642, -108.6000000000000227 ) ) ;
#50524 = AXIS2_PLACEMENT_3D ( 'NONE', #37507, #239548, #19212 ) ;
#50525 = DIRECTION ( 'NONE',  ( 1.000000000000000000, -2.986185139342070877E-16, 6.665775143889692774E-16 ) ) ;
#50527 = EDGE_CURVE ( 'NONE', #76552, #183460, #23771, .T. ) ;
#50526 = ORIENTED_EDGE ( 'NONE', *, *, #226283, .T. ) ;
#50528 = CARTESIAN_POINT ( 'NONE',  ( -16.81453046979149590, 66.06089771857169524, -190.8113809609214115 ) ) ;
#50529 = EDGE_LOOP ( 'NONE', ( #243298, #209635, #141306, #86480 ) ) ;
#50530 = ORIENTED_EDGE ( 'NONE', *, *, #254957, .F. ) ;
#50531 = ORIENTED_EDGE ( 'NONE', *, *, #138533, .F. ) ;
#50532 = DIRECTION ( 'NONE',  ( 0.5000000000001141309, 0.2266847461454224444, 0.8358313381686951482 ) ) ;
#50533 = DIRECTION ( 'NONE',  ( 1.000000000000000000, 0.000000000000000000, 0.000000000000000000 ) ) ;
#50534 = PLANE ( 'NONE',  #125957 ) ;
#50535 = DIRECTION ( 'NONE',  ( -0.000000000000000000, -6.982962677686266711E-15, 1.000000000000000000 ) ) ;
#50536 = DIRECTION ( 'NONE',  ( 1.000000000000000000, 0.000000000000000000, 0.000000000000000000 ) ) ;
#50537 = AXIS2_PLACEMENT_3D ( 'NONE', #170662, #71533, #51914 ) ;
#50539 = CARTESIAN_POINT ( 'NONE',  ( -21.53752568622130070, 0.09897446127749365274, -160.7131921254514282 ) ) ;
#50538 = CARTESIAN_POINT ( 'NONE',  ( -21.46681500593518876, 10.36690126540584700, -227.6878377563191691 ) ) ;
#50541 = ORIENTED_EDGE ( 'NONE', *, *, #250232, .F. ) ;
#50540 = CYLINDRICAL_SURFACE ( 'NONE', #131321, 0.1000000000000124678 ) ;
#50542 = CARTESIAN_POINT ( 'NONE',  ( -21.07928932188134041, 10.02993822722303818, -228.1074463178677263 ) ) ;
#50543 = ORIENTED_EDGE ( 'NONE', *, *, #68219, .T. ) ;
#50544 = DIRECTION ( 'NONE',  ( 0.000000000000000000, -0.1350103645451945777, 0.9908441862701590219 ) ) ;
#50545 = ORIENTED_EDGE ( 'NONE', *, *, #104602, .T. ) ;
#50546 = EDGE_LOOP ( 'NONE', ( #177204, #12424, #69498, #66159 ) ) ;
#50547 = LINE ( 'NONE', #109252, #83768 ) ;
#50548 = CIRCLE ( 'NONE', #33869, 11.89999999999998970 ) ;
#50549 = CARTESIAN_POINT ( 'NONE',  ( -23.25000000000000000, 52.81534179157633702, -244.1198638051726277 ) ) ;
#50551 = EDGE_CURVE ( 'NONE', #238502, #187182, #223206, .T. ) ;
#50550 = CARTESIAN_POINT ( 'NONE',  ( -16.90128866880176162, 66.04620422280855507, -48.66043130113575188 ) ) ;
#50552 = FACE_OUTER_BOUND ( 'NONE', #72286, .T. ) ;
#50553 = AXIS2_PLACEMENT_3D ( 'NONE', #224879, #43696, #223589 ) ;
#50554 = EDGE_CURVE ( 'NONE', #84058, #192064, #195653, .T. ) ;
#50555 = CARTESIAN_POINT ( 'NONE',  ( 18.49999999999999289, 11.65000000001115943, -91.85000000000003695 ) ) ;
#50556 = TOROIDAL_SURFACE ( 'NONE', #75546, 3.899999999999999467, 0.1000000000000000056 ) ;
#50557 = ORIENTED_EDGE ( 'NONE', *, *, #138834, .T. ) ;
#50558 = ORIENTED_EDGE ( 'NONE', *, *, #97876, .F. ) ;
#50560 = ADVANCED_FACE ( 'NONE', ( #104522 ), #208118, .T. ) ;
#50559 = DIRECTION ( 'NONE',  ( -1.000000000000000000, 0.000000000000000000, 0.000000000000000000 ) ) ;
#50561 = VERTEX_POINT ( 'NONE', #244055 ) ;
#50562 = DIRECTION ( 'NONE',  ( 0.000000000000000000, -1.000000000000000000, 0.000000000000000000 ) ) ;
#50563 = CARTESIAN_POINT ( 'NONE',  ( -23.15000000000000213, 1.115600667400684642E-11, -146.7750000000000057 ) ) ;
#50564 = ORIENTED_EDGE ( 'NONE', *, *, #31813, .F. ) ;
#50565 = LINE ( 'NONE', #11480, #227960 ) ;
#50566 = CARTESIAN_POINT ( 'NONE',  ( 18.59999999999998366, 1.115600667400684642E-11, -167.5000000000000284 ) ) ;
#50567 = DIRECTION ( 'NONE',  ( -1.000000000000000000, 0.000000000000000000, 0.000000000000000000 ) ) ;
#50568 = CARTESIAN_POINT ( 'NONE',  ( 20.95512820512820440, 65.37615131630040821, -157.8731074845244393 ) ) ;
#50569 = ORIENTED_EDGE ( 'NONE', *, *, #172116, .F. ) ;
#50570 = SPHERICAL_SURFACE ( 'NONE', #83544, 0.1000000000000000056 ) ;
#50571 = EDGE_CURVE ( 'NONE', #74153, #34034, #22025, .T. ) ;
#50573 = DIRECTION ( 'NONE',  ( -1.000000000000000000, -7.304098846218133681E-16, 4.217023435051677994E-16 ) ) ;
#50572 = AXIS2_PLACEMENT_3D ( 'NONE', #42208, #180431, #3052 ) ;
#50574 = FACE_OUTER_BOUND ( 'NONE', #155093, .T. ) ;
#50575 = DIRECTION ( 'NONE',  ( -0.000000000000000000, -0.000000000000000000, 1.000000000000000000 ) ) ;
#50577 = EDGE_CURVE ( 'NONE', #217587, #75011, #91573, .T. ) ;
#50576 = CARTESIAN_POINT ( 'NONE',  ( -20.54999999999999716, 7.128833340093095217, -233.7327013124392749 ) ) ;
#50578 = AXIS2_PLACEMENT_3D ( 'NONE', #233223, #89818, #72876 ) ;
#50579 = CARTESIAN_POINT ( 'NONE',  ( 21.05000000000000071, 76.00000000001195133, -103.0231074845243171 ) ) ;
#50580 = VECTOR ( 'NONE', #91145, 1000.000000000000114 ) ;
#50581 = EDGE_CURVE ( 'NONE', #16250, #3179, #128999, .T. ) ;
#50582 = ORIENTED_EDGE ( 'NONE', *, *, #54612, .T. ) ;
#50584 = EDGE_CURVE ( 'NONE', #191153, #147896, #199919, .T. ) ;
#50583 = EDGE_CURVE ( 'NONE', #177267, #166644, #16579, .T. ) ;
#50585 = AXIS2_PLACEMENT_3D ( 'NONE', #154142, #13312, #111118 ) ;
#50586 = CARTESIAN_POINT ( 'NONE',  ( -17.05016517655713670, 66.05000000001231797, -157.3504094885308007 ) ) ;
#50587 = VERTEX_POINT ( 'NONE', #186676 ) ;
#50588 = CARTESIAN_POINT ( 'NONE',  ( 15.70340296795548873, 66.64411154550971617, -153.7344645877463734 ) ) ;
#50589 = CIRCLE ( 'NONE', #138080, 0.5000000000000013323 ) ;
#50590 = DIRECTION ( 'NONE',  ( 1.000000000000000000, -7.304098846218134667E-16, -5.100424963727256530E-30 ) ) ;
#50591 = CARTESIAN_POINT ( 'NONE',  ( -23.15000000000000213, 68.31754949648690456, -231.8498166873408763 ) ) ;
#50592 = DIRECTION ( 'NONE',  ( -1.000000000000000000, -3.265361837132813093E-16, 0.000000000000000000 ) ) ;
#50593 = CARTESIAN_POINT ( 'NONE',  ( 20.86036036209897304, 65.37895722344136118, -162.3567590660221924 ) ) ;
#50594 = ORIENTED_EDGE ( 'NONE', *, *, #81127, .F. ) ;
#50595 = LINE ( 'NONE', #207134, #204959 ) ;
#50596 = CARTESIAN_POINT ( 'NONE',  ( 23.14999999999999858, 76.00000000001244871, -170.0231074845243597 ) ) ;
#50597 = DIRECTION ( 'NONE',  ( 1.000000000000000000, -0.000000000000000000, -0.000000000000000000 ) ) ;
#50598 = CARTESIAN_POINT ( 'NONE',  ( -21.05000000000000071, 1.162701749949165642, -175.5999999999999659 ) ) ;
#50599 = CIRCLE ( 'NONE', #246260, 0.1000000000000004774 ) ;
#50600 = EDGE_CURVE ( 'NONE', #192664, #140683, #116519, .T. ) ;
#50601 = EDGE_CURVE ( 'NONE', #8175, #246385, #146237, .T. ) ;
#50602 = VECTOR ( 'NONE', #58627, 1000.000000000000000 ) ;
#50603 = CARTESIAN_POINT ( 'NONE',  ( 20.94999999999999929, 74.16465844978787914, -158.4679561919613775 ) ) ;
#50604 = CIRCLE ( 'NONE', #125627, 0.5000000000000004441 ) ;
#50605 = ORIENTED_EDGE ( 'NONE', *, *, #50610, .F. ) ;
#50606 = ORIENTED_EDGE ( 'NONE', *, *, #87451, .F. ) ;
#50607 = DIRECTION ( 'NONE',  ( 1.000000000000000000, 0.000000000000000000, 0.000000000000000000 ) ) ;
#50608 = CARTESIAN_POINT ( 'NONE',  ( -20.99105743725316842, 6.322468215188231433, 12.11686199560448252 ) ) ;
#50610 = EDGE_CURVE ( 'NONE', #217324, #228701, #47122, .T. ) ;
#50609 = CARTESIAN_POINT ( 'NONE',  ( 20.85000000000000142, 6.982009704867603972, -137.6961521182563217 ) ) ;
#50611 = CARTESIAN_POINT ( 'NONE',  ( -22.00411653962159875, 68.74655713164217730, -170.1221455902930302 ) ) ;
#50612 = ORIENTED_EDGE ( 'NONE', *, *, #26350, .F. ) ;
#50614 = EDGE_CURVE ( 'NONE', #142859, #25020, #145712, .T. ) ;
#50613 = LINE ( 'NONE', #225398, #84765 ) ;
#50615 = ITEM_DEFINED_TRANSFORMATION ( 'NONE', 'NONE', #23681,  #2425 ) ;
#50616 = EDGE_CURVE ( 'NONE', #233607, #25295, #141449, .T. ) ;
#50617 = CARTESIAN_POINT ( 'NONE',  ( 11.60000000000006004, 64.35000000001120668, -18.42310748452479530 ) ) ;
#50618 = ORIENTED_EDGE ( 'NONE', *, *, #164980, .F. ) ;
#50619 = DIRECTION ( 'NONE',  ( -1.000000000000000000, 0.000000000000000000, 0.000000000000000000 ) ) ;
#50620 = ORIENTED_EDGE ( 'NONE', *, *, #69375, .T. ) ;
#50621 = ORIENTED_EDGE ( 'NONE', *, *, #186473, .F. ) ;
#50622 = VERTEX_POINT ( 'NONE', #245363 ) ;
#50623 = EDGE_CURVE ( 'NONE', #204844, #224804, #224835, .T. ) ;
#50624 = CARTESIAN_POINT ( 'NONE',  ( -20.54999999999999716, 2.400000000011155432, -46.72462192276210402 ) ) ;
#50625 = CARTESIAN_POINT ( 'NONE',  ( 23.14999999999999858, 1.115600667400684642E-11, -33.50000000000000000 ) ) ;
#50626 = CARTESIAN_POINT ( 'NONE',  ( 23.14999999999999858, 76.00000000001126921, -203.5231074845248997 ) ) ;
#50627 = VECTOR ( 'NONE', #206667, 1000.000000000000000 ) ;
#50628 = CARTESIAN_POINT ( 'NONE',  ( 18.42636655943170965, -9.496944315759476396, -140.6090805711555731 ) ) ;
#50629 = DIRECTION ( 'NONE',  ( 0.000000000000000000, -5.956132106358139644E-15, 1.000000000000000000 ) ) ;
#50630 = DIRECTION ( 'NONE',  ( -0.000000000000000000, -0.000000000000000000, -1.000000000000000000 ) ) ;
#50631 = CARTESIAN_POINT ( 'NONE',  ( -15.75000000000000355, 26.30888228346803004, -233.3999513616626587 ) ) ;
#50633 = CYLINDRICAL_SURFACE ( 'NONE', #62184, 7.899999999999995914 ) ;
#50632 = DIRECTION ( 'NONE',  ( 2.168404344971008868E-16, -0.000000000000000000, 1.000000000000000000 ) ) ;
#50634 = ADVANCED_FACE ( 'NONE', ( #225765 ), #126689, .F. ) ;
#50635 = CARTESIAN_POINT ( 'NONE',  ( 21.04999999999999716, -1.448506596209664377, -194.7513623756925085 ) ) ;
#50636 = DIRECTION ( 'NONE',  ( 1.000000000000000000, 0.000000000000000000, 0.000000000000000000 ) ) ;
#50637 = DIRECTION ( 'NONE',  ( 0.000000000000000000, 0.9126074666063774821, 0.4088369013363273297 ) ) ;
#50638 = CARTESIAN_POINT ( 'NONE',  ( -23.25000000000000000, 28.42524210734032053, -258.3567845160494585 ) ) ;
#50639 = VERTEX_POINT ( 'NONE', #48424 ) ;
#50640 = ORIENTED_EDGE ( 'NONE', *, *, #41756, .T. ) ;
#50641 = CYLINDRICAL_SURFACE ( 'NONE', #190352, 0.1000000000000055844 ) ;
#50642 = CARTESIAN_POINT ( 'NONE',  ( 23.15000000000000213, -8.999999999988842703, -124.1060308773475924 ) ) ;
#50643 = DIRECTION ( 'NONE',  ( 0.000000000000000000, 0.1335171055202901413, -0.9910465087640860649 ) ) ;
#50644 = CIRCLE ( 'NONE', #225431, 0.09999999999999105438 ) ;
#50645 = CARTESIAN_POINT ( 'NONE',  ( 19.90000000000000568, 1.350000000000000089, 16.50000000000000000 ) ) ;
#50646 = LINE ( 'NONE', #217419, #83512 ) ;
#50647 = ADVANCED_FACE ( 'NONE', ( #27627 ), #69298, .T. ) ;
#50648 = DIRECTION ( 'NONE',  ( 0.000000000000000000, 0.000000000000000000, -1.000000000000000000 ) ) ;
#50649 = EDGE_LOOP ( 'NONE', ( #127073, #22998, #28770, #125222, #20350, #119768 ) ) ;
#50650 = ORIENTED_EDGE ( 'NONE', *, *, #96220, .T. ) ;
#50651 = DIRECTION ( 'NONE',  ( 1.000000000000000000, 0.000000000000000000, 0.000000000000000000 ) ) ;
#50652 = ORIENTED_EDGE ( 'NONE', *, *, #66552, .F. ) ;
#50653 = DIRECTION ( 'NONE',  ( 1.000000000000000000, 0.000000000000000000, 0.000000000000000000 ) ) ;
#50654 = CIRCLE ( 'NONE', #83945, 3.900000000000000799 ) ;
#50655 = EDGE_CURVE ( 'NONE', #219183, #171414, #49717, .T. ) ;
#50656 = CIRCLE ( 'NONE', #142259, 4.150000000000001243 ) ;
#50657 = CIRCLE ( 'NONE', #129781, 0.1000000000000028644 ) ;
#50658 = ORIENTED_EDGE ( 'NONE', *, *, #96906, .T. ) ;
#50659 = CARTESIAN_POINT ( 'NONE',  ( 18.59999999999999076, 65.50857864377465489, -111.7731074845243739 ) ) ;
#50660 = VERTEX_POINT ( 'NONE', #171001 ) ;
#50661 = CARTESIAN_POINT ( 'NONE',  ( -17.71734398241073905, 10.84235722846456085, -10.27486174699440724 ) ) ;
#50662 = CYLINDRICAL_SURFACE ( 'NONE', #24603, 0.1000000000000028644 ) ;
#50663 = DIRECTION ( 'NONE',  ( 0.000000000000000000, -0.000000000000000000, -1.000000000000000000 ) ) ;
#50664 = CARTESIAN_POINT ( 'NONE',  ( 18.54147908293624170, -9.463261657917028558, -141.0489488967557179 ) ) ;
#50665 = CARTESIAN_POINT ( 'NONE',  ( 23.14999999999998437, 76.00000000001195133, -103.0231074845243171 ) ) ;
#50666 = DIRECTION ( 'NONE',  ( 1.000000000000000000, 0.000000000000000000, 0.000000000000000000 ) ) ;
#50667 = CIRCLE ( 'NONE', #196426, 0.5000000000000004441 ) ;
#50668 = DIRECTION ( 'NONE',  ( 1.000000000000000000, 0.000000000000000000, 0.000000000000000000 ) ) ;
#50669 = DIRECTION ( 'NONE',  ( 0.000000000000000000, -0.2617529984165152257, -0.9651348961777124202 ) ) ;
#50671 = VERTEX_POINT ( 'NONE', #127979 ) ;
#50670 = CARTESIAN_POINT ( 'NONE',  ( -23.15000000000000213, 47.48953316408024961, -242.5895867826444601 ) ) ;
#50673 = CARTESIAN_POINT ( 'NONE',  ( -23.25000000000000000, 69.06610602788607878, -166.2374616501508342 ) ) ;
#50672 = CARTESIAN_POINT ( 'NONE',  ( -22.50000000000000000, 1.115600667400684642E-11, -67.00000000000004263 ) ) ;
#50674 = ORIENTED_EDGE ( 'NONE', *, *, #206794, .F. ) ;
#50676 = ORIENTED_EDGE ( 'NONE', *, *, #18207, .T. ) ;
#50675 = CARTESIAN_POINT ( 'NONE',  ( 18.49999999999998934, 69.45000000001188312, -93.00608031408432907 ) ) ;
#50677 = ORIENTED_EDGE ( 'NONE', *, *, #11175, .F. ) ;
#50678 = CARTESIAN_POINT ( 'NONE',  ( 21.05315837483509966, 62.86884413562100349, -207.0506191170989041 ) ) ;
#50679 = CARTESIAN_POINT ( 'NONE',  ( -22.59999999999999432, 11.46682355977092804, -198.4356847424421062 ) ) ;
#50680 = DIRECTION ( 'NONE',  ( -0.000000000000000000, -1.000000000000000000, 6.308085367188393199E-16 ) ) ;
#50681 = CARTESIAN_POINT ( 'NONE',  ( 18.49999999999999645, 1.115600667400684642E-11, -167.4999999999999716 ) ) ;
#50682 = CARTESIAN_POINT ( 'NONE',  ( -22.47071067811865319, 7.720074744509219933, -167.4009075452973434 ) ) ;
#50683 = DIRECTION ( 'NONE',  ( 1.000000000000000000, 0.000000000000000000, 0.000000000000000000 ) ) ;
#50684 = VECTOR ( 'NONE', #216822, 999.9999999999998863 ) ;
#50686 = EDGE_CURVE ( 'NONE', #137320, #113073, #33353, .T. ) ;
#50685 = CIRCLE ( 'NONE', #225659, 0.5999999999999894307 ) ;
#50687 = CARTESIAN_POINT ( 'NONE',  ( 21.05000000000000071, 53.70241689174373079, -235.9987767062293074 ) ) ;
#50688 = ORIENTED_EDGE ( 'NONE', *, *, #61213, .F. ) ;
#50689 = ORIENTED_EDGE ( 'NONE', *, *, #316, .T. ) ;
#50690 = DIRECTION ( 'NONE',  ( -1.000000000000000000, 0.000000000000000000, 0.000000000000000000 ) ) ;
#50691 = ORIENTED_EDGE ( 'NONE', *, *, #189221, .T. ) ;
#50692 = DIRECTION ( 'NONE',  ( 0.000000000000000000, -7.116814260417668513E-15, 1.000000000000000000 ) ) ;
#50693 = ORIENTED_EDGE ( 'NONE', *, *, #247018, .F. ) ;
#50694 = CARTESIAN_POINT ( 'NONE',  ( 22.48660254037844197, 11.65000000001116298, -33.45000000000000995 ) ) ;
#50695 = FACE_OUTER_BOUND ( 'NONE', #177925, .T. ) ;
#50696 = CARTESIAN_POINT ( 'NONE',  ( -20.64999999999999858, -9.499999999988846255, -57.10603087734755690 ) ) ;
#50697 = ADVANCED_FACE ( 'NONE', ( #228364 ), #90107, .T. ) ;
#50698 = CARTESIAN_POINT ( 'NONE',  ( -20.54999999999999716, 85.00000000001197975, -112.9170766071766820 ) ) ;
#50699 = DIRECTION ( 'NONE',  ( 0.000000000000000000, -6.982962677686266711E-15, 1.000000000000000000 ) ) ;
#50700 = VERTEX_POINT ( 'NONE', #229642 ) ;
#50701 = AXIS2_PLACEMENT_3D ( 'NONE', #154594, #234086, #55424 ) ;
#50702 = ADVANCED_FACE ( 'NONE', ( #50970 ), #130530, .T. ) ;
#50703 = DIRECTION ( 'NONE',  ( 1.000000000000000000, 3.265361837132813093E-16, -0.000000000000000000 ) ) ;
#50704 = CYLINDRICAL_SURFACE ( 'NONE', #131305, 0.09999999999999939493 ) ;
#50705 = CARTESIAN_POINT ( 'NONE',  ( -23.25000000000000000, 74.00000000001199396, -115.6477294072864055 ) ) ;
#50706 = DIRECTION ( 'NONE',  ( 0.000000000000000000, 0.2617529984165028467, 0.9651348961777159730 ) ) ;
#50707 = CARTESIAN_POINT ( 'NONE',  ( -23.25000000000000000, 68.56901367119438362, -214.3038979092079046 ) ) ;
#50708 = ORIENTED_EDGE ( 'NONE', *, *, #257599, .T. ) ;
#50710 = FACE_OUTER_BOUND ( 'NONE', #114997, .T. ) ;
#50709 = CARTESIAN_POINT ( 'NONE',  ( 21.05000000000000071, 71.18691588786198565, -47.96462524104817504 ) ) ;
#50711 = ADVANCED_FACE ( 'NONE', ( #110977 ), #166609, .F. ) ;
#50712 = ORIENTED_EDGE ( 'NONE', *, *, #67140, .F. ) ;
#50715 = ORIENTED_EDGE ( 'NONE', *, *, #121240, .F. ) ;
#50714 = CARTESIAN_POINT ( 'NONE',  ( 20.95443524775735256, 67.12144573613950627, -161.4893852089242898 ) ) ;
#50713 = CARTESIAN_POINT ( 'NONE',  ( -21.07928932188134041, 7.128833340093095217, -233.7327013124392749 ) ) ;
#50716 = DIRECTION ( 'NONE',  ( 1.000000000000000000, -0.000000000000000000, -0.000000000000000000 ) ) ;
#50717 = LINE ( 'NONE', #130274, #152811 ) ;
#50718 = EDGE_CURVE ( 'NONE', #57106, #197965, #190538, .T. ) ;
#50719 = DIRECTION ( 'NONE',  ( -1.000000000000000000, 0.000000000000000000, 0.000000000000000000 ) ) ;
#50720 = ORIENTED_EDGE ( 'NONE', *, *, #182228, .F. ) ;
#50721 = FACE_OUTER_BOUND ( 'NONE', #2369, .T. ) ;
#50722 = EDGE_CURVE ( 'NONE', #185627, #63695, #179088, .T. ) ;
#50723 = VECTOR ( 'NONE', #117511, 1000.000000000000000 ) ;
#50724 = CARTESIAN_POINT ( 'NONE',  ( 21.05000000000000071, 87.19425987394825484, -209.6674621343692024 ) ) ;
#50725 = EDGE_CURVE ( 'NONE', #85846, #206700, #183167, .T. ) ;
#50727 = DIRECTION ( 'NONE',  ( 0.000000000000000000, 0.000000000000000000, -1.000000000000000000 ) ) ;
#50726 = CARTESIAN_POINT ( 'NONE',  ( -23.15000000000000213, 62.12148660976906456, -247.5636999539406133 ) ) ;
#50729 = ORIENTED_EDGE ( 'NONE', *, *, #204805, .F. ) ;
#50728 = DIRECTION ( 'NONE',  ( -1.000000000000000000, -0.000000000000000000, 0.000000000000000000 ) ) ;
#50730 = VECTOR ( 'NONE', #254217, 999.9999999999998863 ) ;
#50731 = EDGE_CURVE ( 'NONE', #163993, #185233, #17026, .T. ) ;
#50732 = ORIENTED_EDGE ( 'NONE', *, *, #125578, .F. ) ;
#50733 = AXIS2_PLACEMENT_3D ( 'NONE', #34001, #129213, #90064 ) ;
#50734 = DIRECTION ( 'NONE',  ( 1.000000000000000000, 0.000000000000000000, 0.000000000000000000 ) ) ;
#50735 = CARTESIAN_POINT ( 'NONE',  ( 20.94999999999999929, 1.835341550224413698, -11.55515129256298401 ) ) ;
#50736 = DIRECTION ( 'NONE',  ( 0.000000000000000000, 0.2211802418851555596, -0.9752329468386637945 ) ) ;
#50738 = ORIENTED_EDGE ( 'NONE', *, *, #177442, .T. ) ;
#50737 = VECTOR ( 'NONE', #190475, 1000.000000000000000 ) ;
#50739 = CARTESIAN_POINT ( 'NONE',  ( -23.15000000000000213, -5.011722593499801093, -233.2041167654973322 ) ) ;
#50740 = AXIS2_PLACEMENT_3D ( 'NONE', #94870, #33678, #256448 ) ;
#50741 = CARTESIAN_POINT ( 'NONE',  ( -21.55000000000000426, 65.35370752038342346, -213.3282663891675952 ) ) ;
#50742 = DIRECTION ( 'NONE',  ( 0.000000000000000000, 0.8814952561688476074, -0.4721928772777262417 ) ) ;
#50743 = EDGE_CURVE ( 'NONE', #245468, #13286, #36610, .T. ) ;
#50744 = ORIENTED_EDGE ( 'NONE', *, *, #169699, .T. ) ;
#50745 = CARTESIAN_POINT ( 'NONE',  ( 20.74897398619089017, 59.01508426811044927, -225.6701006227075368 ) ) ;
#50746 = EDGE_CURVE ( 'NONE', #42537, #103956, #173571, .T. ) ;
#50747 = AXIS2_PLACEMENT_3D ( 'NONE', #115360, #52811, #132361 ) ;
#50748 = VERTEX_POINT ( 'NONE', #116122 ) ;
#50749 = AXIS2_PLACEMENT_3D ( 'NONE', #94960, #175809, #76678 ) ;
#50750 = CARTESIAN_POINT ( 'NONE',  ( 23.24999999999999645, 9.273719881888197847, -221.1390486761779925 ) ) ;
#50751 = DIRECTION ( 'NONE',  ( 0.000000000000000000, 1.000000000000000000, 6.938893903907222067E-15 ) ) ;
#50752 = CIRCLE ( 'NONE', #117428, 6.258578643762710669 ) ;
#50753 = ORIENTED_EDGE ( 'NONE', *, *, #41242, .T. ) ;
#50754 = ORIENTED_EDGE ( 'NONE', *, *, #233309, .T. ) ;
#50755 = VECTOR ( 'NONE', #71487, 1000.000000000000000 ) ;
#50756 = EDGE_CURVE ( 'NONE', #66750, #155242, #216465, .T. ) ;
#50757 = DIRECTION ( 'NONE',  ( -1.652117596168391700E-15, -1.000000000000000000, 0.000000000000000000 ) ) ;
#50758 = B_SPLINE_CURVE_WITH_KNOTS ( 'NONE', 3,
 ( #166804, #49393, #145907, #225435, #128936, #165501, #88485 ),
 .UNSPECIFIED., .F., .F.,
 ( 4, 3, 4 ),
 ( 0.000000000000000000, 0.0009834301579440007414, 0.001767853679402678433 ),
 .UNSPECIFIED. ) ;
#50759 = ORIENTED_EDGE ( 'NONE', *, *, #174852, .F. ) ;
#50761 = ORIENTED_EDGE ( 'NONE', *, *, #251912, .T. ) ;
#50760 = LINE ( 'NONE', #146028, #246767 ) ;
#50762 = AXIS2_PLACEMENT_3D ( 'NONE', #1839, #65687, #81367 ) ;
#50763 = ORIENTED_EDGE ( 'NONE', *, *, #15201, .F. ) ;
#50766 = ORIENTED_EDGE ( 'NONE', *, *, #11224, .F. ) ;
#50765 = ORIENTED_EDGE ( 'NONE', *, *, #123107, .F. ) ;
#50764 = DIRECTION ( 'NONE',  ( 0.000000000000000000, 0.000000000000000000, -1.000000000000000000 ) ) ;
#50767 = DIRECTION ( 'NONE',  ( -1.000000000000000000, -0.000000000000000000, 0.000000000000000000 ) ) ;
#50768 = EDGE_LOOP ( 'NONE', ( #44613, #125713, #18159, #206046 ) ) ;
#50769 = CARTESIAN_POINT ( 'NONE',  ( 20.94999999999999574, 67.07338541492480033, -94.55142446530125255 ) ) ;
#50770 = TOROIDAL_SURFACE ( 'NONE', #42419, 0.2000000000000000111, 0.1000000000000000056 ) ;
#50771 = CIRCLE ( 'NONE', #63257, 4.000000000000003553 ) ;
#50772 = FACE_OUTER_BOUND ( 'NONE', #110101, .T. ) ;
#50773 = AXIS2_PLACEMENT_3D ( 'NONE', #42343, #24089, #223525 ) ;
#50774 = ADVANCED_FACE ( 'NONE', ( #233509 ), #203993, .F. ) ;
#50776 = CARTESIAN_POINT ( 'NONE',  ( -18.39999999999999858, 86.89640087696872683, -199.6396878666313341 ) ) ;
#50775 = CIRCLE ( 'NONE', #38346, 0.1000000000000028644 ) ;
#50777 = VERTEX_POINT ( 'NONE', #74454 ) ;
#50778 = VERTEX_POINT ( 'NONE', #54832 ) ;
#50779 = ORIENTED_EDGE ( 'NONE', *, *, #38135, .T. ) ;
#50780 = CYLINDRICAL_SURFACE ( 'NONE', #78942, 0.09999999999999939493 ) ;
#50782 = ORIENTED_EDGE ( 'NONE', *, *, #176930, .F. ) ;
#50781 = CARTESIAN_POINT ( 'NONE',  ( -20.07928932188135107, 66.77928932189321642, -90.67310748452436542 ) ) ;
#50783 = CARTESIAN_POINT ( 'NONE',  ( 23.14999999999998437, -11.48087284838115885, -203.5004116939112464 ) ) ;
#50785 = ORIENTED_EDGE ( 'NONE', *, *, #16400, .T. ) ;
#50784 = CARTESIAN_POINT ( 'NONE',  ( -20.64999999999999858, 2.000000000011154189, -147.2246219227621111 ) ) ;
#50786 = ADVANCED_FACE ( 'NONE', ( #255565 ), #37880, .T. ) ;
#50787 = ORIENTED_EDGE ( 'NONE', *, *, #75327, .T. ) ;
#50788 = CARTESIAN_POINT ( 'NONE',  ( -18.40000000000000213, 64.51332499825495859, -194.2731074845244450 ) ) ;
#50789 = EDGE_CURVE ( 'NONE', #86432, #44321, #87460, .T. ) ;
#50790 = EDGE_CURVE ( 'NONE', #88307, #143912, #161978, .T. ) ;
#50791 = ORIENTED_EDGE ( 'NONE', *, *, #32473, .T. ) ;
#50792 = DIRECTION ( 'NONE',  ( 0.000000000000000000, -1.000000000000000000, 0.000000000000000000 ) ) ;
#50793 = DIRECTION ( 'NONE',  ( 1.000000000000000000, 0.000000000000000000, 0.000000000000000000 ) ) ;
#50794 = ADVANCED_FACE ( 'NONE', ( #254313 ), #8379, .T. ) ;
#50796 = ORIENTED_EDGE ( 'NONE', *, *, #47253, .T. ) ;
#50795 = ORIENTED_EDGE ( 'NONE', *, *, #111492, .T. ) ;
#50797 = ORIENTED_EDGE ( 'NONE', *, *, #12127, .T. ) ;
#50798 = LINE ( 'NONE', #213746, #153058 ) ;
#50799 = VERTEX_POINT ( 'NONE', #193091 ) ;
#50800 = ORIENTED_EDGE ( 'NONE', *, *, #126082, .T. ) ;
#50801 = ADVANCED_FACE ( 'NONE', ( #155272 ), #220574, .F. ) ;
#50802 = LINE ( 'NONE', #105638, #109367 ) ;
#50804 = ORIENTED_EDGE ( 'NONE', *, *, #161872, .T. ) ;
#50803 = DIRECTION ( 'NONE',  ( 3.616040088954490704E-32, 7.105427357601001859E-15, -1.000000000000000000 ) ) ;
#50805 = CARTESIAN_POINT ( 'NONE',  ( -23.15000000000000213, 71.75000000001186606, -90.67310748452433700 ) ) ;
#50807 = LINE ( 'NONE', #32599, #244175 ) ;
#50806 = CARTESIAN_POINT ( 'NONE',  ( -18.34374000495059676, 33.92263863280957281, -235.0698407953532296 ) ) ;
#50808 = CARTESIAN_POINT ( 'NONE',  ( -20.94999999999999929, 14.76712877540431812, -235.7629163147296083 ) ) ;
#50809 = DIRECTION ( 'NONE',  ( 1.000000000000000000, 0.000000000000000000, 0.000000000000000000 ) ) ;
#50810 = ORIENTED_EDGE ( 'NONE', *, *, #256161, .T. ) ;
#50811 = ORIENTED_EDGE ( 'NONE', *, *, #215643, .F. ) ;
#50812 = DIRECTION ( 'NONE',  ( -1.000000000000000000, 3.265361837132813093E-16, 2.280189983783949500E-30 ) ) ;
#50813 = CARTESIAN_POINT ( 'NONE',  ( -18.50000000000000711, 11.65000000001115232, -74.01480577065404987 ) ) ;
#50814 = ORIENTED_EDGE ( 'NONE', *, *, #50655, .T. ) ;
#50815 = ADVANCED_FACE ( 'NONE', ( #196922 ), #32762, .T. ) ;
#50816 = AXIS2_PLACEMENT_3D ( 'NONE', #174798, #32717, #152650 ) ;
#50817 = DIRECTION ( 'NONE',  ( 0.000000000000000000, 0.000000000000000000, 1.000000000000000000 ) ) ;
#50818 = FACE_OUTER_BOUND ( 'NONE', #70344, .T. ) ;
#50819 = ORIENTED_EDGE ( 'NONE', *, *, #181748, .T. ) ;
#50820 = ORIENTED_EDGE ( 'NONE', *, *, #67987, .F. ) ;
#50821 = DIRECTION ( 'NONE',  ( 1.000000000000000000, -0.000000000000000000, -0.000000000000000000 ) ) ;
#50822 = CARTESIAN_POINT ( 'NONE',  ( 21.14999999999999503, 64.27847795353595473, -247.1247091181747066 ) ) ;
#50824 = EDGE_CURVE ( 'NONE', #96187, #68295, #70945, .T. ) ;
#50823 = ORIENTED_EDGE ( 'NONE', *, *, #251366, .F. ) ;
#50825 = DIRECTION ( 'NONE',  ( 1.000000000000000000, 3.265361837132813093E-16, -0.000000000000000000 ) ) ;
#50827 = VERTEX_POINT ( 'NONE', #182525 ) ;
#50826 =( REPRESENTATION_RELATIONSHIP ('NONE','NONE', #36900, #63487 ) REPRESENTATION_RELATIONSHIP_WITH_TRANSFORMATION ( #164175 )SHAPE_REPRESENTATION_RELATIONSHIP( ) );
#50828 = EDGE_CURVE ( 'NONE', #222562, #159519, #203353, .T. ) ;
#50829 = CARTESIAN_POINT ( 'NONE',  ( 18.39999999999999858, -9.499999999988844479, -140.6001893912220737 ) ) ;
#50830 = DIRECTION ( 'NONE',  ( 1.000000000000000000, 0.000000000000000000, 0.000000000000000000 ) ) ;
#50832 = CARTESIAN_POINT ( 'NONE',  ( -21.11833042828115126, -1.364701729829611798, -194.7004781828140665 ) ) ;
#50831 = LINE ( 'NONE', #149986, #219662 ) ;
#50833 = DIRECTION ( 'NONE',  ( 0.000000000000000000, 0.000000000000000000, -1.000000000000000000 ) ) ;
#50834 = DIRECTION ( 'NONE',  ( 0.000000000000000000, 1.000000000000000000, 7.272083257015735086E-15 ) ) ;
#50835 = PLANE ( 'NONE',  #194774 ) ;
#50836 = DIRECTION ( 'NONE',  ( 0.000000000000000000, 0.000000000000000000, -1.000000000000000000 ) ) ;
#50837 = VECTOR ( 'NONE', #204548, 1000.000000000000000 ) ;
#50839 = VERTEX_POINT ( 'NONE', #100365 ) ;
#50838 = DIRECTION ( 'NONE',  ( 1.000000000000000000, 0.000000000000000000, 0.000000000000000000 ) ) ;
#50840 = CIRCLE ( 'NONE', #242393, 0.1000000000000028644 ) ;
#50842 = ORIENTED_EDGE ( 'NONE', *, *, #18017, .T. ) ;
#50841 = ORIENTED_EDGE ( 'NONE', *, *, #1960, .T. ) ;
#50843 = ORIENTED_EDGE ( 'NONE', *, *, #168311, .T. ) ;
#50844 = CARTESIAN_POINT ( 'NONE',  ( -20.85000000000000142, -11.64999999998884306, -167.5000000000000000 ) ) ;
#50845 =( BOUNDED_SURFACE ( )  B_SPLINE_SURFACE ( 3, 2, ( 
 ( #249496, #188225, #252046 ),
 ( #210367, #144254, #89120 ),
 ( #223805, #90398, #189521 ),
 ( #129544, #31754, #70878 ),
 ( #209072, #248203, #72149 ),
 ( #231226, #52551, #132108 ) ),
 .UNSPECIFIED., .F., .F., .F. ) 
 B_SPLINE_SURFACE_WITH_KNOTS ( ( 4, 2, 4 ),
 ( 3, 3 ),
 ( -1.776356839400250465E-15, 0.7853981633974468357, 1.570796326794895448 ),
 ( 0.000000000000000000, 1.000000000000000000 ),
 .UNSPECIFIED. ) 
 GEOMETRIC_REPRESENTATION_ITEM ( )  RATIONAL_B_SPLINE_SURFACE ( (
 ( 1.000000000000000000, 0.5000000000000260902, 1.000000000000000000),
 ( 1.000000000000000000, 0.4993418825348700518, 1.000000000000000000),
 ( 1.000000000000000000, 0.5278258667036815899, 1.000000000000000000),
 ( 1.000000000000000000, 0.6092287576718847797, 1.000000000000000000),
 ( 1.000000000000000000, 0.6611148371761672582, 1.000000000000000000),
 ( 1.000000000000000000, 0.7071067811865597852, 1.000000000000000000) ) ) 
 REPRESENTATION_ITEM ( '' )  SURFACE ( )  );
#50846 = CARTESIAN_POINT ( 'NONE',  ( -18.79999999999999716, 4.513204987021263825, 22.10000000000000142 ) ) ;
#50848 = DIRECTION ( 'NONE',  ( 0.000000000000000000, 0.000000000000000000, -1.000000000000000000 ) ) ;
#50847 = DIRECTION ( 'NONE',  ( 0.000000000000000000, -0.4088369013363281068, 0.9126074666063770380 ) ) ;
#50849 = CARTESIAN_POINT ( 'NONE',  ( 23.14999999999999858, 67.34812900481119868, -214.0300458246130972 ) ) ;
#50850 = ORIENTED_EDGE ( 'NONE', *, *, #49180, .T. ) ;
#50851 = CARTESIAN_POINT ( 'NONE',  ( -22.57320508075687115, 11.75000000001115552, -100.5000000000000568 ) ) ;
#50853 = EDGE_CURVE ( 'NONE', #102162, #51895, #84637, .T. ) ;
#50852 = VERTEX_POINT ( 'NONE', #159112 ) ;
#50854 = CARTESIAN_POINT ( 'NONE',  ( -21.14999999999999858, -7.589415207398531038E-16, 6.540656951701240729 ) ) ;
#50856 = VECTOR ( 'NONE', #226214, 1000.000000000000000 ) ;
#50855 = DIRECTION ( 'NONE',  ( 0.000000000000000000, -0.9651348961777157509, 0.2617529984165031243 ) ) ;
#50857 = DIRECTION ( 'NONE',  ( 0.000000000000000000, -1.000000000000000000, 2.771150684185008344E-14 ) ) ;
#50858 = ORIENTED_EDGE ( 'NONE', *, *, #217086, .T. ) ;
#50859 = B_SPLINE_CURVE_WITH_KNOTS ( 'NONE', 3,
 ( #190903, #72222, #132181, #188291, #207892, #246979, #150474, #210449 ),
 .UNSPECIFIED., .F., .F.,
 ( 4, 2, 2, 4 ),
 ( 0.000000000000000000, 0.0001049670497870194505, 0.0002099340995740389009, 0.0004198681991480204476 ),
 .UNSPECIFIED. ) ;
#50860 = FACE_OUTER_BOUND ( 'NONE', #183331, .T. ) ;
#50861 = PLANE ( 'NONE',  #67370 ) ;
#50862 = ORIENTED_EDGE ( 'NONE', *, *, #144488, .T. ) ;
#50863 = EDGE_LOOP ( 'NONE', ( #32135, #31116, #54248 ) ) ;
#50864 = DIRECTION ( 'NONE',  ( -0.7071067811865474617, 0.7071067811865474617, 0.000000000000000000 ) ) ;
#50865 = CARTESIAN_POINT ( 'NONE',  ( 16.27683809663749770, 9.350000000011137402, -176.7499999999999716 ) ) ;
#50866 = DIRECTION ( 'NONE',  ( 2.952720810173289112E-16, -1.000000000000000000, 0.000000000000000000 ) ) ;
#50867 = DIRECTION ( 'NONE',  ( 0.000000000000000000, -6.240597636138643358E-14, -1.000000000000000000 ) ) ;
#50868 = CARTESIAN_POINT ( 'NONE',  ( -23.25000000000000355, 15.91777359887373500, -218.8720307647289758 ) ) ;
#50869 = CARTESIAN_POINT ( 'NONE',  ( -21.05000000000000071, 6.304961112684661195, -0.02138556593757447166 ) ) ;
#50870 = ORIENTED_EDGE ( 'NONE', *, *, #78279, .F. ) ;
#50871 = DIRECTION ( 'NONE',  ( -1.000000000000000000, -0.000000000000000000, -0.000000000000000000 ) ) ;
#50872 = DIRECTION ( 'NONE',  ( 0.000000000000000000, 0.000000000000000000, 1.000000000000000000 ) ) ;
#50873 = EDGE_CURVE ( 'NONE', #46377, #191700, #204162, .T. ) ;
#50876 = DIRECTION ( 'NONE',  ( 0.000000000000000000, -6.467318590049456648E-15, 1.000000000000000000 ) ) ;
#50875 = CIRCLE ( 'NONE', #167456, 0.09999999999999939493 ) ;
#50874 = CARTESIAN_POINT ( 'NONE',  ( -21.14999999999999858, 1.115600667400684642E-11, -134.0000000000000000 ) ) ;
#50878 = LINE ( 'NONE', #232129, #212439 ) ;
#50877 = AXIS2_PLACEMENT_3D ( 'NONE', #107409, #205211, #241780 ) ;
#50879 = CIRCLE ( 'NONE', #238331, 0.09999999999999939493 ) ;
#50880 = CARTESIAN_POINT ( 'NONE',  ( -18.44362607810621313, -9.490496158084827272, -7.057953866847126001 ) ) ;
#50882 = ADVANCED_FACE ( 'NONE', ( #199519 ), #242460, .F. ) ;
#50881 = DIRECTION ( 'NONE',  ( 0.000000000000000000, -1.000000000000000000, 0.000000000000000000 ) ) ;
#50883 = DIRECTION ( 'NONE',  ( -2.557131231893037478E-16, -0.8660254037844420383, 0.4999999999999941713 ) ) ;
#50885 = VERTEX_POINT ( 'NONE', #220357 ) ;
#50884 = CYLINDRICAL_SURFACE ( 'NONE', #257122, 0.5000000000000004441 ) ;
#50886 = EDGE_CURVE ( 'NONE', #125402, #249684, #179267, .T. ) ;
#50887 = EDGE_CURVE ( 'NONE', #10713, #228818, #21050, .T. ) ;
#50888 = FACE_OUTER_BOUND ( 'NONE', #165974, .T. ) ;
#50889 = AXIS2_PLACEMENT_3D ( 'NONE', #117694, #219356, #18603 ) ;
#50890 = DIRECTION ( 'NONE',  ( 0.000000000000000000, -6.982962677686266711E-15, 1.000000000000000000 ) ) ;
#50891 = LINE ( 'NONE', #226990, #125432 ) ;
#50892 = VERTEX_POINT ( 'NONE', #102942 ) ;
#50893 = TOROIDAL_SURFACE ( 'NONE', #196662, 11.65000000000000036, 0.1000000000000000056 ) ;
#50894 = ADVANCED_FACE ( 'NONE', ( #80808 ), #143367, .F. ) ;
#50895 = DIRECTION ( 'NONE',  ( 1.000000000000000000, -0.000000000000000000, -0.000000000000000000 ) ) ;
#50896 = EDGE_CURVE ( 'NONE', #16721, #202516, #241208, .T. ) ;
#50897 = CARTESIAN_POINT ( 'NONE',  ( -21.59142135623730852, 62.88761514850714462, -221.8809495011140314 ) ) ;
#50898 = CARTESIAN_POINT ( 'NONE',  ( -18.50000000000000000, -9.500000000000005329, -8.099999999999999645 ) ) ;
#50899 = EDGE_LOOP ( 'NONE', ( #63060, #167992, #32341, #218525 ) ) ;
#50900 = CARTESIAN_POINT ( 'NONE',  ( -16.87036670365549895, 12.42497885867826390, -211.1079079717509046 ) ) ;
#50902 = ORIENTED_EDGE ( 'NONE', *, *, #121224, .F. ) ;
#50901 = CARTESIAN_POINT ( 'NONE',  ( 23.14999999999999858, 71.00000000001253397, -182.4283735034374843 ) ) ;
#50903 = VECTOR ( 'NONE', #104337, 1000.000000000000114 ) ;
#50904 = CARTESIAN_POINT ( 'NONE',  ( -16.87036670365549895, 9.989418819312803066, -146.5204398826979855 ) ) ;
#50905 = EDGE_LOOP ( 'NONE', ( #116887, #122372, #20636, #35188 ) ) ;
#50906 = CARTESIAN_POINT ( 'NONE',  ( -16.93710578446424009, 66.05000000001261640, -190.6043035007245408 ) ) ;
#50907 = AXIS2_PLACEMENT_3D ( 'NONE', #217649, #41632, #97697 ) ;
#50908 = APPLICATION_PROTOCOL_DEFINITION ( 'draft international standard', 'automotive_design', 1998, #237440 ) ;
#50909 = DIRECTION ( 'NONE',  ( 0.000000000000000000, 1.000000000000000000, 0.000000000000000000 ) ) ;
#50910 = EDGE_CURVE ( 'NONE', #46606, #82861, #104210, .T. ) ;
#50911 = B_SPLINE_CURVE_WITH_KNOTS ( 'NONE', 3,
 ( #57726, #173889, #74780, #236376 ),
 .UNSPECIFIED., .F., .F.,
 ( 4, 4 ),
 ( 6.278991785631292523E-18, 0.0001058379652594621054 ),
 .UNSPECIFIED. ) ;
#50912 = CARTESIAN_POINT ( 'NONE',  ( -21.65000000000000213, 10.05000000001113847, -188.3499999999999659 ) ) ;
#50913 = CARTESIAN_POINT ( 'NONE',  ( -20.94999999999999929, 7.872214528623318053, -209.6555322433423783 ) ) ;
#50914 = ORIENTED_EDGE ( 'NONE', *, *, #42764, .F. ) ;
#50915 = CIRCLE ( 'NONE', #5112, 1.500000000000001332 ) ;
#50916 = DIRECTION ( 'NONE',  ( 1.000000000000000000, -0.000000000000000000, -0.000000000000000000 ) ) ;
#50917 = CYLINDRICAL_SURFACE ( 'NONE', #38378, 0.09999999999999892308 ) ;
#50918 = CIRCLE ( 'NONE', #146596, 0.5999999999999894307 ) ;
#50919 = ADVANCED_FACE ( 'NONE', ( #198207 ), #179946, .T. ) ;
#50920 = VECTOR ( 'NONE', #110596, 1000.000000000000000 ) ;
#50921 = DIRECTION ( 'NONE',  ( 1.000000000000000000, -0.000000000000000000, -0.000000000000000000 ) ) ;
#50922 = ORIENTED_EDGE ( 'NONE', *, *, #5191, .F. ) ;
#50923 = ORIENTED_EDGE ( 'NONE', *, *, #179466, .T. ) ;
#50924 = EDGE_CURVE ( 'NONE', #209893, #190117, #63841, .T. ) ;
#50926 = CIRCLE ( 'NONE', #150914, 7.899999999999996803 ) ;
#50925 = CARTESIAN_POINT ( 'NONE',  ( -20.64999999999999858, -8.999999999988844479, -191.1060308773475356 ) ) ;
#50928 = VECTOR ( 'NONE', #70831, 1000.000000000000000 ) ;
#50927 = FACE_OUTER_BOUND ( 'NONE', #94779, .T. ) ;
#50929 = DIRECTION ( 'NONE',  ( -1.000000000000000000, -0.000000000000000000, -0.000000000000000000 ) ) ;
#50930 = DIRECTION ( 'NONE',  ( 0.000000000000000000, 0.9579639084728132081, 0.2868887416116073230 ) ) ;
#50932 = CARTESIAN_POINT ( 'NONE',  ( 22.47809213839789066, -2.442448617817909451, -189.6088748368766517 ) ) ;
#50931 = DIRECTION ( 'NONE',  ( -1.000000000000000000, 0.000000000000000000, 0.000000000000000000 ) ) ;
#50934 = EDGE_CURVE ( 'NONE', #172095, #231898, #19589, .T. ) ;
#50933 = VECTOR ( 'NONE', #13843, 1000.000000000000000 ) ;
#50935 = AXIS2_PLACEMENT_3D ( 'NONE', #152555, #91272, #134223 ) ;
#50936 = CARTESIAN_POINT ( 'NONE',  ( -21.12757541349819590, 75.99483878420269889, -176.4964880557759273 ) ) ;
#50937 = CYLINDRICAL_SURFACE ( 'NONE', #185185, 0.09999999999999939493 ) ;
#50938 = CARTESIAN_POINT ( 'NONE',  ( -20.94999999999999929, 1.115600667400684642E-11, -134.0000000000000284 ) ) ;
#50939 = VERTEX_POINT ( 'NONE', #58677 ) ;
#50941 = ORIENTED_EDGE ( 'NONE', *, *, #68505, .T. ) ;
#50940 = DIRECTION ( 'NONE',  ( 0.000000000000000000, 0.2128009952263403282, -0.9770955615653358350 ) ) ;
#50942 = CARTESIAN_POINT ( 'NONE',  ( -23.15000000000000213, -8.663551401858001100, -157.9758988819327215 ) ) ;
#50943 = AXIS2_PLACEMENT_3D ( 'NONE', #21291, #81208, #162074 ) ;
#50944 = CARTESIAN_POINT ( 'NONE',  ( -21.08035267497491816, -1.266598828715301162, -194.7957211280704257 ) ) ;
#50946 = CARTESIAN_POINT ( 'NONE',  ( -21.14999999999999858, -11.74999999998884448, -69.90000000000004832 ) ) ;
#50945 = CARTESIAN_POINT ( 'NONE',  ( -20.94999999999999929, 44.12194005689738674, -258.6913704466671788 ) ) ;
#50947 =( BOUNDED_CURVE ( )  B_SPLINE_CURVE ( 3, ( #254750, #215652, #155733, #235233 ),
 .UNSPECIFIED., .F., .F. ) 
 B_SPLINE_CURVE_WITH_KNOTS ( ( 4, 4 ),
 ( 1.570796326794902997, 3.141592653589791784 ),
 .UNSPECIFIED. ) 
 CURVE ( )  GEOMETRIC_REPRESENTATION_ITEM ( )  RATIONAL_B_SPLINE_CURVE ( ( 1.000000000000000000, 0.8047378541243667138, 0.8047378541243667138, 1.000000000000000000 ) ) 
 REPRESENTATION_ITEM ( '' )  );
#50948 = ORIENTED_EDGE ( 'NONE', *, *, #241622, .F. ) ;
#50949 = CARTESIAN_POINT ( 'NONE',  ( 21.30000000000002558, 1.115600667400684642E-11, -167.4999999999999716 ) ) ;
#50950 = FACE_OUTER_BOUND ( 'NONE', #106145, .T. ) ;
#50951 = EDGE_CURVE ( 'NONE', #69009, #55978, #199382, .T. ) ;
#50952 = CARTESIAN_POINT ( 'NONE',  ( -2.995603634470891112E-16, 87.75000000001205080, -124.2731074845242176 ) ) ;
#50954 = CARTESIAN_POINT ( 'NONE',  ( 22.48660254037844552, 12.58580559757025696, -223.4396719342083770 ) ) ;
#50953 = AXIS2_PLACEMENT_3D ( 'NONE', #227554, #110172, #131025 ) ;
#50955 = VERTEX_POINT ( 'NONE', #139509 ) ;
#50956 = ORIENTED_EDGE ( 'NONE', *, *, #162726, .F. ) ;
#50957 = B_SPLINE_CURVE_WITH_KNOTS ( 'NONE', 3,
 ( #74607, #154147, #38034, #181395, #199675, #83516, #78404, #2715, #18443, #142237 ),
 .UNSPECIFIED., .F., .F.,
 ( 4, 2, 2, 2, 4 ),
 ( 0.000000000000000000, 3.990160268013534029E-05, 7.980320536027068058E-05, 0.0001596064107205331212, 0.0003192128214410723140 ),
 .UNSPECIFIED. ) ;
#50958 = DIRECTION ( 'NONE',  ( 0.000000000000000000, -0.000000000000000000, -1.000000000000000000 ) ) ;
#50959 = VERTEX_POINT ( 'NONE', #219044 ) ;
#50960 = DIRECTION ( 'NONE',  ( 1.000000000000000000, 0.000000000000000000, 0.000000000000000000 ) ) ;
#50961 = CIRCLE ( 'NONE', #17645, 0.09999999999999993616 ) ;
#50962 = CIRCLE ( 'NONE', #205085, 0.09999999999999939493 ) ;
#50963 = DIRECTION ( 'NONE',  ( 1.000000000000000000, -0.000000000000000000, -0.000000000000000000 ) ) ;
#50964 = VECTOR ( 'NONE', #101211, 1000.000000000000000 ) ;
#50965 = DIRECTION ( 'NONE',  ( 1.000000000000000000, 0.000000000000000000, 0.000000000000000000 ) ) ;
#50966 = PLANE ( 'NONE',  #238727 ) ;
#50967 = EDGE_LOOP ( 'NONE', ( #219448, #128214, #44600, #195415 ) ) ;
#50968 = DIRECTION ( 'NONE',  ( 0.000000000000000000, 6.982962677686266711E-15, -1.000000000000000000 ) ) ;
#50969 = CARTESIAN_POINT ( 'NONE',  ( 18.59999999999999787, 76.00000000001267608, -203.5231074845243597 ) ) ;
#50970 = FACE_OUTER_BOUND ( 'NONE', #223894, .T. ) ;
#50971 = CARTESIAN_POINT ( 'NONE',  ( -23.15000000000000213, 87.65000000001192859, -106.1231074845242262 ) ) ;
#50972 = CARTESIAN_POINT ( 'NONE',  ( -22.39999999999999858, 7.790779598384560245, -33.39999999999999858 ) ) ;
#50973 = CARTESIAN_POINT ( 'NONE',  ( -16.77180007708462028, 66.05000000001224691, -149.1587216034792505 ) ) ;
#50974 = EDGE_LOOP ( 'NONE', ( #187751, #210835, #59811 ) ) ;
#50975 = AXIS2_PLACEMENT_3D ( 'NONE', #29764, #109249, #126248 ) ;
#50977 = DIRECTION ( 'NONE',  ( 0.000000000000000000, -3.552713678800554572E-15, -1.000000000000000000 ) ) ;
#50976 = DIRECTION ( 'NONE',  ( -0.000000000000000000, 0.000000000000000000, 1.000000000000000000 ) ) ;
#50978 = ORIENTED_EDGE ( 'NONE', *, *, #229521, .T. ) ;
#50980 = EDGE_LOOP ( 'NONE', ( #224987, #224957, #160430, #163059 ) ) ;
#50979 = DIRECTION ( 'NONE',  ( -1.000000000000000000, 0.000000000000000000, 0.000000000000000000 ) ) ;
#50981 = ORIENTED_EDGE ( 'NONE', *, *, #119195, .F. ) ;
#50982 = CARTESIAN_POINT ( 'NONE',  ( 23.04999999999999716, 67.17743825834560312, -115.6731074845243654 ) ) ;
#50983 = CARTESIAN_POINT ( 'NONE',  ( 12.84435279558019793, 66.58929125296516816, -151.9538990786803367 ) ) ;
#50984 = FACE_OUTER_BOUND ( 'NONE', #82598, .T. ) ;
#50985 = CARTESIAN_POINT ( 'NONE',  ( -18.39999999999999858, 11.47316190337362762, -42.82594606680797256 ) ) ;
#50986 = CIRCLE ( 'NONE', #171858, 0.4000000000000097367 ) ;
#50987 = VERTEX_POINT ( 'NONE', #140811 ) ;
#50988 = CARTESIAN_POINT ( 'NONE',  ( -20.64999999999999858, 27.82649702422227733, -239.8850763025288870 ) ) ;
#50989 = DIRECTION ( 'NONE',  ( -1.000000000000000000, -2.952720810173289112E-16, 0.000000000000000000 ) ) ;
#50990 = VERTEX_POINT ( 'NONE', #2563 ) ;
#50991 = CARTESIAN_POINT ( 'NONE',  ( 18.49713797159841633, -9.446482327567903070, -174.5714581216104477 ) ) ;
#50992 = ADVANCED_FACE ( 'NONE', ( #82086 ), #95826, .F. ) ;
#50993 = DIRECTION ( 'NONE',  ( -1.000000000000000000, 0.000000000000000000, -0.000000000000000000 ) ) ;
#50994 = VERTEX_POINT ( 'NONE', #226755 ) ;
#50995 = DIRECTION ( 'NONE',  ( -1.000000000000000000, -0.000000000000000000, 0.000000000000000000 ) ) ;
#50996 = AXIS2_PLACEMENT_3D ( 'NONE', #254866, #234076, #235358 ) ;
#50997 = VERTEX_POINT ( 'NONE', #228051 ) ;
#50998 = DIRECTION ( 'NONE',  ( 0.000000000000000000, 0.01283462868040404978, 0.9999176327611370985 ) ) ;
#50999 = VERTEX_POINT ( 'NONE', #11585 ) ;
#51000 = CARTESIAN_POINT ( 'NONE',  ( 23.14999999999999858, 5.000000000011153745, -55.09473398108690390 ) ) ;
#51001 = EDGE_CURVE ( 'NONE', #24254, #159793, #144643, .T. ) ;
#51002 = CARTESIAN_POINT ( 'NONE',  ( 20.94999999999999929, 64.25000000001175238, -76.30697314750247529 ) ) ;
#51003 = CYLINDRICAL_SURFACE ( 'NONE', #255741, 2.000000000000001776 ) ;
#51004 = DIRECTION ( 'NONE',  ( 0.000000000000000000, -0.4999999999999943379, -0.8660254037844420383 ) ) ;
#51005 = EDGE_CURVE ( 'NONE', #89546, #111950, #224183, .T. ) ;
#51006 = AXIS2_PLACEMENT_3D ( 'NONE', #3464, #139096, #119595 ) ;
#51007 = FACE_OUTER_BOUND ( 'NONE', #225594, .T. ) ;
#51008 = DIRECTION ( 'NONE',  ( 1.000000000000000000, 0.000000000000000000, -0.000000000000000000 ) ) ;
#51009 = ORIENTED_EDGE ( 'NONE', *, *, #199001, .F. ) ;
#51010 = CARTESIAN_POINT ( 'NONE',  ( -21.05000000000000071, -11.74999999998884448, -197.8999999999999773 ) ) ;
#51012 = EDGE_LOOP ( 'NONE', ( #7577, #252561, #53967, #25081 ) ) ;
#51011 = AXIS2_PLACEMENT_3D ( 'NONE', #43015, #122559, #164252 ) ;
#51014 = DIRECTION ( 'NONE',  ( -0.000000000000000000, 0.4088369013363276072, -0.9126074666063773710 ) ) ;
#51013 = CARTESIAN_POINT ( 'NONE',  ( -21.05000000000000071, 69.58633726514275963, -169.9375146211616254 ) ) ;
#51015 = VERTEX_POINT ( 'NONE', #128954 ) ;
#51016 = CARTESIAN_POINT ( 'NONE',  ( -20.54999999999999716, 66.65000000001205649, -124.2731074845243597 ) ) ;
#51018 = CARTESIAN_POINT ( 'NONE',  ( 20.94999999999999929, 87.29603075034744109, -139.5710066441881452 ) ) ;
#51017 = AXIS2_PLACEMENT_3D ( 'NONE', #242343, #61142, #140677 ) ;
#51019 = EDGE_CURVE ( 'NONE', #48019, #62589, #169400, .T. ) ;
#51020 = DIRECTION ( 'NONE',  ( 0.000000000000000000, -0.7397890806274222131, -0.6728388485993012091 ) ) ;
#51021 = VERTEX_POINT ( 'NONE', #188922 ) ;
#51022 = ORIENTED_EDGE ( 'NONE', *, *, #204143, .F. ) ;
#51023 = EDGE_CURVE ( 'NONE', #225362, #110197, #191750, .T. ) ;
#51024 = ADVANCED_FACE ( 'NONE', ( #89802 ), #126376, .F. ) ;
#51026 = CARTESIAN_POINT ( 'NONE',  ( -33.72168855820452649, 11.47316190337362940, -191.7499999999999716 ) ) ;
#51025 = CARTESIAN_POINT ( 'NONE',  ( -21.14999999999999858, 41.42187432231295219, -260.1830396872097140 ) ) ;
#51028 = ORIENTED_EDGE ( 'NONE', *, *, #143010, .F. ) ;
#51027 = LINE ( 'NONE', #10664, #69750 ) ;
#51029 = AXIS2_PLACEMENT_3D ( 'NONE', #134831, #249680, #54034 ) ;
#51030 = ORIENTED_EDGE ( 'NONE', *, *, #122612, .T. ) ;
#51031 = FACE_BOUND ( 'NONE', #22472, .T. ) ;
#51032 = DIRECTION ( 'NONE',  ( -1.000000000000000000, 0.000000000000000000, 0.000000000000000000 ) ) ;
#51033 = ORIENTED_EDGE ( 'NONE', *, *, #104010, .T. ) ;
#51034 = CARTESIAN_POINT ( 'NONE',  ( -21.29999999999995808, 7.128833340093095217, -233.7327013124392749 ) ) ;
#51035 = ADVANCED_FACE ( 'NONE', ( #68997 ), #115715, .T. ) ;
#51036 = VERTEX_POINT ( 'NONE', #148517 ) ;
#51037 = CIRCLE ( 'NONE', #38600, 0.5000000000000004441 ) ;
#51038 = DIRECTION ( 'NONE',  ( -1.186688945009010077E-16, -1.000000000000000000, -7.759275652592821052E-15 ) ) ;
#51039 = CARTESIAN_POINT ( 'NONE',  ( 21.05000000000000071, -11.48912529307605901, -2.900000000000003464 ) ) ;
#51040 = ORIENTED_EDGE ( 'NONE', *, *, #37035, .T. ) ;
#51041 = CARTESIAN_POINT ( 'NONE',  ( 15.74999999999999645, 9.850000000011137402, -117.2500000000000284 ) ) ;
#51042 = CIRCLE ( 'NONE', #250965, 2.600000000000000089 ) ;
#51043 = AXIS2_PLACEMENT_3D ( 'NONE', #146922, #187370, #227757 ) ;
#51044 = AXIS2_PLACEMENT_3D ( 'NONE', #118681, #198193, #34033 ) ;
#51045 = EDGE_CURVE ( 'NONE', #17147, #190429, #137525, .T. ) ;
#51046 = CIRCLE ( 'NONE', #159440, 0.1000000000000033223 ) ;
#51047 = ORIENTED_EDGE ( 'NONE', *, *, #21642, .F. ) ;
#51048 = DIRECTION ( 'NONE',  ( 0.000000000000000000, -1.000000000000000000, 0.000000000000000000 ) ) ;
#51049 = ORIENTED_EDGE ( 'NONE', *, *, #213842, .T. ) ;
#51050 = ORIENTED_EDGE ( 'NONE', *, *, #83079, .F. ) ;
#51051 = CARTESIAN_POINT ( 'NONE',  ( 20.52683494730124991, 18.86671595410186697, -229.8325257532585795 ) ) ;
#51052 = ORIENTED_EDGE ( 'NONE', *, *, #115761, .F. ) ;
#51053 = DIRECTION ( 'NONE',  ( 0.000000000000000000, 6.982962677686266711E-15, -1.000000000000000000 ) ) ;
#51054 = ORIENTED_EDGE ( 'NONE', *, *, #67408, .F. ) ;
#51056 = ORIENTED_EDGE ( 'NONE', *, *, #152690, .F. ) ;
#51055 = CARTESIAN_POINT ( 'NONE',  ( -23.25000000000000355, 70.35000000001187459, -90.37310748452433984 ) ) ;
#51057 = ORIENTED_EDGE ( 'NONE', *, *, #41578, .F. ) ;
#51058 = CARTESIAN_POINT ( 'NONE',  ( -23.15000000000000213, 36.02367271998545561, -235.8812521208699309 ) ) ;
#51059 = ORIENTED_EDGE ( 'NONE', *, *, #30774, .F. ) ;
#51062 = ORIENTED_EDGE ( 'NONE', *, *, #243215, .F. ) ;
#51061 = EDGE_LOOP ( 'NONE', ( #34435, #216451, #232574, #171801 ) ) ;
#51060 = DIRECTION ( 'NONE',  ( -1.000000000000000000, 0.000000000000000000, 0.000000000000000000 ) ) ;
#51064 = CARTESIAN_POINT ( 'NONE',  ( 23.15000000000000213, -12.41227409413852811, -164.5000000000000000 ) ) ;
#51063 = AXIS2_PLACEMENT_3D ( 'NONE', #190892, #172634, #12246 ) ;
#51065 = EDGE_LOOP ( 'NONE', ( #119440, #39595, #42717, #38580 ) ) ;
#51066 = AXIS2_PLACEMENT_3D ( 'NONE', #100212, #58528, #179796 ) ;
#51067 = EDGE_CURVE ( 'NONE', #222295, #7200, #58402, .T. ) ;
#51068 = CARTESIAN_POINT ( 'NONE',  ( 23.15000000000000213, -8.999999999988842703, -191.1060308773475072 ) ) ;
#51069 = ADVANCED_FACE ( 'NONE', ( #147221 ), #46818, .F. ) ;
#51070 = ORIENTED_EDGE ( 'NONE', *, *, #90479, .F. ) ;
#51071 = CARTESIAN_POINT ( 'NONE',  ( -18.59999999999999787, 9.350000000011156942, -88.15000000000004832 ) ) ;
#51072 = AXIS2_PLACEMENT_3D ( 'NONE', #244511, #127145, #11047 ) ;
#51074 = ORIENTED_EDGE ( 'NONE', *, *, #219810, .F. ) ;
#51073 = CARTESIAN_POINT ( 'NONE',  ( -20.94999999999999929, 77.16412189325330928, -128.6082593989527254 ) ) ;
#51075 = CARTESIAN_POINT ( 'NONE',  ( 20.94999999999999929, 5.000000000011153745, -54.59473398108690390 ) ) ;
#51076 = ORIENTED_EDGE ( 'NONE', *, *, #99495, .F. ) ;
#51077 = EDGE_CURVE ( 'NONE', #85652, #195772, #91761, .T. ) ;
#51079 = ADVANCED_FACE ( 'NONE', ( #74140 ), #175012, .F. ) ;
#51078 = CYLINDRICAL_SURFACE ( 'NONE', #128747, 12.87499999999999822 ) ;
#51080 = CARTESIAN_POINT ( 'NONE',  ( -23.25000000000000000, -0.1008583690875562017, -122.2504328765106294 ) ) ;
#51081 = CIRCLE ( 'NONE', #142677, 0.09999999999999939493 ) ;
#51082 = EDGE_LOOP ( 'NONE', ( #23983, #177765, #246948 ) ) ;
#51083 = CARTESIAN_POINT ( 'NONE',  ( 23.14999999999999147, 1.115600667400684642E-11, -67.00000000000004263 ) ) ;
#51084 = CARTESIAN_POINT ( 'NONE',  ( 18.50000324121758055, 18.34775554461876013, -236.8759397601554042 ) ) ;
#51085 = AXIS2_PLACEMENT_3D ( 'NONE', #96278, #135410, #76723 ) ;
#51086 = ADVANCED_FACE ( 'NONE', ( #33745 ), #12875, .T. ) ;
#51087 = AXIS2_PLACEMENT_3D ( 'NONE', #19383, #177201, #256643 ) ;
#51089 = ORIENTED_EDGE ( 'NONE', *, *, #11670, .F. ) ;
#51088 = CIRCLE ( 'NONE', #84382, 3.899999999999987033 ) ;
#51091 = VERTEX_POINT ( 'NONE', #76661 ) ;
#51090 = CARTESIAN_POINT ( 'NONE',  ( 20.94999999999999929, 76.00000000001190870, -103.0231074845243029 ) ) ;
#51093 = EDGE_CURVE ( 'NONE', #200518, #236679, #53265, .T. ) ;
#51092 = DIRECTION ( 'NONE',  ( 0.000000000000000000, -0.7960711469212456981, 0.6052030477777622375 ) ) ;
#51096 = ADVANCED_FACE ( 'NONE', ( #171964 ), #15433, .F. ) ;
#51095 = EDGE_CURVE ( 'NONE', #7674, #17853, #54315, .T. ) ;
#51094 = AXIS2_PLACEMENT_3D ( 'NONE', #123440, #145556, #227659 ) ;
#51097 = AXIS2_PLACEMENT_3D ( 'NONE', #146927, #223897, #225174 ) ;
#51099 = ORIENTED_EDGE ( 'NONE', *, *, #210839, .F. ) ;
#51098 = VERTEX_POINT ( 'NONE', #212354 ) ;
#51100 = VERTEX_POINT ( 'NONE', #156239 ) ;
#51101 = CARTESIAN_POINT ( 'NONE',  ( -18.50000000000000000, 22.43030315632513094, -231.3223027016406093 ) ) ;
#51102 = ORIENTED_EDGE ( 'NONE', *, *, #235090, .T. ) ;
#51103 = ORIENTED_EDGE ( 'NONE', *, *, #121678, .F. ) ;
#51104 = CARTESIAN_POINT ( 'NONE',  ( 20.94999999999999929, 6.650000000011155876, -110.5170271704400591 ) ) ;
#51105 = VERTEX_POINT ( 'NONE', #196609 ) ;
#51106 = CARTESIAN_POINT ( 'NONE',  ( -18.59999999999999787, -1.249999999988843369, -108.5000000000000426 ) ) ;
#51107 = AXIS2_PLACEMENT_3D ( 'NONE', #35843, #256086, #39705 ) ;
#51108 = FACE_OUTER_BOUND ( 'NONE', #220192, .T. ) ;
#51110 = EDGE_LOOP ( 'NONE', ( #97248, #213765, #104614, #148656, #77567 ) ) ;
#51109 = AXIS2_PLACEMENT_3D ( 'NONE', #216420, #237282, #37818 ) ;
#51111 = EDGE_CURVE ( 'NONE', #136504, #173445, #152390, .T. ) ;
#51112 = VERTEX_POINT ( 'NONE', #91101 ) ;
#51113 = AXIS2_PLACEMENT_3D ( 'NONE', #179400, #39901, #162404 ) ;
#51114 = DIRECTION ( 'NONE',  ( -1.000000000000000000, -0.000000000000000000, -0.000000000000000000 ) ) ;
#51115 = EDGE_CURVE ( 'NONE', #6867, #106375, #220747, .T. ) ;
#51116 = EDGE_CURVE ( 'NONE', #169705, #8702, #250181, .T. ) ;
#51117 = ORIENTED_EDGE ( 'NONE', *, *, #213960, .F. ) ;
#51118 = AXIS2_PLACEMENT_3D ( 'NONE', #238721, #79623, #163060 ) ;
#51119 = CIRCLE ( 'NONE', #213461, 0.1000000000000028644 ) ;
#51120 = AXIS2_PLACEMENT_3D ( 'NONE', #51025, #85022, #164603 ) ;
#51121 = ADVANCED_FACE ( 'NONE', ( #93667 ), #151082, .T. ) ;
#51122 = AXIS2_PLACEMENT_3D ( 'NONE', #231608, #254944, #75120 ) ;
#51123 = CARTESIAN_POINT ( 'NONE',  ( -18.54118089899631272, 85.46353763186019137, -129.4745298866561143 ) ) ;
#51124 = ORIENTED_EDGE ( 'NONE', *, *, #51259, .T. ) ;
#51126 = EDGE_LOOP ( 'NONE', ( #96585, #100426, #222115, #107793 ) ) ;
#51125 = CARTESIAN_POINT ( 'NONE',  ( -21.93642651522410247, 68.67283376068657219, -170.0231074845243882 ) ) ;
#51127 = DIRECTION ( 'NONE',  ( 0.000000000000000000, 0.000000000000000000, 1.000000000000000000 ) ) ;
#51128 = CARTESIAN_POINT ( 'NONE',  ( -18.40000000000000213, 5.650000000011139001, -87.85000000000003695 ) ) ;
#51129 = EDGE_CURVE ( 'NONE', #32586, #5211, #75203, .T. ) ;
#51130 = DIRECTION ( 'NONE',  ( 0.000000000000000000, 0.000000000000000000, 1.000000000000000000 ) ) ;
#51131 = CARTESIAN_POINT ( 'NONE',  ( -20.64999999999999858, 68.75000000001199396, -115.3731074845243540 ) ) ;
#51132 = CARTESIAN_POINT ( 'NONE',  ( 20.94999999999999929, 71.00000000001205080, -124.1178414656112352 ) ) ;
#51133 = DIRECTION ( 'NONE',  ( -1.000000000000000000, 0.000000000000000000, 0.000000000000000000 ) ) ;
#51134 = CARTESIAN_POINT ( 'NONE',  ( -21.05000000000000071, 6.307425219576558995, -33.51681986838567440 ) ) ;
#51135 = DIRECTION ( 'NONE',  ( 1.000000000000000000, 0.000000000000000000, 0.000000000000000000 ) ) ;
#51136 = DIRECTION ( 'NONE',  ( -0.000000000000000000, 0.8814952561688430555, -0.4721928772777346239 ) ) ;
#51137 = AXIS2_PLACEMENT_3D ( 'NONE', #252787, #12941, #132872 ) ;
#51139 = ORIENTED_EDGE ( 'NONE', *, *, #178116, .F. ) ;
#51138 = AXIS2_PLACEMENT_3D ( 'NONE', #160086, #62247, #201748 ) ;
#51140 = AXIS2_PLACEMENT_3D ( 'NONE', #149914, #211149, #50764 ) ;
#51141 = ORIENTED_EDGE ( 'NONE', *, *, #74453, .F. ) ;
#51143 = ORIENTED_EDGE ( 'NONE', *, *, #43298, .T. ) ;
#51142 = CARTESIAN_POINT ( 'NONE',  ( 20.85000000000000142, 6.846123162363745074, -171.2377262668498759 ) ) ;
#51144 = ORIENTED_EDGE ( 'NONE', *, *, #115859, .T. ) ;
#51145 = DIRECTION ( 'NONE',  ( 0.000000000000000000, -0.008583690987135041833, 0.9999631594459055250 ) ) ;
#51146 = DIRECTION ( 'NONE',  ( 1.000000000000000000, 0.000000000000000000, 0.000000000000000000 ) ) ;
#51148 = CARTESIAN_POINT ( 'NONE',  ( 18.49999999999999289, 11.75000000000000355, -8.099999999999999645 ) ) ;
#51147 = CARTESIAN_POINT ( 'NONE',  ( -16.77683809663752257, 14.15900158805613884, -219.2550725561364118 ) ) ;
#51149 = EDGE_LOOP ( 'NONE', ( #175988, #97930, #49930, #154547 ) ) ;
#51150 = ORIENTED_EDGE ( 'NONE', *, *, #166206, .T. ) ;
#51151 = FILL_AREA_STYLE_COLOUR ( '', #135321 ) ;
#51152 = DIRECTION ( 'NONE',  ( -0.7071067811865562325, -0.7071067811865388020, 0.000000000000000000 ) ) ;
#51153 = AXIS2_PLACEMENT_3D ( 'NONE', #71095, #133610, #230149 ) ;
#51154 = ORIENTED_EDGE ( 'NONE', *, *, #36669, .T. ) ;
#51155 = EDGE_LOOP ( 'NONE', ( #242542, #254870, #188337, #138643 ) ) ;
#51156 = DIRECTION ( 'NONE',  ( -0.000000000000000000, 0.9126074666063771490, 0.4088369013363281623 ) ) ;
#51157 = DIRECTION ( 'NONE',  ( 0.000000000000000000, -0.2128009952263604232, 0.9770955615653316162 ) ) ;
#51158 = CARTESIAN_POINT ( 'NONE',  ( 18.52130828395271678, 8.843855271129630324, -245.4074285112719451 ) ) ;
#51159 = CONICAL_SURFACE ( 'NONE', #213689, 6.250000000000005329, 0.7853981633974431720 ) ;
#51160 = FACE_OUTER_BOUND ( 'NONE', #234069, .T. ) ;
#51162 = EDGE_LOOP ( 'NONE', ( #246891, #77595, #144885, #2556 ) ) ;
#51161 = DIRECTION ( 'NONE',  ( 0.000000000000000000, 0.000000000000000000, 1.000000000000000000 ) ) ;
#51163 = FACE_OUTER_BOUND ( 'NONE', #98575, .T. ) ;
#51164 = DIRECTION ( 'NONE',  ( 0.000000000000000000, -0.008583690987135041833, 0.9999631594459055250 ) ) ;
#51165 = DIRECTION ( 'NONE',  ( 1.000000000000000000, 0.000000000000000000, 0.000000000000000000 ) ) ;
#51166 = CARTESIAN_POINT ( 'NONE',  ( 18.49713797159848383, 85.44648232759099926, -95.95164936291408253 ) ) ;
#51167 = ORIENTED_EDGE ( 'NONE', *, *, #45099, .F. ) ;
#51168 = CARTESIAN_POINT ( 'NONE',  ( 15.51872946208854920, 66.62341902196789079, -85.39616123751245880 ) ) ;
#51169 = DIRECTION ( 'NONE',  ( -1.000000000000000000, 0.000000000000000000, 0.000000000000000000 ) ) ;
#51170 = EDGE_CURVE ( 'NONE', #198148, #96525, #87638, .T. ) ;
#51172 = CARTESIAN_POINT ( 'NONE',  ( 21.05000000000000071, 10.42338541492406279, -40.99205192387010044 ) ) ;
#51171 = DIRECTION ( 'NONE',  ( 0.000000000000000000, 0.000000000000000000, -1.000000000000000000 ) ) ;
#51173 = DIRECTION ( 'NONE',  ( 0.1538461538461670663, 0.4665713331246195694, 0.8710008909599673554 ) ) ;
#51174 = CARTESIAN_POINT ( 'NONE',  ( 21.05000000000000071, 77.16270174994990327, -95.12310748452431142 ) ) ;
#51175 = CARTESIAN_POINT ( 'NONE',  ( 20.94999999999999929, 77.34915357198771346, -61.73561014893441978 ) ) ;
#51176 = CARTESIAN_POINT ( 'NONE',  ( 20.85000000000000142, 74.95904887477786360, -233.7774272632847783 ) ) ;
#51178 = EDGE_CURVE ( 'NONE', #71518, #81419, #154351, .T. ) ;
#51177 = DIRECTION ( 'NONE',  ( 1.000000000000000000, -1.836970198721029934E-16, -1.282749433769087582E-30 ) ) ;
#51179 = FACE_OUTER_BOUND ( 'NONE', #64857, .T. ) ;
#51180 = ORIENTED_EDGE ( 'NONE', *, *, #17661, .F. ) ;
#51181 = AXIS2_PLACEMENT_3D ( 'NONE', #103545, #243068, #64445 ) ;
#51182 = ORIENTED_EDGE ( 'NONE', *, *, #44064, .F. ) ;
#51183 = VERTEX_POINT ( 'NONE', #194075 ) ;
#51184 = ADVANCED_FACE ( 'NONE', ( #214894 ), #187637, .T. ) ;
#51185 = CARTESIAN_POINT ( 'NONE',  ( 20.52683494730046476, 67.01946918171053369, -94.51785476198718072 ) ) ;
#51186 = EDGE_CURVE ( 'NONE', #164707, #9130, #108333, .T. ) ;
#51187 = PLANE ( 'NONE',  #6919 ) ;
#51188 = ORIENTED_EDGE ( 'NONE', *, *, #12823, .T. ) ;
#51189 = ORIENTED_EDGE ( 'NONE', *, *, #253119, .F. ) ;
#51190 = AXIS2_PLACEMENT_3D ( 'NONE', #90706, #127279, #206815 ) ;
#51191 = EDGE_LOOP ( 'NONE', ( #211696, #8258, #14193, #229740 ) ) ;
#51192 = CARTESIAN_POINT ( 'NONE',  ( 20.94999999999999929, 76.00000000001145395, -38.92310748452432279 ) ) ;
#51193 = ORIENTED_EDGE ( 'NONE', *, *, #71784, .F. ) ;
#51194 = CIRCLE ( 'NONE', #26302, 0.8750000000000007772 ) ;
#51195 = EDGE_CURVE ( 'NONE', #96922, #42536, #141635, .T. ) ;
#51196 = DIRECTION ( 'NONE',  ( 0.000000000000000000, 0.000000000000000000, -1.000000000000000000 ) ) ;
#51197 = ADVANCED_FACE ( 'NONE', ( #117089 ), #217440, .T. ) ;
#51198 = DIRECTION ( 'NONE',  ( 0.000000000000000000, 0.000000000000000000, 1.000000000000000000 ) ) ;
#51199 = CARTESIAN_POINT ( 'NONE',  ( -23.25000000000000000, 7.128833340094563376, -233.7327013124401276 ) ) ;
#51200 = AXIS2_PLACEMENT_3D ( 'NONE', #125924, #235004, #132041 ) ;
#51201 = DIRECTION ( 'NONE',  ( 0.000000000000000000, 0.8814952561688437216, -0.4721928772777331806 ) ) ;
#51202 = CARTESIAN_POINT ( 'NONE',  ( -23.15000000000000213, 5.950000000011163692, -123.6942976949652149 ) ) ;
#51204 = ORIENTED_EDGE ( 'NONE', *, *, #62490, .F. ) ;
#51203 = CARTESIAN_POINT ( 'NONE',  ( -16.88783316861809070, 30.11618329224522128, -234.7587566525756415 ) ) ;
#51206 = CARTESIAN_POINT ( 'NONE',  ( 21.06086055315989114, 8.774707514967413857, -79.20232215515413543 ) ) ;
#51205 = DIRECTION ( 'NONE',  ( -0.000000000000000000, -0.03181660087581238833, 0.9994937237965575427 ) ) ;
#51207 = CARTESIAN_POINT ( 'NONE',  ( 20.94999999999999574, 0.000000000000000000, 0.000000000000000000 ) ) ;
#51208 = VERTEX_POINT ( 'NONE', #162637 ) ;
#51209 = CARTESIAN_POINT ( 'NONE',  ( 15.15590539855245744, 66.58931770574409370, -121.0919640425760804 ) ) ;
#51210 = CARTESIAN_POINT ( 'NONE',  ( -16.92989507731676468, 66.05000000001183480, -82.40560855391422024 ) ) ;
#51211 = DIRECTION ( 'NONE',  ( 1.000000000000000000, -2.952720810173289112E-16, -2.061873921506763405E-30 ) ) ;
#51212 = VERTEX_POINT ( 'NONE', #19263 ) ;
#51213 =( NAMED_UNIT ( * ) SI_UNIT ( $, .STERADIAN. ) SOLID_ANGLE_UNIT ( ) );
#51215 = FACE_OUTER_BOUND ( 'NONE', #174642, .T. ) ;
#51214 = CIRCLE ( 'NONE', #67809, 0.09999999999999892308 ) ;
#51216 = EDGE_CURVE ( 'NONE', #129923, #32161, #104383, .T. ) ;
#51217 = CIRCLE ( 'NONE', #118468, 0.1000000000000016709 ) ;
#51218 = DIRECTION ( 'NONE',  ( 1.000000000000000000, -0.000000000000000000, -0.000000000000000000 ) ) ;
#51219 = ADVANCED_FACE ( 'NONE', ( #161358 ), #38842, .T. ) ;
#51220 = ORIENTED_EDGE ( 'NONE', *, *, #124749, .F. ) ;
#51221 = DIRECTION ( 'NONE',  ( 1.000000000000000000, 0.000000000000000000, 0.000000000000000000 ) ) ;
#51222 = CARTESIAN_POINT ( 'NONE',  ( -22.47071067811865319, 0.09909245471376171288, -25.77992525550194003 ) ) ;
#51223 = DIRECTION ( 'NONE',  ( 1.000000000000000000, -7.304098846218134667E-16, -5.100424963727256530E-30 ) ) ;
#51224 = ORIENTED_EDGE ( 'NONE', *, *, #212538, .F. ) ;
#51225 = ORIENTED_EDGE ( 'NONE', *, *, #88365, .T. ) ;
#51226 = EDGE_CURVE ( 'NONE', #106961, #159851, #200473, .T. ) ;
#51227 = VECTOR ( 'NONE', #141374, 1000.000000000000114 ) ;
#51228 = AXIS2_PLACEMENT_3D ( 'NONE', #204983, #9364, #6806 ) ;
#51229 = AXIS2_PLACEMENT_3D ( 'NONE', #35007, #234432, #74124 ) ;
#51230 = EDGE_CURVE ( 'NONE', #214553, #105957, #123502, .T. ) ;
#51231 = CARTESIAN_POINT ( 'NONE',  ( -20.94999999999999929, -11.48912529307605901, -2.900000000000001688 ) ) ;
#51232 = CYLINDRICAL_SURFACE ( 'NONE', #231491, 0.09999999999999781286 ) ;
#51233 = CARTESIAN_POINT ( 'NONE',  ( 20.91682497891422798, 65.67736539654997330, -164.4625116876572406 ) ) ;
#51234 = CARTESIAN_POINT ( 'NONE',  ( 23.50000000000005684, 64.35000000001120668, -3.123107484524795474 ) ) ;
#51236 = FACE_OUTER_BOUND ( 'NONE', #17174, .T. ) ;
#51235 = DIRECTION ( 'NONE',  ( -1.000000000000000000, 0.000000000000000000, 0.000000000000000000 ) ) ;
#51237 = EDGE_CURVE ( 'NONE', #96257, #183594, #108696, .T. ) ;
#51238 = DIRECTION ( 'NONE',  ( 0.000000000000000000, -6.417474130781257643E-15, 1.000000000000000000 ) ) ;
#51239 = DIRECTION ( 'NONE',  ( 0.000000000000000000, 1.734723475976807292E-15, -1.000000000000000000 ) ) ;
#51240 = CARTESIAN_POINT ( 'NONE',  ( -18.40000000000000213, 33.85569253519368260, -235.0339796035492554 ) ) ;
#51241 = EDGE_LOOP ( 'NONE', ( #70715, #80161, #74035, #92426 ) ) ;
#51242 = CARTESIAN_POINT ( 'NONE',  ( -18.50000000000000000, 14.86477715130881272, -235.7932433709592601 ) ) ;
#51244 = ORIENTED_EDGE ( 'NONE', *, *, #106905, .F. ) ;
#51243 = DIRECTION ( 'NONE',  ( 0.000000000000000000, -1.000000000000000000, 0.000000000000000000 ) ) ;
#51245 = DIRECTION ( 'NONE',  ( -0.000000000000000000, -1.000000000000000000, -0.000000000000000000 ) ) ;
#51246 = CYLINDRICAL_SURFACE ( 'NONE', #15723, 0.1000000000000001443 ) ;
#51247 = CARTESIAN_POINT ( 'NONE',  ( -21.44999999999999929, 7.350000000011155166, -155.2500000000000284 ) ) ;
#51248 = CARTESIAN_POINT ( 'NONE',  ( -16.97683810757273193, 66.05000000001207638, -123.2595307720638971 ) ) ;
#51250 = ORIENTED_EDGE ( 'NONE', *, *, #67100, .F. ) ;
#51249 = CARTESIAN_POINT ( 'NONE',  ( 22.00356870141344601, 68.74575763752172008, -136.5231074845243597 ) ) ;
#51251 = DIRECTION ( 'NONE',  ( 0.000000000000000000, 1.000000000000000000, -6.308085367188393199E-16 ) ) ;
#51252 = CARTESIAN_POINT ( 'NONE',  ( 23.24999999999999645, 76.00000000001190870, -103.0231074845243029 ) ) ;
#51253 = ADVANCED_FACE ( 'NONE', ( #118377 ), #141809, .F. ) ;
#51254 = CARTESIAN_POINT ( 'NONE',  ( 22.57320508075687826, 11.75000000001115552, -67.00000000000004263 ) ) ;
#51255 = CARTESIAN_POINT ( 'NONE',  ( 20.94999999999999574, 10.52493806863738079, -207.3780514093641330 ) ) ;
#51256 = ORIENTED_EDGE ( 'NONE', *, *, #232609, .F. ) ;
#51257 = CARTESIAN_POINT ( 'NONE',  ( 20.94999999999999929, 4.999999999999997335, -21.09473398108690390 ) ) ;
#51258 = EDGE_LOOP ( 'NONE', ( #160491, #95687, #85758, #240370 ) ) ;
#51259 = EDGE_CURVE ( 'NONE', #205048, #116760, #58359, .T. ) ;
#51260 = AXIS2_PLACEMENT_3D ( 'NONE', #218055, #219352, #60277 ) ;
#51261 = AXIS2_PLACEMENT_3D ( 'NONE', #95451, #152899, #55020 ) ;
#51262 = ORIENTED_EDGE ( 'NONE', *, *, #194064, .F. ) ;
#51263 = CARTESIAN_POINT ( 'NONE',  ( -23.25000000000000000, 1.115600667400684642E-11, -167.4999999999999716 ) ) ;
#51264 = VERTEX_POINT ( 'NONE', #160083 ) ;
#51265 = DIRECTION ( 'NONE',  ( -0.000000000000000000, -6.982962677686266711E-15, 1.000000000000000000 ) ) ;
#51266 = CARTESIAN_POINT ( 'NONE',  ( -23.15000000000000213, 59.16775194334852728, -221.0793150863668473 ) ) ;
#51267 = AXIS2_PLACEMENT_3D ( 'NONE', #69457, #104668, #205072 ) ;
#51268 = CARTESIAN_POINT ( 'NONE',  ( 20.84999999999998721, 10.33248238083634440, -106.0948465439131922 ) ) ;
#51269 = ORIENTED_EDGE ( 'NONE', *, *, #97676, .T. ) ;
#51270 = AXIS2_PLACEMENT_3D ( 'NONE', #3808, #221540, #159057 ) ;
#51271 = CARTESIAN_POINT ( 'NONE',  ( -16.83558968593870731, 9.949999999999983302, -12.66230518761681445 ) ) ;
#51273 = AXIS2_PLACEMENT_3D ( 'NONE', #175260, #33183, #13588 ) ;
#51272 = LINE ( 'NONE', #109987, #174092 ) ;
#51274 = CARTESIAN_POINT ( 'NONE',  ( 20.94999999999999574, 67.07338541492552508, -195.0514244653012952 ) ) ;
#51275 = AXIS2_PLACEMENT_3D ( 'NONE', #156999, #14918, #33219 ) ;
#51276 = CIRCLE ( 'NONE', #205227, 0.2000000000000057288 ) ;
#51277 = DIRECTION ( 'NONE',  ( 0.000000000000000000, 0.6855225566104508061, 0.7280513885559666276 ) ) ;
#51278 = PLANE ( 'NONE',  #48758 ) ;
#51279 = ORIENTED_EDGE ( 'NONE', *, *, #35728, .T. ) ;
#51280 = DIRECTION ( 'NONE',  ( 1.000000000000000000, 0.000000000000000000, 0.000000000000000000 ) ) ;
#51281 = VERTEX_POINT ( 'NONE', #180912 ) ;
#51283 = ORIENTED_EDGE ( 'NONE', *, *, #67311, .T. ) ;
#51282 = DIRECTION ( 'NONE',  ( 1.000000000000000000, 0.000000000000000000, 0.000000000000000000 ) ) ;
#51284 = CIRCLE ( 'NONE', #97058, 2.099999999999990763 ) ;
#51285 = ORIENTED_EDGE ( 'NONE', *, *, #44385, .T. ) ;
#51286 = CARTESIAN_POINT ( 'NONE',  ( 18.45068634130097607, 85.48650607335541451, -196.4543290533561901 ) ) ;
#51287 = ORIENTED_EDGE ( 'NONE', *, *, #175888, .F. ) ;
#51288 = CARTESIAN_POINT ( 'NONE',  ( -18.34374000495059676, 11.47316190336247388, -24.25000000000001066 ) ) ;
#51289 = CARTESIAN_POINT ( 'NONE',  ( -21.05000000000000071, 77.26178616857734482, -161.9366085209788650 ) ) ;
#51290 = CARTESIAN_POINT ( 'NONE',  ( -22.45437739390953169, 76.00000000001173817, -81.17267829612076468 ) ) ;
#51291 = ORIENTED_EDGE ( 'NONE', *, *, #204960, .T. ) ;
#51292 = CARTESIAN_POINT ( 'NONE',  ( -16.94333152886235894, 66.00965798856158528, -123.9151390155787880 ) ) ;
#51293 = DIRECTION ( 'NONE',  ( -3.265361837132813093E-16, 1.000000000000000000, 0.000000000000000000 ) ) ;
#51295 = CARTESIAN_POINT ( 'NONE',  ( -20.94999999999999929, 76.00000000001213607, -136.5231074845243313 ) ) ;
#51294 = AXIS2_PLACEMENT_3D ( 'NONE', #130460, #47054, #146164 ) ;
#51296 = ORIENTED_EDGE ( 'NONE', *, *, #70947, .F. ) ;
#51297 = CIRCLE ( 'NONE', #251214, 0.1000000000000028644 ) ;
#51299 = EDGE_LOOP ( 'NONE', ( #197517, #191951, #221711, #205131 ) ) ;
#51298 = CARTESIAN_POINT ( 'NONE',  ( -21.05000000000000071, 72.06821323333463170, -225.0920403225231610 ) ) ;
#51300 = DIRECTION ( 'NONE',  ( -0.000000000000000000, 1.000000000000000000, -1.224646799147352961E-16 ) ) ;
#51301 = CARTESIAN_POINT ( 'NONE',  ( -23.24999999999999645, -9.599999999988845900, -107.1001893912220879 ) ) ;
#51302 = TOROIDAL_SURFACE ( 'NONE', #38868, 11.90000000000000391, 0.1000000000000000056 ) ;
#51303 = CIRCLE ( 'NONE', #42969, 0.09999999999999939493 ) ;
#51304 = ORIENTED_EDGE ( 'NONE', *, *, #136770, .F. ) ;
#51305 = AXIS2_PLACEMENT_3D ( 'NONE', #202350, #103228, #25024 ) ;
#51306 = VECTOR ( 'NONE', #33166, 1000.000000000000000 ) ;
#51307 = CARTESIAN_POINT ( 'NONE',  ( -21.05000000000000071, 68.13014604066189861, -227.7202878558733516 ) ) ;
#51308 = DIRECTION ( 'NONE',  ( 1.000000000000000000, 0.000000000000000000, 0.000000000000000000 ) ) ;
#51309 = CARTESIAN_POINT ( 'NONE',  ( -22.39999999999999858, 0.3085173699977072914, -229.9658011520297691 ) ) ;
#51310 = ORIENTED_EDGE ( 'NONE', *, *, #203286, .F. ) ;
#51311 = DIRECTION ( 'NONE',  ( 0.000000000000000000, -0.4999999999999608646, 0.8660254037844612451 ) ) ;
#51312 = EDGE_CURVE ( 'NONE', #75286, #111418, #71108, .T. ) ;
#51313 = CARTESIAN_POINT ( 'NONE',  ( -23.15000000000000213, 77.04701199367727327, -199.6625678998140359 ) ) ;
#51314 = ADVANCED_FACE ( 'NONE', ( #197891 ), #41417, .T. ) ;
#51315 = EDGE_CURVE ( 'NONE', #212402, #217199, #257817, .T. ) ;
#51316 = TOROIDAL_SURFACE ( 'NONE', #193013, 4.099999999999999645, 0.1000000000000000056 ) ;
#51317 = AXIS2_PLACEMENT_3D ( 'NONE', #157218, #93352, #73831 ) ;
#51318 = CIRCLE ( 'NONE', #30715, 0.5000000000000004441 ) ;
#51319 = AXIS2_PLACEMENT_3D ( 'NONE', #161461, #240984, #62351 ) ;
#51320 = ORIENTED_EDGE ( 'NONE', *, *, #169672, .T. ) ;
#51321 = CYLINDRICAL_SURFACE ( 'NONE', #161229, 0.1000000000000101918 ) ;
#51322 = ORIENTED_EDGE ( 'NONE', *, *, #145646, .T. ) ;
#51323 = DIRECTION ( 'NONE',  ( 0.000000000000000000, -0.9908441862701596881, -0.1350103645451901924 ) ) ;
#51324 = EDGE_CURVE ( 'NONE', #253084, #176862, #43960, .T. ) ;
#51325 = FACE_OUTER_BOUND ( 'NONE', #179683, .T. ) ;
#51327 = ORIENTED_EDGE ( 'NONE', *, *, #245359, .T. ) ;
#51326 = CARTESIAN_POINT ( 'NONE',  ( 15.06592377766032165, 25.11330806876552657, -232.6826121690050400 ) ) ;
#51328 = CARTESIAN_POINT ( 'NONE',  ( -23.25000000000000000, 77.83585931145600512, -158.5186683157258187 ) ) ;
#51329 = CARTESIAN_POINT ( 'NONE',  ( 21.05000000000000071, 10.42338541491290727, -7.492051923870097774 ) ) ;
#51330 = FACE_OUTER_BOUND ( 'NONE', #20154, .T. ) ;
#51331 = CARTESIAN_POINT ( 'NONE',  ( 21.05000000000000071, 6.299230910098046365, -33.40156250000000426 ) ) ;
#51332 = CARTESIAN_POINT ( 'NONE',  ( -18.50000000000000000, 30.22839164850006455, -235.6129688350293350 ) ) ;
#51333 = DIRECTION ( 'NONE',  ( 1.000000000000000000, 3.448943450116723568E-16, 6.438528483529607644E-16 ) ) ;
#51335 = VERTEX_POINT ( 'NONE', #238301 ) ;
#51334 = CARTESIAN_POINT ( 'NONE',  ( 21.14999999999999858, 11.65000000000000746, 11.75000000000000000 ) ) ;
#51336 = FACE_OUTER_BOUND ( 'NONE', #130559, .T. ) ;
#51337 = AXIS2_PLACEMENT_3D ( 'NONE', #78583, #179018, #254634 ) ;
#51338 = FACE_OUTER_BOUND ( 'NONE', #211447, .T. ) ;
#51339 = EDGE_CURVE ( 'NONE', #95768, #24665, #216829, .T. ) ;
#51340 = EDGE_CURVE ( 'NONE', #88954, #205524, #199191, .T. ) ;
#51341 = DIRECTION ( 'NONE',  ( -1.000000000000000000, -0.000000000000000000, -0.000000000000000000 ) ) ;
#51342 = CARTESIAN_POINT ( 'NONE',  ( -20.54999999999999716, 1.115600667400684642E-11, -67.00000000000004263 ) ) ;
#51343 = ORIENTED_EDGE ( 'NONE', *, *, #163327, .F. ) ;
#51344 = CARTESIAN_POINT ( 'NONE',  ( -15.75000000000000355, 9.850000000011133849, -83.75000000000004263 ) ) ;
#51346 = ADVANCED_FACE ( 'NONE', ( #100052 ), #2247, .T. ) ;
#51345 = CARTESIAN_POINT ( 'NONE',  ( -20.64999999999999858, 85.00000000001149658, -45.91707660717669626 ) ) ;
#51347 = ORIENTED_EDGE ( 'NONE', *, *, #82859, .T. ) ;
#51348 = CIRCLE ( 'NONE', #226332, 0.1000000000000028644 ) ;
#51349 = FACE_OUTER_BOUND ( 'NONE', #150009, .T. ) ;
#51350 = AXIS2_PLACEMENT_3D ( 'NONE', #165826, #43293, #245347 ) ;
#51351 = AXIS2_PLACEMENT_3D ( 'NONE', #85764, #186198, #224019 ) ;
#51352 = DIRECTION ( 'NONE',  ( 1.000000000000000000, 0.000000000000000000, 0.000000000000000000 ) ) ;
#51353 = ORIENTED_EDGE ( 'NONE', *, *, #23463, .T. ) ;
#51354 = LINE ( 'NONE', #224876, #73577 ) ;
#51355 = ORIENTED_EDGE ( 'NONE', *, *, #196005, .T. ) ;
#51356 = DIRECTION ( 'NONE',  ( 2.952720810173290098E-16, -0.4721928772777345129, -0.8814952561688431665 ) ) ;
#51358 = ORIENTED_EDGE ( 'NONE', *, *, #28610, .T. ) ;
#51357 = CARTESIAN_POINT ( 'NONE',  ( -20.64999999999999858, 4.590145742703442444, -213.0289728181953706 ) ) ;
#51359 = CARTESIAN_POINT ( 'NONE',  ( -18.79999999999999716, 11.49641995933507843, -1.885425182446133885 ) ) ;
#51360 = ADVANCED_FACE ( 'NONE', ( #182199 ), #142364, .F. ) ;
#51361 = ORIENTED_EDGE ( 'NONE', *, *, #29942, .T. ) ;
#51362 = CARTESIAN_POINT ( 'NONE',  ( -20.94999999999999929, -11.48912529306489994, -164.6000000000000227 ) ) ;
#51363 = VERTEX_POINT ( 'NONE', #67377 ) ;
#51365 = ORIENTED_EDGE ( 'NONE', *, *, #229567, .F. ) ;
#51364 = ORIENTED_EDGE ( 'NONE', *, *, #66953, .F. ) ;
#51366 = PLANE ( 'NONE',  #219506 ) ;
#51368 = ORIENTED_EDGE ( 'NONE', *, *, #133450, .T. ) ;
#51367 = DIRECTION ( 'NONE',  ( -6.938893903907222856E-15, -0.4088369013363283844, 0.9126074666063769270 ) ) ;
#51369 = CARTESIAN_POINT ( 'NONE',  ( 20.89192007715127986, 65.67101464000481315, -63.94043916224794089 ) ) ;
#51370 = VERTEX_POINT ( 'NONE', #145612 ) ;
#51371 = VECTOR ( 'NONE', #52952, 1000.000000000000000 ) ;
#51372 = AXIS2_PLACEMENT_3D ( 'NONE', #113168, #192715, #93606 ) ;
#51373 = VECTOR ( 'NONE', #238849, 1000.000000000000000 ) ;
#51374 = EDGE_CURVE ( 'NONE', #108499, #246752, #233598, .T. ) ;
#51375 = ORIENTED_EDGE ( 'NONE', *, *, #143766, .T. ) ;
#51376 = CARTESIAN_POINT ( 'NONE',  ( 21.05000000000000071, 1.115600667400684642E-11, -113.4750000000000369 ) ) ;
#51377 = CARTESIAN_POINT ( 'NONE',  ( 23.24999999999999645, 1.115600667400684642E-11, -67.00000000000004263 ) ) ;
#51378 = CARTESIAN_POINT ( 'NONE',  ( -18.47690164073606667, 38.09692775460474223, -261.0587226095922802 ) ) ;
#51379 = VERTEX_POINT ( 'NONE', #248578 ) ;
#51380 = ADVANCED_FACE ( 'NONE', ( #124791 ), #4806, .F. ) ;
#51382 = EDGE_CURVE ( 'NONE', #14355, #243100, #133624, .T. ) ;
#51381 = CARTESIAN_POINT ( 'NONE',  ( 23.24999999999999645, 11.75000000001113953, -143.2500000000000284 ) ) ;
#51383 = CARTESIAN_POINT ( 'NONE',  ( 20.97468175916167610, 65.37473483564055243, -57.26834604911160653 ) ) ;
#51384 = DIRECTION ( 'NONE',  ( -1.000000000000000000, 3.151514657663852580E-16, -8.547182517843351137E-17 ) ) ;
#51385 = CIRCLE ( 'NONE', #5603, 11.80000000000000959 ) ;
#51386 = VERTEX_POINT ( 'NONE', #184742 ) ;
#51387 = AXIS2_PLACEMENT_3D ( 'NONE', #103373, #180375, #4281 ) ;
#51388 = CARTESIAN_POINT ( 'NONE',  ( -20.94999999999999929, 74.16465844978765176, -124.8679561919613263 ) ) ;
#51389 = DIRECTION ( 'NONE',  ( 1.000000000000000000, 0.000000000000000000, 0.000000000000000000 ) ) ;
#51390 = CARTESIAN_POINT ( 'NONE',  ( 18.49999999999998934, 11.65000000001115943, -91.75000000000005684 ) ) ;
#51391 = CIRCLE ( 'NONE', #218000, 0.1999999999999987899 ) ;
#51392 = CARTESIAN_POINT ( 'NONE',  ( 18.49999999999999289, 57.93055674131822741, -245.5071546967800771 ) ) ;
#51393 = EDGE_LOOP ( 'NONE', ( #147326, #169971, #177538, #147509 ) ) ;
#51394 = B_SPLINE_CURVE_WITH_KNOTS ( 'NONE', 3,
 ( #196141, #197416, #34521, #96997, #193580, #14952, #94460, #18777 ),
 .UNSPECIFIED., .F., .F.,
 ( 4, 2, 2, 4 ),
 ( 0.000000000000000000, 6.534141206310459531E-05, 0.0001306828241262091906, 0.0002613656482524183812 ),
 .UNSPECIFIED. ) ;
#51395 = CARTESIAN_POINT ( 'NONE',  ( 22.49999999999998579, 0.1008583691098678958, -55.25043287651065071 ) ) ;
#51396 = ORIENTED_EDGE ( 'NONE', *, *, #199348, .T. ) ;
#51397 = DIRECTION ( 'NONE',  ( 6.484947573744954877E-15, 0.9858045116447881062, -0.1678971852675942011 ) ) ;
#51398 = ORIENTED_EDGE ( 'NONE', *, *, #40837, .T. ) ;
#51399 = EDGE_CURVE ( 'NONE', #138152, #90553, #196010, .T. ) ;
#51400 = EDGE_CURVE ( 'NONE', #191683, #216206, #8731, .T. ) ;
#51401 = DIRECTION ( 'NONE',  ( 0.000000000000000000, 7.056502275159890832E-15, -1.000000000000000000 ) ) ;
#51402 = DIRECTION ( 'NONE',  ( -1.000000000000000000, 0.000000000000000000, 0.000000000000000000 ) ) ;
#51404 = VERTEX_POINT ( 'NONE', #103906 ) ;
#51403 = AXIS2_PLACEMENT_3D ( 'NONE', #511, #216991, #237856 ) ;
#51405 = ORIENTED_EDGE ( 'NONE', *, *, #60144, .F. ) ;
#51406 = DIRECTION ( 'NONE',  ( 0.000000000000000000, 0.000000000000000000, 1.000000000000000000 ) ) ;
#51407 = ORIENTED_EDGE ( 'NONE', *, *, #73637, .T. ) ;
#51408 = ADVANCED_FACE ( 'NONE', ( #208188 ), #225140, .T. ) ;
#51409 = DIRECTION ( 'NONE',  ( -1.000000000000000000, -0.000000000000000000, -0.000000000000000000 ) ) ;
#51410 = AXIS2_PLACEMENT_3D ( 'NONE', #74423, #190504, #170967 ) ;
#51411 = AXIS2_PLACEMENT_3D ( 'NONE', #73, #234853, #56188 ) ;
#51412 = AXIS2_PLACEMENT_3D ( 'NONE', #239587, #139165, #19247 ) ;
#51413 = AXIS2_PLACEMENT_3D ( 'NONE', #52550, #205197, #86519 ) ;
#51414 = ORIENTED_EDGE ( 'NONE', *, *, #240523, .F. ) ;
#51415 = ADVANCED_FACE ( 'NONE', ( #84308 ), #121199, .T. ) ;
#51416 = EDGE_CURVE ( 'NONE', #38945, #137467, #137695, .T. ) ;
#51417 = ADVANCED_FACE ( 'NONE', ( #165193 ), #146886, .T. ) ;
#51418 = VERTEX_POINT ( 'NONE', #246018 ) ;
#51419 = DIRECTION ( 'NONE',  ( -0.000000000000000000, 0.9908441862701591329, 0.1350103645451946055 ) ) ;
#51420 = EDGE_CURVE ( 'NONE', #136449, #248593, #226422, .T. ) ;
#51421 = CARTESIAN_POINT ( 'NONE',  ( -16.79184697841823848, 22.98113411688375507, -230.9381109511705574 ) ) ;
#51422 = DIRECTION ( 'NONE',  ( 0.000000000000000000, 0.000000000000000000, 1.000000000000000000 ) ) ;
#51424 = ORIENTED_EDGE ( 'NONE', *, *, #58228, .F. ) ;
#51423 = CARTESIAN_POINT ( 'NONE',  ( -2.995603634470884209E-16, -11.75000000000000000, -12.25000000000000000 ) ) ;
#51425 = EDGE_CURVE ( 'NONE', #210821, #115244, #220914, .T. ) ;
#51426 = CARTESIAN_POINT ( 'NONE',  ( 20.94999999999999929, 69.35000000001254250, -182.2731074845244166 ) ) ;
#51427 = DIRECTION ( 'NONE',  ( 1.000000000000000000, 0.000000000000000000, 0.000000000000000000 ) ) ;
#51428 = EDGE_CURVE ( 'NONE', #100505, #135153, #96008, .T. ) ;
#51429 = DIRECTION ( 'NONE',  ( -1.652117596168391700E-15, -1.000000000000000000, 0.000000000000000000 ) ) ;
#51430 = CIRCLE ( 'NONE', #247263, 0.09999999999999939493 ) ;
#51432 = LINE ( 'NONE', #71053, #257384 ) ;
#51431 = CARTESIAN_POINT ( 'NONE',  ( -18.58735405345342073, -9.566478620325447935, -140.8227146462660357 ) ) ;
#51433 = CARTESIAN_POINT ( 'NONE',  ( -23.15000000000000213, 11.36448785225375602, -246.7787679937655980 ) ) ;
#51435 = EDGE_CURVE ( 'NONE', #66750, #218042, #24427, .T. ) ;
#51434 = DIRECTION ( 'NONE',  ( 0.000000000000000000, -0.9654727137038715545, 0.2605042016806676242 ) ) ;
#51436 = AXIS2_PLACEMENT_3D ( 'NONE', #146130, #23658, #165725 ) ;
#51437 = DIRECTION ( 'NONE',  ( 0.000000000000000000, 0.4088369013363281623, -0.9126074666063771490 ) ) ;
#51438 = B_SPLINE_CURVE_WITH_KNOTS ( 'NONE', 3,
 ( #13402, #92910, #232461, #113764, #134594, #155505, #193319, #216718 ),
 .UNSPECIFIED., .F., .F.,
 ( 4, 2, 2, 4 ),
 ( 0.000000000000000000, 0.0002114466876442107866, 0.0003171700314663170473, 0.0004228933752884233622 ),
 .UNSPECIFIED. ) ;
#51439 = CARTESIAN_POINT ( 'NONE',  ( 12.25000000000000000, 9.350000000011140955, -184.2499999999999716 ) ) ;
#51440 = ORIENTED_EDGE ( 'NONE', *, *, #23683, .F. ) ;
#51441 = AXIS2_PLACEMENT_3D ( 'NONE', #191873, #52304, #172328 ) ;
#51442 = ORIENTED_EDGE ( 'NONE', *, *, #92571, .T. ) ;
#51443 = AXIS2_PLACEMENT_3D ( 'NONE', #14326, #93826, #13039 ) ;
#51444 = ORIENTED_EDGE ( 'NONE', *, *, #86594, .T. ) ;
#51445 = ADVANCED_FACE ( 'NONE', ( #106470 ), #92065, .F. ) ;
#51446 = CARTESIAN_POINT ( 'NONE',  ( -22.50000000000000000, -1.330006220153263641, -194.8931527402181700 ) ) ;
#51447 = FACE_OUTER_BOUND ( 'NONE', #97920, .T. ) ;
#51448 = ORIENTED_EDGE ( 'NONE', *, *, #222121, .F. ) ;
#51449 = AXIS2_PLACEMENT_3D ( 'NONE', #180360, #239045, #1700 ) ;
#51450 = SURFACE_STYLE_FILL_AREA ( #88012 ) ;
#51451 = CARTESIAN_POINT ( 'NONE',  ( -20.85000000000000142, -11.74999999998884448, -67.00000000000000000 ) ) ;
#51452 = CIRCLE ( 'NONE', #39048, 0.1000000000000028644 ) ;
#51453 = TOROIDAL_SURFACE ( 'NONE', #234662, 0.2000000000000000111, 0.1000000000000000056 ) ;
#51454 = PRODUCT_DEFINITION_SHAPE ( 'NONE', 'NONE',  #206229 ) ;
#51455 = DIRECTION ( 'NONE',  ( 1.000000000000000000, 0.000000000000000000, 0.000000000000000000 ) ) ;
#51456 = ORIENTED_EDGE ( 'NONE', *, *, #21302, .T. ) ;
#51457 = ORIENTED_EDGE ( 'NONE', *, *, #213636, .T. ) ;
#51458 = VECTOR ( 'NONE', #35711, 1000.000000000000000 ) ;
#51459 = CARTESIAN_POINT ( 'NONE',  ( 21.14261333020286671, 60.09565987114967811, -221.2273593472489779 ) ) ;
#51460 = DIRECTION ( 'NONE',  ( 0.000000000000000000, 0.000000000000000000, -1.000000000000000000 ) ) ;
#51461 = ORIENTED_EDGE ( 'NONE', *, *, #184211, .F. ) ;
#51462 = CARTESIAN_POINT ( 'NONE',  ( 21.59780538579342135, 0.09897866960914131207, -93.65290947005678390 ) ) ;
#51464 = ORIENTED_EDGE ( 'NONE', *, *, #146012, .T. ) ;
#51463 = CARTESIAN_POINT ( 'NONE',  ( 21.15000000000005187, 87.50449464844290048, -34.18759587077607165 ) ) ;
#51465 = DIRECTION ( 'NONE',  ( 0.000000000000000000, 0.000000000000000000, 1.000000000000000000 ) ) ;
#51466 = VECTOR ( 'NONE', #172214, 1000.000000000000000 ) ;
#51468 = ORIENTED_EDGE ( 'NONE', *, *, #31393, .F. ) ;
#51467 = CYLINDRICAL_SURFACE ( 'NONE', #98024, 0.1000000000000028644 ) ;
#51469 = DIRECTION ( 'NONE',  ( 0.000000000000000000, 7.086529944415894657E-15, -1.000000000000000000 ) ) ;
#51470 = DIRECTION ( 'NONE',  ( 0.000000000000000000, 0.000000000000000000, -1.000000000000000000 ) ) ;
#51471 = DIRECTION ( 'NONE',  ( 0.000000000000000000, 0.8700118002898322711, -0.4930308989875231696 ) ) ;
#51472 = AXIS2_PLACEMENT_3D ( 'NONE', #138017, #115917, #160199 ) ;
#51473 = ADVANCED_FACE ( 'NONE', ( #192461 ), #166995, .T. ) ;
#51475 = CARTESIAN_POINT ( 'NONE',  ( 20.87631937322880304, 10.47149503677605509, -108.0797458745812065 ) ) ;
#51474 = CARTESIAN_POINT ( 'NONE',  ( 18.59999999999999787, 77.73670573947892137, -24.50568489690058627 ) ) ;
#51476 = CARTESIAN_POINT ( 'NONE',  ( 23.14999999999999503, 14.05000000001115623, -161.9863049292391111 ) ) ;
#51477 = CARTESIAN_POINT ( 'NONE',  ( -18.48179518609409655, 85.51832530050660353, -163.1334019077635276 ) ) ;
#51478 = EDGE_CURVE ( 'NONE', #204167, #178200, #210738, .T. ) ;
#51479 = CARTESIAN_POINT ( 'NONE',  ( -21.05000000000000071, -1.261786168553869603, -41.58649896354548048 ) ) ;
#51480 = DIRECTION ( 'NONE',  ( 0.000000000000000000, 0.000000000000000000, 1.000000000000000000 ) ) ;
#51481 = AXIS2_PLACEMENT_3D ( 'NONE', #145407, #227512, #74902 ) ;
#51483 = ORIENTED_EDGE ( 'NONE', *, *, #8264, .F. ) ;
#51482 = AXIS2_PLACEMENT_3D ( 'NONE', #12301, #69702, #128378 ) ;
#51484 = CARTESIAN_POINT ( 'NONE',  ( -17.27223548804523645, 10.34539739142215886, -78.36639382080713290 ) ) ;
#51485 = CIRCLE ( 'NONE', #168097, 0.1000000000000033223 ) ;
#51486 = ORIENTED_EDGE ( 'NONE', *, *, #79162, .F. ) ;
#51487 = FACE_OUTER_BOUND ( 'NONE', #91891, .T. ) ;
#51488 = ORIENTED_EDGE ( 'NONE', *, *, #54816, .T. ) ;
#51489 = DIRECTION ( 'NONE',  ( 0.000000000000000000, -0.03181660087583042251, 0.9994937237965568766 ) ) ;
#51490 = ADVANCED_FACE ( 'NONE', ( #252411 ), #231596, .T. ) ;
#51491 = DIRECTION ( 'NONE',  ( 0.000000000000000000, 6.982962677686266711E-15, -1.000000000000000000 ) ) ;
#51492 = ORIENTED_EDGE ( 'NONE', *, *, #113019, .T. ) ;
#51493 = CARTESIAN_POINT ( 'NONE',  ( -18.50000000000000000, 65.70729864260955821, -30.56574559737245167 ) ) ;
#51494 = ADVANCED_FACE ( 'NONE', ( #54218 ), #62723, .F. ) ;
#51495 = AXIS2_PLACEMENT_3D ( 'NONE', #120400, #83757, #199916 ) ;
#51496 = AXIS2_PLACEMENT_3D ( 'NONE', #126749, #246685, #148893 ) ;
#51497 = ORIENTED_EDGE ( 'NONE', *, *, #159489, .T. ) ;
#51498 = AXIS2_PLACEMENT_3D ( 'NONE', #198669, #20053, #99539 ) ;
#51499 = EDGE_LOOP ( 'NONE', ( #174658, #12258, #159551, #91355 ) ) ;
#51500 = ADVANCED_BREP_SHAPE_REPRESENTATION ( '', ( #198479, #2425 ), #210534 ) ;
#51501 = DIRECTION ( 'NONE',  ( 0.000000000000000000, 0.000000000000000000, -1.000000000000000000 ) ) ;
#51502 = CARTESIAN_POINT ( 'NONE',  ( 21.05000000000000071, 10.72371710471868056, -41.16491356908760935 ) ) ;
#51503 = CARTESIAN_POINT ( 'NONE',  ( -23.25000000000000000, 14.70949956575304185, -235.9560995168023112 ) ) ;
#51504 = DIRECTION ( 'NONE',  ( 0.000000000000000000, 0.7035695228903320331, 0.7106264324241468033 ) ) ;
#51505 = CARTESIAN_POINT ( 'NONE',  ( -23.25000000000000000, 62.42744096235649920, -225.1319887738535499 ) ) ;
#51507 = LINE ( 'NONE', #230173, #245115 ) ;
#51506 = DIRECTION ( 'NONE',  ( 0.000000000000000000, -0.000000000000000000, -1.000000000000000000 ) ) ;
#51508 = CARTESIAN_POINT ( 'NONE',  ( -13.22483237240078324, 9.436674251854004325, -82.17686193099926584 ) ) ;
#51510 = ORIENTED_EDGE ( 'NONE', *, *, #119112, .F. ) ;
#51509 = CARTESIAN_POINT ( 'NONE',  ( -22.94999999999999929, 0.000000000000000000, 0.000000000000000000 ) ) ;
#51512 = DIRECTION ( 'NONE',  ( 1.713247197920696616E-14, -0.9876197685951263461, 0.1568667991644794590 ) ) ;
#51511 = CARTESIAN_POINT ( 'NONE',  ( 20.77526135991775291, 8.932009016633136511, -75.46856854272438397 ) ) ;
#51513 = DIRECTION ( 'NONE',  ( -0.000000000000000000, 1.000000000000000000, -0.000000000000000000 ) ) ;
#51514 = ORIENTED_EDGE ( 'NONE', *, *, #75089, .T. ) ;
#51515 = CARTESIAN_POINT ( 'NONE',  ( -18.48550754432035959, -9.463399778548783559, -174.5487897524151037 ) ) ;
#51516 = DIRECTION ( 'NONE',  ( 1.000000000000000000, 0.000000000000000000, -0.000000000000000000 ) ) ;
#51517 = FACE_OUTER_BOUND ( 'NONE', #201211, .T. ) ;
#51518 = VERTEX_POINT ( 'NONE', #171650 ) ;
#51519 = FACE_OUTER_BOUND ( 'NONE', #172681, .T. ) ;
#51520 = CARTESIAN_POINT ( 'NONE',  ( -18.47653818581421703, 78.23178856761811062, -231.4551785763766816 ) ) ;
#51521 = VERTEX_POINT ( 'NONE', #212040 ) ;
#51522 = ORIENTED_EDGE ( 'NONE', *, *, #60833, .F. ) ;
#51523 = AXIS2_PLACEMENT_3D ( 'NONE', #156880, #137272, #18622 ) ;
#51524 = LINE ( 'NONE', #88086, #228472 ) ;
#51525 = DIRECTION ( 'NONE',  ( -1.000000000000000000, 0.000000000000000000, 0.000000000000000000 ) ) ;
#51526 = DIRECTION ( 'NONE',  ( 0.000000000000000000, 0.000000000000000000, -1.000000000000000000 ) ) ;
#51527 = CARTESIAN_POINT ( 'NONE',  ( -20.89192007715127986, 10.32898536001801304, -206.5826683222763904 ) ) ;
#51528 = EDGE_LOOP ( 'NONE', ( #108943, #48543, #113860 ) ) ;
#51529 = EDGE_CURVE ( 'NONE', #193883, #90989, #13823, .T. ) ;
#51530 = FACE_OUTER_BOUND ( 'NONE', #35030, .T. ) ;
#51531 = ADVANCED_FACE ( 'NONE', ( #234142 ), #71249, .F. ) ;
#51532 = FACE_OUTER_BOUND ( 'NONE', #236483, .T. ) ;
#51533 = CARTESIAN_POINT ( 'NONE',  ( 18.59999999999999787, -11.74999999998883737, -88.35000000000003695 ) ) ;
#51534 = AXIS2_PLACEMENT_3D ( 'NONE', #69681, #189620, #249594 ) ;
#51536 = ORIENTED_EDGE ( 'NONE', *, *, #257500, .T. ) ;
#51535 = AXIS2_PLACEMENT_3D ( 'NONE', #181225, #202056, #23449 ) ;
#51537 = LINE ( 'NONE', #11170, #42698 ) ;
#51538 = AXIS2_PLACEMENT_3D ( 'NONE', #158644, #59472, #80323 ) ;
#51539 = ADVANCED_FACE ( 'NONE', ( #155925 ), #46145, .T. ) ;
#51541 = ORIENTED_EDGE ( 'NONE', *, *, #48747, .F. ) ;
#51540 = CARTESIAN_POINT ( 'NONE',  ( -17.73285935862584495, 65.14201819622915934, -193.2816692942934651 ) ) ;
#51542 = DIRECTION ( 'NONE',  ( 0.000000000000000000, -1.000000000000000000, 0.000000000000000000 ) ) ;
#51543 = DIRECTION ( 'NONE',  ( 1.000000000000000000, 0.000000000000000000, 0.000000000000000000 ) ) ;
#51544 = CYLINDRICAL_SURFACE ( 'NONE', #1183, 0.09999999999999939493 ) ;
#51545 = DIRECTION ( 'NONE',  ( 0.000000000000000000, 0.000000000000000000, 1.000000000000000000 ) ) ;
#51546 = EDGE_CURVE ( 'NONE', #15592, #198025, #248769, .T. ) ;
#51547 = ORIENTED_EDGE ( 'NONE', *, *, #250668, .F. ) ;
#51548 = FACE_OUTER_BOUND ( 'NONE', #46433, .T. ) ;
#51549 = EDGE_CURVE ( 'NONE', #128131, #24547, #150217, .T. ) ;
#51550 = DIRECTION ( 'NONE',  ( 0.000000000000000000, 0.000000000000000000, 1.000000000000000000 ) ) ;
#51551 = FACE_OUTER_BOUND ( 'NONE', #65860, .T. ) ;
#51552 = ORIENTED_EDGE ( 'NONE', *, *, #106748, .F. ) ;
#51553 = FACE_OUTER_BOUND ( 'NONE', #254407, .T. ) ;
#51554 = DIRECTION ( 'NONE',  ( 1.000000000000000000, -0.000000000000000000, -0.000000000000000000 ) ) ;
#51555 = VECTOR ( 'NONE', #38219, 1000.000000000000000 ) ;
#51556 = ADVANCED_FACE ( 'NONE', ( #76339 ), #195710, .T. ) ;
#51557 = CARTESIAN_POINT ( 'NONE',  ( 21.07928932188134397, 6.328516656404468144, -167.4011048543455615 ) ) ;
#51558 = AXIS2_PLACEMENT_3D ( 'NONE', #36200, #74057, #14066 ) ;
#51559 = CARTESIAN_POINT ( 'NONE',  ( 20.95512820512820440, 65.37615131629972609, -61.85819391543678591 ) ) ;
#51560 = ORIENTED_EDGE ( 'NONE', *, *, #130522, .T. ) ;
#51561 = VERTEX_POINT ( 'NONE', #101008 ) ;
#51563 = DIRECTION ( 'NONE',  ( 1.000000000000000000, 3.265361837132813093E-16, -0.000000000000000000 ) ) ;
#51562 = CIRCLE ( 'NONE', #1517, 0.09999999999999939493 ) ;
#51564 = PLANE ( 'NONE',  #76638 ) ;
#51565 = SPHERICAL_SURFACE ( 'NONE', #187323, 0.1000000000000000056 ) ;
#51566 = EDGE_CURVE ( 'NONE', #122006, #145044, #225182, .T. ) ;
#51567 = CARTESIAN_POINT ( 'NONE',  ( -20.94684162483048695, 38.09882622057443058, -236.0309084375098223 ) ) ;
#51568 = CARTESIAN_POINT ( 'NONE',  ( -23.25000000000000000, 11.60058429089262333, -246.3380203656811887 ) ) ;
#51569 = DIRECTION ( 'NONE',  ( 0.7071067811865463515, -0.7071067811865487940, 4.930380657631324879E-32 ) ) ;
#51570 = CIRCLE ( 'NONE', #118256, 0.09999999999999939493 ) ;
#51571 = CIRCLE ( 'NONE', #201442, 11.74999999999999645 ) ;
#51572 = CARTESIAN_POINT ( 'NONE',  ( -22.50000000000000000, 31.85509083104287598, -238.8280249686205536 ) ) ;
#51573 = VECTOR ( 'NONE', #114840, 1000.000000000000000 ) ;
#51574 = SPHERICAL_SURFACE ( 'NONE', #257850, 0.1000000000000000056 ) ;
#51575 = CIRCLE ( 'NONE', #180808, 0.09999999999999939493 ) ;
#51576 = CARTESIAN_POINT ( 'NONE',  ( -21.14999999999999858, 12.67709964810648238, -223.3751320524553705 ) ) ;
#51577 = ORIENTED_EDGE ( 'NONE', *, *, #181541, .F. ) ;
#51578 = DIRECTION ( 'NONE',  ( 0.000000000000000000, 0.000000000000000000, 1.000000000000000000 ) ) ;
#51579 = CIRCLE ( 'NONE', #230705, 0.09999999999999939493 ) ;
#51580 = VERTEX_POINT ( 'NONE', #59326 ) ;
#51581 = CYLINDRICAL_SURFACE ( 'NONE', #26904, 0.8750000000000007772 ) ;
#51582 = CARTESIAN_POINT ( 'NONE',  ( -16.87036670365549895, 12.52461233780749872, -211.1164619086576408 ) ) ;
#51583 = DIRECTION ( 'NONE',  ( 0.000000000000000000, 0.000000000000000000, -1.000000000000000000 ) ) ;
#51585 = AXIS2_PLACEMENT_3D ( 'NONE', #156629, #137023, #60039 ) ;
#51584 = DIRECTION ( 'NONE',  ( 0.000000000000000000, 0.01283462868040404978, 0.9999176327611370985 ) ) ;
#51586 = CARTESIAN_POINT ( 'NONE',  ( -21.05000000000000071, 76.00000000001165290, -69.52310748452431710 ) ) ;
#51587 = FACE_OUTER_BOUND ( 'NONE', #699, .T. ) ;
#51588 = TOROIDAL_SURFACE ( 'NONE', #126640, 11.65000000000000036, 0.1000000000000000056 ) ;
#51589 = CARTESIAN_POINT ( 'NONE',  ( -20.64999999999999858, 7.150000000011155876, -45.85000000000000142 ) ) ;
#51590 = ORIENTED_EDGE ( 'NONE', *, *, #201517, .F. ) ;
#51592 = CARTESIAN_POINT ( 'NONE',  ( 21.05000000000000071, -9.399999999988844834, -90.60603087734760663 ) ) ;
#51591 = AXIS2_PLACEMENT_3D ( 'NONE', #97439, #177039, #196565 ) ;
#51593 = FACE_OUTER_BOUND ( 'NONE', #220017, .T. ) ;
#51594 = CARTESIAN_POINT ( 'NONE',  ( -21.05000000000000071, 6.400000000011158541, -76.93042463006162279 ) ) ;
#51595 = CYLINDRICAL_SURFACE ( 'NONE', #14504, 0.09999999999999939493 ) ;
#51596 = DIRECTION ( 'NONE',  ( 0.000000000000000000, -0.9651348961777157509, 0.2617529984165028467 ) ) ;
#51597 = ADVANCED_FACE ( 'NONE', ( #116768 ), #136302, .F. ) ;
#51598 = ORIENTED_EDGE ( 'NONE', *, *, #237240, .F. ) ;
#51599 = CARTESIAN_POINT ( 'NONE',  ( 5.900000000000059863, 64.35000000001120668, -26.12310748452479103 ) ) ;
#51600 = CARTESIAN_POINT ( 'NONE',  ( 20.85000000000000142, 70.22889768795992893, -198.1282601183952750 ) ) ;
#51601 = ORIENTED_EDGE ( 'NONE', *, *, #23377, .T. ) ;
#51602 = EDGE_CURVE ( 'NONE', #3343, #209120, #154686, .T. ) ;
#51603 = ORIENTED_EDGE ( 'NONE', *, *, #130079, .T. ) ;
#51604 = CARTESIAN_POINT ( 'NONE',  ( 18.50000000000000000, -9.399999999988843058, -174.3820418481727188 ) ) ;
#51605 = CIRCLE ( 'NONE', #143220, 11.75000000000001066 ) ;
#51606 = EDGE_CURVE ( 'NONE', #154148, #152529, #201439, .T. ) ;
#51607 = ORIENTED_EDGE ( 'NONE', *, *, #159789, .F. ) ;
#51609 = ADVANCED_FACE ( 'NONE', ( #58058 ), #256206, .F. ) ;
#51608 = DIRECTION ( 'NONE',  ( -1.000000000000000000, -0.000000000000000000, -0.000000000000000000 ) ) ;
#51610 = CARTESIAN_POINT ( 'NONE',  ( 18.79999999999999716, 1.350000000000000089, 21.90000000000000213 ) ) ;
#51611 = VECTOR ( 'NONE', #61956, 1000.000000000000000 ) ;
#51613 = VERTEX_POINT ( 'NONE', #159759 ) ;
#51612 = CIRCLE ( 'NONE', #5647, 0.09999999999999907574 ) ;
#51615 = DIRECTION ( 'NONE',  ( 0.000000000000000000, 0.000000000000000000, -1.000000000000000000 ) ) ;
#51614 = TOROIDAL_SURFACE ( 'NONE', #122603, 11.70000000000000639, 0.1000000000000000056 ) ;
#51616 = CIRCLE ( 'NONE', #84946, 0.09999999999999736877 ) ;
#51617 = EDGE_LOOP ( 'NONE', ( #250262, #106505, #129477, #32321 ) ) ;
#51618 = DIRECTION ( 'NONE',  ( 0.000000000000000000, 0.000000000000000000, -1.000000000000000000 ) ) ;
#51619 = ADVANCED_FACE ( 'NONE', ( #180603, #240574, #1939 ), #197582, .F. ) ;
#51620 = DIRECTION ( 'NONE',  ( 0.000000000000000000, 0.000000000000000000, -1.000000000000000000 ) ) ;
#51623 = ORIENTED_EDGE ( 'NONE', *, *, #169377, .F. ) ;
#51622 =( BOUNDED_SURFACE ( )  B_SPLINE_SURFACE ( 3, 2, ( 
 ( #980, #23177, #102656 ),
 ( #182237, #3576, #83080 ),
 ( #162671, #242189, #143080 ),
 ( #150800, #47825, #247323 ),
 ( #191242, #30890, #189931 ),
 ( #246058, #12600, #29602 ) ),
 .UNSPECIFIED., .F., .F., .F. ) 
 B_SPLINE_SURFACE_WITH_KNOTS ( ( 4, 2, 4 ),
 ( 3, 3 ),
 ( 3.141592653589783346, 3.926990816987233845, 4.712388980384684345 ),
 ( 0.000000000000000000, 1.000000000000000000 ),
 .UNSPECIFIED. ) 
 GEOMETRIC_REPRESENTATION_ITEM ( )  RATIONAL_B_SPLINE_SURFACE ( (
 ( 1.000000000000000000, 0.9238795325112774126, 1.000000000000000000),
 ( 1.000000000000000000, 0.9240297172242109003, 1.000000000000000000),
 ( 1.000000000000000000, 0.9038128468041503050, 1.000000000000000000),
 ( 1.000000000000000000, 0.8282379607647244457, 1.000000000000000000),
 ( 1.000000000000000000, 0.7727932973492797064, 1.000000000000000000),
 ( 1.000000000000000000, 0.7071067811865843211, 1.000000000000000000) ) ) 
 REPRESENTATION_ITEM ( '' )  SURFACE ( )  );
#51621 = CARTESIAN_POINT ( 'NONE',  ( -21.05000000000000071, 1.115600667400684642E-11, -134.0000000000000000 ) ) ;
#51624 = DIRECTION ( 'NONE',  ( 0.000000000000000000, 0.000000000000000000, 1.000000000000000000 ) ) ;
#51626 = AXIS2_PLACEMENT_3D ( 'NONE', #174169, #92011, #72471 ) ;
#51625 = DIRECTION ( 'NONE',  ( 0.000000000000000000, 1.000000000000000000, 0.000000000000000000 ) ) ;
#51627 = ADVANCED_FACE ( 'NONE', ( #157213, #141468 ), #78901, .F. ) ;
#51628 = CARTESIAN_POINT ( 'NONE',  ( -20.94999999999999929, 65.70711192142388768, -131.0651054685122574 ) ) ;
#51629 = DIRECTION ( 'NONE',  ( 0.000000000000000000, -6.982962677686266711E-15, 1.000000000000000000 ) ) ;
#51630 = DIRECTION ( 'NONE',  ( 0.000000000000000000, 0.000000000000000000, 1.000000000000000000 ) ) ;
#51631 = VECTOR ( 'NONE', #44267, 1000.000000000000000 ) ;
#51632 = DIRECTION ( 'NONE',  ( -0.000000000000000000, 0.9126074666063771490, 0.4088369013363281623 ) ) ;
#51633 = CIRCLE ( 'NONE', #130781, 0.1000000000000124678 ) ;
#51635 = ORIENTED_EDGE ( 'NONE', *, *, #15774, .T. ) ;
#51634 = DIRECTION ( 'NONE',  ( 0.000000000000000000, -0.2605042016806740079, 0.9654727137038698892 ) ) ;
#51636 = B_SPLINE_CURVE_WITH_KNOTS ( 'NONE', 3,
 ( #238254, #154909, #235687, #55738, #256477, #233160, #135296 ),
 .UNSPECIFIED., .F., .F.,
 ( 4, 3, 4 ),
 ( 0.000000000000000000, 4.520325912680430423E-05, 5.794988040901246848E-05 ),
 .UNSPECIFIED. ) ;
#51638 = EDGE_LOOP ( 'NONE', ( #132788, #88966, #254042, #200561 ) ) ;
#51637 = PRODUCT_RELATED_PRODUCT_CATEGORY ( 'part', '', ( #172353 ) ) ;
#51640 = CARTESIAN_POINT ( 'NONE',  ( 20.95512820512820440, 8.876151316299271343, -42.05862899514094977 ) ) ;
#51639 = FACE_OUTER_BOUND ( 'NONE', #144763, .T. ) ;
#51641 = CIRCLE ( 'NONE', #239116, 0.5000000000000004441 ) ;
#51643 = ORIENTED_EDGE ( 'NONE', *, *, #7681, .T. ) ;
#51642 = DIRECTION ( 'NONE',  ( -1.000000000000000000, 0.000000000000000000, 0.000000000000000000 ) ) ;
#51644 = ORIENTED_EDGE ( 'NONE', *, *, #194335, .F. ) ;
#51645 = CARTESIAN_POINT ( 'NONE',  ( -18.39999999999999858, 77.13860723519891849, -241.8264964602989266 ) ) ;
#51646 = CARTESIAN_POINT ( 'NONE',  ( -20.54999999999999716, 68.85000000001203091, -119.7731074845243597 ) ) ;
#51647 = CIRCLE ( 'NONE', #18365, 0.1999999999999987899 ) ;
#51648 =( BOUNDED_SURFACE ( )  B_SPLINE_SURFACE ( 3, 2, ( 
 ( #205413, #86743, #106304 ),
 ( #166341, #245844, #240285 ),
 ( #83723, #119049, #59025 ),
 ( #64206, #103308, #5482 ),
 ( #180301, #182889, #44646 ),
 ( #39539, #163313, #201141 ) ),
 .UNSPECIFIED., .F., .F., .F. ) 
 B_SPLINE_SURFACE_WITH_KNOTS ( ( 4, 2, 4 ),
 ( 3, 3 ),
 ( 0.0001381104793128073169, 0.0002947094729387728746, 0.0004513084665647384324 ),
 ( 0.000000000000000000, 1.000000000000000000 ),
 .UNSPECIFIED. ) 
 GEOMETRIC_REPRESENTATION_ITEM ( )  RATIONAL_B_SPLINE_SURFACE ( (
 ( 1.000000000000000000, 0.7071067811865229258, 1.000000000000000000),
 ( 1.000000000000000000, 0.6919563088098916737, 1.000000000000000000),
 ( 1.000000000000000000, 0.6959445945717528392, 1.000000000000000000),
 ( 1.000000000000000000, 0.7137882985313381834, 1.000000000000000000),
 ( 1.000000000000000000, 0.7257496306096212768, 1.000000000000000000),
 ( 1.000000000000000000, 0.7250110520819876836, 1.000000000000000000) ) ) 
 REPRESENTATION_ITEM ( '' )  SURFACE ( )  );
#51650 = EDGE_CURVE ( 'NONE', #231082, #153266, #146279, .T. ) ;
#51649 = DIRECTION ( 'NONE',  ( 1.000000000000000000, 0.000000000000000000, 0.000000000000000000 ) ) ;
#51651 = DIRECTION ( 'NONE',  ( -1.000000000000000000, 0.000000000000000000, 0.000000000000000000 ) ) ;
#51652 = ADVANCED_FACE ( 'NONE', ( #220994 ), #82742, .F. ) ;
#51653 = ADVANCED_FACE ( 'NONE', ( #119350 ), #167174, .T. ) ;
#51654 = CARTESIAN_POINT ( 'NONE',  ( -18.57399277249657032, 67.49230083716666684, -195.4236814984208479 ) ) ;
#51655 = CIRCLE ( 'NONE', #5876, 0.4000000000000010214 ) ;
#51656 = CARTESIAN_POINT ( 'NONE',  ( 21.72449340488910252, 10.28395627750227526, -143.2500000000000284 ) ) ;
#51657 = CARTESIAN_POINT ( 'NONE',  ( -23.39999999999994529, 76.00000000001119815, -31.87310748452479459 ) ) ;
#51658 = VECTOR ( 'NONE', #247084, 1000.000000000000000 ) ;
#51659 = ORIENTED_EDGE ( 'NONE', *, *, #226672, .F. ) ;
#51660 = ORIENTED_EDGE ( 'NONE', *, *, #112100, .T. ) ;
#51661 = FACE_OUTER_BOUND ( 'NONE', #68273, .T. ) ;
#51662 = ORIENTED_EDGE ( 'NONE', *, *, #46920, .F. ) ;
#51663 = DIRECTION ( 'NONE',  ( 0.000000000000000000, -0.8068669527897506244, -0.5907332058516622242 ) ) ;
#51664 = ORIENTED_EDGE ( 'NONE', *, *, #255859, .F. ) ;
#51666 = AXIS2_PLACEMENT_3D ( 'NONE', #206054, #105639, #229477 ) ;
#51665 = CARTESIAN_POINT ( 'NONE',  ( 18.54999999999999716, 9.950000000011153034, -87.85000000000010800 ) ) ;
#51667 =( BOUNDED_CURVE ( )  B_SPLINE_CURVE ( 3, ( #50326, #226394, #92038, #148162 ),
 .UNSPECIFIED., .F., .T. ) 
 B_SPLINE_CURVE_WITH_KNOTS ( ( 4, 4 ),
 ( 5.733388419619902088, 5.983100554402347449 ),
 .UNSPECIFIED. ) 
 CURVE ( )  GEOMETRIC_REPRESENTATION_ITEM ( )  RATIONAL_B_SPLINE_CURVE ( ( 1.000000000000000000, 0.9948104011409417691, 0.9948104011409417691, 1.000000000000000000 ) ) 
 REPRESENTATION_ITEM ( '' )  );
#51668 = CIRCLE ( 'NONE', #147565, 11.70000000000000462 ) ;
#51669 = CIRCLE ( 'NONE', #93203, 0.1000000000000028644 ) ;
#51670 = FACE_OUTER_BOUND ( 'NONE', #182009, .T. ) ;
#51671 = CYLINDRICAL_SURFACE ( 'NONE', #89916, 0.1000000000000028644 ) ;
#51672 = VERTEX_POINT ( 'NONE', #3224 ) ;
#51673 = CARTESIAN_POINT ( 'NONE',  ( 18.59999999999999076, 43.44873802792533013, -245.1397081572968659 ) ) ;
#51674 = ORIENTED_EDGE ( 'NONE', *, *, #7954, .T. ) ;
#51675 = PLANE ( 'NONE',  #243919 ) ;
#51676 = ADVANCED_FACE ( 'NONE', ( #60630 ), #236702, .F. ) ;
#51677 = CARTESIAN_POINT ( 'NONE',  ( 18.59999994388910238, 9.037544858871804365, -245.3775128972792174 ) ) ;
#51678 = EDGE_LOOP ( 'NONE', ( #191704, #18630, #32914, #212625 ) ) ;
#51679 = LINE ( 'NONE', #131244, #40322 ) ;
#51680 = VERTEX_POINT ( 'NONE', #98443 ) ;
#51683 = ORIENTED_EDGE ( 'NONE', *, *, #183844, .F. ) ;
#51682 = CARTESIAN_POINT ( 'NONE',  ( 18.51697539158856998, 46.41023286455060770, -243.0722154975327385 ) ) ;
#51681 = CARTESIAN_POINT ( 'NONE',  ( -20.05000000000000426, 9.250000000011157297, -188.7499999999999716 ) ) ;
#51684 = AXIS2_PLACEMENT_3D ( 'NONE', #221669, #143433, #122613 ) ;
#51685 = TOROIDAL_SURFACE ( 'NONE', #193204, 0.2000000000000000111, 0.1000000000000000056 ) ;
#51686 = CARTESIAN_POINT ( 'NONE',  ( -23.15000000000000213, 61.57587952878035509, -212.2000740415318774 ) ) ;
#51687 = AXIS2_PLACEMENT_3D ( 'NONE', #216646, #73325, #214085 ) ;
#51688 = ORIENTED_EDGE ( 'NONE', *, *, #60474, .F. ) ;
#51689 = VERTEX_POINT ( 'NONE', #89197 ) ;
#51690 = ADVANCED_FACE ( 'NONE', ( #29283 ), #25487, .F. ) ;
#51691 = CARTESIAN_POINT ( 'NONE',  ( -20.54999999999999716, 19.35378350773087419, -238.0802544632095987 ) ) ;
#51692 = ORIENTED_EDGE ( 'NONE', *, *, #77341, .F. ) ;
#51693 = DIRECTION ( 'NONE',  ( 1.000000000000000000, 0.000000000000000000, -0.000000000000000000 ) ) ;
#51694 = LINE ( 'NONE', #29628, #134312 ) ;
#51695 = CARTESIAN_POINT ( 'NONE',  ( 18.52643265882457868, 67.49293571122092317, -195.4648732548341741 ) ) ;
#51696 = EDGE_CURVE ( 'NONE', #42405, #95482, #233068, .T. ) ;
#51697 = FACE_OUTER_BOUND ( 'NONE', #132990, .T. ) ;
#51698 = ORIENTED_EDGE ( 'NONE', *, *, #178132, .F. ) ;
#51699 = EDGE_CURVE ( 'NONE', #138262, #197443, #184446, .T. ) ;
#51700 = DIRECTION ( 'NONE',  ( -0.000000000000000000, 0.9274965247785350586, 0.3738317757009704811 ) ) ;
#51701 = CARTESIAN_POINT ( 'NONE',  ( 18.44444291854881612, 86.89436330702220346, -199.6093833839856870 ) ) ;
#51702 = CARTESIAN_POINT ( 'NONE',  ( -13.54795643572458808, 66.54933111084471875, -154.9675609943170400 ) ) ;
#51703 = ORIENTED_EDGE ( 'NONE', *, *, #166281, .F. ) ;
#51704 = CARTESIAN_POINT ( 'NONE',  ( 23.14999999999999503, 36.02367271998545561, -235.8812521208699309 ) ) ;
#51705 = ORIENTED_EDGE ( 'NONE', *, *, #55553, .F. ) ;
#51706 = CYLINDRICAL_SURFACE ( 'NONE', #181533, 0.09999999999999939493 ) ;
#51707 = VERTEX_POINT ( 'NONE', #63199 ) ;
#51708 = ADVANCED_FACE ( 'NONE', ( #106177 ), #4611, .F. ) ;
#51709 = AXIS2_PLACEMENT_3D ( 'NONE', #246347, #207233, #111983 ) ;
#51710 = EDGE_CURVE ( 'NONE', #2800, #232714, #137885, .T. ) ;
#51711 = CARTESIAN_POINT ( 'NONE',  ( -18.59999999999999787, 74.83729825007462466, -195.4231074845243654 ) ) ;
#51712 = DIRECTION ( 'NONE',  ( 1.000000000000000000, -0.000000000000000000, -0.000000000000000000 ) ) ;
#51714 = ORIENTED_EDGE ( 'NONE', *, *, #150660, .F. ) ;
#51713 = SPHERICAL_SURFACE ( 'NONE', #90275, 0.1000000000000000056 ) ;
#51715 = DIRECTION ( 'NONE',  ( 1.000000000000000000, 0.000000000000000000, 0.000000000000000000 ) ) ;
#51716 = ORIENTED_EDGE ( 'NONE', *, *, #28131, .F. ) ;
#51717 = CARTESIAN_POINT ( 'NONE',  ( -20.54999999999999716, 1.115600667400684642E-11, -100.5000000000000426 ) ) ;
#51718 = CARTESIAN_POINT ( 'NONE',  ( -16.92280123533722858, 9.950000000011137047, -113.3506323140851464 ) ) ;
#51719 = ORIENTED_EDGE ( 'NONE', *, *, #184448, .F. ) ;
#51720 = CARTESIAN_POINT ( 'NONE',  ( -21.29999999999995808, 1.115600667400684642E-11, -167.4999999999999716 ) ) ;
#51721 = CARTESIAN_POINT ( 'NONE',  ( 20.73486653747088226, 7.250000000011182166, -79.65000000000004832 ) ) ;
#51722 = ORIENTED_EDGE ( 'NONE', *, *, #160460, .T. ) ;
#51724 = CARTESIAN_POINT ( 'NONE',  ( -16.93262454970420094, 10.00202046794151300, -146.5729237737627102 ) ) ;
#51723 = AXIS2_PLACEMENT_3D ( 'NONE', #205996, #27400, #121368 ) ;
#51725 = EDGE_CURVE ( 'NONE', #237228, #411, #245716, .T. ) ;
#51726 = AXIS2_PLACEMENT_3D ( 'NONE', #134052, #192767, #235722 ) ;
#51727 = EDGE_CURVE ( 'NONE', #252613, #7494, #54706, .T. ) ;
#51728 = EDGE_LOOP ( 'NONE', ( #215816, #62853, #130353, #147900 ) ) ;
#51729 = AXIS2_PLACEMENT_3D ( 'NONE', #185263, #6616, #9188 ) ;
#51730 = AXIS2_PLACEMENT_3D ( 'NONE', #41278, #119513, #158655 ) ;
#51731 = CARTESIAN_POINT ( 'NONE',  ( 12.93279065517212878, 9.417690691074257714, -118.6416006967646410 ) ) ;
#51732 = DIRECTION ( 'NONE',  ( -1.000000000000000000, -0.000000000000000000, -0.000000000000000000 ) ) ;
#51733 = EDGE_CURVE ( 'NONE', #1074, #177806, #50393, .T. ) ;
#51736 = VERTEX_POINT ( 'NONE', #147911 ) ;
#51735 = VERTEX_POINT ( 'NONE', #224852 ) ;
#51734 = LINE ( 'NONE', #90885, #242889 ) ;
#51737 = CARTESIAN_POINT ( 'NONE',  ( -20.94999999999999929, 67.23127455305835554, -235.8551265064784559 ) ) ;
#51738 = DIRECTION ( 'NONE',  ( 1.000000000000000000, 7.304098846218135653E-16, 5.100424963727256530E-30 ) ) ;
#51739 = ADVANCED_FACE ( 'NONE', ( #188300 ), #46216, .F. ) ;
#51740 = CARTESIAN_POINT ( 'NONE',  ( 20.12500000000000355, 66.74195072709457577, -94.65976864738193797 ) ) ;
#51741 = VECTOR ( 'NONE', #254350, 1000.000000000000000 ) ;
#51743 = CARTESIAN_POINT ( 'NONE',  ( -15.57281606413133801, 66.62934494888806114, -51.99728422854350640 ) ) ;
#51742 = CARTESIAN_POINT ( 'NONE',  ( -23.15000000000000213, 76.00000000001205080, -123.7481074845242972 ) ) ;
#51744 = CARTESIAN_POINT ( 'NONE',  ( 21.14999999999999858, 1.658775325997237315, -230.6916041481598540 ) ) ;
#51746 = EDGE_CURVE ( 'NONE', #163852, #201338, #250342, .T. ) ;
#51745 = CYLINDRICAL_SURFACE ( 'NONE', #52721, 0.1000000000000028644 ) ;
#51747 = CARTESIAN_POINT ( 'NONE',  ( -20.94999999999999929, 4.252251777740766236, -211.8999245327126744 ) ) ;
#51748 = AXIS2_PLACEMENT_3D ( 'NONE', #98671, #17885, #177006 ) ;
#51749 = CARTESIAN_POINT ( 'NONE',  ( 20.84999999999998721, 87.75000000001190870, -103.0231074845242176 ) ) ;
#51750 = ORIENTED_EDGE ( 'NONE', *, *, #111064, .F. ) ;
#51751 = ORIENTED_EDGE ( 'NONE', *, *, #205647, .F. ) ;
#51752 = CIRCLE ( 'NONE', #234955, 0.1000000000000028644 ) ;
#51753 = CARTESIAN_POINT ( 'NONE',  ( -21.14999999999999858, 69.45934304831071415, -102.9231074845243512 ) ) ;
#51755 = ORIENTED_EDGE ( 'NONE', *, *, #49874, .T. ) ;
#51754 = CARTESIAN_POINT ( 'NONE',  ( 21.04999999999999716, 10.68430915749624077, -175.0266967903268096 ) ) ;
#51756 = ORIENTED_EDGE ( 'NONE', *, *, #196185, .T. ) ;
#51757 = SPHERICAL_SURFACE ( 'NONE', #210122, 0.1000000000000000056 ) ;
#51758 = ORIENTED_EDGE ( 'NONE', *, *, #118426, .T. ) ;
#51759 = CARTESIAN_POINT ( 'NONE',  ( 20.97468175916166899, 43.49871072350438084, -234.8442676856975879 ) ) ;
#51760 = EDGE_CURVE ( 'NONE', #82125, #175678, #229506, .T. ) ;
#51761 = EDGE_CURVE ( 'NONE', #177294, #16167, #117068, .T. ) ;
#51762 = CIRCLE ( 'NONE', #85073, 1.749999999999998002 ) ;
#51763 = B_SPLINE_CURVE_WITH_KNOTS ( 'NONE', 3,
 ( #38933, #118474, #98853, #119762, #41507, #199287 ),
 .UNSPECIFIED., .F., .F.,
 ( 4, 2, 4 ),
 ( 0.000000000000000000, 0.0001895189928937356105, 0.0003790379857874712211 ),
 .UNSPECIFIED. ) ;
#51764 = AXIS2_PLACEMENT_3D ( 'NONE', #183160, #207880, #25381 ) ;
#51765 = ORIENTED_EDGE ( 'NONE', *, *, #109033, .T. ) ;
#51766 = CIRCLE ( 'NONE', #5991, 0.09999999999999939493 ) ;
#51767 = CARTESIAN_POINT ( 'NONE',  ( 18.59999999999999076, 10.49142135624846439, -125.2500000000000284 ) ) ;
#51768 = CARTESIAN_POINT ( 'NONE',  ( -22.59999999999999787, 0.1008583690987122083, 11.74956712348939192 ) ) ;
#51769 = AXIS2_PLACEMENT_3D ( 'NONE', #125477, #204982, #184150 ) ;
#51771 = VERTEX_POINT ( 'NONE', #222261 ) ;
#51770 = VERTEX_POINT ( 'NONE', #144027 ) ;
#51772 = ORIENTED_EDGE ( 'NONE', *, *, #167134, .T. ) ;
#51773 = ORIENTED_EDGE ( 'NONE', *, *, #140895, .F. ) ;
#51774 = ORIENTED_EDGE ( 'NONE', *, *, #110074, .T. ) ;
#51776 = DIRECTION ( 'NONE',  ( 0.000000000000000000, -0.2617529984165031243, -0.9651348961777157509 ) ) ;
#51775 = VECTOR ( 'NONE', #180983, 1000.000000000000114 ) ;
#51777 = DIRECTION ( 'NONE',  ( 0.000000000000000000, 0.8814952561688430555, -0.4721928772777346239 ) ) ;
#51778 = CARTESIAN_POINT ( 'NONE',  ( -14.77538296656415184, 9.436662931810239741, -185.8230367322947814 ) ) ;
#51780 = ORIENTED_EDGE ( 'NONE', *, *, #138812, .T. ) ;
#51779 = CARTESIAN_POINT ( 'NONE',  ( -18.59999999999999787, 64.25000000001158185, -57.37310748452440379 ) ) ;
#51781 = DIRECTION ( 'NONE',  ( -1.000000000000000000, 2.952720810173289112E-16, 2.061873921506763405E-30 ) ) ;
#51782 = DIRECTION ( 'NONE',  ( 1.000000000000000000, 0.000000000000000000, 0.000000000000000000 ) ) ;
#51784 = ORIENTED_EDGE ( 'NONE', *, *, #234632, .F. ) ;
#51783 = FACE_OUTER_BOUND ( 'NONE', #32252, .T. ) ;
#51785 = DIRECTION ( 'NONE',  ( 0.7071067811865474617, 0.7071067811865474617, -0.000000000000000000 ) ) ;
#51786 = ORIENTED_EDGE ( 'NONE', *, *, #11175, .T. ) ;
#51787 = AXIS2_PLACEMENT_3D ( 'NONE', #186107, #110409, #189960 ) ;
#51788 = DIRECTION ( 'NONE',  ( 1.000000000000000000, 0.000000000000000000, 0.000000000000000000 ) ) ;
#51789 = CIRCLE ( 'NONE', #18503, 0.1000000000000028644 ) ;
#51790 = ORIENTED_EDGE ( 'NONE', *, *, #233988, .F. ) ;
#51791 = VECTOR ( 'NONE', #10925, 1000.000000000000000 ) ;
#51792 = CARTESIAN_POINT ( 'NONE',  ( 18.39999999999999858, 78.33723480602354527, -231.5810597241785729 ) ) ;
#51793 = DIRECTION ( 'NONE',  ( 0.2834754621636358940, -0.2834754621636437211, 0.9161240771326893961 ) ) ;
#51794 = ORIENTED_EDGE ( 'NONE', *, *, #124086, .F. ) ;
#51795 = CARTESIAN_POINT ( 'NONE',  ( 18.49999999999999289, 65.70729864261026876, -131.0657455973724836 ) ) ;
#51796 = CARTESIAN_POINT ( 'NONE',  ( -18.59999999999999787, 65.66751761918722252, -164.4282609406112670 ) ) ;
#51797 = ADVANCED_FACE ( 'NONE', ( #8399 ), #87892, .T. ) ;
#51798 = DIRECTION ( 'NONE',  ( -1.073024830501117725E-15, 0.2128009952263604232, -0.9770955615653316162 ) ) ;
#51799 = DIRECTION ( 'NONE',  ( 0.000000000000000000, 0.000000000000000000, -1.000000000000000000 ) ) ;
#51800 = ORIENTED_EDGE ( 'NONE', *, *, #230181, .T. ) ;
#51801 = VERTEX_POINT ( 'NONE', #223558 ) ;
#51802 = LINE ( 'NONE', #72703, #26330 ) ;
#51803 = CARTESIAN_POINT ( 'NONE',  ( 20.09999999999999787, 63.27875933230978234, -213.1799721866121047 ) ) ;
#51804 = ORIENTED_EDGE ( 'NONE', *, *, #82417, .F. ) ;
#51805 = DIRECTION ( 'NONE',  ( 1.000000000000000000, 2.952720810173289112E-16, -0.000000000000000000 ) ) ;
#51806 = ORIENTED_EDGE ( 'NONE', *, *, #112093, .F. ) ;
#51807 = CARTESIAN_POINT ( 'NONE',  ( -22.45354308602430038, 2.198891012223663321E-07, -55.24956710953974692 ) ) ;
#51808 = CARTESIAN_POINT ( 'NONE',  ( 20.85000000000000142, 43.53458741986632674, -253.2342671440096922 ) ) ;
#51809 = SPHERICAL_SURFACE ( 'NONE', #128316, 0.1000000000000000056 ) ;
#51810 = CIRCLE ( 'NONE', #97585, 1.500000000000001332 ) ;
#51811 = VECTOR ( 'NONE', #62619, 1000.000000000000000 ) ;
#51812 = VERTEX_POINT ( 'NONE', #9668 ) ;
#51813 = CARTESIAN_POINT ( 'NONE',  ( -16.81744102076748959, 63.08573235307424198, -213.1276215869287967 ) ) ;
#51814 = ADVANCED_FACE ( 'NONE', ( #43664 ), #123198, .T. ) ;
#51815 = AXIS2_PLACEMENT_3D ( 'NONE', #2248, #19265, #98758 ) ;
#51816 = VERTEX_POINT ( 'NONE', #210457 ) ;
#51817 = ORIENTED_EDGE ( 'NONE', *, *, #5590, .F. ) ;
#51818 = ORIENTED_EDGE ( 'NONE', *, *, #240178, .T. ) ;
#51819 = CARTESIAN_POINT ( 'NONE',  ( -23.25000000000000000, 2.000000000011154189, -87.27537807723794572 ) ) ;
#51820 = CARTESIAN_POINT ( 'NONE',  ( -23.25000000000000000, 7.675662554762638479, -241.7139905447625381 ) ) ;
#51821 = AXIS2_PLACEMENT_3D ( 'NONE', #31019, #110512, #233059 ) ;
#51822 = CARTESIAN_POINT ( 'NONE',  ( -21.09813707148783735, 0.03135149954059197192, -127.6149378942633348 ) ) ;
#51823 = DIRECTION ( 'NONE',  ( 1.000000000000000000, 0.000000000000000000, 0.000000000000000000 ) ) ;
#51824 = CARTESIAN_POINT ( 'NONE',  ( -20.94999999999999929, 1.162701749949165642, -108.4000000000000341 ) ) ;
#51826 = CARTESIAN_POINT ( 'NONE',  ( -21.14999999999999858, 64.27847795353595473, -247.1247091181747066 ) ) ;
#51825 = DIRECTION ( 'NONE',  ( 1.186688945009010077E-16, 1.000000000000000000, 6.982962677686266711E-15 ) ) ;
#51828 = EDGE_LOOP ( 'NONE', ( #198949, #23881, #128491, #221927 ) ) ;
#51827 = DIRECTION ( 'NONE',  ( -1.000000000000000000, 0.000000000000000000, 0.000000000000000000 ) ) ;
#51829 = CARTESIAN_POINT ( 'NONE',  ( -22.01447462590973103, 10.47144741134476931, -227.2829313272817444 ) ) ;
#51830 = ORIENTED_EDGE ( 'NONE', *, *, #15029, .F. ) ;
#51831 = AXIS2_PLACEMENT_3D ( 'NONE', #147849, #86545, #227366 ) ;
#51832 = CARTESIAN_POINT ( 'NONE',  ( -14.11697426661281440, 9.457410944778567696, -149.0000839737900549 ) ) ;
#51833 = ORIENTED_EDGE ( 'NONE', *, *, #209889, .T. ) ;
#51834 = ORIENTED_EDGE ( 'NONE', *, *, #186549, .F. ) ;
#51835 = CARTESIAN_POINT ( 'NONE',  ( -16.93415306273742260, 66.00437773999901481, -48.61305054216397536 ) ) ;
#51836 = VECTOR ( 'NONE', #81596, 1000.000000000000000 ) ;
#51837 = DIRECTION ( 'NONE',  ( 0.000000000000000000, -1.000000000000000000, -6.982962677686265922E-15 ) ) ;
#51838 = CARTESIAN_POINT ( 'NONE',  ( -21.05000000000000071, 76.09999996531227850, -210.0006596670181409 ) ) ;
#51839 = CARTESIAN_POINT ( 'NONE',  ( -23.15000000000000213, -9.000000000000001776, -24.10603087734756045 ) ) ;
#51840 = CIRCLE ( 'NONE', #14473, 1.899999999999993028 ) ;
#51841 = CARTESIAN_POINT ( 'NONE',  ( 20.93302460841142931, 18.38637412622486877, -236.9471295141160283 ) ) ;
#51842 = ORIENTED_EDGE ( 'NONE', *, *, #218304, .F. ) ;
#51843 = VERTEX_POINT ( 'NONE', #154366 ) ;
#51844 = FACE_OUTER_BOUND ( 'NONE', #35646, .T. ) ;
#51845 = ORIENTED_EDGE ( 'NONE', *, *, #88560, .F. ) ;
#51846 = CARTESIAN_POINT ( 'NONE',  ( 23.14999999999999503, 69.35000000001254250, -182.2731074845244166 ) ) ;
#51847 = CARTESIAN_POINT ( 'NONE',  ( 21.05000000000000071, 67.23127455305835554, -235.8551265064784559 ) ) ;
#51848 = ORIENTED_EDGE ( 'NONE', *, *, #72051, .T. ) ;
#51849 = CARTESIAN_POINT ( 'NONE',  ( -18.59999999999999787, 78.48087866980282001, -232.8271061603568910 ) ) ;
#51851 = VECTOR ( 'NONE', #250450, 1000.000000000000000 ) ;
#51850 = CARTESIAN_POINT ( 'NONE',  ( -20.99551997958364069, 11.75000000001110756, -60.15165913768996120 ) ) ;
#51852 = LINE ( 'NONE', #213509, #169662 ) ;
#51853 = DIRECTION ( 'NONE',  ( 0.000000000000000000, 0.4558084472153119959, -0.8900778951570285091 ) ) ;
#51854 = ORIENTED_EDGE ( 'NONE', *, *, #57582, .F. ) ;
#51855 = CARTESIAN_POINT ( 'NONE',  ( 22.57856590037849287, 76.00412833007608526, -81.27316594719980003 ) ) ;
#51856 = CARTESIAN_POINT ( 'NONE',  ( 22.88900146558018989, 8.703904791123973084, -121.3500000000000227 ) ) ;
#51857 = CARTESIAN_POINT ( 'NONE',  ( -21.29999999999995808, 7.128833340093095217, -233.7327013124392749 ) ) ;
#51858 = CIRCLE ( 'NONE', #226235, 0.1000000000000106498 ) ;
#51859 = CARTESIAN_POINT ( 'NONE',  ( 22.39999999999999503, 64.35000000001194564, -103.0231074845244024 ) ) ;
#51860 = EDGE_CURVE ( 'NONE', #95323, #99517, #93054, .T. ) ;
#51861 = CARTESIAN_POINT ( 'NONE',  ( -20.97625342178426067, 57.84918772564461875, -226.1321410197392368 ) ) ;
#51862 = AXIS2_PLACEMENT_3D ( 'NONE', #143186, #84460, #139327 ) ;
#51863 = CIRCLE ( 'NONE', #143457, 2.000000000000001776 ) ;
#51864 = VERTEX_POINT ( 'NONE', #133473 ) ;
#51865 = CIRCLE ( 'NONE', #255846, 0.09999999999999711897 ) ;
#51866 = ADVANCED_FACE ( 'NONE', ( #51330 ), #35688, .F. ) ;
#51867 = CARTESIAN_POINT ( 'NONE',  ( 21.05000000000000071, 10.72371711692550100, -12.17623960113813020 ) ) ;
#51868 = VERTEX_POINT ( 'NONE', #110049 ) ;
#51869 = CARTESIAN_POINT ( 'NONE',  ( 14.87567385445977131, 66.56923500458995591, -154.7925700897740455 ) ) ;
#51870 = PLANE ( 'NONE',  #96020 ) ;
#51871 = EDGE_CURVE ( 'NONE', #99952, #155667, #71293, .T. ) ;
#51872 = DIRECTION ( 'NONE',  ( -1.000000000000000000, 0.000000000000000000, 0.000000000000000000 ) ) ;
#51873 = CARTESIAN_POINT ( 'NONE',  ( -20.85000000000000142, -11.64999999998884306, -100.5000000000000426 ) ) ;
#51874 = LINE ( 'NONE', #70206, #175710 ) ;
#51875 = DIRECTION ( 'NONE',  ( 0.000000000000000000, 0.000000000000000000, -1.000000000000000000 ) ) ;
#51876 = ORIENTED_EDGE ( 'NONE', *, *, #252747, .T. ) ;
#51877 = CARTESIAN_POINT ( 'NONE',  ( -16.89146115310546037, 66.04855675435534579, -82.16828506557017420 ) ) ;
#51878 = CARTESIAN_POINT ( 'NONE',  ( 22.47071067811865674, 10.68684811775432841, -226.8807012965928607 ) ) ;
#51879 = CARTESIAN_POINT ( 'NONE',  ( 21.15000000000005542, 87.50449464844290048, -37.85861909827351468 ) ) ;
#51880 = EDGE_CURVE ( 'NONE', #106685, #109071, #99553, .T. ) ;
#51881 = VECTOR ( 'NONE', #234286, 1000.000000000000000 ) ;
#51882 = DIRECTION ( 'NONE',  ( 0.000000000000000000, 0.000000000000000000, -1.000000000000000000 ) ) ;
#51883 = VERTEX_POINT ( 'NONE', #214296 ) ;
#51884 = VERTEX_POINT ( 'NONE', #211741 ) ;
#51885 = LINE ( 'NONE', #246267, #162434 ) ;
#51886 = DIRECTION ( 'NONE',  ( 0.000000000000000000, 0.2128009952263604232, -0.9770955615653316162 ) ) ;
#51887 = CARTESIAN_POINT ( 'NONE',  ( 20.94999999999999574, 1.849084418638171856, -45.15601052144712213 ) ) ;
#51889 = FACE_OUTER_BOUND ( 'NONE', #132625, .T. ) ;
#51888 = AXIS2_PLACEMENT_3D ( 'NONE', #116087, #193055, #213887 ) ;
#51890 = CARTESIAN_POINT ( 'NONE',  ( -16.86337532320262156, 44.03295079807835322, -235.3120272856442625 ) ) ;
#51891 = EDGE_CURVE ( 'NONE', #246179, #57491, #46304, .T. ) ;
#51892 = ORIENTED_EDGE ( 'NONE', *, *, #56964, .F. ) ;
#51893 = DIRECTION ( 'NONE',  ( -0.000000000000000000, 1.000000000000000000, -0.000000000000000000 ) ) ;
#51894 = DIRECTION ( 'NONE',  ( 0.000000000000000000, 0.9908441862701605762, -0.1350103645451835310 ) ) ;
#51895 = VERTEX_POINT ( 'NONE', #112629 ) ;
#51896 = DIRECTION ( 'NONE',  ( -3.035766082959430717E-14, 0.2128009952263604232, -0.9770955615653316162 ) ) ;
#51897 = CIRCLE ( 'NONE', #256430, 0.09999999999999939493 ) ;
#51898 = CIRCLE ( 'NONE', #1832, 0.1999999999999987899 ) ;
#51899 = EDGE_LOOP ( 'NONE', ( #229769, #229779, #253223, #47502 ) ) ;
#51900 = ORIENTED_EDGE ( 'NONE', *, *, #155228, .F. ) ;
#51901 = VERTEX_POINT ( 'NONE', #252125 ) ;
#51902 = DIRECTION ( 'NONE',  ( 1.000000000000000000, 0.000000000000000000, 0.000000000000000000 ) ) ;
#51903 = FACE_OUTER_BOUND ( 'NONE', #133679, .T. ) ;
#51904 = FACE_OUTER_BOUND ( 'NONE', #20765, .T. ) ;
#51905 = ADVANCED_FACE ( 'NONE', ( #150481 ), #30541, .F. ) ;
#51906 = CARTESIAN_POINT ( 'NONE',  ( 18.46905048506369340, -9.473744257371240707, -140.6759862922554589 ) ) ;
#51907 = PLANE ( 'NONE',  #148832 ) ;
#51908 = DIRECTION ( 'NONE',  ( -0.000000000000000000, -6.982962677686266711E-15, 1.000000000000000000 ) ) ;
#51909 = CARTESIAN_POINT ( 'NONE',  ( 21.05000000000000071, 76.00000000001237765, -170.0231074845243597 ) ) ;
#51911 = CARTESIAN_POINT ( 'NONE',  ( -21.05000000000000071, 74.63912941282003999, -128.4501095574333647 ) ) ;
#51910 = LINE ( 'NONE', #127629, #141094 ) ;
#51912 = DIRECTION ( 'NONE',  ( 0.000000000000000000, 1.000000000000000000, 6.982962677686266711E-15 ) ) ;
#51913 = DIRECTION ( 'NONE',  ( 0.000000000000000000, -1.000000000000000000, 0.000000000000000000 ) ) ;
#51914 = DIRECTION ( 'NONE',  ( 0.000000000000000000, 1.000000000000000000, 0.000000000000000000 ) ) ;
#51916 = CARTESIAN_POINT ( 'NONE',  ( -18.59999999999999787, 85.50000000001209344, -128.4231074845242233 ) ) ;
#51915 = VECTOR ( 'NONE', #229101, 1000.000000000000000 ) ;
#51917 = VERTEX_POINT ( 'NONE', #111346 ) ;
#51918 = AXIS2_PLACEMENT_3D ( 'NONE', #241529, #182867, #184111 ) ;
#51919 = CARTESIAN_POINT ( 'NONE',  ( -18.59999999999999787, -9.480686695278976117, -40.44111516875784673 ) ) ;
#51920 = DIRECTION ( 'NONE',  ( 1.000000000000000000, 3.448943450116723568E-16, 6.438528483529607644E-16 ) ) ;
#51922 = CARTESIAN_POINT ( 'NONE',  ( -18.59999999999999787, 30.09302283515540211, -235.6538990729184491 ) ) ;
#51921 = AXIS2_PLACEMENT_3D ( 'NONE', #158697, #176976, #2140 ) ;
#51923 = AXIS2_PLACEMENT_3D ( 'NONE', #50329, #114176, #32099 ) ;
#51924 = EDGE_CURVE ( 'NONE', #147068, #9191, #75586, .T. ) ;
#51926 = DIRECTION ( 'NONE',  ( 1.000000000000000000, 0.000000000000000000, 0.000000000000000000 ) ) ;
#51925 = STYLED_ITEM ( 'NONE', ( #74929 ), #157328 ) ;
#51927 = CARTESIAN_POINT ( 'NONE',  ( 20.12500000000000000, 63.35728523183471594, -212.8904317177587870 ) ) ;
#51928 = LINE ( 'NONE', #94917, #251876 ) ;
#51929 = ORIENTED_EDGE ( 'NONE', *, *, #13770, .T. ) ;
#51930 = EDGE_CURVE ( 'NONE', #41838, #118431, #211357, .T. ) ;
#51931 = EDGE_LOOP ( 'NONE', ( #229915, #255076, #160919, #33065 ) ) ;
#51932 = CARTESIAN_POINT ( 'NONE',  ( -20.94999999999999929, -11.41227409414968719, -3.000000000000002665 ) ) ;
#51933 = EDGE_LOOP ( 'NONE', ( #43912, #75406, #159397, #250886, #20305, #98681, #178848, #45985, #164430, #199635, #43482, #223047 ) ) ;
#51935 = EDGE_CURVE ( 'NONE', #9164, #3546, #33135, .T. ) ;
#51934 = DIRECTION ( 'NONE',  ( -0.000000000000000000, -1.000000000000000000, -6.982962677686266711E-15 ) ) ;
#51936 = CARTESIAN_POINT ( 'NONE',  ( -20.54999999999999716, 68.85000000001222986, -148.8731074845244109 ) ) ;
#51937 = AXIS2_PLACEMENT_3D ( 'NONE', #250014, #233043, #72692 ) ;
#51938 = AXIS2_PLACEMENT_3D ( 'NONE', #123900, #199600, #97869 ) ;
#51939 = CIRCLE ( 'NONE', #110212, 0.09999999999999982514 ) ;
#51940 = ORIENTED_EDGE ( 'NONE', *, *, #90764, .T. ) ;
#51941 = DIRECTION ( 'NONE',  ( -1.000000000000000000, 2.952720810173289112E-16, 2.061873921506763405E-30 ) ) ;
#51942 = EDGE_CURVE ( 'NONE', #136430, #68363, #108859, .T. ) ;
#51943 = ORIENTED_EDGE ( 'NONE', *, *, #247634, .T. ) ;
#51944 = CARTESIAN_POINT ( 'NONE',  ( -18.34374000495060386, 11.47316190336247033, -9.249999999999998224 ) ) ;
#51945 = CYLINDRICAL_SURFACE ( 'NONE', #249440, 0.09999999999998898659 ) ;
#51947 = CIRCLE ( 'NONE', #206104, 0.09999999999998898659 ) ;
#51946 = DIRECTION ( 'NONE',  ( 0.000000000000000000, 0.4721928772777242433, 0.8814952561688484955 ) ) ;
#51948 = EDGE_CURVE ( 'NONE', #229414, #219191, #204541, .T. ) ;
#51950 = DIRECTION ( 'NONE',  ( -1.000000000000000000, 0.000000000000000000, 0.000000000000000000 ) ) ;
#51949 = VECTOR ( 'NONE', #12867, 1000.000000000000000 ) ;
#51951 = EDGE_CURVE ( 'NONE', #127380, #149877, #50076, .T. ) ;
#51952 = CARTESIAN_POINT ( 'NONE',  ( 21.07928932188134397, 6.328516656404459262, -133.9011048543456184 ) ) ;
#51954 = VECTOR ( 'NONE', #141172, 1000.000000000000000 ) ;
#51953 = PLANE ( 'NONE',  #237318 ) ;
#51955 = DIRECTION ( 'NONE',  ( 0.000000000000000000, -0.4721928772776973204, -0.8814952561688629284 ) ) ;
#51956 = FACE_OUTER_BOUND ( 'NONE', #155277, .T. ) ;
#51958 = ORIENTED_EDGE ( 'NONE', *, *, #104808, .T. ) ;
#51957 = DIRECTION ( 'NONE',  ( 0.000000000000000000, -1.000000000000000000, -6.982962677686265922E-15 ) ) ;
#51960 = CARTESIAN_POINT ( 'NONE',  ( -20.64999999999999858, 70.80971041069356886, -215.3055740759912453 ) ) ;
#51959 = DIRECTION ( 'NONE',  ( -0.000000000000000000, 1.000000000000000000, 6.982962677686266711E-15 ) ) ;
#51961 = CIRCLE ( 'NONE', #118650, 0.1000000000000028644 ) ;
#51962 = ORIENTED_EDGE ( 'NONE', *, *, #196634, .F. ) ;
#51964 = ORIENTED_EDGE ( 'NONE', *, *, #73005, .T. ) ;
#51963 = CARTESIAN_POINT ( 'NONE',  ( 20.94999999999999929, 1.115600667400684642E-11, -141.8000000000000398 ) ) ;
#51965 = ORIENTED_EDGE ( 'NONE', *, *, #23485, .F. ) ;
#51966 = DIRECTION ( 'NONE',  ( 1.000000000000000000, 0.000000000000000000, 0.000000000000000000 ) ) ;
#51967 = DIRECTION ( 'NONE',  ( 0.000000000000000000, -0.2617529984165031243, -0.9651348961777157509 ) ) ;
#51968 = EDGE_CURVE ( 'NONE', #68040, #196986, #215567, .T. ) ;
#51969 = AXIS2_PLACEMENT_3D ( 'NONE', #110413, #88257, #189961 ) ;
#51970 = VECTOR ( 'NONE', #122187, 1000.000000000000000 ) ;
#51971 = CARTESIAN_POINT ( 'NONE',  ( 22.46250603428203618, 75.97885582387293368, -81.17297058186441916 ) ) ;
#51972 = CARTESIAN_POINT ( 'NONE',  ( 20.94999999999999574, -1.835341550213255957, -179.0551512925629538 ) ) ;
#51973 = CARTESIAN_POINT ( 'NONE',  ( -18.59999999999999787, 77.13501884592155022, -28.30613060109199353 ) ) ;
#51974 = EDGE_CURVE ( 'NONE', #17807, #150586, #158215, .T. ) ;
#51975 = ADVANCED_FACE ( 'NONE', ( #216848 ), #96201, .T. ) ;
#51976 = AXIS2_PLACEMENT_3D ( 'NONE', #19007, #201492, #141523 ) ;
#51977 = DIRECTION ( 'NONE',  ( 0.000000000000000000, -7.487053152578127080E-15, 1.000000000000000000 ) ) ;
#51978 = AXIS2_PLACEMENT_3D ( 'NONE', #75445, #77962, #17996 ) ;
#51979 = CARTESIAN_POINT ( 'NONE',  ( -17.27223548805715936, 12.52722179100237376, -209.9045420924107646 ) ) ;
#51980 = CARTESIAN_POINT ( 'NONE',  ( -18.59999999999999787, -9.849999999999994316, 30.09999999999999787 ) ) ;
#51981 = ORIENTED_EDGE ( 'NONE', *, *, #200806, .T. ) ;
#51982 = ORIENTED_EDGE ( 'NONE', *, *, #240256, .F. ) ;
#51983 = FACE_OUTER_BOUND ( 'NONE', #119339, .T. ) ;
#51984 = ORIENTED_EDGE ( 'NONE', *, *, #231288, .F. ) ;
#51985 = CARTESIAN_POINT ( 'NONE',  ( 20.94999999999999929, 76.00000000001142553, -36.02310748452432421 ) ) ;
#51986 = ORIENTED_EDGE ( 'NONE', *, *, #180508, .T. ) ;
#51987 = CARTESIAN_POINT ( 'NONE',  ( 22.50000000000000000, 11.64957080755595520, -33.40000000000000568 ) ) ;
#51988 = EDGE_CURVE ( 'NONE', #130891, #72948, #218120, .T. ) ;
#51989 = CARTESIAN_POINT ( 'NONE',  ( -20.94999999999999929, 64.35000000001232934, -163.0083017138704236 ) ) ;
#51990 = CYLINDRICAL_SURFACE ( 'NONE', #101815, 4.049999999999994493 ) ;
#51991 = EDGE_CURVE ( 'NONE', #252315, #243292, #125452, .T. ) ;
#51992 = CARTESIAN_POINT ( 'NONE',  ( -20.90000000000000213, -1.212568896937008089, -8.000000000000000000 ) ) ;
#51993 = FACE_BOUND ( 'NONE', #28989, .T. ) ;
#51994 = VERTEX_POINT ( 'NONE', #197290 ) ;
#51995 = CARTESIAN_POINT ( 'NONE',  ( -23.15000000000000213, 0.000000000000000000, -4.049999999999998934 ) ) ;
#51996 = AXIS2_PLACEMENT_3D ( 'NONE', #185074, #84646, #164245 ) ;
#51997 = DIRECTION ( 'NONE',  ( 0.000000000000000000, 0.8700118002898393765, -0.4930308989875104575 ) ) ;
#51998 = AXIS2_PLACEMENT_3D ( 'NONE', #53320, #132869, #149869 ) ;
#51999 = EDGE_CURVE ( 'NONE', #62499, #52922, #79625, .T. ) ;
#52000 = CARTESIAN_POINT ( 'NONE',  ( -23.15000000000000213, 82.67551891922275331, -215.5849511313000164 ) ) ;
#52001 = LINE ( 'NONE', #32504, #224040 ) ;
#52002 = FACE_OUTER_BOUND ( 'NONE', #109331, .T. ) ;
#52003 = AXIS2_PLACEMENT_3D ( 'NONE', #25401, #243137, #166213 ) ;
#52004 = EDGE_LOOP ( 'NONE', ( #35856, #31504, #125818 ) ) ;
#52006 = DIRECTION ( 'NONE',  ( 0.000000000000000000, 0.9126074666063769270, 0.4088369013363280513 ) ) ;
#52005 = DIRECTION ( 'NONE',  ( -1.000000000000000000, 0.000000000000000000, 0.000000000000000000 ) ) ;
#52007 = ORIENTED_EDGE ( 'NONE', *, *, #158792, .T. ) ;
#52010 = ORIENTED_EDGE ( 'NONE', *, *, #118057, .T. ) ;
#52009 = CARTESIAN_POINT ( 'NONE',  ( -18.34374000495059676, 64.52683809664949877, -112.2731074845243739 ) ) ;
#52008 = CYLINDRICAL_SURFACE ( 'NONE', #219833, 0.5000000000000004441 ) ;
#52011 = DIRECTION ( 'NONE',  ( 0.000000000000000000, 0.000000000000000000, -1.000000000000000000 ) ) ;
#52012 = AXIS2_PLACEMENT_3D ( 'NONE', #85037, #221985, #107197 ) ;
#52013 = CYLINDRICAL_SURFACE ( 'NONE', #41804, 0.8750000000000007772 ) ;
#52014 = AXIS2_PLACEMENT_3D ( 'NONE', #10499, #247814, #169611 ) ;
#52015 = ORIENTED_EDGE ( 'NONE', *, *, #92937, .F. ) ;
#52016 = FACE_BOUND ( 'NONE', #148133, .T. ) ;
#52017 = LINE ( 'NONE', #50724, #115423 ) ;
#52018 = DIRECTION ( 'NONE',  ( 1.000000000000000000, 0.000000000000000000, 0.000000000000000000 ) ) ;
#52020 = ORIENTED_EDGE ( 'NONE', *, *, #54044, .T. ) ;
#52019 = CARTESIAN_POINT ( 'NONE',  ( -18.40000000000000213, 64.25000000001159606, -56.87310748452440379 ) ) ;
#52021 = VECTOR ( 'NONE', #197417, 1000.000000000000000 ) ;
#52022 = EDGE_CURVE ( 'NONE', #61549, #108560, #519, .T. ) ;
#52023 = AXIS2_PLACEMENT_3D ( 'NONE', #102158, #181737, #86446 ) ;
#52024 = ORIENTED_EDGE ( 'NONE', *, *, #122504, .F. ) ;
#52025 = EDGE_CURVE ( 'NONE', #111063, #192857, #167973, .T. ) ;
#52026 = CARTESIAN_POINT ( 'NONE',  ( -17.80356949363855534, 10.87673139701218972, -110.7869269757733548 ) ) ;
#52027 = CARTESIAN_POINT ( 'NONE',  ( 18.59999999999999076, 11.65000000001115943, -67.00000000000000000 ) ) ;
#52028 = CYLINDRICAL_SURFACE ( 'NONE', #109309, 0.09999999999999939493 ) ;
#52029 = EDGE_LOOP ( 'NONE', ( #80743, #3313, #100783, #229744 ) ) ;
#52030 = LINE ( 'NONE', #172040, #76900 ) ;
#52031 = EDGE_CURVE ( 'NONE', #10835, #207046, #17314, .T. ) ;
#52032 = EDGE_CURVE ( 'NONE', #215740, #126512, #222288, .T. ) ;
#52033 = DIRECTION ( 'NONE',  ( -2.952720810173289112E-16, 1.000000000000000000, 0.000000000000000000 ) ) ;
#52034 = AXIS2_PLACEMENT_3D ( 'NONE', #170523, #229166, #231736 ) ;
#52035 = ORIENTED_EDGE ( 'NONE', *, *, #251691, .T. ) ;
#52036 = FACE_OUTER_BOUND ( 'NONE', #46847, .T. ) ;
#52037 = ADVANCED_FACE ( 'NONE', ( #160771 ), #240287, .F. ) ;
#52038 = DIRECTION ( 'NONE',  ( 1.000000000000000000, 0.000000000000000000, 0.000000000000000000 ) ) ;
#52039 = VERTEX_POINT ( 'NONE', #196028 ) ;
#52040 = DIRECTION ( 'NONE',  ( -0.000000000000000000, 0.9651348961777157509, -0.2617529984165031243 ) ) ;
#52041 = DIRECTION ( 'NONE',  ( 1.000000000000000000, -0.000000000000000000, -0.000000000000000000 ) ) ;
#52042 = TOROIDAL_SURFACE ( 'NONE', #68834, 11.90000000000000213, 0.1000000000000000056 ) ;
#52043 = ADVANCED_FACE ( 'NONE', ( #198570 ), #83879, .T. ) ;
#52044 = EDGE_LOOP ( 'NONE', ( #70240, #206983, #230255, #1889, #124724 ) ) ;
#52045 = VECTOR ( 'NONE', #207518, 1000.000000000000000 ) ;
#52046 = ORIENTED_EDGE ( 'NONE', *, *, #10623, .F. ) ;
#52047 = EDGE_CURVE ( 'NONE', #166555, #197879, #250515, .T. ) ;
#52048 = FACE_OUTER_BOUND ( 'NONE', #104492, .T. ) ;
#52049 = ORIENTED_EDGE ( 'NONE', *, *, #250360, .T. ) ;
#52051 = ORIENTED_EDGE ( 'NONE', *, *, #106080, .F. ) ;
#52050 = CYLINDRICAL_SURFACE ( 'NONE', #1244, 0.1000000000000028644 ) ;
#52052 = ADVANCED_FACE ( 'NONE', ( #120365 ), #76060, .T. ) ;
#52053 = ORIENTED_EDGE ( 'NONE', *, *, #168311, .F. ) ;
#52056 = ORIENTED_EDGE ( 'NONE', *, *, #87337, .T. ) ;
#52055 = ORIENTED_EDGE ( 'NONE', *, *, #147574, .T. ) ;
#52054 = CARTESIAN_POINT ( 'NONE',  ( -21.14999999999999858, 69.45934304831114048, -170.0231074845243882 ) ) ;
#52057 = CARTESIAN_POINT ( 'NONE',  ( -20.85000000000000142, 87.65000000001191438, -103.0231074845242176 ) ) ;
#52058 = ORIENTED_EDGE ( 'NONE', *, *, #72076, .T. ) ;
#52059 = DIRECTION ( 'NONE',  ( 1.000000000000000000, 0.000000000000000000, 0.000000000000000000 ) ) ;
#52060 = FACE_OUTER_BOUND ( 'NONE', #51678, .T. ) ;
#52061 = EDGE_CURVE ( 'NONE', #191238, #51021, #176472, .T. ) ;
#52062 = AXIS2_PLACEMENT_3D ( 'NONE', #118853, #198369, #140982 ) ;
#52063 = ADVANCED_FACE ( 'NONE', ( #236419 ), #128040, .F. ) ;
#52064 = DIRECTION ( 'NONE',  ( 1.000000000000000000, 0.000000000000000000, 0.000000000000000000 ) ) ;
#52065 = CARTESIAN_POINT ( 'NONE',  ( -18.59999999999999787, 64.25000000001253397, -182.2731074845244450 ) ) ;
#52066 = VERTEX_POINT ( 'NONE', #68055 ) ;
#52067 = ORIENTED_EDGE ( 'NONE', *, *, #168727, .F. ) ;
#52068 = ORIENTED_EDGE ( 'NONE', *, *, #51880, .F. ) ;
#52069 = EDGE_CURVE ( 'NONE', #17135, #140018, #58956, .T. ) ;
#52070 = CARTESIAN_POINT ( 'NONE',  ( -22.39999999999999858, 64.35000000001195986, -103.1231074845243825 ) ) ;
#52071 = TOROIDAL_SURFACE ( 'NONE', #227054, 0.2000000000000000111, 0.1000000000000000056 ) ;
#52073 = ORIENTED_EDGE ( 'NONE', *, *, #242103, .T. ) ;
#52072 = LINE ( 'NONE', #131624, #257704 ) ;
#52074 = DIRECTION ( 'NONE',  ( 0.000000000000000000, -1.000000000000000000, 6.308085367188393199E-16 ) ) ;
#52076 = ORIENTED_EDGE ( 'NONE', *, *, #204943, .F. ) ;
#52075 = CARTESIAN_POINT ( 'NONE',  ( 18.49999999999999645, 70.05000000001267324, -193.2174051794895320 ) ) ;
#52077 = VERTEX_POINT ( 'NONE', #23827 ) ;
#52078 = ADVANCED_FACE ( 'NONE', ( #103312 ), #86305, .T. ) ;
#52079 = FACE_OUTER_BOUND ( 'NONE', #42683, .T. ) ;
#52080 = ADVANCED_FACE ( 'NONE', ( #227117 ), #229684, .F. ) ;
#52081 = ORIENTED_EDGE ( 'NONE', *, *, #7788, .F. ) ;
#52082 = LINE ( 'NONE', #211178, #122898 ) ;
#52083 = DIRECTION ( 'NONE',  ( 0.000000000000000000, -0.8741572761215442577, 0.4856429311786202851 ) ) ;
#52086 = ORIENTED_EDGE ( 'NONE', *, *, #94992, .T. ) ;
#52085 = ORIENTED_EDGE ( 'NONE', *, *, #200338, .F. ) ;
#52084 = VECTOR ( 'NONE', #33517, 1000.000000000000000 ) ;
#52087 = CIRCLE ( 'NONE', #243646, 0.1000000000000002554 ) ;
#52088 = ORIENTED_EDGE ( 'NONE', *, *, #128282, .F. ) ;
#52089 = DIRECTION ( 'NONE',  ( 0.000000000000000000, 6.608470384673547079E-15, -1.000000000000000000 ) ) ;
#52090 = ORIENTED_EDGE ( 'NONE', *, *, #24959, .F. ) ;
#52091 = EDGE_LOOP ( 'NONE', ( #208804, #230620, #84044, #174932 ) ) ;
#52092 = DIRECTION ( 'NONE',  ( -0.7071067811865388020, 0.7071067811865561215, 0.000000000000000000 ) ) ;
#52094 = ORIENTED_EDGE ( 'NONE', *, *, #98439, .T. ) ;
#52093 = CARTESIAN_POINT ( 'NONE',  ( -22.39999999999999858, 64.25000000001269029, -203.4231074845244507 ) ) ;
#52095 = EDGE_CURVE ( 'NONE', #160549, #88017, #4782, .T. ) ;
#52096 = DIRECTION ( 'NONE',  ( 0.000000000000000000, 1.776356839400310418E-15, -1.000000000000000000 ) ) ;
#52098 = DIRECTION ( 'NONE',  ( -1.000000000000000000, 0.000000000000000000, 0.000000000000000000 ) ) ;
#52097 = DIRECTION ( 'NONE',  ( 0.000000000000000000, 0.000000000000000000, 1.000000000000000000 ) ) ;
#52099 = DIRECTION ( 'NONE',  ( 0.000000000000000000, 1.734723475976997999E-14, -1.000000000000000000 ) ) ;
#52100 = CARTESIAN_POINT ( 'NONE',  ( 19.75857864376268935, 64.25000000001220712, -145.1731074845244507 ) ) ;
#52101 = VERTEX_POINT ( 'NONE', #27691 ) ;
#52102 = B_SPLINE_CURVE_WITH_KNOTS ( 'NONE', 3,
 ( #90370, #68257, #49965, #169967 ),
 .UNSPECIFIED., .F., .F.,
 ( 4, 4 ),
 ( 3.469446951953614189E-18, 0.0001058379652594568606 ),
 .UNSPECIFIED. ) ;
#52103 = VERTEX_POINT ( 'NONE', #204976 ) ;
#52104 = CARTESIAN_POINT ( 'NONE',  ( 18.33996824403519099, 85.56963985944324236, -96.20404184700757355 ) ) ;
#52105 = EDGE_CURVE ( 'NONE', #41556, #198415, #122909, .T. ) ;
#52106 = DIRECTION ( 'NONE',  ( -0.000000000000000000, -1.000000000000000000, -6.982962677686266711E-15 ) ) ;
#52107 = DIRECTION ( 'NONE',  ( 0.000000000000000000, 0.2128009952263603677, -0.9770955615653313941 ) ) ;
#52108 = AXIS2_PLACEMENT_3D ( 'NONE', #128720, #70047, #149583 ) ;
#52109 = EDGE_LOOP ( 'NONE', ( #177345, #204119, #147307, #8593 ) ) ;
#52110 = AXIS2_PLACEMENT_3D ( 'NONE', #6450, #165547, #120025 ) ;
#52111 = AXIS2_PLACEMENT_3D ( 'NONE', #192349, #231488, #170268 ) ;
#52112 = VECTOR ( 'NONE', #137063, 1000.000000000000000 ) ;
#52113 = CARTESIAN_POINT ( 'NONE',  ( 20.94999999999999929, 77.83534155023599510, -57.96795619196132776 ) ) ;
#52114 = LINE ( 'NONE', #211206, #171757 ) ;
#52115 = ORIENTED_EDGE ( 'NONE', *, *, #254847, .T. ) ;
#52116 = VERTEX_POINT ( 'NONE', #246683 ) ;
#52117 = MECHANICAL_DESIGN_GEOMETRIC_PRESENTATION_REPRESENTATION (  '', ( #143711 ), #89528 ) ;
#52118 = LINE ( 'NONE', #216336, #105087 ) ;
#52119 = EDGE_CURVE ( 'NONE', #163484, #89234, #102715, .T. ) ;
#52120 = CARTESIAN_POINT ( 'NONE',  ( 22.39999999999999503, 1.115600667400684642E-11, -122.3504291924552234 ) ) ;
#52121 = ORIENTED_EDGE ( 'NONE', *, *, #15182, .T. ) ;
#52122 = DIRECTION ( 'NONE',  ( 0.000000000000000000, -6.982962677686266711E-15, 1.000000000000000000 ) ) ;
#52123 = ORIENTED_EDGE ( 'NONE', *, *, #82563, .T. ) ;
#52124 = CARTESIAN_POINT ( 'NONE',  ( 18.50000000000000355, -9.421074344976428705, -140.8244720594310593 ) ) ;
#52125 = LINE ( 'NONE', #35190, #183086 ) ;
#52127 = CARTESIAN_POINT ( 'NONE',  ( -21.09096482362077296, -1.315623836012118852, -194.7738144117574848 ) ) ;
#52126 = LINE ( 'NONE', #67849, #78017 ) ;
#52128 = DIRECTION ( 'NONE',  ( 0.000000000000000000, 1.000000000000000000, 6.982962677686266711E-15 ) ) ;
#52129 = DIRECTION ( 'NONE',  ( 1.000000000000000000, 0.000000000000000000, 0.000000000000000000 ) ) ;
#52130 = CARTESIAN_POINT ( 'NONE',  ( 18.50000000000000000, -9.399999999988843058, -174.7972597596632625 ) ) ;
#52131 = FACE_OUTER_BOUND ( 'NONE', #195793, .T. ) ;
#52133 = EDGE_LOOP ( 'NONE', ( #169984, #19409, #44495, #208889 ) ) ;
#52132 = DIRECTION ( 'NONE',  ( 0.000000000000000000, 0.000000000000000000, 1.000000000000000000 ) ) ;
#52134 = ADVANCED_FACE ( 'NONE', ( #185440 ), #8097, .T. ) ;
#52135 = CIRCLE ( 'NONE', #73040, 0.1000000000000035028 ) ;
#52136 = CIRCLE ( 'NONE', #27247, 0.09999999999998898659 ) ;
#52138 = VERTEX_POINT ( 'NONE', #5485 ) ;
#52137 = ORIENTED_EDGE ( 'NONE', *, *, #104862, .F. ) ;
#52139 = VERTEX_POINT ( 'NONE', #25107 ) ;
#52140 = AXIS2_PLACEMENT_3D ( 'NONE', #49062, #167763, #103883 ) ;
#52141 = DIRECTION ( 'NONE',  ( -1.000000000000000000, -0.000000000000000000, -0.000000000000000000 ) ) ;
#52142 = DIRECTION ( 'NONE',  ( 0.000000000000000000, 0.9126074666063660468, 0.4088369013363524762 ) ) ;
#52144 = DIRECTION ( 'NONE',  ( 0.000000000000000000, 0.000000000000000000, -1.000000000000000000 ) ) ;
#52143 = CARTESIAN_POINT ( 'NONE',  ( -16.85939681242905763, 66.09477481408723065, -182.9831855293329852 ) ) ;
#52145 = DIRECTION ( 'NONE',  ( 1.000000000000000000, 0.000000000000000000, -0.000000000000000000 ) ) ;
#52146 = ORIENTED_EDGE ( 'NONE', *, *, #62544, .F. ) ;
#52147 = AXIS2_PLACEMENT_3D ( 'NONE', #38204, #53899, #77301 ) ;
#52148 = CARTESIAN_POINT ( 'NONE',  ( 21.07094088545303734, 69.67983277809517517, -69.62200118707659158 ) ) ;
#52149 = CIRCLE ( 'NONE', #210394, 0.09999999999998898659 ) ;
#52150 = TOROIDAL_SURFACE ( 'NONE', #168741, 11.89999999999999858, 0.1000000000000000056 ) ;
#52151 = ORIENTED_EDGE ( 'NONE', *, *, #159789, .T. ) ;
#52152 = ORIENTED_EDGE ( 'NONE', *, *, #220723, .T. ) ;
#52153 = FACE_OUTER_BOUND ( 'NONE', #73551, .T. ) ;
#52154 = FACE_OUTER_BOUND ( 'NONE', #236201, .T. ) ;
#52155 = DIRECTION ( 'NONE',  ( 1.000000000000000000, 0.000000000000000000, 0.000000000000000000 ) ) ;
#52156 = EDGE_LOOP ( 'NONE', ( #50110, #129269, #56168, #43401, #39042 ) ) ;
#52157 = CARTESIAN_POINT ( 'NONE',  ( -23.15000000000000213, 4.350000000011156054, -179.8499999999999943 ) ) ;
#52158 = AXIS2_PLACEMENT_3D ( 'NONE', #112686, #187104, #68422 ) ;
#52159 = CARTESIAN_POINT ( 'NONE',  ( 22.45380639572245585, 1.426796592706731485E-07, -155.7495671089028804 ) ) ;
#52160 = VERTEX_POINT ( 'NONE', #22531 ) ;
#52161 = EDGE_LOOP ( 'NONE', ( #154093, #86383, #251853, #221151 ) ) ;
#52162 = DIRECTION ( 'NONE',  ( 0.000000000000000000, -0.000000000000000000, -1.000000000000000000 ) ) ;
#52163 = CIRCLE ( 'NONE', #197907, 0.9750000000000036415 ) ;
#52164 = DIRECTION ( 'NONE',  ( 1.000000000000000000, 0.000000000000000000, 0.000000000000000000 ) ) ;
#52165 = DIRECTION ( 'NONE',  ( -0.000000000000000000, -6.982962677686266711E-15, 1.000000000000000000 ) ) ;
#52166 = CARTESIAN_POINT ( 'NONE',  ( 22.50000000000000000, 0.1000000000111554016, -92.70922040162665212 ) ) ;
#52167 = LINE ( 'NONE', #189127, #160814 ) ;
#52168 = VECTOR ( 'NONE', #106437, 1000.000000000000000 ) ;
#52169 = DIRECTION ( 'NONE',  ( -1.000000000000000000, -0.000000000000000000, -0.000000000000000000 ) ) ;
#52171 = EDGE_LOOP ( 'NONE', ( #40414, #139676, #217580, #12955 ) ) ;
#52170 = CIRCLE ( 'NONE', #152162, 4.049999999999998934 ) ;
#52172 = CARTESIAN_POINT ( 'NONE',  ( 18.39999999999999503, 70.35000000001153353, -48.67310748452436542 ) ) ;
#52173 = CARTESIAN_POINT ( 'NONE',  ( -20.94999999999999929, -11.64999999998884483, -164.6000000000000227 ) ) ;
#52175 = DIRECTION ( 'NONE',  ( 1.000000000000000000, 0.000000000000000000, 0.000000000000000000 ) ) ;
#52174 = DIRECTION ( 'NONE',  ( 2.952720810173288126E-16, -0.4721928772777346794, -0.8814952561688429444 ) ) ;
#52177 = EDGE_CURVE ( 'NONE', #113692, #55133, #225817, .T. ) ;
#52176 = DIRECTION ( 'NONE',  ( 0.000000000000000000, -3.513364001978347611E-15, -1.000000000000000000 ) ) ;
#52178 = CARTESIAN_POINT ( 'NONE',  ( -18.47653818581420637, -9.465280387762964764, -7.125960816139832232 ) ) ;
#52179 = FACE_OUTER_BOUND ( 'NONE', #201918, .T. ) ;
#52181 = EDGE_LOOP ( 'NONE', ( #85390, #232981, #215337, #32173 ) ) ;
#52180 = DIRECTION ( 'NONE',  ( -0.000000000000000000, 1.000000000000000000, 1.626303258728266709E-15 ) ) ;
#52182 = EDGE_CURVE ( 'NONE', #172545, #143593, #79811, .T. ) ;
#52183 = DIRECTION ( 'NONE',  ( 1.000000000000000000, 0.000000000000000000, 0.000000000000000000 ) ) ;
#52184 = EDGE_CURVE ( 'NONE', #34405, #235569, #50589, .T. ) ;
#52186 = CIRCLE ( 'NONE', #110449, 0.2000000000000057288 ) ;
#52185 = CARTESIAN_POINT ( 'NONE',  ( 22.39999999999999503, -0.09999999998884338825, -155.8504291924551808 ) ) ;
#52187 = AXIS2_PLACEMENT_3D ( 'NONE', #243180, #206629, #223602 ) ;
#52188 = DIRECTION ( 'NONE',  ( -1.000000000000000000, -0.000000000000000000, -0.000000000000000000 ) ) ;
#52189 = AXIS2_PLACEMENT_3D ( 'NONE', #256581, #59691, #18020 ) ;
#52190 = DIRECTION ( 'NONE',  ( 0.000000000000000000, 0.000000000000000000, -1.000000000000000000 ) ) ;
#52191 = EDGE_CURVE ( 'NONE', #57461, #103650, #217174, .T. ) ;
#52192 = CARTESIAN_POINT ( 'NONE',  ( -20.65000000000000568, 7.250000000011138646, -146.6500000000000341 ) ) ;
#52193 = DIRECTION ( 'NONE',  ( -0.7071067811865475727, 0.6824534298470373850, -0.1850873201762210096 ) ) ;
#52194 = CARTESIAN_POINT ( 'NONE',  ( -16.92989143108097849, 66.05000000001157900, -56.64062360976772226 ) ) ;
#52195 = AXIS2_PLACEMENT_3D ( 'NONE', #168206, #250266, #49501 ) ;
#52196 = EDGE_CURVE ( 'NONE', #105902, #248551, #142371, .T. ) ;
#52198 = ORIENTED_EDGE ( 'NONE', *, *, #122153, .F. ) ;
#52197 = EDGE_CURVE ( 'NONE', #43496, #71417, #224553, .T. ) ;
#52199 = DIRECTION ( 'NONE',  ( 0.000000000000000000, 0.000000000000000000, 1.000000000000000000 ) ) ;
#52201 = ORIENTED_EDGE ( 'NONE', *, *, #39456, .T. ) ;
#52200 = DIRECTION ( 'NONE',  ( 1.000000000000000000, -2.952720810173289112E-16, -2.061873921506763405E-30 ) ) ;
#52202 = FACE_OUTER_BOUND ( 'NONE', #151693, .T. ) ;
#52203 = EDGE_CURVE ( 'NONE', #87393, #211799, #105871, .T. ) ;
#52204 = DIRECTION ( 'NONE',  ( 0.000000000000000000, -1.000000000000000000, -0.000000000000000000 ) ) ;
#52205 = AXIS2_PLACEMENT_3D ( 'NONE', #216940, #78707, #239093 ) ;
#52206 = ORIENTED_EDGE ( 'NONE', *, *, #236230, .F. ) ;
#52207 = CARTESIAN_POINT ( 'NONE',  ( -21.64999999999999858, 65.95000000001255103, -182.7731074845244450 ) ) ;
#52208 = CIRCLE ( 'NONE', #143790, 11.65000000000001457 ) ;
#52209 = PRODUCT_CONTEXT ( 'NONE', #163958, 'mechanical' ) ;
#52210 = DIRECTION ( 'NONE',  ( 0.000000000000000000, 0.1335171055202867274, -0.9910465087640866200 ) ) ;
#52212 = EDGE_CURVE ( 'NONE', #36755, #77589, #87598, .T. ) ;
#52211 = DIRECTION ( 'NONE',  ( 0.000000000000000000, 1.000000000000000000, 0.000000000000000000 ) ) ;
#52213 = VECTOR ( 'NONE', #88586, 1000.000000000000114 ) ;
#52214 = ORIENTED_EDGE ( 'NONE', *, *, #142428, .T. ) ;
#52215 = FACE_OUTER_BOUND ( 'NONE', #35458, .T. ) ;
#52216 = FACE_OUTER_BOUND ( 'NONE', #162292, .T. ) ;
#52217 = CARTESIAN_POINT ( 'NONE',  ( -23.15000000000000213, 85.00000000001149658, -45.91707660717669626 ) ) ;
#52218 = ORIENTED_EDGE ( 'NONE', *, *, #191646, .F. ) ;
#52219 = ORIENTED_EDGE ( 'NONE', *, *, #11538, .F. ) ;
#52220 = DIRECTION ( 'NONE',  ( 1.000000000000000000, 0.000000000000000000, 0.000000000000000000 ) ) ;
#52221 = EDGE_CURVE ( 'NONE', #72258, #41069, #179809, .T. ) ;
#52222 = DIRECTION ( 'NONE',  ( 0.000000000000000000, 1.224646799142185182E-16, 1.000000000000000000 ) ) ;
#52223 = CARTESIAN_POINT ( 'NONE',  ( -21.05000000000000071, -1.835341550213255957, -145.5551512925629822 ) ) ;
#52225 = DIRECTION ( 'NONE',  ( -7.304098846218134667E-16, 1.000000000000000000, 6.982962677686267499E-15 ) ) ;
#52224 = DIRECTION ( 'NONE',  ( 2.840903330521631775E-16, 0.8700118002898354908, -0.4930308989875170078 ) ) ;
#52226 = CARTESIAN_POINT ( 'NONE',  ( -23.25000000000000000, -8.596261682231832069, -124.5498724828497501 ) ) ;
#52227 = DIRECTION ( 'NONE',  ( -1.020425574104004196E-15, -6.982962677686266711E-15, 1.000000000000000000 ) ) ;
#52228 = FACE_OUTER_BOUND ( 'NONE', #139952, .T. ) ;
#52229 = ORIENTED_EDGE ( 'NONE', *, *, #254966, .T. ) ;
#52230 = VECTOR ( 'NONE', #36774, 1000.000000000000000 ) ;
#52232 = ORIENTED_EDGE ( 'NONE', *, *, #83321, .F. ) ;
#52231 = DIRECTION ( 'NONE',  ( 0.000000000000000000, 0.000000000000000000, -1.000000000000000000 ) ) ;
#52233 = VECTOR ( 'NONE', #64485, 1000.000000000000000 ) ;
#52234 = CARTESIAN_POINT ( 'NONE',  ( 20.99999999999999645, 66.25000000001207923, -123.8731074845243683 ) ) ;
#52235 = CARTESIAN_POINT ( 'NONE',  ( -21.08376601933334626, -1.287257433775161664, -194.7897398709591812 ) ) ;
#52237 = CARTESIAN_POINT ( 'NONE',  ( -20.64999999999999858, 68.75000000001151079, -48.37310748452436826 ) ) ;
#52236 = CARTESIAN_POINT ( 'NONE',  ( 23.14999999999999858, 11.60000000001116227, -160.5717967697245285 ) ) ;
#52238 = EDGE_CURVE ( 'NONE', #47971, #182741, #113149, .T. ) ;
#52239 = ORIENTED_EDGE ( 'NONE', *, *, #63762, .F. ) ;
#52240 = DIRECTION ( 'NONE',  ( 0.000000000000000000, 0.03181660087583042945, -0.9994937237965569876 ) ) ;
#52241 = CARTESIAN_POINT ( 'NONE',  ( 19.83283456528358712, 64.25000000001196554, -111.6731074851050636 ) ) ;
#52242 = CARTESIAN_POINT ( 'NONE',  ( -21.04999999999999716, 69.55922910635004541, -103.0055102975163521 ) ) ;
#52243 = DIRECTION ( 'NONE',  ( 0.000000000000000000, -0.9525900758537791946, 0.3042567129660269654 ) ) ;
#52244 = EDGE_LOOP ( 'NONE', ( #86133, #174255, #25358 ) ) ;
#52245 = ORIENTED_EDGE ( 'NONE', *, *, #200962, .T. ) ;
#52246 = CARTESIAN_POINT ( 'NONE',  ( 23.14999999999998437, 0.000000000000000000, 0.000000000000000000 ) ) ;
#52247 = ORIENTED_EDGE ( 'NONE', *, *, #117044, .T. ) ;
#52248 = DIRECTION ( 'NONE',  ( 0.5000000000001141309, 0.000000000000000000, -0.8660254037843729824 ) ) ;
#52249 = AXIS2_PLACEMENT_3D ( 'NONE', #187181, #43804, #184584 ) ;
#52250 = EDGE_CURVE ( 'NONE', #77989, #123153, #21578, .T. ) ;
#52251 = CARTESIAN_POINT ( 'NONE',  ( -20.94999999999999929, 77.16412189325258453, -28.10825939895270764 ) ) ;
#52252 = CARTESIAN_POINT ( 'NONE',  ( -20.00857864376270001, 11.66622623553636018, -211.0987209794895421 ) ) ;
#52253 = VECTOR ( 'NONE', #106436, 1000.000000000000000 ) ;
#52254 = DIRECTION ( 'NONE',  ( -1.000000000000000000, 0.000000000000000000, 0.000000000000000000 ) ) ;
#52255 = ORIENTED_EDGE ( 'NONE', *, *, #92089, .T. ) ;
#52256 = CARTESIAN_POINT ( 'NONE',  ( -18.79999999999999716, 1.350000000000000089, 21.90000000000000213 ) ) ;
#52257 = ADVANCED_FACE ( 'NONE', ( #157582 ), #175838, .T. ) ;
#52258 = DIRECTION ( 'NONE',  ( 0.000000000000000000, 0.1495327102803689356, 0.9887567792719336168 ) ) ;
#52259 = CARTESIAN_POINT ( 'NONE',  ( -23.25000000000000000, 85.00000000001222134, -146.4170766071767389 ) ) ;
#52260 = EDGE_CURVE ( 'NONE', #242736, #64537, #146446, .T. ) ;
#52261 = DIRECTION ( 'NONE',  ( 0.000000000000000000, 0.000000000000000000, 1.000000000000000000 ) ) ;
#52262 = ADVANCED_FACE ( 'NONE', ( #97524, #169767 ), #108469, .T. ) ;
#52263 = CARTESIAN_POINT ( 'NONE',  ( -20.94999999999999929, 68.87972903831379767, -32.36354444268504693 ) ) ;
#52264 = DIRECTION ( 'NONE',  ( 0.000000000000000000, 0.000000000000000000, 1.000000000000000000 ) ) ;
#52265 = CARTESIAN_POINT ( 'NONE',  ( -16.87683809663752399, 66.15000000001225544, -149.9254715027207396 ) ) ;
#52266 = ORIENTED_EDGE ( 'NONE', *, *, #257553, .T. ) ;
#52268 = CARTESIAN_POINT ( 'NONE',  ( -16.84421487269769102, 9.950000000011135270, -180.1695021224448965 ) ) ;
#52267 = DIRECTION ( 'NONE',  ( 0.000000000000000000, 1.000000000000000000, 0.000000000000000000 ) ) ;
#52269 = B_SPLINE_CURVE_WITH_KNOTS ( 'NONE', 3,
 ( #24876, #164368, #121419, #43137, #243886, #219181, #144769, #40601, #199657, #21023 ),
 .UNSPECIFIED., .F., .F.,
 ( 4, 2, 2, 2, 4 ),
 ( 0.000000000000000000, 0.0001660831991681966670, 0.0002491247987522938892, 0.0002906455985443780351, 0.0003321663983364622351 ),
 .UNSPECIFIED. ) ;
#52270 = ORIENTED_EDGE ( 'NONE', *, *, #106532, .T. ) ;
#52272 = ORIENTED_EDGE ( 'NONE', *, *, #242883, .T. ) ;
#52271 = DIRECTION ( 'NONE',  ( 0.000000000000000000, -0.9126074666063763718, -0.4088369013363294391 ) ) ;
#52273 = VECTOR ( 'NONE', #221078, 1000.000000000000000 ) ;
#52274 = ORIENTED_EDGE ( 'NONE', *, *, #9594, .F. ) ;
#52275 = VECTOR ( 'NONE', #125027, 1000.000000000000000 ) ;
#52276 = CARTESIAN_POINT ( 'NONE',  ( -16.92973740335376220, 9.992503814478528312, -146.5939409647978664 ) ) ;
#52277 = CARTESIAN_POINT ( 'NONE',  ( 13.88638282980483929, 66.54257354752334663, -151.5230656161243985 ) ) ;
#52278 = CARTESIAN_POINT ( 'NONE',  ( 18.58143601961842961, 65.56427058491711080, -78.27310748452438816 ) ) ;
#52279 = EDGE_CURVE ( 'NONE', #114275, #131063, #213094, .T. ) ;
#52280 = DIRECTION ( 'NONE',  ( 0.000000000000000000, 0.000000000000000000, -1.000000000000000000 ) ) ;
#52281 = ORIENTED_EDGE ( 'NONE', *, *, #184061, .T. ) ;
#52282 = CARTESIAN_POINT ( 'NONE',  ( -20.85000000000000142, 1.115600667400684642E-11, -100.5000000000000426 ) ) ;
#52283 = EDGE_LOOP ( 'NONE', ( #126141, #178790, #105584 ) ) ;
#52284 = DIRECTION ( 'NONE',  ( 0.000000000000000000, -0.2617529984165031243, -0.9651348961777157509 ) ) ;
#52285 = CARTESIAN_POINT ( 'NONE',  ( 21.12757541349815682, 6.473380571251452942, 0.005161215809745128835 ) ) ;
#52286 = ORIENTED_EDGE ( 'NONE', *, *, #77080, .F. ) ;
#52288 = DIRECTION ( 'NONE',  ( -6.938893903907222856E-15, -0.9651348961777157509, 0.2617529984165031243 ) ) ;
#52287 = CIRCLE ( 'NONE', #247935, 0.1000000000000013933 ) ;
#52289 = CIRCLE ( 'NONE', #235452, 0.1000000000000000472 ) ;
#52290 = CIRCLE ( 'NONE', #189683, 0.09999999999999939493 ) ;
#52291 = VERTEX_POINT ( 'NONE', #54577 ) ;
#52292 = DIRECTION ( 'NONE',  ( 0.000000000000000000, 0.000000000000000000, 1.000000000000000000 ) ) ;
#52293 = VERTEX_POINT ( 'NONE', #196651 ) ;
#52294 = LINE ( 'NONE', #173606, #209276 ) ;
#52295 = MECHANICAL_DESIGN_GEOMETRIC_PRESENTATION_REPRESENTATION (  '', ( #89720 ), #39866 ) ;
#52296 = EDGE_CURVE ( 'NONE', #45297, #98196, #96381, .T. ) ;
#52297 = DIRECTION ( 'NONE',  ( 1.000000000000000000, -7.304098846218134667E-16, -5.100424963727255829E-30 ) ) ;
#52298 = CARTESIAN_POINT ( 'NONE',  ( -20.64999999999999858, 67.23127455305835554, -235.8551265064784559 ) ) ;
#52299 = EDGE_CURVE ( 'NONE', #7536, #172048, #134104, .T. ) ;
#52300 = CARTESIAN_POINT ( 'NONE',  ( 18.49999999999999289, 10.32573593129922607, -58.35000000000001563 ) ) ;
#52301 = EDGE_CURVE ( 'NONE', #139384, #107287, #208833, .T. ) ;
#52302 = LINE ( 'NONE', #172326, #37968 ) ;
#52303 = CARTESIAN_POINT ( 'NONE',  ( 18.48413544395648600, -9.664304033616620160, -73.68310499303828465 ) ) ;
#52304 = DIRECTION ( 'NONE',  ( -1.000000000000000000, -0.000000000000000000, -0.000000000000000000 ) ) ;
#52305 = EDGE_LOOP ( 'NONE', ( #45692, #14766, #223588, #158990 ) ) ;
#52306 = DIRECTION ( 'NONE',  ( -0.000000000000000000, 0.1350103645451904977, 0.9908441862701597991 ) ) ;
#52307 = CIRCLE ( 'NONE', #110590, 0.09999999999999062417 ) ;
#52308 = EDGE_LOOP ( 'NONE', ( #40256, #56695, #196172 ) ) ;
#52311 = ORIENTED_EDGE ( 'NONE', *, *, #251507, .T. ) ;
#52310 = DIRECTION ( 'NONE',  ( -2.557131231893037478E-16, -0.8660254037844420383, 0.4999999999999941713 ) ) ;
#52309 = CARTESIAN_POINT ( 'NONE',  ( -20.99142135623731065, 64.40000000001219860, -143.4513107147999449 ) ) ;
#52312 =( GEOMETRIC_REPRESENTATION_CONTEXT ( 3 ) GLOBAL_UNCERTAINTY_ASSIGNED_CONTEXT ( ( #13821 ) ) GLOBAL_UNIT_ASSIGNED_CONTEXT ( ( #120776, #81583, #63325 ) ) REPRESENTATION_CONTEXT ( 'NONE', 'WORKASPACE' ) );
#52313 = ORIENTED_EDGE ( 'NONE', *, *, #168303, .F. ) ;
#52314 = DIRECTION ( 'NONE',  ( 0.000000000000000000, 0.000000000000000000, 1.000000000000000000 ) ) ;
#52315 = CIRCLE ( 'NONE', #160707, 7.900000000000003908 ) ;
#52316 = DIRECTION ( 'NONE',  ( 1.000000000000000000, -0.000000000000000000, -0.000000000000000000 ) ) ;
#52317 = SPHERICAL_SURFACE ( 'NONE', #14592, 0.1000000000000000056 ) ;
#52318 = DIRECTION ( 'NONE',  ( -0.000000000000000000, 0.8814952561688430555, -0.4721928772777346239 ) ) ;
#52319 = ORIENTED_EDGE ( 'NONE', *, *, #135002, .F. ) ;
#52321 = EDGE_LOOP ( 'NONE', ( #86936, #196942 ) ) ;
#52320 = FACE_OUTER_BOUND ( 'NONE', #50229, .T. ) ;
#52322 = CIRCLE ( 'NONE', #214830, 0.1000000000000028644 ) ;
#52323 = CIRCLE ( 'NONE', #139812, 0.09999999999999939493 ) ;
#52325 = CARTESIAN_POINT ( 'NONE',  ( 18.52928932188134326, 15.28939250479744771, -222.8979625946709007 ) ) ;
#52324 = DIRECTION ( 'NONE',  ( 1.000000000000000000, 0.000000000000000000, 0.000000000000000000 ) ) ;
#52326 = AXIS2_PLACEMENT_3D ( 'NONE', #6564, #204757, #140962 ) ;
#52328 = VERTEX_POINT ( 'NONE', #189299 ) ;
#52327 = DIRECTION ( 'NONE',  ( -0.000000000000000000, 1.000000000000000000, 1.734723475976807292E-15 ) ) ;
#52329 = VERTEX_POINT ( 'NONE', #249275 ) ;
#52330 = ADVANCED_FACE ( 'NONE', ( #254056 ), #74188, .T. ) ;
#52331 = DIRECTION ( 'NONE',  ( -0.7071067811865474617, 0.7071067811865474617, 4.937700262164531476E-15 ) ) ;
#52332 = AXIS2_PLACEMENT_3D ( 'NONE', #150241, #108526, #208908 ) ;
#52333 = DIRECTION ( 'NONE',  ( 0.000000000000000000, 1.000000000000000000, 6.938893903907222067E-15 ) ) ;
#52334 = ORIENTED_EDGE ( 'NONE', *, *, #136102, .T. ) ;
#52335 = DIRECTION ( 'NONE',  ( 0.000000000000000000, 8.326672684689590899E-13, -1.000000000000000000 ) ) ;
#52336 = ORIENTED_EDGE ( 'NONE', *, *, #100259, .F. ) ;
#52337 = CIRCLE ( 'NONE', #2457, 11.74999999999999822 ) ;
#52338 = EDGE_CURVE ( 'NONE', #214176, #74197, #233945, .T. ) ;
#52339 = DIRECTION ( 'NONE',  ( 1.000000000000000000, -2.986185139342070877E-16, 6.665775143889692774E-16 ) ) ;
#52340 = DIRECTION ( 'NONE',  ( 0.000000000000000000, -0.000000000000000000, 1.000000000000000000 ) ) ;
#52341 = CIRCLE ( 'NONE', #47677, 6.258578643762712446 ) ;
#52343 = ORIENTED_EDGE ( 'NONE', *, *, #169442, .T. ) ;
#52342 = CIRCLE ( 'NONE', #198111, 0.1000000000000106498 ) ;
#52344 = CARTESIAN_POINT ( 'NONE',  ( 18.59999999999999432, 77.73625713160970463, -158.4544551555068495 ) ) ;
#52345 = EDGE_CURVE ( 'NONE', #162036, #32328, #120827, .T. ) ;
#52346 = EDGE_CURVE ( 'NONE', #145730, #26511, #150564, .T. ) ;
#52347 = CYLINDRICAL_SURFACE ( 'NONE', #168788, 0.09999999999999939493 ) ;
#52348 = EDGE_CURVE ( 'NONE', #30729, #85564, #42410, .T. ) ;
#52349 = ORIENTED_EDGE ( 'NONE', *, *, #105692, .F. ) ;
#52350 = VERTEX_POINT ( 'NONE', #168493 ) ;
#52353 = EDGE_CURVE ( 'NONE', #94765, #16521, #101354, .T. ) ;
#52352 = EDGE_CURVE ( 'NONE', #222558, #24865, #141811, .T. ) ;
#52351 = CARTESIAN_POINT ( 'NONE',  ( 20.30531438145591139, 18.76867081783750635, -228.5135550048062782 ) ) ;
#52354 = ORIENTED_EDGE ( 'NONE', *, *, #239136, .T. ) ;
#52355 = PLANE ( 'NONE',  #92190 ) ;
#52356 = VERTEX_POINT ( 'NONE', #182242 ) ;
#52358 = VERTEX_POINT ( 'NONE', #20613 ) ;
#52357 = DIRECTION ( 'NONE',  ( 1.284434275755705789E-16, -0.7071067811865472397, 0.7071067811865479058 ) ) ;
#52359 = APPLICATION_CONTEXT ( 'automotive_design' ) ;
#52360 = ORIENTED_EDGE ( 'NONE', *, *, #181825, .T. ) ;
#52361 = AXIS2_PLACEMENT_3D ( 'NONE', #83711, #186724, #144991 ) ;
#52362 = CARTESIAN_POINT ( 'NONE',  ( -5.900000000000002132, -11.34999999999999964, 13.90000000000000213 ) ) ;
#52363 = ORIENTED_EDGE ( 'NONE', *, *, #50554, .T. ) ;
#52364 = AXIS2_PLACEMENT_3D ( 'NONE', #199928, #194801, #235189 ) ;
#52367 = ORIENTED_EDGE ( 'NONE', *, *, #166687, .T. ) ;
#52366 = ORIENTED_EDGE ( 'NONE', *, *, #39602, .T. ) ;
#52365 = CARTESIAN_POINT ( 'NONE',  ( -16.93255653858138388, 66.00154854603441379, -56.94146411653471773 ) ) ;
#52368 = AXIS2_PLACEMENT_3D ( 'NONE', #187383, #28332, #50396 ) ;
#52369 = CARTESIAN_POINT ( 'NONE',  ( -23.15000000000000213, 71.75000000001199396, -115.2731074845243171 ) ) ;
#52370 = EDGE_LOOP ( 'NONE', ( #135710, #51698, #48899, #126215 ) ) ;
#52371 = ADVANCED_FACE ( 'NONE', ( #238348 ), #59690, .F. ) ;
#52372 = ADVANCED_FACE ( 'NONE', ( #62283 ), #179679, .T. ) ;
#52373 = AXIS2_PLACEMENT_3D ( 'NONE', #140904, #121375, #117486 ) ;
#52374 = CARTESIAN_POINT ( 'NONE',  ( -20.54999999999999716, 2.400000000011155432, -147.2246219227621111 ) ) ;
#52375 = ORIENTED_EDGE ( 'NONE', *, *, #123107, .T. ) ;
#52376 = EDGE_CURVE ( 'NONE', #248304, #190389, #125787, .T. ) ;
#52377 = CYLINDRICAL_SURFACE ( 'NONE', #91287, 0.09999999999999939493 ) ;
#52378 =( BOUNDED_CURVE ( )  B_SPLINE_CURVE ( 3, ( #199720, #83564, #163152, #144843 ),
 .UNSPECIFIED., .F., .F. ) 
 B_SPLINE_CURVE_WITH_KNOTS ( ( 4, 4 ),
 ( 5.731445031868798168, 5.983100554402348337 ),
 .UNSPECIFIED. ) 
 CURVE ( )  GEOMETRIC_REPRESENTATION_ITEM ( )  RATIONAL_B_SPLINE_CURVE ( ( 1.000000000000000000, 0.9947294176030464508, 0.9947294176030464508, 1.000000000000000000 ) ) 
 REPRESENTATION_ITEM ( '' )  );
#52380 = ORIENTED_EDGE ( 'NONE', *, *, #186320, .F. ) ;
#52379 = FACE_OUTER_BOUND ( 'NONE', #48303, .T. ) ;
#52381 = DIRECTION ( 'NONE',  ( 1.000000000000000000, -0.000000000000000000, -0.000000000000000000 ) ) ;
#52382 = ORIENTED_EDGE ( 'NONE', *, *, #139807, .F. ) ;
#52384 = VECTOR ( 'NONE', #180114, 1000.000000000000000 ) ;
#52383 = CARTESIAN_POINT ( 'NONE',  ( -18.59999999999999787, 70.47363787294415260, -228.3418745167492432 ) ) ;
#52385 = CARTESIAN_POINT ( 'NONE',  ( 21.05000000000000071, 76.00000000001165290, -69.52310748452431710 ) ) ;
#52386 = AXIS2_PLACEMENT_3D ( 'NONE', #135221, #54415, #193944 ) ;
#52387 = VERTEX_POINT ( 'NONE', #19308 ) ;
#52388 = EDGE_CURVE ( 'NONE', #103673, #106788, #38328, .T. ) ;
#52389 = FACE_OUTER_BOUND ( 'NONE', #183034, .T. ) ;
#52390 = TOROIDAL_SURFACE ( 'NONE', #89998, 11.65000000000000036, 0.1000000000000000056 ) ;
#52391 = EDGE_LOOP ( 'NONE', ( #147056, #127727, #175168, #225551 ) ) ;
#52392 = ADVANCED_FACE ( 'NONE', ( #239645 ), #40185, .T. ) ;
#52393 = ORIENTED_EDGE ( 'NONE', *, *, #130909, .T. ) ;
#52394 = CARTESIAN_POINT ( 'NONE',  ( -23.30000000000000426, -11.79999999999999893, -347.0000000000001137 ) ) ;
#52396 = ORIENTED_EDGE ( 'NONE', *, *, #125305, .T. ) ;
#52395 = EDGE_LOOP ( 'NONE', ( #39803, #96764, #116547, #197676 ) ) ;
#52397 = ORIENTED_EDGE ( 'NONE', *, *, #38185, .T. ) ;
#52398 = CYLINDRICAL_SURFACE ( 'NONE', #186136, 0.09999999999999939493 ) ;
#52399 = EDGE_LOOP ( 'NONE', ( #136726, #17774, #127234, #66016, #110359, #247913, #49511, #211177 ) ) ;
#52400 = EDGE_LOOP ( 'NONE', ( #232922, #53902, #38231 ) ) ;
#52401 = CARTESIAN_POINT ( 'NONE',  ( -23.25000000000000000, -11.74999999998884448, -88.75000000000004263 ) ) ;
#52402 = AXIS2_PLACEMENT_3D ( 'NONE', #248690, #247388, #128750 ) ;
#52403 = VERTEX_POINT ( 'NONE', #986 ) ;
#52404 = ADVANCED_FACE ( 'NONE', ( #100098 ), #71655, .F. ) ;
#52405 = DIRECTION ( 'NONE',  ( 0.000000000000000000, 0.2128009952263605065, -0.9770955615653315052 ) ) ;
#52406 = CYLINDRICAL_SURFACE ( 'NONE', #35924, 0.9000000000000014655 ) ;
#52407 = ORIENTED_EDGE ( 'NONE', *, *, #193794, .T. ) ;
#52408 = ORIENTED_EDGE ( 'NONE', *, *, #112335, .T. ) ;
#52409 = ADVANCED_FACE ( 'NONE', ( #161404 ), #60991, .F. ) ;
#52410 = CARTESIAN_POINT ( 'NONE',  ( 18.59999999999998366, 0.000000000000000000, -33.50000000000000000 ) ) ;
#52411 = ORIENTED_EDGE ( 'NONE', *, *, #144477, .F. ) ;
#52412 = AXIS2_PLACEMENT_3D ( 'NONE', #228897, #12436, #108934 ) ;
#52413 = VECTOR ( 'NONE', #114375, 1000.000000000000000 ) ;
#52414 = CIRCLE ( 'NONE', #10745, 0.09999999999998898659 ) ;
#52415 = AXIS2_PLACEMENT_3D ( 'NONE', #154244, #78490, #158096 ) ;
#52416 = CARTESIAN_POINT ( 'NONE',  ( 22.88900146558018989, 67.29609520889948726, -157.3731074845244109 ) ) ;
#52417 = VERTEX_POINT ( 'NONE', #41464 ) ;
#52418 = ORIENTED_EDGE ( 'NONE', *, *, #116819, .F. ) ;
#52419 = FACE_OUTER_BOUND ( 'NONE', #113284, .T. ) ;
#52420 = EDGE_CURVE ( 'NONE', #6309, #139646, #86597, .T. ) ;
#52422 = ORIENTED_EDGE ( 'NONE', *, *, #256211, .F. ) ;
#52421 = DIRECTION ( 'NONE',  ( 1.000000000000000000, -0.000000000000000000, -0.000000000000000000 ) ) ;
#52423 = DIRECTION ( 'NONE',  ( 0.000000000000000000, 7.116814260417676401E-15, -1.000000000000000000 ) ) ;
#52424 = CARTESIAN_POINT ( 'NONE',  ( 23.15000000000000213, 87.48912529308852015, -173.1231074845242688 ) ) ;
#52425 = CARTESIAN_POINT ( 'NONE',  ( 20.95017935633852346, 65.52451072038677182, -128.9456676871338914 ) ) ;
#52426 = CYLINDRICAL_SURFACE ( 'NONE', #7944, 0.09999999999999939493 ) ;
#52427 = CARTESIAN_POINT ( 'NONE',  ( 21.05000000000000071, -9.000000000000000000, -23.60603087734755690 ) ) ;
#52428 = CARTESIAN_POINT ( 'NONE',  ( 23.14999999999999503, 11.75000000001115552, -88.25000000000005684 ) ) ;
#52429 = CARTESIAN_POINT ( 'NONE',  ( 11.60000000000006182, 66.35000000001119247, -23.62310748452479103 ) ) ;
#52430 = CARTESIAN_POINT ( 'NONE',  ( 18.54271179734066521, 38.05662890930041442, -261.2177829373591180 ) ) ;
#52431 = B_SPLINE_CURVE_WITH_KNOTS ( 'NONE', 3,
 ( #244553, #148037, #166346, #47622, #28111, #223697, #146716, #226253, #24255, #107616 ),
 .UNSPECIFIED., .F., .F.,
 ( 4, 3, 3, 4 ),
 ( 0.000000000000000000, 1.004626015991589319E-05, 1.831183478183387304E-05, 2.062343583996250457E-05 ),
 .UNSPECIFIED. ) ;
#52432 = DIRECTION ( 'NONE',  ( 0.000000000000000000, 0.000000000000000000, 1.000000000000000000 ) ) ;
#52433 = VECTOR ( 'NONE', #50883, 1000.000000000000000 ) ;
#52434 = VECTOR ( 'NONE', #172482, 1000.000000000000000 ) ;
#52435 = B_SPLINE_CURVE_WITH_KNOTS ( 'NONE', 3,
 ( #220563, #41946, #158068, #101869, #237561, #127888, #23677, #223117, #126597, #45769 ),
 .UNSPECIFIED., .F., .F.,
 ( 4, 2, 2, 2, 4 ),
 ( 0.000000000000000000, 0.0001660831991681999738, 0.0002491247987522991476, 0.0002906455985443850824, 0.0003321663983364709629 ),
 .UNSPECIFIED. ) ;
#52436 = EDGE_LOOP ( 'NONE', ( #53213, #50007, #150209, #204309, #105295, #157754, #75977 ) ) ;
#52438 = ORIENTED_EDGE ( 'NONE', *, *, #243724, .F. ) ;
#52437 = ORIENTED_EDGE ( 'NONE', *, *, #209683, .F. ) ;
#52439 = CIRCLE ( 'NONE', #48357, 0.09999999999999971412 ) ;
#52440 = ORIENTED_EDGE ( 'NONE', *, *, #110384, .T. ) ;
#52441 = CARTESIAN_POINT ( 'NONE',  ( -20.54999999999999716, -9.399999999988848387, -43.39396912265245021 ) ) ;
#52442 = DIRECTION ( 'NONE',  ( 0.000000000000000000, -0.5826443254699606999, -0.8127272543711416830 ) ) ;
#52444 = CARTESIAN_POINT ( 'NONE',  ( 21.05000000000000071, 1.115600667400684642E-11, -67.00000000000000000 ) ) ;
#52443 = DIRECTION ( 'NONE',  ( -1.000000000000000000, 0.000000000000000000, 0.000000000000000000 ) ) ;
#52445 = EDGE_LOOP ( 'NONE', ( #165280, #164404, #47295 ) ) ;
#52446 = ORIENTED_EDGE ( 'NONE', *, *, #110149, .T. ) ;
#52447 = SHAPE_REPRESENTATION_RELATIONSHIP ( 'NONE' , 'NONE' ,  #213520, #26624 ) ;
#52448 = CARTESIAN_POINT ( 'NONE',  ( 18.50000000000000355, -9.421456145484386369, -40.74198208401926991 ) ) ;
#52449 = CARTESIAN_POINT ( 'NONE',  ( 18.50016250449482058, 10.29766095125179959, -172.9743663933279265 ) ) ;
#52450 = DIRECTION ( 'NONE',  ( 1.000000000000000000, 0.000000000000000000, 0.000000000000000000 ) ) ;
#52451 = EDGE_LOOP ( 'NONE', ( #18392, #30817, #209918, #161057 ) ) ;
#52452 = ORIENTED_EDGE ( 'NONE', *, *, #193984, .T. ) ;
#52453 = AXIS2_PLACEMENT_3D ( 'NONE', #218198, #237789, #17451 ) ;
#52454 = CARTESIAN_POINT ( 'NONE',  ( -20.94999999999999929, -1.851028230129704522, -78.65391326942254580 ) ) ;
#52455 = CARTESIAN_POINT ( 'NONE',  ( -22.59999999999999787, 1.115600667400684642E-11, -100.5000000000000284 ) ) ;
#52456 = DIRECTION ( 'NONE',  ( 0.000000000000000000, 0.000000000000000000, -1.000000000000000000 ) ) ;
#52458 = VERTEX_POINT ( 'NONE', #243482 ) ;
#52457 = FACE_OUTER_BOUND ( 'NONE', #241279, .T. ) ;
#52459 = CARTESIAN_POINT ( 'NONE',  ( 20.94999999999999929, 4.850467289730776344, -121.9657325909983570 ) ) ;
#52460 = LINE ( 'NONE', #206418, #139731 ) ;
#52461 = CARTESIAN_POINT ( 'NONE',  ( -20.94999999999999929, 77.73625713160946304, -124.9544551555067926 ) ) ;
#52462 = LINE ( 'NONE', #195870, #229252 ) ;
#52463 = VERTEX_POINT ( 'NONE', #137952 ) ;
#52464 = CARTESIAN_POINT ( 'NONE',  ( 12.26145404764308999, 66.64858632091046786, -86.04276391697545989 ) ) ;
#52465 = DIRECTION ( 'NONE',  ( 0.000000000000000000, 0.000000000000000000, -1.000000000000000000 ) ) ;
#52466 = DIRECTION ( 'NONE',  ( 1.000000000000000000, 0.000000000000000000, 0.000000000000000000 ) ) ;
#52468 = DIRECTION ( 'NONE',  ( -0.000000000000000000, -1.000000000000000000, -6.982962677686266711E-15 ) ) ;
#52467 = DIRECTION ( 'NONE',  ( 1.000000000000000000, 0.000000000000000000, 0.000000000000000000 ) ) ;
#52470 = EDGE_CURVE ( 'NONE', #86456, #7699, #225741, .T. ) ;
#52469 = DIRECTION ( 'NONE',  ( 0.000000000000000000, -1.000000000000000000, 0.000000000000000000 ) ) ;
#52471 = CARTESIAN_POINT ( 'NONE',  ( 20.94999999999999929, 76.00000000001267608, -203.5231074845243597 ) ) ;
#52472 = AXIS2_PLACEMENT_3D ( 'NONE', #22278, #241323, #26126 ) ;
#52473 = DIRECTION ( 'NONE',  ( 0.000000000000000000, -1.000000000000000000, -6.982962677686266711E-15 ) ) ;
#52474 = CYLINDRICAL_SURFACE ( 'NONE', #172271, 11.74999999999999645 ) ;
#52475 = VECTOR ( 'NONE', #59352, 1000.000000000000227 ) ;
#52476 = CARTESIAN_POINT ( 'NONE',  ( -21.13614978966382196, 69.50089529817834944, -136.5231074845243313 ) ) ;
#52477 = VECTOR ( 'NONE', #178294, 1000.000000000000000 ) ;
#52478 = ORIENTED_EDGE ( 'NONE', *, *, #79236, .T. ) ;
#52479 = CIRCLE ( 'NONE', #219075, 2.000000000000001776 ) ;
#52480 = ORIENTED_EDGE ( 'NONE', *, *, #240919, .F. ) ;
#52481 =( BOUNDED_CURVE ( )  B_SPLINE_CURVE ( 3, ( #83381, #5123, #105506, #84652 ),
 .UNSPECIFIED., .F., .F. ) 
 B_SPLINE_CURVE_WITH_KNOTS ( ( 4, 4 ),
 ( 0.000000000000000000, 1.570796326794908992 ),
 .UNSPECIFIED. ) 
 CURVE ( )  GEOMETRIC_REPRESENTATION_ITEM ( )  RATIONAL_B_SPLINE_CURVE ( ( 1.000000000000000000, 0.8047378541243619399, 0.8047378541243619399, 1.000000000000000000 ) ) 
 REPRESENTATION_ITEM ( '' )  );
#52483 = ORIENTED_EDGE ( 'NONE', *, *, #235684, .F. ) ;
#52482 = STYLED_ITEM ( 'NONE', ( #31988 ), #237827 ) ;
#52484 = CARTESIAN_POINT ( 'NONE',  ( 20.41140022480505323, 65.58956915761027062, -95.40810618088978856 ) ) ;
#52485 = DIRECTION ( 'NONE',  ( -1.000000000000000000, -0.000000000000000000, -0.000000000000000000 ) ) ;
#52486 = ORIENTED_EDGE ( 'NONE', *, *, #36753, .T. ) ;
#52487 = CARTESIAN_POINT ( 'NONE',  ( 18.39999999999999858, 85.60000000001210196, -129.9229180933022576 ) ) ;
#52488 = EDGE_CURVE ( 'NONE', #85468, #187769, #63245, .T. ) ;
#52489 = EDGE_CURVE ( 'NONE', #148648, #115416, #150746, .T. ) ;
#52490 = ORIENTED_EDGE ( 'NONE', *, *, #14978, .F. ) ;
#52491 = EDGE_LOOP ( 'NONE', ( #30861, #95898, #69931, #83189 ) ) ;
#52492 = CARTESIAN_POINT ( 'NONE',  ( 21.30740335185486245, 6.556657922039159203, -66.90106547422419681 ) ) ;
#52493 = CIRCLE ( 'NONE', #227465, 0.1000000000000026840 ) ;
#52494 = VERTEX_POINT ( 'NONE', #8733 ) ;
#52495 = CARTESIAN_POINT ( 'NONE',  ( -16.80117486205003630, 66.05034273169948733, -82.17425261159890226 ) ) ;
#52496 = VECTOR ( 'NONE', #232932, 1000.000000000000000 ) ;
#52497 = FACE_OUTER_BOUND ( 'NONE', #155092, .T. ) ;
#52498 = CARTESIAN_POINT ( 'NONE',  ( -21.14999999999999858, -11.75000000000000000, -2.900000000000001688 ) ) ;
#52499 = EDGE_CURVE ( 'NONE', #205311, #242990, #184067, .T. ) ;
#52500 = CARTESIAN_POINT ( 'NONE',  ( -21.33487959338958362, 6.725558151922345296, -67.00000000000004263 ) ) ;
#52501 = EDGE_CURVE ( 'NONE', #9091, #111624, #85654, .T. ) ;
#52502 = CARTESIAN_POINT ( 'NONE',  ( 22.39999999999999503, 76.00000000001276135, -215.1726782920691505 ) ) ;
#52505 = ORIENTED_EDGE ( 'NONE', *, *, #144570, .F. ) ;
#52504 = DIRECTION ( 'NONE',  ( 0.000000000000000000, -1.000000000000000000, 0.000000000000000000 ) ) ;
#52503 = AXIS2_PLACEMENT_3D ( 'NONE', #19598, #178697, #97806 ) ;
#52507 = LINE ( 'NONE', #177640, #141923 ) ;
#52506 = CARTESIAN_POINT ( 'NONE',  ( 23.14999999999999858, 2.100000000011158274, -167.5000000000000284 ) ) ;
#52508 = FACE_OUTER_BOUND ( 'NONE', #20815, .T. ) ;
#52509 = CARTESIAN_POINT ( 'NONE',  ( -18.50000000000000000, 79.19526988099229925, -196.1889237952725296 ) ) ;
#52510 = AXIS2_PLACEMENT_3D ( 'NONE', #195380, #132829, #212372 ) ;
#52512 = EDGE_CURVE ( 'NONE', #238460, #179010, #129880, .T. ) ;
#52511 = DIRECTION ( 'NONE',  ( 0.000000000000000000, 6.982962677686266711E-15, -1.000000000000000000 ) ) ;
#52513 = CARTESIAN_POINT ( 'NONE',  ( -22.50000000000000000, 64.25000000001195133, -103.0231074845244024 ) ) ;
#52515 = ORIENTED_EDGE ( 'NONE', *, *, #240703, .T. ) ;
#52514 = AXIS2_PLACEMENT_3D ( 'NONE', #60754, #221116, #120774 ) ;
#52516 = SURFACE_SIDE_STYLE ('',( #231193 ) ) ;
#52517 = DIRECTION ( 'NONE',  ( 1.000000000000000000, 0.000000000000000000, 0.000000000000000000 ) ) ;
#52518 = EDGE_CURVE ( 'NONE', #154587, #122321, #155010, .T. ) ;
#52519 = DIRECTION ( 'NONE',  ( -1.000000000000000000, 0.000000000000000000, 0.000000000000000000 ) ) ;
#52520 = VERTEX_POINT ( 'NONE', #165234 ) ;
#52521 = VECTOR ( 'NONE', #243228, 1000.000000000000000 ) ;
#52522 = CARTESIAN_POINT ( 'NONE',  ( 21.14999999999999503, 11.75000000000000000, -3.469446951953614189E-15 ) ) ;
#52523 = CIRCLE ( 'NONE', #44366, 0.09999999999999982514 ) ;
#52524 = EDGE_CURVE ( 'NONE', #225850, #56768, #175896, .T. ) ;
#52525 = AXIS2_PLACEMENT_3D ( 'NONE', #83002, #43913, #179594 ) ;
#52526 = DIRECTION ( 'NONE',  ( 0.000000000000000000, 0.000000000000000000, -1.000000000000000000 ) ) ;
#52527 = DIRECTION ( 'NONE',  ( 0.7071067811865474617, -0.7071067811865474617, -4.937700262164531476E-15 ) ) ;
#52528 = ORIENTED_EDGE ( 'NONE', *, *, #251511, .F. ) ;
#52529 = AXIS2_PLACEMENT_3D ( 'NONE', #141545, #42448, #22918 ) ;
#52530 = ORIENTED_EDGE ( 'NONE', *, *, #233998, .T. ) ;
#52531 = EDGE_CURVE ( 'NONE', #85365, #163018, #234122, .T. ) ;
#52532 = FACE_OUTER_BOUND ( 'NONE', #152270, .T. ) ;
#52533 = DIRECTION ( 'NONE',  ( 0.000000000000000000, 1.000000000000000000, 0.000000000000000000 ) ) ;
#52534 = DIRECTION ( 'NONE',  ( 1.000000000000000000, -3.265361837132813093E-16, -2.280189983783949500E-30 ) ) ;
#52535 = DIRECTION ( 'NONE',  ( 0.000000000000000000, 0.000000000000000000, -1.000000000000000000 ) ) ;
#52536 = AXIS2_PLACEMENT_3D ( 'NONE', #167902, #198329, #219168 ) ;
#52538 = LINE ( 'NONE', #30438, #166813 ) ;
#52537 = DIRECTION ( 'NONE',  ( 0.000000000000000000, 0.000000000000000000, 1.000000000000000000 ) ) ;
#52539 = DIRECTION ( 'NONE',  ( -0.000000000000000000, 0.8660254037844383745, -0.5000000000000003331 ) ) ;
#52540 = CARTESIAN_POINT ( 'NONE',  ( 15.69410316191958898, 9.356746017089401235, -50.70335972136417979 ) ) ;
#52541 = DIRECTION ( 'NONE',  ( 1.000000000000000000, 0.000000000000000000, -0.000000000000000000 ) ) ;
#52542 = ORIENTED_EDGE ( 'NONE', *, *, #36669, .F. ) ;
#52543 = CARTESIAN_POINT ( 'NONE',  ( -17.71734398241073194, 10.84235722847571459, -190.7251382530055821 ) ) ;
#52545 = ORIENTED_EDGE ( 'NONE', *, *, #232400, .F. ) ;
#52544 = DIRECTION ( 'NONE',  ( -0.000000000000000000, 0.2128009952263603677, -0.9770955615653313941 ) ) ;
#52546 = CARTESIAN_POINT ( 'NONE',  ( 23.50000000000005684, 73.52684270758111040, -52.27034697567518862 ) ) ;
#52547 = DIRECTION ( 'NONE',  ( 0.000000000000000000, -0.7397360091702823714, 0.6728971962616756564 ) ) ;
#52549 = CARTESIAN_POINT ( 'NONE',  ( -18.52328366898032286, -0.8637155613953195754, -242.3456170079330150 ) ) ;
#52548 = DIRECTION ( 'NONE',  ( -1.000000000000000000, 0.000000000000000000, 0.000000000000000000 ) ) ;
#52550 = CARTESIAN_POINT ( 'NONE',  ( 20.94999999999999929, 85.00000000001149658, -45.91707660717670336 ) ) ;
#52551 = CARTESIAN_POINT ( 'NONE',  ( 20.94999999999999929, 11.75000000001115552, -194.2161343370218844 ) ) ;
#52553 = ORIENTED_EDGE ( 'NONE', *, *, #84789, .T. ) ;
#52552 = DIRECTION ( 'NONE',  ( -1.000000000000000000, 0.000000000000000000, 0.000000000000000000 ) ) ;
#52554 = CARTESIAN_POINT ( 'NONE',  ( 20.12500000000000000, 51.97441255244040548, -232.0063394385699667 ) ) ;
#52555 = CARTESIAN_POINT ( 'NONE',  ( -16.97683809663752186, 50.93224991157930504, -232.2540631895259082 ) ) ;
#52556 = CARTESIAN_POINT ( 'NONE',  ( -23.15000000000000213, 4.350000000011156054, -45.75000000000000711 ) ) ;
#52557 = CARTESIAN_POINT ( 'NONE',  ( -23.15000000000000213, 19.97490019448090948, -235.9060780337186145 ) ) ;
#52558 = VERTEX_POINT ( 'NONE', #105210 ) ;
#52559 = FACE_OUTER_BOUND ( 'NONE', #217431, .T. ) ;
#52560 = AXIS2_PLACEMENT_3D ( 'NONE', #137959, #15488, #94998 ) ;
#52561 = ORIENTED_EDGE ( 'NONE', *, *, #255231, .F. ) ;
#52562 = AXIS2_PLACEMENT_3D ( 'NONE', #76514, #214747, #136471 ) ;
#52563 = VECTOR ( 'NONE', #146624, 1000.000000000000000 ) ;
#52564 = LINE ( 'NONE', #227358, #167457 ) ;
#52565 = VERTEX_POINT ( 'NONE', #227769 ) ;
#52566 = CARTESIAN_POINT ( 'NONE',  ( -21.14999999999999858, 87.65000000001214175, -136.5231074845242176 ) ) ;
#52567 = ORIENTED_EDGE ( 'NONE', *, *, #147099, .F. ) ;
#52568 = AXIS2_PLACEMENT_3D ( 'NONE', #3626, #171736, #169167 ) ;
#52569 = EDGE_CURVE ( 'NONE', #85875, #201436, #29609, .T. ) ;
#52570 = FACE_OUTER_BOUND ( 'NONE', #33885, .T. ) ;
#52572 = EDGE_CURVE ( 'NONE', #99532, #175526, #13390, .T. ) ;
#52571 = DIRECTION ( 'NONE',  ( 1.000000000000000000, -2.849773892568378313E-16, 7.728835255496647986E-17 ) ) ;
#52573 = LINE ( 'NONE', #94272, #6045 ) ;
#52574 = EDGE_LOOP ( 'NONE', ( #191339, #197002, #244859 ) ) ;
#52575 = ADVANCED_FACE ( 'NONE', ( #184792 ), #186086, .F. ) ;
#52577 = EDGE_CURVE ( 'NONE', #19725, #118478, #148235, .T. ) ;
#52576 = CIRCLE ( 'NONE', #73470, 0.09999999999999939493 ) ;
#52578 = CARTESIAN_POINT ( 'NONE',  ( -16.87683809663750267, 9.949999999999983302, -13.40236401819648115 ) ) ;
#52579 = DIRECTION ( 'NONE',  ( 0.000000000000000000, -1.000000000000000000, 0.000000000000000000 ) ) ;
#52580 = AXIS2_PLACEMENT_3D ( 'NONE', #134326, #212612, #150082 ) ;
#52581 = ADVANCED_FACE ( 'NONE', ( #208231 ), #25866, .T. ) ;
#52582 = LINE ( 'NONE', #151727, #216397 ) ;
#52583 = DIRECTION ( 'NONE',  ( -1.000000000000000000, 0.000000000000000000, -0.000000000000000000 ) ) ;
#52584 = DIRECTION ( 'NONE',  ( -1.000000000000000000, 0.000000000000000000, -0.000000000000000000 ) ) ;
#52585 = ADVANCED_FACE ( 'NONE', ( #68708 ), #204903, .F. ) ;
#52586 = ORIENTED_EDGE ( 'NONE', *, *, #18710, .F. ) ;
#52588 = EDGE_CURVE ( 'NONE', #79626, #79879, #159667, .T. ) ;
#52587 = DIRECTION ( 'NONE',  ( 1.000000000000000000, -0.000000000000000000, -0.000000000000000000 ) ) ;
#52589 = ORIENTED_EDGE ( 'NONE', *, *, #120913, .T. ) ;
#52591 = ORIENTED_EDGE ( 'NONE', *, *, #237248, .F. ) ;
#52590 = PLANE ( 'NONE',  #110600 ) ;
#52592 = ORIENTED_EDGE ( 'NONE', *, *, #69077, .F. ) ;
#52593 = CARTESIAN_POINT ( 'NONE',  ( -23.25000000000000355, 5.650000000011139001, -121.3500000000000369 ) ) ;
#52594 = CARTESIAN_POINT ( 'NONE',  ( -16.87487986503753845, 66.04999244492699972, -190.8731327448377044 ) ) ;
#52595 = DIRECTION ( 'NONE',  ( 0.000000000000000000, -0.2128009952263604232, 0.9770955615653316162 ) ) ;
#52596 = EDGE_CURVE ( 'NONE', #121380, #23903, #17462, .T. ) ;
#52597 = DIRECTION ( 'NONE',  ( 0.000000000000000000, -0.8430646840892555005, -0.5378121776619452232 ) ) ;
#52599 = ORIENTED_EDGE ( 'NONE', *, *, #134514, .F. ) ;
#52598 = TOROIDAL_SURFACE ( 'NONE', #231682, 0.2000000000000000111, 0.1000000000000000056 ) ;
#52600 = CYLINDRICAL_SURFACE ( 'NONE', #238643, 0.1000000000000028644 ) ;
#52601 = CARTESIAN_POINT ( 'NONE',  ( 18.60000000000000142, -9.523946312306554418, -140.8820279953382908 ) ) ;
#52602 = VERTEX_POINT ( 'NONE', #222168 ) ;
#52603 = ADVANCED_FACE ( 'NONE', ( #140069 ), #219617, .T. ) ;
#52605 = EDGE_LOOP ( 'NONE', ( #100837, #255828, #214806, #117944, #56407, #132068, #106730, #186458, #37392, #206565, #28503 ) ) ;
#52604 = CARTESIAN_POINT ( 'NONE',  ( -16.92570016628983609, 66.04121104227213834, -115.6437581545634004 ) ) ;
#52606 = LINE ( 'NONE', #193429, #77741 ) ;
#52607 = CARTESIAN_POINT ( 'NONE',  ( -21.44999999999999929, 65.86663596189677605, -213.5709895136416776 ) ) ;
#52608 = ADVANCED_FACE ( 'NONE', ( #123112 ), #198773, .T. ) ;
#52609 = EDGE_CURVE ( 'NONE', #235213, #252182, #246605, .T. ) ;
#52610 = AXIS2_PLACEMENT_3D ( 'NONE', #229876, #145182, #125633 ) ;
#52611 = ORIENTED_EDGE ( 'NONE', *, *, #99967, .T. ) ;
#52612 = AXIS2_PLACEMENT_3D ( 'NONE', #41288, #3389, #82910 ) ;
#52613 = CIRCLE ( 'NONE', #252509, 11.65000000000000036 ) ;
#52614 = VECTOR ( 'NONE', #219893, 1000.000000000000000 ) ;
#52615 = ORIENTED_EDGE ( 'NONE', *, *, #219697, .T. ) ;
#52616 = CARTESIAN_POINT ( 'NONE',  ( -20.54999999999999716, 2.000000000011154189, -180.7246219227620543 ) ) ;
#52617 = EDGE_CURVE ( 'NONE', #60849, #228310, #238220, .T. ) ;
#52618 = CARTESIAN_POINT ( 'NONE',  ( -20.93975676684922504, 18.37846419038447010, -236.9325101954432853 ) ) ;
#52619 = ORIENTED_EDGE ( 'NONE', *, *, #124539, .T. ) ;
#52620 = DIRECTION ( 'NONE',  ( 0.000000000000000000, 0.000000000000000000, -1.000000000000000000 ) ) ;
#52621 = EDGE_CURVE ( 'NONE', #182212, #191326, #69271, .T. ) ;
#52622 = DIRECTION ( 'NONE',  ( 1.000000000000000000, 0.000000000000000000, 0.000000000000000000 ) ) ;
#52623 = EDGE_CURVE ( 'NONE', #114526, #200649, #46679, .T. ) ;
#52624 = CARTESIAN_POINT ( 'NONE',  ( 18.59999999999999787, 70.10000000001235776, -159.8040077198679683 ) ) ;
#52625 = CIRCLE ( 'NONE', #65290, 0.1000000000000008799 ) ;
#52626 = TOROIDAL_SURFACE ( 'NONE', #214946, 6.258578643762712446, 0.1000000000000000056 ) ;
#52627 = VERTEX_POINT ( 'NONE', #99651 ) ;
#52628 = CARTESIAN_POINT ( 'NONE',  ( 21.76363531954645936, 68.98706345214095847, -203.6221093588238489 ) ) ;
#52629 = CIRCLE ( 'NONE', #198389, 0.1000000000000028644 ) ;
#52630 = ORIENTED_EDGE ( 'NONE', *, *, #104510, .F. ) ;
#52631 = LINE ( 'NONE', #187043, #185262 ) ;
#52632 = FACE_OUTER_BOUND ( 'NONE', #116535, .T. ) ;
#52634 = ORIENTED_EDGE ( 'NONE', *, *, #177955, .T. ) ;
#52633 = CARTESIAN_POINT ( 'NONE',  ( -2.995603634470891112E-16, -11.74999999998884448, -125.2500000000000284 ) ) ;
#52635 = CARTESIAN_POINT ( 'NONE',  ( -5.900000000000002132, -11.75000000000000000, 14.10000000000000142 ) ) ;
#52636 = FACE_OUTER_BOUND ( 'NONE', #191211, .T. ) ;
#52637 = CARTESIAN_POINT ( 'NONE',  ( 21.05000000000000071, 76.00000000001260503, -191.3731074845243540 ) ) ;
#52638 = CARTESIAN_POINT ( 'NONE',  ( -16.87331047859651179, 22.97806745954242302, -230.9350634111226270 ) ) ;
#52639 = CARTESIAN_POINT ( 'NONE',  ( 20.85000000000000142, 75.83895117929318985, -103.3072973288845162 ) ) ;
#52640 = DIRECTION ( 'NONE',  ( 1.000000000000000000, 0.000000000000000000, 0.000000000000000000 ) ) ;
#52641 = CARTESIAN_POINT ( 'NONE',  ( 21.08035267497491105, 6.331706839794169817, -66.91731137522391748 ) ) ;
#52643 = VERTEX_POINT ( 'NONE', #100917 ) ;
#52642 = CARTESIAN_POINT ( 'NONE',  ( -20.94999999999999929, 68.97833521811131163, -32.18954208262707795 ) ) ;
#52644 = AXIS2_PLACEMENT_3D ( 'NONE', #101783, #122693, #149957 ) ;
#52645 = CARTESIAN_POINT ( 'NONE',  ( -20.64999999999999858, 1.115600667400684642E-11, -134.0000000000000000 ) ) ;
#52646 = CYLINDRICAL_SURFACE ( 'NONE', #140364, 0.1000000000000028644 ) ;
#52647 = LINE ( 'NONE', #74832, #7417 ) ;
#52648 = FACE_OUTER_BOUND ( 'NONE', #139348, .T. ) ;
#52649 = CIRCLE ( 'NONE', #178155, 0.1000000000000028644 ) ;
#52650 = ORIENTED_EDGE ( 'NONE', *, *, #20814, .T. ) ;
#52651 = ADVANCED_FACE ( 'NONE', ( #124396 ), #119261, .F. ) ;
#52652 = DIRECTION ( 'NONE',  ( 0.000000000000000000, -0.8700118002898322711, 0.4930308989875231140 ) ) ;
#52653 = DIRECTION ( 'NONE',  ( -1.000000000000000000, -0.000000000000000000, -0.000000000000000000 ) ) ;
#52654 = VECTOR ( 'NONE', #126649, 1000.000000000000000 ) ;
#52655 = EDGE_CURVE ( 'NONE', #59337, #9791, #200826, .T. ) ;
#52656 = ORIENTED_EDGE ( 'NONE', *, *, #146101, .T. ) ;
#52657 = CIRCLE ( 'NONE', #198426, 0.09999999999999939493 ) ;
#52658 = CIRCLE ( 'NONE', #65141, 0.1000000000000026007 ) ;
#52659 = CARTESIAN_POINT ( 'NONE',  ( 18.59999999999997655, 76.00000000001142553, -36.02310748452432421 ) ) ;
#52660 = CARTESIAN_POINT ( 'NONE',  ( -16.94037747912386394, 10.01353938249748765, -79.55113095797554479 ) ) ;
#52661 =( GEOMETRIC_REPRESENTATION_CONTEXT ( 3 ) GLOBAL_UNCERTAINTY_ASSIGNED_CONTEXT ( ( #220031 ) ) GLOBAL_UNIT_ASSIGNED_CONTEXT ( ( #248138, #229865, #210312 ) ) REPRESENTATION_CONTEXT ( 'NONE', 'WORKASPACE' ) );
#52662 = EDGE_CURVE ( 'NONE', #121787, #103650, #75927, .T. ) ;
#52663 = VERTEX_POINT ( 'NONE', #61849 ) ;
#52665 = EDGE_CURVE ( 'NONE', #188424, #205311, #42286, .T. ) ;
#52664 = DIRECTION ( 'NONE',  ( 0.000000000000000000, -1.000000000000000000, -6.938893903907030216E-14 ) ) ;
#52666 = ORIENTED_EDGE ( 'NONE', *, *, #50436, .T. ) ;
#52667 = CARTESIAN_POINT ( 'NONE',  ( 20.95512840106821528, 65.37615130623873938, -124.3206282637254816 ) ) ;
#52668 = ORIENTED_EDGE ( 'NONE', *, *, #232407, .F. ) ;
#52669 = FACE_OUTER_BOUND ( 'NONE', #31794, .T. ) ;
#52670 = ORIENTED_EDGE ( 'NONE', *, *, #245732, .F. ) ;
#52671 = CARTESIAN_POINT ( 'NONE',  ( 20.73486653747090003, 11.52084357182978458, -219.8296352432475658 ) ) ;
#52672 = ORIENTED_EDGE ( 'NONE', *, *, #72927, .F. ) ;
#52674 = ORIENTED_EDGE ( 'NONE', *, *, #186013, .T. ) ;
#52673 = ORIENTED_EDGE ( 'NONE', *, *, #229146, .F. ) ;
#52675 = DIRECTION ( 'NONE',  ( -2.952720810173288619E-16, 1.000000000000000000, 0.000000000000000000 ) ) ;
#52677 = ORIENTED_EDGE ( 'NONE', *, *, #23208, .T. ) ;
#52676 = CARTESIAN_POINT ( 'NONE',  ( -21.55000000000000426, 44.76114064897694789, -237.4293191035423831 ) ) ;
#52678 = CARTESIAN_POINT ( 'NONE',  ( 20.94999999999999929, 65.70729864260985664, -64.06574559737245522 ) ) ;
#52680 = ORIENTED_EDGE ( 'NONE', *, *, #249892, .F. ) ;
#52679 = CIRCLE ( 'NONE', #94373, 11.65000000000000036 ) ;
#52682 = EDGE_CURVE ( 'NONE', #79119, #253401, #221644, .T. ) ;
#52681 = VECTOR ( 'NONE', #176496, 1000.000000000000000 ) ;
#52683 = AXIS2_PLACEMENT_3D ( 'NONE', #16257, #116611, #37103 ) ;
#52684 = ORIENTED_EDGE ( 'NONE', *, *, #160111, .F. ) ;
#52685 = AXIS2_PLACEMENT_3D ( 'NONE', #213619, #31184, #254023 ) ;
#52686 = PLANE ( 'NONE',  #3791 ) ;
#52687 = DIRECTION ( 'NONE',  ( 1.000000000000000000, -0.000000000000000000, -0.000000000000000000 ) ) ;
#52688 = CARTESIAN_POINT ( 'NONE',  ( 18.59999999999999076, 69.01799029515596828, -166.3269553662681233 ) ) ;
#52689 = EDGE_LOOP ( 'NONE', ( #109804, #171911, #131763, #19039 ) ) ;
#52690 = AXIS2_PLACEMENT_3D ( 'NONE', #201453, #118071, #101024 ) ;
#52691 = CARTESIAN_POINT ( 'NONE',  ( -20.94999999999999929, 64.25000000001210765, -129.5083017138703667 ) ) ;
#52692 = CIRCLE ( 'NONE', #131814, 0.09999999999998898659 ) ;
#52693 = CARTESIAN_POINT ( 'NONE',  ( -18.43599941264910314, -9.519327428583675754, -73.97297678952132571 ) ) ;
#52694 = FACE_OUTER_BOUND ( 'NONE', #250480, .T. ) ;
#52695 = ORIENTED_EDGE ( 'NONE', *, *, #213625, .F. ) ;
#52696 = CARTESIAN_POINT ( 'NONE',  ( -20.90000000000000213, 1.786320531569725478, -11.50977166988710820 ) ) ;
#52697 = EDGE_CURVE ( 'NONE', #50748, #104681, #121831, .T. ) ;
#52698 =( NAMED_UNIT ( * ) PLANE_ANGLE_UNIT ( ) SI_UNIT ( $, .RADIAN. ) );
#52699 = EDGE_LOOP ( 'NONE', ( #121674, #250689, #41449, #41502 ) ) ;
#52700 = EDGE_CURVE ( 'NONE', #109775, #253844, #136487, .T. ) ;
#52701 = FACE_OUTER_BOUND ( 'NONE', #231149, .T. ) ;
#52702 = VERTEX_POINT ( 'NONE', #135170 ) ;
#52703 = CARTESIAN_POINT ( 'NONE',  ( -20.94999999999999929, 64.35000000001220144, -143.3069731475025321 ) ) ;
#52704 = VERTEX_POINT ( 'NONE', #16540 ) ;
#52705 = CIRCLE ( 'NONE', #240173, 0.1000000000000124678 ) ;
#52706 = AXIS2_PLACEMENT_3D ( 'NONE', #63065, #22696, #240434 ) ;
#52707 = VECTOR ( 'NONE', #181842, 1000.000000000000000 ) ;
#52708 = CARTESIAN_POINT ( 'NONE',  ( -12.93407622233967658, 25.11330806876552657, -232.6826121690050684 ) ) ;
#52709 = LINE ( 'NONE', #132256, #106262 ) ;
#52710 = ORIENTED_EDGE ( 'NONE', *, *, #243861, .F. ) ;
#52711 = EDGE_LOOP ( 'NONE', ( #48072, #76761, #247853, #257726 ) ) ;
#52712 = CARTESIAN_POINT ( 'NONE',  ( -21.05000000000000071, 74.75000000001232081, -162.0231074845243597 ) ) ;
#52713 = CARTESIAN_POINT ( 'NONE',  ( 22.10000000000000497, 3.362550747017869490, 28.82623795144604983 ) ) ;
#52714 = ORIENTED_EDGE ( 'NONE', *, *, #199562, .T. ) ;
#52715 = VERTEX_POINT ( 'NONE', #193891 ) ;
#52716 = EDGE_CURVE ( 'NONE', #164020, #178186, #142535, .T. ) ;
#52717 = CARTESIAN_POINT ( 'NONE',  ( 23.15000000000000213, -11.64999999998883595, -63.89999999999999858 ) ) ;
#52718 = DIRECTION ( 'NONE',  ( 0.000000000000000000, 9.769962616701377556E-15, 1.000000000000000000 ) ) ;
#52719 = EDGE_CURVE ( 'NONE', #255897, #6721, #137734, .T. ) ;
#52720 = EDGE_LOOP ( 'NONE', ( #123761, #15712, #17403, #205999 ) ) ;
#52721 = AXIS2_PLACEMENT_3D ( 'NONE', #231712, #210852, #113032 ) ;
#52722 = EDGE_CURVE ( 'NONE', #175406, #230288, #192395, .T. ) ;
#52723 = ORIENTED_EDGE ( 'NONE', *, *, #8096, .F. ) ;
#52724 = B_SPLINE_CURVE_WITH_KNOTS ( 'NONE', 3,
 ( #27275, #230583, #207169, #166782, #51906, #8957, #228005, #50628, #248856, #70246 ),
 .UNSPECIFIED., .F., .F.,
 ( 4, 2, 2, 2, 4 ),
 ( 0.000000000000000000, 0.0001660831991681949865, 0.0002491247987522924798, 0.0002906455985443746198, 0.0003321663983364568141 ),
 .UNSPECIFIED. ) ;
#52725 = CARTESIAN_POINT ( 'NONE',  ( 20.85000000000000142, 43.30036367478129478, -245.0872390055602352 ) ) ;
#52726 = LINE ( 'NONE', #214380, #184563 ) ;
#52727 = EDGE_CURVE ( 'NONE', #59827, #143912, #96559, .T. ) ;
#52728 = CARTESIAN_POINT ( 'NONE',  ( -21.05000000000000071, 1.115600667400684642E-11, -41.40000000000000568 ) ) ;
#52730 = ORIENTED_EDGE ( 'NONE', *, *, #1459, .T. ) ;
#52729 = CARTESIAN_POINT ( 'NONE',  ( -18.40000000000000213, 64.25000000001261924, -190.8731074845244393 ) ) ;
#52731 = AXIS2_PLACEMENT_3D ( 'NONE', #189945, #249915, #71298 ) ;
#52732 = DIRECTION ( 'NONE',  ( 0.000000000000000000, 2.891205793294679805E-16, -1.000000000000000000 ) ) ;
#52733 = CARTESIAN_POINT ( 'NONE',  ( 0.8999999999999993561, -11.65000000000000036, 23.40000000000000568 ) ) ;
#52734 = CIRCLE ( 'NONE', #181929, 11.90000000000000746 ) ;
#52735 = CARTESIAN_POINT ( 'NONE',  ( -13.40000000000000036, -12.25000000000000178, 15.00000000000000355 ) ) ;
#52736 = EDGE_CURVE ( 'NONE', #209114, #257571, #117439, .T. ) ;
#52738 = CARTESIAN_POINT ( 'NONE',  ( -16.94107738177415357, 60.85118289042637940, -221.1214263997032390 ) ) ;
#52737 = CARTESIAN_POINT ( 'NONE',  ( 21.13435531349811569, 76.00000000001169553, -76.01682854811622292 ) ) ;
#52740 = AXIS2_PLACEMENT_3D ( 'NONE', #190741, #211563, #29113 ) ;
#52739 = DIRECTION ( 'NONE',  ( 1.836970198721029934E-16, 1.000000000000000000, 6.982962677686266711E-15 ) ) ;
#52741 = VECTOR ( 'NONE', #124230, 1000.000000000000000 ) ;
#52742 = CARTESIAN_POINT ( 'NONE',  ( 18.46858270002952196, -9.474202674699409243, -107.6020219347038704 ) ) ;
#52743 = FACE_OUTER_BOUND ( 'NONE', #9139, .T. ) ;
#52744 = CARTESIAN_POINT ( 'NONE',  ( -21.05000000000000071, 43.57281345108133053, -239.9888335660389487 ) ) ;
#52746 = ORIENTED_EDGE ( 'NONE', *, *, #177579, .T. ) ;
#52745 = AXIS2_PLACEMENT_3D ( 'NONE', #41860, #2692, #1406 ) ;
#52747 = ORIENTED_EDGE ( 'NONE', *, *, #195130, .T. ) ;
#52748 = DIRECTION ( 'NONE',  ( 1.000000000000000000, 0.000000000000000000, 0.000000000000000000 ) ) ;
#52749 = CIRCLE ( 'NONE', #198517, 0.09999999999998898659 ) ;
#52750 = PLANE ( 'NONE',  #194342 ) ;
#52751 = ORIENTED_EDGE ( 'NONE', *, *, #188211, .F. ) ;
#52752 = AXIS2_PLACEMENT_3D ( 'NONE', #189196, #50929, #91378 ) ;
#52753 = CARTESIAN_POINT ( 'NONE',  ( 20.94999999999999929, 85.00000000001179501, -79.01707660717669057 ) ) ;
#52754 = DIRECTION ( 'NONE',  ( -1.000000000000000000, -0.000000000000000000, -0.000000000000000000 ) ) ;
#52755 = ORIENTED_EDGE ( 'NONE', *, *, #211614, .T. ) ;
#52756 = EDGE_LOOP ( 'NONE', ( #108647, #181132, #222340, #44602 ) ) ;
#52757 = CARTESIAN_POINT ( 'NONE',  ( -23.49999999999994316, 64.35000000001120668, -26.12310748452479103 ) ) ;
#52758 = DIRECTION ( 'NONE',  ( 1.000000000000000000, 0.000000000000000000, 0.000000000000000000 ) ) ;
#52759 = VERTEX_POINT ( 'NONE', #138996 ) ;
#52760 = AXIS2_PLACEMENT_3D ( 'NONE', #128139, #222056, #244202 ) ;
#52761 = DIRECTION ( 'NONE',  ( 0.000000000000000000, 0.1350103645451876666, -0.9908441862701600211 ) ) ;
#52763 = VERTEX_POINT ( 'NONE', #213432 ) ;
#52762 = LINE ( 'NONE', #74940, #105991 ) ;
#52764 = LINE ( 'NONE', #193583, #241175 ) ;
#52766 = VERTEX_POINT ( 'NONE', #17788 ) ;
#52765 = DIRECTION ( 'NONE',  ( -1.000000000000000000, -1.394253735153568729E-16, -2.602809386958776729E-16 ) ) ;
#52767 = DIRECTION ( 'NONE',  ( 0.000000000000000000, 6.982962677686266711E-15, -1.000000000000000000 ) ) ;
#52768 = CARTESIAN_POINT ( 'NONE',  ( -16.92507428761701505, 9.950000000011138823, -46.21339745962156087 ) ) ;
#52769 = FACE_OUTER_BOUND ( 'NONE', #79827, .T. ) ;
#52770 = CARTESIAN_POINT ( 'NONE',  ( 21.05000000000000071, 6.724511449164477739, -231.8762197454659884 ) ) ;
#52772 = CARTESIAN_POINT ( 'NONE',  ( 20.50589344624992449, 10.48318793148740546, -108.0729949786726536 ) ) ;
#52771 = CARTESIAN_POINT ( 'NONE',  ( -20.94999999999999929, 76.00000000001244871, -170.0231074845243597 ) ) ;
#52774 = EDGE_CURVE ( 'NONE', #38011, #122081, #56896, .T. ) ;
#52773 = LINE ( 'NONE', #12407, #257790 ) ;
#52775 = DIRECTION ( 'NONE',  ( 0.000000000000000000, 0.8814952561688444987, -0.4721928772777320149 ) ) ;
#52776 = CARTESIAN_POINT ( 'NONE',  ( -18.59999994787167310, 85.52363768977448899, -163.1406579497524376 ) ) ;
#52777 = VECTOR ( 'NONE', #60208, 1000.000000000000000 ) ;
#52778 = VECTOR ( 'NONE', #66926, 1000.000000000000000 ) ;
#52779 = CARTESIAN_POINT ( 'NONE',  ( 21.05000000000000071, 1.542939424703665630, -230.7237943920232226 ) ) ;
#52780 = AXIS2_PLACEMENT_3D ( 'NONE', #168143, #29895, #229367 ) ;
#52782 = DIRECTION ( 'NONE',  ( 1.000000000000000000, 0.000000000000000000, 0.000000000000000000 ) ) ;
#52781 = AXIS2_PLACEMENT_3D ( 'NONE', #143592, #223119, #35834 ) ;
#52783 = ORIENTED_EDGE ( 'NONE', *, *, #62845, .T. ) ;
#52784 = CARTESIAN_POINT ( 'NONE',  ( -16.94107738177415357, 10.01423928514777728, -79.55000000000003979 ) ) ;
#52785 = VERTEX_POINT ( 'NONE', #215988 ) ;
#52786 = PLANE ( 'NONE',  #122786 ) ;
#52787 = ORIENTED_EDGE ( 'NONE', *, *, #234296, .F. ) ;
#52788 = DIRECTION ( 'NONE',  ( -1.000000000000000000, 1.836970198721029934E-16, 1.282749433769087582E-30 ) ) ;
#52789 = EDGE_CURVE ( 'NONE', #163445, #136731, #238411, .T. ) ;
#52790 = DIRECTION ( 'NONE',  ( 0.000000000000000000, -0.4721928772777346239, -0.8814952561688430555 ) ) ;
#52791 = ADVANCED_FACE ( 'NONE', ( #20393 ), #192075, .T. ) ;
#52792 = EDGE_CURVE ( 'NONE', #203870, #186764, #157354, .T. ) ;
#52793 = ORIENTED_EDGE ( 'NONE', *, *, #34418, .F. ) ;
#52794 = AXIS2_PLACEMENT_3D ( 'NONE', #215746, #93240, #91961 ) ;
#52795 = CARTESIAN_POINT ( 'NONE',  ( -21.09096482362050295, 30.83537840773808725, -252.1168136673605602 ) ) ;
#52796 = AXIS2_PLACEMENT_3D ( 'NONE', #71461, #126264, #85829 ) ;
#52797 = CIRCLE ( 'NONE', #198558, 4.099999999999998757 ) ;
#52798 = B_SPLINE_CURVE_WITH_KNOTS ( 'NONE', 3,
 ( #50245, #227610, #48976, #69853, #105057, #209329, #226309, #204193, #228908, #163808, #4698, #67259, #184637, #208077, #25581, #85499, #145506, #243319, #245909, #29461, #225027, #26881 ),
 .UNSPECIFIED., .F., .F.,
 ( 4, 3, 3, 3, 3, 3, 3, 4 ),
 ( 0.000000000000000000, 7.307836821080901168E-06, 4.161455748548376624E-05, 7.576591810647682044E-05, 0.0001098090429817505560, 0.0001438003617351163335, 0.0001777914035423660871, 0.0002117966137403033873 ),
 .UNSPECIFIED. ) ;
#52799 = EDGE_LOOP ( 'NONE', ( #54818, #119761, #19620, #89501 ) ) ;
#52800 = ORIENTED_EDGE ( 'NONE', *, *, #173531, .F. ) ;
#52801 = CARTESIAN_POINT ( 'NONE',  ( -20.85000000000000142, -1.835859311432481045, -112.0044391687985694 ) ) ;
#52802 = CARTESIAN_POINT ( 'NONE',  ( 20.85000000000000142, -1.835859311432481045, -145.5044391687985694 ) ) ;
#52803 = AXIS2_PLACEMENT_3D ( 'NONE', #47794, #186050, #226427 ) ;
#52804 = DIRECTION ( 'NONE',  ( 1.000000000000000000, 0.000000000000000000, 0.000000000000000000 ) ) ;
#52805 = CARTESIAN_POINT ( 'NONE',  ( 12.33938619321247465, 26.81104512947605656, -233.6567807927322917 ) ) ;
#52806 = CARTESIAN_POINT ( 'NONE',  ( -20.94999999999999929, 77.83534155023671985, -158.4679561919613491 ) ) ;
#52807 = ADVANCED_FACE ( 'NONE', ( #175613 ), #156068, .F. ) ;
#52809 = DIRECTION ( 'NONE',  ( 0.000000000000000000, 0.000000000000000000, -1.000000000000000000 ) ) ;
#52808 = CARTESIAN_POINT ( 'NONE',  ( -23.15000000000000213, -6.688413578037177842, -212.5825622730469036 ) ) ;
#52810 = DIRECTION ( 'NONE',  ( 0.000000000000000000, -0.8660254037844377084, -0.5000000000000016653 ) ) ;
#52812 = ORIENTED_EDGE ( 'NONE', *, *, #111758, .T. ) ;
#52811 = DIRECTION ( 'NONE',  ( -0.7071067811865475727, 0.7071067811865475727, 4.937700262164531476E-15 ) ) ;
#52814 = CARTESIAN_POINT ( 'NONE',  ( 23.15000000000000213, -11.48912529306489994, -97.40000000000004832 ) ) ;
#52813 = DIRECTION ( 'NONE',  ( 0.000000000000000000, 0.000000000000000000, 1.000000000000000000 ) ) ;
#52815 = DIRECTION ( 'NONE',  ( 1.000000000000000000, -0.000000000000000000, -0.000000000000000000 ) ) ;
#52816 = ORIENTED_EDGE ( 'NONE', *, *, #132501, .F. ) ;
#52817 = FACE_OUTER_BOUND ( 'NONE', #17328, .T. ) ;
#52818 = CARTESIAN_POINT ( 'NONE',  ( -18.59999999999999787, -9.499999999988849808, -41.60000000000000142 ) ) ;
#52819 = DIRECTION ( 'NONE',  ( 1.000000000000000000, 0.000000000000000000, 0.000000000000000000 ) ) ;
#52820 = EDGE_LOOP ( 'NONE', ( #186963, #120121, #174081, #163922 ) ) ;
#52821 = CARTESIAN_POINT ( 'NONE',  ( -16.80100426158792715, 60.95459208743462654, -221.0117235116689756 ) ) ;
#52822 = AXIS2_PLACEMENT_3D ( 'NONE', #156386, #54677, #238455 ) ;
#52823 = CARTESIAN_POINT ( 'NONE',  ( 21.05000000000000071, 76.00000000001213607, -136.5231074845242745 ) ) ;
#52824 = CARTESIAN_POINT ( 'NONE',  ( -18.50000000000000000, 78.21362219944489880, -231.2727646510690533 ) ) ;
#52825 = EDGE_LOOP ( 'NONE', ( #46367, #166715, #170857, #122128 ) ) ;
#52826 = ORIENTED_EDGE ( 'NONE', *, *, #167578, .T. ) ;
#52827 = B_SPLINE_CURVE_WITH_KNOTS ( 'NONE', 3,
 ( #163149, #207414, #243947, #124020, #45749, #88705, #84838 ),
 .UNSPECIFIED., .F., .F.,
 ( 4, 3, 4 ),
 ( 0.000000000000000000, 0.0007844235214594269838, 0.001767853679404345069 ),
 .UNSPECIFIED. ) ;
#52828 = CARTESIAN_POINT ( 'NONE',  ( -17.01825945287481545, 9.950000000011138823, -87.75000000000005684 ) ) ;
#52829 = EDGE_CURVE ( 'NONE', #217322, #63208, #176908, .T. ) ;
#52830 = EDGE_CURVE ( 'NONE', #93031, #142612, #33893, .T. ) ;
#52831 = B_SPLINE_CURVE_WITH_KNOTS ( 'NONE', 3,
 ( #68607, #93290, #92006, #227662, #192400, #231537, #232831, #52872, #132430, #32067 ),
 .UNSPECIFIED., .F., .F.,
 ( 4, 2, 2, 2, 4 ),
 ( 0.000000000000000000, 3.990160268013653969E-05, 7.980320536027307938E-05, 0.0001596064107205525013, 0.0003192128214411112910 ),
 .UNSPECIFIED. ) ;
#52832 = CARTESIAN_POINT ( 'NONE',  ( -16.87036670365549895, 9.989418819312803066, -180.0204398826979286 ) ) ;
#52833 = DIRECTION ( 'NONE',  ( 0.000000000000000000, 0.000000000000000000, -1.000000000000000000 ) ) ;
#52834 = DIRECTION ( 'NONE',  ( 0.000000000000000000, 0.000000000000000000, 1.000000000000000000 ) ) ;
#52835 = EDGE_LOOP ( 'NONE', ( #138447, #255144, #177648, #205050 ) ) ;
#52836 = CIRCLE ( 'NONE', #27947, 12.97499999999998366 ) ;
#52837 = CARTESIAN_POINT ( 'NONE',  ( 14.87567385445977486, 46.70278183066207589, -234.7177704364561066 ) ) ;
#52838 = DIRECTION ( 'NONE',  ( 1.000000000000000000, -0.000000000000000000, -0.000000000000000000 ) ) ;
#52839 = EDGE_CURVE ( 'NONE', #257429, #33688, #17640, .T. ) ;
#52840 = AXIS2_PLACEMENT_3D ( 'NONE', #76938, #157814, #58641 ) ;
#52841 = CARTESIAN_POINT ( 'NONE',  ( 18.39999999999999503, 62.23844973457045882, -209.3750075427748527 ) ) ;
#52842 = AXIS2_PLACEMENT_3D ( 'NONE', #257841, #216185, #76681 ) ;
#52843 = AXIS2_PLACEMENT_3D ( 'NONE', #92525, #172122, #251612 ) ;
#52844 = ORIENTED_EDGE ( 'NONE', *, *, #163325, .T. ) ;
#52845 = CARTESIAN_POINT ( 'NONE',  ( -21.05000000000000071, -11.64999999998884483, -100.5000000000000284 ) ) ;
#52846 = AXIS2_PLACEMENT_3D ( 'NONE', #81056, #100602, #215451 ) ;
#52848 = ORIENTED_EDGE ( 'NONE', *, *, #97769, .T. ) ;
#52847 = CARTESIAN_POINT ( 'NONE',  ( -18.41431012584568450, 64.51252797080444168, -194.2963434976261112 ) ) ;
#52849 = FACE_OUTER_BOUND ( 'NONE', #27738, .T. ) ;
#52850 = AXIS2_PLACEMENT_3D ( 'NONE', #95394, #73297, #253175 ) ;
#52851 = DIRECTION ( 'NONE',  ( -1.000000000000000000, -7.304098846218134667E-16, -5.311601492717084346E-30 ) ) ;
#52852 = DIRECTION ( 'NONE',  ( -0.000000000000000000, 1.000000000000000000, 6.352154140967427193E-15 ) ) ;
#52853 = LINE ( 'NONE', #49010, #159603 ) ;
#52854 = VECTOR ( 'NONE', #146789, 1000.000000000000000 ) ;
#52855 = FACE_OUTER_BOUND ( 'NONE', #229564, .T. ) ;
#52856 = VERTEX_POINT ( 'NONE', #39969 ) ;
#52857 = DIRECTION ( 'NONE',  ( 0.000000000000000000, 4.336808689942043768E-15, -1.000000000000000000 ) ) ;
#52858 = CARTESIAN_POINT ( 'NONE',  ( -20.94999999999999929, 79.19526988099229925, -196.1889237952725296 ) ) ;
#52859 = CYLINDRICAL_SURFACE ( 'NONE', #157291, 0.1000000000000033362 ) ;
#52860 = VERTEX_POINT ( 'NONE', #99873 ) ;
#52861 = CARTESIAN_POINT ( 'NONE',  ( 20.94999999999999574, -11.48912529306490349, -36.50000000000000711 ) ) ;
#52862 = DIRECTION ( 'NONE',  ( 1.000000000000000000, 0.000000000000000000, 0.000000000000000000 ) ) ;
#52863 = DIRECTION ( 'NONE',  ( 1.000000000000000000, 0.000000000000000000, -0.000000000000000000 ) ) ;
#52864 = CARTESIAN_POINT ( 'NONE',  ( -21.05000000000000071, -1.835341550213255957, -78.55515129256302487 ) ) ;
#52865 = AXIS2_PLACEMENT_3D ( 'NONE', #5378, #21151, #181498 ) ;
#52866 = CYLINDRICAL_SURFACE ( 'NONE', #155119, 0.5000000000000004441 ) ;
#52867 = AXIS2_PLACEMENT_3D ( 'NONE', #9385, #206319, #165928 ) ;
#52868 = ORIENTED_EDGE ( 'NONE', *, *, #230674, .T. ) ;
#52869 = VERTEX_POINT ( 'NONE', #54361 ) ;
#52870 = ADVANCED_FACE ( 'NONE', ( #222388 ), #234312, .F. ) ;
#52871 = CIRCLE ( 'NONE', #215200, 0.1000000000000028644 ) ;
#52872 = CARTESIAN_POINT ( 'NONE',  ( -18.49499033040907037, -9.438148771733509079, -141.1981532259235053 ) ) ;
#52874 = ADVANCED_FACE ( 'NONE', ( #223688 ), #24247, .T. ) ;
#52873 = DIRECTION ( 'NONE',  ( 0.000000000000000000, -6.938893903907222067E-15, 1.000000000000000000 ) ) ;
#52875 = VECTOR ( 'NONE', #47171, 1000.000000000000000 ) ;
#52876 = DIRECTION ( 'NONE',  ( 0.000000000000000000, 1.000000000000000000, 0.000000000000000000 ) ) ;
#52877 = FACE_OUTER_BOUND ( 'NONE', #41451, .T. ) ;
#52878 = VECTOR ( 'NONE', #43061, 1000.000000000000000 ) ;
#52879 = EDGE_CURVE ( 'NONE', #236598, #145192, #38511, .T. ) ;
#52880 = EDGE_CURVE ( 'NONE', #128947, #171646, #159333, .T. ) ;
#52881 = CIRCLE ( 'NONE', #32073, 0.1000000000000066391 ) ;
#52882 = DIRECTION ( 'NONE',  ( 1.000000000000000000, 0.000000000000000000, 0.000000000000000000 ) ) ;
#52883 = EDGE_CURVE ( 'NONE', #171051, #156829, #173502, .T. ) ;
#52884 = CARTESIAN_POINT ( 'NONE',  ( 18.49999999999999289, 15.53922597307775000, -223.0482397989536025 ) ) ;
#52885 = DIRECTION ( 'NONE',  ( 1.000000000000000000, 0.000000000000000000, 0.000000000000000000 ) ) ;
#52886 = ADVANCED_FACE ( 'NONE', ( #3353 ), #184574, .T. ) ;
#52887 = TOROIDAL_SURFACE ( 'NONE', #48799, 11.90000000000000213, 0.1000000000000000056 ) ;
#52889 = EDGE_CURVE ( 'NONE', #206261, #250604, #9455, .T. ) ;
#52888 = EDGE_CURVE ( 'NONE', #204082, #33572, #205069, .T. ) ;
#52890 = AXIS2_PLACEMENT_3D ( 'NONE', #80711, #198112, #157757 ) ;
#52891 = ORIENTED_EDGE ( 'NONE', *, *, #40936, .T. ) ;
#52892 = LINE ( 'NONE', #13774, #181904 ) ;
#52893 = VERTEX_POINT ( 'NONE', #62073 ) ;
#52894 = CARTESIAN_POINT ( 'NONE',  ( 20.85000000000000142, 8.809961202382808665, -241.4517562488062481 ) ) ;
#52895 = CARTESIAN_POINT ( 'NONE',  ( 20.94999999999999929, 76.00000000001244871, -170.0231074845243597 ) ) ;
#52897 = ADVANCED_FACE ( 'NONE', ( #224966 ), #200297, .F. ) ;
#52896 = CYLINDRICAL_SURFACE ( 'NONE', #132697, 0.09999999999999939493 ) ;
#52898 = FACE_OUTER_BOUND ( 'NONE', #46691, .T. ) ;
#52899 = LINE ( 'NONE', #72489, #168758 ) ;
#52900 = CARTESIAN_POINT ( 'NONE',  ( 18.44206774312970154, 85.49102735755175786, -62.89687997982598944 ) ) ;
#52901 = CARTESIAN_POINT ( 'NONE',  ( 23.15000000000000213, -9.599999999988845900, -143.8939691226524644 ) ) ;
#52902 = ORIENTED_EDGE ( 'NONE', *, *, #118066, .T. ) ;
#52903 = LINE ( 'NONE', #191163, #8205 ) ;
#52904 = ADVANCED_FACE ( 'NONE', ( #46338 ), #26047, .T. ) ;
#52905 = DIRECTION ( 'NONE',  ( 1.000000000000000000, 0.000000000000000000, 0.000000000000000000 ) ) ;
#52906 = DIRECTION ( 'NONE',  ( 0.000000000000000000, -0.1568667991644355497, -0.9876197685951332295 ) ) ;
#52907 = CARTESIAN_POINT ( 'NONE',  ( 21.05000000000000071, 10.71906255309368383, -222.4921384173655383 ) ) ;
#52908 = EDGE_CURVE ( 'NONE', #153129, #75064, #46859, .T. ) ;
#52909 = EDGE_CURVE ( 'NONE', #138714, #19770, #102438, .T. ) ;
#52910 = DIRECTION ( 'NONE',  ( -0.000000000000000000, 0.3848449534832868446, 0.9229812358755982160 ) ) ;
#52911 = EDGE_LOOP ( 'NONE', ( #225695, #1913, #96577, #123278 ) ) ;
#52912 = VECTOR ( 'NONE', #8799, 1000.000000000000000 ) ;
#52913 = DIRECTION ( 'NONE',  ( 1.000000000000000000, -0.000000000000000000, -0.000000000000000000 ) ) ;
#52915 = ADVANCED_FACE ( 'NONE', ( #63333 ), #128463, .T. ) ;
#52914 = DIRECTION ( 'NONE',  ( 0.000000000000000000, 0.000000000000000000, -1.000000000000000000 ) ) ;
#52916 = ORIENTED_EDGE ( 'NONE', *, *, #174264, .F. ) ;
#52917 = ORIENTED_EDGE ( 'NONE', *, *, #117924, .T. ) ;
#52918 = CARTESIAN_POINT ( 'NONE',  ( 22.49544290803662960, 55.87396915977497969, -232.8425975917333233 ) ) ;
#52919 = CARTESIAN_POINT ( 'NONE',  ( -21.05000000000000071, -11.74999999998884448, -164.5000000000000000 ) ) ;
#52920 = EDGE_CURVE ( 'NONE', #56738, #122095, #1052, .T. ) ;
#52921 = VECTOR ( 'NONE', #154401, 1000.000000000000000 ) ;
#52922 = VERTEX_POINT ( 'NONE', #231429 ) ;
#52924 = AXIS2_PLACEMENT_3D ( 'NONE', #186573, #230842, #110870 ) ;
#52923 = CARTESIAN_POINT ( 'NONE',  ( 21.05000000000000071, 56.45527679911575802, -225.2871936083021467 ) ) ;
#52925 = CARTESIAN_POINT ( 'NONE',  ( -16.87683809663752399, 9.850000000011123191, -147.4023640181965220 ) ) ;
#52926 = CIRCLE ( 'NONE', #186222, 0.09999999999999939493 ) ;
#52927 = EDGE_CURVE ( 'NONE', #74293, #65743, #134345, .T. ) ;
#52928 = ORIENTED_EDGE ( 'NONE', *, *, #163355, .T. ) ;
#52929 = DIRECTION ( 'NONE',  ( 0.000000000000000000, 0.000000000000000000, -1.000000000000000000 ) ) ;
#52930 = ORIENTED_EDGE ( 'NONE', *, *, #83535, .F. ) ;
#52931 = CARTESIAN_POINT ( 'NONE',  ( 21.05000000000000071, 76.00000000001170974, -69.52310748452431710 ) ) ;
#52932 = EDGE_CURVE ( 'NONE', #178186, #175143, #226245, .T. ) ;
#52933 = CARTESIAN_POINT ( 'NONE',  ( -20.54999999999999716, 4.349999999999999645, -12.35000000000000142 ) ) ;
#52935 = ORIENTED_EDGE ( 'NONE', *, *, #71494, .F. ) ;
#52934 = CARTESIAN_POINT ( 'NONE',  ( 22.50000000000000000, 1.148907358139439339E-11, -201.0000000000015064 ) ) ;
#52937 = UNCERTAINTY_MEASURE_WITH_UNIT (LENGTH_MEASURE( 1.000000000000000082E-05 ), #226677, 'distance_accuracy_value', 'NONE');
#52936 = DIRECTION ( 'NONE',  ( -1.000000000000000000, 1.875376730785737719E-16, 1.309568571767809260E-30 ) ) ;
#52938 = DIRECTION ( 'NONE',  ( -0.5932847527679298016, -0.7769265190100953511, 0.2107092456252275259 ) ) ;
#52939 = SPHERICAL_SURFACE ( 'NONE', #243369, 0.1000000000000000056 ) ;
#52940 = CARTESIAN_POINT ( 'NONE',  ( -16.81095280782811230, 66.05000000001261640, -190.8731074845252920 ) ) ;
#52941 = CARTESIAN_POINT ( 'NONE',  ( 23.50000000000005684, 87.50449464844290048, -37.85861909827351468 ) ) ;
#52942 = CARTESIAN_POINT ( 'NONE',  ( -21.14999999999999858, 76.00000000001271871, -209.7816861282870775 ) ) ;
#52944 = ORIENTED_EDGE ( 'NONE', *, *, #8709, .T. ) ;
#52943 = CARTESIAN_POINT ( 'NONE',  ( -22.59999999999999787, 25.89494711235935043, -254.2627752153468350 ) ) ;
#52945 = ORIENTED_EDGE ( 'NONE', *, *, #107713, .F. ) ;
#52947 = CARTESIAN_POINT ( 'NONE',  ( -13.77083647240106323, 9.457410930301319851, -85.49991590874631697 ) ) ;
#52946 = LINE ( 'NONE', #128656, #57991 ) ;
#52949 = VERTEX_POINT ( 'NONE', #71075 ) ;
#52948 = CARTESIAN_POINT ( 'NONE',  ( 21.04999999999999716, 8.894723818389266512, -75.48708432315146410 ) ) ;
#52950 = ORIENTED_EDGE ( 'NONE', *, *, #196797, .T. ) ;
#52951 = CARTESIAN_POINT ( 'NONE',  ( -20.64999999999999858, 1.115600667400684642E-11, -113.3750000000000284 ) ) ;
#52952 = DIRECTION ( 'NONE',  ( 1.000000000000000000, -0.000000000000000000, -0.000000000000000000 ) ) ;
#52953 = AXIS2_PLACEMENT_3D ( 'NONE', #220949, #18903, #121882 ) ;
#52954 = CYLINDRICAL_SURFACE ( 'NONE', #213262, 0.09999999999999939493 ) ;
#52955 = DIRECTION ( 'NONE',  ( 0.000000000000000000, 1.000000000000000000, 0.000000000000000000 ) ) ;
#52956 = DIRECTION ( 'NONE',  ( -0.000000000000000000, -0.000000000000000000, 1.000000000000000000 ) ) ;
#52957 = DIRECTION ( 'NONE',  ( 1.000000000000000000, -0.000000000000000000, -0.000000000000000000 ) ) ;
#52958 = LINE ( 'NONE', #38547, #235509 ) ;
#52960 = ORIENTED_EDGE ( 'NONE', *, *, #125966, .F. ) ;
#52959 = EDGE_CURVE ( 'NONE', #36655, #52558, #84231, .T. ) ;
#52961 = ORIENTED_EDGE ( 'NONE', *, *, #157827, .F. ) ;
#52962 = CARTESIAN_POINT ( 'NONE',  ( 21.05000000000000782, 30.86995437684140953, -252.0366859498353449 ) ) ;
#52963 = AXIS2_PLACEMENT_3D ( 'NONE', #59891, #140733, #238549 ) ;
#52964 = CIRCLE ( 'NONE', #169733, 0.5999999999999998668 ) ;
#52965 = ADVANCED_FACE ( 'NONE', ( #209274 ), #167609, .F. ) ;
#52966 = EDGE_LOOP ( 'NONE', ( #250376, #257513, #32523, #69586 ) ) ;
#52967 = AXIS2_PLACEMENT_3D ( 'NONE', #113911, #134737, #19966 ) ;
#52969 = CARTESIAN_POINT ( 'NONE',  ( 18.50000000000000000, 85.40000000001160174, -62.52382180668540457 ) ) ;
#52968 = AXIS2_PLACEMENT_3D ( 'NONE', #193001, #52180, #95174 ) ;
#52970 = VERTEX_POINT ( 'NONE', #151904 ) ;
#52971 = DIRECTION ( 'NONE',  ( 0.000000000000000000, 0.000000000000000000, -1.000000000000000000 ) ) ;
#52972 = DIRECTION ( 'NONE',  ( -0.7071067811865486830, 0.6909108974501224631, 0.1504730267678053013 ) ) ;
#52973 = EDGE_CURVE ( 'NONE', #104499, #135971, #86742, .T. ) ;
#52975 = ADVANCED_FACE ( 'NONE', ( #30674 ), #31955, .F. ) ;
#52974 = CARTESIAN_POINT ( 'NONE',  ( 18.59999999999999076, 6.982009704867611077, -137.6961521182563501 ) ) ;
#52976 = ORIENTED_EDGE ( 'NONE', *, *, #11742, .F. ) ;
#52977 = CARTESIAN_POINT ( 'NONE',  ( -20.64999999999999858, 70.60814576644823148, -215.7631455941064189 ) ) ;
#52978 = ORIENTED_EDGE ( 'NONE', *, *, #5093, .T. ) ;
#52979 = CYLINDRICAL_SURFACE ( 'NONE', #152377, 0.09999999999999939493 ) ;
#52980 = CARTESIAN_POINT ( 'NONE',  ( 18.58703555225010717, 8.967833031541422528, -245.3886906379661923 ) ) ;
#52981 = VECTOR ( 'NONE', #125152, 1000.000000000000000 ) ;
#52982 = EDGE_LOOP ( 'NONE', ( #134387, #190107 ) ) ;
#52984 = CARTESIAN_POINT ( 'NONE',  ( -21.55000000000000071, 7.350000000011155166, -45.85000000000000142 ) ) ;
#52983 = AXIS2_PLACEMENT_3D ( 'NONE', #106071, #207801, #233768 ) ;
#52985 = ORIENTED_EDGE ( 'NONE', *, *, #229216, .T. ) ;
#52988 = ORIENTED_EDGE ( 'NONE', *, *, #139293, .F. ) ;
#52987 = LINE ( 'NONE', #97207, #42988 ) ;
#52986 = CARTESIAN_POINT ( 'NONE',  ( -20.85000000000000142, 70.37092869010230345, -198.1237041667535550 ) ) ;
#52989 = B_SPLINE_CURVE_WITH_KNOTS ( 'NONE', 3,
 ( #41073, #196260, #141424, #235381, #217087, #161003, #76300, #155884 ),
 .UNSPECIFIED., .F., .F.,
 ( 4, 2, 2, 4 ),
 ( 0.000000000000000000, 0.0001306511400390773054, 0.0001959767100586598141, 0.0002613022800782423228 ),
 .UNSPECIFIED. ) ;
#52990 = CARTESIAN_POINT ( 'NONE',  ( 18.49999999999999289, 65.67426406872341715, -44.67310748452440095 ) ) ;
#52991 = ORIENTED_EDGE ( 'NONE', *, *, #236251, .T. ) ;
#52992 = EDGE_CURVE ( 'NONE', #195501, #55978, #196708, .T. ) ;
#52993 = CIRCLE ( 'NONE', #198742, 0.09999999999999939493 ) ;
#52994 = ORIENTED_EDGE ( 'NONE', *, *, #197086, .T. ) ;
#52995 = DIRECTION ( 'NONE',  ( 0.7071067811865474617, 0.7071067811865474617, 0.000000000000000000 ) ) ;
#52996 = ORIENTED_EDGE ( 'NONE', *, *, #29348, .T. ) ;
#52997 = DIRECTION ( 'NONE',  ( 0.000000000000000000, 6.938893903907222067E-15, -1.000000000000000000 ) ) ;
#52998 = DIRECTION ( 'NONE',  ( 0.000000000000000000, 0.000000000000000000, -1.000000000000000000 ) ) ;
#52999 = CARTESIAN_POINT ( 'NONE',  ( 20.94999999999999929, 76.00000000001126921, -203.5231074845248997 ) ) ;
#53000 = DIRECTION ( 'NONE',  ( 0.000000000000000000, 0.000000000000000000, -1.000000000000000000 ) ) ;
#53001 = CARTESIAN_POINT ( 'NONE',  ( -20.54999999999999716, 11.60058429089262333, -246.3380203656811887 ) ) ;
#53002 = VERTEX_POINT ( 'NONE', #208016 ) ;
#53003 = DIRECTION ( 'NONE',  ( 0.000000000000000000, -0.9856811345164829818, -0.1686199900910294314 ) ) ;
#53004 = PLANE ( 'NONE',  #191027 ) ;
#53005 = CARTESIAN_POINT ( 'NONE',  ( 21.11927991906888025, 6.448493118502572230, -33.49091632052610379 ) ) ;
#53006 = VECTOR ( 'NONE', #139980, 1000.000000000000114 ) ;
#53007 = ORIENTED_EDGE ( 'NONE', *, *, #219729, .T. ) ;
#53008 = EDGE_CURVE ( 'NONE', #204472, #6436, #180175, .T. ) ;
#53009 = CARTESIAN_POINT ( 'NONE',  ( 23.50000000000005684, 83.97335046823651794, -37.38386894789040582 ) ) ;
#53010 = ORIENTED_EDGE ( 'NONE', *, *, #254803, .F. ) ;
#53011 = DIRECTION ( 'NONE',  ( 0.000000000000000000, 0.7397360091702777085, -0.6728971962616808744 ) ) ;
#53012 = ORIENTED_EDGE ( 'NONE', *, *, #119328, .T. ) ;
#53013 = CARTESIAN_POINT ( 'NONE',  ( -21.00000000000000000, -0.3305886640091971196, 0.04453801223857078301 ) ) ;
#53014 = CARTESIAN_POINT ( 'NONE',  ( 21.05000000000000071, 70.50000000001199396, -115.4283735034374274 ) ) ;
#53016 = ORIENTED_EDGE ( 'NONE', *, *, #95700, .T. ) ;
#53015 = CARTESIAN_POINT ( 'NONE',  ( 23.15000000000000213, -11.48912529306489994, -164.4000000000000057 ) ) ;
#53017 = LINE ( 'NONE', #11337, #67042 ) ;
#53018 = ORIENTED_EDGE ( 'NONE', *, *, #199533, .F. ) ;
#53019 = CIRCLE ( 'NONE', #202860, 0.9750000000000036415 ) ;
#53020 = EDGE_CURVE ( 'NONE', #106580, #70167, #146261, .T. ) ;
#53021 = CARTESIAN_POINT ( 'NONE',  ( 22.39999999999999503, -0.1008583690875579364, -88.75043287651064361 ) ) ;
#53022 = CARTESIAN_POINT ( 'NONE',  ( -22.19999999999999929, -11.75000000000000000, 14.10000000000000142 ) ) ;
#53023 = EDGE_CURVE ( 'NONE', #136369, #207244, #246773, .T. ) ;
#53024 = VERTEX_POINT ( 'NONE', #250953 ) ;
#53025 = CIRCLE ( 'NONE', #69630, 0.09999999999998898659 ) ;
#53026 = CARTESIAN_POINT ( 'NONE',  ( 22.39999999999999503, 75.90000000001219860, -142.7731074845243029 ) ) ;
#53027 = DIRECTION ( 'NONE',  ( 0.000000000000000000, -0.9908441862701596881, 0.1350103645451904977 ) ) ;
#53028 = EDGE_LOOP ( 'NONE', ( #101189, #83162, #199071, #214437, #188747, #154693, #168253, #160914, #236226, #179734, #31052, #41785, #208693, #128114 ) ) ;
#53029 = DIRECTION ( 'NONE',  ( 0.000000000000000000, 0.000000000000000000, -1.000000000000000000 ) ) ;
#53030 = AXIS2_PLACEMENT_3D ( 'NONE', #165213, #126067, #166529 ) ;
#53031 = AXIS2_PLACEMENT_3D ( 'NONE', #21686, #123349, #239448 ) ;
#53032 = ORIENTED_EDGE ( 'NONE', *, *, #13795, .T. ) ;
#53033 = CIRCLE ( 'NONE', #33365, 0.09999999999999939493 ) ;
#53034 = EDGE_CURVE ( 'NONE', #63323, #26083, #68494, .T. ) ;
#53035 = CARTESIAN_POINT ( 'NONE',  ( 20.12500000000000000, 66.25000000001263345, -195.4113362024101548 ) ) ;
#53037 = DIRECTION ( 'NONE',  ( 1.000000000000000000, -0.000000000000000000, -0.000000000000000000 ) ) ;
#53036 = AXIS2_PLACEMENT_3D ( 'NONE', #156379, #235867, #237172 ) ;
#53038 = AXIS2_PLACEMENT_3D ( 'NONE', #70166, #229223, #209648 ) ;
#53039 = ADVANCED_FACE ( 'NONE', ( #29400 ), #48914, .T. ) ;
#53040 = EDGE_CURVE ( 'NONE', #51561, #204905, #89316, .T. ) ;
#53043 = EDGE_LOOP ( 'NONE', ( #51674, #116303, #157612, #19815 ) ) ;
#53042 = VERTEX_POINT ( 'NONE', #228852 ) ;
#53041 = CARTESIAN_POINT ( 'NONE',  ( -21.05000000000000071, 79.26035508877831148, -236.0091442494974956 ) ) ;
#53044 = DIRECTION ( 'NONE',  ( 0.000000000000000000, -6.853228547068871147E-15, 1.000000000000000000 ) ) ;
#53045 = CARTESIAN_POINT ( 'NONE',  ( -22.45372860728439690, 0.01492061955964466002, -155.8502028652960973 ) ) ;
#53046 = CARTESIAN_POINT ( 'NONE',  ( 21.87500000000000355, 9.750000000011153745, -54.65000000000000568 ) ) ;
#53047 = EDGE_CURVE ( 'NONE', #246470, #120433, #210570, .T. ) ;
#53048 = CARTESIAN_POINT ( 'NONE',  ( -20.85000000000000142, 77.25000000001209344, -128.7226267301092548 ) ) ;
#53049 = CARTESIAN_POINT ( 'NONE',  ( -20.54999999999999716, 62.04503132991428060, -248.4786563706009588 ) ) ;
#53050 = CARTESIAN_POINT ( 'NONE',  ( -21.55000000000000071, 7.350000000011155166, -54.65000000000000568 ) ) ;
#53051 = VECTOR ( 'NONE', #161318, 1000.000000000000000 ) ;
#53052 = LINE ( 'NONE', #188713, #26585 ) ;
#53053 = CARTESIAN_POINT ( 'NONE',  ( -21.05000000000000071, 76.00000000001213607, -136.5231074845243313 ) ) ;
#53054 = ORIENTED_EDGE ( 'NONE', *, *, #175708, .F. ) ;
#53055 = ORIENTED_EDGE ( 'NONE', *, *, #191610, .F. ) ;
#53057 = DIRECTION ( 'NONE',  ( 0.000000000000000000, 0.9908441862701596881, -0.1350103645451904977 ) ) ;
#53056 = CIRCLE ( 'NONE', #15688, 0.09999999999999939493 ) ;
#53059 = EDGE_LOOP ( 'NONE', ( #82953, #82902, #179179, #83300 ) ) ;
#53058 = FACE_OUTER_BOUND ( 'NONE', #96372, .T. ) ;
#53060 = CIRCLE ( 'NONE', #240513, 0.09999999999999939493 ) ;
#53061 = ORIENTED_EDGE ( 'NONE', *, *, #241362, .F. ) ;
#53062 = EDGE_CURVE ( 'NONE', #44396, #256585, #150939, .T. ) ;
#53063 = LINE ( 'NONE', #187465, #197614 ) ;
#53064 = ORIENTED_EDGE ( 'NONE', *, *, #128136, .T. ) ;
#53065 = CARTESIAN_POINT ( 'NONE',  ( 21.05000012384814312, 43.42722438913664718, -234.8725066798682519 ) ) ;
#53066 = ORIENTED_EDGE ( 'NONE', *, *, #55506, .F. ) ;
#53067 = DIRECTION ( 'NONE',  ( 1.186688945009010077E-16, -1.000000000000000000, -0.000000000000000000 ) ) ;
#53070 = EDGE_LOOP ( 'NONE', ( #157225, #93377, #150849, #97364, #180005 ) ) ;
#53069 = ORIENTED_EDGE ( 'NONE', *, *, #206944, .F. ) ;
#53068 = CIRCLE ( 'NONE', #32461, 0.5000000000000004441 ) ;
#53071 = EDGE_LOOP ( 'NONE', ( #181400, #215004, #105499, #179135, #196429 ) ) ;
#53072 = CIRCLE ( 'NONE', #202925, 1.749999999999998002 ) ;
#53073 = AXIS2_PLACEMENT_3D ( 'NONE', #108004, #5018, #187563 ) ;
#53074 = VERTEX_POINT ( 'NONE', #254776 ) ;
#53075 = ORIENTED_EDGE ( 'NONE', *, *, #108977, .F. ) ;
#53076 = FACE_OUTER_BOUND ( 'NONE', #158315, .T. ) ;
#53077 = CARTESIAN_POINT ( 'NONE',  ( -22.50000000000000000, 67.23127455305841238, -235.8551265064783991 ) ) ;
#53078 = CARTESIAN_POINT ( 'NONE',  ( -12.30589683808040924, 9.356746017089406564, -184.7033597213641656 ) ) ;
#53080 = VERTEX_POINT ( 'NONE', #133588 ) ;
#53079 = CYLINDRICAL_SURFACE ( 'NONE', #33434, 0.09999999999998898659 ) ;
#53081 = CARTESIAN_POINT ( 'NONE',  ( 23.14999999999998437, 80.05000000001237481, -170.0231074845243313 ) ) ;
#53082 = CARTESIAN_POINT ( 'NONE',  ( 22.47007471830799474, 7.720710651937603863, -167.4999999999999432 ) ) ;
#53084 = ORIENTED_EDGE ( 'NONE', *, *, #54654, .F. ) ;
#53083 = DIRECTION ( 'NONE',  ( -1.000000000000000000, 0.000000000000000000, 0.000000000000000000 ) ) ;
#53085 = CARTESIAN_POINT ( 'NONE',  ( -21.05000000000000071, 1.360870587203197646, -41.57299792709095954 ) ) ;
#53086 = EDGE_LOOP ( 'NONE', ( #209388, #127436, #106935, #108697 ) ) ;
#53087 = LINE ( 'NONE', #34844, #195443 ) ;
#53088 = ORIENTED_EDGE ( 'NONE', *, *, #79263, .T. ) ;
#53089 = TOROIDAL_SURFACE ( 'NONE', #244802, 11.90000000000000391, 0.1000000000000000056 ) ;
#53090 = DIRECTION ( 'NONE',  ( 0.000000000000000000, 0.000000000000000000, -1.000000000000000000 ) ) ;
#53091 = PLANE ( 'NONE',  #124909 ) ;
#53092 = AXIS2_PLACEMENT_3D ( 'NONE', #224360, #122720, #202237 ) ;
#53093 = VERTEX_POINT ( 'NONE', #54053 ) ;
#53094 = CARTESIAN_POINT ( 'NONE',  ( -22.47071067811865319, 75.90090754531013317, -211.2431822290224375 ) ) ;
#53095 = CYLINDRICAL_SURFACE ( 'NONE', #134845, 0.09999999999999997780 ) ;
#53096 = EDGE_CURVE ( 'NONE', #41155, #257555, #59306, .T. ) ;
#53097 = CARTESIAN_POINT ( 'NONE',  ( 21.05000000000000071, 18.18127959618848877, -237.5711165786817389 ) ) ;
#53098 = CARTESIAN_POINT ( 'NONE',  ( 20.12500000000000355, 10.24195072709382970, -41.36020372708612314 ) ) ;
#53099 = ORIENTED_EDGE ( 'NONE', *, *, #162021, .F. ) ;
#53100 = VERTEX_POINT ( 'NONE', #155761 ) ;
#53101 = AXIS2_PLACEMENT_3D ( 'NONE', #42188, #218216, #95715 ) ;
#53102 = LINE ( 'NONE', #174393, #88643 ) ;
#53103 = CARTESIAN_POINT ( 'NONE',  ( -18.35668295345803713, 62.50563584222673796, -209.4474707446456421 ) ) ;
#53104 = ORIENTED_EDGE ( 'NONE', *, *, #34104, .T. ) ;
#53105 = CARTESIAN_POINT ( 'NONE',  ( -20.54999999999999716, 4.768403829798271154, -213.4961173936592331 ) ) ;
#53106 = ORIENTED_EDGE ( 'NONE', *, *, #157809, .T. ) ;
#53107 = CARTESIAN_POINT ( 'NONE',  ( 21.05000000000000071, 67.44464249442897597, -214.0562211244547655 ) ) ;
#53108 = EDGE_CURVE ( 'NONE', #164610, #176897, #177877, .T. ) ;
#53109 = DIRECTION ( 'NONE',  ( 1.000000000000000000, -0.000000000000000000, -0.000000000000000000 ) ) ;
#53110 = CIRCLE ( 'NONE', #144683, 0.1000000000000013933 ) ;
#53111 = CARTESIAN_POINT ( 'NONE',  ( 21.05000000000000071, 85.00000000001149658, -45.91707660717670336 ) ) ;
#53112 = CIRCLE ( 'NONE', #164975, 11.90000000000000213 ) ;
#53113 = EDGE_CURVE ( 'NONE', #126073, #231419, #193577, .T. ) ;
#53115 = EDGE_CURVE ( 'NONE', #253585, #204559, #17285, .T. ) ;
#53114 = CIRCLE ( 'NONE', #94804, 0.2000000000000057288 ) ;
#53116 = AXIS2_PLACEMENT_3D ( 'NONE', #73698, #33299, #34560 ) ;
#53117 = ORIENTED_EDGE ( 'NONE', *, *, #3637, .F. ) ;
#53118 = VECTOR ( 'NONE', #43663, 1000.000000000000000 ) ;
#53119 = LINE ( 'NONE', #149680, #231697 ) ;
#53120 = CIRCLE ( 'NONE', #232220, 0.1000000000000028644 ) ;
#53121 = ORIENTED_EDGE ( 'NONE', *, *, #160337, .F. ) ;
#53122 = ORIENTED_EDGE ( 'NONE', *, *, #78876, .T. ) ;
#53123 = EDGE_LOOP ( 'NONE', ( #137244, #190832, #21329, #17213, #254409, #248994, #214348, #25547, #117336, #83616, #241733 ) ) ;
#53124 = DIRECTION ( 'NONE',  ( 0.000000000000000000, 0.2128009952263663074, -0.9770955615653301729 ) ) ;
#53125 = CARTESIAN_POINT ( 'NONE',  ( 21.00000000000000000, 66.25000000001229239, -157.6731074845244223 ) ) ;
#53126 = DIRECTION ( 'NONE',  ( -0.000000000000000000, -0.1290532225515392817, -0.9916376685811522096 ) ) ;
#53127 = CARTESIAN_POINT ( 'NONE',  ( -18.59999999999999787, 11.65000000001115232, -112.6500000000000341 ) ) ;
#53128 = CARTESIAN_POINT ( 'NONE',  ( -18.59999999999999787, 11.65000000001115232, -121.7500000000000426 ) ) ;
#53129 = ADVANCED_FACE ( 'NONE', ( #197413 ), #116602, .F. ) ;
#53131 = DIRECTION ( 'NONE',  ( 1.000000000000000000, 0.000000000000000000, 0.000000000000000000 ) ) ;
#53130 = FACE_OUTER_BOUND ( 'NONE', #58301, .T. ) ;
#53133 = ORIENTED_EDGE ( 'NONE', *, *, #107528, .F. ) ;
#53132 = CARTESIAN_POINT ( 'NONE',  ( -18.59999999999999787, 77.13501884592184865, -61.80613060109197932 ) ) ;
#53134 = LINE ( 'NONE', #166703, #145838 ) ;
#53135 = EDGE_LOOP ( 'NONE', ( #98201, #220013, #58423, #167546 ) ) ;
#53136 = EDGE_CURVE ( 'NONE', #49802, #72649, #29790, .T. ) ;
#53137 = DIRECTION ( 'NONE',  ( -0.000000000000000000, 0.000000000000000000, 1.000000000000000000 ) ) ;
#53138 = EDGE_LOOP ( 'NONE', ( #85595, #74200, #213963, #111404 ) ) ;
#53139 = ORIENTED_EDGE ( 'NONE', *, *, #150428, .F. ) ;
#53140 = CARTESIAN_POINT ( 'NONE',  ( -20.64999999999999858, 24.04029978241813126, -253.0016354099517457 ) ) ;
#53141 = AXIS2_PLACEMENT_3D ( 'NONE', #18910, #137559, #219675 ) ;
#53142 = DIRECTION ( 'NONE',  ( 1.000000000000000000, 0.000000000000000000, 0.000000000000000000 ) ) ;
#53143 = CARTESIAN_POINT ( 'NONE',  ( 20.94999999999999574, 87.48912529308798014, -100.0231074845242318 ) ) ;
#53144 = DIRECTION ( 'NONE',  ( -1.000000000000000000, -0.000000000000000000, -0.000000000000000000 ) ) ;
#53145 = CIRCLE ( 'NONE', #57212, 0.09999999999999990841 ) ;
#53146 = DIRECTION ( 'NONE',  ( 0.000000000000000000, 0.8814952561688418342, -0.4721928772777367889 ) ) ;
#53147 = ORIENTED_EDGE ( 'NONE', *, *, #88236, .T. ) ;
#53148 = VERTEX_POINT ( 'NONE', #73653 ) ;
#53149 = EDGE_CURVE ( 'NONE', #56583, #41677, #55303, .T. ) ;
#53150 = CYLINDRICAL_SURFACE ( 'NONE', #44933, 0.09999999999999939493 ) ;
#53152 = ORIENTED_EDGE ( 'NONE', *, *, #168861, .F. ) ;
#53151 = EDGE_CURVE ( 'NONE', #22950, #138951, #146423, .T. ) ;
#53153 = DIRECTION ( 'NONE',  ( 1.000000000000000000, 0.000000000000000000, 0.000000000000000000 ) ) ;
#53154 = SPHERICAL_SURFACE ( 'NONE', #202833, 0.1000000000000000056 ) ;
#53155 = ORIENTED_EDGE ( 'NONE', *, *, #83660, .F. ) ;
#53156 = ADVANCED_FACE ( 'NONE', ( #94459 ), #157032, .F. ) ;
#53157 = LINE ( 'NONE', #192682, #61354 ) ;
#53158 = DIRECTION ( 'NONE',  ( 0.000000000000000000, 0.8700118002898356018, -0.4930308989875170078 ) ) ;
#53159 = CARTESIAN_POINT ( 'NONE',  ( -21.05000000000000071, 6.285074713407414748, -199.7187976872275499 ) ) ;
#53160 = DIRECTION ( 'NONE',  ( 0.000000000000000000, 6.982962677686266711E-15, -1.000000000000000000 ) ) ;
#53161 = ORIENTED_EDGE ( 'NONE', *, *, #241162, .T. ) ;
#53162 = LINE ( 'NONE', #550, #91570 ) ;
#53163 = CARTESIAN_POINT ( 'NONE',  ( 23.14999999999999503, 23.29878867550048938, -248.4686781323362084 ) ) ;
#53164 = CARTESIAN_POINT ( 'NONE',  ( -21.05000000000000071, 1.162701749938009677, -8.099999999999999645 ) ) ;
#53165 = ADVANCED_FACE ( 'NONE', ( #38357 ), #196139, .T. ) ;
#53166 = AXIS2_PLACEMENT_3D ( 'NONE', #239534, #219961, #157462 ) ;
#53168 = CIRCLE ( 'NONE', #128185, 0.2000000000000057288 ) ;
#53167 = DIRECTION ( 'NONE',  ( 0.000000000000000000, 0.6728971962616697722, 0.7397360091702875895 ) ) ;
#53169 = AXIS2_PLACEMENT_3D ( 'NONE', #11492, #93576, #111870 ) ;
#53170 = EDGE_LOOP ( 'NONE', ( #70408, #119439, #40860, #97553, #7072 ) ) ;
#53171 = LINE ( 'NONE', #15349, #74547 ) ;
#53172 = ORIENTED_EDGE ( 'NONE', *, *, #3323, .T. ) ;
#53173 = DIRECTION ( 'NONE',  ( -1.000000000000000000, 0.000000000000000000, -0.000000000000000000 ) ) ;
#53174 = CARTESIAN_POINT ( 'NONE',  ( 20.90000000000000213, 1.885425182446133885, -11.49641995933507843 ) ) ;
#53175 = DIRECTION ( 'NONE',  ( 0.000000000000000000, -0.4856429311786358283, -0.8741572761215357090 ) ) ;
#53176 = CARTESIAN_POINT ( 'NONE',  ( 20.94999999999999929, 4.252251777740766236, -211.8999245327126744 ) ) ;
#53177 = CARTESIAN_POINT ( 'NONE',  ( -16.27683809663751191, 66.65000000001190017, -90.47310748452437679 ) ) ;
#53178 = CARTESIAN_POINT ( 'NONE',  ( -21.05000000000000071, 44.18518595211054389, -258.7688298343402380 ) ) ;
#53179 = EDGE_LOOP ( 'NONE', ( #24482, #209859, #208511, #124269 ) ) ;
#53180 = EDGE_CURVE ( 'NONE', #153971, #94181, #25648, .T. ) ;
#53181 = CARTESIAN_POINT ( 'NONE',  ( -17.11825945287481687, 65.95000000001225260, -149.1731074845244507 ) ) ;
#53182 = CARTESIAN_POINT ( 'NONE',  ( -18.59999999999999787, 11.65000000001115232, -88.75000000000004263 ) ) ;
#53183 = CIRCLE ( 'NONE', #240615, 0.09999999999999939493 ) ;
#53184 = DIRECTION ( 'NONE',  ( 1.000000000000000000, 3.265361837132813093E-16, -0.000000000000000000 ) ) ;
#53185 = DIRECTION ( 'NONE',  ( 0.1538461538461510236, 0.9880948137434718559, 0.000000000000000000 ) ) ;
#53186 = CIRCLE ( 'NONE', #61374, 0.8750000000000007772 ) ;
#53187 = FACE_OUTER_BOUND ( 'NONE', #254143, .T. ) ;
#53188 = VECTOR ( 'NONE', #253415, 1000.000000000000114 ) ;
#53189 = EDGE_LOOP ( 'NONE', ( #175382, #157677, #149949, #146594, #162208, #99093, #246149, #175649, #72579, #148920, #40030, #94846, #212078, #211122, #157633, #199965, #219444, #247792, #18001, #192927, #74244, #114612, #137626, #120738, #120676 ) ) ;
#53190 = VERTEX_POINT ( 'NONE', #236535 ) ;
#53191 = DIRECTION ( 'NONE',  ( 1.000000000000000000, 0.000000000000000000, 0.000000000000000000 ) ) ;
#53192 = DIRECTION ( 'NONE',  ( 0.000000000000000000, -0.8700118002898359348, 0.4930308989875165082 ) ) ;
#53194 = EDGE_CURVE ( 'NONE', #160249, #16468, #57889, .T. ) ;
#53193 = DIRECTION ( 'NONE',  ( 1.000000000000000000, 0.000000000000000000, -0.000000000000000000 ) ) ;
#53195 = CARTESIAN_POINT ( 'NONE',  ( -23.25000000000000000, 7.128833340093095217, -233.7327013124392749 ) ) ;
#53196 = DIRECTION ( 'NONE',  ( -3.469446951953352918E-14, 0.4721928772776973204, 0.8814952561688629284 ) ) ;
#53197 =( BOUNDED_CURVE ( )  B_SPLINE_CURVE ( 3, ( #60185, #122762, #84853, #223111 ),
 .UNSPECIFIED., .F., .F. ) 
 B_SPLINE_CURVE_WITH_KNOTS ( ( 4, 4 ),
 ( 0.06456096931748350753, 3.077031684272309775 ),
 .UNSPECIFIED. ) 
 CURVE ( )  GEOMETRIC_REPRESENTATION_ITEM ( )  RATIONAL_B_SPLINE_CURVE ( ( 1.000000000000000000, 0.3763440860215095940, 0.3763440860215095940, 1.000000000000000000 ) ) 
 REPRESENTATION_ITEM ( '' )  );
#53198 = ORIENTED_EDGE ( 'NONE', *, *, #210910, .F. ) ;
#53199 = CARTESIAN_POINT ( 'NONE',  ( -20.94999999999999929, -11.29603075032412640, -130.9521008403361861 ) ) ;
#53200 = EDGE_CURVE ( 'NONE', #28455, #211815, #129699, .T. ) ;
#53201 = CONTEXT_DEPENDENT_SHAPE_REPRESENTATION ( #170862, #103857 ) ;
#53202 = FACE_OUTER_BOUND ( 'NONE', #144194, .T. ) ;
#53203 = EDGE_LOOP ( 'NONE', ( #218591, #69736, #72757, #2182, #202484 ) ) ;
#53204 = CARTESIAN_POINT ( 'NONE',  ( -20.94999999999999929, 76.00000000001253397, -181.7231074845243484 ) ) ;
#53205 = FACE_OUTER_BOUND ( 'NONE', #91831, .T. ) ;
#53206 = TOROIDAL_SURFACE ( 'NONE', #103066, 12.77500000000000036, 0.1000000000000000056 ) ;
#53207 = AXIS2_PLACEMENT_3D ( 'NONE', #202784, #222315, #179393 ) ;
#53208 = EDGE_CURVE ( 'NONE', #248066, #11990, #225531, .T. ) ;
#53209 = ADVANCED_FACE ( 'NONE', ( #154482 ), #214408, .T. ) ;
#53210 = ORIENTED_EDGE ( 'NONE', *, *, #242514, .T. ) ;
#53212 =( BOUNDED_SURFACE ( )  B_SPLINE_SURFACE ( 3, 2, ( 
 ( #52265, #194393, #133116 ),
 ( #56117, #113545, #233514 ),
 ( #130534, #193096, #190541 ),
 ( #152709, #213930, #95264 ),
 ( #35335, #169713, #10604 ),
 ( #173576, #210098, #135658 ),
 ( #134369, #171006, #92688 ),
 ( #172286, #114827, #251772 ),
 ( #110980, #230953, #36613 ),
 ( #131820, #73170, #50973 ) ),
 .UNSPECIFIED., .F., .F., .F. ) 
 B_SPLINE_SURFACE_WITH_KNOTS ( ( 4, 2, 2, 2, 4 ),
 ( 3, 3 ),
 ( 0.002161241639767276426, 0.002579950749615843482, 0.002789305304540127227, 0.002893982582002269099, 0.002998659859464410972 ),
 ( 0.000000000000000000, 1.000000000000000000 ),
 .UNSPECIFIED. ) 
 GEOMETRIC_REPRESENTATION_ITEM ( )  RATIONAL_B_SPLINE_SURFACE ( (
 ( 1.000000000000000000, 0.7071067811865475727, 1.000000000000000000),
 ( 1.000000000000000000, 0.7632447400667128345, 1.000000000000000000),
 ( 1.000000000000000000, 0.8158073005106601938, 1.000000000000000000),
 ( 1.000000000000000000, 0.8906973462397633767, 1.000000000000000000),
 ( 1.000000000000000000, 0.9149408947802050163, 1.000000000000000000),
 ( 1.000000000000000000, 0.9493368785274935995, 1.000000000000000000),
 ( 1.000000000000000000, 0.9605194247158138632, 1.000000000000000000),
 ( 1.000000000000000000, 0.9803630264779780168, 1.000000000000000000),
 ( 1.000000000000000000, 0.9900844824272214684, 1.000000000000000000),
 ( 1.000000000000000000, 0.9894588281429246290, 1.000000000000000000) ) ) 
 REPRESENTATION_ITEM ( '' )  SURFACE ( )  );
#53211 = DIRECTION ( 'NONE',  ( 1.000000000000000000, 7.304098846218134667E-16, -0.000000000000000000 ) ) ;
#53213 = ORIENTED_EDGE ( 'NONE', *, *, #136116, .F. ) ;
#53214 = CARTESIAN_POINT ( 'NONE',  ( 20.04142135623730070, 51.38014393322265505, -230.1906178717505611 ) ) ;
#53215 = CARTESIAN_POINT ( 'NONE',  ( 18.59999999999999432, 1.162701749938009677, -8.099999999999999645 ) ) ;
#53216 = AXIS2_PLACEMENT_3D ( 'NONE', #24040, #246907, #184363 ) ;
#53217 = CARTESIAN_POINT ( 'NONE',  ( -16.97683809663752186, 23.59405348476697739, -231.3784738672519552 ) ) ;
#53218 = FACE_OUTER_BOUND ( 'NONE', #111646, .T. ) ;
#53219 = DIRECTION ( 'NONE',  ( -1.000000000000000000, -0.000000000000000000, -0.000000000000000000 ) ) ;
#53220 = DIRECTION ( 'NONE',  ( -0.000000000000000000, -0.8660254037844468122, -0.4999999999999860112 ) ) ;
#53221 = DIRECTION ( 'NONE',  ( 0.000000000000000000, -7.429790795770644761E-15, 1.000000000000000000 ) ) ;
#53224 = DIRECTION ( 'NONE',  ( 0.000000000000000000, 0.000000000000000000, 1.000000000000000000 ) ) ;
#53223 = VECTOR ( 'NONE', #253048, 1000.000000000000000 ) ;
#53222 = CARTESIAN_POINT ( 'NONE',  ( -16.94445028196807002, 66.00793639031451221, -149.1304376629428816 ) ) ;
#53225 = EDGE_CURVE ( 'NONE', #163390, #122995, #194876, .T. ) ;
#53226 = DIRECTION ( 'NONE',  ( -0.000000000000000000, -0.000000000000000000, -1.000000000000000000 ) ) ;
#53227 = CARTESIAN_POINT ( 'NONE',  ( 20.97462148592293829, 22.12183205585962043, -231.6962180060701542 ) ) ;
#53228 = DIRECTION ( 'NONE',  ( -1.000000000000000000, 0.000000000000000000, 0.000000000000000000 ) ) ;
#53229 = ORIENTED_EDGE ( 'NONE', *, *, #18098, .T. ) ;
#53230 = CIRCLE ( 'NONE', #140712, 0.1000000000000028644 ) ;
#53231 = CARTESIAN_POINT ( 'NONE',  ( -18.50000000000000000, -9.421290279523317324, -40.32388217902604310 ) ) ;
#53232 = ADVANCED_FACE ( 'NONE', ( #216964 ), #145134, .T. ) ;
#53233 = AXIS2_PLACEMENT_3D ( 'NONE', #155922, #112921, #232893 ) ;
#53234 = DIRECTION ( 'NONE',  ( 0.000000000000000000, 0.000000000000000000, -1.000000000000000000 ) ) ;
#53235 = CARTESIAN_POINT ( 'NONE',  ( -23.15000000000000213, 85.50000000001188027, -93.12913836187179584 ) ) ;
#53236 =( BOUNDED_SURFACE ( )  B_SPLINE_SURFACE ( 3, 2, ( 
 ( #242910, #64283, #224626 ),
 ( #82524, #43438, #124268 ),
 ( #45993, #203786, #176866 ),
 ( #25178, #116868, #235518 ) ),
 .UNSPECIFIED., .F., .F., .F. ) 
 B_SPLINE_SURFACE_WITH_KNOTS ( ( 4, 4 ),
 ( 3, 3 ),
 ( 3.658908243880890421, 4.712388980384689674 ),
 ( 0.000000000000000000, 1.000000000000000000 ),
 .UNSPECIFIED. ) 
 GEOMETRIC_REPRESENTATION_ITEM ( )  RATIONAL_B_SPLINE_SURFACE ( (
 ( 1.000000000000000000, 0.8984936768950618768, 1.000000000000000000),
 ( 1.000000000000000000, 0.8646876308615185636, 1.000000000000000000),
 ( 1.000000000000000000, 0.7953136715913637911, 1.000000000000000000),
 ( 1.000000000000000000, 0.7071067811865475727, 1.000000000000000000) ) ) 
 REPRESENTATION_ITEM ( '' )  SURFACE ( )  );
#53237 = VECTOR ( 'NONE', #184257, 1000.000000000000000 ) ;
#53238 = DIRECTION ( 'NONE',  ( -1.000000000000000000, 0.000000000000000000, -0.000000000000000000 ) ) ;
#53240 = EDGE_CURVE ( 'NONE', #198941, #9680, #8907, .T. ) ;
#53239 = PLANE ( 'NONE',  #179073 ) ;
#53241 = AXIS2_PLACEMENT_3D ( 'NONE', #223442, #167367, #205157 ) ;
#53242 = CYLINDRICAL_SURFACE ( 'NONE', #156053, 0.09999999999999781286 ) ;
#53243 = ORIENTED_EDGE ( 'NONE', *, *, #143991, .T. ) ;
#53244 = EDGE_CURVE ( 'NONE', #212047, #200852, #175510, .T. ) ;
#53245 = SPHERICAL_SURFACE ( 'NONE', #151429, 0.1000000000000000056 ) ;
#53246 = ORIENTED_EDGE ( 'NONE', *, *, #225001, .F. ) ;
#53247 = DIRECTION ( 'NONE',  ( -1.000000000000000000, -1.394253735153569469E-16, -2.602809386958778209E-16 ) ) ;
#53248 = CARTESIAN_POINT ( 'NONE',  ( -23.25000000000000000, 87.75000000001266187, -200.4231074845242802 ) ) ;
#53249 = EDGE_CURVE ( 'NONE', #186535, #3891, #100840, .T. ) ;
#53250 = VECTOR ( 'NONE', #165835, 1000.000000000000000 ) ;
#53251 = VECTOR ( 'NONE', #43434, 1000.000000000000000 ) ;
#53252 = CIRCLE ( 'NONE', #223917, 2.100000000000004530 ) ;
#53253 = AXIS2_PLACEMENT_3D ( 'NONE', #59091, #198639, #201208 ) ;
#53255 = EDGE_LOOP ( 'NONE', ( #147139, #92782, #233219, #125832 ) ) ;
#53254 = TOROIDAL_SURFACE ( 'NONE', #178175, 0.2000000000000000111, 0.1000000000000000056 ) ;
#53256 = DIRECTION ( 'NONE',  ( -0.9880948137434723000, 0.1538461538461483591, -0.000000000000000000 ) ) ;
#53257 = ORIENTED_EDGE ( 'NONE', *, *, #59620, .T. ) ;
#53258 = EDGE_CURVE ( 'NONE', #114996, #189246, #14575, .T. ) ;
#53259 = AXIS2_PLACEMENT_3D ( 'NONE', #92129, #97215, #191261 ) ;
#53260 = CARTESIAN_POINT ( 'NONE',  ( -23.15000000000000213, -8.663551401869156621, -23.97589888193269658 ) ) ;
#53261 = ADVANCED_FACE ( 'NONE', ( #159587 ), #162171, .T. ) ;
#53262 = CARTESIAN_POINT ( 'NONE',  ( 21.11345278033298456, 67.11787792664036090, -124.2770853137694473 ) ) ;
#53264 = CARTESIAN_POINT ( 'NONE',  ( 18.39999999999999503, 13.90230816252088530, -210.9187585823742666 ) ) ;
#53263 = UNCERTAINTY_MEASURE_WITH_UNIT (LENGTH_MEASURE( 1.000000000000000082E-05 ), #55069, 'distance_accuracy_value', 'NONE');
#53265 = LINE ( 'NONE', #111967, #79255 ) ;
#53266 = DIRECTION ( 'NONE',  ( -0.000000000000000000, 6.982962677686266711E-15, -1.000000000000000000 ) ) ;
#53267 = FACE_BOUND ( 'NONE', #207674, .T. ) ;
#53268 = DIRECTION ( 'NONE',  ( -0.000000000000000000, 1.000000000000000000, -0.000000000000000000 ) ) ;
#53269 = DIRECTION ( 'NONE',  ( 0.000000000000000000, 0.4088369013362458948, -0.9126074666064137864 ) ) ;
#53271 = ORIENTED_EDGE ( 'NONE', *, *, #201124, .T. ) ;
#53270 = CARTESIAN_POINT ( 'NONE',  ( 21.05000000000000071, 85.50000000001222134, -146.4170766071767389 ) ) ;
#53273 = CARTESIAN_POINT ( 'NONE',  ( 21.14999999999999858, 11.65000000001116298, -79.15000000000004832 ) ) ;
#53272 = CARTESIAN_POINT ( 'NONE',  ( 23.24999999999999645, 76.00000000001170974, -69.52310748452431710 ) ) ;
#53274 = EDGE_LOOP ( 'NONE', ( #198089, #78044, #32400, #190722 ) ) ;
#53276 = ORIENTED_EDGE ( 'NONE', *, *, #158826, .F. ) ;
#53275 =( LENGTH_UNIT ( ) NAMED_UNIT ( * ) SI_UNIT ( .MILLI., .METRE. ) );
#53277 = TOROIDAL_SURFACE ( 'NONE', #140753, 0.6000000000000013101, 0.1000000000000000056 ) ;
#53278 = EDGE_LOOP ( 'NONE', ( #204668, #214963, #252794, #15461 ) ) ;
#53279 = FACE_OUTER_BOUND ( 'NONE', #36763, .T. ) ;
#53280 = AXIS2_PLACEMENT_3D ( 'NONE', #252552, #110483, #11404 ) ;
#53281 = AXIS2_PLACEMENT_3D ( 'NONE', #217034, #556, #81360 ) ;
#53282 = CARTESIAN_POINT ( 'NONE',  ( 18.59999999999999787, -10.84999999999999076, -15.00000000000000000 ) ) ;
#53283 = CARTESIAN_POINT ( 'NONE',  ( -21.44999999999999929, 68.75000000001223555, -148.8731074845244109 ) ) ;
#53284 = CARTESIAN_POINT ( 'NONE',  ( 18.39999999999999503, -9.499999999999996447, -6.999362097180139131 ) ) ;
#53285 = LINE ( 'NONE', #233226, #185792 ) ;
#53286 = DIRECTION ( 'NONE',  ( 1.000000000000000000, -0.000000000000000000, 0.000000000000000000 ) ) ;
#53287 = DIRECTION ( 'NONE',  ( -1.000000000000000000, -8.674042436075348305E-17, -1.619280515896124405E-16 ) ) ;
#53288 = AXIS2_PLACEMENT_3D ( 'NONE', #23330, #121150, #256723 ) ;
#53289 = DIRECTION ( 'NONE',  ( -1.000000000000000000, -0.000000000000000000, -0.000000000000000000 ) ) ;
#53290 = ORIENTED_EDGE ( 'NONE', *, *, #132832, .F. ) ;
#53291 = ORIENTED_EDGE ( 'NONE', *, *, #59183, .F. ) ;
#53292 = FACE_OUTER_BOUND ( 'NONE', #102238, .T. ) ;
#53293 = EDGE_CURVE ( 'NONE', #244409, #247770, #83845, .T. ) ;
#53294 = ORIENTED_EDGE ( 'NONE', *, *, #76527, .F. ) ;
#53295 = FACE_OUTER_BOUND ( 'NONE', #244275, .T. ) ;
#53296 = EDGE_LOOP ( 'NONE', ( #169110, #40589, #243288, #225183 ) ) ;
#53297 = CARTESIAN_POINT ( 'NONE',  ( 18.60000000000000142, -9.480686695278970788, -40.44111516875785384 ) ) ;
#53298 = CIRCLE ( 'NONE', #161656, 11.64999999999999325 ) ;
#53299 = FACE_OUTER_BOUND ( 'NONE', #90661, .T. ) ;
#53300 = DIRECTION ( 'NONE',  ( 1.000000000000000000, 0.000000000000000000, 0.000000000000000000 ) ) ;
#53301 = FACE_OUTER_BOUND ( 'NONE', #53135, .T. ) ;
#53302 = FACE_OUTER_BOUND ( 'NONE', #156942, .T. ) ;
#53303 = VERTEX_POINT ( 'NONE', #203834 ) ;
#53304 = TOROIDAL_SURFACE ( 'NONE', #199051, 0.4000000000000017431, 0.1000000000000000056 ) ;
#53305 = CARTESIAN_POINT ( 'NONE',  ( 21.00000000000000000, 9.750000000011153745, -88.15000000000004832 ) ) ;
#53306 = TOROIDAL_SURFACE ( 'NONE', #232395, 0.2000000000000000111, 0.1000000000000000056 ) ;
#53307 = CARTESIAN_POINT ( 'NONE',  ( 20.85000000000000142, 68.87972903831429505, -99.36354444268502561 ) ) ;
#53308 = DIRECTION ( 'NONE',  ( 1.073024830501117725E-15, 0.2617529984165031243, 0.9651348961777157509 ) ) ;
#53309 = AXIS2_PLACEMENT_3D ( 'NONE', #252123, #153078, #93052 ) ;
#53310 = LINE ( 'NONE', #14206, #240439 ) ;
#53311 = EDGE_CURVE ( 'NONE', #135750, #90736, #241684, .T. ) ;
#53312 = VERTEX_POINT ( 'NONE', #239121 ) ;
#53314 = DIRECTION ( 'NONE',  ( 0.000000000000000000, -7.429790795770644761E-15, 1.000000000000000000 ) ) ;
#53313 = LINE ( 'NONE', #94997, #129123 ) ;
#53315 = ORIENTED_EDGE ( 'NONE', *, *, #129665, .T. ) ;
#53318 = ORIENTED_EDGE ( 'NONE', *, *, #55155, .T. ) ;
#53317 = CARTESIAN_POINT ( 'NONE',  ( 20.85000000000000142, 87.65000000001144542, -38.92310748452424463 ) ) ;
#53316 = CARTESIAN_POINT ( 'NONE',  ( -18.50000000000000711, 11.75000000001115197, -74.01480577065404987 ) ) ;
#53319 = VECTOR ( 'NONE', #200291, 1000.000000000000000 ) ;
#53320 = CARTESIAN_POINT ( 'NONE',  ( 23.14999999999999147, 76.00000000001237765, -170.0231074845243597 ) ) ;
#53321 = DIRECTION ( 'NONE',  ( 1.000000000000000000, -3.265361837132813093E-16, -2.280189983783949500E-30 ) ) ;
#53322 = ORIENTED_EDGE ( 'NONE', *, *, #222296, .F. ) ;
#53323 = DIRECTION ( 'NONE',  ( 0.000000000000000000, 0.000000000000000000, -1.000000000000000000 ) ) ;
#53324 = DIRECTION ( 'NONE',  ( 0.000000000000000000, -0.1298341882520022694, -0.9915357197604853789 ) ) ;
#53326 = EDGE_LOOP ( 'NONE', ( #119090, #146361, #120659, #169657 ) ) ;
#53325 = LINE ( 'NONE', #132876, #210046 ) ;
#53327 = AXIS2_PLACEMENT_3D ( 'NONE', #46816, #188920, #222897 ) ;
#53328 = ORIENTED_EDGE ( 'NONE', *, *, #108051, .T. ) ;
#53329 = DIRECTION ( 'NONE',  ( 0.000000000000000000, 0.9915357197604982575, -0.1298341882519033486 ) ) ;
#53330 = CARTESIAN_POINT ( 'NONE',  ( 20.94999999999999929, 46.45388641681647357, -243.1520440498138385 ) ) ;
#53331 = DIRECTION ( 'NONE',  ( 0.000000000000000000, 0.9858045116447881062, -0.1678971852675942011 ) ) ;
#53332 = VECTOR ( 'NONE', #204629, 1000.000000000000000 ) ;
#53333 = B_SPLINE_CURVE_WITH_KNOTS ( 'NONE', 3,
 ( #246823, #68202, #109876, #10797 ),
 .UNSPECIFIED., .F., .F.,
 ( 4, 4 ),
 ( 0.000000000000000000, 7.713889350926232550E-05 ),
 .UNSPECIFIED. ) ;
#53334 = CARTESIAN_POINT ( 'NONE',  ( 21.05000000000000071, -4.969162394454520459, -233.3995358778103935 ) ) ;
#53335 = VERTEX_POINT ( 'NONE', #220829 ) ;
#53336 = CARTESIAN_POINT ( 'NONE',  ( -18.59999999999999787, 21.13195309841794867, -243.6318585593224100 ) ) ;
#53337 = DIRECTION ( 'NONE',  ( -1.000000000000000000, -2.986185139342072849E-16, 6.665775143889691788E-16 ) ) ;
#53338 = DIRECTION ( 'NONE',  ( 0.000000000000000000, -1.000000000000000000, 0.000000000000000000 ) ) ;
#53339 = ORIENTED_EDGE ( 'NONE', *, *, #185465, .T. ) ;
#53340 = CARTESIAN_POINT ( 'NONE',  ( 20.97250901189795513, 58.98335100983494073, -225.6767934319825031 ) ) ;
#53341 = CARTESIAN_POINT ( 'NONE',  ( -20.54999999999999716, 7.249999999999999112, -21.25000000000000000 ) ) ;
#53342 = EDGE_CURVE ( 'NONE', #18319, #127125, #160883, .T. ) ;
#53343 = ORIENTED_EDGE ( 'NONE', *, *, #218646, .T. ) ;
#53344 = VECTOR ( 'NONE', #27600, 1000.000000000000000 ) ;
#53345 = AXIS2_PLACEMENT_3D ( 'NONE', #159362, #180206, #101905 ) ;
#53347 = AXIS2_PLACEMENT_3D ( 'NONE', #102408, #163711, #223658 ) ;
#53346 = FACE_OUTER_BOUND ( 'NONE', #159183, .T. ) ;
#53348 = LINE ( 'NONE', #12965, #218787 ) ;
#53349 = CIRCLE ( 'NONE', #11867, 0.09999999999999939493 ) ;
#53350 = EDGE_LOOP ( 'NONE', ( #49773, #60680, #62481, #67815 ) ) ;
#53351 = ORIENTED_EDGE ( 'NONE', *, *, #56746, .T. ) ;
#53352 = EDGE_CURVE ( 'NONE', #86370, #137392, #133784, .T. ) ;
#53353 = CARTESIAN_POINT ( 'NONE',  ( -20.15000000000000568, 9.291421356248463326, -155.2500000000000284 ) ) ;
#53354 = VERTEX_POINT ( 'NONE', #85138 ) ;
#53356 = ORIENTED_EDGE ( 'NONE', *, *, #183941, .F. ) ;
#53355 = DIRECTION ( 'NONE',  ( 0.000000000000000000, 0.000000000000000000, 1.000000000000000000 ) ) ;
#53357 = EDGE_CURVE ( 'NONE', #67636, #204739, #104710, .T. ) ;
#53360 = ORIENTED_EDGE ( 'NONE', *, *, #46960, .F. ) ;
#53359 = ORIENTED_EDGE ( 'NONE', *, *, #25094, .F. ) ;
#53358 = DIRECTION ( 'NONE',  ( 0.000000000000000000, 0.8777080977375655291, -0.4791956752370622463 ) ) ;
#53361 = AXIS2_PLACEMENT_3D ( 'NONE', #61851, #217041, #141373 ) ;
#53362 = CARTESIAN_POINT ( 'NONE',  ( 21.13736287352038445, 29.30757664734318624, -236.4848457208103412 ) ) ;
#53363 = CIRCLE ( 'NONE', #20062, 0.1000000000000023231 ) ;
#53365 = EDGE_CURVE ( 'NONE', #38939, #146901, #244233, .T. ) ;
#53364 = ORIENTED_EDGE ( 'NONE', *, *, #93326, .F. ) ;
#53366 = DIRECTION ( 'NONE',  ( 0.000000000000000000, -0.1568667991644863147, 0.9876197685951252359 ) ) ;
#53367 = CARTESIAN_POINT ( 'NONE',  ( 21.10642757222115407, 10.72315628916975250, -112.7406975237852436 ) ) ;
#53368 = DIRECTION ( 'NONE',  ( 0.000000000000000000, -1.000000000000000000, 0.000000000000000000 ) ) ;
#53369 = CARTESIAN_POINT ( 'NONE',  ( -20.94999999999999929, 72.93748991853820485, -214.8151857698041738 ) ) ;
#53370 = AXIS2_PLACEMENT_3D ( 'NONE', #114659, #15589, #254151 ) ;
#53371 = DIRECTION ( 'NONE',  ( 1.000000000000000000, 0.000000000000000000, 0.000000000000000000 ) ) ;
#53372 = EDGE_LOOP ( 'NONE', ( #109258, #253790, #222394, #62234, #32305 ) ) ;
#53373 = ORIENTED_EDGE ( 'NONE', *, *, #129460, .T. ) ;
#53374 = EDGE_LOOP ( 'NONE', ( #92161, #111697, #231889, #206327, #185586, #186783 ) ) ;
#53375 = CARTESIAN_POINT ( 'NONE',  ( 21.14999999999999858, -0.09999999998884338825, -155.8504291924551808 ) ) ;
#53377 = EDGE_LOOP ( 'NONE', ( #58870, #190647, #111395, #185049 ) ) ;
#53376 = CARTESIAN_POINT ( 'NONE',  ( -16.93211319090181632, 66.00001321885507366, -182.6006019852513589 ) ) ;
#53378 = CYLINDRICAL_SURFACE ( 'NONE', #125745, 0.09999999999999939493 ) ;
#53380 = EDGE_LOOP ( 'NONE', ( #98898, #252846, #256733, #173490 ) ) ;
#53379 = DIRECTION ( 'NONE',  ( 1.000000000000000000, 0.000000000000000000, 0.000000000000000000 ) ) ;
#53381 = EDGE_CURVE ( 'NONE', #180654, #171717, #250497, .T. ) ;
#53382 = EDGE_LOOP ( 'NONE', ( #121803, #46980, #228766, #211546 ) ) ;
#53383 = FACE_OUTER_BOUND ( 'NONE', #211588, .T. ) ;
#53384 = EDGE_LOOP ( 'NONE', ( #70548, #167209, #31270, #75524 ) ) ;
#53385 = CYLINDRICAL_SURFACE ( 'NONE', #227107, 0.09999999999999681366 ) ;
#53386 = DIRECTION ( 'NONE',  ( 0.000000000000000000, -0.000000000000000000, 1.000000000000000000 ) ) ;
#53387 = VECTOR ( 'NONE', #141958, 1000.000000000000000 ) ;
#53388 = AXIS2_PLACEMENT_3D ( 'NONE', #224606, #65532, #169824 ) ;
#53389 = CIRCLE ( 'NONE', #95079, 0.09999999999999954758 ) ;
#53391 = ORIENTED_EDGE ( 'NONE', *, *, #80279, .T. ) ;
#53390 = ORIENTED_EDGE ( 'NONE', *, *, #235520, .F. ) ;
#53392 = ORIENTED_EDGE ( 'NONE', *, *, #201426, .F. ) ;
#53393 = FACE_OUTER_BOUND ( 'NONE', #189612, .T. ) ;
#53394 = ORIENTED_EDGE ( 'NONE', *, *, #76572, .F. ) ;
#53395 = ORIENTED_EDGE ( 'NONE', *, *, #50731, .F. ) ;
#53397 = ORIENTED_EDGE ( 'NONE', *, *, #105037, .F. ) ;
#53396 = FACE_OUTER_BOUND ( 'NONE', #176773, .T. ) ;
#53398 = DIRECTION ( 'NONE',  ( 1.000000000000000000, 0.000000000000000000, 0.000000000000000000 ) ) ;
#53400 = B_SPLINE_CURVE_WITH_KNOTS ( 'NONE', 3,
 ( #108804, #9705, #113944, #13581, #129662, #51369, #173981, #30587, #110093, #228777, #132234, #252163, #210493, #31875, #130949, #172695, #89241, #73574, #52678 ),
 .UNSPECIFIED., .F., .F.,
 ( 4, 3, 3, 3, 3, 3, 4 ),
 ( 1.387778780781445676E-17, 2.646747978909012316E-05, 5.271166642128706850E-05, 9.008788829884963154E-05, 0.0001426648776560992193, 0.0001897378458659761016, 0.0001917382627806360094 ),
 .UNSPECIFIED. ) ;
#53399 = VECTOR ( 'NONE', #38161, 1000.000000000000000 ) ;
#53402 = CARTESIAN_POINT ( 'NONE',  ( 21.03675099975490070, 11.29478665154959316, -211.1545853719440800 ) ) ;
#53401 = FACE_OUTER_BOUND ( 'NONE', #8630, .T. ) ;
#53403 = DIRECTION ( 'NONE',  ( 0.000000000000000000, 0.9770955615653550419, 0.2128009952262526761 ) ) ;
#53404 = DIRECTION ( 'NONE',  ( 1.000000000000000000, 0.000000000000000000, 0.000000000000000000 ) ) ;
#53405 = ORIENTED_EDGE ( 'NONE', *, *, #25343, .T. ) ;
#53406 = ORIENTED_EDGE ( 'NONE', *, *, #156226, .F. ) ;
#53407 = CARTESIAN_POINT ( 'NONE',  ( 18.39999999999999858, 85.50000000001185185, -96.10095763519375112 ) ) ;
#53408 = DIRECTION ( 'NONE',  ( 0.000000000000000000, 0.000000000000000000, -1.000000000000000000 ) ) ;
#53409 = CARTESIAN_POINT ( 'NONE',  ( 23.24999999999999289, 64.35000000001221565, -148.2731074845243882 ) ) ;
#53410 = ORIENTED_EDGE ( 'NONE', *, *, #49447, .T. ) ;
#53411 = CARTESIAN_POINT ( 'NONE',  ( -21.05000000000000071, 18.18127959618848877, -237.5711165786817389 ) ) ;
#53412 = VECTOR ( 'NONE', #43042, 1000.000000000000000 ) ;
#53413 = ADVANCED_FACE ( 'NONE', ( #120486 ), #483, .T. ) ;
#53414 = CARTESIAN_POINT ( 'NONE',  ( -16.93658211146644987, 51.65037976959903432, -231.8840172928964591 ) ) ;
#53415 = CARTESIAN_POINT ( 'NONE',  ( 18.59999999999999076, 77.25000000001209344, -128.5231074845242745 ) ) ;
#53416 = CIRCLE ( 'NONE', #199161, 12.77499999999999503 ) ;
#53417 = ORIENTED_EDGE ( 'NONE', *, *, #213163, .F. ) ;
#53418 = ORIENTED_EDGE ( 'NONE', *, *, #192188, .T. ) ;
#53419 = DIRECTION ( 'NONE',  ( 1.000000000000000000, -1.836970198721029934E-16, -1.282749433769087582E-30 ) ) ;
#53420 = CARTESIAN_POINT ( 'NONE',  ( -16.79814274880124358, 66.05072745733475870, -123.8706744474763752 ) ) ;
#53421 = ORIENTED_EDGE ( 'NONE', *, *, #162211, .F. ) ;
#53422 = LINE ( 'NONE', #75582, #18164 ) ;
#53423 = ORIENTED_EDGE ( 'NONE', *, *, #226020, .F. ) ;
#53424 = LINE ( 'NONE', #91278, #168998 ) ;
#53426 = ADVANCED_FACE ( 'NONE', ( #80006 ), #13194, .F. ) ;
#53425 = CARTESIAN_POINT ( 'NONE',  ( -16.77683809663752257, 9.945835743215303282, -154.8360509808958057 ) ) ;
#53428 = DIRECTION ( 'NONE',  ( 0.000000000000000000, 7.086529944415894657E-15, -1.000000000000000000 ) ) ;
#53427 = DIRECTION ( 'NONE',  ( 0.000000000000000000, 0.9126074666063770380, 0.4088369013363281068 ) ) ;
#53429 = CIRCLE ( 'NONE', #82604, 0.1000000000000102612 ) ;
#53430 = DIRECTION ( 'NONE',  ( 0.000000000000000000, 0.000000000000000000, -1.000000000000000000 ) ) ;
#53431 = CARTESIAN_POINT ( 'NONE',  ( 18.52643265882457868, 65.68026841930954163, -164.4725740131889893 ) ) ;
#53432 = DIRECTION ( 'NONE',  ( 1.000000000000000000, 0.000000000000000000, -0.000000000000000000 ) ) ;
#53433 = EDGE_CURVE ( 'NONE', #39957, #95339, #54682, .T. ) ;
#53434 = EDGE_CURVE ( 'NONE', #35976, #178841, #200433, .T. ) ;
#53435 = CIRCLE ( 'NONE', #186720, 1.500000000000001332 ) ;
#53437 = ORIENTED_EDGE ( 'NONE', *, *, #200586, .T. ) ;
#53436 = FACE_OUTER_BOUND ( 'NONE', #15571, .T. ) ;
#53438 = AXIS2_PLACEMENT_3D ( 'NONE', #220490, #101774, #2696 ) ;
#53441 = ORIENTED_EDGE ( 'NONE', *, *, #229237, .F. ) ;
#53440 = ORIENTED_EDGE ( 'NONE', *, *, #92158, .F. ) ;
#53439 = CIRCLE ( 'NONE', #140925, 0.09999999999998898659 ) ;
#53442 = VERTEX_POINT ( 'NONE', #72052 ) ;
#53443 = CIRCLE ( 'NONE', #95133, 0.09999999999999939493 ) ;
#53444 = DIRECTION ( 'NONE',  ( 0.000000000000000000, -0.8700118002898357128, 0.4930308989875170633 ) ) ;
#53445 = EDGE_CURVE ( 'NONE', #68619, #158463, #150304, .T. ) ;
#53446 = CARTESIAN_POINT ( 'NONE',  ( 22.39999999999999503, 0.000000000000000000, 11.64957080754479968 ) ) ;
#53447 = EDGE_CURVE ( 'NONE', #187354, #18995, #225937, .T. ) ;
#53449 = CARTESIAN_POINT ( 'NONE',  ( -22.49544290803785174, 11.74987023786834506, -33.43468804074269940 ) ) ;
#53448 = CARTESIAN_POINT ( 'NONE',  ( -16.80469485234340965, 66.05784833687151547, -182.7131406405933092 ) ) ;
#53450 = CARTESIAN_POINT ( 'NONE',  ( 21.05000000000000071, 5.850000000011105428, -110.6324972242780120 ) ) ;
#53451 = ORIENTED_EDGE ( 'NONE', *, *, #96735, .F. ) ;
#53452 = EDGE_CURVE ( 'NONE', #433, #86347, #21062, .T. ) ;
#53453 = CARTESIAN_POINT ( 'NONE',  ( -18.59999999999999787, 1.162701749949165642, -175.5999999999999659 ) ) ;
#53454 = ORIENTED_EDGE ( 'NONE', *, *, #103943, .T. ) ;
#53455 = ORIENTED_EDGE ( 'NONE', *, *, #208102, .T. ) ;
#53456 = CARTESIAN_POINT ( 'NONE',  ( 20.85000000000000142, -1.263275465206102233, -74.90186466674640542 ) ) ;
#53457 = DIRECTION ( 'NONE',  ( 1.000000000000000000, -0.000000000000000000, 0.000000000000000000 ) ) ;
#53458 = CARTESIAN_POINT ( 'NONE',  ( -18.34374000495059676, 11.47316190337362940, -91.25000000000005684 ) ) ;
#53459 = AXIS2_PLACEMENT_3D ( 'NONE', #47861, #109122, #126116 ) ;
#53460 = CIRCLE ( 'NONE', #194940, 0.09999999999998898659 ) ;
#53461 = DIRECTION ( 'NONE',  ( 0.000000000000000000, 0.6728971962617102953, -0.7397360091702507301 ) ) ;
#53462 = CARTESIAN_POINT ( 'NONE',  ( 22.49999999999999645, 0.1008583691098678403, -155.7504328765105868 ) ) ;
#53463 = ORIENTED_EDGE ( 'NONE', *, *, #29260, .T. ) ;
#53464 = ORIENTED_EDGE ( 'NONE', *, *, #213875, .F. ) ;
#53465 = CARTESIAN_POINT ( 'NONE',  ( -16.92570016628983609, 9.958788957751018245, -54.37934932996099491 ) ) ;
#53466 = EDGE_CURVE ( 'NONE', #214984, #39096, #192259, .T. ) ;
#53467 = CARTESIAN_POINT ( 'NONE',  ( -18.59999999999999787, -9.321008403350132809, -40.73593824907788274 ) ) ;
#53468 = EDGE_CURVE ( 'NONE', #100214, #12612, #113138, .T. ) ;
#53469 = FACE_OUTER_BOUND ( 'NONE', #209082, .T. ) ;
#53470 = CARTESIAN_POINT ( 'NONE',  ( 18.59999999999999787, 77.25000000001136868, -28.22262673010923706 ) ) ;
#53471 = ADVANCED_FACE ( 'NONE', ( #188135 ), #208818, .T. ) ;
#53472 = DIRECTION ( 'NONE',  ( 0.7071359030027419834, 0.000000000000000000, -0.7070776581709371511 ) ) ;
#53473 = DIRECTION ( 'NONE',  ( -1.000000000000000000, 0.000000000000000000, 0.000000000000000000 ) ) ;
#53474 = CIRCLE ( 'NONE', #36752, 0.1000000000000004774 ) ;
#53476 = DIRECTION ( 'NONE',  ( 0.000000000000000000, 0.000000000000000000, -1.000000000000000000 ) ) ;
#53475 = LINE ( 'NONE', #170908, #61970 ) ;
#53477 = CARTESIAN_POINT ( 'NONE',  ( -20.85000000000000142, 76.00000000001213607, -136.5231074845243313 ) ) ;
#53478 = CIRCLE ( 'NONE', #236609, 0.09999999999999105438 ) ;
#53479 = DIRECTION ( 'NONE',  ( -0.000000000000000000, 0.1350103645451876666, -0.9908441862701600211 ) ) ;
#53480 = DIRECTION ( 'NONE',  ( 0.7071067811865474617, 0.6909108974501236844, 0.1504730267678057731 ) ) ;
#53482 = CARTESIAN_POINT ( 'NONE',  ( 20.04999999999999716, 67.25000000001251976, -182.6731074845244223 ) ) ;
#53481 = AXIS2_PLACEMENT_3D ( 'NONE', #215481, #78532, #21172 ) ;
#53484 = ORIENTED_EDGE ( 'NONE', *, *, #97584, .T. ) ;
#53483 = CARTESIAN_POINT ( 'NONE',  ( -23.25000000000000000, -1.249999999988843369, -108.3004807544151191 ) ) ;
#53485 = VECTOR ( 'NONE', #187827, 1000.000000000000000 ) ;
#53486 = EDGE_CURVE ( 'NONE', #170111, #240969, #121371, .T. ) ;
#53487 = ADVANCED_FACE ( 'NONE', ( #208976 ), #128165, .T. ) ;
#53488 = DIRECTION ( 'NONE',  ( 0.000000000000000000, 0.000000000000000000, -1.000000000000000000 ) ) ;
#53489 = CIRCLE ( 'NONE', #140984, 0.1000000000000018374 ) ;
#53490 = CARTESIAN_POINT ( 'NONE',  ( -22.49544290803753199, 64.25012976215464278, -103.0884194437819730 ) ) ;
#53491 = AXIS2_PLACEMENT_3D ( 'NONE', #237895, #138756, #61839 ) ;
#53492 = AXIS2_PLACEMENT_3D ( 'NONE', #49939, #129492, #250708 ) ;
#53493 = ADVANCED_FACE ( 'NONE', ( #189426 ), #171188, .F. ) ;
#53494 = DIRECTION ( 'NONE',  ( 1.186688945009009831E-16, -0.9770955615653313941, -0.2128009952263603677 ) ) ;
#53495 = CIRCLE ( 'NONE', #136677, 0.1000000000000028644 ) ;
#53496 = CYLINDRICAL_SURFACE ( 'NONE', #98948, 0.1000000000000000472 ) ;
#53497 = CARTESIAN_POINT ( 'NONE',  ( 23.24999999999997513, 11.65000000000000746, -26.48519422934605672 ) ) ;
#53498 = CIRCLE ( 'NONE', #82499, 4.049999999999998046 ) ;
#53499 = CARTESIAN_POINT ( 'NONE',  ( 21.14999999999999858, 6.257814610487280937, -66.90220970869124528 ) ) ;
#53500 = LINE ( 'NONE', #16955, #111427 ) ;
#53501 = EDGE_LOOP ( 'NONE', ( #44483, #173603, #226238, #194199 ) ) ;
#53502 = DIRECTION ( 'NONE',  ( -1.000000000000000000, -0.000000000000000000, -0.000000000000000000 ) ) ;
#53504 = ORIENTED_EDGE ( 'NONE', *, *, #69115, .T. ) ;
#53503 = DIRECTION ( 'NONE',  ( 0.000000000000000000, 0.000000000000000000, -1.000000000000000000 ) ) ;
#53505 = CYLINDRICAL_SURFACE ( 'NONE', #84026, 0.1000000000000028644 ) ;
#53506 = CARTESIAN_POINT ( 'NONE',  ( 21.05000000000000071, 1.115600667400684642E-11, -112.6500000000000341 ) ) ;
#53507 = ORIENTED_EDGE ( 'NONE', *, *, #55829, .F. ) ;
#53508 = CARTESIAN_POINT ( 'NONE',  ( -16.79270642812251069, 66.05375578307388196, -190.8620407630891123 ) ) ;
#53509 = AXIS2_PLACEMENT_3D ( 'NONE', #237031, #17966, #137907 ) ;
#53510 = EDGE_CURVE ( 'NONE', #193905, #102067, #213080, .T. ) ;
#53511 = PRODUCT_CONTEXT ( 'NONE', #182240, 'mechanical' ) ;
#53512 = CARTESIAN_POINT ( 'NONE',  ( -23.25000000000000000, 77.73670573947892137, -24.50568489690058627 ) ) ;
#53513 = CARTESIAN_POINT ( 'NONE',  ( -18.42609945526404402, 85.49999971050237946, -96.02374499427590138 ) ) ;
#53514 = ORIENTED_EDGE ( 'NONE', *, *, #64214, .F. ) ;
#53516 = ADVANCED_FACE ( 'NONE', ( #130721 ), #126878, .T. ) ;
#53515 = CARTESIAN_POINT ( 'NONE',  ( -18.50000000000000000, 76.00000000001213607, -136.5231074845242745 ) ) ;
#53517 = CARTESIAN_POINT ( 'NONE',  ( -21.05000000000000071, 1.115600667400684642E-11, -67.00000000000004263 ) ) ;
#53518 = EDGE_CURVE ( 'NONE', #142842, #152113, #125771, .T. ) ;
#53519 = EDGE_CURVE ( 'NONE', #182339, #117379, #84032, .T. ) ;
#53520 = FACE_OUTER_BOUND ( 'NONE', #160077, .T. ) ;
#53521 = ORIENTED_EDGE ( 'NONE', *, *, #248400, .T. ) ;
#53522 = ORIENTED_EDGE ( 'NONE', *, *, #158411, .F. ) ;
#53523 = EDGE_CURVE ( 'NONE', #176760, #92784, #185563, .T. ) ;
#53524 = FACE_OUTER_BOUND ( 'NONE', #87128, .T. ) ;
#53525 = DIRECTION ( 'NONE',  ( 1.000000000000000000, -1.875376730785737719E-16, -1.309568571767809260E-30 ) ) ;
#53526 = DIRECTION ( 'NONE',  ( -0.8660254037844653530, 0.000000000000000000, 0.4999999999999539257 ) ) ;
#53528 = CARTESIAN_POINT ( 'NONE',  ( 22.40736611211992368, -2.479040261793999722, -189.6172560698084624 ) ) ;
#53527 = DIRECTION ( 'NONE',  ( 0.000000000000000000, -0.7106264324241465813, 0.7035695228903324772 ) ) ;
#53529 = AXIS2_PLACEMENT_3D ( 'NONE', #154930, #191494, #71537 ) ;
#53531 = DIRECTION ( 'NONE',  ( 0.000000000000000000, 7.147358527629762208E-15, -1.000000000000000000 ) ) ;
#53530 = AXIS2_PLACEMENT_3D ( 'NONE', #205377, #26792, #245816 ) ;
#53532 = CARTESIAN_POINT ( 'NONE',  ( -20.00857864376270001, 9.250000000011157297, -155.2500000000000284 ) ) ;
#53533 = CARTESIAN_POINT ( 'NONE',  ( -20.94999999999999929, 74.26374286841466699, -124.9544551555068068 ) ) ;
#53534 = AXIS2_PLACEMENT_3D ( 'NONE', #140068, #137503, #158408 ) ;
#53535 = CARTESIAN_POINT ( 'NONE',  ( 20.94999999999997442, -1.263275465206102233, -175.4018646667464338 ) ) ;
#53536 = ORIENTED_EDGE ( 'NONE', *, *, #157329, .T. ) ;
#53537 = EDGE_CURVE ( 'NONE', #246153, #174077, #172472, .T. ) ;
#53539 = VERTEX_POINT ( 'NONE', #100236 ) ;
#53538 = DIRECTION ( 'NONE',  ( 0.000000000000000000, -0.000000000000000000, -1.000000000000000000 ) ) ;
#53540 = CARTESIAN_POINT ( 'NONE',  ( -18.39999999999999858, 11.75000000001113953, -143.2500000000000284 ) ) ;
#53541 = EDGE_CURVE ( 'NONE', #235775, #19042, #229837, .T. ) ;
#53542 = CARTESIAN_POINT ( 'NONE',  ( -20.54999999999999716, 67.23127455305835554, -235.8551265064784559 ) ) ;
#53544 = DIRECTION ( 'NONE',  ( 0.000000000000000000, -1.000000000000000000, 6.308085367188393199E-16 ) ) ;
#53543 = DIRECTION ( 'NONE',  ( 1.000000000000000000, -0.000000000000000000, 0.000000000000000000 ) ) ;
#53545 = AXIS2_PLACEMENT_3D ( 'NONE', #69535, #72099, #252000 ) ;
#53546 = ORIENTED_EDGE ( 'NONE', *, *, #246995, .F. ) ;
#53547 = FACE_OUTER_BOUND ( 'NONE', #121318, .T. ) ;
#53549 = EDGE_CURVE ( 'NONE', #192176, #120569, #113312, .T. ) ;
#53548 = CARTESIAN_POINT ( 'NONE',  ( 20.94999999999999929, 1.115650877919449413E-11, -196.8999999999999773 ) ) ;
#53550 = DIRECTION ( 'NONE',  ( -1.000000000000000000, 0.000000000000000000, 0.000000000000000000 ) ) ;
#53551 = CARTESIAN_POINT ( 'NONE',  ( 20.99999999999999645, 11.49509093111729108, -207.9633242410238552 ) ) ;
#53552 = EDGE_LOOP ( 'NONE', ( #58565, #1047, #93679, #249201 ) ) ;
#53553 = ORIENTED_EDGE ( 'NONE', *, *, #241499, .T. ) ;
#53554 = AXIS2_PLACEMENT_3D ( 'NONE', #186797, #207646, #45979 ) ;
#53555 = CIRCLE ( 'NONE', #7769, 0.1000000000000043771 ) ;
#53557 = VECTOR ( 'NONE', #86255, 1000.000000000000000 ) ;
#53556 = CARTESIAN_POINT ( 'NONE',  ( 21.07928932188134397, 69.67148334361836248, -69.62200263017875557 ) ) ;
#53558 = VERTEX_POINT ( 'NONE', #40338 ) ;
#53559 = FACE_OUTER_BOUND ( 'NONE', #118808, .T. ) ;
#53560 = ADVANCED_FACE ( 'NONE', ( #179826 ), #129862, .T. ) ;
#53562 = CARTESIAN_POINT ( 'NONE',  ( 23.24999999999999289, 6.550000000011156231, -54.85000000000000142 ) ) ;
#53561 = AXIS2_PLACEMENT_3D ( 'NONE', #96048, #59461, #15264 ) ;
#53563 = CARTESIAN_POINT ( 'NONE',  ( -21.10320863425827298, 65.53183290861515786, -242.0257079080814435 ) ) ;
#53564 = EDGE_CURVE ( 'NONE', #247, #70381, #35520, .T. ) ;
#53565 = ORIENTED_EDGE ( 'NONE', *, *, #245231, .T. ) ;
#53566 = DIRECTION ( 'NONE',  ( -2.827886303505249259E-16, -0.9667078373770114919, -0.2558827019434133931 ) ) ;
#53567 = EDGE_CURVE ( 'NONE', #9105, #87561, #1144, .T. ) ;
#53568 = DIRECTION ( 'NONE',  ( 0.7071067811865486830, 0.3338907855510734324, 0.6233112732207604090 ) ) ;
#53569 = EDGE_CURVE ( 'NONE', #208155, #18900, #167503, .T. ) ;
#53570 = CARTESIAN_POINT ( 'NONE',  ( -20.64999999999999858, 36.65892442174472876, -249.5511627012454596 ) ) ;
#53571 = CARTESIAN_POINT ( 'NONE',  ( -18.40000000000000213, 23.82801463864234037, -229.3483719500187306 ) ) ;
#53572 = CARTESIAN_POINT ( 'NONE',  ( 5.551115123125782702E-14, 64.35000000001120668, -3.123107484524795474 ) ) ;
#53574 = DIRECTION ( 'NONE',  ( 0.000000000000000000, -0.01283462868041947667, -0.9999176327611367654 ) ) ;
#53573 = DIRECTION ( 'NONE',  ( -1.000000000000000000, -0.000000000000000000, -0.000000000000000000 ) ) ;
#53575 = FACE_OUTER_BOUND ( 'NONE', #211931, .T. ) ;
#53576 = CIRCLE ( 'NONE', #141066, 0.1000000000000028644 ) ;
#53577 = ORIENTED_EDGE ( 'NONE', *, *, #13517, .F. ) ;
#53579 = CARTESIAN_POINT ( 'NONE',  ( -16.97048326478264713, 9.950000000011137047, -180.6411068801271256 ) ) ;
#53578 = DIRECTION ( 'NONE',  ( 1.186688945009010077E-16, 0.9651348961777157509, -0.2617529984165031243 ) ) ;
#53581 = ORIENTED_EDGE ( 'NONE', *, *, #185770, .T. ) ;
#53580 = AXIS2_PLACEMENT_3D ( 'NONE', #46933, #45672, #223009 ) ;
#53583 = ORIENTED_EDGE ( 'NONE', *, *, #30875, .T. ) ;
#53582 = DIRECTION ( 'NONE',  ( 0.000000000000000000, -0.9770955615653312831, -0.2128009952263614779 ) ) ;
#53584 = AXIS2_PLACEMENT_3D ( 'NONE', #86869, #26954, #106430 ) ;
#53585 = VERTEX_POINT ( 'NONE', #193280 ) ;
#53586 = CARTESIAN_POINT ( 'NONE',  ( -16.92570016628984320, 9.958788957751020021, -146.6206506700390264 ) ) ;
#53587 = CARTESIAN_POINT ( 'NONE',  ( 18.59999999999996945, 10.33248238083634440, -72.59484654391314962 ) ) ;
#53588 = FACE_OUTER_BOUND ( 'NONE', #212461, .T. ) ;
#53589 = CARTESIAN_POINT ( 'NONE',  ( 20.94999999999999929, 65.52661458509918191, -128.9444530202758301 ) ) ;
#53590 = VERTEX_POINT ( 'NONE', #160275 ) ;
#53591 = EDGE_CURVE ( 'NONE', #213303, #147103, #109014, .T. ) ;
#53592 =( NAMED_UNIT ( * ) PLANE_ANGLE_UNIT ( ) SI_UNIT ( $, .RADIAN. ) );
#53593 = VECTOR ( 'NONE', #169229, 1000.000000000000000 ) ;
#53594 = DIRECTION ( 'NONE',  ( -0.000000000000000000, -0.000000000000000000, 1.000000000000000000 ) ) ;
#53595 = VERTEX_POINT ( 'NONE', #121151 ) ;
#53596 = CARTESIAN_POINT ( 'NONE',  ( -23.25000000000000000, 65.31479887318495514, -236.7136839992847115 ) ) ;
#53597 = CARTESIAN_POINT ( 'NONE',  ( -23.25000000000000000, 76.00000000001156764, -56.74810748452433273 ) ) ;
#53598 = VECTOR ( 'NONE', #58115, 1000.000000000000000 ) ;
#53599 = ORIENTED_EDGE ( 'NONE', *, *, #84627, .F. ) ;
#53600 = VECTOR ( 'NONE', #105064, 1000.000000000000000 ) ;
#53601 = CARTESIAN_POINT ( 'NONE',  ( 23.14999999999999858, 76.00000000001246292, -172.0231074845243597 ) ) ;
#53602 = VECTOR ( 'NONE', #250219, 1000.000000000000000 ) ;
#53603 = VERTEX_POINT ( 'NONE', #75892 ) ;
#53604 = CARTESIAN_POINT ( 'NONE',  ( -23.24999999999999645, -9.599999999988845900, -140.7001893912220680 ) ) ;
#53606 = VERTEX_POINT ( 'NONE', #133302 ) ;
#53605 = VECTOR ( 'NONE', #171928, 1000.000000000000114 ) ;
#53607 = DIRECTION ( 'NONE',  ( -0.000000000000000000, -0.000000000000000000, -1.000000000000000000 ) ) ;
#53608 = EDGE_CURVE ( 'NONE', #127092, #139553, #239788, .T. ) ;
#53609 = FACE_OUTER_BOUND ( 'NONE', #237445, .T. ) ;
#53610 = CARTESIAN_POINT ( 'NONE',  ( -23.25000000000000000, 71.65000000001228386, -157.7731074845243882 ) ) ;
#53611 = SHAPE_REPRESENTATION ( 'Injection Molded Chain Links 7', ( #2425 ), #52661 ) ;
#53612 = DIRECTION ( 'NONE',  ( -3.265361837132813093E-16, -1.000000000000000000, 7.445645354460596589E-46 ) ) ;
#53613 = AXIS2_PLACEMENT_3D ( 'NONE', #216980, #138705, #55322 ) ;
#53614 = AXIS2_PLACEMENT_3D ( 'NONE', #79787, #199787, #220615 ) ;
#53615 = CARTESIAN_POINT ( 'NONE',  ( 21.56666275994539461, 76.00000000001200817, -109.9804758914176404 ) ) ;
#53617 = EDGE_CURVE ( 'NONE', #67383, #129669, #14662, .T. ) ;
#53616 = FACE_OUTER_BOUND ( 'NONE', #209617, .T. ) ;
#53618 = VERTEX_POINT ( 'NONE', #115018 ) ;
#53619 = FACE_OUTER_BOUND ( 'NONE', #136863, .T. ) ;
#53620 = VERTEX_POINT ( 'NONE', #52454 ) ;
#53622 = EDGE_LOOP ( 'NONE', ( #112919, #18869, #84247, #15302 ) ) ;
#53621 = PLANE ( 'NONE',  #232155 ) ;
#53623 = VECTOR ( 'NONE', #9181, 1000.000000000000114 ) ;
#53624 = VERTEX_POINT ( 'NONE', #220233 ) ;
#53625 = DIRECTION ( 'NONE',  ( -1.000000000000000000, 0.000000000000000000, 0.000000000000000000 ) ) ;
#53626 = CIRCLE ( 'NONE', #249264, 0.1999999999999987899 ) ;
#53627 = AXIS2_PLACEMENT_3D ( 'NONE', #173437, #252907, #134235 ) ;
#53628 = CARTESIAN_POINT ( 'NONE',  ( 20.94999999999999929, 0.6656436123793473270, -212.6810495496487476 ) ) ;
#53629 = TOROIDAL_SURFACE ( 'NONE', #161983, 2.100000000000002309, 0.1000000000000000056 ) ;
#53630 = FACE_OUTER_BOUND ( 'NONE', #143178, .T. ) ;
#53631 = CARTESIAN_POINT ( 'NONE',  ( 20.95420533658165141, 59.03391012955845696, -225.7910507217099507 ) ) ;
#53632 = VERTEX_POINT ( 'NONE', #41606 ) ;
#53634 = VERTEX_POINT ( 'NONE', #113730 ) ;
#53633 = CARTESIAN_POINT ( 'NONE',  ( 23.24999999999999289, 69.55000000001246008, -181.7731074845244166 ) ) ;
#53635 = AXIS2_PLACEMENT_3D ( 'NONE', #150280, #68157, #128141 ) ;
#53636 = CARTESIAN_POINT ( 'NONE',  ( 18.59999999999999787, 68.50594083727658301, -224.0235912779512830 ) ) ;
#53638 = ORIENTED_EDGE ( 'NONE', *, *, #68816, .F. ) ;
#53637 = CARTESIAN_POINT ( 'NONE',  ( -16.91776028072577631, 9.963400393640901243, -54.37502401470212732 ) ) ;
#53639 = PRODUCT_DEFINITION_SHAPE ( 'NONE', 'NONE',  #144083 ) ;
#53640 = EDGE_LOOP ( 'NONE', ( #31362, #21296, #93363, #192791 ) ) ;
#53641 = AXIS2_PLACEMENT_3D ( 'NONE', #7148, #243195, #106239 ) ;
#53642 = TOROIDAL_SURFACE ( 'NONE', #107604, 7.791421356237316687, 0.1000000000000000056 ) ;
#53643 = CARTESIAN_POINT ( 'NONE',  ( 20.95576188350343116, 11.98566591433073647, -206.1793010702357947 ) ) ;
#53644 = LINE ( 'NONE', #14541, #209674 ) ;
#53645 = ORIENTED_EDGE ( 'NONE', *, *, #99249, .F. ) ;
#53646 = DIRECTION ( 'NONE',  ( 1.000000000000000000, 0.000000000000000000, 0.000000000000000000 ) ) ;
#53647 = ORIENTED_EDGE ( 'NONE', *, *, #70388, .F. ) ;
#53648 = CARTESIAN_POINT ( 'NONE',  ( 21.00000000000000000, 30.37633856152204359, -235.1250019192171408 ) ) ;
#53649 = FACE_OUTER_BOUND ( 'NONE', #112603, .T. ) ;
#53650 = ORIENTED_EDGE ( 'NONE', *, *, #20855, .T. ) ;
#53651 = CARTESIAN_POINT ( 'NONE',  ( 21.05000000000000071, 76.00000000001188027, -98.92310748452429436 ) ) ;
#53652 = ADVANCED_FACE ( 'NONE', ( #181111 ), #214124, .F. ) ;
#53653 = CIRCLE ( 'NONE', #232728, 0.09999999999999911737 ) ;
#53654 = CIRCLE ( 'NONE', #120341, 0.09999999999999939493 ) ;
#53655 = DIRECTION ( 'NONE',  ( 1.000000000000000000, -0.000000000000000000, -0.000000000000000000 ) ) ;
#53656 = CIRCLE ( 'NONE', #70451, 0.1000000000000028644 ) ;
#53657 = ORIENTED_EDGE ( 'NONE', *, *, #87908, .F. ) ;
#53658 = ORIENTED_EDGE ( 'NONE', *, *, #230123, .F. ) ;
#53659 = LINE ( 'NONE', #194480, #223545 ) ;
#53660 = ORIENTED_EDGE ( 'NONE', *, *, #237096, .F. ) ;
#53661 = EDGE_CURVE ( 'NONE', #52417, #168004, #233694, .T. ) ;
#53662 = CYLINDRICAL_SURFACE ( 'NONE', #175436, 0.09999999999999939493 ) ;
#53663 = ORIENTED_EDGE ( 'NONE', *, *, #55725, .T. ) ;
#53665 = ORIENTED_EDGE ( 'NONE', *, *, #32491, .F. ) ;
#53664 = CYLINDRICAL_SURFACE ( 'NONE', #192814, 0.09999999999999939493 ) ;
#53666 = ADVANCED_FACE ( 'NONE', ( #211557 ), #15952, .F. ) ;
#53667 = ORIENTED_EDGE ( 'NONE', *, *, #73162, .T. ) ;
#53668 = CARTESIAN_POINT ( 'NONE',  ( -18.59999999999999787, 74.25000000001156764, -57.85359592662268824 ) ) ;
#53669 = AXIS2_PLACEMENT_3D ( 'NONE', #50897, #52193, #211290 ) ;
#53670 = ORIENTED_EDGE ( 'NONE', *, *, #167003, .T. ) ;
#53673 = VERTEX_POINT ( 'NONE', #192011 ) ;
#53672 = ORIENTED_EDGE ( 'NONE', *, *, #17484, .T. ) ;
#53671 = CARTESIAN_POINT ( 'NONE',  ( -23.15000000000000213, 87.48912529308852015, -173.1231074845242688 ) ) ;
#53674 = CIRCLE ( 'NONE', #182877, 0.09999999999999939493 ) ;
#53676 = EDGE_CURVE ( 'NONE', #135352, #199332, #13367, .T. ) ;
#53675 = ORIENTED_EDGE ( 'NONE', *, *, #16429, .F. ) ;
#53677 = DIRECTION ( 'NONE',  ( 1.000000000000000000, 0.000000000000000000, 0.000000000000000000 ) ) ;
#53678 = ORIENTED_EDGE ( 'NONE', *, *, #189097, .T. ) ;
#53679 = DIRECTION ( 'NONE',  ( 0.000000000000000000, 0.2617529984165035684, 0.9651348961777156399 ) ) ;
#53681 = EDGE_LOOP ( 'NONE', ( #18967, #113384, #27572, #45929 ) ) ;
#53680 = FACE_OUTER_BOUND ( 'NONE', #214907, .T. ) ;
#53682 = FACE_OUTER_BOUND ( 'NONE', #137433, .T. ) ;
#53683 = ORIENTED_EDGE ( 'NONE', *, *, #94418, .T. ) ;
#53684 = ADVANCED_FACE ( 'NONE', ( #127536 ), #165385, .F. ) ;
#53685 = VECTOR ( 'NONE', #201744, 1000.000000000000000 ) ;
#53686 = ORIENTED_EDGE ( 'NONE', *, *, #206835, .T. ) ;
#53687 = CARTESIAN_POINT ( 'NONE',  ( 20.94999999999999574, 87.65000000001266756, -200.5231074845242745 ) ) ;
#53688 = DIRECTION ( 'NONE',  ( 0.000000000000000000, 0.000000000000000000, 1.000000000000000000 ) ) ;
#53689 = EDGE_CURVE ( 'NONE', #152331, #150045, #75734, .T. ) ;
#53690 = VERTEX_POINT ( 'NONE', #166695 ) ;
#53692 = EDGE_LOOP ( 'NONE', ( #127680, #71389, #112219, #235474 ) ) ;
#53691 = CARTESIAN_POINT ( 'NONE',  ( 21.05000000000000071, 40.81706895266054147, -238.0716534883986526 ) ) ;
#53693 = CARTESIAN_POINT ( 'NONE',  ( 19.58285714285715073, 65.61500148966067059, -128.8934228171344216 ) ) ;
#53695 = ORIENTED_EDGE ( 'NONE', *, *, #87822, .F. ) ;
#53694 = ORIENTED_EDGE ( 'NONE', *, *, #91405, .F. ) ;
#53696 = EDGE_LOOP ( 'NONE', ( #84498, #20078, #169951, #165910 ) ) ;
#53697 = DIRECTION ( 'NONE',  ( -0.7071067811865487940, 0.7071067811865463515, -7.215498431451184074E-16 ) ) ;
#53698 = ORIENTED_EDGE ( 'NONE', *, *, #224087, .F. ) ;
#53699 = ORIENTED_EDGE ( 'NONE', *, *, #151633, .F. ) ;
#53700 = DIRECTION ( 'NONE',  ( 1.000000000000000000, 6.938893903907222067E-15, 0.000000000000000000 ) ) ;
#53701 = VERTEX_POINT ( 'NONE', #25883 ) ;
#53702 = CARTESIAN_POINT ( 'NONE',  ( -23.25000000000000000, 36.65892442174935439, -249.5511627012433848 ) ) ;
#53703 = DIRECTION ( 'NONE',  ( 0.000000000000000000, -7.116814260417693756E-15, 1.000000000000000000 ) ) ;
#53704 = EDGE_CURVE ( 'NONE', #65749, #140123, #142341, .T. ) ;
#53705 = ORIENTED_EDGE ( 'NONE', *, *, #199566, .T. ) ;
#53706 = ORIENTED_EDGE ( 'NONE', *, *, #12491, .T. ) ;
#53707 = CIRCLE ( 'NONE', #216188, 0.09999999999998712696 ) ;
#53708 = CARTESIAN_POINT ( 'NONE',  ( -18.50000000000000000, 63.93636616954134411, -213.0474835168086827 ) ) ;
#53709 = AXIS2_PLACEMENT_3D ( 'NONE', #39327, #19757, #120164 ) ;
#53710 = AXIS2_PLACEMENT_3D ( 'NONE', #10476, #189110, #232104 ) ;
#53711 = ORIENTED_EDGE ( 'NONE', *, *, #38950, .F. ) ;
#53712 = EDGE_CURVE ( 'NONE', #175328, #69740, #192425, .T. ) ;
#53713 = AXIS2_PLACEMENT_3D ( 'NONE', #163187, #199759, #160638 ) ;
#53714 = CARTESIAN_POINT ( 'NONE',  ( -23.15000000000000213, 64.35000000001268461, -203.5231074845244166 ) ) ;
#53715 = ORIENTED_EDGE ( 'NONE', *, *, #2673, .F. ) ;
#53716 = ORIENTED_EDGE ( 'NONE', *, *, #215560, .F. ) ;
#53717 = LINE ( 'NONE', #193241, #216884 ) ;
#53719 = ORIENTED_EDGE ( 'NONE', *, *, #220058, .T. ) ;
#53718 = CARTESIAN_POINT ( 'NONE',  ( 18.50000000000000355, 85.42145614550645405, -162.7811254005061414 ) ) ;
#53720 = DIRECTION ( 'NONE',  ( 1.000000000000000000, 0.000000000000000000, 0.000000000000000000 ) ) ;
#53721 = CYLINDRICAL_SURFACE ( 'NONE', #10403, 12.87499999999999822 ) ;
#53722 = CARTESIAN_POINT ( 'NONE',  ( 20.95566103547454517, 65.38175234906502453, -128.8912672915437554 ) ) ;
#53724 = EDGE_CURVE ( 'NONE', #28509, #132417, #196514, .T. ) ;
#53723 = DIRECTION ( 'NONE',  ( 1.000000000000000000, 0.000000000000000000, 0.000000000000000000 ) ) ;
#53725 = DIRECTION ( 'NONE',  ( 1.000000000000000000, -1.207181226542539700E-16, 2.694675058168174199E-16 ) ) ;
#53726 = CARTESIAN_POINT ( 'NONE',  ( 19.97071067811865674, 11.72071067812981759, -58.20857864376270641 ) ) ;
#53727 = B_SPLINE_CURVE_WITH_KNOTS ( 'NONE', 3,
 ( #221445, #256697, #119831, #1114, #19431, #201914, #157699, #158965, #136791, #76824, #59803, #216331, #37731, #156405, #218890, #199360, #80654, #160248, #239761, #203189, #126214, #67530, #127513, #63674, #244881, #147055 ),
 .UNSPECIFIED., .F., .F.,
 ( 4, 2, 2, 2, 2, 2, 2, 2, 2, 2, 2, 2, 4 ),
 ( 0.005476422646581355184, 0.006160811967703536639, 0.006845201288825718093, 0.007187395949386838311, 0.007529590609947957661, 0.007871785270509077878, 0.008213979931070198096, 0.008556174591631318313, 0.008898369252192438530, 0.009240563912753557013, 0.009582758573314677231, 0.01026714789443685868, 0.01095153721555904187 ),
 .UNSPECIFIED. ) ;
#53729 = DIRECTION ( 'NONE',  ( -1.000000000000000000, -0.000000000000000000, -0.000000000000000000 ) ) ;
#53728 = TOROIDAL_SURFACE ( 'NONE', #199502, 0.2000000000000000111, 0.1000000000000000056 ) ;
#53731 = CARTESIAN_POINT ( 'NONE',  ( 21.14999999999999858, 33.98486250090727623, -243.5821103306120108 ) ) ;
#53730 = VECTOR ( 'NONE', #5331, 1000.000000000000000 ) ;
#53732 = LINE ( 'NONE', #14631, #161448 ) ;
#53733 = VECTOR ( 'NONE', #67695, 1000.000000000000000 ) ;
#53734 = CARTESIAN_POINT ( 'NONE',  ( 22.39999999999999503, 76.00000000001222134, -148.1726782920690937 ) ) ;
#53735 = DIRECTION ( 'NONE',  ( -1.000000000000000000, 0.000000000000000000, 0.000000000000000000 ) ) ;
#53736 = EDGE_CURVE ( 'NONE', #24899, #27072, #9082, .T. ) ;
#53737 = ORIENTED_EDGE ( 'NONE', *, *, #28010, .T. ) ;
#53738 = EDGE_CURVE ( 'NONE', #59872, #85212, #79961, .T. ) ;
#53739 = AXIS2_PLACEMENT_3D ( 'NONE', #223389, #143856, #162174 ) ;
#53741 = EDGE_LOOP ( 'NONE', ( #224840, #255824, #127528, #220209, #226576, #180089 ) ) ;
#53740 = ORIENTED_EDGE ( 'NONE', *, *, #190902, .T. ) ;
#53742 = ORIENTED_EDGE ( 'NONE', *, *, #144632, .T. ) ;
#53743 = CARTESIAN_POINT ( 'NONE',  ( 21.08479644141222664, 75.94144555744861691, -209.8681461422562506 ) ) ;
#53744 = EDGE_CURVE ( 'NONE', #137789, #206482, #66285, .T. ) ;
#53745 = DIRECTION ( 'NONE',  ( 1.000000000000000000, 0.000000000000000000, 0.000000000000000000 ) ) ;
#53746 = DIRECTION ( 'NONE',  ( -1.000000000000000000, -0.000000000000000000, -0.000000000000000000 ) ) ;
#53747 = ORIENTED_EDGE ( 'NONE', *, *, #40381, .T. ) ;
#53748 = ORIENTED_EDGE ( 'NONE', *, *, #81527, .F. ) ;
#53749 = EDGE_CURVE ( 'NONE', #201739, #102509, #47987, .T. ) ;
#53750 = ADVANCED_FACE ( 'NONE', ( #4991 ), #71639, .T. ) ;
#53751 = DIRECTION ( 'NONE',  ( 0.000000000000000000, 0.4721928772776973204, 0.8814952561688629284 ) ) ;
#53752 = DIRECTION ( 'NONE',  ( 1.000000000000000000, -0.000000000000000000, -0.000000000000000000 ) ) ;
#53753 = CARTESIAN_POINT ( 'NONE',  ( 20.94999999999999929, 85.50000000001261924, -193.6291383618718385 ) ) ;
#53754 = ORIENTED_EDGE ( 'NONE', *, *, #45722, .F. ) ;
#53755 = VERTEX_POINT ( 'NONE', #145799 ) ;
#53756 = AXIS2_PLACEMENT_3D ( 'NONE', #7519, #205710, #162764 ) ;
#53757 = AXIS2_PLACEMENT_3D ( 'NONE', #40461, #237344, #176106 ) ;
#53758 = CARTESIAN_POINT ( 'NONE',  ( -17.11825945287482753, 65.95000000001260787, -190.7731074845244166 ) ) ;
#53759 = CARTESIAN_POINT ( 'NONE',  ( 18.54116936837188234, 8.873462500583581658, -245.4030598191407648 ) ) ;
#53760 = EDGE_CURVE ( 'NONE', #209946, #56169, #182388, .T. ) ;
#53761 = DIRECTION ( 'NONE',  ( 0.000000000000000000, 0.1455152366551700771, 0.9893560106964479628 ) ) ;
#53762 = VERTEX_POINT ( 'NONE', #126239 ) ;
#53763 = AXIS2_PLACEMENT_3D ( 'NONE', #55620, #189716, #30669 ) ;
#53764 = CARTESIAN_POINT ( 'NONE',  ( -21.59142135623730852, 44.62899621218267043, -237.3789420470153857 ) ) ;
#53765 = DIRECTION ( 'NONE',  ( 1.836970198721029934E-16, 1.000000000000000000, 6.982962677686266711E-15 ) ) ;
#53766 = EDGE_CURVE ( 'NONE', #4734, #162626, #186232, .T. ) ;
#53767 = CARTESIAN_POINT ( 'NONE',  ( 20.94999999999999574, 1.750000000011155743, -145.6695115579016715 ) ) ;
#53768 = ORIENTED_EDGE ( 'NONE', *, *, #193579, .T. ) ;
#53769 = DIRECTION ( 'NONE',  ( -1.000000000000000000, 0.000000000000000000, 0.000000000000000000 ) ) ;
#53770 = DIRECTION ( 'NONE',  ( 1.000000000000000000, 0.000000000000000000, 0.000000000000000000 ) ) ;
#53771 = CARTESIAN_POINT ( 'NONE',  ( -21.05000000000000071, 77.83534155023700407, -191.9679561919613491 ) ) ;
#53773 = DIRECTION ( 'NONE',  ( -0.7071067811865474617, 0.7071067811865474617, 0.000000000000000000 ) ) ;
#53772 = DIRECTION ( 'NONE',  ( -1.000000000000000000, -0.000000000000000000, -0.000000000000000000 ) ) ;
#53774 = DIRECTION ( 'NONE',  ( 1.000000000000000000, 0.000000000000000000, 0.000000000000000000 ) ) ;
#53775 = CARTESIAN_POINT ( 'NONE',  ( -16.93935632781549572, 9.984730499736244269, -121.3896607487103410 ) ) ;
#53776 = VECTOR ( 'NONE', #228915, 1000.000000000000000 ) ;
#53777 = CARTESIAN_POINT ( 'NONE',  ( -23.25000000000000000, 1.115600667400684642E-11, -100.5000000000000284 ) ) ;
#53778 = LINE ( 'NONE', #229850, #155871 ) ;
#53779 = CIRCLE ( 'NONE', #241237, 0.1000000000000028644 ) ;
#53780 = EDGE_LOOP ( 'NONE', ( #87284, #86024, #44508, #101748 ) ) ;
#53781 = VECTOR ( 'NONE', #104821, 999.9999999999998863 ) ;
#53782 = ORIENTED_EDGE ( 'NONE', *, *, #210505, .T. ) ;
#53783 = DIRECTION ( 'NONE',  ( 0.000000000000000000, -0.4791956752371546169, -0.8777080977375152360 ) ) ;
#53784 = DIRECTION ( 'NONE',  ( -0.000000000000000000, -0.8660254037844459241, -0.4999999999999873990 ) ) ;
#53785 = ADVANCED_FACE ( 'NONE', ( #64985, #84504 ), #184938, .F. ) ;
#53786 = ORIENTED_EDGE ( 'NONE', *, *, #56196, .F. ) ;
#53787 = EDGE_CURVE ( 'NONE', #155470, #13808, #34239, .T. ) ;
#53788 = DIRECTION ( 'NONE',  ( 0.000000000000000000, -0.000000000000000000, 1.000000000000000000 ) ) ;
#53789 = CIRCLE ( 'NONE', #8020, 0.1000000000000028644 ) ;
#53790 = AXIS2_PLACEMENT_3D ( 'NONE', #222861, #220315, #80768 ) ;
#53791 = VERTEX_POINT ( 'NONE', #242341 ) ;
#53792 = EDGE_CURVE ( 'NONE', #174796, #205763, #226617, .T. ) ;
#53793 = ORIENTED_EDGE ( 'NONE', *, *, #231711, .F. ) ;
#53794 = CARTESIAN_POINT ( 'NONE',  ( 21.04999999999907700, 75.94851711812999895, -109.3232873024352045 ) ) ;
#53795 = ORIENTED_EDGE ( 'NONE', *, *, #137043, .T. ) ;
#53796 = AXIS2_PLACEMENT_3D ( 'NONE', #169272, #153571, #233082 ) ;
#53797 = DIRECTION ( 'NONE',  ( 0.000000000000000000, -0.8700118002898359348, 0.4930308989875165082 ) ) ;
#53798 = VECTOR ( 'NONE', #151051, 1000.000000000000000 ) ;
#53799 = PRESENTATION_LAYER_ASSIGNMENT (  '', '', ( #253690 ) ) ;
#53800 = CARTESIAN_POINT ( 'NONE',  ( -16.81453563122429529, 30.14675705701981556, -234.7874993013237486 ) ) ;
#53801 = CARTESIAN_POINT ( 'NONE',  ( 18.49999999999999645, 1.115600667400684642E-11, -67.00000000000000000 ) ) ;
#53802 = AXIS2_PLACEMENT_3D ( 'NONE', #257975, #100205, #194233 ) ;
#53803 = CARTESIAN_POINT ( 'NONE',  ( -18.69999999999999929, -8.250000000000005329, 22.10000000000000142 ) ) ;
#53804 = CARTESIAN_POINT ( 'NONE',  ( 18.39999999999999503, 5.650000000011139001, -191.7499999999999716 ) ) ;
#53806 = ORIENTED_EDGE ( 'NONE', *, *, #70850, .T. ) ;
#53805 = CARTESIAN_POINT ( 'NONE',  ( 18.49999999999999289, 62.39550153362034735, -208.7959266050682459 ) ) ;
#53808 = CARTESIAN_POINT ( 'NONE',  ( -20.85000000000000142, 64.35000000001245724, -170.0231074845244166 ) ) ;
#53807 = CARTESIAN_POINT ( 'NONE',  ( -21.05000000000000071, 74.73821383144705521, -128.4366085209788366 ) ) ;
#53809 = AXIS2_PLACEMENT_3D ( 'NONE', #133272, #57564, #113704 ) ;
#53810 = CARTESIAN_POINT ( 'NONE',  ( -16.88460203013676875, 9.954759003246872240, -154.8658918095382546 ) ) ;
#53811 = DIRECTION ( 'NONE',  ( 0.000000000000000000, 0.000000000000000000, -1.000000000000000000 ) ) ;
#53812 = CYLINDRICAL_SURFACE ( 'NONE', #206259, 0.09999999999999939493 ) ;
#53813 = LINE ( 'NONE', #35562, #125257 ) ;
#53814 = VERTEX_POINT ( 'NONE', #241086 ) ;
#53815 = EDGE_CURVE ( 'NONE', #143381, #16002, #246578, .T. ) ;
#53816 = FILL_AREA_STYLE_COLOUR ( '', #48575 ) ;
#53817 = CARTESIAN_POINT ( 'NONE',  ( -20.94999999999999929, 6.846123162363745074, -137.7377262668498759 ) ) ;
#53818 = ORIENTED_EDGE ( 'NONE', *, *, #31748, .T. ) ;
#53819 = EDGE_CURVE ( 'NONE', #76080, #253923, #217348, .T. ) ;
#53820 = DIRECTION ( 'NONE',  ( -1.186688945009010077E-16, -1.000000000000000000, -7.759275652592821052E-15 ) ) ;
#53822 = ORIENTED_EDGE ( 'NONE', *, *, #117153, .T. ) ;
#53821 = VECTOR ( 'NONE', #66357, 1000.000000000000000 ) ;
#53823 = DIRECTION ( 'NONE',  ( 0.000000000000000000, 0.2128009952263601456, -0.9770955615653316162 ) ) ;
#53824 = DIRECTION ( 'NONE',  ( -0.000000000000000000, 0.000000000000000000, 1.000000000000000000 ) ) ;
#53825 = ADVANCED_FACE ( 'NONE', ( #248776 ), #208377, .F. ) ;
#53826 = DIRECTION ( 'NONE',  ( -0.000000000000000000, -0.2128009952263604232, 0.9770955615653316162 ) ) ;
#53827 = ORIENTED_EDGE ( 'NONE', *, *, #168303, .T. ) ;
#53828 = EDGE_LOOP ( 'NONE', ( #66511, #107201, #88079, #54882 ) ) ;
#53829 = VECTOR ( 'NONE', #226666, 1000.000000000000000 ) ;
#53830 = EDGE_CURVE ( 'NONE', #211751, #8256, #133939, .T. ) ;
#53831 = AXIS2_PLACEMENT_3D ( 'NONE', #63879, #65150, #142124 ) ;
#53832 = CARTESIAN_POINT ( 'NONE',  ( 21.03675099975492202, 8.875180032795963569, -112.8255421367780826 ) ) ;
#53833 = CARTESIAN_POINT ( 'NONE',  ( -20.94999999999999929, 61.95000000001234497, -164.5094124137634708 ) ) ;
#53834 = DIRECTION ( 'NONE',  ( -0.7071067811865389130, -0.6453109281988527179, -0.2890913453342165984 ) ) ;
#53835 = CARTESIAN_POINT ( 'NONE',  ( -18.43569575749026157, -9.519327731081284938, -140.9729763765592452 ) ) ;
#53836 = EDGE_CURVE ( 'NONE', #9803, #226695, #10161, .T. ) ;
#53837 = CIRCLE ( 'NONE', #199610, 0.2000000000000057288 ) ;
#53839 = CARTESIAN_POINT ( 'NONE',  ( -18.59999999999999787, 1.835341550235567887, -45.05515129256298223 ) ) ;
#53838 = DIRECTION ( 'NONE',  ( 0.000000000000000000, 0.7092521942343974484, 0.7049548389604062271 ) ) ;
#53840 = DIRECTION ( 'NONE',  ( 0.000000000000000000, -0.2128009952263485993, 0.9770955615653341697 ) ) ;
#53841 = CARTESIAN_POINT ( 'NONE',  ( -23.15000000000000213, 42.94327155031035659, -233.8606566173841372 ) ) ;
#53842 = FACE_OUTER_BOUND ( 'NONE', #48277, .T. ) ;
#53843 = VERTEX_POINT ( 'NONE', #128829 ) ;
#53844 = DIRECTION ( 'NONE',  ( 1.000000000000000000, 0.000000000000000000, 0.000000000000000000 ) ) ;
#53845 = AXIS2_PLACEMENT_3D ( 'NONE', #146146, #144857, #206133 ) ;
#53846 = EDGE_CURVE ( 'NONE', #229015, #58850, #25840, .T. ) ;
#53848 = ORIENTED_EDGE ( 'NONE', *, *, #37475, .F. ) ;
#53847 = CARTESIAN_POINT ( 'NONE',  ( -20.94999999999999929, 36.65892442174935439, -249.5511627012433848 ) ) ;
#53849 = PLANE ( 'NONE',  #205997 ) ;
#53851 = EDGE_CURVE ( 'NONE', #123645, #40222, #154858, .T. ) ;
#53850 = ADVANCED_FACE ( 'NONE', ( #191392 ), #92243, .T. ) ;
#53852 = DIRECTION ( 'NONE',  ( 0.000000000000000000, -0.8814952561688430555, 0.4721928772777346239 ) ) ;
#53854 = DIRECTION ( 'NONE',  ( -0.000000000000000000, -0.2617529984165031243, -0.9651348961777157509 ) ) ;
#53853 = DIRECTION ( 'NONE',  ( -1.000000000000000000, -0.000000000000000000, -0.000000000000000000 ) ) ;
#53856 = ORIENTED_EDGE ( 'NONE', *, *, #90651, .F. ) ;
#53855 = DIRECTION ( 'NONE',  ( -1.000000000000000000, 2.952720810173289112E-16, 2.061873921506763405E-30 ) ) ;
#53857 = CARTESIAN_POINT ( 'NONE',  ( 18.49999999999998934, 6.550000000011156231, -88.15000000000004832 ) ) ;
#53858 = DIRECTION ( 'NONE',  ( 2.715809747126117987E-16, 1.000000000000000000, 5.431619494252235382E-15 ) ) ;
#53859 = DIRECTION ( 'NONE',  ( 1.000000000000000000, -0.000000000000000000, -0.000000000000000000 ) ) ;
#53860 = CARTESIAN_POINT ( 'NONE',  ( 20.95000000000005613, 67.85000000001119247, -3.123107484524795474 ) ) ;
#53861 = CARTESIAN_POINT ( 'NONE',  ( -21.05000000000000071, 87.65000000001235492, -167.0231074845242460 ) ) ;
#53862 = ORIENTED_EDGE ( 'NONE', *, *, #240250, .T. ) ;
#53863 = CYLINDRICAL_SURFACE ( 'NONE', #101242, 0.5000000000000004441 ) ;
#53865 = ORIENTED_EDGE ( 'NONE', *, *, #47657, .F. ) ;
#53864 = AXIS2_PLACEMENT_3D ( 'NONE', #200410, #60885, #41364 ) ;
#53866 = AXIS2_PLACEMENT_3D ( 'NONE', #216602, #200890, #237454 ) ;
#53867 = CARTESIAN_POINT ( 'NONE',  ( -17.11825945287481332, 9.950000000011138823, -121.2500000000000426 ) ) ;
#53868 = VERTEX_POINT ( 'NONE', #109240 ) ;
#53869 = CARTESIAN_POINT ( 'NONE',  ( -20.64999999999999858, -8.999999999988844479, -191.5060308773475413 ) ) ;
#53870 = ADVANCED_FACE ( 'NONE', ( #152260 ), #175699, .T. ) ;
#53872 = ADVANCED_FACE ( 'NONE', ( #231782 ), #74017, .F. ) ;
#53871 = AXIS2_PLACEMENT_3D ( 'NONE', #155110, #76813, #256689 ) ;
#53873 = VERTEX_POINT ( 'NONE', #149690 ) ;
#53874 = CARTESIAN_POINT ( 'NONE',  ( -21.78635804494510708, 7.035661485164336426, -167.4009949344922745 ) ) ;
#53875 = DIRECTION ( 'NONE',  ( 0.000000000000000000, 0.8430646840892555005, 0.5378121776619452232 ) ) ;
#53876 = EDGE_CURVE ( 'NONE', #169303, #73622, #229213, .T. ) ;
#53877 = CARTESIAN_POINT ( 'NONE',  ( -13.40000000000000213, -11.65000000000000036, 15.00000000000000355 ) ) ;
#53878 = ORIENTED_EDGE ( 'NONE', *, *, #231976, .T. ) ;
#53879 = ADVANCED_FACE ( 'NONE', ( #33620 ), #50534, .F. ) ;
#53880 = CARTESIAN_POINT ( 'NONE',  ( -16.89155683852557743, 9.949999999999981526, -13.27737184954015603 ) ) ;
#53881 = EDGE_CURVE ( 'NONE', #213499, #160549, #130089, .T. ) ;
#53882 = CARTESIAN_POINT ( 'NONE',  ( 18.49999999999999645, -1.835341550213255957, -112.0551512925630107 ) ) ;
#53883 = DIRECTION ( 'NONE',  ( 0.000000000000000000, 0.4930308989875165082, 0.8700118002898358238 ) ) ;
#53885 = AXIS2_PLACEMENT_3D ( 'NONE', #254016, #75424, #233210 ) ;
#53884 = CARTESIAN_POINT ( 'NONE',  ( -21.05000000000000071, 76.00000000001213607, -136.5231074845242745 ) ) ;
#53886 = ORIENTED_EDGE ( 'NONE', *, *, #99272, .F. ) ;
#53887 = CARTESIAN_POINT ( 'NONE',  ( -18.43459694179558639, 85.49421012501012740, -129.9061022818631841 ) ) ;
#53888 = ORIENTED_EDGE ( 'NONE', *, *, #242921, .F. ) ;
#53890 = EDGE_LOOP ( 'NONE', ( #64918, #207864, #218478, #142595 ) ) ;
#53889 = CARTESIAN_POINT ( 'NONE',  ( 21.10710606213542206, 67.22310597611866001, -90.78211095812494591 ) ) ;
#53891 = ORIENTED_EDGE ( 'NONE', *, *, #43177, .F. ) ;
#53892 = CARTESIAN_POINT ( 'NONE',  ( -21.65000000000000213, 7.250000000011138646, -79.65000000000004832 ) ) ;
#53893 = DIRECTION ( 'NONE',  ( 1.000000000000000000, 0.000000000000000000, -0.000000000000000000 ) ) ;
#53894 = CARTESIAN_POINT ( 'NONE',  ( -22.50875500270927532, 76.10085791378634212, -81.27267461192221276 ) ) ;
#53895 = ORIENTED_EDGE ( 'NONE', *, *, #120942, .T. ) ;
#53896 = EDGE_CURVE ( 'NONE', #161970, #105589, #33069, .T. ) ;
#53897 = LINE ( 'NONE', #171331, #59533 ) ;
#53898 = B_SPLINE_CURVE_WITH_KNOTS ( 'NONE', 3,
 ( #205639, #126101, #203082, #6155 ),
 .UNSPECIFIED., .F., .F.,
 ( 4, 4 ),
 ( 0.000000000000000000, 0.0002118541922231917721 ),
 .UNSPECIFIED. ) ;
#53899 = DIRECTION ( 'NONE',  ( 1.000000000000000000, -6.239415780002328221E-16, -5.674754385112861898E-16 ) ) ;
#53900 = VERTEX_POINT ( 'NONE', #98628 ) ;
#53902 = ORIENTED_EDGE ( 'NONE', *, *, #109131, .T. ) ;
#53901 = CARTESIAN_POINT ( 'NONE',  ( -23.15000000000000213, 11.65000000000000036, -12.15000000000000036 ) ) ;
#53903 = CARTESIAN_POINT ( 'NONE',  ( -21.05000000000000071, -12.41227409413852811, -198.0999999999999659 ) ) ;
#53904 = CARTESIAN_POINT ( 'NONE',  ( -20.54999999999999716, 74.00000000001229239, -156.7984855617622770 ) ) ;
#53905 = EDGE_CURVE ( 'NONE', #227863, #148073, #92638, .T. ) ;
#53906 = CIRCLE ( 'NONE', #241352, 11.80000000000000426 ) ;
#53907 = AXIS2_PLACEMENT_3D ( 'NONE', #241064, #256707, #201926 ) ;
#53909 = AXIS2_PLACEMENT_3D ( 'NONE', #113113, #207086, #229221 ) ;
#53908 = LINE ( 'NONE', #124775, #47324 ) ;
#53910 = ORIENTED_EDGE ( 'NONE', *, *, #100042, .F. ) ;
#53911 = LINE ( 'NONE', #51307, #239577 ) ;
#53912 = CARTESIAN_POINT ( 'NONE',  ( -20.85882249326303040, 18.41524492703433324, -237.0006385043383546 ) ) ;
#53913 = EDGE_LOOP ( 'NONE', ( #215632, #220479, #205592, #28792 ) ) ;
#53914 = DIRECTION ( 'NONE',  ( 1.000000000000000000, 0.000000000000000000, 0.000000000000000000 ) ) ;
#53915 = EDGE_CURVE ( 'NONE', #187671, #224622, #172990, .T. ) ;
#53916 = CARTESIAN_POINT ( 'NONE',  ( -22.50875500270928242, -2.598867398075993318, -189.5410127739348809 ) ) ;
#53917 = DIRECTION ( 'NONE',  ( -0.000000000000000000, -0.8814952561688430555, 0.4721928772777346239 ) ) ;
#53918 = CIRCLE ( 'NONE', #149227, 11.64999999999999325 ) ;
#53919 = AXIS2_PLACEMENT_3D ( 'NONE', #11490, #253919, #75329 ) ;
#53920 = AXIS2_PLACEMENT_3D ( 'NONE', #8697, #223869, #146897 ) ;
#53921 = TOROIDAL_SURFACE ( 'NONE', #174608, 7.800000000000000711, 0.1000000000000000056 ) ;
#53922 = ORIENTED_EDGE ( 'NONE', *, *, #134453, .F. ) ;
#53923 = CARTESIAN_POINT ( 'NONE',  ( 23.14999999999999858, 71.22429906543236200, -81.37187558857031888 ) ) ;
#53924 = EDGE_LOOP ( 'NONE', ( #247509, #191959, #180193 ) ) ;
#53925 = FACE_OUTER_BOUND ( 'NONE', #196975, .T. ) ;
#53926 = CARTESIAN_POINT ( 'NONE',  ( 20.94999999999999929, 7.021664781911246322, -137.8335654018973457 ) ) ;
#53929 = EDGE_LOOP ( 'NONE', ( #231988, #15122, #126695, #10515 ) ) ;
#53928 = DIRECTION ( 'NONE',  ( 0.000000000000000000, 0.000000000000000000, -1.000000000000000000 ) ) ;
#53927 =( BOUNDED_SURFACE ( )  B_SPLINE_SURFACE ( 3, 2, ( 
 ( #48400, #105784, #185355 ),
 ( #217407, #37520, #161320 ),
 ( #257778, #100009, #81726 ),
 ( #58322, #97446, #137868 ),
 ( #76625, #118340, #62208 ),
 ( #117049, #238262, #197853 ) ),
 .UNSPECIFIED., .F., .F., .F. ) 
 B_SPLINE_SURFACE_WITH_KNOTS ( ( 4, 2, 4 ),
 ( 3, 3 ),
 ( 6.719893378900011955E-05, 0.0002757154632485553998, 0.0004842319927081106530 ),
 ( 0.000000000000000000, 1.000000000000000000 ),
 .UNSPECIFIED. ) 
 GEOMETRIC_REPRESENTATION_ITEM ( )  RATIONAL_B_SPLINE_SURFACE ( (
 ( 1.000000000000000000, 0.7250110520820690629, 1.000000000000000000),
 ( 1.000000000000000000, 0.7277932058357374778, 1.000000000000000000),
 ( 1.000000000000000000, 0.7278452872618936809, 1.000000000000000000),
 ( 1.000000000000000000, 0.7221445671547916945, 1.000000000000000000),
 ( 1.000000000000000000, 0.7163662143780868963, 1.000000000000000000),
 ( 1.000000000000000000, 0.7071067811865475727, 1.000000000000000000) ) ) 
 REPRESENTATION_ITEM ( '' )  SURFACE ( )  );
#53930 = DIRECTION ( 'NONE',  ( -1.000000000000000000, -1.040834085586090568E-13, 0.000000000000000000 ) ) ;
#53931 = CARTESIAN_POINT ( 'NONE',  ( 21.10642757222115407, 65.27684371085297244, -57.28240996073919433 ) ) ;
#53932 = FACE_OUTER_BOUND ( 'NONE', #227693, .T. ) ;
#53933 = CARTESIAN_POINT ( 'NONE',  ( -16.97048361161166952, 9.949999999999981526, -20.35888434443039685 ) ) ;
#53934 = DIRECTION ( 'NONE',  ( -1.000000000000000000, -0.000000000000000000, -0.000000000000000000 ) ) ;
#53935 = DIRECTION ( 'NONE',  ( -1.000000000000000000, 0.000000000000000000, 0.000000000000000000 ) ) ;
#53937 = ORIENTED_EDGE ( 'NONE', *, *, #26461, .F. ) ;
#53936 = DIRECTION ( 'NONE',  ( 1.000000000000000000, 0.000000000000000000, 0.000000000000000000 ) ) ;
#53938 = VECTOR ( 'NONE', #92371, 1000.000000000000000 ) ;
#53939 = SPHERICAL_SURFACE ( 'NONE', #176714, 0.1000000000000000056 ) ;
#53940 = VECTOR ( 'NONE', #120194, 1000.000000000000000 ) ;
#53941 = DIRECTION ( 'NONE',  ( -6.938893903907209445E-14, -0.9999176327611370985, -0.01283462868040260302 ) ) ;
#53942 = DIRECTION ( 'NONE',  ( -0.000000000000000000, 0.9770955615653313941, 0.2128009952263603954 ) ) ;
#53943 = ORIENTED_EDGE ( 'NONE', *, *, #88253, .T. ) ;
#53944 = CARTESIAN_POINT ( 'NONE',  ( -21.05000000000000071, 68.51069317435826633, -224.1259271199053842 ) ) ;
#53945 = ADVANCED_FACE ( 'NONE', ( #214764 ), #159956, .F. ) ;
#53946 = CARTESIAN_POINT ( 'NONE',  ( 22.39999999999999503, 0.1000000000111554016, -59.20922040162665922 ) ) ;
#53947 = DIRECTION ( 'NONE',  ( 0.000000000000000000, 0.000000000000000000, 1.000000000000000000 ) ) ;
#53948 = VERTEX_POINT ( 'NONE', #79086 ) ;
#53949 = TOROIDAL_SURFACE ( 'NONE', #253852, 12.77499999999999858, 0.1000000000000000056 ) ;
#53950 = DIRECTION ( 'NONE',  ( 0.000000000000000000, 0.2128009952263601734, -0.9770955615653316162 ) ) ;
#53951 = TOROIDAL_SURFACE ( 'NONE', #249777, 7.800000000000000711, 0.1000000000000000056 ) ;
#53952 = CARTESIAN_POINT ( 'NONE',  ( -16.93230518875208190, 10.00075036143099716, -79.57577834810155082 ) ) ;
#53953 = ORIENTED_EDGE ( 'NONE', *, *, #170422, .F. ) ;
#53954 = CARTESIAN_POINT ( 'NONE',  ( -18.36973785203556275, 11.47550320049537476, -124.7500000000000284 ) ) ;
#53955 = AXIS2_PLACEMENT_3D ( 'NONE', #198754, #197468, #114078 ) ;
#53956 = ORIENTED_EDGE ( 'NONE', *, *, #64241, .F. ) ;
#53957 = ADVANCED_FACE ( 'NONE', ( #37438 ), #158682, .F. ) ;
#53959 = ORIENTED_EDGE ( 'NONE', *, *, #223491, .F. ) ;
#53958 = CARTESIAN_POINT ( 'NONE',  ( 21.05000000000000071, 6.496686585778244982, -134.0146561185100325 ) ) ;
#53960 = CIRCLE ( 'NONE', #49866, 0.1000000000000028644 ) ;
#53961 = CIRCLE ( 'NONE', #141270, 7.720710678118663850 ) ;
#53963 = EDGE_CURVE ( 'NONE', #73323, #187889, #139278, .T. ) ;
#53962 = DIRECTION ( 'NONE',  ( -0.000000000000000000, -0.000000000000000000, 1.000000000000000000 ) ) ;
#53964 = ORIENTED_EDGE ( 'NONE', *, *, #133355, .F. ) ;
#53965 = CARTESIAN_POINT ( 'NONE',  ( -21.14999999999999858, 64.35000000001195986, -102.9231074845243938 ) ) ;
#53966 = VERTEX_POINT ( 'NONE', #56944 ) ;
#53968 = ORIENTED_EDGE ( 'NONE', *, *, #20589, .F. ) ;
#53967 = ORIENTED_EDGE ( 'NONE', *, *, #239650, .T. ) ;
#53969 = DIRECTION ( 'NONE',  ( -0.000000000000000000, 0.8660254037844411501, 0.4999999999999956701 ) ) ;
#53971 = ORIENTED_EDGE ( 'NONE', *, *, #11065, .F. ) ;
#53970 = CARTESIAN_POINT ( 'NONE',  ( 21.05000000000000071, 10.72371710471867701, -146.1611902941274650 ) ) ;
#53972 = CARTESIAN_POINT ( 'NONE',  ( -21.05000000000000071, 0.6656436123793491033, -212.6810495496487476 ) ) ;
#53973 = VERTEX_POINT ( 'NONE', #195240 ) ;
#53974 = VECTOR ( 'NONE', #42547, 1000.000000000000000 ) ;
#53975 = AXIS2_PLACEMENT_3D ( 'NONE', #141031, #41944, #200999 ) ;
#53976 = AXIS2_PLACEMENT_3D ( 'NONE', #29411, #187183, #108900 ) ;
#53977 = CIRCLE ( 'NONE', #191576, 0.09999999999999609201 ) ;
#53978 = EDGE_CURVE ( 'NONE', #167923, #250282, #242487, .T. ) ;
#53979 = ADVANCED_FACE ( 'NONE', ( #15309 ), #239478, .T. ) ;
#53980 = ORIENTED_EDGE ( 'NONE', *, *, #70326, .F. ) ;
#53982 = VECTOR ( 'NONE', #56915, 1000.000000000000227 ) ;
#53981 = DIRECTION ( 'NONE',  ( -0.7071067811865487940, 0.7071067811865463515, -7.215498431451184074E-16 ) ) ;
#53983 = FACE_OUTER_BOUND ( 'NONE', #63343, .T. ) ;
#53984 = DIRECTION ( 'NONE',  ( 1.000000000000000000, -0.000000000000000000, -0.000000000000000000 ) ) ;
#53985 = ORIENTED_EDGE ( 'NONE', *, *, #70947, .T. ) ;
#53986 = EDGE_CURVE ( 'NONE', #186652, #79572, #96714, .T. ) ;
#53987 = CARTESIAN_POINT ( 'NONE',  ( -23.24999999999999645, -9.599999999988845900, -174.1001893912220737 ) ) ;
#53988 = CARTESIAN_POINT ( 'NONE',  ( -16.92507428761702926, 9.950000000011137047, -146.7133974596215751 ) ) ;
#53989 = CARTESIAN_POINT ( 'NONE',  ( 20.94999999999999929, 5.900000000011162093, -190.7809002353436085 ) ) ;
#53990 = ORIENTED_EDGE ( 'NONE', *, *, #244008, .T. ) ;
#53991 = CARTESIAN_POINT ( 'NONE',  ( -22.16821283564876666, 59.93584560259382243, -233.8765425695785893 ) ) ;
#53992 = CARTESIAN_POINT ( 'NONE',  ( -18.41817142474017999, 37.99506873957891884, -261.0425698592600270 ) ) ;
#53993 = DIRECTION ( 'NONE',  ( 1.000000000000000000, 0.000000000000000000, 0.000000000000000000 ) ) ;
#53994 = EDGE_CURVE ( 'NONE', #39025, #168716, #167692, .T. ) ;
#53995 = ORIENTED_EDGE ( 'NONE', *, *, #70372, .T. ) ;
#53996 = DIRECTION ( 'NONE',  ( 1.000000000000000000, 0.000000000000000000, 0.000000000000000000 ) ) ;
#53997 = VERTEX_POINT ( 'NONE', #99925 ) ;
#53999 = AXIS2_PLACEMENT_3D ( 'NONE', #183123, #107419, #245654 ) ;
#53998 = CARTESIAN_POINT ( 'NONE',  ( -18.49719636458527106, -7.725155196047287731, -209.9198384750837931 ) ) ;
#54000 = ORIENTED_EDGE ( 'NONE', *, *, #165653, .F. ) ;
#54001 = ADVANCED_FACE ( 'NONE', ( #822 ), #254897, .F. ) ;
#54002 = CARTESIAN_POINT ( 'NONE',  ( 11.60000000000000142, -11.65000000000000036, 12.40000000000000391 ) ) ;
#54003 = ORIENTED_EDGE ( 'NONE', *, *, #146154, .T. ) ;
#54004 = ORIENTED_EDGE ( 'NONE', *, *, #141783, .F. ) ;
#54005 = CARTESIAN_POINT ( 'NONE',  ( -18.50000000000000000, 43.24695311518262741, -245.0026972281755775 ) ) ;
#54006 = CARTESIAN_POINT ( 'NONE',  ( -16.94445028196807002, 9.992063609708893068, -188.3926698215815350 ) ) ;
#54007 = VERTEX_POINT ( 'NONE', #80361 ) ;
#54008 = ADVANCED_FACE ( 'NONE', ( #137782 ), #200989, .T. ) ;
#54009 = ORIENTED_EDGE ( 'NONE', *, *, #31314, .F. ) ;
#54010 = CARTESIAN_POINT ( 'NONE',  ( 21.14999999999999503, 87.75000000001246292, -181.7731074845242745 ) ) ;
#54011 = CIRCLE ( 'NONE', #29119, 0.09999999999998898659 ) ;
#54012 = EDGE_CURVE ( 'NONE', #237605, #34456, #88532, .T. ) ;
#54013 = ORIENTED_EDGE ( 'NONE', *, *, #159332, .F. ) ;
#54014 = VECTOR ( 'NONE', #28256, 1000.000000000000000 ) ;
#54015 = ORIENTED_EDGE ( 'NONE', *, *, #63669, .T. ) ;
#54016 = CIRCLE ( 'NONE', #8067, 0.4999999999999944489 ) ;
#54017 = DIRECTION ( 'NONE',  ( -1.000000000000000000, 0.000000000000000000, 0.000000000000000000 ) ) ;
#54018 =( BOUNDED_SURFACE ( )  B_SPLINE_SURFACE ( 3, 2, ( 
 ( #46471, #68629, #43921 ),
 ( #127311, #85572, #47752 ),
 ( #124752, #206849, #84272 ),
 ( #183443, #145578, #6066 ),
 ( #144275, #25649, #223823 ),
 ( #126015, #105132, #29527 ),
 ( #109015, #4766, #204263 ),
 ( #24382, #28245, #205545 ) ),
 .UNSPECIFIED., .F., .F., .F. ) 
 B_SPLINE_SURFACE_WITH_KNOTS ( ( 4, 2, 2, 4 ),
 ( 3, 3 ),
 ( 0.0001723339234021441008, 0.0002782939632049931823, 0.0003842540030078422908, 0.0005961740826135404538 ),
 ( 0.000000000000000000, 1.000000000000000000 ),
 .UNSPECIFIED. ) 
 GEOMETRIC_REPRESENTATION_ITEM ( )  RATIONAL_B_SPLINE_SURFACE ( (
 ( 1.000000000000000000, 0.9504532311154585411, 1.000000000000000000),
 ( 1.000000000000000000, 0.9506023220709699517, 1.000000000000000000),
 ( 1.000000000000000000, 0.9395774818181729104, 1.000000000000000000),
 ( 1.000000000000000000, 0.9079328464647203889, 1.000000000000000000),
 ( 1.000000000000000000, 0.8875702416204832579, 1.000000000000000000),
 ( 1.000000000000000000, 0.8205919608041678526, 1.000000000000000000),
 ( 1.000000000000000000, 0.7666842783597330735, 1.000000000000000000),
 ( 1.000000000000000000, 0.7071067811864603092, 1.000000000000000000) ) ) 
 REPRESENTATION_ITEM ( '' )  SURFACE ( )  );
#54019 = EDGE_CURVE ( 'NONE', #153767, #118994, #88338, .T. ) ;
#54020 = DIRECTION ( 'NONE',  ( 0.000000000000000000, 0.000000000000000000, -1.000000000000000000 ) ) ;
#54021 = DIRECTION ( 'NONE',  ( 0.000000000000000000, -0.9875055080513754913, 0.1575844902526733482 ) ) ;
#54023 = VERTEX_POINT ( 'NONE', #142908 ) ;
#54022 = DIRECTION ( 'NONE',  ( 0.000000000000000000, 0.000000000000000000, -1.000000000000000000 ) ) ;
#54024 = CARTESIAN_POINT ( 'NONE',  ( 23.14999999999999858, 4.775700934590591196, -88.65123189595408348 ) ) ;
#54025 = AXIS2_PLACEMENT_3D ( 'NONE', #185979, #167729, #225079 ) ;
#54026 = CARTESIAN_POINT ( 'NONE',  ( -22.59999985501179154, 12.61921324905064701, -223.3442716046673411 ) ) ;
#54027 = DIRECTION ( 'NONE',  ( 1.000000000000000000, -1.875376730785737719E-16, -1.309568571767809260E-30 ) ) ;
#54028 = AXIS2_PLACEMENT_3D ( 'NONE', #33860, #92493, #96327 ) ;
#54030 = CARTESIAN_POINT ( 'NONE',  ( -40.23850191057533010, 65.19115966511134275, -30.02310748452479316 ) ) ;
#54029 = CARTESIAN_POINT ( 'NONE',  ( 18.49999999999999645, 45.93315328338058379, -256.6017782078560003 ) ) ;
#54031 = CARTESIAN_POINT ( 'NONE',  ( 20.95262331984769588, 10.50415726280101403, -108.0608883295933396 ) ) ;
#54032 = CARTESIAN_POINT ( 'NONE',  ( 18.49999999999999645, 77.86671491006991630, -191.7704322382423356 ) ) ;
#54033 = FACE_OUTER_BOUND ( 'NONE', #42176, .T. ) ;
#54034 = DIRECTION ( 'NONE',  ( 0.000000000000000000, 0.000000000000000000, 1.000000000000000000 ) ) ;
#54035 = CIRCLE ( 'NONE', #116419, 11.74999999999999645 ) ;
#54036 = VERTEX_POINT ( 'NONE', #84179 ) ;
#54037 = EDGE_CURVE ( 'NONE', #233320, #27558, #21924, .T. ) ;
#54039 = ORIENTED_EDGE ( 'NONE', *, *, #189030, .F. ) ;
#54038 = DIRECTION ( 'NONE',  ( -0.000000000000000000, 6.982962677686266711E-15, -1.000000000000000000 ) ) ;
#54040 = ADVANCED_FACE ( 'NONE', ( #7261 ), #64675, .F. ) ;
#54041 = PLANE ( 'NONE',  #165142 ) ;
#54042 = CARTESIAN_POINT ( 'NONE',  ( 20.94999999999999929, 69.35000000001180354, -81.77310748452435973 ) ) ;
#54043 = ORIENTED_EDGE ( 'NONE', *, *, #244413, .F. ) ;
#54044 = EDGE_CURVE ( 'NONE', #190824, #77502, #165066, .T. ) ;
#54045 = EDGE_CURVE ( 'NONE', #112163, #120222, #184222, .T. ) ;
#54047 = DIRECTION ( 'NONE',  ( 0.000000000000000000, -7.056502275159890832E-15, 1.000000000000000000 ) ) ;
#54046 = CIRCLE ( 'NONE', #120718, 0.09999999999999693856 ) ;
#54048 = ADVANCED_FACE ( 'NONE', ( #24294 ), #166386, .F. ) ;
#54049 = CARTESIAN_POINT ( 'NONE',  ( 21.00000000000000000, 66.25000000001179501, -81.87310748452438247 ) ) ;
#54050 = EDGE_CURVE ( 'NONE', #58384, #39320, #42580, .T. ) ;
#54051 = ORIENTED_EDGE ( 'NONE', *, *, #155840, .T. ) ;
#54052 = FACE_OUTER_BOUND ( 'NONE', #188605, .T. ) ;
#54053 = CARTESIAN_POINT ( 'NONE',  ( -21.44999999999999929, 68.85000000001180354, -81.77310748452435973 ) ) ;
#54054 = EDGE_CURVE ( 'NONE', #89222, #95759, #130047, .T. ) ;
#54055 = DIRECTION ( 'NONE',  ( 0.000000000000000000, -1.776356839400308446E-15, -1.000000000000000000 ) ) ;
#54057 = ORIENTED_EDGE ( 'NONE', *, *, #159555, .F. ) ;
#54056 = CARTESIAN_POINT ( 'NONE',  ( -20.54999999999999716, 25.94586868676353575, -241.5435999122864530 ) ) ;
#54058 = CARTESIAN_POINT ( 'NONE',  ( -18.69999999999999929, 6.644425182197218227, 9.641788261573355001 ) ) ;
#54060 = VERTEX_POINT ( 'NONE', #86790 ) ;
#54059 = DIRECTION ( 'NONE',  ( 0.000000000000000000, 0.2617529984165031243, 0.9651348961777157509 ) ) ;
#54061 = CARTESIAN_POINT ( 'NONE',  ( -21.05000000000000071, 10.23283250993384641, -228.1194284103923451 ) ) ;
#54062 = DIRECTION ( 'NONE',  ( 0.000000000000000000, 0.2617529984165152257, 0.9651348961777124202 ) ) ;
#54063 = CYLINDRICAL_SURFACE ( 'NONE', #40829, 0.09999999999999939493 ) ;
#54064 = DIRECTION ( 'NONE',  ( 0.000000000000000000, 0.4930308989875313852, 0.8700118002898274971 ) ) ;
#54065 = CIRCLE ( 'NONE', #199852, 2.700000000000001066 ) ;
#54068 = CARTESIAN_POINT ( 'NONE',  ( 21.13461538461538680, 8.885417037985613220, -179.7500000000000000 ) ) ;
#54067 = AXIS2_PLACEMENT_3D ( 'NONE', #157039, #34530, #17501 ) ;
#54066 = CARTESIAN_POINT ( 'NONE',  ( -16.87401514999227814, 9.950000000011137047, -154.7800179925321231 ) ) ;
#54069 = DIRECTION ( 'NONE',  ( 1.000000000000000000, 0.000000000000000000, 0.000000000000000000 ) ) ;
#54070 = AXIS2_PLACEMENT_3D ( 'NONE', #188251, #89142, #168745 ) ;
#54071 = AXIS2_PLACEMENT_3D ( 'NONE', #8575, #89370, #205473 ) ;
#54072 = CARTESIAN_POINT ( 'NONE',  ( -21.44999999999999929, 68.75000000001260503, -191.1731074845243938 ) ) ;
#54073 = DIRECTION ( 'NONE',  ( 1.000000000000000000, 3.265361837132813093E-16, -0.000000000000000000 ) ) ;
#54074 = DIRECTION ( 'NONE',  ( 0.000000000000000000, -0.000000000000000000, 1.000000000000000000 ) ) ;
#54075 = CARTESIAN_POINT ( 'NONE',  ( -18.59999999999999787, 85.50000000001161027, -61.42310748452425884 ) ) ;
#54076 = ORIENTED_EDGE ( 'NONE', *, *, #215702, .F. ) ;
#54077 = EDGE_CURVE ( 'NONE', #141361, #59365, #75904, .T. ) ;
#54078 = CARTESIAN_POINT ( 'NONE',  ( -18.37013991200266005, 11.49974761622312691, -76.20697698948293919 ) ) ;
#54079 = VECTOR ( 'NONE', #42614, 1000.000000000000000 ) ;
#54080 = ORIENTED_EDGE ( 'NONE', *, *, #115647, .T. ) ;
#54081 = VERTEX_POINT ( 'NONE', #205462 ) ;
#54082 = DIRECTION ( 'NONE',  ( 1.000000000000000000, 0.000000000000000000, 0.000000000000000000 ) ) ;
#54083 = DIRECTION ( 'NONE',  ( 1.000000000000000000, 0.000000000000000000, 0.000000000000000000 ) ) ;
#54084 = EDGE_CURVE ( 'NONE', #72361, #197038, #246758, .T. ) ;
#54085 = ORIENTED_EDGE ( 'NONE', *, *, #140784, .T. ) ;
#54086 = ADVANCED_FACE ( 'NONE', ( #144198 ), #185909, .F. ) ;
#54087 = ORIENTED_EDGE ( 'NONE', *, *, #11570, .T. ) ;
#54088 = AXIS2_PLACEMENT_3D ( 'NONE', #46870, #87280, #248956 ) ;
#54089 = CARTESIAN_POINT ( 'NONE',  ( -21.05000000000000071, 30.73075574124491283, -252.3164853687435709 ) ) ;
#54090 = ORIENTED_EDGE ( 'NONE', *, *, #196586, .T. ) ;
#54091 = VECTOR ( 'NONE', #81645, 1000.000000000000000 ) ;
#54092 = ORIENTED_EDGE ( 'NONE', *, *, #223839, .T. ) ;
#54093 = CARTESIAN_POINT ( 'NONE',  ( -23.15000000000000213, 86.43238724539048690, -209.5644480942280836 ) ) ;
#54094 = CARTESIAN_POINT ( 'NONE',  ( -16.78569801330232281, 66.05206626689808047, -56.86619457917689147 ) ) ;
#54095 = CARTESIAN_POINT ( 'NONE',  ( 23.24999999999999289, 11.65000000001116298, -179.6499999999999773 ) ) ;
#54096 = FACE_OUTER_BOUND ( 'NONE', #242265, .T. ) ;
#54097 = CARTESIAN_POINT ( 'NONE',  ( 12.60053434924910576, 9.389534562346701918, -15.67480930438995479 ) ) ;
#54099 = CARTESIAN_POINT ( 'NONE',  ( 20.94999999999999929, 76.00000000001142553, -36.02310748452432421 ) ) ;
#54098 = CARTESIAN_POINT ( 'NONE',  ( 20.84999999999998721, 11.75000000001115552, -134.0000000000000284 ) ) ;
#54100 = CARTESIAN_POINT ( 'NONE',  ( 18.49999999999999289, 10.41716543472751688, -58.34999999942034776 ) ) ;
#54102 = ORIENTED_EDGE ( 'NONE', *, *, #169593, .T. ) ;
#54101 = CARTESIAN_POINT ( 'NONE',  ( -18.59999999999999787, 38.28679861725830591, -261.0868692510649680 ) ) ;
#54104 = CARTESIAN_POINT ( 'NONE',  ( -20.64999999999999858, 7.150000000011155876, -188.7499999999999716 ) ) ;
#54103 = DIRECTION ( 'NONE',  ( -1.000000000000000000, 0.000000000000000000, 0.000000000000000000 ) ) ;
#54105 = CARTESIAN_POINT ( 'NONE',  ( -20.54999999999999716, 87.75000000001153921, -52.77310748452423894 ) ) ;
#54106 = ORIENTED_EDGE ( 'NONE', *, *, #104389, .F. ) ;
#54107 = CARTESIAN_POINT ( 'NONE',  ( 18.39999999999999858, -9.599999999988845900, -107.1001893912220879 ) ) ;
#54108 = CARTESIAN_POINT ( 'NONE',  ( 21.11747605621531321, 8.778708005504054057, -146.2445631697897852 ) ) ;
#54109 = FACE_OUTER_BOUND ( 'NONE', #88918, .T. ) ;
#54110 = EDGE_LOOP ( 'NONE', ( #182911, #135053, #168947, #252821 ) ) ;
#54111 = DIRECTION ( 'NONE',  ( 1.000000000000000000, 2.952720810173289112E-16, -0.000000000000000000 ) ) ;
#54112 = AXIS2_PLACEMENT_3D ( 'NONE', #51621, #129899, #128641 ) ;
#54113 = DIRECTION ( 'NONE',  ( 0.000000000000000000, 0.000000000000000000, -1.000000000000000000 ) ) ;
#54114 = CARTESIAN_POINT ( 'NONE',  ( 12.84233041328156588, 66.58946139148298471, -87.59041948738348538 ) ) ;
#54115 = ORIENTED_EDGE ( 'NONE', *, *, #98409, .T. ) ;
#54116 = VERTEX_POINT ( 'NONE', #3405 ) ;
#54117 = CARTESIAN_POINT ( 'NONE',  ( 22.40000000000010516, 64.15556351076629937, -247.1958793361852429 ) ) ;
#54119 = CARTESIAN_POINT ( 'NONE',  ( -17.80356949363524777, 65.12326860301459419, -159.7361805087439279 ) ) ;
#54118 = AXIS2_PLACEMENT_3D ( 'NONE', #67879, #52155, #73061 ) ;
#54120 = DIRECTION ( 'NONE',  ( 1.000000000000000000, 2.952720810173289112E-16, -0.000000000000000000 ) ) ;
#54121 = ORIENTED_EDGE ( 'NONE', *, *, #3930, .F. ) ;
#54122 = CARTESIAN_POINT ( 'NONE',  ( 14.56326696814972266, 46.56726880910646571, -234.7610735323249571 ) ) ;
#54123 = EDGE_CURVE ( 'NONE', #17415, #235498, #21713, .T. ) ;
#54124 = CARTESIAN_POINT ( 'NONE',  ( -22.50000000000000000, 64.35012909624819599, -170.1056273753973471 ) ) ;
#54125 = DIRECTION ( 'NONE',  ( -1.000000000000000000, 0.000000000000000000, 0.000000000000000000 ) ) ;
#54126 = EDGE_CURVE ( 'NONE', #53673, #86047, #81638, .T. ) ;
#54127 = AXIS2_PLACEMENT_3D ( 'NONE', #68973, #188901, #229321 ) ;
#54129 = FACE_OUTER_BOUND ( 'NONE', #65812, .T. ) ;
#54128 = AXIS2_PLACEMENT_3D ( 'NONE', #48120, #10303, #68998 ) ;
#54130 = ADVANCED_FACE ( 'NONE', ( #161225 ), #245895, .T. ) ;
#54132 = ORIENTED_EDGE ( 'NONE', *, *, #164510, .T. ) ;
#54131 = CARTESIAN_POINT ( 'NONE',  ( -16.93294127766158752, 65.99671989705693420, -82.09320021869514505 ) ) ;
#54133 = CARTESIAN_POINT ( 'NONE',  ( 13.40000000000000036, -12.24999999999999822, 15.00000000000000355 ) ) ;
#54134 = EDGE_CURVE ( 'NONE', #71322, #212672, #212442, .T. ) ;
#54135 = DIRECTION ( 'NONE',  ( 1.000000000000000000, -0.000000000000000000, -0.000000000000000000 ) ) ;
#54136 = CARTESIAN_POINT ( 'NONE',  ( -18.39999999999999858, 11.47316190337362762, -76.32594606680801519 ) ) ;
#54137 = AXIS2_PLACEMENT_3D ( 'NONE', #209037, #146474, #248165 ) ;
#54138 = CARTESIAN_POINT ( 'NONE',  ( 21.05000000000000071, -0.09999999998884338825, -93.95934304829877703 ) ) ;
#54139 = CARTESIAN_POINT ( 'NONE',  ( -21.05000000000000071, 74.83729825007360148, -61.42310748452432989 ) ) ;
#54141 = EDGE_LOOP ( 'NONE', ( #87778, #180061, #3116, #167527 ) ) ;
#54140 = DIRECTION ( 'NONE',  ( -0.000000000000000000, -0.9875055080513799322, 0.1575844902526464253 ) ) ;
#54142 = CARTESIAN_POINT ( 'NONE',  ( -20.94999999999999929, 1.115600667400684642E-11, -200.9999999999999432 ) ) ;
#54143 = CARTESIAN_POINT ( 'NONE',  ( 20.94999999999999929, 61.88149656937974896, -248.1136133839584090 ) ) ;
#54144 = DIRECTION ( 'NONE',  ( 0.000000000000000000, 0.000000000000000000, -1.000000000000000000 ) ) ;
#54145 = AXIS2_PLACEMENT_3D ( 'NONE', #131817, #56111, #135654 ) ;
#54146 = ORIENTED_EDGE ( 'NONE', *, *, #122571, .F. ) ;
#54147 = LINE ( 'NONE', #17583, #188584 ) ;
#54148 = CARTESIAN_POINT ( 'NONE',  ( -21.05000000000000071, 1.115600667400684642E-11, -100.5000000000000426 ) ) ;
#54149 = FACE_OUTER_BOUND ( 'NONE', #6037, .T. ) ;
#54150 = CARTESIAN_POINT ( 'NONE',  ( -23.15000000000000213, -11.65000000000000036, -30.39999999999999503 ) ) ;
#54151 = SPHERICAL_SURFACE ( 'NONE', #67280, 0.1000000000000000056 ) ;
#54152 = SPHERICAL_SURFACE ( 'NONE', #26099, 0.1000000000000000056 ) ;
#54153 = EDGE_CURVE ( 'NONE', #124577, #177733, #124664, .T. ) ;
#54155 = EDGE_CURVE ( 'NONE', #129105, #250227, #225889, .T. ) ;
#54154 = AXIS2_PLACEMENT_3D ( 'NONE', #185710, #134368, #194392 ) ;
#54157 = VERTEX_POINT ( 'NONE', #170254 ) ;
#54156 = AXIS2_PLACEMENT_3D ( 'NONE', #232131, #252946, #233420 ) ;
#54158 = ORIENTED_EDGE ( 'NONE', *, *, #81499, .T. ) ;
#54159 = AXIS2_PLACEMENT_3D ( 'NONE', #200006, #237841, #201276 ) ;
#54160 = AXIS2_PLACEMENT_3D ( 'NONE', #255782, #38083, #56322 ) ;
#54161 = FACE_BOUND ( 'NONE', #199596, .T. ) ;
#54162 = FACE_OUTER_BOUND ( 'NONE', #47675, .T. ) ;
#54163 = AXIS2_PLACEMENT_3D ( 'NONE', #160899, #123045, #240420 ) ;
#54164 = CARTESIAN_POINT ( 'NONE',  ( 20.94999999999999929, -8.999999999988842703, -90.60603087734760663 ) ) ;
#54165 = DIRECTION ( 'NONE',  ( -1.020425574104004196E-15, -6.982962677686266711E-15, 1.000000000000000000 ) ) ;
#54166 = CARTESIAN_POINT ( 'NONE',  ( 21.05000000000000071, 85.50000000001261924, -193.6291383618718385 ) ) ;
#54167 = EDGE_CURVE ( 'NONE', #70706, #144450, #167655, .T. ) ;
#54168 = DIRECTION ( 'NONE',  ( 1.000000000000000000, 0.000000000000000000, 0.000000000000000000 ) ) ;
#54169 = ADVANCED_FACE ( 'NONE', ( #128510 ), #28151, .F. ) ;
#54170 = CARTESIAN_POINT ( 'NONE',  ( -23.25000000000000355, 53.37686160793744961, -235.8706811220569932 ) ) ;
#54171 = ORIENTED_EDGE ( 'NONE', *, *, #63236, .F. ) ;
#54172 = CARTESIAN_POINT ( 'NONE',  ( -23.25000000000000000, 7.675662554762638479, -241.7139905447625381 ) ) ;
#54173 = ORIENTED_EDGE ( 'NONE', *, *, #81753, .T. ) ;
#54174 = CARTESIAN_POINT ( 'NONE',  ( 23.25000000000000000, 87.65000000001172964, -72.62310748452422615 ) ) ;
#54175 = DIRECTION ( 'NONE',  ( 1.000000000000000000, 0.000000000000000000, 0.000000000000000000 ) ) ;
#54176 = CARTESIAN_POINT ( 'NONE',  ( 21.05000000000000071, 10.62872031400434736, -7.664913569087605794 ) ) ;
#54178 = EDGE_LOOP ( 'NONE', ( #181119, #241060, #136086, #96596 ) ) ;
#54177 = CARTESIAN_POINT ( 'NONE',  ( 18.49999999999999645, 70.30054753569118020, -216.0653814410942175 ) ) ;
#54179 = EDGE_CURVE ( 'NONE', #54887, #129010, #46840, .T. ) ;
#54180 = LINE ( 'NONE', #68627, #215450 ) ;
#54181 = DIRECTION ( 'NONE',  ( -2.342056488767300981E-15, -0.9371753822965326330, 0.3488585713686107592 ) ) ;
#54182 = CARTESIAN_POINT ( 'NONE',  ( 18.40916198585730257, 85.50000000001166711, -62.92291785270108306 ) ) ;
#54183 = ADVANCED_FACE ( 'NONE', ( #12434 ), #192336, .F. ) ;
#54185 = ORIENTED_EDGE ( 'NONE', *, *, #912, .T. ) ;
#54184 = AXIS2_PLACEMENT_3D ( 'NONE', #167210, #246702, #28994 ) ;
#54186 = CARTESIAN_POINT ( 'NONE',  ( -20.64999999999999858, -9.000000000000003553, -9.393969122652443104 ) ) ;
#54187 = CYLINDRICAL_SURFACE ( 'NONE', #204914, 0.8750000000000007772 ) ;
#54188 = DIRECTION ( 'NONE',  ( 1.000000000000000000, 0.000000000000000000, 0.000000000000000000 ) ) ;
#54189 = CARTESIAN_POINT ( 'NONE',  ( -18.46093223321789978, 85.48068296828677148, -162.9385569705971193 ) ) ;
#54190 = EDGE_CURVE ( 'NONE', #109684, #122934, #208064, .T. ) ;
#54191 = DIRECTION ( 'NONE',  ( 1.000000000000000000, 3.265361837132813093E-16, -0.000000000000000000 ) ) ;
#54192 = AXIS2_PLACEMENT_3D ( 'NONE', #215114, #118602, #176017 ) ;
#54193 = VERTEX_POINT ( 'NONE', #206761 ) ;
#54194 = DIRECTION ( 'NONE',  ( 0.000000000000000000, 0.000000000000000000, -1.000000000000000000 ) ) ;
#54195 = CARTESIAN_POINT ( 'NONE',  ( -16.80100426158790583, 66.05684947961573528, -90.34016173169030139 ) ) ;
#54196 = ORIENTED_EDGE ( 'NONE', *, *, #196329, .F. ) ;
#54197 = DIRECTION ( 'NONE',  ( -0.000000000000000000, -0.000000000000000000, -1.000000000000000000 ) ) ;
#54198 = ADVANCED_FACE ( 'NONE', ( #107653 ), #17616, .T. ) ;
#54199 = EDGE_LOOP ( 'NONE', ( #69775, #184814, #234399, #229474, #77403 ) ) ;
#54200 = CARTESIAN_POINT ( 'NONE',  ( 18.54999999999999716, 67.25000000001227818, -157.3731074845244393 ) ) ;
#54201 = CARTESIAN_POINT ( 'NONE',  ( 21.72449340488910607, 10.28395627750227703, -176.7499999999999716 ) ) ;
#54202 = VECTOR ( 'NONE', #116422, 1000.000000000000000 ) ;
#54203 = EDGE_CURVE ( 'NONE', #115380, #146108, #50926, .T. ) ;
#54204 = AXIS2_PLACEMENT_3D ( 'NONE', #104665, #143816, #65574 ) ;
#54205 = ORIENTED_EDGE ( 'NONE', *, *, #39106, .T. ) ;
#54206 = CARTESIAN_POINT ( 'NONE',  ( 18.58725287972279361, -9.566626910681346629, -174.3225048057644244 ) ) ;
#54207 = FACE_OUTER_BOUND ( 'NONE', #54547, .T. ) ;
#54208 = ORIENTED_EDGE ( 'NONE', *, *, #2906, .T. ) ;
#54209 = AXIS2_PLACEMENT_3D ( 'NONE', #56304, #217940, #39358 ) ;
#54210 = AXIS2_PLACEMENT_3D ( 'NONE', #219276, #100585, #115358 ) ;
#54211 = ORIENTED_EDGE ( 'NONE', *, *, #15932, .F. ) ;
#54212 = CARTESIAN_POINT ( 'NONE',  ( 21.07928932188134397, 75.90110485435778287, -142.8516241409176075 ) ) ;
#54213 = CARTESIAN_POINT ( 'NONE',  ( -21.04999999999994387, 64.35000000001120668, -30.02310748452479316 ) ) ;
#54215 = ORIENTED_EDGE ( 'NONE', *, *, #199205, .T. ) ;
#54214 = CARTESIAN_POINT ( 'NONE',  ( 21.97500000000000497, 9.750000000011153745, -79.35000000000005116 ) ) ;
#54216 = DIRECTION ( 'NONE',  ( 3.616040088954497272E-32, -1.224646799147352961E-16, 1.000000000000000000 ) ) ;
#54217 = DIRECTION ( 'NONE',  ( 0.000000000000000000, -0.7973076739542579450, 0.6035730884107166627 ) ) ;
#54218 = FACE_OUTER_BOUND ( 'NONE', #4883, .T. ) ;
#54219 = CARTESIAN_POINT ( 'NONE',  ( -18.35663730107557257, 11.47390742652235573, -76.25000000000004263 ) ) ;
#54220 = PLANE ( 'NONE',  #37792 ) ;
#54221 = CARTESIAN_POINT ( 'NONE',  ( -21.37071067811865532, 8.070710678129811910, -188.7499999999999716 ) ) ;
#54222 = CARTESIAN_POINT ( 'NONE',  ( -16.77779411503079388, 66.05389855308817459, -157.3600500669045914 ) ) ;
#54224 = VERTEX_POINT ( 'NONE', #249740 ) ;
#54223 = DIRECTION ( 'NONE',  ( 7.589415207398576792E-15, 1.000000000000000000, 6.982962677686266711E-15 ) ) ;
#54225 = VERTEX_POINT ( 'NONE', #131067 ) ;
#54228 = CARTESIAN_POINT ( 'NONE',  ( -16.80070461187981223, 51.62163376436579654, -231.9452277169720560 ) ) ;
#54227 = CARTESIAN_POINT ( 'NONE',  ( -21.51976009735018991, 69.08954155835245103, -69.52310748452435973 ) ) ;
#54226 = AXIS2_PLACEMENT_3D ( 'NONE', #195193, #92201, #176909 ) ;
#54229 = AXIS2_PLACEMENT_3D ( 'NONE', #129018, #67750, #70351 ) ;
#54231 = ORIENTED_EDGE ( 'NONE', *, *, #164632, .F. ) ;
#54230 = DIRECTION ( 'NONE',  ( -0.000000000000000000, 0.1350103645451945777, -0.9908441862701590219 ) ) ;
#54232 = ORIENTED_EDGE ( 'NONE', *, *, #24420, .F. ) ;
#54233 = DIRECTION ( 'NONE',  ( 0.000000000000000000, 0.8660254037844411501, 0.4999999999999956701 ) ) ;
#54234 = DIRECTION ( 'NONE',  ( 0.000000000000000000, 0.1350103645451904977, -0.9908441862701596881 ) ) ;
#54235 = CARTESIAN_POINT ( 'NONE',  ( 20.94999999999999929, -1.835341550213257733, -78.55515129256302487 ) ) ;
#54236 = DIRECTION ( 'NONE',  ( 0.000000000000000000, 1.776356839400244943E-15, -1.000000000000000000 ) ) ;
#54237 = CARTESIAN_POINT ( 'NONE',  ( 18.59999999999999432, 85.48068669529136798, -163.0819923157664562 ) ) ;
#54238 = DIRECTION ( 'NONE',  ( 0.000000000000000000, 0.000000000000000000, -1.000000000000000000 ) ) ;
#54239 = CARTESIAN_POINT ( 'NONE',  ( 18.59999999999999432, 14.81796439977981272, -236.5325475414793743 ) ) ;
#54240 = CIRCLE ( 'NONE', #249888, 1.900000000000005906 ) ;
#54241 = ORIENTED_EDGE ( 'NONE', *, *, #160012, .F. ) ;
#54242 = ORIENTED_EDGE ( 'NONE', *, *, #118507, .F. ) ;
#54243 = VECTOR ( 'NONE', #205113, 1000.000000000000000 ) ;
#54244 = EDGE_CURVE ( 'NONE', #88538, #121084, #146794, .T. ) ;
#54245 = CARTESIAN_POINT ( 'NONE',  ( -18.59999999999999787, 64.35000000001150511, -48.17310748452440095 ) ) ;
#54246 = CIRCLE ( 'NONE', #216575, 0.09999999999999939493 ) ;
#54247 = VECTOR ( 'NONE', #832, 1000.000000000000000 ) ;
#54248 = ORIENTED_EDGE ( 'NONE', *, *, #212490, .T. ) ;
#54249 = DIRECTION ( 'NONE',  ( 0.000000000000000000, -1.000000000000000000, 0.000000000000000000 ) ) ;
#54250 = EDGE_LOOP ( 'NONE', ( #121133, #439, #162908, #193570 ) ) ;
#54251 = LINE ( 'NONE', #251159, #55848 ) ;
#54252 = AXIS2_PLACEMENT_3D ( 'NONE', #10881, #250759, #207819 ) ;
#54253 = FACE_OUTER_BOUND ( 'NONE', #219809, .T. ) ;
#54254 = EDGE_CURVE ( 'NONE', #43859, #209826, #108932, .T. ) ;
#54255 = DIRECTION ( 'NONE',  ( -1.000000000000000000, 0.000000000000000000, 0.000000000000000000 ) ) ;
#54256 = ORIENTED_EDGE ( 'NONE', *, *, #13429, .F. ) ;
#54257 = VERTEX_POINT ( 'NONE', #111513 ) ;
#54258 = ADVANCED_FACE ( 'NONE', ( #228896 ), #150639, .F. ) ;
#54259 = EDGE_CURVE ( 'NONE', #222677, #195237, #129784, .T. ) ;
#54260 = CARTESIAN_POINT ( 'NONE',  ( -21.64999999999999858, 68.75000000001224976, -148.7731074845244166 ) ) ;
#54262 = AXIS2_PLACEMENT_3D ( 'NONE', #137740, #73973, #97312 ) ;
#54261 = CARTESIAN_POINT ( 'NONE',  ( 18.40000000000000213, 8.841736820195471580, -245.4273993276876240 ) ) ;
#54263 = VERTEX_POINT ( 'NONE', #209315 ) ;
#54264 = CARTESIAN_POINT ( 'NONE',  ( 13.99999999999999822, 9.850000000011137402, -83.75000000000004263 ) ) ;
#54265 = ORIENTED_EDGE ( 'NONE', *, *, #201465, .T. ) ;
#54268 = ORIENTED_EDGE ( 'NONE', *, *, #208631, .T. ) ;
#54267 = DIRECTION ( 'NONE',  ( 0.000000000000000000, -1.000000000000000000, -6.982962677686265922E-15 ) ) ;
#54266 = LINE ( 'NONE', #133807, #161794 ) ;
#54269 = FACE_OUTER_BOUND ( 'NONE', #96438, .T. ) ;
#54270 = ORIENTED_EDGE ( 'NONE', *, *, #5973, .F. ) ;
#54271 = B_SPLINE_CURVE_WITH_KNOTS ( 'NONE', 3,
 ( #220784, #143801, #180385, #138644, #21330, #83794, #163389 ),
 .UNSPECIFIED., .F., .F.,
 ( 4, 3, 4 ),
 ( 0.000000000000000000, 4.520325912680675046E-05, 5.794988040901435228E-05 ),
 .UNSPECIFIED. ) ;
#54272 = ORIENTED_EDGE ( 'NONE', *, *, #49033, .T. ) ;
#54273 = ADVANCED_FACE ( 'NONE', ( #132351 ), #211912, .F. ) ;
#54274 = CARTESIAN_POINT ( 'NONE',  ( 22.47007471830798053, 1.834461605516000565E-15, 7.720710651926451895 ) ) ;
#54275 = EDGE_CURVE ( 'NONE', #189217, #46937, #17800, .T. ) ;
#54276 = ORIENTED_EDGE ( 'NONE', *, *, #167696, .F. ) ;
#54277 = FACE_OUTER_BOUND ( 'NONE', #85047, .T. ) ;
#54278 = CARTESIAN_POINT ( 'NONE',  ( 22.40736611211992368, 64.18196446391819165, -247.0985338183330668 ) ) ;
#54279 = DIRECTION ( 'NONE',  ( -0.000000000000000000, -0.8700118002898321601, 0.4930308989875230030 ) ) ;
#54280 = DIRECTION ( 'NONE',  ( 0.000000000000000000, 1.000000000000000000, 0.000000000000000000 ) ) ;
#54281 = DIRECTION ( 'NONE',  ( 1.000000000000000000, 0.000000000000000000, 0.000000000000000000 ) ) ;
#54282 = VERTEX_POINT ( 'NONE', #31997 ) ;
#54283 = CARTESIAN_POINT ( 'NONE',  ( -16.93230518875208190, 44.04699785180793015, -235.2829609980169892 ) ) ;
#54284 = DIRECTION ( 'NONE',  ( 0.000000000000000000, -6.352154140967427193E-15, 1.000000000000000000 ) ) ;
#54285 = CARTESIAN_POINT ( 'NONE',  ( -20.96428641294271600, 11.75000000001149303, -160.6748931779414704 ) ) ;
#54286 = VECTOR ( 'NONE', #99447, 1000.000000000000000 ) ;
#54287 = VERTEX_POINT ( 'NONE', #172814 ) ;
#54288 = FACE_OUTER_BOUND ( 'NONE', #188956, .T. ) ;
#54289 = ORIENTED_EDGE ( 'NONE', *, *, #209430, .T. ) ;
#54290 = CARTESIAN_POINT ( 'NONE',  ( -23.15000000000000213, -9.599999999988844124, -122.2500000000000284 ) ) ;
#54291 = ORIENTED_EDGE ( 'NONE', *, *, #222807, .T. ) ;
#54292 = EDGE_CURVE ( 'NONE', #166165, #185482, #22121, .T. ) ;
#54293 = CARTESIAN_POINT ( 'NONE',  ( 18.59999999999999076, 54.57427006634497957, -228.7596887170734306 ) ) ;
#54294 = CARTESIAN_POINT ( 'NONE',  ( 18.59999999999999076, 62.49201502323811752, -208.8221019049098857 ) ) ;
#54295 = AXIS2_PLACEMENT_3D ( 'NONE', #29771, #226636, #126255 ) ;
#54297 = ORIENTED_EDGE ( 'NONE', *, *, #242328, .F. ) ;
#54296 = DIRECTION ( 'NONE',  ( 0.000000000000000000, 0.000000000000000000, 1.000000000000000000 ) ) ;
#54298 = DIRECTION ( 'NONE',  ( 0.000000000000000000, 0.000000000000000000, 1.000000000000000000 ) ) ;
#54299 = ORIENTED_EDGE ( 'NONE', *, *, #20775, .T. ) ;
#54300 = CARTESIAN_POINT ( 'NONE',  ( -20.54999999999999716, 1.940186915899004161, -87.67088078894671810 ) ) ;
#54301 = DIRECTION ( 'NONE',  ( 0.000000000000000000, 0.000000000000000000, 1.000000000000000000 ) ) ;
#54303 = ADVANCED_FACE ( 'NONE', ( #187218 ), #47025, .T. ) ;
#54302 = ORIENTED_EDGE ( 'NONE', *, *, #190407, .T. ) ;
#54304 = DIRECTION ( 'NONE',  ( 0.000000000000000000, -0.000000000000000000, 1.000000000000000000 ) ) ;
#54305 = CARTESIAN_POINT ( 'NONE',  ( 20.95289811251229750, 67.10683199555329281, -94.52129799060584503 ) ) ;
#54306 = VERTEX_POINT ( 'NONE', #88062 ) ;
#54307 = CARTESIAN_POINT ( 'NONE',  ( -16.93302609847409457, 9.996682520814371031, -146.5863884953625700 ) ) ;
#54308 = AXIS2_PLACEMENT_3D ( 'NONE', #247255, #146863, #226398 ) ;
#54309 = CIRCLE ( 'NONE', #87624, 11.70000000000000995 ) ;
#54310 = ORIENTED_EDGE ( 'NONE', *, *, #229229, .T. ) ;
#54311 = CARTESIAN_POINT ( 'NONE',  ( -18.59999999999999787, 46.45388641681647357, -243.1520440498138385 ) ) ;
#54312 = PLANE ( 'NONE',  #59869 ) ;
#54313 = TOROIDAL_SURFACE ( 'NONE', #149, 0.2000000000000000111, 0.1000000000000000056 ) ;
#54314 = VECTOR ( 'NONE', #143615, 1000.000000000000000 ) ;
#54315 = CIRCLE ( 'NONE', #245880, 7.800000000000001599 ) ;
#54317 = ORIENTED_EDGE ( 'NONE', *, *, #75327, .F. ) ;
#54316 = DIRECTION ( 'NONE',  ( 0.000000000000000000, 0.000000000000000000, 1.000000000000000000 ) ) ;
#54318 = ADVANCED_FACE ( 'NONE', ( #155801 ), #193618, .T. ) ;
#54319 = DIRECTION ( 'NONE',  ( 0.000000000000000000, 1.000000000000000000, 6.853228547068871147E-15 ) ) ;
#54320 = CYLINDRICAL_SURFACE ( 'NONE', #223031, 0.09999999999999939493 ) ;
#54321 = CYLINDRICAL_SURFACE ( 'NONE', #36045, 12.87499999999999467 ) ;
#54323 = FACE_OUTER_BOUND ( 'NONE', #156992, .T. ) ;
#54322 = DIRECTION ( 'NONE',  ( 0.000000000000000000, 0.000000000000000000, 1.000000000000000000 ) ) ;
#54324 = DIRECTION ( 'NONE',  ( -0.000000000000000000, -0.000000000000000000, -1.000000000000000000 ) ) ;
#54325 = DIRECTION ( 'NONE',  ( 0.000000000000000000, 0.000000000000000000, 1.000000000000000000 ) ) ;
#54326 = CARTESIAN_POINT ( 'NONE',  ( -22.59080734064477625, 11.75000000000000355, 0.03074970809701978169 ) ) ;
#54327 = VECTOR ( 'NONE', #253927, 1000.000000000000000 ) ;
#54328 = DIRECTION ( 'NONE',  ( -1.000000000000000000, -0.000000000000000000, -0.000000000000000000 ) ) ;
#54329 = AXIS2_PLACEMENT_3D ( 'NONE', #163306, #221950, #43359 ) ;
#54330 = AXIS2_PLACEMENT_3D ( 'NONE', #171872, #210963, #133976 ) ;
#54331 = ORIENTED_EDGE ( 'NONE', *, *, #64293, .T. ) ;
#54332 = AXIS2_PLACEMENT_3D ( 'NONE', #255138, #236911, #115692 ) ;
#54334 = VERTEX_POINT ( 'NONE', #98320 ) ;
#54333 = CIRCLE ( 'NONE', #145920, 11.65000000000000036 ) ;
#54335 = ADVANCED_FACE ( 'NONE', ( #117913 ), #13723, .F. ) ;
#54336 = CARTESIAN_POINT ( 'NONE',  ( -21.05000000000000071, 76.10000000001174669, -81.17267829206912211 ) ) ;
#54337 = EDGE_CURVE ( 'NONE', #250604, #79652, #67895, .T. ) ;
#54339 = ORIENTED_EDGE ( 'NONE', *, *, #153960, .F. ) ;
#54338 = CARTESIAN_POINT ( 'NONE',  ( 20.95512820512820440, 51.70841171101545086, -231.1679749149966767 ) ) ;
#54340 = ORIENTED_EDGE ( 'NONE', *, *, #200622, .F. ) ;
#54341 = DIRECTION ( 'NONE',  ( 1.000000000000000000, 3.265361837132813093E-16, -0.000000000000000000 ) ) ;
#54342 = ORIENTED_EDGE ( 'NONE', *, *, #65620, .T. ) ;
#54343 = LINE ( 'NONE', #94757, #12877 ) ;
#54344 = EDGE_CURVE ( 'NONE', #190690, #159239, #214447, .T. ) ;
#54345 = EDGE_CURVE ( 'NONE', #221781, #189976, #59192, .T. ) ;
#54346 = CIRCLE ( 'NONE', #108529, 0.1000000000000028644 ) ;
#54347 = ORIENTED_EDGE ( 'NONE', *, *, #129594, .F. ) ;
#54348 = EDGE_CURVE ( 'NONE', #198727, #188180, #142704, .T. ) ;
#54349 = CARTESIAN_POINT ( 'NONE',  ( -23.15000000000000213, 87.65000000001192859, -106.1231074845242262 ) ) ;
#54350 = ADVANCED_FACE ( 'NONE', ( #237875 ), #130235, .F. ) ;
#54352 = ORIENTED_EDGE ( 'NONE', *, *, #236977, .T. ) ;
#54351 = VERTEX_POINT ( 'NONE', #18820 ) ;
#54353 = ORIENTED_EDGE ( 'NONE', *, *, #86238, .T. ) ;
#54355 = EDGE_CURVE ( 'NONE', #90335, #20565, #180321, .T. ) ;
#54354 = ADVANCED_FACE ( 'NONE', ( #17526 ), #137471, .F. ) ;
#54356 = ORIENTED_EDGE ( 'NONE', *, *, #17995, .F. ) ;
#54357 = ORIENTED_EDGE ( 'NONE', *, *, #246804, .F. ) ;
#54358 = B_SPLINE_CURVE_WITH_KNOTS ( 'NONE', 3,
 ( #29587, #230312, #146908, #51654, #131214, #105188, #184768, #66112, #225159, #215869, #234162, #75129, #232915, #55494, #95927, #33448, #210756, #37278, #154667 ),
 .UNSPECIFIED., .F., .F.,
 ( 4, 3, 3, 3, 3, 3, 4 ),
 ( 0.000000000000000000, 2.646747978908111750E-05, 5.271166642128749541E-05, 9.008788829883769176E-05, 0.0001426648776561031766, 0.0001897378458659604891, 0.0001917382627806266582 ),
 .UNSPECIFIED. ) ;
#54359 = FACE_OUTER_BOUND ( 'NONE', #252308, .T. ) ;
#54360 = FACE_OUTER_BOUND ( 'NONE', #73262, .T. ) ;
#54361 = CARTESIAN_POINT ( 'NONE',  ( -16.94107738177414291, 10.01423928514777373, -87.95000000000004547 ) ) ;
#54363 = ORIENTED_EDGE ( 'NONE', *, *, #130987, .T. ) ;
#54362 = CARTESIAN_POINT ( 'NONE',  ( -20.64999999999999858, 4.350000000011156054, -79.25000000000004263 ) ) ;
#54364 = CARTESIAN_POINT ( 'NONE',  ( -22.00356870142023880, 33.69312245273549422, -242.9308869566657165 ) ) ;
#54365 = DIRECTION ( 'NONE',  ( 0.000000000000000000, 0.8814952561688434995, -0.4721928772777335137 ) ) ;
#54367 = EDGE_LOOP ( 'NONE', ( #6855, #189756, #119064, #91199 ) ) ;
#54366 = CARTESIAN_POINT ( 'NONE',  ( 20.95203847575071521, 10.50106053928516303, -141.5670713486235570 ) ) ;
#54368 = CARTESIAN_POINT ( 'NONE',  ( -18.50000000000000000, -9.399999999988850163, -40.79725975966329088 ) ) ;
#54369 = ORIENTED_EDGE ( 'NONE', *, *, #235817, .T. ) ;
#54370 = CARTESIAN_POINT ( 'NONE',  ( -23.15000000000000213, 0.000000000000000000, -33.50000000000000000 ) ) ;
#54371 = TOROIDAL_SURFACE ( 'NONE', #158462, 12.77499999999999858, 0.1000000000000000056 ) ;
#54373 = ORIENTED_EDGE ( 'NONE', *, *, #139478, .F. ) ;
#54372 = CARTESIAN_POINT ( 'NONE',  ( 21.72449340488910607, 14.48530878454960202, -219.1840063279242088 ) ) ;
#54374 = FACE_OUTER_BOUND ( 'NONE', #169369, .T. ) ;
#54376 = ADVANCED_FACE ( 'NONE', ( #78777 ), #37132, .T. ) ;
#54375 = FACE_OUTER_BOUND ( 'NONE', #219447, .T. ) ;
#54377 = VECTOR ( 'NONE', #182298, 1000.000000000000000 ) ;
#54378 = ORIENTED_EDGE ( 'NONE', *, *, #230674, .F. ) ;
#54380 = CARTESIAN_POINT ( 'NONE',  ( -18.50000000000000000, 1.115600667400684642E-11, -200.9999999999999432 ) ) ;
#54379 = CARTESIAN_POINT ( 'NONE',  ( -16.87242674293849021, 9.950000000011138823, -121.3510902463723937 ) ) ;
#54381 = EDGE_CURVE ( 'NONE', #87179, #101113, #255084, .T. ) ;
#54382 = EDGE_CURVE ( 'NONE', #193788, #199100, #213633, .T. ) ;
#54383 = DIRECTION ( 'NONE',  ( 0.000000000000000000, 0.000000000000000000, 1.000000000000000000 ) ) ;
#54384 = AXIS2_PLACEMENT_3D ( 'NONE', #45004, #125814, #28042 ) ;
#54385 = DIRECTION ( 'NONE',  ( 0.000000000000000000, -0.5826443254700256480, -0.8127272543710952757 ) ) ;
#54386 = DIRECTION ( 'NONE',  ( 1.000000000000000000, 0.000000000000000000, 0.000000000000000000 ) ) ;
#54387 = ORIENTED_EDGE ( 'NONE', *, *, #235407, .T. ) ;
#54388 = ORIENTED_EDGE ( 'NONE', *, *, #80520, .F. ) ;
#54389 = EDGE_CURVE ( 'NONE', #105519, #162952, #115355, .T. ) ;
#54391 = AXIS2_PLACEMENT_3D ( 'NONE', #42864, #143231, #222764 ) ;
#54390 = LINE ( 'NONE', #234305, #180433 ) ;
#54392 = CARTESIAN_POINT ( 'NONE',  ( -23.25000000000000000, 6.933893972137497030, -171.2856458343736108 ) ) ;
#54393 = EDGE_LOOP ( 'NONE', ( #42196, #226035 ) ) ;
#54394 = LINE ( 'NONE', #251300, #243183 ) ;
#54395 = EDGE_LOOP ( 'NONE', ( #15019, #257977, #43118, #148338 ) ) ;
#54396 = PLANE ( 'NONE',  #166882 ) ;
#54397 = ADVANCED_FACE ( 'NONE', ( #157072 ), #101147, .T. ) ;
#54398 = CIRCLE ( 'NONE', #87699, 0.1000000000000028644 ) ;
#54399 = ORIENTED_EDGE ( 'NONE', *, *, #132931, .F. ) ;
#54400 = CARTESIAN_POINT ( 'NONE',  ( 18.59999999999999432, -1.866714910046153308, -179.2526752462819672 ) ) ;
#54401 = SHAPE_REPRESENTATION_RELATIONSHIP ( 'NONE' , 'NONE' ,  #224939, #144531 ) ;
#54402 = AXIS2_PLACEMENT_3D ( 'NONE', #164117, #59842, #243639 ) ;
#54404 = ORIENTED_EDGE ( 'NONE', *, *, #94616, .T. ) ;
#54403 = VECTOR ( 'NONE', #110516, 1000.000000000000000 ) ;
#54405 = ORIENTED_EDGE ( 'NONE', *, *, #30710, .F. ) ;
#54406 = ORIENTED_EDGE ( 'NONE', *, *, #238717, .F. ) ;
#54407 = VECTOR ( 'NONE', #69455, 1000.000000000000000 ) ;
#54408 = DIRECTION ( 'NONE',  ( 0.7071359030027593029, -0.7070776581709197206, 0.000000000000000000 ) ) ;
#54409 = CARTESIAN_POINT ( 'NONE',  ( 15.75000000000000355, 66.65000000001157332, -53.00453852712175262 ) ) ;
#54410 = CARTESIAN_POINT ( 'NONE',  ( -21.07971444708686093, 0.08782343632898097219, -127.6702079183734924 ) ) ;
#54411 = CARTESIAN_POINT ( 'NONE',  ( 20.09999999999999787, 9.750000000011137757, -121.3500000000000227 ) ) ;
#54412 = CARTESIAN_POINT ( 'NONE',  ( 15.57250062127604018, 66.62931007840943209, -118.9966423578633368 ) ) ;
#54414 = DIRECTION ( 'NONE',  ( -1.000000000000000000, -0.000000000000000000, -0.000000000000000000 ) ) ;
#54413 = DIRECTION ( 'NONE',  ( -1.000000000000000000, 0.000000000000000000, 0.000000000000000000 ) ) ;
#54416 = EDGE_LOOP ( 'NONE', ( #210194, #102554, #244953, #243218 ) ) ;
#54415 = DIRECTION ( 'NONE',  ( -1.000000000000000000, -2.952720810173289112E-16, 0.000000000000000000 ) ) ;
#54417 = DIRECTION ( 'NONE',  ( -0.000000000000000000, 0.4791956752371484551, 0.8777080977375184556 ) ) ;
#54418 = ORIENTED_EDGE ( 'NONE', *, *, #181548, .F. ) ;
#54419 = CARTESIAN_POINT ( 'NONE',  ( -12.25000000000000178, 9.350000000011139178, -150.7500000000000284 ) ) ;
#54420 = ORIENTED_EDGE ( 'NONE', *, *, #34415, .F. ) ;
#54421 = ORIENTED_EDGE ( 'NONE', *, *, #227737, .F. ) ;
#54422 = CARTESIAN_POINT ( 'NONE',  ( -23.49999999999994316, 74.94272479589878344, -8.023107484524793165 ) ) ;
#54423 = CARTESIAN_POINT ( 'NONE',  ( -18.59999999999999787, 64.35000000001254250, -182.1731074845244507 ) ) ;
#54424 = CARTESIAN_POINT ( 'NONE',  ( 21.07928932188134397, 75.90110485435759813, -109.3516241409176217 ) ) ;
#54425 = CARTESIAN_POINT ( 'NONE',  ( 21.14999999999999858, 20.97908333644147660, -233.6079013178409411 ) ) ;
#54426 = CIRCLE ( 'NONE', #29516, 0.09999999999998898659 ) ;
#54427 = FACE_OUTER_BOUND ( 'NONE', #248059, .T. ) ;
#54428 = EDGE_LOOP ( 'NONE', ( #210028, #240753, #112102, #201577, #147230 ) ) ;
#54429 = ORIENTED_EDGE ( 'NONE', *, *, #2583, .T. ) ;
#54430 = FACE_OUTER_BOUND ( 'NONE', #124824, .T. ) ;
#54431 = EDGE_LOOP ( 'NONE', ( #141106, #23038, #139334, #196670 ) ) ;
#54432 = CARTESIAN_POINT ( 'NONE',  ( -22.50000000000000000, 1.115600667400684642E-11, -167.4999999999999716 ) ) ;
#54433 = ORIENTED_EDGE ( 'NONE', *, *, #221160, .T. ) ;
#54434 = DIRECTION ( 'NONE',  ( 1.000000000000000000, -0.000000000000000000, -0.000000000000000000 ) ) ;
#54435 = CARTESIAN_POINT ( 'NONE',  ( -20.94999999999999929, 11.75000000001115019, -60.21613433702190576 ) ) ;
#54436 = FACE_OUTER_BOUND ( 'NONE', #252872, .T. ) ;
#54437 = DIRECTION ( 'NONE',  ( 0.000000000000000000, -0.1071148137998806232, -0.9942466578594150173 ) ) ;
#54438 = ORIENTED_EDGE ( 'NONE', *, *, #64106, .T. ) ;
#54439 = DIRECTION ( 'NONE',  ( -1.000000000000000000, 0.000000000000000000, -0.000000000000000000 ) ) ;
#54440 = CIRCLE ( 'NONE', #225103, 2.100000000000002309 ) ;
#54441 = ADVANCED_FACE ( 'NONE', ( #99615 ), #234471, .T. ) ;
#54442 = AXIS2_PLACEMENT_3D ( 'NONE', #42896, #78148, #18194 ) ;
#54443 = CYLINDRICAL_SURFACE ( 'NONE', #53919, 0.1000000000000098310 ) ;
#54444 = VECTOR ( 'NONE', #73706, 1000.000000000000000 ) ;
#54445 = DIRECTION ( 'NONE',  ( 1.000000000000000000, 0.000000000000000000, 0.000000000000000000 ) ) ;
#54446 = ADVANCED_FACE ( 'NONE', ( #116643 ), #42761, .F. ) ;
#54447 = ORIENTED_EDGE ( 'NONE', *, *, #157061, .F. ) ;
#54448 = AXIS2_PLACEMENT_3D ( 'NONE', #210365, #112549, #173850 ) ;
#54449 = ADVANCED_FACE ( 'NONE', ( #180477 ), #123075, .F. ) ;
#54450 = FACE_OUTER_BOUND ( 'NONE', #162363, .T. ) ;
#54451 = ADVANCED_FACE ( 'NONE', ( #42253 ), #43539, .T. ) ;
#54452 = ORIENTED_EDGE ( 'NONE', *, *, #46919, .F. ) ;
#54453 = CARTESIAN_POINT ( 'NONE',  ( -18.50000000000000000, 11.65000000001115232, -179.6499999999999773 ) ) ;
#54454 = DIRECTION ( 'NONE',  ( 0.000000000000000000, 1.000000000000000000, 0.000000000000000000 ) ) ;
#54455 = CARTESIAN_POINT ( 'NONE',  ( -21.05000000000000071, 77.83534155023627932, -91.46795619196130644 ) ) ;
#54456 = CARTESIAN_POINT ( 'NONE',  ( 11.60000000000000320, -8.250000000000003553, 17.60000000000000497 ) ) ;
#54457 = CARTESIAN_POINT ( 'NONE',  ( 20.27550659511089037, 9.216043722520002035, -79.65000000000004832 ) ) ;
#54458 = CARTESIAN_POINT ( 'NONE',  ( 21.14999999999999503, 64.35000000001213039, -136.4231074845243938 ) ) ;
#54459 = AXIS2_PLACEMENT_3D ( 'NONE', #224438, #204868, #45810 ) ;
#54460 = VERTEX_POINT ( 'NONE', #201313 ) ;
#54461 = CARTESIAN_POINT ( 'NONE',  ( -16.94037747912386394, 65.98646061752573644, -123.9719765265488718 ) ) ;
#54462 = CARTESIAN_POINT ( 'NONE',  ( 20.94999999999999929, 64.35000000001249987, -176.8647081744214802 ) ) ;
#54463 = CYLINDRICAL_SURFACE ( 'NONE', #146415, 0.1000000000000006162 ) ;
#54464 = CARTESIAN_POINT ( 'NONE',  ( -20.90000000000000213, 3.461118860469513336, 28.84309995045515507 ) ) ;
#54465 = EDGE_CURVE ( 'NONE', #120046, #119120, #72001, .T. ) ;
#54466 = ADVANCED_FACE ( 'NONE', ( #140036 ), #246946, .T. ) ;
#54467 = ORIENTED_EDGE ( 'NONE', *, *, #50718, .F. ) ;
#54468 = EDGE_LOOP ( 'NONE', ( #254888, #53740, #14247, #105897 ) ) ;
#54469 = PLANE ( 'NONE',  #145842 ) ;
#54470 = DIRECTION ( 'NONE',  ( 0.000000000000000000, 0.9770955615653551529, 0.2128009952262517601 ) ) ;
#54471 = CARTESIAN_POINT ( 'NONE',  ( -20.64999999999999858, 78.98983215084128062, -228.7927651294584450 ) ) ;
#54472 = FACE_OUTER_BOUND ( 'NONE', #23211, .T. ) ;
#54473 = DIRECTION ( 'NONE',  ( -1.000000000000000000, -0.000000000000000000, 0.000000000000000000 ) ) ;
#54474 = AXIS2_PLACEMENT_3D ( 'NONE', #253625, #72459, #13752 ) ;
#54475 = VERTEX_POINT ( 'NONE', #183053 ) ;
#54476 = SPHERICAL_SURFACE ( 'NONE', #22283, 0.1000000000000000056 ) ;
#54477 = CARTESIAN_POINT ( 'NONE',  ( -20.54999999999999716, 2.000000000011154189, -154.2753780772379173 ) ) ;
#54478 = CIRCLE ( 'NONE', #162846, 0.09999999999999939493 ) ;
#54479 = ORIENTED_EDGE ( 'NONE', *, *, #252797, .T. ) ;
#54480 = DIRECTION ( 'NONE',  ( 0.000000000000000000, -0.9908441862701605762, -0.1350103645451835310 ) ) ;
#54481 = ADVANCED_FACE ( 'NONE', ( #23987 ), #134505, .F. ) ;
#54482 = CARTESIAN_POINT ( 'NONE',  ( 23.14999999999999858, 70.10000000001149090, -46.24220724918073699 ) ) ;
#54483 = AXIS2_PLACEMENT_3D ( 'NONE', #221956, #81172, #223259 ) ;
#54484 = EDGE_CURVE ( 'NONE', #256436, #247484, #171989, .T. ) ;
#54485 = VERTEX_POINT ( 'NONE', #102177 ) ;
#54486 = CARTESIAN_POINT ( 'NONE',  ( -21.14999999999999858, 12.92448621296781752, -205.1280733356431938 ) ) ;
#54487 = AXIS2_PLACEMENT_3D ( 'NONE', #192048, #248141, #212879 ) ;
#54488 = ORIENTED_EDGE ( 'NONE', *, *, #134463, .F. ) ;
#54489 = DIRECTION ( 'NONE',  ( 1.000000000000000000, 0.000000000000000000, 0.000000000000000000 ) ) ;
#54490 = CARTESIAN_POINT ( 'NONE',  ( 20.85000000000000142, 77.83585931145570669, -125.0186683157258045 ) ) ;
#54491 = CARTESIAN_POINT ( 'NONE',  ( 21.05000012384953223, 10.62872029888669978, -112.6779773300352332 ) ) ;
#54492 = ADVANCED_FACE ( 'NONE', ( #124356 ), #238576, .T. ) ;
#54493 = CARTESIAN_POINT ( 'NONE',  ( -20.85000000000000142, 36.65892442174935439, -249.5511627012433848 ) ) ;
#54494 = DIRECTION ( 'NONE',  ( 1.000000000000000000, 0.000000000000000000, 0.000000000000000000 ) ) ;
#54495 = FACE_OUTER_BOUND ( 'NONE', #66810, .T. ) ;
#54496 = CARTESIAN_POINT ( 'NONE',  ( 20.85000000000000142, 6.982009704867603972, -171.1961521182563217 ) ) ;
#54497 = EDGE_CURVE ( 'NONE', #104861, #247198, #55375, .T. ) ;
#54499 = CARTESIAN_POINT ( 'NONE',  ( 18.39999999999999503, 8.212522512469059066, -212.1579332307740344 ) ) ;
#54498 = CARTESIAN_POINT ( 'NONE',  ( 20.95420533658165141, 10.54586447477073285, -108.0675060206932727 ) ) ;
#54500 = LINE ( 'NONE', #33709, #146291 ) ;
#54501 = CARTESIAN_POINT ( 'NONE',  ( -20.94999999999999929, -1.835341550213255957, -78.65515129256303339 ) ) ;
#54502 = FACE_OUTER_BOUND ( 'NONE', #245452, .T. ) ;
#54504 = EDGE_CURVE ( 'NONE', #182052, #39363, #220868, .T. ) ;
#54503 = CIRCLE ( 'NONE', #58760, 4.049999999999998046 ) ;
#54505 = ORIENTED_EDGE ( 'NONE', *, *, #9726, .T. ) ;
#54506 = CARTESIAN_POINT ( 'NONE',  ( -21.02374657821582105, 11.60000000083146077, -93.57179677019813369 ) ) ;
#54507 = AXIS2_PLACEMENT_3D ( 'NONE', #173615, #15800, #32804 ) ;
#54508 = FACE_OUTER_BOUND ( 'NONE', #124798, .T. ) ;
#54509 = LINE ( 'NONE', #111943, #220319 ) ;
#54510 = EDGE_CURVE ( 'NONE', #76314, #166025, #203877, .T. ) ;
#54511 = EDGE_LOOP ( 'NONE', ( #15335, #181333, #86687, #142882 ) ) ;
#54512 = AXIS2_PLACEMENT_3D ( 'NONE', #200724, #39103, #118638 ) ;
#54513 = DIRECTION ( 'NONE',  ( 0.000000000000000000, 0.8777080977375072424, -0.4791956752371691608 ) ) ;
#54514 = DIRECTION ( 'NONE',  ( -0.000000000000000000, 1.000000000000000000, 6.982962677686266711E-15 ) ) ;
#54515 = FACE_OUTER_BOUND ( 'NONE', #187466, .T. ) ;
#54516 = CIRCLE ( 'NONE', #221093, 0.09999999999998898659 ) ;
#54517 = EDGE_CURVE ( 'NONE', #103813, #71577, #122056, .T. ) ;
#54518 = AXIS2_PLACEMENT_3D ( 'NONE', #221291, #239604, #218725 ) ;
#54519 = VERTEX_POINT ( 'NONE', #184310 ) ;
#54520 = CARTESIAN_POINT ( 'NONE',  ( -21.65000000000000213, 7.708578643773852157, -121.7500000000000426 ) ) ;
#54521 = EDGE_CURVE ( 'NONE', #16906, #118817, #145178, .T. ) ;
#54522 = ORIENTED_EDGE ( 'NONE', *, *, #110334, .F. ) ;
#54523 = DIRECTION ( 'NONE',  ( 0.000000000000000000, 0.000000000000000000, -1.000000000000000000 ) ) ;
#54524 = DIRECTION ( 'NONE',  ( 0.000000000000000000, -0.3896596508880124654, -0.9209589331071350582 ) ) ;
#54525 = VECTOR ( 'NONE', #191123, 1000.000000000000000 ) ;
#54526 = AXIS2_PLACEMENT_3D ( 'NONE', #70650, #150170, #18344 ) ;
#54527 = AXIS2_PLACEMENT_3D ( 'NONE', #219937, #19169, #221204 ) ;
#54528 = AXIS2_PLACEMENT_3D ( 'NONE', #218935, #160289, #139387 ) ;
#54529 = CIRCLE ( 'NONE', #158609, 6.258578643762696458 ) ;
#54530 = ORIENTED_EDGE ( 'NONE', *, *, #129486, .F. ) ;
#54531 = DIRECTION ( 'NONE',  ( 0.000000000000000000, 0.000000000000000000, -1.000000000000000000 ) ) ;
#54532 = EDGE_CURVE ( 'NONE', #74763, #248708, #120526, .T. ) ;
#54533 = ORIENTED_EDGE ( 'NONE', *, *, #53365, .F. ) ;
#54534 = DIRECTION ( 'NONE',  ( 0.000000000000000000, 0.2128009952263605342, -0.9770955615653315052 ) ) ;
#54535 = DIRECTION ( 'NONE',  ( 0.000000000000000000, -1.000000000000000000, -6.982962677686266711E-15 ) ) ;
#54536 = DIRECTION ( 'NONE',  ( 0.000000000000000000, -0.8814952561688476074, 0.4721928772777262417 ) ) ;
#54537 = DIRECTION ( 'NONE',  ( 0.000000000000000000, 0.1618390714546044939, -0.9868171638914228216 ) ) ;
#54538 = VECTOR ( 'NONE', #175925, 1000.000000000000000 ) ;
#54539 = LINE ( 'NONE', #235736, #154145 ) ;
#54540 = DIRECTION ( 'NONE',  ( 0.000000000000000000, 0.000000000000000000, 1.000000000000000000 ) ) ;
#54541 = CARTESIAN_POINT ( 'NONE',  ( 19.99999999999998934, 11.65000000001115943, -188.7499999999999716 ) ) ;
#54543 = ORIENTED_EDGE ( 'NONE', *, *, #158899, .F. ) ;
#54542 = CARTESIAN_POINT ( 'NONE',  ( 22.88900146558018989, 8.703904791123973084, -113.1500000000000483 ) ) ;
#54544 = ORIENTED_EDGE ( 'NONE', *, *, #104928, .F. ) ;
#54546 = CARTESIAN_POINT ( 'NONE',  ( -21.44999999999999929, 68.85000000001180354, -81.87310748452436826 ) ) ;
#54545 = DIRECTION ( 'NONE',  ( 1.000000000000000000, 0.000000000000000000, 0.000000000000000000 ) ) ;
#54547 = EDGE_LOOP ( 'NONE', ( #148206, #67488, #256230, #75365 ) ) ;
#54549 = ORIENTED_EDGE ( 'NONE', *, *, #190067, .T. ) ;
#54548 = CARTESIAN_POINT ( 'NONE',  ( 23.15000000000000213, 87.39257802171759693, -106.0970570643561501 ) ) ;
#54550 = ORIENTED_EDGE ( 'NONE', *, *, #50896, .F. ) ;
#54551 = PLANE ( 'NONE',  #24974 ) ;
#54552 = DIRECTION ( 'NONE',  ( 0.000000000000000000, 0.000000000000000000, -1.000000000000000000 ) ) ;
#54553 = DIRECTION ( 'NONE',  ( 1.000000000000000000, -0.000000000000000000, 0.000000000000000000 ) ) ;
#54554 = CARTESIAN_POINT ( 'NONE',  ( 18.39999999999999858, -9.519327731092435130, -6.972976376559340217 ) ) ;
#54555 = CARTESIAN_POINT ( 'NONE',  ( 21.15000000000005542, 83.98667523412385094, -37.28476067066772970 ) ) ;
#54556 = DIRECTION ( 'NONE',  ( 0.000000000000000000, 0.000000000000000000, -1.000000000000000000 ) ) ;
#54557 = DIRECTION ( 'NONE',  ( 0.000000000000000000, -0.9910465087640865089, 0.1335171055202864221 ) ) ;
#54558 = AXIS2_PLACEMENT_3D ( 'NONE', #152159, #49174, #208268 ) ;
#54559 = DIRECTION ( 'NONE',  ( 1.000000000000000000, 0.000000000000000000, 0.000000000000000000 ) ) ;
#54560 = EDGE_LOOP ( 'NONE', ( #179737, #85210, #174267, #249840 ) ) ;
#54561 = ORIENTED_EDGE ( 'NONE', *, *, #194767, .F. ) ;
#54562 = DIRECTION ( 'NONE',  ( -1.000000000000000000, 0.000000000000000000, 0.000000000000000000 ) ) ;
#54563 = AXIS2_PLACEMENT_3D ( 'NONE', #95677, #155696, #235206 ) ;
#54564 = ORIENTED_EDGE ( 'NONE', *, *, #121316, .F. ) ;
#54565 = DIRECTION ( 'NONE',  ( 3.469446951953801622E-14, -0.1575844902526687130, -0.9875055080513762684 ) ) ;
#54566 = ORIENTED_EDGE ( 'NONE', *, *, #194506, .F. ) ;
#54567 = CARTESIAN_POINT ( 'NONE',  ( 22.49436431346199683, 11.64995094766461392, -33.43309647027773934 ) ) ;
#54568 = CIRCLE ( 'NONE', #96254, 0.2000000000000057288 ) ;
#54569 = CARTESIAN_POINT ( 'NONE',  ( -21.14999999999999858, 65.59307282722802768, -241.8954991560463554 ) ) ;
#54570 = LINE ( 'NONE', #175829, #9686 ) ;
#54571 = EDGE_CURVE ( 'NONE', #231129, #10053, #104086, .T. ) ;
#54572 = DIRECTION ( 'NONE',  ( 0.000000000000000000, 0.2128009952263485993, -0.9770955615653341697 ) ) ;
#54573 = CARTESIAN_POINT ( 'NONE',  ( 20.94999999999999574, 1.835341550235567887, -78.65515129256303339 ) ) ;
#54574 = EDGE_LOOP ( 'NONE', ( #188102, #80707, #201791, #150583 ) ) ;
#54575 = LINE ( 'NONE', #55833, #108654 ) ;
#54576 = EDGE_CURVE ( 'NONE', #213315, #40685, #33002, .T. ) ;
#54577 = CARTESIAN_POINT ( 'NONE',  ( 18.49999999999999289, 14.86477715130881272, -235.7932433709592601 ) ) ;
#54578 = EDGE_CURVE ( 'NONE', #124124, #211251, #9440, .T. ) ;
#54579 = CARTESIAN_POINT ( 'NONE',  ( -15.75000000000000355, 66.15000000001185754, -86.27310748452437394 ) ) ;
#54580 = CYLINDRICAL_SURFACE ( 'NONE', #146268, 0.1000000000000075273 ) ;
#54581 = LINE ( 'NONE', #214944, #157457 ) ;
#54582 = EDGE_LOOP ( 'NONE', ( #127617, #186098, #122293 ) ) ;
#54585 = CARTESIAN_POINT ( 'NONE',  ( -18.44232395689941129, 85.55228255706126106, -29.18085549971751291 ) ) ;
#54584 = CARTESIAN_POINT ( 'NONE',  ( -21.07094088545304089, 6.320167221927643020, -133.9011062974477966 ) ) ;
#54583 = AXIS2_PLACEMENT_3D ( 'NONE', #144525, #205794, #127549 ) ;
#54586 = ORIENTED_EDGE ( 'NONE', *, *, #40448, .F. ) ;
#54589 = ORIENTED_EDGE ( 'NONE', *, *, #25871, .T. ) ;
#54588 = CARTESIAN_POINT ( 'NONE',  ( -18.59999999999999787, 18.18127959618848166, -237.5711165786817389 ) ) ;
#54587 = PLANE ( 'NONE',  #257375 ) ;
#54590 = AXIS2_PLACEMENT_3D ( 'NONE', #125878, #146708, #103726 ) ;
#54591 = DIRECTION ( 'NONE',  ( 1.224646799147353207E-16, -1.000000000000000000, -6.982962677686266711E-15 ) ) ;
#54592 = VECTOR ( 'NONE', #140552, 1000.000000000000000 ) ;
#54593 = CARTESIAN_POINT ( 'NONE',  ( -22.49533356619859603, 64.34999999370755575, -69.58823006484709595 ) ) ;
#54594 = VERTEX_POINT ( 'NONE', #87768 ) ;
#54595 = CARTESIAN_POINT ( 'NONE',  ( 23.25000000000000000, -11.74999999998883560, -21.75000000000000355 ) ) ;
#54596 = ADVANCED_FACE ( 'NONE', ( #128208 ), #221803, .T. ) ;
#54597 = DIRECTION ( 'NONE',  ( 0.000000000000000000, 2.362176648138631684E-15, -1.000000000000000000 ) ) ;
#54598 = DIRECTION ( 'NONE',  ( 1.000000000000000000, 0.000000000000000000, 0.000000000000000000 ) ) ;
#54600 = VERTEX_POINT ( 'NONE', #29150 ) ;
#54599 = SPHERICAL_SURFACE ( 'NONE', #218196, 0.1000000000000000056 ) ;
#54601 = AXIS2_PLACEMENT_3D ( 'NONE', #228464, #191921, #129341 ) ;
#54602 = ORIENTED_EDGE ( 'NONE', *, *, #162807, .T. ) ;
#54603 = FACE_OUTER_BOUND ( 'NONE', #68779, .T. ) ;
#54604 = CARTESIAN_POINT ( 'NONE',  ( 18.49351773456764292, -9.443025695134114272, -74.18532552602735564 ) ) ;
#54605 = DIRECTION ( 'NONE',  ( -0.7071067811865301422, 0.7071067811865648922, 0.000000000000000000 ) ) ;
#54606 = DIRECTION ( 'NONE',  ( 0.000000000000000000, 0.2617529984164856383, 0.9651348961777204138 ) ) ;
#54607 = EDGE_LOOP ( 'NONE', ( #139859, #121088, #248205, #75962 ) ) ;
#54608 = DIRECTION ( 'NONE',  ( 0.000000000000000000, 0.2128009952263582305, -0.9770955615653319493 ) ) ;
#54609 = EDGE_CURVE ( 'NONE', #143336, #53900, #107344, .T. ) ;
#54610 = CYLINDRICAL_SURFACE ( 'NONE', #138937, 0.09999999999999933942 ) ;
#54611 = CARTESIAN_POINT ( 'NONE',  ( -23.25000000000000000, 85.00000000001222134, -146.4170766071767389 ) ) ;
#54612 = EDGE_CURVE ( 'NONE', #139650, #97714, #5505, .T. ) ;
#54613 = ORIENTED_EDGE ( 'NONE', *, *, #158967, .T. ) ;
#54614 = LINE ( 'NONE', #230709, #117112 ) ;
#54615 = CARTESIAN_POINT ( 'NONE',  ( -22.47071067811865319, 65.11488425470513164, -243.2801022963548689 ) ) ;
#54616 = VECTOR ( 'NONE', #159753, 1000.000000000000000 ) ;
#54617 = AXIS2_PLACEMENT_3D ( 'NONE', #115171, #193439, #14814 ) ;
#54618 = CIRCLE ( 'NONE', #133727, 12.77499999999999503 ) ;
#54620 = EDGE_CURVE ( 'NONE', #175899, #92498, #201344, .T. ) ;
#54619 = EDGE_LOOP ( 'NONE', ( #143222, #53959, #187745, #63399 ) ) ;
#54621 = DIRECTION ( 'NONE',  ( 0.000000000000000000, 0.2617529984166090395, 0.9651348961776869961 ) ) ;
#54622 = CARTESIAN_POINT ( 'NONE',  ( -20.90000000000000213, 8.000000000000000000, 1.212568896937007867 ) ) ;
#54623 = CARTESIAN_POINT ( 'NONE',  ( -20.54999999999999716, 1.115600667400684642E-11, -167.5000000000000284 ) ) ;
#54624 = ORIENTED_EDGE ( 'NONE', *, *, #150379, .T. ) ;
#54625 = ORIENTED_EDGE ( 'NONE', *, *, #231550, .F. ) ;
#54626 = DIRECTION ( 'NONE',  ( -1.000000000000000000, 0.000000000000000000, -0.000000000000000000 ) ) ;
#54627 = ORIENTED_EDGE ( 'NONE', *, *, #212912, .T. ) ;
#54629 = VERTEX_POINT ( 'NONE', #246850 ) ;
#54628 = CARTESIAN_POINT ( 'NONE',  ( 22.40000000000020819, 25.97741635855176057, -254.4468634167663197 ) ) ;
#54630 = AXIS2_PLACEMENT_3D ( 'NONE', #15705, #97742, #136900 ) ;
#54634 = ADVANCED_FACE ( 'NONE', ( #30400 ), #70826, .T. ) ;
#54633 = ORIENTED_EDGE ( 'NONE', *, *, #47852, .F. ) ;
#54632 = ORIENTED_EDGE ( 'NONE', *, *, #213959, .F. ) ;
#54631 = DIRECTION ( 'NONE',  ( 0.000000000000000000, -8.987377189994711700E-15, 1.000000000000000000 ) ) ;
#54635 = CARTESIAN_POINT ( 'NONE',  ( 18.49999999999999645, 79.37986612816742138, -196.2658927859692142 ) ) ;
#54636 = CARTESIAN_POINT ( 'NONE',  ( -16.96982749440685012, 12.51506674510725858, -211.7067928272783490 ) ) ;
#54637 = DIRECTION ( 'NONE',  ( -1.000000000000000000, -2.885090398161910739E-16, -6.283419270304611573E-17 ) ) ;
#54638 = FACE_OUTER_BOUND ( 'NONE', #110041, .T. ) ;
#54639 = FACE_OUTER_BOUND ( 'NONE', #91628, .T. ) ;
#54640 = VERTEX_POINT ( 'NONE', #171229 ) ;
#54641 = EDGE_LOOP ( 'NONE', ( #215981, #100446, #215077, #165200, #173762, #188083, #91112, #32826, #45897, #20628 ) ) ;
#54642 = ORIENTED_EDGE ( 'NONE', *, *, #11113, .F. ) ;
#54643 = EDGE_CURVE ( 'NONE', #152543, #175862, #76252, .T. ) ;
#54644 = DIRECTION ( 'NONE',  ( 0.000000000000000000, 6.982962677686266711E-15, -1.000000000000000000 ) ) ;
#54645 =( BOUNDED_SURFACE ( )  B_SPLINE_SURFACE ( 3, 2, ( 
 ( #110433, #135114, #30935 ),
 ( #189979, #132575, #73912 ),
 ( #11340, #75188, #71334 ),
 ( #90865, #32209, #251213 ),
 ( #154728, #153467, #150845 ),
 ( #113009, #95990, #114285 ) ),
 .UNSPECIFIED., .F., .F., .F. ) 
 B_SPLINE_SURFACE_WITH_KNOTS ( ( 4, 2, 4 ),
 ( 3, 3 ),
 ( 1.570796326794897668, 2.356194490192346169, 3.141592653589794448 ),
 ( 0.000000000000000000, 1.000000000000000000 ),
 .UNSPECIFIED. ) 
 GEOMETRIC_REPRESENTATION_ITEM ( )  RATIONAL_B_SPLINE_SURFACE ( (
 ( 1.000000000000000000, 0.7071067811864732988, 1.000000000000000000),
 ( 1.000000000000000000, 0.6611148371780445343, 1.000000000000000000),
 ( 1.000000000000000000, 0.6092287576693995454, 1.000000000000000000),
 ( 1.000000000000000000, 0.5278258667060209408, 1.000000000000000000),
 ( 1.000000000000000000, 0.4993418825331956135, 1.000000000000000000),
 ( 1.000000000000000000, 0.4999999999999739098, 1.000000000000000000) ) ) 
 REPRESENTATION_ITEM ( '' )  SURFACE ( )  );
#54647 = ORIENTED_EDGE ( 'NONE', *, *, #156357, .F. ) ;
#54646 = CARTESIAN_POINT ( 'NONE',  ( 20.94999999999999574, -1.162701749926853712, -41.50000000000000000 ) ) ;
#54648 = CARTESIAN_POINT ( 'NONE',  ( -21.55000000000000071, 68.65000000001229807, -157.7731074845244166 ) ) ;
#54649 = ORIENTED_EDGE ( 'NONE', *, *, #38397, .T. ) ;
#54651 = CARTESIAN_POINT ( 'NONE',  ( 21.93340585971692747, 7.324147022868173984, -100.5000000000000426 ) ) ;
#54650 = VECTOR ( 'NONE', #161647, 1000.000000000000000 ) ;
#54652 = ORIENTED_EDGE ( 'NONE', *, *, #104808, .F. ) ;
#54653 = CARTESIAN_POINT ( 'NONE',  ( -18.50000000000000000, -0.5913595841389538421, -242.4574432119242999 ) ) ;
#54654 = EDGE_CURVE ( 'NONE', #191384, #204466, #172183, .T. ) ;
#54655 = EDGE_CURVE ( 'NONE', #148073, #241077, #231179, .T. ) ;
#54656 = AXIS2_PLACEMENT_3D ( 'NONE', #147819, #48695, #244325 ) ;
#54657 = ORIENTED_EDGE ( 'NONE', *, *, #181583, .T. ) ;
#54659 = AXIS2_PLACEMENT_3D ( 'NONE', #133800, #210776, #110388 ) ;
#54658 = DIRECTION ( 'NONE',  ( 0.000000000000000000, 0.4088369013363296611, -0.9126074666063762608 ) ) ;
#54660 = LINE ( 'NONE', #212477, #177862 ) ;
#54661 = ADVANCED_FACE ( 'NONE', ( #250707 ), #229874, .F. ) ;
#54663 = VERTEX_POINT ( 'NONE', #210317 ) ;
#54662 = ORIENTED_EDGE ( 'NONE', *, *, #85843, .T. ) ;
#54664 = ORIENTED_EDGE ( 'NONE', *, *, #78839, .F. ) ;
#54667 = EDGE_CURVE ( 'NONE', #211757, #236891, #111209, .T. ) ;
#54666 = CARTESIAN_POINT ( 'NONE',  ( -18.50000000000000000, 11.75000000001115197, -167.5999999999999659 ) ) ;
#54665 = AXIS2_PLACEMENT_3D ( 'NONE', #141056, #19835, #143611 ) ;
#54668 = ORIENTED_EDGE ( 'NONE', *, *, #94979, .F. ) ;
#54669 = ORIENTED_EDGE ( 'NONE', *, *, #227368, .T. ) ;
#54670 = DIRECTION ( 'NONE',  ( 1.000000000000000000, 0.000000000000000000, 0.000000000000000000 ) ) ;
#54671 = VECTOR ( 'NONE', #35248, 1000.000000000000000 ) ;
#54673 = EDGE_LOOP ( 'NONE', ( #38193, #143543, #143554, #242988 ) ) ;
#54672 = DIRECTION ( 'NONE',  ( -1.000000000000000000, 0.000000000000000000, 0.000000000000000000 ) ) ;
#54674 = DIRECTION ( 'NONE',  ( -1.000000000000000000, -0.000000000000000000, -0.000000000000000000 ) ) ;
#54675 = EDGE_CURVE ( 'NONE', #142779, #239027, #73206, .T. ) ;
#54677 = DIRECTION ( 'NONE',  ( 1.000000000000000000, 0.000000000000000000, 0.000000000000000000 ) ) ;
#54676 = DIRECTION ( 'NONE',  ( 0.000000000000000000, 0.9876197685951252359, -0.1568667991644863424 ) ) ;
#54678 = CARTESIAN_POINT ( 'NONE',  ( 23.14999999999999858, 3.318160649989770672, -234.5626251938229245 ) ) ;
#54679 = CARTESIAN_POINT ( 'NONE',  ( 18.47654891039378811, -9.465274948371156682, -74.12597590519470714 ) ) ;
#54680 = DIRECTION ( 'NONE',  ( -1.000000000000000000, -0.000000000000000000, -0.000000000000000000 ) ) ;
#54681 = ORIENTED_EDGE ( 'NONE', *, *, #251919, .T. ) ;
#54682 = CIRCLE ( 'NONE', #229666, 0.1000000000000028644 ) ;
#54683 = ORIENTED_EDGE ( 'NONE', *, *, #97080, .F. ) ;
#54684 = CARTESIAN_POINT ( 'NONE',  ( 18.31572054635706692, 85.54847543579089120, -96.17253731977575626 ) ) ;
#54685 = CARTESIAN_POINT ( 'NONE',  ( 20.94999999999999929, 28.63831050940605394, -258.0693639473472558 ) ) ;
#54687 = EDGE_CURVE ( 'NONE', #172274, #137741, #60677, .T. ) ;
#54686 = CYLINDRICAL_SURFACE ( 'NONE', #49710, 0.1000000000000028644 ) ;
#54689 = VERTEX_POINT ( 'NONE', #217979 ) ;
#54688 = AXIS2_PLACEMENT_3D ( 'NONE', #12895, #33762, #251468 ) ;
#54690 = DIRECTION ( 'NONE',  ( 0.000000000000000000, 0.9651348961777379554, -0.2617529984164210233 ) ) ;
#54691 = ADVANCED_FACE ( 'NONE', ( #138440 ), #205420, .F. ) ;
#54693 = ADVANCED_FACE ( 'NONE', ( #34273 ), #152936, .T. ) ;
#54692 = AXIS2_PLACEMENT_3D ( 'NONE', #186414, #127717, #84684 ) ;
#54694 = DIRECTION ( 'NONE',  ( 0.000000000000000000, 1.000000000000000000, 0.000000000000000000 ) ) ;
#54695 = FACE_OUTER_BOUND ( 'NONE', #225354, .T. ) ;
#54696 = EDGE_LOOP ( 'NONE', ( #82364, #48200, #234366, #227195 ) ) ;
#54697 = EDGE_LOOP ( 'NONE', ( #2441, #51848, #75686 ) ) ;
#54698 = EDGE_CURVE ( 'NONE', #107411, #97198, #6016, .T. ) ;
#54699 = DIRECTION ( 'NONE',  ( -0.000000000000000000, -6.982962677686266711E-15, 1.000000000000000000 ) ) ;
#54700 = DIRECTION ( 'NONE',  ( 0.000000000000000000, 1.000000000000000000, 0.000000000000000000 ) ) ;
#54701 = EDGE_LOOP ( 'NONE', ( #235199, #35421, #190225, #253662 ) ) ;
#54702 = CARTESIAN_POINT ( 'NONE',  ( 20.94999999999999929, 4.813084112160684214, -55.05848224347618469 ) ) ;
#54703 = ORIENTED_EDGE ( 'NONE', *, *, #168603, .F. ) ;
#54704 = CARTESIAN_POINT ( 'NONE',  ( -21.59142135623730852, 68.15000000001253966, -182.2731074845244166 ) ) ;
#54706 = CIRCLE ( 'NONE', #158784, 0.2000000000000057288 ) ;
#54705 = FACE_OUTER_BOUND ( 'NONE', #190061, .T. ) ;
#54707 = LINE ( 'NONE', #235900, #28175 ) ;
#54708 = EDGE_CURVE ( 'NONE', #148702, #223782, #51438, .T. ) ;
#54710 = EDGE_CURVE ( 'NONE', #203487, #104152, #192990, .T. ) ;
#54709 = CARTESIAN_POINT ( 'NONE',  ( 18.50016250449482413, 65.70233904877169095, -164.5487410911965469 ) ) ;
#54711 = PLANE ( 'NONE',  #86902 ) ;
#54712 = EDGE_CURVE ( 'NONE', #168194, #86723, #96744, .T. ) ;
#54713 = CARTESIAN_POINT ( 'NONE',  ( -21.05000000000000071, 74.16465844978819177, -191.8679561919614116 ) ) ;
#54714 = AXIS2_PLACEMENT_3D ( 'NONE', #95001, #19318, #194132 ) ;
#54715 = CIRCLE ( 'NONE', #167182, 0.4999999999999944489 ) ;
#54717 = ORIENTED_EDGE ( 'NONE', *, *, #202684, .T. ) ;
#54716 = ORIENTED_EDGE ( 'NONE', *, *, #35219, .T. ) ;
#54718 = ORIENTED_EDGE ( 'NONE', *, *, #48549, .T. ) ;
#54719 = DIRECTION ( 'NONE',  ( 0.000000000000000000, 1.000000000000000000, 0.000000000000000000 ) ) ;
#54720 = CARTESIAN_POINT ( 'NONE',  ( 20.94999999999999929, 7.783179459866048866, -245.3643104511423303 ) ) ;
#54721 = CYLINDRICAL_SURFACE ( 'NONE', #34337, 14.30833333333333890 ) ;
#54722 = EDGE_CURVE ( 'NONE', #47267, #33310, #188683, .T. ) ;
#54723 =( BOUNDED_CURVE ( )  B_SPLINE_CURVE ( 3, ( #31174, #49413, #33748, #128957 ),
 .UNSPECIFIED., .F., .F. ) 
 B_SPLINE_CURVE_WITH_KNOTS ( ( 4, 4 ),
 ( 3.192897208853992641, 4.712388980384691450 ),
 .UNSPECIFIED. ) 
 CURVE ( )  GEOMETRIC_REPRESENTATION_ITEM ( )  RATIONAL_B_SPLINE_CURVE ( ( 1.000000000000000000, 0.8166740347213222728, 0.8166740347213222728, 1.000000000000000000 ) ) 
 REPRESENTATION_ITEM ( '' )  );
#54725 = CARTESIAN_POINT ( 'NONE',  ( -12.84409460144754078, 66.58931770574392317, -87.59196404257612301 ) ) ;
#54724 = CARTESIAN_POINT ( 'NONE',  ( -21.05000000000000071, 26.34542992457388522, -244.0265060370938954 ) ) ;
#54726 = PLANE ( 'NONE',  #166537 ) ;
#54727 = ORIENTED_EDGE ( 'NONE', *, *, #234528, .T. ) ;
#54728 = DIRECTION ( 'NONE',  ( 0.000000000000000000, -0.1298341882520124002, -0.9915357197604841577 ) ) ;
#54729 = ORIENTED_EDGE ( 'NONE', *, *, #52196, .F. ) ;
#54730 = ORIENTED_EDGE ( 'NONE', *, *, #72374, .T. ) ;
#54731 = DIRECTION ( 'NONE',  ( -0.000000000000000000, 0.000000000000000000, -1.000000000000000000 ) ) ;
#54732 = CARTESIAN_POINT ( 'NONE',  ( -23.25000000000000000, 4.150000000011156764, -155.2500000000000284 ) ) ;
#54733 = CARTESIAN_POINT ( 'NONE',  ( 21.07094088545369814, 75.90110629746051529, -209.8432747064415196 ) ) ;
#54734 = CARTESIAN_POINT ( 'NONE',  ( -21.05000000000000071, 86.32947205150912851, -209.3293116780858156 ) ) ;
#54735 = CARTESIAN_POINT ( 'NONE',  ( -20.64999999999999858, 1.115600667400684642E-11, -67.00000000000000000 ) ) ;
#54736 = ORIENTED_EDGE ( 'NONE', *, *, #223473, .T. ) ;
#54737 = ORIENTED_EDGE ( 'NONE', *, *, #149311, .T. ) ;
#54738 = CYLINDRICAL_SURFACE ( 'NONE', #235276, 0.09999999999999939493 ) ;
#54739 = FACE_OUTER_BOUND ( 'NONE', #135748, .T. ) ;
#54740 = DIRECTION ( 'NONE',  ( 1.000000000000000000, -0.000000000000000000, -0.000000000000000000 ) ) ;
#54741 = DIRECTION ( 'NONE',  ( 0.000000000000000000, 0.000000000000000000, -1.000000000000000000 ) ) ;
#54742 = CARTESIAN_POINT ( 'NONE',  ( 22.47071067811865319, 76.00000000001237765, -170.0231074845243597 ) ) ;
#54743 = DIRECTION ( 'NONE',  ( 0.000000000000000000, 6.982962677686266711E-15, -1.000000000000000000 ) ) ;
#54744 = AXIS2_PLACEMENT_3D ( 'NONE', #183253, #164968, #82822 ) ;
#54745 = DIRECTION ( 'NONE',  ( 1.000000000000000000, 0.000000000000000000, 0.000000000000000000 ) ) ;
#54747 = SPHERICAL_SURFACE ( 'NONE', #99731, 0.1000000000000000056 ) ;
#54746 = DIRECTION ( 'NONE',  ( 0.000000000000000000, 0.000000000000000000, 1.000000000000000000 ) ) ;
#54748 = CARTESIAN_POINT ( 'NONE',  ( -20.54999999999999716, 1.940186915899009490, -146.8291192110533530 ) ) ;
#54749 = CARTESIAN_POINT ( 'NONE',  ( -23.25000000000000000, 76.00000000001165290, -69.52310748452431710 ) ) ;
#54750 = EDGE_CURVE ( 'NONE', #39792, #135788, #176247, .T. ) ;
#54751 = DIRECTION ( 'NONE',  ( 1.000000000000000000, 0.000000000000000000, 0.000000000000000000 ) ) ;
#54752 = LINE ( 'NONE', #69217, #223305 ) ;
#54754 = VERTEX_POINT ( 'NONE', #58900 ) ;
#54753 = LINE ( 'NONE', #173488, #98924 ) ;
#54755 = ADVANCED_FACE ( 'NONE', ( #173807 ), #74689, .F. ) ;
#54756 =( BOUNDED_SURFACE ( )  B_SPLINE_SURFACE ( 3, 2, ( 
 ( #78795, #240464, #39726 ),
 ( #159651, #61834, #60525 ),
 ( #141360, #220886, #140055 ),
 ( #219601, #42272, #44832 ),
 ( #126938, #87786, #207781 ),
 ( #27872, #206474, #107362 ),
 ( #186938, #129510, #209041 ),
 ( #46106, #29168, #8287 ),
 ( #145199, #167376, #128227 ),
 ( #25287, #225998, #124379 ) ),
 .UNSPECIFIED., .F., .F., .F. ) 
 B_SPLINE_SURFACE_WITH_KNOTS ( ( 4, 2, 2, 2, 4 ),
 ( 3, 3 ),
 ( 0.002161241639767248670, 0.002579950749615824400, 0.002789305304540112482, 0.002893982582002256523, 0.002998659859464400564 ),
 ( 0.000000000000000000, 1.000000000000000000 ),
 .UNSPECIFIED. ) 
 GEOMETRIC_REPRESENTATION_ITEM ( )  RATIONAL_B_SPLINE_SURFACE ( (
 ( 1.000000000000000000, 0.7071067811865475727, 1.000000000000000000),
 ( 1.000000000000000000, 0.7632447400665458570, 1.000000000000000000),
 ( 1.000000000000000000, 0.8158073005108548159, 1.000000000000000000),
 ( 1.000000000000000000, 0.8906973462396701180, 1.000000000000000000),
 ( 1.000000000000000000, 0.9149408947804109626, 1.000000000000000000),
 ( 1.000000000000000000, 0.9493368785273814670, 1.000000000000000000),
 ( 1.000000000000000000, 0.9605194247155347531, 1.000000000000000000),
 ( 1.000000000000000000, 0.9803630264782571269, 1.000000000000000000),
 ( 1.000000000000000000, 0.9900844824270105260, 1.000000000000000000),
 ( 1.000000000000000000, 0.9894588281429241849, 1.000000000000000000) ) ) 
 REPRESENTATION_ITEM ( '' )  SURFACE ( )  );
#54757 = CIRCLE ( 'NONE', #137942, 0.2000000000000000944 ) ;
#54758 = DIRECTION ( 'NONE',  ( -1.836970198721029934E-16, -0.4088369013363280513, 0.9126074666063769270 ) ) ;
#54759 = ORIENTED_EDGE ( 'NONE', *, *, #192042, .F. ) ;
#54760 = DIRECTION ( 'NONE',  ( 1.000000000000000000, 0.000000000000000000, -0.000000000000000000 ) ) ;
#54761 = DIRECTION ( 'NONE',  ( 0.000000000000000000, -0.9126074666063757057, -0.4088369013363309379 ) ) ;
#54762 = EDGE_CURVE ( 'NONE', #82771, #173389, #238767, .T. ) ;
#54763 = CARTESIAN_POINT ( 'NONE',  ( 25.10847955711010115, 9.068702471349586958, -347.0000000000001137 ) ) ;
#54764 = CARTESIAN_POINT ( 'NONE',  ( 21.05000000000000071, -9.499999999988848032, -76.89396912265249284 ) ) ;
#54765 = AXIS2_PLACEMENT_3D ( 'NONE', #107665, #28168, #30734 ) ;
#54766 = AXIS2_PLACEMENT_3D ( 'NONE', #166028, #184271, #65608 ) ;
#54767 = CARTESIAN_POINT ( 'NONE',  ( -20.94999999999999929, 74.16465844978787914, -158.3679561919613832 ) ) ;
#54768 = CARTESIAN_POINT ( 'NONE',  ( 18.58719872626880587, 85.56664439761028973, -62.70062928812723868 ) ) ;
#54770 = CYLINDRICAL_SURFACE ( 'NONE', #211024, 0.1000000000000028644 ) ;
#54769 = CIRCLE ( 'NONE', #175592, 0.09999999999999892308 ) ;
#54771 = VERTEX_POINT ( 'NONE', #175082 ) ;
#54772 = DIRECTION ( 'NONE',  ( 1.000000000000000000, 0.000000000000000000, 0.000000000000000000 ) ) ;
#54774 = ORIENTED_EDGE ( 'NONE', *, *, #108751, .F. ) ;
#54773 = FACE_OUTER_BOUND ( 'NONE', #228539, .T. ) ;
#54775 = DIRECTION ( 'NONE',  ( 0.000000000000000000, 0.000000000000000000, -1.000000000000000000 ) ) ;
#54776 = FACE_OUTER_BOUND ( 'NONE', #1391, .T. ) ;
#54777 = CARTESIAN_POINT ( 'NONE',  ( -22.49533356619865643, 31.83654316555210784, -238.9459102234746695 ) ) ;
#54778 = EDGE_LOOP ( 'NONE', ( #163314, #22748, #240782, #149065 ) ) ;
#54779 = LINE ( 'NONE', #33991, #213603 ) ;
#54780 = APPLICATION_PROTOCOL_DEFINITION ( 'draft international standard', 'automotive_design', 1998, #192501 ) ;
#54781 = CARTESIAN_POINT ( 'NONE',  ( 22.49999999999999645, 11.36547683798393393, -198.4402660583091063 ) ) ;
#54782 = CARTESIAN_POINT ( 'NONE',  ( -18.49346865148321584, 85.44307379853681539, -95.83791122920942485 ) ) ;
#54783 = CIRCLE ( 'NONE', #200534, 11.89999999999999858 ) ;
#54784 = EDGE_LOOP ( 'NONE', ( #53464, #236034, #240046, #237775 ) ) ;
#54785 = DIRECTION ( 'NONE',  ( 1.000000000000000000, 0.000000000000000000, -0.000000000000000000 ) ) ;
#54786 = DIRECTION ( 'NONE',  ( -1.000000000000000000, 0.000000000000000000, 0.000000000000000000 ) ) ;
#54787 = DIRECTION ( 'NONE',  ( 0.000000000000000000, 0.4721928772777352346, 0.8814952561688428334 ) ) ;
#54788 = ORIENTED_EDGE ( 'NONE', *, *, #27012, .F. ) ;
#54789 = VERTEX_POINT ( 'NONE', #137181 ) ;
#54790 = LINE ( 'NONE', #249169, #221603 ) ;
#54791 = ADVANCED_FACE ( 'NONE', ( #98026 ), #177631, .F. ) ;
#54792 = CARTESIAN_POINT ( 'NONE',  ( 23.14999999999998437, 1.580567032079710055, -244.0902705724231794 ) ) ;
#54793 = CARTESIAN_POINT ( 'NONE',  ( -20.94999999999999929, 1.115600667400684642E-11, -189.2999999999999545 ) ) ;
#54795 = CARTESIAN_POINT ( 'NONE',  ( 22.60000000000000142, 75.89914163091376054, -181.7726746080137445 ) ) ;
#54794 = AXIS2_PLACEMENT_3D ( 'NONE', #201119, #137284, #79860 ) ;
#54796 = CIRCLE ( 'NONE', #200549, 0.1000000000000124678 ) ;
#54797 = ADVANCED_FACE ( 'NONE', ( #202300 ), #79751, .F. ) ;
#54800 = DIRECTION ( 'NONE',  ( 0.000000000000000000, 0.000000000000000000, 1.000000000000000000 ) ) ;
#54799 = VECTOR ( 'NONE', #110265, 1000.000000000000000 ) ;
#54798 = CARTESIAN_POINT ( 'NONE',  ( 23.14999999999999858, 1.115600667400684642E-11, -134.0000000000000284 ) ) ;
#54801 = FACE_OUTER_BOUND ( 'NONE', #185118, .T. ) ;
#54802 = CARTESIAN_POINT ( 'NONE',  ( 21.05000000000000071, 48.05226059848062192, -246.4732437245379231 ) ) ;
#54803 = DIRECTION ( 'NONE',  ( 0.000000000000000000, 0.2128009952263650861, -0.9770955615653305060 ) ) ;
#54804 = ORIENTED_EDGE ( 'NONE', *, *, #114999, .T. ) ;
#54805 = EDGE_LOOP ( 'NONE', ( #110338, #163108, #24189, #92750 ) ) ;
#54806 = CARTESIAN_POINT ( 'NONE',  ( -23.15000000000000213, -8.663551401858004652, -177.0241011180672785 ) ) ;
#54807 = DIRECTION ( 'NONE',  ( -1.000000000000000000, -0.000000000000000000, -0.000000000000000000 ) ) ;
#54809 = DIRECTION ( 'NONE',  ( -1.000000000000000000, -0.000000000000000000, 0.000000000000000000 ) ) ;
#54808 = LINE ( 'NONE', #195644, #142260 ) ;
#54810 = EDGE_CURVE ( 'NONE', #81259, #234897, #124058, .T. ) ;
#54811 = DIRECTION ( 'NONE',  ( 0.000000000000000000, -1.000000000000000000, 0.000000000000000000 ) ) ;
#54812 = CARTESIAN_POINT ( 'NONE',  ( 19.94784844284961167, 64.28691006698306865, -111.8209087672259017 ) ) ;
#54813 = FACE_OUTER_BOUND ( 'NONE', #21673, .T. ) ;
#54814 = ADVANCED_FACE ( 'NONE', ( #45786 ), #24968, .T. ) ;
#54815 = ORIENTED_EDGE ( 'NONE', *, *, #133059, .T. ) ;
#54816 = EDGE_CURVE ( 'NONE', #217495, #118818, #19830, .T. ) ;
#54818 = ORIENTED_EDGE ( 'NONE', *, *, #166415, .T. ) ;
#54817 = AXIS2_PLACEMENT_3D ( 'NONE', #170643, #135289, #190165 ) ;
#54819 = DIRECTION ( 'NONE',  ( 7.304098846218134667E-16, 1.000000000000000000, -0.000000000000000000 ) ) ;
#54820 = EDGE_CURVE ( 'NONE', #122321, #254423, #134696, .T. ) ;
#54821 = VERTEX_POINT ( 'NONE', #240148 ) ;
#54822 = DIRECTION ( 'NONE',  ( -4.408576920032448588E-17, 0.1350103645451876666, -0.9908441862701600211 ) ) ;
#54823 = DIRECTION ( 'NONE',  ( 0.000000000000000000, 0.4930308989874980785, 0.8700118002898462599 ) ) ;
#54824 = CARTESIAN_POINT ( 'NONE',  ( 21.04999999999999716, 8.872080675388993143, -142.5210474188322962 ) ) ;
#54825 = VERTEX_POINT ( 'NONE', #203580 ) ;
#54826 = CARTESIAN_POINT ( 'NONE',  ( 21.05000000000000071, 84.66355140188123585, -126.9990063664569391 ) ) ;
#54827 = EDGE_CURVE ( 'NONE', #53690, #139621, #41961, .T. ) ;
#54828 = CIRCLE ( 'NONE', #200589, 0.1999999999999987899 ) ;
#54829 = PLANE ( 'NONE',  #203600 ) ;
#54830 = DIRECTION ( 'NONE',  ( 0.000000000000000000, -0.7965107556683636014, 0.6046243595031649543 ) ) ;
#54831 = AXIS2_PLACEMENT_3D ( 'NONE', #86142, #146141, #206128 ) ;
#54832 = CARTESIAN_POINT ( 'NONE',  ( -16.87683809663752399, 62.98531230502843670, -213.8799296553602005 ) ) ;
#54833 = CARTESIAN_POINT ( 'NONE',  ( 20.04142135623730070, 64.25000000001250555, -178.8731074845244393 ) ) ;
#54835 = DIRECTION ( 'NONE',  ( 1.000000000000000000, 0.000000000000000000, 0.000000000000000000 ) ) ;
#54834 = DIRECTION ( 'NONE',  ( 0.000000000000000000, 0.2617529984164915779, 0.9651348961777189706 ) ) ;
#54837 = CARTESIAN_POINT ( 'NONE',  ( -20.85000000000000142, 64.25000000001148237, -42.80697314750250371 ) ) ;
#54836 = VECTOR ( 'NONE', #112232, 1000.000000000000000 ) ;
#54838 = ORIENTED_EDGE ( 'NONE', *, *, #12376, .T. ) ;
#54840 = DIRECTION ( 'NONE',  ( 1.000000000000000000, 0.000000000000000000, 0.000000000000000000 ) ) ;
#54839 = DIRECTION ( 'NONE',  ( -0.000000000000000000, -6.982962677686266711E-15, 1.000000000000000000 ) ) ;
#54841 = ORIENTED_EDGE ( 'NONE', *, *, #225689, .T. ) ;
#54843 = ORIENTED_EDGE ( 'NONE', *, *, #44511, .T. ) ;
#54842 = CARTESIAN_POINT ( 'NONE',  ( 21.14999999999998082, -11.74999999998884448, -67.00000000000004263 ) ) ;
#54844 = ORIENTED_EDGE ( 'NONE', *, *, #169067, .T. ) ;
#54845 = CARTESIAN_POINT ( 'NONE',  ( -16.85718274719486587, 9.976142314632873820, -146.5633463321825616 ) ) ;
#54846 = CARTESIAN_POINT ( 'NONE',  ( 21.10000000000000142, -1.720267447010333833E-15, 11.89999999999999858 ) ) ;
#54847 = CARTESIAN_POINT ( 'NONE',  ( 18.59999999999999432, 65.50857864377445594, -78.27310748452438816 ) ) ;
#54848 = DIRECTION ( 'NONE',  ( 0.000000000000000000, 0.6728971962616869806, -0.7397360091702719354 ) ) ;
#54849 = CIRCLE ( 'NONE', #200610, 0.09999999999999939493 ) ;
#54850 = ORIENTED_EDGE ( 'NONE', *, *, #2264, .T. ) ;
#54851 = DIRECTION ( 'NONE',  ( 0.000000000000000000, 0.000000000000000000, 1.000000000000000000 ) ) ;
#54852 = ORIENTED_EDGE ( 'NONE', *, *, #122772, .F. ) ;
#54853 = AXIS2_PLACEMENT_3D ( 'NONE', #243626, #225324, #83241 ) ;
#54854 = DIRECTION ( 'NONE',  ( 0.000000000000000000, 0.000000000000000000, 1.000000000000000000 ) ) ;
#54855 = CIRCLE ( 'NONE', #184042, 0.09999999999999939493 ) ;
#54856 = CARTESIAN_POINT ( 'NONE',  ( -16.94107738177414291, 51.68386028857255354, -231.8469600742508021 ) ) ;
#54857 = AXIS2_PLACEMENT_3D ( 'NONE', #62260, #230309, #188616 ) ;
#54858 = ORIENTED_EDGE ( 'NONE', *, *, #250346, .F. ) ;
#54859 = ORIENTED_EDGE ( 'NONE', *, *, #86724, .F. ) ;
#54860 = DIRECTION ( 'NONE',  ( 1.000000000000000000, -0.000000000000000000, -0.000000000000000000 ) ) ;
#54861 = AXIS2_PLACEMENT_3D ( 'NONE', #182244, #180958, #106520 ) ;
#54862 = ADVANCED_FACE ( 'NONE', ( #199753 ), #99317, .T. ) ;
#54863 = VERTEX_POINT ( 'NONE', #242697 ) ;
#54864 = CARTESIAN_POINT ( 'NONE',  ( -18.40000000000000213, 64.52683809664949877, -112.3490535513323323 ) ) ;
#54865 = ORIENTED_EDGE ( 'NONE', *, *, #222530, .T. ) ;
#54866 = CARTESIAN_POINT ( 'NONE',  ( 22.60000000000000142, 12.58798907299599179, -223.3278890275437050 ) ) ;
#54867 = AXIS2_PLACEMENT_3D ( 'NONE', #165119, #206812, #163839 ) ;
#54868 = DIRECTION ( 'NONE',  ( 1.186688945009010077E-16, -1.000000000000000000, -0.000000000000000000 ) ) ;
#54869 = CARTESIAN_POINT ( 'NONE',  ( 21.05000000000000071, 60.92751661265764795, -225.4207664198654015 ) ) ;
#54871 = EDGE_CURVE ( 'NONE', #141855, #9223, #84873, .T. ) ;
#54870 = AXIS2_PLACEMENT_3D ( 'NONE', #220711, #117753, #98155 ) ;
#54872 = CARTESIAN_POINT ( 'NONE',  ( 20.94999999999999929, 61.95000000001248708, -175.5368025552853624 ) ) ;
#54873 = EDGE_CURVE ( 'NONE', #222093, #24156, #61510, .T. ) ;
#54874 = ADVANCED_FACE ( 'NONE', ( #238857 ), #81040, .F. ) ;
#54875 = CARTESIAN_POINT ( 'NONE',  ( 21.30000000000002558, 1.115600667400684642E-11, -33.50000000000000000 ) ) ;
#54876 = DIRECTION ( 'NONE',  ( -0.000000000000000000, 0.9770955615653313941, 0.2128009952263603954 ) ) ;
#54877 = DIRECTION ( 'NONE',  ( 1.000000000000000000, -0.000000000000000000, 0.000000000000000000 ) ) ;
#54878 = AXIS2_PLACEMENT_3D ( 'NONE', #43644, #44929, #64492 ) ;
#54879 = EDGE_LOOP ( 'NONE', ( #76243, #101058, #22826, #233965 ) ) ;
#54881 = CARTESIAN_POINT ( 'NONE',  ( 20.05000000000002913, 68.75000000001178080, -82.17310748452436542 ) ) ;
#54880 = CARTESIAN_POINT ( 'NONE',  ( -18.40000000000000213, 54.09900352584865857, -229.1663746252470446 ) ) ;
#54882 = ORIENTED_EDGE ( 'NONE', *, *, #90224, .T. ) ;
#54885 = ORIENTED_EDGE ( 'NONE', *, *, #77257, .F. ) ;
#54884 = DIRECTION ( 'NONE',  ( -0.000000000000000000, 0.4088369013363281068, -0.9126074666063770380 ) ) ;
#54883 = DIRECTION ( 'NONE',  ( 2.952720810173289112E-16, -1.000000000000000000, 0.000000000000000000 ) ) ;
#54886 = AXIS2_PLACEMENT_3D ( 'NONE', #32092, #225105, #46475 ) ;
#54887 = VERTEX_POINT ( 'NONE', #144875 ) ;
#54888 = DIRECTION ( 'NONE',  ( 0.000000000000000000, 0.000000000000000000, 1.000000000000000000 ) ) ;
#54889 = AXIS2_PLACEMENT_3D ( 'NONE', #54735, #251658, #36493 ) ;
#54890 = CARTESIAN_POINT ( 'NONE',  ( 21.13435531349813701, 1.115486826172573664E-11, -60.50627893640798050 ) ) ;
#54891 = CARTESIAN_POINT ( 'NONE',  ( 23.14999999999999147, 1.115600667400684642E-11, -67.00000000000004263 ) ) ;
#54892 = CARTESIAN_POINT ( 'NONE',  ( -23.15000000000000213, 4.350000000011156054, -88.25000000000005684 ) ) ;
#54893 = ORIENTED_EDGE ( 'NONE', *, *, #69917, .T. ) ;
#54895 = EDGE_LOOP ( 'NONE', ( #199627, #34030, #141048, #149643 ) ) ;
#54894 = DIRECTION ( 'NONE',  ( 0.000000000000000000, -8.717686153663073805E-15, 1.000000000000000000 ) ) ;
#54896 = EDGE_CURVE ( 'NONE', #59470, #42819, #121504, .T. ) ;
#54897 = EDGE_CURVE ( 'NONE', #225036, #178041, #241433, .T. ) ;
#54899 = DIRECTION ( 'NONE',  ( 1.000000000000000000, -0.000000000000000000, -0.000000000000000000 ) ) ;
#54898 = CARTESIAN_POINT ( 'NONE',  ( 20.94999999999999929, 85.40000000001198543, -112.9170766071766820 ) ) ;
#54901 = ORIENTED_EDGE ( 'NONE', *, *, #171673, .F. ) ;
#54900 = DIRECTION ( 'NONE',  ( 0.000000000000000000, -0.8814952561688513821, 0.4721928772777189698 ) ) ;
#54902 = ORIENTED_EDGE ( 'NONE', *, *, #89182, .F. ) ;
#54903 = CIRCLE ( 'NONE', #229711, 0.2000000000000057288 ) ;
#54904 = FACE_OUTER_BOUND ( 'NONE', #172598, .T. ) ;
#54905 = CARTESIAN_POINT ( 'NONE',  ( -20.94999999999999929, 76.00000000001267608, -203.5231074845243597 ) ) ;
#54906 = ORIENTED_EDGE ( 'NONE', *, *, #180695, .T. ) ;
#54907 = DIRECTION ( 'NONE',  ( 1.000000000000000000, 0.000000000000000000, -0.000000000000000000 ) ) ;
#54908 = ORIENTED_EDGE ( 'NONE', *, *, #157263, .F. ) ;
#54909 = EDGE_CURVE ( 'NONE', #120853, #123327, #88903, .T. ) ;
#54911 = EDGE_CURVE ( 'NONE', #41259, #226219, #126328, .T. ) ;
#54910 = CARTESIAN_POINT ( 'NONE',  ( -23.15000000000000213, 19.73066058418984170, -238.2142830767208466 ) ) ;
#54912 = CARTESIAN_POINT ( 'NONE',  ( 20.04142135623730070, 11.65000000001115943, -122.2500000000000284 ) ) ;
#54913 = EDGE_CURVE ( 'NONE', #50622, #121769, #130431, .T. ) ;
#54914 = VERTEX_POINT ( 'NONE', #243981 ) ;
#54915 = LINE ( 'NONE', #254387, #25182 ) ;
#54916 = DIRECTION ( 'NONE',  ( 0.000000000000000000, -6.982962677686267499E-15, 1.000000000000000000 ) ) ;
#54918 = ORIENTED_EDGE ( 'NONE', *, *, #200962, .F. ) ;
#54917 = VECTOR ( 'NONE', #142031, 1000.000000000000000 ) ;
#54919 = ORIENTED_EDGE ( 'NONE', *, *, #156602, .T. ) ;
#54920 = CARTESIAN_POINT ( 'NONE',  ( 18.43565242384934422, -9.519327731081284938, -107.4729763765593731 ) ) ;
#54921 = ORIENTED_EDGE ( 'NONE', *, *, #72718, .F. ) ;
#54922 = ORIENTED_EDGE ( 'NONE', *, *, #242174, .T. ) ;
#54924 = ORIENTED_EDGE ( 'NONE', *, *, #43760, .T. ) ;
#54923 = CARTESIAN_POINT ( 'NONE',  ( -23.25000000000000000, 85.00000000001149658, -45.31707660717669484 ) ) ;
#54925 = EDGE_LOOP ( 'NONE', ( #187718, #80126, #175524, #26727 ) ) ;
#54926 = DIRECTION ( 'NONE',  ( -0.000000000000000000, -1.000000000000000000, 0.000000000000000000 ) ) ;
#54927 = ORIENTED_EDGE ( 'NONE', *, *, #3453, .F. ) ;
#54931 = ADVANCED_FACE ( 'NONE', ( #184010 ), #234674, .T. ) ;
#54930 = ORIENTED_EDGE ( 'NONE', *, *, #157543, .F. ) ;
#54929 = ORIENTED_EDGE ( 'NONE', *, *, #218440, .T. ) ;
#54928 = CARTESIAN_POINT ( 'NONE',  ( -18.50000000000000000, 26.73568686665825567, -252.5275129665054408 ) ) ;
#54932 = AXIS2_PLACEMENT_3D ( 'NONE', #191752, #13097, #234698 ) ;
#54933 = ORIENTED_EDGE ( 'NONE', *, *, #28896, .F. ) ;
#54934 = VECTOR ( 'NONE', #133430, 1000.000000000000000 ) ;
#54935 = DIRECTION ( 'NONE',  ( 0.000000000000000000, 0.9651348961777118651, -0.2617529984165174461 ) ) ;
#54936 = VERTEX_POINT ( 'NONE', #5350 ) ;
#54937 = EDGE_CURVE ( 'NONE', #184435, #24761, #86169, .T. ) ;
#54938 = FACE_OUTER_BOUND ( 'NONE', #110524, .T. ) ;
#54940 = ORIENTED_EDGE ( 'NONE', *, *, #15429, .F. ) ;
#54939 = CARTESIAN_POINT ( 'NONE',  ( -23.15000000000000213, -11.48912529307605546, -30.50000000000000000 ) ) ;
#54941 = DIRECTION ( 'NONE',  ( 0.000000000000000000, 0.000000000000000000, -1.000000000000000000 ) ) ;
#54942 = ORIENTED_EDGE ( 'NONE', *, *, #200928, .T. ) ;
#54943 = B_SPLINE_CURVE_WITH_KNOTS ( 'NONE', 3,
 ( #209813, #74184, #109406, #108143, #188962, #153740, #131551, #248946, #72895, #233247 ),
 .UNSPECIFIED., .F., .F.,
 ( 4, 3, 3, 4 ),
 ( 3.103167691559091397E-17, 0.0002000000000008536833, 0.001000000000082982687, 0.001967863649483335420 ),
 .UNSPECIFIED. ) ;
#54944 = VERTEX_POINT ( 'NONE', #67921 ) ;
#54945 = EDGE_CURVE ( 'NONE', #87130, #7471, #159661, .T. ) ;
#54946 = DIRECTION ( 'NONE',  ( -1.000000000000000000, -0.000000000000000000, -0.000000000000000000 ) ) ;
#54947 = FACE_OUTER_BOUND ( 'NONE', #190374, .T. ) ;
#54948 = AXIS2_PLACEMENT_3D ( 'NONE', #17762, #20377, #236820 ) ;
#54949 = ADVANCED_FACE ( 'NONE', ( #229575 ), #204845, .F. ) ;
#54950 = ORIENTED_EDGE ( 'NONE', *, *, #118830, .F. ) ;
#54951 = ORIENTED_EDGE ( 'NONE', *, *, #35736, .F. ) ;
#54952 = CARTESIAN_POINT ( 'NONE',  ( 18.59999999999996945, 10.33248238082518711, -39.09484654391314962 ) ) ;
#54953 = DIRECTION ( 'NONE',  ( 0.7071067811865463515, 0.7071067811865487940, 4.937700262164540154E-15 ) ) ;
#54954 = EDGE_CURVE ( 'NONE', #164178, #65545, #122243, .T. ) ;
#54956 = ORIENTED_EDGE ( 'NONE', *, *, #251155, .T. ) ;
#54955 = ORIENTED_EDGE ( 'NONE', *, *, #200067, .F. ) ;
#54957 = EDGE_LOOP ( 'NONE', ( #106052, #211774, #176922, #199499 ) ) ;
#54959 = EDGE_CURVE ( 'NONE', #252010, #86370, #138762, .T. ) ;
#54958 = FACE_OUTER_BOUND ( 'NONE', #93481, .T. ) ;
#54960 = ORIENTED_EDGE ( 'NONE', *, *, #60215, .T. ) ;
#54961 = ORIENTED_EDGE ( 'NONE', *, *, #210, .T. ) ;
#54962 = EDGE_LOOP ( 'NONE', ( #144449, #221618, #168730, #153549 ) ) ;
#54963 = DIRECTION ( 'NONE',  ( 1.000000000000000000, 0.000000000000000000, 0.000000000000000000 ) ) ;
#54964 = LINE ( 'NONE', #74595, #181666 ) ;
#54965 = ORIENTED_EDGE ( 'NONE', *, *, #82467, .T. ) ;
#54966 = AXIS2_PLACEMENT_3D ( 'NONE', #169430, #132842, #211085 ) ;
#54967 = AXIS2_PLACEMENT_3D ( 'NONE', #89131, #172581, #153001 ) ;
#54968 = ORIENTED_EDGE ( 'NONE', *, *, #8817, .F. ) ;
#54969 = VECTOR ( 'NONE', #1857, 1000.000000000000000 ) ;
#54970 = DIRECTION ( 'NONE',  ( -0.000000000000000000, 1.000000000000000000, 1.734723475976807292E-15 ) ) ;
#54971 = ORIENTED_EDGE ( 'NONE', *, *, #156545, .F. ) ;
#54972 = ADVANCED_FACE ( 'NONE', ( #10527 ), #187885, .T. ) ;
#54973 = EDGE_CURVE ( 'NONE', #7521, #228920, #206151, .T. ) ;
#54974 = DIRECTION ( 'NONE',  ( -0.7071067811865127117, -0.7071067811865821007, 0.000000000000000000 ) ) ;
#54975 = ORIENTED_EDGE ( 'NONE', *, *, #62544, .T. ) ;
#54976 = ORIENTED_EDGE ( 'NONE', *, *, #48133, .F. ) ;
#54977 = EDGE_CURVE ( 'NONE', #241591, #38009, #185302, .T. ) ;
#54978 = DIRECTION ( 'NONE',  ( -0.000000000000000000, -1.000000000000000000, -7.272083257015735086E-15 ) ) ;
#54980 = ORIENTED_EDGE ( 'NONE', *, *, #122202, .F. ) ;
#54979 = CARTESIAN_POINT ( 'NONE',  ( -16.89021194854739960, 9.950000000011138823, -121.2425681316043296 ) ) ;
#54981 = DIRECTION ( 'NONE',  ( 1.000000000000000000, 0.000000000000000000, 0.000000000000000000 ) ) ;
#54982 = CARTESIAN_POINT ( 'NONE',  ( 18.59999999999999432, 74.83729825007360148, -61.42310748452432989 ) ) ;
#54983 = CARTESIAN_POINT ( 'NONE',  ( 20.95462737510932882, 65.44321804836833678, -128.9531574279620827 ) ) ;
#54984 = CARTESIAN_POINT ( 'NONE',  ( 18.50000000000000711, 33.77764400792123212, -236.3455570846021203 ) ) ;
#54985 = AXIS2_PLACEMENT_3D ( 'NONE', #166459, #84258, #185985 ) ;
#54986 = DIRECTION ( 'NONE',  ( -4.408576920032446739E-17, -0.8096735173027155286, 0.5868805631290315850 ) ) ;
#54987 = CARTESIAN_POINT ( 'NONE',  ( 21.14999999999999858, 61.95748721176698126, -221.7323031544521541 ) ) ;
#54988 = CARTESIAN_POINT ( 'NONE',  ( -23.25000000000000000, 11.75000000001115552, -160.4851942293460638 ) ) ;
#54989 = CARTESIAN_POINT ( 'NONE',  ( 22.32929514600007792, 10.62008199960298427, -227.0053766058674967 ) ) ;
#54991 = EDGE_CURVE ( 'NONE', #251409, #60900, #31401, .T. ) ;
#54990 = CARTESIAN_POINT ( 'NONE',  ( -16.80100914604134843, 66.05685090590866082, -149.2060633572367863 ) ) ;
#54992 = DIRECTION ( 'NONE',  ( 1.000000000000000000, 2.952720810173289112E-16, -0.000000000000000000 ) ) ;
#54993 = FACE_OUTER_BOUND ( 'NONE', #46070, .T. ) ;
#54994 = EDGE_CURVE ( 'NONE', #120323, #85330, #9225, .T. ) ;
#54995 = ORIENTED_EDGE ( 'NONE', *, *, #75518, .T. ) ;
#54996 = AXIS2_PLACEMENT_3D ( 'NONE', #32916, #17178, #135804 ) ;
#54997 = ADVANCED_FACE ( 'NONE', ( #208735 ), #6652, .T. ) ;
#54999 = ORIENTED_EDGE ( 'NONE', *, *, #233329, .T. ) ;
#54998 = VERTEX_POINT ( 'NONE', #125334 ) ;
#55000 = EDGE_LOOP ( 'NONE', ( #46009, #226030, #122165, #164063 ) ) ;
#55001 = CARTESIAN_POINT ( 'NONE',  ( -21.09813707148783379, 0.03135149954058890492, -94.11493789426334899 ) ) ;
#55002 = AXIS2_PLACEMENT_3D ( 'NONE', #15563, #168234, #69108 ) ;
#55003 = DIRECTION ( 'NONE',  ( 1.000000000000000000, 0.000000000000000000, 0.000000000000000000 ) ) ;
#55005 = PLANE ( 'NONE',  #48733 ) ;
#55004 = DIRECTION ( 'NONE',  ( 0.000000000000000000, 0.000000000000000000, -1.000000000000000000 ) ) ;
#55006 = EDGE_CURVE ( 'NONE', #210749, #39196, #68260, .T. ) ;
#55007 = EDGE_LOOP ( 'NONE', ( #60397, #208724, #104882, #43835 ) ) ;
#55008 = ORIENTED_EDGE ( 'NONE', *, *, #1312, .F. ) ;
#55009 = DIRECTION ( 'NONE',  ( 0.000000000000000000, 0.000000000000000000, -1.000000000000000000 ) ) ;
#55010 = SURFACE_SIDE_STYLE ('',( #113724 ) ) ;
#55011 = FACE_OUTER_BOUND ( 'NONE', #164366, .T. ) ;
#55012 = CIRCLE ( 'NONE', #38467, 0.1000000000000002831 ) ;
#55013 = CARTESIAN_POINT ( 'NONE',  ( -16.87435696428308063, 9.950002462943377424, -180.1499917651665328 ) ) ;
#55014 = AXIS2_PLACEMENT_3D ( 'NONE', #201219, #22606, #105948 ) ;
#55015 = LINE ( 'NONE', #158043, #203787 ) ;
#55016 = ORIENTED_EDGE ( 'NONE', *, *, #257450, .T. ) ;
#55017 = VERTEX_POINT ( 'NONE', #27554 ) ;
#55018 = DIRECTION ( 'NONE',  ( 1.000000000000000000, 0.000000000000000000, 0.000000000000000000 ) ) ;
#55019 = AXIS2_PLACEMENT_3D ( 'NONE', #109299, #49343, #83304 ) ;
#55020 = DIRECTION ( 'NONE',  ( 0.000000000000000000, 1.776356839400188145E-15, 1.000000000000000000 ) ) ;
#55021 = ORIENTED_EDGE ( 'NONE', *, *, #192373, .F. ) ;
#55022 = CARTESIAN_POINT ( 'NONE',  ( -21.14999999999999858, 18.60982576078065520, -226.6665746245395496 ) ) ;
#55024 = ORIENTED_EDGE ( 'NONE', *, *, #138206, .F. ) ;
#55023 = CARTESIAN_POINT ( 'NONE',  ( -20.94999999999999929, -11.48912529306490349, -70.00000000000004263 ) ) ;
#55025 = DIRECTION ( 'NONE',  ( -0.000000000000000000, 7.109473446599835262E-15, -1.000000000000000000 ) ) ;
#55026 = DIRECTION ( 'NONE',  ( 1.000000000000000000, 7.304098846218134667E-16, 5.100424963727256530E-30 ) ) ;
#55028 = VECTOR ( 'NONE', #55018, 1000.000000000000000 ) ;
#55027 = CARTESIAN_POINT ( 'NONE',  ( 21.14999999999999858, 69.35000000001259934, -191.3731074845244109 ) ) ;
#55029 = ORIENTED_EDGE ( 'NONE', *, *, #42173, .F. ) ;
#55030 = DIRECTION ( 'NONE',  ( 0.000000000000000000, 0.000000000000000000, 1.000000000000000000 ) ) ;
#55031 = DIRECTION ( 'NONE',  ( 0.000000000000000000, 1.000000000000000000, 0.000000000000000000 ) ) ;
#55032 = DIRECTION ( 'NONE',  ( 1.000000000000000000, 0.000000000000000000, 0.000000000000000000 ) ) ;
#55033 = AXIS2_PLACEMENT_3D ( 'NONE', #72100, #250713, #13407 ) ;
#55035 = FACE_OUTER_BOUND ( 'NONE', #22365, .T. ) ;
#55034 = CARTESIAN_POINT ( 'NONE',  ( -16.78493832629887095, 66.05416425680792258, -123.8591584654201512 ) ) ;
#55036 = FACE_OUTER_BOUND ( 'NONE', #182535, .T. ) ;
#55038 = CARTESIAN_POINT ( 'NONE',  ( 21.10257677756356287, 0.02495074957913891861, -27.10161825746727260 ) ) ;
#55037 = AXIS2_PLACEMENT_3D ( 'NONE', #24132, #4530, #81477 ) ;
#55039 = FACE_OUTER_BOUND ( 'NONE', #254899, .T. ) ;
#55040 = CARTESIAN_POINT ( 'NONE',  ( 21.93642651522410603, 7.327166239336949438, -33.50000000000000000 ) ) ;
#55041 = ORIENTED_EDGE ( 'NONE', *, *, #8912, .T. ) ;
#55042 = EDGE_LOOP ( 'NONE', ( #141445, #80553, #87928, #41444 ) ) ;
#55043 = EDGE_CURVE ( 'NONE', #105777, #201510, #55743, .T. ) ;
#55044 = DIRECTION ( 'NONE',  ( -0.000000000000000000, 1.000000000000000000, 6.352154140967427193E-15 ) ) ;
#55045 = EDGE_LOOP ( 'NONE', ( #229172, #106642, #69090, #163384 ) ) ;
#55046 = AXIS2_PLACEMENT_3D ( 'NONE', #85216, #203914, #104781 ) ;
#55047 = DIRECTION ( 'NONE',  ( 1.000000000000000000, 0.000000000000000000, 0.000000000000000000 ) ) ;
#55048 = ORIENTED_EDGE ( 'NONE', *, *, #235471, .F. ) ;
#55049 = EDGE_CURVE ( 'NONE', #192458, #170828, #193176, .T. ) ;
#55050 = ORIENTED_EDGE ( 'NONE', *, *, #185197, .T. ) ;
#55051 = DIRECTION ( 'NONE',  ( 0.000000000000000000, 1.000000000000000000, 6.982962677686267499E-15 ) ) ;
#55052 = AXIS2_PLACEMENT_3D ( 'NONE', #54477, #134014, #213548 ) ;
#55053 = ORIENTED_EDGE ( 'NONE', *, *, #35593, .F. ) ;
#55054 =( BOUNDED_SURFACE ( )  B_SPLINE_SURFACE ( 3, 2, ( 
 ( #145109, #180407, #81271 ),
 ( #40923, #4314, #60438 ),
 ( #123008, #5585, #83822 ),
 ( #1744, #163415, #64307 ),
 ( #198676, #201237, #241657 ),
 ( #141274, #224652, #103405 ) ),
 .UNSPECIFIED., .F., .F., .T. ) 
 B_SPLINE_SURFACE_WITH_KNOTS ( ( 4, 2, 4 ),
 ( 3, 3 ),
 ( 0.0001792624049599606851, 0.0003686986002125007805, 0.0005581347954650409029 ),
 ( 0.000000000000000000, 1.000000000000000000 ),
 .UNSPECIFIED. ) 
 GEOMETRIC_REPRESENTATION_ITEM ( )  RATIONAL_B_SPLINE_SURFACE ( (
 ( 1.000000000000000000, 0.9238795325112759693, 1.000000000000000000),
 ( 1.000000000000000000, 0.9229318695234719483, 1.000000000000000000),
 ( 1.000000000000000000, 0.8926288119235574747, 1.000000000000000000),
 ( 1.000000000000000000, 0.8123777807266254758, 1.000000000000000000),
 ( 1.000000000000000000, 0.7629087100934772714, 1.000000000000000000),
 ( 1.000000000000000000, 0.7071067811865352493, 1.000000000000000000) ) ) 
 REPRESENTATION_ITEM ( '' )  SURFACE ( )  );
#55055 = CIRCLE ( 'NONE', #13400, 0.1000000000000058481 ) ;
#55057 = CARTESIAN_POINT ( 'NONE',  ( -16.94132844910801339, 30.26709352238295736, -234.7914533465139755 ) ) ;
#55056 = VECTOR ( 'NONE', #84523, 1000.000000000000000 ) ;
#55058 = CARTESIAN_POINT ( 'NONE',  ( 20.84999999999998721, 64.25000000001244871, -170.0231074845244166 ) ) ;
#55059 = CARTESIAN_POINT ( 'NONE',  ( 20.85000000000000142, -1.835859311432481045, -212.5044391687984842 ) ) ;
#55060 = DIRECTION ( 'NONE',  ( -1.000000000000000000, 0.000000000000000000, 0.000000000000000000 ) ) ;
#55062 = ORIENTED_EDGE ( 'NONE', *, *, #85724, .F. ) ;
#55061 = CARTESIAN_POINT ( 'NONE',  ( -16.80891096016327424, 30.22189824094511934, -234.8153852565851878 ) ) ;
#55064 = CARTESIAN_POINT ( 'NONE',  ( 19.81427058490544013, 11.66856398039208109, -192.2499999999999716 ) ) ;
#55063 = DIRECTION ( 'NONE',  ( 2.952720810173289112E-16, -1.000000000000000000, 0.000000000000000000 ) ) ;
#55065 = LINE ( 'NONE', #178932, #98178 ) ;
#55066 = CARTESIAN_POINT ( 'NONE',  ( -12.93407622233967835, 9.417789466963366607, -115.8573845439769059 ) ) ;
#55067 = CARTESIAN_POINT ( 'NONE',  ( -23.25000000000000000, 11.75000000001115552, -121.8500000000000227 ) ) ;
#55068 = ORIENTED_EDGE ( 'NONE', *, *, #69602, .F. ) ;
#55069 =( LENGTH_UNIT ( ) NAMED_UNIT ( * ) SI_UNIT ( .MILLI., .METRE. ) );
#55070 = DIRECTION ( 'NONE',  ( -1.000000000000000000, 0.000000000000000000, 0.000000000000000000 ) ) ;
#55071 = ORIENTED_EDGE ( 'NONE', *, *, #148795, .F. ) ;
#55072 = B_SPLINE_CURVE_WITH_KNOTS ( 'NONE', 3,
 ( #77490, #55348, #217015, #214450, #20130, #35847, #115357, #38398 ),
 .UNSPECIFIED., .F., .F.,
 ( 4, 2, 2, 4 ),
 ( 0.000000000000000000, 0.0001094981963948359418, 0.0002189963927896718837, 0.0004379927855794091447 ),
 .UNSPECIFIED. ) ;
#55073 = DIRECTION ( 'NONE',  ( 0.000000000000000000, 0.000000000000000000, 1.000000000000000000 ) ) ;
#55074 = CIRCLE ( 'NONE', #125819, 0.5000000000000004441 ) ;
#55075 = ORIENTED_EDGE ( 'NONE', *, *, #36718, .T. ) ;
#55076 = PLANE ( 'NONE',  #122077 ) ;
#55077 = DIRECTION ( 'NONE',  ( 0.000000000000000000, 0.000000000000000000, 1.000000000000000000 ) ) ;
#55078 = DIRECTION ( 'NONE',  ( 0.000000000000000000, -0.8814952561688430555, 0.4721928772777346239 ) ) ;
#55079 = ORIENTED_EDGE ( 'NONE', *, *, #63523, .T. ) ;
#55080 = ORIENTED_EDGE ( 'NONE', *, *, #60988, .F. ) ;
#55081 = CARTESIAN_POINT ( 'NONE',  ( -16.97683809663752186, 66.05000000001230376, -156.6207434663279514 ) ) ;
#55082 = CYLINDRICAL_SURFACE ( 'NONE', #15014, 0.09999999999999939493 ) ;
#55083 = SPHERICAL_SURFACE ( 'NONE', #245272, 0.1000000000000000056 ) ;
#55084 = DIRECTION ( 'NONE',  ( 1.000000000000000000, 0.000000000000000000, 0.000000000000000000 ) ) ;
#55085 = ADVANCED_FACE ( 'NONE', ( #150047 ), #70526, .F. ) ;
#55086 = DIRECTION ( 'NONE',  ( 2.715809747126117987E-16, 1.000000000000000000, 6.517943393102682774E-15 ) ) ;
#55087 = CARTESIAN_POINT ( 'NONE',  ( 20.94999999999999574, 4.252251777740764460, -211.8999245327126744 ) ) ;
#55088 = CARTESIAN_POINT ( 'NONE',  ( 20.95512840106821528, 65.37615130623854043, -90.82062826372546738 ) ) ;
#55089 = ORIENTED_EDGE ( 'NONE', *, *, #198288, .T. ) ;
#55090 = CARTESIAN_POINT ( 'NONE',  ( -18.79999999999999716, -1.410778198689824459, -7.973296578895943121 ) ) ;
#55091 = CIRCLE ( 'NONE', #121782, 2.100000000000004530 ) ;
#55093 = ORIENTED_EDGE ( 'NONE', *, *, #189115, .T. ) ;
#55092 = CARTESIAN_POINT ( 'NONE',  ( -20.94999999999999929, 7.120270961708750512, -204.6595630418393057 ) ) ;
#55094 = FACE_OUTER_BOUND ( 'NONE', #88084, .T. ) ;
#55095 = FACE_OUTER_BOUND ( 'NONE', #208988, .T. ) ;
#55097 = CARTESIAN_POINT ( 'NONE',  ( -21.64999999999999858, 63.37018259659601682, -222.0118260003222872 ) ) ;
#55096 = CARTESIAN_POINT ( 'NONE',  ( -20.64999999999999858, 68.37653524343949130, -222.4633752038642172 ) ) ;
#55098 = ADVANCED_FACE ( 'NONE', ( #148757 ), #207448, .T. ) ;
#55100 = VERTEX_POINT ( 'NONE', #73097 ) ;
#55099 = CARTESIAN_POINT ( 'NONE',  ( -15.15766958671843412, 62.18838770701754015, -218.4972640811180611 ) ) ;
#55101 = CARTESIAN_POINT ( 'NONE',  ( -20.54999999999999716, 49.57218508014541669, -254.1759139559835035 ) ) ;
#55102 = LINE ( 'NONE', #194683, #16382 ) ;
#55103 = DIRECTION ( 'NONE',  ( -1.000000000000000000, -0.000000000000000000, -0.000000000000000000 ) ) ;
#55104 = CARTESIAN_POINT ( 'NONE',  ( -20.85000000000000142, 77.83585931145570669, -125.0186683157258045 ) ) ;
#55105 = CARTESIAN_POINT ( 'NONE',  ( -18.50211644919735932, 10.30207779525983192, -139.4895520716782755 ) ) ;
#55106 = ADVANCED_FACE ( 'NONE', ( #173503 ), #32698, .F. ) ;
#55107 = VERTEX_POINT ( 'NONE', #78175 ) ;
#55108 = CARTESIAN_POINT ( 'NONE',  ( 23.14999999999999503, 69.45000000001205365, -124.1731074845243370 ) ) ;
#55109 = ORIENTED_EDGE ( 'NONE', *, *, #49151, .F. ) ;
#55111 = AXIS2_PLACEMENT_3D ( 'NONE', #30770, #88114, #71174 ) ;
#55110 = CARTESIAN_POINT ( 'NONE',  ( 22.40000000000020819, 76.10085836911243007, -215.2726746080140572 ) ) ;
#55112 = EDGE_CURVE ( 'NONE', #214748, #32792, #234706, .T. ) ;
#55113 = ORIENTED_EDGE ( 'NONE', *, *, #68031, .T. ) ;
#55114 = CARTESIAN_POINT ( 'NONE',  ( -20.94999675878240808, 46.33100819526731584, -243.0553980158188381 ) ) ;
#55115 = ORIENTED_EDGE ( 'NONE', *, *, #57073, .T. ) ;
#55116 = CIRCLE ( 'NONE', #71911, 0.1000000000000028783 ) ;
#55117 = CARTESIAN_POINT ( 'NONE',  ( -23.25000000000000000, -9.599999999988847676, -76.89396912265249284 ) ) ;
#55118 = CARTESIAN_POINT ( 'NONE',  ( 23.14999999999999858, 64.04577702392042227, -222.1950530992138226 ) ) ;
#55119 = AXIS2_PLACEMENT_3D ( 'NONE', #204489, #244910, #182390 ) ;
#55120 = DIRECTION ( 'NONE',  ( 0.000000000000000000, -0.2617529984164955192, -0.9651348961777178603 ) ) ;
#55121 = VERTEX_POINT ( 'NONE', #232148 ) ;
#55122 = EDGE_CURVE ( 'NONE', #53620, #72835, #84786, .T. ) ;
#55123 = CARTESIAN_POINT ( 'NONE',  ( -16.96982749440708815, 9.949999999999983302, -13.12477840881186530 ) ) ;
#55124 = DIRECTION ( 'NONE',  ( 1.000000000000000000, 0.000000000000000000, 0.000000000000000000 ) ) ;
#55125 = TOROIDAL_SURFACE ( 'NONE', #155160, 0.6000000000000004219, 0.1000000000000000056 ) ;
#55126 = CARTESIAN_POINT ( 'NONE',  ( -18.59999999999999787, -26.43935341560094443, -18.14150860750746475 ) ) ;
#55127 = CIRCLE ( 'NONE', #21843, 0.1000000000000053763 ) ;
#55128 = DIRECTION ( 'NONE',  ( 0.000000000000000000, 0.000000000000000000, 1.000000000000000000 ) ) ;
#55129 = CARTESIAN_POINT ( 'NONE',  ( -18.59999999999999787, 38.25685495413521409, -235.9601135138701693 ) ) ;
#55130 = ORIENTED_EDGE ( 'NONE', *, *, #142404, .T. ) ;
#55131 = CARTESIAN_POINT ( 'NONE',  ( -18.46919391072061956, 85.67072438828979841, -129.8493039527246822 ) ) ;
#55132 = VERTEX_POINT ( 'NONE', #54767 ) ;
#55133 = VERTEX_POINT ( 'NONE', #33979 ) ;
#55134 = VERTEX_POINT ( 'NONE', #96448 ) ;
#55135 = CARTESIAN_POINT ( 'NONE',  ( 22.39999999999999503, 1.115541036281197940E-11, -59.20922040162666633 ) ) ;
#55136 = DIRECTION ( 'NONE',  ( -6.938893903907222856E-15, 1.000000000000000000, 2.891205793294679805E-16 ) ) ;
#55137 = DIRECTION ( 'NONE',  ( -0.000000000000000000, 0.4721928772777347905, 0.8814952561688430555 ) ) ;
#55138 = AXIS2_PLACEMENT_3D ( 'NONE', #233541, #230982, #134398 ) ;
#55139 = FACE_OUTER_BOUND ( 'NONE', #204874, .T. ) ;
#55140 = ORIENTED_EDGE ( 'NONE', *, *, #215031, .T. ) ;
#55141 = DIRECTION ( 'NONE',  ( 0.000000000000000000, 0.2617529984165071211, 0.9651348961777146407 ) ) ;
#55142 = CARTESIAN_POINT ( 'NONE',  ( 23.14999999999999503, 6.450000000011156587, -88.75000000000004263 ) ) ;
#55143 = ORIENTED_EDGE ( 'NONE', *, *, #47046, .T. ) ;
#55144 = EDGE_CURVE ( 'NONE', #230388, #201537, #214013, .T. ) ;
#55145 = VECTOR ( 'NONE', #99655, 1000.000000000000000 ) ;
#55147 = ORIENTED_EDGE ( 'NONE', *, *, #12659, .F. ) ;
#55146 = CARTESIAN_POINT ( 'NONE',  ( -20.94999999999999929, 36.65892442174935439, -249.5511627012433848 ) ) ;
#55148 = AXIS2_PLACEMENT_3D ( 'NONE', #160114, #203057, #165223 ) ;
#55149 = CIRCLE ( 'NONE', #234225, 0.1000000000000028644 ) ;
#55150 = DIRECTION ( 'NONE',  ( 1.444674012291107001E-15, -0.9910827722268042983, 0.1332476588733650935 ) ) ;
#55151 = DIRECTION ( 'NONE',  ( -1.000000000000000000, 0.000000000000000000, -0.000000000000000000 ) ) ;
#55152 = VECTOR ( 'NONE', #156836, 1000.000000000000000 ) ;
#55153 = CARTESIAN_POINT ( 'NONE',  ( -16.83558968593864336, 9.950000000011137047, -79.66230518761653911 ) ) ;
#55154 = VERTEX_POINT ( 'NONE', #113463 ) ;
#55155 = EDGE_CURVE ( 'NONE', #111358, #223130, #201521, .T. ) ;
#55156 = CARTESIAN_POINT ( 'NONE',  ( -20.94999027547553894, 18.34807417603272128, -236.8765254748879556 ) ) ;
#55157 = EDGE_LOOP ( 'NONE', ( #254529, #27434, #205682 ) ) ;
#55158 = FACE_OUTER_BOUND ( 'NONE', #119024, .T. ) ;
#55159 = CARTESIAN_POINT ( 'NONE',  ( 13.22461703343584993, 66.56333706821246210, -51.20007075222952153 ) ) ;
#55160 = EDGE_CURVE ( 'NONE', #176751, #31646, #89095, .T. ) ;
#55161 = PLANE ( 'NONE',  #51063 ) ;
#55162 = ADVANCED_FACE ( 'NONE', ( #212583 ), #147367, .F. ) ;
#55163 = AXIS2_PLACEMENT_3D ( 'NONE', #94313, #212987, #13516 ) ;
#55164 = VECTOR ( 'NONE', #246475, 999.9999999999998863 ) ;
#55165 = EDGE_LOOP ( 'NONE', ( #197754, #136135, #180766, #81599 ) ) ;
#55166 = CARTESIAN_POINT ( 'NONE',  ( 20.94999999999999574, 76.00000000001165290, -69.52310748452431710 ) ) ;
#55167 = ORIENTED_EDGE ( 'NONE', *, *, #49871, .T. ) ;
#55168 = CARTESIAN_POINT ( 'NONE',  ( -17.11825945287481687, 10.05000000001113847, -188.3499999999999659 ) ) ;
#55169 = DIRECTION ( 'NONE',  ( 0.000000000000000000, 0.000000000000000000, 1.000000000000000000 ) ) ;
#55170 = VECTOR ( 'NONE', #17463, 1000.000000000000000 ) ;
#55173 = ADVANCED_FACE ( 'NONE', ( #76899 ), #13101, .T. ) ;
#55172 = VERTEX_POINT ( 'NONE', #155199 ) ;
#55171 = DIRECTION ( 'NONE',  ( 0.000000000000000000, 1.000000000000000000, 0.000000000000000000 ) ) ;
#55174 = DIRECTION ( 'NONE',  ( 0.000000000000000000, 0.000000000000000000, -1.000000000000000000 ) ) ;
#55175 = CARTESIAN_POINT ( 'NONE',  ( -20.94999999999999929, 43.57568952063339651, -245.1784935019914826 ) ) ;
#55176 = CARTESIAN_POINT ( 'NONE',  ( -16.84419801905645286, 9.949999999999985079, -20.83051015377798265 ) ) ;
#55177 = DIRECTION ( 'NONE',  ( 0.000000000000000000, 0.9651348961777157509, -0.2617529984165031243 ) ) ;
#55178 = VECTOR ( 'NONE', #6004, 1000.000000000000000 ) ;
#55179 = EDGE_CURVE ( 'NONE', #246415, #79128, #26580, .T. ) ;
#55180 = LINE ( 'NONE', #192183, #222367 ) ;
#55181 = EDGE_CURVE ( 'NONE', #28211, #223089, #56031, .T. ) ;
#55182 = FACE_OUTER_BOUND ( 'NONE', #94621, .T. ) ;
#55184 = EDGE_LOOP ( 'NONE', ( #31653, #176661, #18685, #106687 ) ) ;
#55183 = DIRECTION ( 'NONE',  ( 0.000000000000000000, 0.1455152366551500653, 0.9893560106964507384 ) ) ;
#55185 = VECTOR ( 'NONE', #184811, 1000.000000000000000 ) ;
#55186 = AXIS2_PLACEMENT_3D ( 'NONE', #29989, #32564, #230739 ) ;
#55187 = CIRCLE ( 'NONE', #238374, 0.09999999999999761857 ) ;
#55188 = AXIS2_PLACEMENT_3D ( 'NONE', #97418, #156172, #235668 ) ;
#55190 = EDGE_CURVE ( 'NONE', #27906, #252932, #155766, .T. ) ;
#55189 = DIRECTION ( 'NONE',  ( 1.000000000000000000, 0.000000000000000000, 0.000000000000000000 ) ) ;
#55192 = EDGE_CURVE ( 'NONE', #59396, #40979, #122436, .T. ) ;
#55191 = CARTESIAN_POINT ( 'NONE',  ( -18.39418127959864790, 16.38129732710523001, -222.2507808268338465 ) ) ;
#55193 = DIRECTION ( 'NONE',  ( -1.000000000000000000, 0.000000000000000000, -0.000000000000000000 ) ) ;
#55194 = ADVANCED_FACE ( 'NONE', ( #95190 ), #254240, .F. ) ;
#55195 = AXIS2_PLACEMENT_3D ( 'NONE', #116957, #94817, #38710 ) ;
#55196 = ORIENTED_EDGE ( 'NONE', *, *, #58298, .F. ) ;
#55197 = CARTESIAN_POINT ( 'NONE',  ( -21.05000000000000071, 74.83729825007388570, -94.92310748452432279 ) ) ;
#55198 = TOROIDAL_SURFACE ( 'NONE', #205248, 11.65000000000000036, 0.1000000000000000056 ) ;
#55199 = CARTESIAN_POINT ( 'NONE',  ( -18.50000000000000000, 18.51199663233067838, -231.2535697180530292 ) ) ;
#55200 = CARTESIAN_POINT ( 'NONE',  ( 15.74999999999999645, 9.350000000011139178, -184.2499999999999716 ) ) ;
#55201 = VECTOR ( 'NONE', #9158, 1000.000000000000000 ) ;
#55202 = ORIENTED_EDGE ( 'NONE', *, *, #196561, .F. ) ;
#55203 = CARTESIAN_POINT ( 'NONE',  ( -20.94999999999999929, 77.16270174994990327, -95.12310748452431142 ) ) ;
#55204 = AXIS2_PLACEMENT_3D ( 'NONE', #255665, #172377, #211455 ) ;
#55205 = AXIS2_PLACEMENT_3D ( 'NONE', #106093, #143953, #142656 ) ;
#55206 = CARTESIAN_POINT ( 'NONE',  ( 20.94999999999999574, 87.48912529308842068, -167.0231074845242745 ) ) ;
#55207 = ORIENTED_EDGE ( 'NONE', *, *, #149141, .F. ) ;
#55208 = DIRECTION ( 'NONE',  ( 0.000000000000000000, -6.982962677686266711E-15, 1.000000000000000000 ) ) ;
#55209 = EDGE_CURVE ( 'NONE', #80209, #186900, #238965, .T. ) ;
#55210 = ORIENTED_EDGE ( 'NONE', *, *, #225840, .T. ) ;
#55211 = B_SPLINE_CURVE_WITH_KNOTS ( 'NONE', 3,
 ( #44070, #203134, #24525, #104009 ),
 .UNSPECIFIED., .F., .F.,
 ( 4, 4 ),
 ( 0.000000000000000000, 0.001767853679387123818 ),
 .UNSPECIFIED. ) ;
#55212 = ADVANCED_FACE ( 'NONE', ( #117323 ), #196843, .T. ) ;
#55213 = SPHERICAL_SURFACE ( 'NONE', #58864, 0.1000000000000000056 ) ;
#55215 = VERTEX_POINT ( 'NONE', #52192 ) ;
#55214 = CARTESIAN_POINT ( 'NONE',  ( 21.05000000000000071, 6.258847123090562015, -133.9682416469444775 ) ) ;
#55216 = DIRECTION ( 'NONE',  ( 7.304098846218135653E-16, 0.9651348961777157509, -0.2617529984165031243 ) ) ;
#55217 = EDGE_LOOP ( 'NONE', ( #242125, #187996, #28993, #136710, #218626, #90414, #128687, #77529, #129944, #124350, #65399, #158211, #77296, #147073, #139527, #68495, #234985 ) ) ;
#55218 = DIRECTION ( 'NONE',  ( 1.000000000000000000, 0.000000000000000000, 0.000000000000000000 ) ) ;
#55219 = ORIENTED_EDGE ( 'NONE', *, *, #67633, .F. ) ;
#55222 = ADVANCED_FACE ( 'NONE', ( #178608 ), #182446, .F. ) ;
#55221 = EDGE_LOOP ( 'NONE', ( #30578, #90418, #256985, #141711 ) ) ;
#55220 = ORIENTED_EDGE ( 'NONE', *, *, #142002, .F. ) ;
#55223 = CARTESIAN_POINT ( 'NONE',  ( 18.49999999999999289, 11.75000000001115552, -125.3500000000000512 ) ) ;
#55225 = ORIENTED_EDGE ( 'NONE', *, *, #257731, .F. ) ;
#55224 = CARTESIAN_POINT ( 'NONE',  ( 21.07189867249812210, 10.72498027010430377, -146.2124514422767732 ) ) ;
#55226 = B_SPLINE_CURVE_WITH_KNOTS ( 'NONE', 3,
 ( #66772, #107167, #68047, #141482 ),
 .UNSPECIFIED., .F., .F.,
 ( 4, 4 ),
 ( 0.000000000000000000, 0.0002118541922231684618 ),
 .UNSPECIFIED. ) ;
#55227 = FACE_OUTER_BOUND ( 'NONE', #9860, .T. ) ;
#55229 = ORIENTED_EDGE ( 'NONE', *, *, #129604, .T. ) ;
#55228 = AXIS2_PLACEMENT_3D ( 'NONE', #160029, #238249, #144260 ) ;
#55230 = AXIS2_PLACEMENT_3D ( 'NONE', #55146, #134699, #135982 ) ;
#55231 = AXIS2_PLACEMENT_3D ( 'NONE', #228918, #89387, #72426 ) ;
#55232 = VERTEX_POINT ( 'NONE', #221525 ) ;
#55233 = FACE_OUTER_BOUND ( 'NONE', #71395, .T. ) ;
#55234 = DIRECTION ( 'NONE',  ( 0.000000000000000000, -0.000000000000000000, 1.000000000000000000 ) ) ;
#55235 = DIRECTION ( 'NONE',  ( 0.000000000000000000, 0.2128009952263485993, -0.9770955615653341697 ) ) ;
#55236 = ORIENTED_EDGE ( 'NONE', *, *, #130908, .F. ) ;
#55237 = DIRECTION ( 'NONE',  ( 1.000000000000000000, 0.000000000000000000, 0.000000000000000000 ) ) ;
#55238 = CARTESIAN_POINT ( 'NONE',  ( -20.94999999999999929, -4.557064143889601127, -233.1584191572127622 ) ) ;
#55239 = LINE ( 'NONE', #214351, #118894 ) ;
#55241 = ORIENTED_EDGE ( 'NONE', *, *, #183659, .F. ) ;
#55240 = ADVANCED_FACE ( 'NONE', ( #99007 ), #198136, .T. ) ;
#55242 = DIRECTION ( 'NONE',  ( 1.000000000000000000, 0.000000000000000000, -0.000000000000000000 ) ) ;
#55243 = CARTESIAN_POINT ( 'NONE',  ( 20.85000000000000142, 76.00000000001185185, -95.22310748452429152 ) ) ;
#55244 = CARTESIAN_POINT ( 'NONE',  ( 21.14999999999999858, 76.10000000001174669, -81.17267829206912211 ) ) ;
#55245 = ADVANCED_FACE ( 'NONE', ( #79458 ), #134855, .T. ) ;
#55246 = VERTEX_POINT ( 'NONE', #104158 ) ;
#55248 = DIRECTION ( 'NONE',  ( 0.000000000000000000, 0.3738317757009345654, 0.9274965247785492695 ) ) ;
#55247 = VECTOR ( 'NONE', #168940, 1000.000000000000000 ) ;
#55249 = ORIENTED_EDGE ( 'NONE', *, *, #159946, .F. ) ;
#55250 = ORIENTED_EDGE ( 'NONE', *, *, #159496, .T. ) ;
#55251 = CARTESIAN_POINT ( 'NONE',  ( -13.43673303185029333, 24.89049957252425571, -232.5305204729233424 ) ) ;
#55252 = ORIENTED_EDGE ( 'NONE', *, *, #129528, .T. ) ;
#55253 = AXIS2_PLACEMENT_3D ( 'NONE', #232200, #53543, #148801 ) ;
#55254 = ORIENTED_EDGE ( 'NONE', *, *, #233955, .F. ) ;
#55256 = ADVANCED_FACE ( 'NONE', ( #3796 ), #102866, .T. ) ;
#55255 = DIRECTION ( 'NONE',  ( 0.2834754621636358940, -0.2834754621636437211, 0.9161240771326893961 ) ) ;
#55257 = CARTESIAN_POINT ( 'NONE',  ( 23.24999999999997513, 64.25000000001249134, -177.0379132551784096 ) ) ;
#55258 = VERTEX_POINT ( 'NONE', #101572 ) ;
#55259 = VERTEX_POINT ( 'NONE', #121208 ) ;
#55260 = DIRECTION ( 'NONE',  ( 2.952720810173289605E-16, -0.9770955615653357240, -0.2128009952263412996 ) ) ;
#55261 = EDGE_CURVE ( 'NONE', #221652, #41677, #176434, .T. ) ;
#55262 = DIRECTION ( 'NONE',  ( 1.000000000000000000, 0.000000000000000000, 0.000000000000000000 ) ) ;
#55263 = ORIENTED_EDGE ( 'NONE', *, *, #41460, .F. ) ;
#55264 = ADVANCED_FACE ( 'NONE', ( #63760 ), #222823, .T. ) ;
#55265 = ORIENTED_EDGE ( 'NONE', *, *, #95038, .T. ) ;
#55266 = EDGE_CURVE ( 'NONE', #245547, #95482, #234860, .T. ) ;
#55267 = VECTOR ( 'NONE', #210380, 1000.000000000000000 ) ;
#55270 = EDGE_CURVE ( 'NONE', #116539, #153561, #105642, .T. ) ;
#55269 = ADVANCED_FACE ( 'NONE', ( #123750 ), #181161, .T. ) ;
#55268 = DIRECTION ( 'NONE',  ( 0.000000000000000000, 0.8068669527897506244, 0.5907332058516622242 ) ) ;
#55271 = DIRECTION ( 'NONE',  ( 0.000000000000000000, -1.086323898850447076E-14, 1.000000000000000000 ) ) ;
#55272 = EDGE_CURVE ( 'NONE', #247168, #224679, #97245, .T. ) ;
#55273 = CARTESIAN_POINT ( 'NONE',  ( -16.87383368123029825, 9.950000000011138823, -46.15000000000000568 ) ) ;
#55274 = DIRECTION ( 'NONE',  ( 3.469446951953635015E-14, -0.000000000000000000, 1.000000000000000000 ) ) ;
#55275 = DIRECTION ( 'NONE',  ( 0.000000000000000000, 0.000000000000000000, 1.000000000000000000 ) ) ;
#55276 = CARTESIAN_POINT ( 'NONE',  ( -18.59999999999999787, 1.162701749938009677, -8.099999999999999645 ) ) ;
#55277 = DIRECTION ( 'NONE',  ( 0.000000000000000000, -0.8814952561688425003, 0.4721928772777359007 ) ) ;
#55279 = DIRECTION ( 'NONE',  ( -0.000000000000000000, -0.9910465087640860649, 0.1335171055202901413 ) ) ;
#55278 = CARTESIAN_POINT ( 'NONE',  ( -16.87036670365549895, 9.989418819301647545, -12.52043988269794639 ) ) ;
#55280 = DIRECTION ( 'NONE',  ( 1.000000000000000000, -0.000000000000000000, -0.000000000000000000 ) ) ;
#55281 = CARTESIAN_POINT ( 'NONE',  ( -16.80070461187903064, 22.97539108935011498, -230.9336297528783746 ) ) ;
#55282 = CIRCLE ( 'NONE', #201072, 0.1000000000000028644 ) ;
#55283 = LINE ( 'NONE', #154460, #147744 ) ;
#55284 = SPHERICAL_SURFACE ( 'NONE', #188418, 0.1000000000000000056 ) ;
#55285 = EDGE_CURVE ( 'NONE', #96459, #34079, #251416, .T. ) ;
#55286 = EDGE_CURVE ( 'NONE', #89573, #70952, #188879, .T. ) ;
#55287 = CIRCLE ( 'NONE', #30399, 11.89999999999999325 ) ;
#55288 = ORIENTED_EDGE ( 'NONE', *, *, #158884, .T. ) ;
#55289 = VECTOR ( 'NONE', #161230, 1000.000000000000000 ) ;
#55290 = EDGE_CURVE ( 'NONE', #181442, #153430, #39062, .T. ) ;
#55292 = ORIENTED_EDGE ( 'NONE', *, *, #137823, .T. ) ;
#55291 = CARTESIAN_POINT ( 'NONE',  ( -18.59999999999999787, -10.72142460728770352, 6.051435706882140053 ) ) ;
#55293 = EDGE_CURVE ( 'NONE', #184620, #117140, #39093, .T. ) ;
#55294 = DIRECTION ( 'NONE',  ( 1.000000000000000000, 0.000000000000000000, 0.000000000000000000 ) ) ;
#55295 = DIRECTION ( 'NONE',  ( -0.000000000000000000, 0.000000000000000000, 1.000000000000000000 ) ) ;
#55296 = ADVANCED_FACE ( 'NONE', ( #220291 ), #35162, .F. ) ;
#55297 = ORIENTED_EDGE ( 'NONE', *, *, #216567, .T. ) ;
#55298 = AXIS2_PLACEMENT_3D ( 'NONE', #104680, #182987, #102118 ) ;
#55299 = CIRCLE ( 'NONE', #121976, 0.1000000000000028644 ) ;
#55300 = FACE_OUTER_BOUND ( 'NONE', #50152, .T. ) ;
#55301 = VERTEX_POINT ( 'NONE', #241141 ) ;
#55302 = PLANE ( 'NONE',  #242207 ) ;
#55303 = LINE ( 'NONE', #158332, #42221 ) ;
#55304 = CIRCLE ( 'NONE', #213558, 0.1000000000000021289 ) ;
#55305 = ADVANCED_FACE ( 'NONE', ( #52849 ), #34606, .T. ) ;
#55306 = DIRECTION ( 'NONE',  ( 0.000000000000000000, 0.9887567792719329507, 0.1495327102803732933 ) ) ;
#55308 = ORIENTED_EDGE ( 'NONE', *, *, #239272, .F. ) ;
#55307 = CARTESIAN_POINT ( 'NONE',  ( -23.15000000000000213, 11.65000000001115588, -121.8500000000000369 ) ) ;
#55309 = CYLINDRICAL_SURFACE ( 'NONE', #170474, 11.74999999999999645 ) ;
#55311 = EDGE_LOOP ( 'NONE', ( #8328, #236907, #220483, #170788 ) ) ;
#55310 = CARTESIAN_POINT ( 'NONE',  ( -23.15000000000000213, 1.115600667400684642E-11, -55.19999999999999574 ) ) ;
#55312 = AXIS2_PLACEMENT_3D ( 'NONE', #239197, #83922, #140076 ) ;
#55313 = LINE ( 'NONE', #134858, #212588 ) ;
#55315 = CARTESIAN_POINT ( 'NONE',  ( 21.06490991615909536, 10.72489134758711238, -12.20371135353312830 ) ) ;
#55314 = CIRCLE ( 'NONE', #238708, 0.1000000000000009354 ) ;
#55316 = TOROIDAL_SURFACE ( 'NONE', #242797, 0.6000000000000009770, 0.1000000000000000056 ) ;
#55317 = CARTESIAN_POINT ( 'NONE',  ( 21.05000000000000071, 44.15903683684981473, -236.5744930507153185 ) ) ;
#55318 = DIRECTION ( 'NONE',  ( 0.000000000000000000, 0.000000000000000000, 1.000000000000000000 ) ) ;
#55319 = CIRCLE ( 'NONE', #96846, 0.5000000000000004441 ) ;
#55320 = EDGE_CURVE ( 'NONE', #183834, #190169, #166757, .T. ) ;
#55322 = DIRECTION ( 'NONE',  ( 0.000000000000000000, 5.329070518200807403E-15, -1.000000000000000000 ) ) ;
#55321 = DIRECTION ( 'NONE',  ( -0.000000000000000000, -0.4721928772777351790, -0.8814952561688427224 ) ) ;
#55323 = CARTESIAN_POINT ( 'NONE',  ( -13.39999999999994529, 64.35000000001120668, -23.62310748452479103 ) ) ;
#55324 = DIRECTION ( 'NONE',  ( -0.000000000000000000, 6.982962677686266711E-15, -1.000000000000000000 ) ) ;
#55325 = CARTESIAN_POINT ( 'NONE',  ( 21.59780538579341780, 0.09897866960914131207, -160.6529094700567271 ) ) ;
#55326 = CARTESIAN_POINT ( 'NONE',  ( 23.15000000000000213, -9.599999999988842347, -124.1060308773475924 ) ) ;
#55327 = ORIENTED_EDGE ( 'NONE', *, *, #96836, .T. ) ;
#55328 = DIRECTION ( 'NONE',  ( 0.000000000000000000, 0.000000000000000000, 1.000000000000000000 ) ) ;
#55329 = VERTEX_POINT ( 'NONE', #112837 ) ;
#55330 = VERTEX_POINT ( 'NONE', #7651 ) ;
#55331 = ADVANCED_FACE ( 'NONE', ( #106724 ), #222341, .T. ) ;
#55332 = CARTESIAN_POINT ( 'NONE',  ( -23.25000000000000000, 76.00000000001126921, -203.5231074845248997 ) ) ;
#55333 = CARTESIAN_POINT ( 'NONE',  ( 23.25000000000000000, 87.75000000001202238, -114.7731074845242318 ) ) ;
#55334 = EDGE_LOOP ( 'NONE', ( #1150, #168768, #207649, #246265 ) ) ;
#55335 = ORIENTED_EDGE ( 'NONE', *, *, #56704, .F. ) ;
#55336 = CARTESIAN_POINT ( 'NONE',  ( 18.55857864376267941, 55.00748275915436381, -229.9713042450930516 ) ) ;
#55337 =( NAMED_UNIT ( * ) SI_UNIT ( $, .STERADIAN. ) SOLID_ANGLE_UNIT ( ) );
#55338 = CIRCLE ( 'NONE', #51261, 6.329289321881370611 ) ;
#55339 = EDGE_CURVE ( 'NONE', #59315, #240058, #132405, .T. ) ;
#55340 = ORIENTED_EDGE ( 'NONE', *, *, #198327, .T. ) ;
#55341 = ORIENTED_EDGE ( 'NONE', *, *, #230952, .T. ) ;
#55342 = DIRECTION ( 'NONE',  ( 0.2834754621636358940, 0.2834754621636501049, -0.9161240771326873977 ) ) ;
#55343 = DIRECTION ( 'NONE',  ( 0.000000000000000000, 0.1575844902526876978, 0.9875055080513731598 ) ) ;
#55344 = DIRECTION ( 'NONE',  ( 0.000000000000000000, -0.2617529984165031243, -0.9651348961777157509 ) ) ;
#55345 = CARTESIAN_POINT ( 'NONE',  ( -18.50000000000000000, 79.37986612816742138, -196.2658927859692142 ) ) ;
#55346 = CIRCLE ( 'NONE', #146950, 0.09999999999999939493 ) ;
#55347 = AXIS2_PLACEMENT_3D ( 'NONE', #254459, #134525, #73324 ) ;
#55349 = DIRECTION ( 'NONE',  ( -1.000000000000000000, -7.774224845003864090E-15, -1.451301502210102000E-14 ) ) ;
#55348 = CARTESIAN_POINT ( 'NONE',  ( -18.43707690579160996, 77.26488334054519669, -241.9697969554614758 ) ) ;
#55350 = FACE_OUTER_BOUND ( 'NONE', #147836, .T. ) ;
#55352 = VERTEX_POINT ( 'NONE', #185001 ) ;
#55351 = DIRECTION ( 'NONE',  ( -0.000000000000000000, 0.8660254037844502539, 0.4999999999999799050 ) ) ;
#55354 = CARTESIAN_POINT ( 'NONE',  ( -22.47071067811865319, 65.11488425470513164, -243.2801022963548689 ) ) ;
#55353 = DIRECTION ( 'NONE',  ( 1.000000000000000000, 0.000000000000000000, 0.000000000000000000 ) ) ;
#55355 = CARTESIAN_POINT ( 'NONE',  ( 21.14999999999999858, -0.09999999999999939493, 6.540656951701244282 ) ) ;
#55356 = ORIENTED_EDGE ( 'NONE', *, *, #69326, .F. ) ;
#55357 = VECTOR ( 'NONE', #10540, 1000.000000000000000 ) ;
#55358 = CARTESIAN_POINT ( 'NONE',  ( -23.15000000000000213, 1.999999999999998224, -20.77537807723789953 ) ) ;
#55359 = CARTESIAN_POINT ( 'NONE',  ( -18.59999999999999787, 68.51069317435826633, -224.1259271199053842 ) ) ;
#55360 = ORIENTED_EDGE ( 'NONE', *, *, #128003, .F. ) ;
#55361 = AXIS2_PLACEMENT_3D ( 'NONE', #164942, #85367, #188361 ) ;
#55363 = FACE_OUTER_BOUND ( 'NONE', #58996, .T. ) ;
#55362 = AXIS2_PLACEMENT_3D ( 'NONE', #148989, #10748, #88972 ) ;
#55364 = VECTOR ( 'NONE', #76482, 1000.000000000000000 ) ;
#55365 = CARTESIAN_POINT ( 'NONE',  ( -20.64999999999999858, 71.65000000001151648, -48.37310748452434694 ) ) ;
#55366 = DIRECTION ( 'NONE',  ( 0.000000000000000000, 0.000000000000000000, 1.000000000000000000 ) ) ;
#55367 = ORIENTED_EDGE ( 'NONE', *, *, #6833, .F. ) ;
#55368 = ORIENTED_EDGE ( 'NONE', *, *, #116312, .T. ) ;
#55369 = AXIS2_PLACEMENT_3D ( 'NONE', #172974, #249905, #189930 ) ;
#55370 = CYLINDRICAL_SURFACE ( 'NONE', #111744, 3.999999999999994671 ) ;
#55371 = LINE ( 'NONE', #237896, #248996 ) ;
#55372 = DIRECTION ( 'NONE',  ( 2.952720810173289112E-16, 0.9651348961777155289, -0.2617529984165037904 ) ) ;
#55373 = CARTESIAN_POINT ( 'NONE',  ( 20.94999999999999929, 1.115600667400684642E-11, -180.4749999999999659 ) ) ;
#55374 = VERTEX_POINT ( 'NONE', #25934 ) ;
#55375 = CIRCLE ( 'NONE', #163577, 0.09999999999999741040 ) ;
#55377 = AXIS2_PLACEMENT_3D ( 'NONE', #163632, #161067, #1958 ) ;
#55376 = LINE ( 'NONE', #131102, #87828 ) ;
#55379 = EDGE_CURVE ( 'NONE', #172600, #225538, #51655, .T. ) ;
#55378 = DIRECTION ( 'NONE',  ( -1.000000000000000000, 0.000000000000000000, 0.000000000000000000 ) ) ;
#55380 = DIRECTION ( 'NONE',  ( 1.186688945009009831E-16, -1.000000000000000000, 0.000000000000000000 ) ) ;
#55381 = VECTOR ( 'NONE', #230367, 1000.000000000000000 ) ;
#55382 = DIRECTION ( 'NONE',  ( -0.000000000000000000, -0.8814952561688430555, 0.4721928772777346239 ) ) ;
#55383 = CARTESIAN_POINT ( 'NONE',  ( -18.49513951962167724, -9.437725026666544892, -207.7780725750291140 ) ) ;
#55384 = AXIS2_PLACEMENT_3D ( 'NONE', #102719, #199293, #177188 ) ;
#55385 = CIRCLE ( 'NONE', #201167, 0.1000000000000028644 ) ;
#55386 = VECTOR ( 'NONE', #127086, 1000.000000000000114 ) ;
#55388 = ORIENTED_EDGE ( 'NONE', *, *, #190146, .F. ) ;
#55387 = CARTESIAN_POINT ( 'NONE',  ( 23.14999999999999858, 71.00000000001186606, -90.61784146561124942 ) ) ;
#55389 = AXIS2_PLACEMENT_3D ( 'NONE', #229894, #51221, #130785 ) ;
#55390 = DIRECTION ( 'NONE',  ( -1.000000000000000000, 0.000000000000000000, 0.000000000000000000 ) ) ;
#55391 = DIRECTION ( 'NONE',  ( 1.000000000000000000, 0.000000000000000000, 0.000000000000000000 ) ) ;
#55392 = DIRECTION ( 'NONE',  ( 0.000000000000000000, 0.9126074666064005747, 0.4088369013362753712 ) ) ;
#55393 = CARTESIAN_POINT ( 'NONE',  ( 21.04999999999999716, -0.03753606327451301794, -94.16772772606439901 ) ) ;
#55394 = ADVANCED_FACE ( 'NONE', ( #191118 ), #39249, .T. ) ;
#55395 = LINE ( 'NONE', #176686, #162893 ) ;
#55397 = ORIENTED_EDGE ( 'NONE', *, *, #128614, .F. ) ;
#55396 = CARTESIAN_POINT ( 'NONE',  ( -21.14999999999999858, -0.09999999998884338825, -122.3504291924552234 ) ) ;
#55398 = CARTESIAN_POINT ( 'NONE',  ( -21.00000000000000000, 8.058024882095860875, 1.378482379536266178 ) ) ;
#55399 = CARTESIAN_POINT ( 'NONE',  ( -21.14999999999999858, -0.09999999998884338825, -60.45934304829880546 ) ) ;
#55400 = DIRECTION ( 'NONE',  ( -0.000000000000000000, 0.9126074666063770380, 0.4088369013363281068 ) ) ;
#55401 = EDGE_CURVE ( 'NONE', #51801, #22303, #101729, .T. ) ;
#55402 = VERTEX_POINT ( 'NONE', #172861 ) ;
#55403 = CARTESIAN_POINT ( 'NONE',  ( 20.85000000000000142, 64.25000000001170974, -69.52310748452438816 ) ) ;
#55404 = DIRECTION ( 'NONE',  ( 1.000000000000000000, 7.304098846218134667E-16, 0.000000000000000000 ) ) ;
#55405 = DIRECTION ( 'NONE',  ( -1.836970198721029934E-16, 1.000000000000000000, 0.000000000000000000 ) ) ;
#55406 = CARTESIAN_POINT ( 'NONE',  ( 18.59999999999999432, 74.83729825007360148, -61.52310748452433131 ) ) ;
#55407 = CARTESIAN_POINT ( 'NONE',  ( -18.40000000000000213, 78.24072131640578220, -231.5548844243369331 ) ) ;
#55409 = EDGE_CURVE ( 'NONE', #139907, #13339, #12472, .T. ) ;
#55408 = AXIS2_PLACEMENT_3D ( 'NONE', #116190, #131881, #195735 ) ;
#55410 = CARTESIAN_POINT ( 'NONE',  ( -18.50000000000000000, 11.65000000001115232, -54.85000000000000142 ) ) ;
#55411 = CIRCLE ( 'NONE', #134539, 0.09999999999999530098 ) ;
#55412 = CIRCLE ( 'NONE', #109605, 7.899999999999990585 ) ;
#55413 = VERTEX_POINT ( 'NONE', #91982 ) ;
#55414 = EDGE_LOOP ( 'NONE', ( #3723, #121756, #20041, #100615, #52051 ) ) ;
#55415 = ADVANCED_FACE ( 'NONE', ( #72446 ), #114107, .T. ) ;
#55416 = FACE_OUTER_BOUND ( 'NONE', #152086, .T. ) ;
#55417 = CARTESIAN_POINT ( 'NONE',  ( -17.11825945287482043, 66.05000000001203375, -115.6731074845243796 ) ) ;
#55418 = ADVANCED_FACE ( 'NONE', ( #252330 ), #67611, .F. ) ;
#55419 =( BOUNDED_SURFACE ( )  B_SPLINE_SURFACE ( 3, 2, ( 
 ( #214403, #35797, #257327 ),
 ( #155758, #115304, #16241 ),
 ( #218240, #95731, #175320 ),
 ( #479, #254771, #18769 ) ),
 .UNSPECIFIED., .F., .F., .F. ) 
 B_SPLINE_SURFACE_WITH_KNOTS ( ( 4, 4 ),
 ( 3, 3 ),
 ( 3.658908243880901523, 4.712388980384689674 ),
 ( 0.000000000000000000, 1.000000000000000000 ),
 .UNSPECIFIED. ) 
 GEOMETRIC_REPRESENTATION_ITEM ( )  RATIONAL_B_SPLINE_SURFACE ( (
 ( 1.000000000000000000, 0.8984936768950558816, 1.000000000000000000),
 ( 1.000000000000000000, 0.8646876308615779605, 1.000000000000000000),
 ( 1.000000000000000000, 0.7953136715912922927, 1.000000000000000000),
 ( 1.000000000000000000, 0.7071067811865719976, 1.000000000000000000) ) ) 
 REPRESENTATION_ITEM ( '' )  SURFACE ( )  );
#55420 = CARTESIAN_POINT ( 'NONE',  ( -21.00250684356851849, 38.25685495240594491, -235.9601135146448598 ) ) ;
#55421 = DIRECTION ( 'NONE',  ( -1.000000000000000000, 0.000000000000000000, -0.000000000000000000 ) ) ;
#55422 = EDGE_CURVE ( 'NONE', #80866, #33844, #214192, .T. ) ;
#55423 = CARTESIAN_POINT ( 'NONE',  ( -16.27683809663751191, 66.65000000001209912, -127.2731074845243882 ) ) ;
#55424 = DIRECTION ( 'NONE',  ( 0.000000000000000000, 0.8700118002898356018, -0.4930308989875170078 ) ) ;
#55425 = ADVANCED_FACE ( 'NONE', ( #204553 ), #93370, .T. ) ;
#55426 = CARTESIAN_POINT ( 'NONE',  ( -20.54999999999999716, -11.74999999998884626, -45.85000000000000853 ) ) ;
#55427 = DIRECTION ( 'NONE',  ( 1.000000000000000000, 0.000000000000000000, 0.000000000000000000 ) ) ;
#55428 = EDGE_LOOP ( 'NONE', ( #240619, #33640, #247681, #186508, #22898 ) ) ;
#55429 = CARTESIAN_POINT ( 'NONE',  ( -23.25000000000000355, 70.35000000001207354, -123.8731074845243398 ) ) ;
#55430 = ORIENTED_EDGE ( 'NONE', *, *, #201077, .T. ) ;
#55431 = AXIS2_PLACEMENT_3D ( 'NONE', #224812, #61903, #46179 ) ;
#55432 = ORIENTED_EDGE ( 'NONE', *, *, #165153, .F. ) ;
#55433 = CARTESIAN_POINT ( 'NONE',  ( 23.25000000000000000, 81.82295291318693842, -214.8938525951558915 ) ) ;
#55434 = CARTESIAN_POINT ( 'NONE',  ( -20.54999999999999716, -8.999999999988846255, -76.89396912265249284 ) ) ;
#55435 = FACE_OUTER_BOUND ( 'NONE', #220410, .T. ) ;
#55437 = ORIENTED_EDGE ( 'NONE', *, *, #246905, .T. ) ;
#55436 = CARTESIAN_POINT ( 'NONE',  ( -21.45000000000000284, 68.29142135624991283, -191.1731074845243938 ) ) ;
#55438 = DIRECTION ( 'NONE',  ( 0.000000000000000000, 0.2617529984165152257, 0.9651348961777124202 ) ) ;
#55439 = FACE_OUTER_BOUND ( 'NONE', #13465, .T. ) ;
#55440 = CARTESIAN_POINT ( 'NONE',  ( -22.19999999999999929, -1.467286812112899463, 28.00000000000000000 ) ) ;
#55441 = ORIENTED_EDGE ( 'NONE', *, *, #225547, .T. ) ;
#55442 = EDGE_CURVE ( 'NONE', #55258, #168942, #56933, .T. ) ;
#55443 = LINE ( 'NONE', #217096, #133102 ) ;
#55444 = CARTESIAN_POINT ( 'NONE',  ( 18.49999999999998934, 65.71984138295503897, -145.2985354133222415 ) ) ;
#55445 = DIRECTION ( 'NONE',  ( 0.000000000000000000, -0.9893560106964500722, 0.1455152366551550613 ) ) ;
#55446 = DIRECTION ( 'NONE',  ( 1.000000000000000000, 0.000000000000000000, 0.000000000000000000 ) ) ;
#55447 = CIRCLE ( 'NONE', #201226, 11.64999999999999325 ) ;
#55448 = VECTOR ( 'NONE', #8025, 1000.000000000000000 ) ;
#55449 = ORIENTED_EDGE ( 'NONE', *, *, #17575, .T. ) ;
#55450 = LINE ( 'NONE', #230265, #64606 ) ;
#55452 = EDGE_CURVE ( 'NONE', #173035, #126285, #184969, .T. ) ;
#55451 = CYLINDRICAL_SURFACE ( 'NONE', #121191, 11.74999999999999289 ) ;
#55453 = ORIENTED_EDGE ( 'NONE', *, *, #123908, .F. ) ;
#55454 = CARTESIAN_POINT ( 'NONE',  ( 23.14999999999999147, 0.000000000000000000, 0.000000000000000000 ) ) ;
#55455 = DIRECTION ( 'NONE',  ( 1.000000000000000000, 0.000000000000000000, 0.000000000000000000 ) ) ;
#55456 = LINE ( 'NONE', #41099, #97146 ) ;
#55457 = VERTEX_POINT ( 'NONE', #57974 ) ;
#55458 = CARTESIAN_POINT ( 'NONE',  ( -20.94999999999999929, 77.13501884592155022, -28.30613060109199353 ) ) ;
#55459 = FACE_OUTER_BOUND ( 'NONE', #244039, .T. ) ;
#55460 = ORIENTED_EDGE ( 'NONE', *, *, #95168, .F. ) ;
#55461 = AXIS2_PLACEMENT_3D ( 'NONE', #27013, #229045, #49102 ) ;
#55462 = ADVANCED_FACE ( 'NONE', ( #59230 ), #95814, .T. ) ;
#55463 = CIRCLE ( 'NONE', #222068, 0.9000000000000014655 ) ;
#55464 = VERTEX_POINT ( 'NONE', #194962 ) ;
#55465 = CARTESIAN_POINT ( 'NONE',  ( -16.86578989773640913, 9.984809801269951990, -87.96466488662228755 ) ) ;
#55466 = CARTESIAN_POINT ( 'NONE',  ( 20.27550659511089037, 66.78395627750295205, -82.17310748452437963 ) ) ;
#55469 = ADVANCED_FACE ( 'NONE', ( #56673 ), #75025, .T. ) ;
#55468 = EDGE_LOOP ( 'NONE', ( #196746, #103837, #218496, #37001 ) ) ;
#55467 = DIRECTION ( 'NONE',  ( -1.000000000000000000, -0.000000000000000000, -0.000000000000000000 ) ) ;
#55470 = CARTESIAN_POINT ( 'NONE',  ( 21.05000000000000071, 76.00000000001186606, -90.87310748452429721 ) ) ;
#55471 = CARTESIAN_POINT ( 'NONE',  ( -20.85882249326303040, 65.66751761918692409, -130.9282609406112670 ) ) ;
#55472 = DIRECTION ( 'NONE',  ( 0.000000000000000000, 0.9651348961777157509, -0.2617529984165031243 ) ) ;
#55473 = DIRECTION ( 'NONE',  ( 0.000000000000000000, -6.308085367188393199E-16, -1.000000000000000000 ) ) ;
#55474 = AXIS2_PLACEMENT_3D ( 'NONE', #244880, #144478, #50510 ) ;
#55475 = EDGE_CURVE ( 'NONE', #135639, #127734, #126707, .T. ) ;
#55476 = FACE_OUTER_BOUND ( 'NONE', #208851, .T. ) ;
#55478 = DIRECTION ( 'NONE',  ( 0.000000000000000000, -6.982962677686267499E-15, 1.000000000000000000 ) ) ;
#55477 = TOROIDAL_SURFACE ( 'NONE', #217997, 0.6000000000000013101, 0.1000000000000000056 ) ;
#55479 = ADVANCED_FACE ( 'NONE', ( #177958 ), #30870, .T. ) ;
#55481 = EDGE_LOOP ( 'NONE', ( #156384, #70580, #71028 ) ) ;
#55480 = CARTESIAN_POINT ( 'NONE',  ( 20.85000000000000142, 7.128833340094563376, -233.7327013124401276 ) ) ;
#55483 = ORIENTED_EDGE ( 'NONE', *, *, #35554, .T. ) ;
#55482 = FACE_OUTER_BOUND ( 'NONE', #116381, .T. ) ;
#55485 = DIRECTION ( 'NONE',  ( 0.000000000000000000, 0.000000000000000000, 1.000000000000000000 ) ) ;
#55484 = DIRECTION ( 'NONE',  ( -1.000000000000000000, 0.000000000000000000, 0.000000000000000000 ) ) ;
#55487 = ORIENTED_EDGE ( 'NONE', *, *, #162121, .T. ) ;
#55486 = CARTESIAN_POINT ( 'NONE',  ( 21.05000000000000071, 8.876614585098257848, -75.38508047884472774 ) ) ;
#55488 = EDGE_LOOP ( 'NONE', ( #134650, #222400, #9984, #104769 ) ) ;
#55489 = CARTESIAN_POINT ( 'NONE',  ( -20.64999999999999858, -8.999999999988844479, -90.60603087734760663 ) ) ;
#55490 = DIRECTION ( 'NONE',  ( 0.000000000000000000, -1.000000000000000000, 0.000000000000000000 ) ) ;
#55492 = ADVANCED_FACE ( 'NONE', ( #138774 ), #157118, .F. ) ;
#55491 = DIRECTION ( 'NONE',  ( -1.652117596168391109E-15, -0.4721928772777345684, -0.8814952561688429444 ) ) ;
#55493 = CARTESIAN_POINT ( 'NONE',  ( 19.75857864376269646, 11.65000000001116476, -58.25000000000000000 ) ) ;
#55494 = CARTESIAN_POINT ( 'NONE',  ( -18.50211644919735932, 67.49401193140450061, -195.5283494629371432 ) ) ;
#55495 = FACE_OUTER_BOUND ( 'NONE', #228659, .T. ) ;
#55496 = CIRCLE ( 'NONE', #13849, 11.90000000000000568 ) ;
#55497 = CIRCLE ( 'NONE', #230530, 0.09999999999999939493 ) ;
#55499 = CIRCLE ( 'NONE', #17935, 12.77500000000000924 ) ;
#55498 = FACE_OUTER_BOUND ( 'NONE', #117881, .T. ) ;
#55500 = ORIENTED_EDGE ( 'NONE', *, *, #161650, .F. ) ;
#55501 = EDGE_LOOP ( 'NONE', ( #230470, #75316, #64775, #127019, #188659 ) ) ;
#55502 = CARTESIAN_POINT ( 'NONE',  ( 21.13435531349758634, 30.73270609305163603, -252.2060354990268252 ) ) ;
#55503 = ORIENTED_EDGE ( 'NONE', *, *, #218976, .F. ) ;
#55504 = CARTESIAN_POINT ( 'NONE',  ( 18.59999999999999787, -10.80884033489985363, 6.100000000000002309 ) ) ;
#55505 = CARTESIAN_POINT ( 'NONE',  ( 18.56579813702274961, 68.10670728244119232, -224.1434476749765565 ) ) ;
#55506 = EDGE_CURVE ( 'NONE', #199581, #104599, #218329, .T. ) ;
#55507 =( BOUNDED_CURVE ( )  B_SPLINE_CURVE ( 3, ( #28516, #70190, #225365, #8908 ),
 .UNSPECIFIED., .F., .T. ) 
 B_SPLINE_CURVE_WITH_KNOTS ( ( 4, 4 ),
 ( 3.141592653589793116, 4.712388980384689674 ),
 .UNSPECIFIED. ) 
 CURVE ( )  GEOMETRIC_REPRESENTATION_ITEM ( )  RATIONAL_B_SPLINE_CURVE ( ( 1.000000000000000000, 0.8047378541243649375, 0.8047378541243649375, 1.000000000000000000 ) ) 
 REPRESENTATION_ITEM ( '' )  );
#55508 = CARTESIAN_POINT ( 'NONE',  ( 16.27683809663750125, 11.10425270649115959, -208.0484446391143649 ) ) ;
#55509 = VERTEX_POINT ( 'NONE', #236620 ) ;
#55510 = EDGE_CURVE ( 'NONE', #84289, #227126, #176602, .T. ) ;
#55511 = ORIENTED_EDGE ( 'NONE', *, *, #69646, .F. ) ;
#55512 = ADVANCED_FACE ( 'NONE', ( #176681 ), #151678, .T. ) ;
#55513 = CARTESIAN_POINT ( 'NONE',  ( 21.05000000000000071, 85.40000000001207070, -126.6291383618717816 ) ) ;
#55514 = VERTEX_POINT ( 'NONE', #256125 ) ;
#55515 = CARTESIAN_POINT ( 'NONE',  ( -13.40000000000000213, -8.250000000000005329, 15.00000000000000355 ) ) ;
#55516 = DIRECTION ( 'NONE',  ( 1.000000000000000000, 0.000000000000000000, 0.000000000000000000 ) ) ;
#55517 = TOROIDAL_SURFACE ( 'NONE', #5466, 11.65000000000000036, 0.1000000000000000056 ) ;
#55518 = VERTEX_POINT ( 'NONE', #39749 ) ;
#55519 = AXIS2_PLACEMENT_3D ( 'NONE', #132013, #57596, #159303 ) ;
#55520 = CARTESIAN_POINT ( 'NONE',  ( -20.94999999999999929, 12.97363049771892207, -205.3537238898406940 ) ) ;
#55521 = ORIENTED_EDGE ( 'NONE', *, *, #123060, .T. ) ;
#55523 = ORIENTED_EDGE ( 'NONE', *, *, #234368, .T. ) ;
#55522 = CARTESIAN_POINT ( 'NONE',  ( 16.87683809663750267, 9.949999999999983302, -12.65000000000000036 ) ) ;
#55524 = CIRCLE ( 'NONE', #201879, 0.09999999999999939493 ) ;
#55525 = CARTESIAN_POINT ( 'NONE',  ( -21.05315837417582614, 64.25000000264169842, -42.86475148229496313 ) ) ;
#55526 = ORIENTED_EDGE ( 'NONE', *, *, #77388, .T. ) ;
#55527 = ORIENTED_EDGE ( 'NONE', *, *, #14646, .T. ) ;
#55528 = CIRCLE ( 'NONE', #126304, 0.09999999999999741040 ) ;
#55529 = CIRCLE ( 'NONE', #192963, 0.5999999999999998668 ) ;
#55530 = DIRECTION ( 'NONE',  ( 1.000000000000000000, 0.000000000000000000, 0.000000000000000000 ) ) ;
#55531 = ORIENTED_EDGE ( 'NONE', *, *, #137375, .F. ) ;
#55532 = SPHERICAL_SURFACE ( 'NONE', #210042, 0.1000000000000000056 ) ;
#55533 = CARTESIAN_POINT ( 'NONE',  ( 21.14999999999999858, 69.45934304831041572, -69.52310748452435973 ) ) ;
#55534 = DIRECTION ( 'NONE',  ( 1.000000000000000000, 0.000000000000000000, 0.000000000000000000 ) ) ;
#55535 = CARTESIAN_POINT ( 'NONE',  ( -21.12757541349819590, 0.005161215820883788274, -60.52661942874848222 ) ) ;
#55536 = EDGE_CURVE ( 'NONE', #189870, #109393, #43497, .T. ) ;
#55537 = ORIENTED_EDGE ( 'NONE', *, *, #128585, .T. ) ;
#55538 = AXIS2_PLACEMENT_3D ( 'NONE', #29060, #228518, #48576 ) ;
#55539 = VECTOR ( 'NONE', #81877, 1000.000000000000114 ) ;
#55540 = LINE ( 'NONE', #140228, #198503 ) ;
#55541 = CARTESIAN_POINT ( 'NONE',  ( -20.94999999999999929, 47.95459712139159336, -246.5019368548292675 ) ) ;
#55543 = CARTESIAN_POINT ( 'NONE',  ( 23.15000000000000213, 85.00000000001149658, -45.91707660717670336 ) ) ;
#55542 = TOROIDAL_SURFACE ( 'NONE', #163926, 11.70000000000000462, 0.1000000000000000056 ) ;
#55544 = EDGE_CURVE ( 'NONE', #42862, #181967, #97442, .T. ) ;
#55545 = ORIENTED_EDGE ( 'NONE', *, *, #8418, .F. ) ;
#55546 = FACE_OUTER_BOUND ( 'NONE', #63305, .T. ) ;
#55547 = VERTEX_POINT ( 'NONE', #159676 ) ;
#55548 = DIRECTION ( 'NONE',  ( 1.000000000000000000, 0.000000000000000000, 0.000000000000000000 ) ) ;
#55550 = ORIENTED_EDGE ( 'NONE', *, *, #203848, .F. ) ;
#55549 = AXIS2_PLACEMENT_3D ( 'NONE', #100740, #239018, #36993 ) ;
#55551 = CARTESIAN_POINT ( 'NONE',  ( 21.05000000000000071, 1.115600667400684642E-11, -167.5000000000000284 ) ) ;
#55554 = ORIENTED_EDGE ( 'NONE', *, *, #194000, .T. ) ;
#55553 = EDGE_CURVE ( 'NONE', #156063, #114275, #18862, .T. ) ;
#55552 = CARTESIAN_POINT ( 'NONE',  ( 23.15000000000000213, 84.66355140188123585, -126.9990063664569391 ) ) ;
#55555 = CARTESIAN_POINT ( 'NONE',  ( -18.34374000495059676, 11.47316190337362940, -124.7500000000000426 ) ) ;
#55556 = EDGE_LOOP ( 'NONE', ( #65204, #255478, #182061, #231073 ) ) ;
#55557 = VECTOR ( 'NONE', #64065, 1000.000000000000000 ) ;
#55558 = CARTESIAN_POINT ( 'NONE',  ( 21.05000000000000071, 38.33376540847015690, -250.4483291680710693 ) ) ;
#55559 = EDGE_CURVE ( 'NONE', #153327, #95642, #55938, .T. ) ;
#55560 = DIRECTION ( 'NONE',  ( 0.000000000000000000, 0.000000000000000000, -1.000000000000000000 ) ) ;
#55561 = ORIENTED_EDGE ( 'NONE', *, *, #47788, .F. ) ;
#55562 = CIRCLE ( 'NONE', #122247, 0.09999999999999939493 ) ;
#55563 = LINE ( 'NONE', #142816, #47479 ) ;
#55565 = EDGE_CURVE ( 'NONE', #71736, #118383, #243209, .T. ) ;
#55564 = CARTESIAN_POINT ( 'NONE',  ( -20.96077737575314970, 11.62390063401601381, -194.1407919571067566 ) ) ;
#55566 = ORIENTED_EDGE ( 'NONE', *, *, #228458, .F. ) ;
#55567 = CARTESIAN_POINT ( 'NONE',  ( 21.05000000000046256, 10.18588724833545989, -228.0632827051668414 ) ) ;
#55568 = CIRCLE ( 'NONE', #234688, 0.5000000000000004441 ) ;
#55569 = ORIENTED_EDGE ( 'NONE', *, *, #5808, .T. ) ;
#55570 = EDGE_CURVE ( 'NONE', #45673, #132976, #130789, .T. ) ;
#55571 = DIRECTION ( 'NONE',  ( 0.000000000000000000, 0.000000000000000000, -1.000000000000000000 ) ) ;
#55572 = AXIS2_PLACEMENT_3D ( 'NONE', #147483, #94880, #227011 ) ;
#55574 = EDGE_CURVE ( 'NONE', #237061, #88867, #235042, .T. ) ;
#55573 = DIRECTION ( 'NONE',  ( -1.000000000000000000, 0.000000000000000000, -0.000000000000000000 ) ) ;
#55576 = ORIENTED_EDGE ( 'NONE', *, *, #256119, .F. ) ;
#55575 = LINE ( 'NONE', #39930, #117992 ) ;
#55577 = CARTESIAN_POINT ( 'NONE',  ( -20.64999999999999858, 84.73084112150721126, -93.42503276553991043 ) ) ;
#55578 = FACE_OUTER_BOUND ( 'NONE', #233827, .T. ) ;
#55579 = FACE_OUTER_BOUND ( 'NONE', #45277, .T. ) ;
#55581 = CARTESIAN_POINT ( 'NONE',  ( -23.15000000000000213, 7.128833340094563376, -233.7327013124401276 ) ) ;
#55580 = CARTESIAN_POINT ( 'NONE',  ( 21.15000000000005187, 74.94272479589878344, -3.023107484524792277 ) ) ;
#55582 = CARTESIAN_POINT ( 'NONE',  ( -20.64999999999999858, 7.250000000011155521, -121.6500000000000341 ) ) ;
#55583 = DIRECTION ( 'NONE',  ( -1.000000000000000000, 0.000000000000000000, 0.000000000000000000 ) ) ;
#55584 = CIRCLE ( 'NONE', #18026, 0.1000000000000028644 ) ;
#55585 = CARTESIAN_POINT ( 'NONE',  ( 18.45068634130097252, -9.486506073331602451, -40.56877843116809856 ) ) ;
#55586 = AXIS2_PLACEMENT_3D ( 'NONE', #178055, #115483, #78904 ) ;
#55587 = CARTESIAN_POINT ( 'NONE',  ( 20.94999999999999929, 76.00000000001126921, -203.5231074845248997 ) ) ;
#55589 = EDGE_CURVE ( 'NONE', #192971, #123899, #243047, .T. ) ;
#55588 = VECTOR ( 'NONE', #119396, 1000.000000000000000 ) ;
#55590 = AXIS2_PLACEMENT_3D ( 'NONE', #200266, #85407, #103696 ) ;
#55591 = ADVANCED_FACE ( 'NONE', ( #64424 ), #189258, .T. ) ;
#55592 = ORIENTED_EDGE ( 'NONE', *, *, #236387, .F. ) ;
#55593 = ORIENTED_EDGE ( 'NONE', *, *, #203975, .T. ) ;
#55594 = CARTESIAN_POINT ( 'NONE',  ( 21.05000000000000071, 77.07318729351892728, -199.5660544101962728 ) ) ;
#55595 = VERTEX_POINT ( 'NONE', #240485 ) ;
#55596 = VERTEX_POINT ( 'NONE', #65697 ) ;
#55597 = LINE ( 'NONE', #193871, #93579 ) ;
#55598 = VERTEX_POINT ( 'NONE', #4429 ) ;
#55599 = DIRECTION ( 'NONE',  ( 0.000000000000000000, -0.9126074666063771490, -0.4088369013363281623 ) ) ;
#55600 = ADVANCED_FACE ( 'NONE', ( #145224 ), #76622, .T. ) ;
#55601 = ORIENTED_EDGE ( 'NONE', *, *, #22877, .T. ) ;
#55602 = CARTESIAN_POINT ( 'NONE',  ( -20.94999999999999929, 79.28653038861995128, -235.9126307598797325 ) ) ;
#55603 = ADVANCED_FACE ( 'NONE', ( #143943 ), #64171, .T. ) ;
#55605 = EDGE_LOOP ( 'NONE', ( #175834, #200025, #25518, #193792 ) ) ;
#55604 = VERTEX_POINT ( 'NONE', #162255 ) ;
#55606 = ORIENTED_EDGE ( 'NONE', *, *, #140249, .T. ) ;
#55607 = ORIENTED_EDGE ( 'NONE', *, *, #146951, .T. ) ;
#55608 = ORIENTED_EDGE ( 'NONE', *, *, #104327, .F. ) ;
#55609 = DIRECTION ( 'NONE',  ( 0.000000000000000000, -0.9651348961777157509, 0.2617529984165031243 ) ) ;
#55610 = AXIS2_PLACEMENT_3D ( 'NONE', #8055, #228385, #10619 ) ;
#55611 = CARTESIAN_POINT ( 'NONE',  ( -18.46902351632713035, -9.509470118680869888, -6.986453934257316867 ) ) ;
#55613 = VERTEX_POINT ( 'NONE', #123117 ) ;
#55612 = CARTESIAN_POINT ( 'NONE',  ( 21.05000000000000071, 1.115600667400684642E-11, -134.0000000000000000 ) ) ;
#55614 = CARTESIAN_POINT ( 'NONE',  ( 20.30466543256828160, 40.38736318471006115, -237.6856447363348650 ) ) ;
#55615 = EDGE_CURVE ( 'NONE', #211067, #184002, #143269, .T. ) ;
#55616 = CARTESIAN_POINT ( 'NONE',  ( 14.11444803880197085, 12.43281162335558676, -213.6438014222476056 ) ) ;
#55618 = ORIENTED_EDGE ( 'NONE', *, *, #150387, .F. ) ;
#55617 = FACE_OUTER_BOUND ( 'NONE', #71674, .T. ) ;
#55619 = EDGE_LOOP ( 'NONE', ( #64279, #72221, #183296, #64535 ) ) ;
#55620 = CARTESIAN_POINT ( 'NONE',  ( 20.94999999999999929, 76.00000000001190870, -103.0231074845243029 ) ) ;
#55622 = EDGE_LOOP ( 'NONE', ( #252594, #225593, #112032, #161139 ) ) ;
#55621 = DIRECTION ( 'NONE',  ( 0.000000000000000000, 1.000000000000000000, 0.000000000000000000 ) ) ;
#55623 = DIRECTION ( 'NONE',  ( 1.000000000000000000, 0.000000000000000000, 0.000000000000000000 ) ) ;
#55624 = FACE_OUTER_BOUND ( 'NONE', #3934, .T. ) ;
#55626 = ADVANCED_FACE ( 'NONE', ( #125670 ), #239086, .T. ) ;
#55625 = ORIENTED_EDGE ( 'NONE', *, *, #130285, .T. ) ;
#55628 = CARTESIAN_POINT ( 'NONE',  ( -21.14999999999999858, 64.25000000001190870, -96.23924182154622997 ) ) ;
#55627 = DIRECTION ( 'NONE',  ( 0.000000000000000000, 0.000000000000000000, 1.000000000000000000 ) ) ;
#55629 = AXIS2_PLACEMENT_3D ( 'NONE', #160785, #179066, #79893 ) ;
#55630 = LINE ( 'NONE', #120806, #126693 ) ;
#55631 = AXIS2_PLACEMENT_3D ( 'NONE', #16704, #115785, #152376 ) ;
#55632 = DIRECTION ( 'NONE',  ( 0.000000000000000000, -0.000000000000000000, 1.000000000000000000 ) ) ;
#55633 = DIRECTION ( 'NONE',  ( 1.000000000000000000, 0.000000000000000000, 0.000000000000000000 ) ) ;
#55634 = ORIENTED_EDGE ( 'NONE', *, *, #50873, .T. ) ;
#55636 = VERTEX_POINT ( 'NONE', #241761 ) ;
#55635 = AXIS2_PLACEMENT_3D ( 'NONE', #140313, #120797, #219862 ) ;
#55637 = CARTESIAN_POINT ( 'NONE',  ( 23.14999999999999858, 76.00000000001173817, -73.52310748452431710 ) ) ;
#55638 = DIRECTION ( 'NONE',  ( 0.000000000000000000, 0.9908441862701605762, -0.1350103645451835310 ) ) ;
#55639 = ORIENTED_EDGE ( 'NONE', *, *, #213764, .T. ) ;
#55640 = CARTESIAN_POINT ( 'NONE',  ( -23.25000000000000000, 87.75000000001213607, -136.5231074845242176 ) ) ;
#55641 = ORIENTED_EDGE ( 'NONE', *, *, #184198, .T. ) ;
#55642 = EDGE_CURVE ( 'NONE', #128967, #50451, #1848, .T. ) ;
#55643 = DIRECTION ( 'NONE',  ( -1.000000000000000000, -0.000000000000000000, -0.000000000000000000 ) ) ;
#55644 = DIRECTION ( 'NONE',  ( 0.000000000000000000, 0.000000000000000000, 1.000000000000000000 ) ) ;
#55645 = VERTEX_POINT ( 'NONE', #203924 ) ;
#55646 = AXIS2_PLACEMENT_3D ( 'NONE', #630, #58040, #138845 ) ;
#55647 = CARTESIAN_POINT ( 'NONE',  ( 20.94999999999999929, 11.65000000001115943, -134.0000000000000284 ) ) ;
#55648 = ORIENTED_EDGE ( 'NONE', *, *, #213135, .T. ) ;
#55649 = ORIENTED_EDGE ( 'NONE', *, *, #90077, .T. ) ;
#55650 = AXIS2_PLACEMENT_3D ( 'NONE', #114237, #212071, #13861 ) ;
#55651 = ORIENTED_EDGE ( 'NONE', *, *, #26721, .F. ) ;
#55652 = CIRCLE ( 'NONE', #243127, 0.09999999999999939493 ) ;
#55653 = CARTESIAN_POINT ( 'NONE',  ( 18.49999999999999645, 44.52640028187936849, -247.3006740988509193 ) ) ;
#55654 = DIRECTION ( 'NONE',  ( 0.000000000000000000, 0.000000000000000000, 1.000000000000000000 ) ) ;
#55655 = CARTESIAN_POINT ( 'NONE',  ( 20.99999999999999645, 9.750000000011137757, -154.8500000000000227 ) ) ;
#55656 = LINE ( 'NONE', #94818, #36212 ) ;
#55657 = LINE ( 'NONE', #157407, #204968 ) ;
#55659 = CARTESIAN_POINT ( 'NONE',  ( 23.14999999999999858, 1.115600667400684642E-11, -167.4999999999999716 ) ) ;
#55658 = DIRECTION ( 'NONE',  ( 0.000000000000000000, 0.000000000000000000, -1.000000000000000000 ) ) ;
#55661 = VERTEX_POINT ( 'NONE', #7008 ) ;
#55660 = CYLINDRICAL_SURFACE ( 'NONE', #68794, 0.1000000000000124678 ) ;
#55662 = DIRECTION ( 'NONE',  ( 0.000000000000000000, 6.982962677686266711E-15, -1.000000000000000000 ) ) ;
#55663 = EDGE_LOOP ( 'NONE', ( #167233, #113966, #137149, #66744 ) ) ;
#55664 = DIRECTION ( 'NONE',  ( -0.000000000000000000, 1.000000000000000000, 6.982962677686266711E-15 ) ) ;
#55665 = ORIENTED_EDGE ( 'NONE', *, *, #247727, .T. ) ;
#55666 = EDGE_LOOP ( 'NONE', ( #70397, #206194, #33099, #174214 ) ) ;
#55667 = CARTESIAN_POINT ( 'NONE',  ( -16.93433913041102912, 65.99402157848757611, -48.58774205712922623 ) ) ;
#55668 = AXIS2_PLACEMENT_3D ( 'NONE', #168939, #46357, #64650 ) ;
#55669 = CARTESIAN_POINT ( 'NONE',  ( -16.88495309932522659, 66.04537294153871585, -56.88855881071248177 ) ) ;
#55670 = AXIS2_PLACEMENT_3D ( 'NONE', #64911, #219690, #136281 ) ;
#55671 = DIRECTION ( 'NONE',  ( 0.000000000000000000, -0.000000000000000000, 1.000000000000000000 ) ) ;
#55672 = CIRCLE ( 'NONE', #63909, 0.1000000000000020595 ) ;
#55673 = CARTESIAN_POINT ( 'NONE',  ( -20.64999999999999858, 1.115623935689868526E-11, -199.0999999999999375 ) ) ;
#55674 = ORIENTED_EDGE ( 'NONE', *, *, #235803, .F. ) ;
#55675 = ORIENTED_EDGE ( 'NONE', *, *, #117083, .F. ) ;
#55676 = AXIS2_PLACEMENT_3D ( 'NONE', #157931, #140893, #237422 ) ;
#55677 = LINE ( 'NONE', #216064, #61676 ) ;
#55678 = EDGE_LOOP ( 'NONE', ( #6311, #126468, #67675, #115085 ) ) ;
#55679 = DIRECTION ( 'NONE',  ( 0.000000000000000000, -0.9908441862701420355, -0.1350103645453197554 ) ) ;
#55680 = DIRECTION ( 'NONE',  ( -1.000000000000000000, 0.000000000000000000, 0.000000000000000000 ) ) ;
#55681 = VERTEX_POINT ( 'NONE', #163519 ) ;
#55682 = CYLINDRICAL_SURFACE ( 'NONE', #111612, 0.5000000000000004441 ) ;
#55683 = CARTESIAN_POINT ( 'NONE',  ( -20.96428641294228612, 11.75000000001149125, -60.17489317794078119 ) ) ;
#55684 = DIRECTION ( 'NONE',  ( 1.000000000000000000, 0.000000000000000000, 0.000000000000000000 ) ) ;
#55685 = CARTESIAN_POINT ( 'NONE',  ( 20.97468175916167255, 65.37473483564126298, -157.7683460491116421 ) ) ;
#55686 = ORIENTED_EDGE ( 'NONE', *, *, #165111, .T. ) ;
#55687 = AXIS2_PLACEMENT_3D ( 'NONE', #40428, #177368, #176080 ) ;
#55688 = VECTOR ( 'NONE', #247932, 1000.000000000000000 ) ;
#55689 = CIRCLE ( 'NONE', #180629, 0.1000000000000028644 ) ;
#55690 = FACE_OUTER_BOUND ( 'NONE', #237487, .T. ) ;
#55691 = EDGE_CURVE ( 'NONE', #30344, #75338, #139134, .T. ) ;
#55692 = DIRECTION ( 'NONE',  ( -1.000000000000000000, 0.000000000000000000, -0.000000000000000000 ) ) ;
#55693 = EDGE_LOOP ( 'NONE', ( #205940, #165329, #77022, #225266 ) ) ;
#55694 = CARTESIAN_POINT ( 'NONE',  ( 23.14999999999999503, 36.06460295787456261, -236.0166209342146146 ) ) ;
#55695 = ORIENTED_EDGE ( 'NONE', *, *, #173932, .F. ) ;
#55696 = LINE ( 'NONE', #214808, #34876 ) ;
#55697 = CARTESIAN_POINT ( 'NONE',  ( -16.93521499325732549, 14.21491466131654668, -219.3013425272998518 ) ) ;
#55698 = CARTESIAN_POINT ( 'NONE',  ( 21.14999999999999858, 63.99342642423710714, -222.3880800784493772 ) ) ;
#55699 = FACE_OUTER_BOUND ( 'NONE', #107128, .T. ) ;
#55700 = CARTESIAN_POINT ( 'NONE',  ( -21.64999999999999858, 7.350000000011155166, -179.8499999999999943 ) ) ;
#55701 = DIRECTION ( 'NONE',  ( -0.000000000000000000, -0.000000000000000000, 1.000000000000000000 ) ) ;
#55702 = EDGE_CURVE ( 'NONE', #101410, #3545, #245628, .T. ) ;
#55703 = EDGE_LOOP ( 'NONE', ( #219416, #237301, #257910, #126820 ) ) ;
#55704 = CARTESIAN_POINT ( 'NONE',  ( -16.92209698673614326, 66.05000000001224691, -149.2337430515783581 ) ) ;
#55705 = AXIS2_PLACEMENT_3D ( 'NONE', #59619, #218709, #40126 ) ;
#55706 = CARTESIAN_POINT ( 'NONE',  ( -16.88005004766534967, 66.04989949669077021, -82.17277137257562458 ) ) ;
#55707 = DIRECTION ( 'NONE',  ( 0.000000000000000000, -0.9908441862701791170, 0.1350103645450472789 ) ) ;
#55709 = TOROIDAL_SURFACE ( 'NONE', #84937, 11.65000000000000036, 0.1000000000000000056 ) ;
#55708 = CARTESIAN_POINT ( 'NONE',  ( 20.94999999999999574, 1.162701749938009677, -8.099999999999999645 ) ) ;
#55710 = AXIS2_PLACEMENT_3D ( 'NONE', #151083, #89803, #209773 ) ;
#55711 = DIRECTION ( 'NONE',  ( 1.000000000000000000, 0.000000000000000000, 0.000000000000000000 ) ) ;
#55712 = EDGE_LOOP ( 'NONE', ( #239425, #253349, #230194, #206179 ) ) ;
#55713 = ORIENTED_EDGE ( 'NONE', *, *, #169386, .F. ) ;
#55714 = CARTESIAN_POINT ( 'NONE',  ( -21.05000000000000071, 76.00000000001267608, -203.5231074845243597 ) ) ;
#55715 = AXIS2_PLACEMENT_3D ( 'NONE', #143718, #163301, #47168 ) ;
#55716 = CARTESIAN_POINT ( 'NONE',  ( 21.14999999999999503, 64.35000000001164722, -69.42310748452440805 ) ) ;
#55718 = EDGE_CURVE ( 'NONE', #26810, #240054, #72760, .T. ) ;
#55717 = CARTESIAN_POINT ( 'NONE',  ( -15.55912972643741199, 8.490870273573719373, -113.0500000000000398 ) ) ;
#55719 = CARTESIAN_POINT ( 'NONE',  ( 21.05000000000000071, 59.13236860818124541, -225.8959333647716505 ) ) ;
#55720 = LINE ( 'NONE', #234390, #174714 ) ;
#55721 = EDGE_CURVE ( 'NONE', #175831, #165098, #160966, .T. ) ;
#55722 = ORIENTED_EDGE ( 'NONE', *, *, #176870, .F. ) ;
#55723 = CYLINDRICAL_SURFACE ( 'NONE', #222144, 0.09999999999999939493 ) ;
#55724 = AXIS2_PLACEMENT_3D ( 'NONE', #187288, #28227, #148139 ) ;
#55725 = EDGE_CURVE ( 'NONE', #157401, #212672, #68280, .T. ) ;
#55727 = AXIS2_PLACEMENT_3D ( 'NONE', #149647, #224013, #50495 ) ;
#55726 = DIRECTION ( 'NONE',  ( 0.000000000000000000, 0.2617529984165120616, 0.9651348961777134194 ) ) ;
#55728 = ORIENTED_EDGE ( 'NONE', *, *, #147704, .T. ) ;
#55729 = DIRECTION ( 'NONE',  ( 0.000000000000000000, -0.9770955615653316162, -0.2128009952263604232 ) ) ;
#55730 = AXIS2_PLACEMENT_3D ( 'NONE', #8960, #246293, #247568 ) ;
#55731 = ADVANCED_FACE ( 'NONE', ( #12176 ), #160230, .T. ) ;
#55732 = VECTOR ( 'NONE', #220528, 1000.000000000000000 ) ;
#55733 = PRODUCT_DEFINITION_SHAPE ( 'NONE', 'NONE',  #258117 ) ;
#55734 = CARTESIAN_POINT ( 'NONE',  ( 18.59999999999999076, 6.450000000011156587, -144.0170271704400307 ) ) ;
#55735 = CIRCLE ( 'NONE', #234850, 0.5000000000000008882 ) ;
#55736 = EDGE_CURVE ( 'NONE', #140838, #41279, #114421, .T. ) ;
#55737 = EDGE_LOOP ( 'NONE', ( #53084, #247382, #83465, #233748 ) ) ;
#55738 = CARTESIAN_POINT ( 'NONE',  ( -18.35663730107557257, 64.52609257350141547, -194.2731074845244450 ) ) ;
#55739 = ORIENTED_EDGE ( 'NONE', *, *, #251038, .F. ) ;
#55740 = DIRECTION ( 'NONE',  ( 1.000000000000000000, 0.000000000000000000, 0.000000000000000000 ) ) ;
#55741 = DIRECTION ( 'NONE',  ( 0.000000000000000000, -1.000000000000000000, -6.982962677686265922E-15 ) ) ;
#55743 = CIRCLE ( 'NONE', #243033, 0.1000000000000000472 ) ;
#55742 = DIRECTION ( 'NONE',  ( -0.000000000000000000, 0.9876197685951276783, 0.1568667991644721316 ) ) ;
#55744 = CARTESIAN_POINT ( 'NONE',  ( -20.64999999999999858, 6.268811756569107274, -220.3853799378769622 ) ) ;
#55745 = CARTESIAN_POINT ( 'NONE',  ( -23.25000000000000000, -1.736705739456431807, -179.0174225876237415 ) ) ;
#55746 = CARTESIAN_POINT ( 'NONE',  ( -18.59999999999999787, 11.65000000001115232, -74.01480577065404987 ) ) ;
#55747 = DIRECTION ( 'NONE',  ( 0.000000000000000000, -6.982962677686266711E-15, 1.000000000000000000 ) ) ;
#55748 = EDGE_CURVE ( 'NONE', #133820, #12214, #189516, .T. ) ;
#55750 = DIRECTION ( 'NONE',  ( 2.952720810173289112E-16, -1.000000000000000000, -0.000000000000000000 ) ) ;
#55749 = DIRECTION ( 'NONE',  ( -1.000000000000000000, 0.000000000000000000, 0.000000000000000000 ) ) ;
#55751 = CIRCLE ( 'NONE', #243037, 0.5000000000000001110 ) ;
#55752 = CARTESIAN_POINT ( 'NONE',  ( -18.59999999999999787, 7.070967871809997973, -204.7465642218682547 ) ) ;
#55753 = CARTESIAN_POINT ( 'NONE',  ( 21.05000000000000071, 85.50000000001149658, -45.91707660717669626 ) ) ;
#55754 = CARTESIAN_POINT ( 'NONE',  ( -18.50000000000000000, -1.687074390080403941, -54.18542703345839584 ) ) ;
#55755 = ORIENTED_EDGE ( 'NONE', *, *, #90782, .F. ) ;
#55756 = AXIS2_PLACEMENT_3D ( 'NONE', #148662, #66549, #250313 ) ;
#55757 = DIRECTION ( 'NONE',  ( 1.000000000000000000, 0.000000000000000000, -0.000000000000000000 ) ) ;
#55758 = CARTESIAN_POINT ( 'NONE',  ( 21.05000000000000071, -8.730841121495327428, -9.598074718984332065 ) ) ;
#55759 = AXIS2_PLACEMENT_3D ( 'NONE', #177212, #179758, #215015 ) ;
#55760 = AXIS2_PLACEMENT_3D ( 'NONE', #82682, #241791, #162278 ) ;
#55761 = EDGE_LOOP ( 'NONE', ( #189370, #242203, #235291, #215795 ) ) ;
#55762 = CARTESIAN_POINT ( 'NONE',  ( -23.15000000000000213, 4.350000000011156054, -79.35000000000005116 ) ) ;
#55763 = DIRECTION ( 'NONE',  ( -0.000000000000000000, -6.982962677686266711E-15, 1.000000000000000000 ) ) ;
#55764 = CARTESIAN_POINT ( 'NONE',  ( 20.94999999999999929, 46.41626913442612334, -243.0004334082109096 ) ) ;
#55765 = APPLICATION_CONTEXT ( 'automotive_design' ) ;
#55766 = ORIENTED_EDGE ( 'NONE', *, *, #74976, .F. ) ;
#55767 = DIRECTION ( 'NONE',  ( -0.000000000000000000, 1.000000000000000000, -0.000000000000000000 ) ) ;
#55768 = ORIENTED_EDGE ( 'NONE', *, *, #127259, .T. ) ;
#55769 = CARTESIAN_POINT ( 'NONE',  ( 20.94999999999999929, 36.65892442174472876, -249.5511627012454596 ) ) ;
#55770 = DIRECTION ( 'NONE',  ( 1.000000000000000000, 0.000000000000000000, -0.000000000000000000 ) ) ;
#55771 = AXIS2_PLACEMENT_3D ( 'NONE', #144324, #79225, #140488 ) ;
#55772 = CIRCLE ( 'NONE', #109976, 11.65000000000000036 ) ;
#55773 = ADVANCED_FACE ( 'NONE', ( #130809 ), #32739, .F. ) ;
#55774 = EDGE_CURVE ( 'NONE', #242867, #19033, #219271, .T. ) ;
#55775 = ORIENTED_EDGE ( 'NONE', *, *, #84104, .F. ) ;
#55776 = DIRECTION ( 'NONE',  ( 1.000000000000000000, 0.000000000000000000, 0.000000000000000000 ) ) ;
#55777 = EDGE_LOOP ( 'NONE', ( #136040, #25175, #157484, #161412 ) ) ;
#55778 = EDGE_CURVE ( 'NONE', #100761, #168461, #33050, .T. ) ;
#55780 = ADVANCED_FACE ( 'NONE', ( #112547 ), #210363, .T. ) ;
#55779 = DIRECTION ( 'NONE',  ( 0.7070776581709139474, 0.7071359030027652981, 2.946958787807621248E-14 ) ) ;
#55781 = CARTESIAN_POINT ( 'NONE',  ( 21.13461538461538680, 67.11458296203758778, -124.1731074845243512 ) ) ;
#55783 = DIRECTION ( 'NONE',  ( 1.020425574104003999E-15, 0.2128009952263603677, -0.9770955615653313941 ) ) ;
#55782 = UNCERTAINTY_MEASURE_WITH_UNIT (LENGTH_MEASURE( 1.000000000000000082E-05 ), #14008, 'distance_accuracy_value', 'NONE');
#55784 = DIRECTION ( 'NONE',  ( 2.694716079187272946E-16, -1.000000000000000000, 0.000000000000000000 ) ) ;
#55785 = DIRECTION ( 'NONE',  ( -1.000000000000000000, -0.000000000000000000, -0.000000000000000000 ) ) ;
#55786 = CARTESIAN_POINT ( 'NONE',  ( -21.14999999999999858, 76.00000000001199396, -109.2816861282870065 ) ) ;
#55787 = EDGE_CURVE ( 'NONE', #225819, #217036, #14490, .T. ) ;
#55788 = CARTESIAN_POINT ( 'NONE',  ( 18.39999999999999503, 70.35000000001181775, -82.17310748452435121 ) ) ;
#55789 = FACE_OUTER_BOUND ( 'NONE', #137189, .T. ) ;
#55791 = EDGE_LOOP ( 'NONE', ( #243649, #80888, #122806, #98019 ) ) ;
#55790 = DIRECTION ( 'NONE',  ( -1.000000000000000000, -1.836970198721029934E-16, 0.000000000000000000 ) ) ;
#55792 = ORIENTED_EDGE ( 'NONE', *, *, #26916, .F. ) ;
#55794 = DIRECTION ( 'NONE',  ( -0.7071067811865389130, 0.000000000000000000, 0.7071067811865561215 ) ) ;
#55793 = CARTESIAN_POINT ( 'NONE',  ( -21.05000000000000426, 6.332272273935660500, -0.03753606328566801847 ) ) ;
#55796 = EDGE_LOOP ( 'NONE', ( #247593, #136238, #174862, #42847 ) ) ;
#55795 =( NAMED_UNIT ( * ) PLANE_ANGLE_UNIT ( ) SI_UNIT ( $, .RADIAN. ) );
#55797 = EDGE_CURVE ( 'NONE', #161777, #76140, #59300, .T. ) ;
#55798 = ORIENTED_EDGE ( 'NONE', *, *, #166904, .F. ) ;
#55799 = DIRECTION ( 'NONE',  ( -1.000000000000000000, 0.000000000000000000, 0.000000000000000000 ) ) ;
#55800 = EDGE_CURVE ( 'NONE', #86874, #195448, #175891, .T. ) ;
#55801 = CARTESIAN_POINT ( 'NONE',  ( 20.97438252431638972, 8.925423506087151182, -175.9723706890107735 ) ) ;
#55802 = AXIS2_PLACEMENT_3D ( 'NONE', #242484, #221620, #44307 ) ;
#55804 = ADVANCED_FACE ( 'NONE', ( #192092, #186964 ), #53849, .T. ) ;
#55803 = FACE_OUTER_BOUND ( 'NONE', #28801, .T. ) ;
#55805 = CARTESIAN_POINT ( 'NONE',  ( 6.100000000000049383, 64.25000000001119815, -51.02310748452480738 ) ) ;
#55806 = CARTESIAN_POINT ( 'NONE',  ( -23.15000000000000213, 17.01923898301589944, -224.3994341343041867 ) ) ;
#55807 = LINE ( 'NONE', #135367, #247865 ) ;
#55808 = FACE_OUTER_BOUND ( 'NONE', #13252, .T. ) ;
#55809 = EDGE_CURVE ( 'NONE', #201418, #89935, #247689, .T. ) ;
#55810 = CYLINDRICAL_SURFACE ( 'NONE', #81193, 0.09999999999999939493 ) ;
#55811 = ORIENTED_EDGE ( 'NONE', *, *, #230789, .T. ) ;
#55812 = ORIENTED_EDGE ( 'NONE', *, *, #142407, .T. ) ;
#55813 = CARTESIAN_POINT ( 'NONE',  ( -20.15000000000000568, 66.70857864377450142, -81.87310748452438247 ) ) ;
#55814 = EDGE_CURVE ( 'NONE', #136089, #149361, #134639, .T. ) ;
#55816 = ADVANCED_FACE ( 'NONE', ( #55094 ), #76997, .F. ) ;
#55815 = CIRCLE ( 'NONE', #176673, 0.09999999999999939493 ) ;
#55817 = AXIS2_PLACEMENT_3D ( 'NONE', #127336, #86897, #8675 ) ;
#55818 = VERTEX_POINT ( 'NONE', #155549 ) ;
#55819 = DIRECTION ( 'NONE',  ( -1.000000000000000000, -0.000000000000000000, -0.000000000000000000 ) ) ;
#55820 = ORIENTED_EDGE ( 'NONE', *, *, #197140, .T. ) ;
#55821 = CARTESIAN_POINT ( 'NONE',  ( 18.46163235739470920, -9.480150806918276274, -40.15761053987758800 ) ) ;
#55822 = AXIS2_PLACEMENT_3D ( 'NONE', #160595, #161871, #21082 ) ;
#55823 = AXIS2_PLACEMENT_3D ( 'NONE', #169244, #190055, #109216 ) ;
#55824 = EDGE_CURVE ( 'NONE', #128131, #60636, #135247, .T. ) ;
#55825 = DIRECTION ( 'NONE',  ( 0.000000000000000000, 6.982962677686266711E-15, -1.000000000000000000 ) ) ;
#55826 = DIRECTION ( 'NONE',  ( -0.000000000000000000, 1.000000000000000000, 6.982962677686267499E-15 ) ) ;
#55828 = VERTEX_POINT ( 'NONE', #98069 ) ;
#55827 = CARTESIAN_POINT ( 'NONE',  ( -21.05000000000000071, 5.850000000011108092, -43.63249722427796939 ) ) ;
#55829 = EDGE_CURVE ( 'NONE', #169542, #251285, #22857, .T. ) ;
#55830 = CARTESIAN_POINT ( 'NONE',  ( 18.49999999999999645, -1.835859311432484375, -112.0044391687985694 ) ) ;
#55831 = ORIENTED_EDGE ( 'NONE', *, *, #3205, .F. ) ;
#55832 = EDGE_CURVE ( 'NONE', #64423, #16861, #218027, .T. ) ;
#55833 = CARTESIAN_POINT ( 'NONE',  ( 18.39999999999999503, 11.47316190337363828, -180.1499999999999773 ) ) ;
#55834 = CARTESIAN_POINT ( 'NONE',  ( -18.59999999999999787, 85.52395432076417592, -29.14109042769694469 ) ) ;
#55835 = DIRECTION ( 'NONE',  ( 1.000000000000000000, 0.000000000000000000, 0.000000000000000000 ) ) ;
#55837 = CIRCLE ( 'NONE', #243293, 0.5000000000000004441 ) ;
#55836 = DIRECTION ( 'NONE',  ( 0.000000000000000000, -0.4721928772776935457, -0.8814952561688651489 ) ) ;
#55838 = CARTESIAN_POINT ( 'NONE',  ( 19.92426406871192412, 11.75000000001116085, -125.3500000000000512 ) ) ;
#55839 = ORIENTED_EDGE ( 'NONE', *, *, #217458, .T. ) ;
#55841 = CARTESIAN_POINT ( 'NONE',  ( 18.49999999999999645, 58.44755627554218336, -246.4682640075163818 ) ) ;
#55840 = FACE_OUTER_BOUND ( 'NONE', #113637, .T. ) ;
#55843 = ORIENTED_EDGE ( 'NONE', *, *, #159153, .T. ) ;
#55842 = AXIS2_PLACEMENT_3D ( 'NONE', #137826, #38754, #120881 ) ;
#55846 = EDGE_LOOP ( 'NONE', ( #94213, #57779, #168838, #154175 ) ) ;
#55845 = DIRECTION ( 'NONE',  ( -0.000000000000000000, -6.982962677686266711E-15, 1.000000000000000000 ) ) ;
#55844 = FACE_OUTER_BOUND ( 'NONE', #189846, .T. ) ;
#55847 = DIRECTION ( 'NONE',  ( 1.000000000000000000, -0.000000000000000000, -0.000000000000000000 ) ) ;
#55848 = VECTOR ( 'NONE', #154678, 1000.000000000000227 ) ;
#55849 = AXIS2_PLACEMENT_3D ( 'NONE', #210827, #111729, #171735 ) ;
#55850 = FACE_OUTER_BOUND ( 'NONE', #6153, .T. ) ;
#55851 = ORIENTED_EDGE ( 'NONE', *, *, #134384, .F. ) ;
#55853 = PLANE ( 'NONE',  #230412 ) ;
#55852 = AXIS2_PLACEMENT_3D ( 'NONE', #39461, #64124, #241480 ) ;
#55854 = DIRECTION ( 'NONE',  ( 1.000000000000000000, 0.000000000000000000, 0.000000000000000000 ) ) ;
#55855 = DIRECTION ( 'NONE',  ( 0.000000000000000000, 0.000000000000000000, -1.000000000000000000 ) ) ;
#55857 = ORIENTED_EDGE ( 'NONE', *, *, #76512, .F. ) ;
#55856 = DIRECTION ( 'NONE',  ( -1.000000000000000000, 0.000000000000000000, 0.000000000000000000 ) ) ;
#55858 = AXIS2_PLACEMENT_3D ( 'NONE', #226267, #208039, #9813 ) ;
#55859 = CIRCLE ( 'NONE', #197528, 0.09999999999998898659 ) ;
#55860 = DIRECTION ( 'NONE',  ( -0.7071067811865462405, -0.2890913453342134898, 0.6453109281988460566 ) ) ;
#55861 = VECTOR ( 'NONE', #143385, 1000.000000000000000 ) ;
#55862 = VERTEX_POINT ( 'NONE', #215480 ) ;
#55863 = CARTESIAN_POINT ( 'NONE',  ( -16.92778301347268766, 10.00094491684630604, -180.0714818920313860 ) ) ;
#55864 = CARTESIAN_POINT ( 'NONE',  ( 18.46947024752519084, -9.509297157144997570, -73.98668944869785946 ) ) ;
#55865 = VECTOR ( 'NONE', #10969, 1000.000000000000114 ) ;
#55866 = CARTESIAN_POINT ( 'NONE',  ( 23.04999999999999716, 67.17743825834568838, -127.2731074845243597 ) ) ;
#55867 = ORIENTED_EDGE ( 'NONE', *, *, #4485, .T. ) ;
#55868 = LINE ( 'NONE', #135424, #221722 ) ;
#55869 = EDGE_LOOP ( 'NONE', ( #203478, #242335 ) ) ;
#55870 = DIRECTION ( 'NONE',  ( 0.000000000000000000, -0.6410630849193120762, 0.7674881895858300940 ) ) ;
#55871 = AXIS2_PLACEMENT_3D ( 'NONE', #232954, #73890, #193808 ) ;
#55872 = DIRECTION ( 'NONE',  ( 0.000000000000000000, 0.000000000000000000, -1.000000000000000000 ) ) ;
#55873 = DIRECTION ( 'NONE',  ( -1.000000000000000000, -0.000000000000000000, 0.000000000000000000 ) ) ;
#55874 = ORIENTED_EDGE ( 'NONE', *, *, #256033, .T. ) ;
#55875 = CARTESIAN_POINT ( 'NONE',  ( 21.14261333020286671, 22.98702397223716076, -230.0712318222100805 ) ) ;
#55876 = AXIS2_PLACEMENT_3D ( 'NONE', #238688, #241278, #199595 ) ;
#55877 = TOROIDAL_SURFACE ( 'NONE', #1726, 0.2000000000000000111, 0.1000000000000000056 ) ;
#55879 = CIRCLE ( 'NONE', #1728, 0.1000000000000028644 ) ;
#55878 = CARTESIAN_POINT ( 'NONE',  ( 21.05000000000000071, 70.47363787294415260, -228.3418745167492432 ) ) ;
#55880 = ADVANCED_FACE ( 'NONE', ( #77246 ), #7563, .T. ) ;
#55881 = ORIENTED_EDGE ( 'NONE', *, *, #75902, .T. ) ;
#55882 = LINE ( 'NONE', #232003, #255555 ) ;
#55884 = ADVANCED_FACE ( 'NONE', ( #95534 ), #216762, .T. ) ;
#55883 = DIRECTION ( 'NONE',  ( -1.000000000000000000, -0.000000000000000000, 0.000000000000000000 ) ) ;
#55885 = DIRECTION ( 'NONE',  ( 1.000000000000000000, 0.000000000000000000, 0.000000000000000000 ) ) ;
#55886 = EDGE_LOOP ( 'NONE', ( #39556, #51141, #217938, #215062 ) ) ;
#55887 = ORIENTED_EDGE ( 'NONE', *, *, #85209, .F. ) ;
#55888 = EDGE_CURVE ( 'NONE', #16173, #188424, #17301, .T. ) ;
#55889 = LINE ( 'NONE', #114611, #133321 ) ;
#55890 = VERTEX_POINT ( 'NONE', #94246 ) ;
#55893 = EDGE_CURVE ( 'NONE', #22349, #23444, #251786, .T. ) ;
#55892 = ORIENTED_EDGE ( 'NONE', *, *, #253272, .F. ) ;
#55891 = CARTESIAN_POINT ( 'NONE',  ( 18.49999999999999645, 5.950000000011100632, -144.3057023050348846 ) ) ;
#55896 = ORIENTED_EDGE ( 'NONE', *, *, #185421, .F. ) ;
#55895 = ORIENTED_EDGE ( 'NONE', *, *, #229306, .F. ) ;
#55894 = LINE ( 'NONE', #214992, #22157 ) ;
#55897 = CIRCLE ( 'NONE', #160009, 0.09999999999999939493 ) ;
#55898 = AXIS2_PLACEMENT_3D ( 'NONE', #71916, #174913, #254364 ) ;
#55899 = CARTESIAN_POINT ( 'NONE',  ( 20.94999999999999929, 85.40000000001207070, -126.6291383618717816 ) ) ;
#55900 = CARTESIAN_POINT ( 'NONE',  ( -16.84793658983426567, 12.43183352348533610, -211.3246197489285976 ) ) ;
#55901 = CARTESIAN_POINT ( 'NONE',  ( 21.05000000000000071, 10.72371710471867701, -112.6500000000000341 ) ) ;
#55902 = CIRCLE ( 'NONE', #126674, 0.1000000000000079159 ) ;
#55903 = CARTESIAN_POINT ( 'NONE',  ( -21.14999999999999858, 4.184122562697131897, -245.3714803909117279 ) ) ;
#55904 = DIRECTION ( 'NONE',  ( 1.000000000000000000, 0.000000000000000000, 1.073024830501117725E-15 ) ) ;
#55905 = CARTESIAN_POINT ( 'NONE',  ( 23.14999999999999858, 9.180734019381761257, -233.2858192224647382 ) ) ;
#55907 = EDGE_CURVE ( 'NONE', #157934, #253084, #164316, .T. ) ;
#55906 = ORIENTED_EDGE ( 'NONE', *, *, #154252, .T. ) ;
#55908 = ORIENTED_EDGE ( 'NONE', *, *, #257450, .F. ) ;
#55910 = ORIENTED_EDGE ( 'NONE', *, *, #241963, .F. ) ;
#55909 = CIRCLE ( 'NONE', #235015, 0.5999999999999894307 ) ;
#55911 = CARTESIAN_POINT ( 'NONE',  ( 21.00000000000000000, 66.25000000001186606, -90.67310748452437963 ) ) ;
#55912 = VECTOR ( 'NONE', #183337, 1000.000000000000000 ) ;
#55914 = ORIENTED_EDGE ( 'NONE', *, *, #79742, .F. ) ;
#55913 = DIRECTION ( 'NONE',  ( -1.000000000000000000, 0.000000000000000000, 0.000000000000000000 ) ) ;
#55915 = CARTESIAN_POINT ( 'NONE',  ( -17.22361732159831860, 60.22314076454453868, -222.1729100509217858 ) ) ;
#55916 = ORIENTED_EDGE ( 'NONE', *, *, #202249, .F. ) ;
#55917 = CARTESIAN_POINT ( 'NONE',  ( -20.64999999999999858, 2.500000000011154633, -154.2753780772379173 ) ) ;
#55918 = ORIENTED_EDGE ( 'NONE', *, *, #178344, .T. ) ;
#55919 = DIRECTION ( 'NONE',  ( 0.7071067811865474617, -0.6824534298470372740, 0.1850873201762209819 ) ) ;
#55920 = CIRCLE ( 'NONE', #93348, 0.1000000000000028644 ) ;
#55921 = CIRCLE ( 'NONE', #80880, 3.899999999999987033 ) ;
#55922 = ADVANCED_FACE ( 'NONE', ( #158129 ), #198486, .T. ) ;
#55923 = ORIENTED_EDGE ( 'NONE', *, *, #253119, .T. ) ;
#55924 = AXIS2_PLACEMENT_3D ( 'NONE', #17509, #59172, #94475 ) ;
#55925 = CYLINDRICAL_SURFACE ( 'NONE', #89547, 0.09999999999999108213 ) ;
#55926 = DIRECTION ( 'NONE',  ( 1.000000000000000000, 0.000000000000000000, 0.000000000000000000 ) ) ;
#55927 = EDGE_CURVE ( 'NONE', #133309, #139578, #240816, .T. ) ;
#55928 = CIRCLE ( 'NONE', #14289, 0.09999999999999543976 ) ;
#55930 = ORIENTED_EDGE ( 'NONE', *, *, #50601, .T. ) ;
#55929 = ORIENTED_EDGE ( 'NONE', *, *, #132784, .F. ) ;
#55931 = ORIENTED_EDGE ( 'NONE', *, *, #192513, .T. ) ;
#55932 = FACE_OUTER_BOUND ( 'NONE', #91239, .T. ) ;
#55933 = ORIENTED_EDGE ( 'NONE', *, *, #130596, .F. ) ;
#55934 = ORIENTED_EDGE ( 'NONE', *, *, #99174, .T. ) ;
#55935 = FACE_OUTER_BOUND ( 'NONE', #148903, .T. ) ;
#55937 = EDGE_LOOP ( 'NONE', ( #134462, #183548, #48923, #168804 ) ) ;
#55936 = LINE ( 'NONE', #95088, #26966 ) ;
#55938 = CIRCLE ( 'NONE', #201706, 0.1999999999999987899 ) ;
#55940 = CARTESIAN_POINT ( 'NONE',  ( 22.50000000000000000, 68.25000000001213607, -136.6231074845243540 ) ) ;
#55939 = DIRECTION ( 'NONE',  ( -1.000000000000000000, -0.000000000000000000, -0.000000000000000000 ) ) ;
#55941 = EDGE_CURVE ( 'NONE', #174912, #68363, #35349, .T. ) ;
#55942 = LINE ( 'NONE', #37716, #78304 ) ;
#55943 = FACE_OUTER_BOUND ( 'NONE', #156474, .T. ) ;
#55944 = CARTESIAN_POINT ( 'NONE',  ( -17.11825945287481332, 10.05000000001113847, -121.3500000000000369 ) ) ;
#55945 = EDGE_LOOP ( 'NONE', ( #192290, #38384, #79670, #56856 ) ) ;
#55946 = ADVANCED_FACE ( 'NONE', ( #104494 ), #97629, .F. ) ;
#55947 = ORIENTED_EDGE ( 'NONE', *, *, #72850, .T. ) ;
#55948 = CARTESIAN_POINT ( 'NONE',  ( 18.50000000000000355, 85.40000000001185754, -96.14106563635154146 ) ) ;
#55949 = AXIS2_PLACEMENT_3D ( 'NONE', #122021, #182003, #84115 ) ;
#55950 = CARTESIAN_POINT ( 'NONE',  ( -20.64999999999999858, 71.65000000001155911, -57.17310748452435121 ) ) ;
#55951 = CARTESIAN_POINT ( 'NONE',  ( 21.05000000000000071, 1.115600667400684642E-11, -134.0000000000000284 ) ) ;
#55953 = EDGE_CURVE ( 'NONE', #47050, #50777, #101928, .T. ) ;
#55952 = ORIENTED_EDGE ( 'NONE', *, *, #192029, .T. ) ;
#55954 = CARTESIAN_POINT ( 'NONE',  ( -15.75000000000000355, 9.850000000011133849, -184.2499999999999716 ) ) ;
#55955 = AXIS2_PLACEMENT_3D ( 'NONE', #130036, #186187, #187483 ) ;
#55956 = AXIS2_PLACEMENT_3D ( 'NONE', #235856, #80616, #157660 ) ;
#55957 = DIRECTION ( 'NONE',  ( 1.000000000000000000, 0.000000000000000000, 0.000000000000000000 ) ) ;
#55958 = VECTOR ( 'NONE', #181536, 1000.000000000000000 ) ;
#55959 = CARTESIAN_POINT ( 'NONE',  ( 18.59999999999999787, -8.250000000000005329, 32.89999999999999858 ) ) ;
#55960 = ORIENTED_EDGE ( 'NONE', *, *, #47273, .T. ) ;
#55961 = ORIENTED_EDGE ( 'NONE', *, *, #218509, .T. ) ;
#55962 = CARTESIAN_POINT ( 'NONE',  ( 18.54999999999999716, 8.750000000011173285, -180.1499999999999773 ) ) ;
#55963 = ORIENTED_EDGE ( 'NONE', *, *, #27548, .F. ) ;
#55964 = LINE ( 'NONE', #54702, #234646 ) ;
#55965 = ORIENTED_EDGE ( 'NONE', *, *, #198069, .F. ) ;
#55966 = EDGE_CURVE ( 'NONE', #141897, #588, #89451, .T. ) ;
#55967 = DIRECTION ( 'NONE',  ( 1.000000000000000000, 0.000000000000000000, 0.000000000000000000 ) ) ;
#55968 = CARTESIAN_POINT ( 'NONE',  ( -23.15000000000000213, 33.13294339707397285, -247.6623911921324463 ) ) ;
#55970 = CARTESIAN_POINT ( 'NONE',  ( -21.05000000000000071, -1.362227297915485025, -194.8443758818181664 ) ) ;
#55969 = DIRECTION ( 'NONE',  ( 0.000000000000000000, 0.000000000000000000, 1.000000000000000000 ) ) ;
#55971 = LINE ( 'NONE', #35194, #148981 ) ;
#55973 = ADVANCED_FACE ( 'NONE', ( #43274 ), #85968, .T. ) ;
#55972 = LINE ( 'NONE', #177262, #157912 ) ;
#55974 = CARTESIAN_POINT ( 'NONE',  ( 0.8999999999999993561, -8.250000000000005329, 26.00000000000000355 ) ) ;
#55975 = VECTOR ( 'NONE', #248072, 1000.000000000000000 ) ;
#55977 = ORIENTED_EDGE ( 'NONE', *, *, #151863, .F. ) ;
#55976 = ORIENTED_EDGE ( 'NONE', *, *, #133206, .F. ) ;
#55978 = VERTEX_POINT ( 'NONE', #6705 ) ;
#55979 = DIRECTION ( 'NONE',  ( 6.938893903907270030E-14, -0.000000000000000000, 1.000000000000000000 ) ) ;
#55980 = CARTESIAN_POINT ( 'NONE',  ( 22.49999999999999645, 0.08880997638693272078, 11.64976291803192154 ) ) ;
#55981 = AXIS2_PLACEMENT_3D ( 'NONE', #210356, #151690, #111248 ) ;
#55982 = CARTESIAN_POINT ( 'NONE',  ( -20.94999999999999929, 0.000000000000000000, -33.50000000000000000 ) ) ;
#55983 = LINE ( 'NONE', #118572, #225810 ) ;
#55985 = CARTESIAN_POINT ( 'NONE',  ( -13.77178122865954180, 66.54397173950395938, -88.01190944945868466 ) ) ;
#55984 = DIRECTION ( 'NONE',  ( 0.000000000000000000, 6.982962677686266711E-15, -1.000000000000000000 ) ) ;
#55986 = DIRECTION ( 'NONE',  ( 0.000000000000000000, -1.000000000000000000, 0.000000000000000000 ) ) ;
#55987 = ORIENTED_EDGE ( 'NONE', *, *, #193493, .F. ) ;
#55988 = DIRECTION ( 'NONE',  ( 0.000000000000000000, -1.000000000000000000, 0.000000000000000000 ) ) ;
#55989 = ORIENTED_EDGE ( 'NONE', *, *, #138085, .T. ) ;
#55990 = ORIENTED_EDGE ( 'NONE', *, *, #62928, .T. ) ;
#55991 = CARTESIAN_POINT ( 'NONE',  ( -21.04999999999999716, 69.65527659592140708, -69.53782534104793456 ) ) ;
#55992 = DIRECTION ( 'NONE',  ( 0.000000000000000000, -0.9209589331071360574, 0.3896596508880098009 ) ) ;
#55993 = CARTESIAN_POINT ( 'NONE',  ( 20.94999999999999574, 8.926614585098251453, -175.9716830192230930 ) ) ;
#55994 = DIRECTION ( 'NONE',  ( -1.000000000000000000, 0.000000000000000000, 0.000000000000000000 ) ) ;
#55995 = AXIS2_PLACEMENT_3D ( 'NONE', #246985, #125750, #85321 ) ;
#55996 = DIRECTION ( 'NONE',  ( 0.000000000000000000, -0.9126074666063660468, -0.4088369013363524762 ) ) ;
#55997 = VERTEX_POINT ( 'NONE', #26282 ) ;
#55998 = ORIENTED_EDGE ( 'NONE', *, *, #93152, .F. ) ;
#55999 = DIRECTION ( 'NONE',  ( 1.733608814749328402E-15, 0.9910827722268042983, 0.1332476588733650935 ) ) ;
#56000 = DIRECTION ( 'NONE',  ( 1.000000000000000000, 0.000000000000000000, 0.000000000000000000 ) ) ;
#56001 = CARTESIAN_POINT ( 'NONE',  ( 23.14999999999999503, 8.882751598337874199, -187.0399955572217721 ) ) ;
#56002 = CARTESIAN_POINT ( 'NONE',  ( 21.05000000000000071, 8.826429739528350638, -175.9140547129436527 ) ) ;
#56003 = DIRECTION ( 'NONE',  ( 0.000000000000000000, 0.000000000000000000, -1.000000000000000000 ) ) ;
#56004 = CARTESIAN_POINT ( 'NONE',  ( 20.94999999999999929, -9.000000000000001776, -9.893969122652443104 ) ) ;
#56005 = DIRECTION ( 'NONE',  ( -0.000000000000000000, 0.2128009952263603677, -0.9770955615653313941 ) ) ;
#56007 = LINE ( 'NONE', #176015, #257917 ) ;
#56006 = LINE ( 'NONE', #216388, #166049 ) ;
#56008 = DIRECTION ( 'NONE',  ( 0.7071359030028113724, 0.000000000000000000, -0.7070776581708677622 ) ) ;
#56009 = DIRECTION ( 'NONE',  ( -1.000000000000000000, 0.000000000000000000, -0.000000000000000000 ) ) ;
#56010 = DIRECTION ( 'NONE',  ( 1.000000000000000000, -0.000000000000000000, -0.000000000000000000 ) ) ;
#56011 = DIRECTION ( 'NONE',  ( 0.000000000000000000, 0.008583690987127922528, 0.9999631594459055250 ) ) ;
#56012 = AXIS2_PLACEMENT_3D ( 'NONE', #42757, #23223, #225216 ) ;
#56014 = ORIENTED_EDGE ( 'NONE', *, *, #154436, .F. ) ;
#56013 = CARTESIAN_POINT ( 'NONE',  ( -20.64999999999999858, -9.399999999988846611, -57.10603087734755690 ) ) ;
#56015 = AXIS2_PLACEMENT_3D ( 'NONE', #237375, #54860, #14500 ) ;
#56016 = VECTOR ( 'NONE', #98963, 1000.000000000000000 ) ;
#56017 = CIRCLE ( 'NONE', #73015, 0.09999999999999939493 ) ;
#56018 = DIRECTION ( 'NONE',  ( -1.000000000000000000, -0.000000000000000000, 0.000000000000000000 ) ) ;
#56019 = EDGE_CURVE ( 'NONE', #160550, #92616, #106003, .T. ) ;
#56020 = EDGE_LOOP ( 'NONE', ( #102142, #163067, #152554, #180797 ) ) ;
#56021 = DIRECTION ( 'NONE',  ( -1.836970198721029934E-16, 1.000000000000000000, 0.000000000000000000 ) ) ;
#56022 = ADVANCED_FACE ( 'NONE', ( #240198 ), #141093, .F. ) ;
#56023 = EDGE_CURVE ( 'NONE', #228463, #35453, #201896, .T. ) ;
#56024 = ORIENTED_EDGE ( 'NONE', *, *, #66943, .F. ) ;
#56026 = CYLINDRICAL_SURFACE ( 'NONE', #238100, 0.09999999999999892308 ) ;
#56025 = CIRCLE ( 'NONE', #214281, 0.1999999999999987899 ) ;
#56027 = CARTESIAN_POINT ( 'NONE',  ( 14.45963434102924161, 9.451541661396667848, -85.45387549883061240 ) ) ;
#56028 = CARTESIAN_POINT ( 'NONE',  ( 22.50000000000000000, 59.68594599439719417, -233.9123800762197902 ) ) ;
#56029 = B_SPLINE_CURVE_WITH_KNOTS ( 'NONE', 3,
 ( #37487, #171887, #212276, #16640, #135268, #113157, #14074, #115726, #192702, #177014, #213528, #133996, #174469, #117009, #253934, #93594, #255171, #54461, #34940 ),
 .UNSPECIFIED., .F., .F.,
 ( 4, 3, 3, 3, 3, 3, 4 ),
 ( 0.0001624081864585828479, 0.0001685232196531679001, 0.0001764526673566893435, 0.0001916878551483146103, 0.0002009890782182573881, 0.0002238845907555200366, 0.0002283406619926361904 ),
 .UNSPECIFIED. ) ;
#56030 = AXIS2_PLACEMENT_3D ( 'NONE', #84471, #165349, #46660 ) ;
#56031 = LINE ( 'NONE', #92602, #51466 ) ;
#56032 = CIRCLE ( 'NONE', #43407, 0.09999999999999939493 ) ;
#56033 = CARTESIAN_POINT ( 'NONE',  ( 18.60000000000000497, 85.52394631232935751, -62.64107948918602631 ) ) ;
#56034 = DIRECTION ( 'NONE',  ( 0.000000000000000000, -1.000000000000000000, 0.000000000000000000 ) ) ;
#56035 = CIRCLE ( 'NONE', #185246, 4.000000000000003553 ) ;
#56036 = AXIS2_PLACEMENT_3D ( 'NONE', #8974, #127645, #125085 ) ;
#56037 = ORIENTED_EDGE ( 'NONE', *, *, #135238, .T. ) ;
#56038 = CARTESIAN_POINT ( 'NONE',  ( -21.52071067811865746, 68.22071067813087097, -148.7731074845244166 ) ) ;
#56040 = EDGE_LOOP ( 'NONE', ( #35, #152823, #137921, #208344 ) ) ;
#56039 = CARTESIAN_POINT ( 'NONE',  ( -18.59999999999999787, 66.85000000001173248, -81.27310748452438816 ) ) ;
#56041 = CARTESIAN_POINT ( 'NONE',  ( -20.12071067811865888, 66.67928932189320790, -90.67310748452437963 ) ) ;
#56042 = EDGE_CURVE ( 'NONE', #210729, #133901, #202341, .T. ) ;
#56043 = DIRECTION ( 'NONE',  ( 0.000000000000000000, 0.000000000000000000, 1.000000000000000000 ) ) ;
#56044 = CARTESIAN_POINT ( 'NONE',  ( 5.900000000000061640, 64.65000000001120384, -22.12310748452479103 ) ) ;
#56045 = VERTEX_POINT ( 'NONE', #90080 ) ;
#56046 = CARTESIAN_POINT ( 'NONE',  ( 23.14999999999998437, 1.115600667400684642E-11, -67.00000000000004263 ) ) ;
#56047 = CIRCLE ( 'NONE', #210393, 0.09999999999999939493 ) ;
#56048 = TOROIDAL_SURFACE ( 'NONE', #80998, 0.6000000000000013101, 0.1000000000000000056 ) ;
#56049 = APPLICATION_PROTOCOL_DEFINITION ( 'draft international standard', 'automotive_design', 1998, #83934 ) ;
#56050 = CIRCLE ( 'NONE', #126991, 0.1000000000000124678 ) ;
#56052 = AXIS2_PLACEMENT_3D ( 'NONE', #21532, #118046, #215841 ) ;
#56051 = CARTESIAN_POINT ( 'NONE',  ( -19.89999999999999858, 1.350000000000000089, 16.60000000000000142 ) ) ;
#56053 = CYLINDRICAL_SURFACE ( 'NONE', #71496, 0.09999999999999939493 ) ;
#56054 = ORIENTED_EDGE ( 'NONE', *, *, #75390, .T. ) ;
#56055 = DIRECTION ( 'NONE',  ( 0.000000000000000000, 0.000000000000000000, -1.000000000000000000 ) ) ;
#56056 = LINE ( 'NONE', #256790, #192318 ) ;
#56057 = CIRCLE ( 'NONE', #164246, 12.87499999999999822 ) ;
#56058 = CIRCLE ( 'NONE', #89210, 0.1000000000000089567 ) ;
#56059 = DIRECTION ( 'NONE',  ( 1.000000000000000000, 0.000000000000000000, 0.000000000000000000 ) ) ;
#56060 = EDGE_CURVE ( 'NONE', #77748, #160821, #166013, .T. ) ;
#56061 = ORIENTED_EDGE ( 'NONE', *, *, #258026, .T. ) ;
#56062 = ADVANCED_FACE ( 'NONE', ( #246593 ), #147504, .F. ) ;
#56063 = ORIENTED_EDGE ( 'NONE', *, *, #174825, .T. ) ;
#56064 = VECTOR ( 'NONE', #253760, 1000.000000000000000 ) ;
#56065 = DIRECTION ( 'NONE',  ( 0.000000000000000000, 0.000000000000000000, 1.000000000000000000 ) ) ;
#56066 = VECTOR ( 'NONE', #213955, 1000.000000000000227 ) ;
#56067 = DIRECTION ( 'NONE',  ( 0.000000000000000000, 0.000000000000000000, -1.000000000000000000 ) ) ;
#56068 = FACE_OUTER_BOUND ( 'NONE', #121963, .T. ) ;
#56069 = DIRECTION ( 'NONE',  ( 0.7071067811865388020, -0.7071067811865561215, 0.000000000000000000 ) ) ;
#56070 = EDGE_CURVE ( 'NONE', #226085, #18582, #118531, .T. ) ;
#56072 = FACE_OUTER_BOUND ( 'NONE', #179011, .T. ) ;
#56071 = DIRECTION ( 'NONE',  ( -0.000000000000000000, 1.000000000000000000, -0.000000000000000000 ) ) ;
#56073 = CARTESIAN_POINT ( 'NONE',  ( 18.39999999999999503, 11.74999999999998224, -12.65000000000000213 ) ) ;
#56074 = CARTESIAN_POINT ( 'NONE',  ( -16.92132318717937522, 9.966070024017081863, -113.1224066303521028 ) ) ;
#56075 = CARTESIAN_POINT ( 'NONE',  ( -16.27683809663750480, 41.27791846035906786, -237.2365415511148115 ) ) ;
#56076 = DIRECTION ( 'NONE',  ( 0.000000000000000000, -6.467318590049456648E-15, 1.000000000000000000 ) ) ;
#56077 = ORIENTED_EDGE ( 'NONE', *, *, #184297, .F. ) ;
#56078 = ORIENTED_EDGE ( 'NONE', *, *, #79457, .F. ) ;
#56079 = CARTESIAN_POINT ( 'NONE',  ( -18.59999999999999787, 97.49741144064424248, -225.2667035127916790 ) ) ;
#56080 = CARTESIAN_POINT ( 'NONE',  ( -17.80356949364090013, 65.12326860300883880, -146.8100344602939060 ) ) ;
#56082 = DIRECTION ( 'NONE',  ( 0.000000000000000000, 0.000000000000000000, -1.000000000000000000 ) ) ;
#56081 = DIRECTION ( 'NONE',  ( -2.978066053179069723E-16, -1.000000000000000000, -7.147358527629766941E-15 ) ) ;
#56083 = CARTESIAN_POINT ( 'NONE',  ( -23.25000000000000000, 77.83585931145498193, -24.51866831572578675 ) ) ;
#56084 = FACE_OUTER_BOUND ( 'NONE', #199415, .T. ) ;
#56085 = CARTESIAN_POINT ( 'NONE',  ( 15.69410316191959609, 12.80332707393613845, -215.8182015632437754 ) ) ;
#56086 = ORIENTED_EDGE ( 'NONE', *, *, #211051, .T. ) ;
#56087 = EDGE_LOOP ( 'NONE', ( #234654, #230800, #45815, #240328 ) ) ;
#56088 = EDGE_CURVE ( 'NONE', #256392, #187202, #43681, .T. ) ;
#56089 = AXIS2_PLACEMENT_3D ( 'NONE', #54546, #254021, #257828 ) ;
#56090 = B_SPLINE_CURVE_WITH_KNOTS ( 'NONE', 3,
 ( #232060, #156389, #113380, #54679, #213758, #35166, #114660, #194227, #15590, #95096 ),
 .UNSPECIFIED., .F., .F.,
 ( 4, 2, 2, 2, 4 ),
 ( 0.000000000000000000, 0.0001584437871625023631, 0.0002376656807437556318, 0.0002772766275343830386, 0.0003168875743250104725 ),
 .UNSPECIFIED. ) ;
#56091 = AXIS2_PLACEMENT_3D ( 'NONE', #14215, #190273, #250233 ) ;
#56092 = CARTESIAN_POINT ( 'NONE',  ( 23.14999999999999503, 11.65000000000000746, -12.25000000000000000 ) ) ;
#56093 = ORIENTED_EDGE ( 'NONE', *, *, #121777, .F. ) ;
#56094 = DIRECTION ( 'NONE',  ( 0.000000000000000000, -0.9126074666063622720, -0.4088369013363611360 ) ) ;
#56095 = AXIS2_PLACEMENT_3D ( 'NONE', #144028, #223560, #124493 ) ;
#56096 = CARTESIAN_POINT ( 'NONE',  ( -18.40000000000000213, 64.52683809664931402, -82.07310748452439952 ) ) ;
#56097 = CARTESIAN_POINT ( 'NONE',  ( -21.14999999999999858, 65.51923798433686841, -242.1677427744926092 ) ) ;
#56098 = CIRCLE ( 'NONE', #160203, 0.09999999999999520384 ) ;
#56099 = ADVANCED_FACE ( 'NONE', ( #211334 ), #227033, .T. ) ;
#56100 = CIRCLE ( 'NONE', #76965, 0.2000000000000111688 ) ;
#56101 = EDGE_CURVE ( 'NONE', #77358, #169886, #110307, .T. ) ;
#56102 = EDGE_LOOP ( 'NONE', ( #102742, #22442, #178948, #33012 ) ) ;
#56103 = DIRECTION ( 'NONE',  ( -1.000000000000000000, 0.000000000000000000, 0.000000000000000000 ) ) ;
#56104 = VERTEX_POINT ( 'NONE', #229615 ) ;
#56105 = EDGE_CURVE ( 'NONE', #253318, #14640, #210113, .T. ) ;
#56107 = ADVANCED_FACE ( 'NONE', ( #88787 ), #148799, .T. ) ;
#56106 = DIRECTION ( 'NONE',  ( 0.000000000000000000, -0.9893560106964500722, 0.1455152366551550613 ) ) ;
#56109 = CIRCLE ( 'NONE', #226826, 0.09999999999999939493 ) ;
#56108 = SPHERICAL_SURFACE ( 'NONE', #244961, 0.1000000000000000056 ) ;
#56110 = DIRECTION ( 'NONE',  ( 0.000000000000000000, -0.7092521942343286145, -0.7049548389604757270 ) ) ;
#56111 = DIRECTION ( 'NONE',  ( 0.000000000000000000, 0.4088369013363281623, -0.9126074666063771490 ) ) ;
#56113 = CIRCLE ( 'NONE', #76976, 0.09999999999998898659 ) ;
#56112 = CARTESIAN_POINT ( 'NONE',  ( -16.81744102076749314, 9.949999999999986855, -12.65000000000000213 ) ) ;
#56115 = CARTESIAN_POINT ( 'NONE',  ( 15.74999999999999645, 66.15000000001258229, -186.7731074845244450 ) ) ;
#56114 = DIRECTION ( 'NONE',  ( -0.000000000000000000, 0.1350103645451626311, 0.9908441862701635738 ) ) ;
#56116 = CIRCLE ( 'NONE', #64516, 0.09999999999999939493 ) ;
#56117 = CARTESIAN_POINT ( 'NONE',  ( -16.87683809663752399, 66.13411015067987364, -149.7905342915939855 ) ) ;
#56118 = VERTEX_POINT ( 'NONE', #50942 ) ;
#56120 = CARTESIAN_POINT ( 'NONE',  ( -23.25000000000000000, 42.20719072976272912, -239.1935934412594804 ) ) ;
#56119 = DIRECTION ( 'NONE',  ( 0.000000000000000000, -1.000000000000000000, 0.000000000000000000 ) ) ;
#56121 = EDGE_LOOP ( 'NONE', ( #68398, #188371, #205919, #235179 ) ) ;
#56123 = ORIENTED_EDGE ( 'NONE', *, *, #24060, .F. ) ;
#56122 = CARTESIAN_POINT ( 'NONE',  ( 23.15000000000000213, -4.756823075239758225, -233.1486023682345490 ) ) ;
#56124 = TOROIDAL_SURFACE ( 'NONE', #81246, 0.2000000000000000111, 0.1000000000000000056 ) ;
#56125 = ADVANCED_FACE ( 'NONE', ( #189206 ), #11872, .T. ) ;
#56126 = VERTEX_POINT ( 'NONE', #91389 ) ;
#56127 = DIRECTION ( 'NONE',  ( 0.000000000000000000, 0.9126074666063545004, 0.4088369013363783999 ) ) ;
#56128 = EDGE_CURVE ( 'NONE', #69570, #147074, #70568, .T. ) ;
#56129 = DIRECTION ( 'NONE',  ( 0.000000000000000000, -0.9595780032479205301, 0.2814428106787130734 ) ) ;
#56130 = DIRECTION ( 'NONE',  ( -0.000000000000000000, 1.000000000000000000, 6.982962677686267499E-15 ) ) ;
#56131 = DIRECTION ( 'NONE',  ( -1.000000000000000000, 0.000000000000000000, 0.000000000000000000 ) ) ;
#56132 = ORIENTED_EDGE ( 'NONE', *, *, #139542, .T. ) ;
#56133 = LINE ( 'NONE', #139528, #192262 ) ;
#56135 = EDGE_CURVE ( 'NONE', #231683, #214079, #31069, .T. ) ;
#56134 = DIRECTION ( 'NONE',  ( 1.000000000000000000, 0.000000000000000000, 0.000000000000000000 ) ) ;
#56136 = ORIENTED_EDGE ( 'NONE', *, *, #149542, .F. ) ;
#56137 = CARTESIAN_POINT ( 'NONE',  ( 22.48660254037844197, 12.58580559757026940, -223.4396719342083486 ) ) ;
#56138 = ADVANCED_FACE ( 'NONE', ( #215179 ), #176084, .F. ) ;
#56139 = PLANE ( 'NONE',  #143198 ) ;
#56140 = ORIENTED_EDGE ( 'NONE', *, *, #228080, .T. ) ;
#56141 = ORIENTED_EDGE ( 'NONE', *, *, #181821, .F. ) ;
#56142 = CARTESIAN_POINT ( 'NONE',  ( 18.49999999999999645, -3.391987963166880338, -191.5331142350599691 ) ) ;
#56143 = EDGE_CURVE ( 'NONE', #13712, #87244, #81251, .T. ) ;
#56144 = ADVANCED_FACE ( 'NONE', ( #113512 ), #14441, .T. ) ;
#56145 = CIRCLE ( 'NONE', #230977, 0.1000000000000052097 ) ;
#56146 = ORIENTED_EDGE ( 'NONE', *, *, #70681, .T. ) ;
#56147 = VECTOR ( 'NONE', #34036, 1000.000000000000000 ) ;
#56148 = CARTESIAN_POINT ( 'NONE',  ( -19.99999999999999645, 5.454087299794355914, 16.60000000000000142 ) ) ;
#56149 = ORIENTED_EDGE ( 'NONE', *, *, #243074, .T. ) ;
#56150 = CARTESIAN_POINT ( 'NONE',  ( -21.55000000000000426, 12.05403912736948158, -220.1228874760914209 ) ) ;
#56151 = EDGE_CURVE ( 'NONE', #133700, #214401, #134338, .T. ) ;
#56152 = CARTESIAN_POINT ( 'NONE',  ( 21.05000000000000071, 5.000000000011153745, -88.09473398108696074 ) ) ;
#56153 = DIRECTION ( 'NONE',  ( 0.000000000000000000, -3.122502256758250246E-14, -1.000000000000000000 ) ) ;
#56154 = CARTESIAN_POINT ( 'NONE',  ( -16.86733706339143524, 63.08420242447057547, -213.0721725863693905 ) ) ;
#56155 = EDGE_CURVE ( 'NONE', #20030, #158859, #139530, .T. ) ;
#56156 = EDGE_CURVE ( 'NONE', #161481, #121706, #47940, .T. ) ;
#56157 = FACE_OUTER_BOUND ( 'NONE', #146706, .T. ) ;
#56158 = CARTESIAN_POINT ( 'NONE',  ( 18.48197441911643324, -9.517954794694091447, -73.89021164220768867 ) ) ;
#56159 = CARTESIAN_POINT ( 'NONE',  ( -23.15000000000000213, 54.80101577392981937, -239.2322065708440846 ) ) ;
#56160 = B_SPLINE_CURVE_WITH_KNOTS ( 'NONE', 3,
 ( #79785, #178952, #116383, #53832, #195928, #156816 ),
 .UNSPECIFIED., .F., .F.,
 ( 4, 2, 4 ),
 ( 0.000000000000000000, 0.0001496588209255844779, 0.0002993176418511689558 ),
 .UNSPECIFIED. ) ;
#56161 = EDGE_LOOP ( 'NONE', ( #133500, #243173, #1242, #130868, #77776 ) ) ;
#56162 = AXIS2_PLACEMENT_3D ( 'NONE', #208665, #146092, #27487 ) ;
#56164 = DIRECTION ( 'NONE',  ( 0.000000000000000000, 0.000000000000000000, -1.000000000000000000 ) ) ;
#56163 = CARTESIAN_POINT ( 'NONE',  ( 20.97468175916186439, 22.94852194069405371, -230.1531915370501906 ) ) ;
#56165 = ORIENTED_EDGE ( 'NONE', *, *, #209196, .T. ) ;
#56168 = ORIENTED_EDGE ( 'NONE', *, *, #38787, .T. ) ;
#56167 = DIRECTION ( 'NONE',  ( -0.000000000000000000, -1.000000000000000000, 0.000000000000000000 ) ) ;
#56166 = DIRECTION ( 'NONE',  ( 1.000000000000000000, 2.885090398161910739E-16, 6.283419270304611573E-17 ) ) ;
#56169 = VERTEX_POINT ( 'NONE', #54806 ) ;
#56170 = DIRECTION ( 'NONE',  ( 1.000000000000000000, 0.000000000000000000, 0.000000000000000000 ) ) ;
#56171 = CARTESIAN_POINT ( 'NONE',  ( 12.25000000000000000, 66.65000000001228386, -153.2731074845244166 ) ) ;
#56172 = DIRECTION ( 'NONE',  ( 0.000000000000000000, 0.000000000000000000, -1.000000000000000000 ) ) ;
#56173 = CARTESIAN_POINT ( 'NONE',  ( -16.81453046979149235, 9.939102281452070642, -113.2117265236030335 ) ) ;
#56174 = VECTOR ( 'NONE', #34011, 1000.000000000000000 ) ;
#56176 = EDGE_LOOP ( 'NONE', ( #97926, #237340, #106250, #44564 ) ) ;
#56175 =( BOUNDED_SURFACE ( )  B_SPLINE_SURFACE ( 3, 2, ( 
 ( #242897, #61698, #142500 ),
 ( #65540, #224611, #125523 ),
 ( #141235, #105930, #90223 ),
 ( #49832, #9414, #68120 ),
 ( #169829, #91536, #27745 ),
 ( #129373, #225870, #147653 ) ),
 .UNSPECIFIED., .F., .F., .F. ) 
 B_SPLINE_SURFACE_WITH_KNOTS ( ( 4, 2, 4 ),
 ( 3, 3 ),
 ( 3.141592653589783346, 3.926990816987233845, 4.712388980384684345 ),
 ( 0.000000000000000000, 1.000000000000000000 ),
 .UNSPECIFIED. ) 
 GEOMETRIC_REPRESENTATION_ITEM ( )  RATIONAL_B_SPLINE_SURFACE ( (
 ( 1.000000000000000000, 0.9238795325112774126, 1.000000000000000000),
 ( 1.000000000000000000, 0.9240297172243541191, 1.000000000000000000),
 ( 1.000000000000000000, 0.9038128468039285934, 1.000000000000000000),
 ( 1.000000000000000000, 0.8282379607649370534, 1.000000000000000000),
 ( 1.000000000000000000, 0.7727932973491273838, 1.000000000000000000),
 ( 1.000000000000000000, 0.7071067811865475727, 1.000000000000000000) ) ) 
 REPRESENTATION_ITEM ( '' )  SURFACE ( )  );
#56178 = ORIENTED_EDGE ( 'NONE', *, *, #7300, .T. ) ;
#56177 = DIRECTION ( 'NONE',  ( -1.000000000000000000, -7.304098846218134667E-16, 0.000000000000000000 ) ) ;
#56179 = EDGE_CURVE ( 'NONE', #67031, #199047, #197794, .T. ) ;
#56181 = CARTESIAN_POINT ( 'NONE',  ( 21.05000000000000071, 5.000000000011153745, -179.9052660189130677 ) ) ;
#56180 = FACE_OUTER_BOUND ( 'NONE', #77189, .T. ) ;
#56183 = VERTEX_POINT ( 'NONE', #173542 ) ;
#56182 = CYLINDRICAL_SURFACE ( 'NONE', #68384, 0.09999999999999635569 ) ;
#56184 = VERTEX_POINT ( 'NONE', #156531 ) ;
#56185 = CARTESIAN_POINT ( 'NONE',  ( 22.49544290803779489, 11.74987023786863283, -167.4346880407425147 ) ) ;
#56186 = CIRCLE ( 'NONE', #131209, 0.09999999999999939493 ) ;
#56187 = CIRCLE ( 'NONE', #185201, 0.1000000000000066946 ) ;
#56188 = DIRECTION ( 'NONE',  ( -1.000000000000000000, 0.000000000000000000, 0.000000000000000000 ) ) ;
#56189 = ORIENTED_EDGE ( 'NONE', *, *, #95679, .T. ) ;
#56190 = FACE_OUTER_BOUND ( 'NONE', #13966, .T. ) ;
#56191 = EDGE_LOOP ( 'NONE', ( #153050, #69142, #20040 ) ) ;
#56192 = CARTESIAN_POINT ( 'NONE',  ( -18.41418431465368144, -9.499999999989071853, -107.1001893912215195 ) ) ;
#56193 = LINE ( 'NONE', #17113, #101604 ) ;
#56194 = VERTEX_POINT ( 'NONE', #152673 ) ;
#56195 = CARTESIAN_POINT ( 'NONE',  ( -22.50000000000000000, 1.115600667400684642E-11, -67.00000000000004263 ) ) ;
#56196 = EDGE_CURVE ( 'NONE', #73651, #21018, #216453, .T. ) ;
#56197 = CIRCLE ( 'NONE', #89519, 0.1000000000000046685 ) ;
#56199 = EDGE_CURVE ( 'NONE', #203190, #62297, #210284, .T. ) ;
#56198 = DIRECTION ( 'NONE',  ( 0.000000000000000000, 0.000000000000000000, 1.000000000000000000 ) ) ;
#56200 = AXIS2_PLACEMENT_3D ( 'NONE', #238654, #43029, #182551 ) ;
#56201 = CIRCLE ( 'NONE', #185223, 0.1000000000000009492 ) ;
#56202 = CIRCLE ( 'NONE', #197865, 0.4000000000000114575 ) ;
#56203 = ORIENTED_EDGE ( 'NONE', *, *, #177266, .T. ) ;
#56204 = VERTEX_POINT ( 'NONE', #133083 ) ;
#56205 = CARTESIAN_POINT ( 'NONE',  ( 20.19326291203161716, 18.76649736222367437, -228.4452775901896473 ) ) ;
#56206 = VERTEX_POINT ( 'NONE', #153974 ) ;
#56207 = ADVANCED_FACE ( 'NONE', ( #95230 ), #213894, .F. ) ;
#56208 = ORIENTED_EDGE ( 'NONE', *, *, #161393, .F. ) ;
#56211 = ADVANCED_FACE ( 'NONE', ( #174820 ), #212626, .T. ) ;
#56210 = ORIENTED_EDGE ( 'NONE', *, *, #156519, .F. ) ;
#56209 = DIRECTION ( 'NONE',  ( -1.000000000000000000, -0.000000000000000000, -0.000000000000000000 ) ) ;
#56212 = ORIENTED_EDGE ( 'NONE', *, *, #42057, .F. ) ;
#56213 = CYLINDRICAL_SURFACE ( 'NONE', #118352, 0.1000000000000055844 ) ;
#56214 = VERTEX_POINT ( 'NONE', #97766 ) ;
#56217 = ORIENTED_EDGE ( 'NONE', *, *, #38088, .F. ) ;
#56216 = EDGE_LOOP ( 'NONE', ( #209271, #248660, #239222, #206755 ) ) ;
#56215 = DIRECTION ( 'NONE',  ( -4.408576920032448588E-17, 0.1350103645451876666, -0.9908441862701600211 ) ) ;
#56218 = ORIENTED_EDGE ( 'NONE', *, *, #152951, .T. ) ;
#56219 = DIRECTION ( 'NONE',  ( -0.000000000000000000, 0.4791956752371485107, 0.8777080977375185666 ) ) ;
#56220 = VECTOR ( 'NONE', #62640, 1000.000000000000000 ) ;
#56221 = DIRECTION ( 'NONE',  ( 1.000000000000000000, 0.000000000000000000, 0.000000000000000000 ) ) ;
#56222 = VECTOR ( 'NONE', #31296, 1000.000000000000000 ) ;
#56223 = DIRECTION ( 'NONE',  ( 0.7071067811865474617, -0.7071067811865474617, -4.937700262164531476E-15 ) ) ;
#56224 = AXIS2_PLACEMENT_3D ( 'NONE', #208163, #29541, #89465 ) ;
#56225 = VERTEX_POINT ( 'NONE', #172250 ) ;
#56226 = DIRECTION ( 'NONE',  ( 0.000000000000000000, 0.000000000000000000, -1.000000000000000000 ) ) ;
#56228 = EDGE_LOOP ( 'NONE', ( #238879, #66438, #154902, #53484, #108836, #151509, #77766, #154542, #2515, #129532, #170216, #99964, #173056, #90914, #107770, #134899, #96280, #73255, #217305, #90995, #24914, #123941, #73302 ) ) ;
#56227 = CARTESIAN_POINT ( 'NONE',  ( 20.94999999999999929, 64.35000000001190301, -103.0231074845243882 ) ) ;
#56229 = PLANE ( 'NONE',  #117570 ) ;
#56230 = EDGE_LOOP ( 'NONE', ( #210652, #100362, #216049, #197680 ) ) ;
#56231 =( BOUNDED_SURFACE ( )  B_SPLINE_SURFACE ( 3, 2, ( 
 ( #213508, #54435, #15341 ),
 ( #74043, #55683, #152286 ),
 ( #32346, #51850, #170596 ),
 ( #250080, #193969, #150983 ),
 ( #190112, #33648, #11481 ),
 ( #71464, #230523, #251348 ) ),
 .UNSPECIFIED., .F., .F., .F. ) 
 B_SPLINE_SURFACE_WITH_KNOTS ( ( 4, 2, 4 ),
 ( 3, 3 ),
 ( 1.570796326794897668, 2.356194490192346169, 3.141592653589794448 ),
 ( 0.000000000000000000, 1.000000000000000000 ),
 .UNSPECIFIED. ) 
 GEOMETRIC_REPRESENTATION_ITEM ( )  RATIONAL_B_SPLINE_SURFACE ( (
 ( 1.000000000000000000, 0.7071067811865597852, 1.000000000000000000),
 ( 1.000000000000000000, 0.6611148371776427446, 1.000000000000000000),
 ( 1.000000000000000000, 0.6092287576699335627, 1.000000000000000000),
 ( 1.000000000000000000, 0.5278258667054436248, 1.000000000000000000),
 ( 1.000000000000000000, 0.4993418825336356504, 1.000000000000000000),
 ( 1.000000000000000000, 0.4999999999999960587, 1.000000000000000000) ) ) 
 REPRESENTATION_ITEM ( '' )  SURFACE ( )  );
#56232 = ORIENTED_EDGE ( 'NONE', *, *, #229731, .T. ) ;
#56233 = AXIS2_PLACEMENT_3D ( 'NONE', #55142, #156881, #134697 ) ;
#56234 = CIRCLE ( 'NONE', #156238, 0.09999999999999543976 ) ;
#56235 = AXIS2_PLACEMENT_3D ( 'NONE', #85391, #244502, #125833 ) ;
#56236 = CARTESIAN_POINT ( 'NONE',  ( 21.07094088545370170, 0.09889370256337753906, -161.1798327780828117 ) ) ;
#56237 = CARTESIAN_POINT ( 'NONE',  ( 18.60000000000001563, 85.36423601037868991, -95.84285308379965329 ) ) ;
#56238 = TOROIDAL_SURFACE ( 'NONE', #202013, 0.2000000000000000111, 0.1000000000000000056 ) ;
#56239 = ORIENTED_EDGE ( 'NONE', *, *, #132397, .F. ) ;
#56240 = ORIENTED_EDGE ( 'NONE', *, *, #174241, .T. ) ;
#56241 = CARTESIAN_POINT ( 'NONE',  ( 21.05000000000000071, 1.115600667400684642E-11, -29.19999999999996732 ) ) ;
#56242 = DIRECTION ( 'NONE',  ( 0.000000000000000000, -1.000000000000000000, -6.982962677686265922E-15 ) ) ;
#56243 = EDGE_CURVE ( 'NONE', #127278, #27329, #218633, .T. ) ;
#56246 = ORIENTED_EDGE ( 'NONE', *, *, #137943, .F. ) ;
#56245 = ORIENTED_EDGE ( 'NONE', *, *, #165990, .F. ) ;
#56244 = AXIS2_PLACEMENT_3D ( 'NONE', #152140, #89557, #112992 ) ;
#56247 = ORIENTED_EDGE ( 'NONE', *, *, #110331, .T. ) ;
#56248 = DIRECTION ( 'NONE',  ( 1.000000000000000000, 0.000000000000000000, -0.000000000000000000 ) ) ;
#56249 = VERTEX_POINT ( 'NONE', #53540 ) ;
#56250 = CIRCLE ( 'NONE', #231081, 4.299999999999956302 ) ;
#56251 = ORIENTED_EDGE ( 'NONE', *, *, #237777, .F. ) ;
#56252 = FACE_OUTER_BOUND ( 'NONE', #221122, .T. ) ;
#56253 = ORIENTED_EDGE ( 'NONE', *, *, #33173, .F. ) ;
#56254 = AXIS2_PLACEMENT_3D ( 'NONE', #91519, #68098, #171100 ) ;
#56255 = AXIS2_PLACEMENT_3D ( 'NONE', #6122, #163939, #183499 ) ;
#56257 = LINE ( 'NONE', #217891, #173334 ) ;
#56256 = CARTESIAN_POINT ( 'NONE',  ( -23.25000000000000000, 69.09936979046463534, -247.6075824278584605 ) ) ;
#56258 = EDGE_CURVE ( 'NONE', #213775, #237327, #164496, .T. ) ;
#56259 = ORIENTED_EDGE ( 'NONE', *, *, #42119, .T. ) ;
#56260 = EDGE_CURVE ( 'NONE', #202492, #111962, #60418, .T. ) ;
#56261 = VERTEX_POINT ( 'NONE', #149641 ) ;
#56262 = CARTESIAN_POINT ( 'NONE',  ( -23.39999999999994529, 76.00000000001119815, -3.123107484524795474 ) ) ;
#56263 = ORIENTED_EDGE ( 'NONE', *, *, #60846, .T. ) ;
#56264 =( BOUNDED_CURVE ( )  B_SPLINE_CURVE ( 3, ( #132558, #212103, #131264, #33496 ),
 .UNSPECIFIED., .F., .T. ) 
 B_SPLINE_CURVE_WITH_KNOTS ( ( 4, 4 ),
 ( 3.141592653589793116, 4.712388980384689674 ),
 .UNSPECIFIED. ) 
 CURVE ( )  GEOMETRIC_REPRESENTATION_ITEM ( )  RATIONAL_B_SPLINE_CURVE ( ( 1.000000000000000000, 0.8047378541243649375, 0.8047378541243649375, 1.000000000000000000 ) ) 
 REPRESENTATION_ITEM ( '' )  );
#56265 = ADVANCED_FACE ( 'NONE', ( #28432, #88328 ), #152217, .F. ) ;
#56266 = CARTESIAN_POINT ( 'NONE',  ( 20.94999999999999929, 1.115600667400684642E-11, -198.0999999999999659 ) ) ;
#56267 = ORIENTED_EDGE ( 'NONE', *, *, #257941, .T. ) ;
#56268 = ORIENTED_EDGE ( 'NONE', *, *, #19963, .F. ) ;
#56269 = FACE_OUTER_BOUND ( 'NONE', #166520, .T. ) ;
#56272 = EDGE_CURVE ( 'NONE', #3898, #11614, #35527, .T. ) ;
#56271 = ORIENTED_EDGE ( 'NONE', *, *, #96790, .T. ) ;
#56270 = CARTESIAN_POINT ( 'NONE',  ( -20.94999999999999929, 1.835341550235569663, -78.55515129256302487 ) ) ;
#56273 = DIRECTION ( 'NONE',  ( 1.000000000000000000, -1.207181226542539700E-16, 2.694675058168174199E-16 ) ) ;
#56274 = DIRECTION ( 'NONE',  ( -1.000000000000000000, 0.000000000000000000, 0.000000000000000000 ) ) ;
#56275 = ORIENTED_EDGE ( 'NONE', *, *, #89119, .F. ) ;
#56276 = EDGE_CURVE ( 'NONE', #70073, #192399, #32265, .T. ) ;
#56277 = DIRECTION ( 'NONE',  ( 0.000000000000000000, 6.982962677686266711E-15, -1.000000000000000000 ) ) ;
#56278 = CARTESIAN_POINT ( 'NONE',  ( -23.15000000000000213, 64.35000000001214460, -136.5231074845243597 ) ) ;
#56279 = CARTESIAN_POINT ( 'NONE',  ( 20.94999999999999929, 76.00000000001170974, -69.52310748452431710 ) ) ;
#56280 = CARTESIAN_POINT ( 'NONE',  ( -21.44999999999999929, 68.65000000001261071, -191.2731074845244166 ) ) ;
#56281 = TOROIDAL_SURFACE ( 'NONE', #226985, 12.97499999999999609, 0.1000000000000000056 ) ;
#56282 = CARTESIAN_POINT ( 'NONE',  ( 18.50000000000000000, -9.399999999988843058, -73.99928567783889832 ) ) ;
#56283 = DIRECTION ( 'NONE',  ( -1.000000000000000000, -1.394253735153569469E-16, -2.602809386958778209E-16 ) ) ;
#56284 = CARTESIAN_POINT ( 'NONE',  ( 21.05000000000000071, 64.35000000001214460, -136.4231074845243938 ) ) ;
#56285 = CIRCLE ( 'NONE', #214683, 0.5000000000000004441 ) ;
#56287 = EDGE_CURVE ( 'NONE', #169346, #58482, #66499, .T. ) ;
#56286 = DIRECTION ( 'NONE',  ( -0.5735764363510466035, 0.8191520442889914655, 0.000000000000000000 ) ) ;
#56288 = DIRECTION ( 'NONE',  ( 0.000000000000000000, -7.086529944415894657E-15, 1.000000000000000000 ) ) ;
#56289 = VECTOR ( 'NONE', #77333, 999.9999999999998863 ) ;
#56290 = VERTEX_POINT ( 'NONE', #251270 ) ;
#56291 = AXIS2_PLACEMENT_3D ( 'NONE', #229723, #51048, #31562 ) ;
#56293 = ORIENTED_EDGE ( 'NONE', *, *, #189167, .F. ) ;
#56292 = VERTEX_POINT ( 'NONE', #8829 ) ;
#56294 = AXIS2_PLACEMENT_3D ( 'NONE', #246521, #31375, #91316 ) ;
#56295 = ORIENTED_EDGE ( 'NONE', *, *, #35719, .T. ) ;
#56297 = EDGE_CURVE ( 'NONE', #235080, #192701, #247426, .T. ) ;
#56296 = LINE ( 'NONE', #251941, #161264 ) ;
#56298 = DIRECTION ( 'NONE',  ( 0.000000000000000000, 0.000000000000000000, 1.000000000000000000 ) ) ;
#56300 = DIRECTION ( 'NONE',  ( 1.000000000000000000, -3.265361837132813093E-16, -2.280189983783949500E-30 ) ) ;
#56299 = CARTESIAN_POINT ( 'NONE',  ( -20.54999999999999716, 84.73084112150711178, -79.12118220350858167 ) ) ;
#56302 = ORIENTED_EDGE ( 'NONE', *, *, #164322, .T. ) ;
#56301 = VECTOR ( 'NONE', #195867, 1000.000000000000000 ) ;
#56303 = DIRECTION ( 'NONE',  ( 1.000000000000000000, 0.000000000000000000, 0.000000000000000000 ) ) ;
#56304 = CARTESIAN_POINT ( 'NONE',  ( 21.30000000000002558, 76.00000000001237765, -170.0231074845243597 ) ) ;
#56305 = CIRCLE ( 'NONE', #202075, 0.1000000000000028644 ) ;
#56306 = CARTESIAN_POINT ( 'NONE',  ( -20.64999999999999858, 2.400000000011155432, -187.7753780772378889 ) ) ;
#56307 = CARTESIAN_POINT ( 'NONE',  ( 20.94999999999999929, -8.999999999988842703, -191.1060308773475072 ) ) ;
#56308 = ORIENTED_EDGE ( 'NONE', *, *, #162986, .F. ) ;
#56309 = ORIENTED_EDGE ( 'NONE', *, *, #149713, .T. ) ;
#56310 = DIRECTION ( 'NONE',  ( 1.000000000000000000, -0.000000000000000000, 0.000000000000000000 ) ) ;
#56311 = CARTESIAN_POINT ( 'NONE',  ( 20.94999999999999574, 77.16270174995064224, -195.4231074845243370 ) ) ;
#56312 = ORIENTED_EDGE ( 'NONE', *, *, #186651, .T. ) ;
#56313 = CARTESIAN_POINT ( 'NONE',  ( 20.94999999999999929, 1.115600667400684642E-11, -67.00000000000000000 ) ) ;
#56314 = CARTESIAN_POINT ( 'NONE',  ( 21.14999999999999858, 75.90220970870339556, -142.7809220950004203 ) ) ;
#56315 = AXIS2_PLACEMENT_3D ( 'NONE', #230061, #207952, #110105 ) ;
#56316 = DIRECTION ( 'NONE',  ( 0.000000000000000000, -1.000000000000000000, -6.982962677686265922E-15 ) ) ;
#56317 = DIRECTION ( 'NONE',  ( 0.000000000000000000, 1.000000000000000000, 6.982962677686266711E-15 ) ) ;
#56318 = FACE_OUTER_BOUND ( 'NONE', #140715, .T. ) ;
#56319 = ORIENTED_EDGE ( 'NONE', *, *, #39965, .T. ) ;
#56320 = CARTESIAN_POINT ( 'NONE',  ( 20.94999999999999574, 43.44873802792533724, -245.1397081572968659 ) ) ;
#56321 = DIRECTION ( 'NONE',  ( 0.000000000000000000, 0.000000000000000000, -1.000000000000000000 ) ) ;
#56322 = DIRECTION ( 'NONE',  ( 0.000000000000000000, -6.982962677686266711E-15, 1.000000000000000000 ) ) ;
#56324 = CARTESIAN_POINT ( 'NONE',  ( -16.87036670365548474, 66.01058118071090064, -182.5435473672224020 ) ) ;
#56323 = DIRECTION ( 'NONE',  ( 1.000000000000000000, 0.000000000000000000, 0.000000000000000000 ) ) ;
#56325 = LINE ( 'NONE', #1495, #33217 ) ;
#56326 = DIRECTION ( 'NONE',  ( 1.000000000000000000, 0.000000000000000000, 0.000000000000000000 ) ) ;
#56327 = DIRECTION ( 'NONE',  ( -1.000000000000000000, 0.000000000000000000, 0.000000000000000000 ) ) ;
#56328 = DIRECTION ( 'NONE',  ( 1.000000000000000000, 0.000000000000000000, 0.000000000000000000 ) ) ;
#56330 = ORIENTED_EDGE ( 'NONE', *, *, #208937, .F. ) ;
#56329 = AXIS2_PLACEMENT_3D ( 'NONE', #67191, #175010, #254462 ) ;
#56331 = EDGE_CURVE ( 'NONE', #204733, #230108, #176991, .T. ) ;
#56332 = VECTOR ( 'NONE', #129871, 1000.000000000000000 ) ;
#56333 = ORIENTED_EDGE ( 'NONE', *, *, #107357, .F. ) ;
#56334 = FACE_OUTER_BOUND ( 'NONE', #112903, .T. ) ;
#56335 = ORIENTED_EDGE ( 'NONE', *, *, #229567, .T. ) ;
#56336 = EDGE_CURVE ( 'NONE', #58672, #189831, #44798, .T. ) ;
#56337 = DIRECTION ( 'NONE',  ( 0.000000000000000000, 0.000000000000000000, 1.000000000000000000 ) ) ;
#56338 = VERTEX_POINT ( 'NONE', #147032 ) ;
#56339 = EDGE_CURVE ( 'NONE', #158124, #85588, #68812, .T. ) ;
#56340 =( LENGTH_UNIT ( ) NAMED_UNIT ( * ) SI_UNIT ( .MILLI., .METRE. ) );
#56341 = EDGE_CURVE ( 'NONE', #155942, #23713, #106195, .T. ) ;
#56342 = DIRECTION ( 'NONE',  ( 1.000000000000000000, 0.000000000000000000, 0.000000000000000000 ) ) ;
#56343 = AXIS2_PLACEMENT_3D ( 'NONE', #250963, #52765, #112761 ) ;
#56344 = ORIENTED_EDGE ( 'NONE', *, *, #197187, .F. ) ;
#56345 = CARTESIAN_POINT ( 'NONE',  ( -16.94445028196807002, 30.26380394232451465, -234.7901145182196956 ) ) ;
#56346 = CARTESIAN_POINT ( 'NONE',  ( -14.45422546970484667, 9.450602096099681049, -51.94389596309667922 ) ) ;
#56347 = CARTESIAN_POINT ( 'NONE',  ( -20.64999999999999858, 68.75000000001223555, -148.8731074845244109 ) ) ;
#56348 = DIRECTION ( 'NONE',  ( 0.000000000000000000, 6.982962677686266711E-15, -1.000000000000000000 ) ) ;
#56350 = ORIENTED_EDGE ( 'NONE', *, *, #26855, .F. ) ;
#56349 = LINE ( 'NONE', #75941, #125959 ) ;
#56352 = CARTESIAN_POINT ( 'NONE',  ( 20.01093837587850288, 11.75000000001116263, -192.2543974345975926 ) ) ;
#56351 = CARTESIAN_POINT ( 'NONE',  ( 20.94999999999999574, 1.162701749949165642, -41.40000000000000568 ) ) ;
#56353 = EDGE_CURVE ( 'NONE', #106103, #249368, #93745, .T. ) ;
#56354 = CARTESIAN_POINT ( 'NONE',  ( -23.15000000000000213, 2.500000000011156409, -147.2246219227621111 ) ) ;
#56355 = DIRECTION ( 'NONE',  ( 0.000000000000000000, -6.352154140967427193E-15, 1.000000000000000000 ) ) ;
#56356 = CARTESIAN_POINT ( 'NONE',  ( 20.85000000000000142, 0.1610488207187191212, -33.21581015563977957 ) ) ;
#56358 = EDGE_CURVE ( 'NONE', #4326, #157944, #34465, .T. ) ;
#56357 = CARTESIAN_POINT ( 'NONE',  ( -21.05000000000000071, -4.557064143889599350, -233.1584191572127622 ) ) ;
#56359 = EDGE_LOOP ( 'NONE', ( #212880, #145028, #227056, #215647 ) ) ;
#56360 = DIRECTION ( 'NONE',  ( 1.000000000000000000, 0.000000000000000000, 0.000000000000000000 ) ) ;
#56361 = DIRECTION ( 'NONE',  ( 0.000000000000000000, 0.000000000000000000, 1.000000000000000000 ) ) ;
#56362 = PRODUCT_RELATED_PRODUCT_CATEGORY ( 'part', '', ( #247102 ) ) ;
#56363 = ORIENTED_EDGE ( 'NONE', *, *, #176340, .T. ) ;
#56364 = DIRECTION ( 'NONE',  ( 0.000000000000000000, -6.982962677686266711E-15, 1.000000000000000000 ) ) ;
#56365 = ORIENTED_EDGE ( 'NONE', *, *, #132859, .F. ) ;
#56366 = AXIS2_PLACEMENT_3D ( 'NONE', #224926, #87974, #223640 ) ;
#56368 = FACE_OUTER_BOUND ( 'NONE', #182295, .T. ) ;
#56367 = COLOUR_RGB ( '', 0.40784314, 0.44705882, 0.49803922) ;
#56369 = ADVANCED_FACE ( 'NONE', ( #89251 ), #14670, .T. ) ;
#56370 = CARTESIAN_POINT ( 'NONE',  ( 20.94999999999999574, -11.64999999998883595, -170.4999999999999716 ) ) ;
#56371 = CARTESIAN_POINT ( 'NONE',  ( 18.39999999999999858, 85.51932773110476660, -163.0501311079649440 ) ) ;
#56372 = EDGE_CURVE ( 'NONE', #123814, #155690, #214539, .T. ) ;
#56373 = ORIENTED_EDGE ( 'NONE', *, *, #151885, .T. ) ;
#56374 = EDGE_CURVE ( 'NONE', #241262, #205787, #232652, .T. ) ;
#56375 = ORIENTED_EDGE ( 'NONE', *, *, #169312, .F. ) ;
#56376 = LINE ( 'NONE', #38136, #56935 ) ;
#56377 = CARTESIAN_POINT ( 'NONE',  ( 20.95346350065193519, 10.49492647445341831, -207.4255753433062353 ) ) ;
#56378 = CARTESIAN_POINT ( 'NONE',  ( -16.85722902420173241, 63.05548745535527644, -213.2391404860300952 ) ) ;
#56379 = EDGE_CURVE ( 'NONE', #221674, #85751, #239508, .T. ) ;
#56382 = DIRECTION ( 'NONE',  ( 1.000000000000000000, 0.000000000000000000, 0.000000000000000000 ) ) ;
#56381 = CIRCLE ( 'NONE', #243835, 0.09999999999998898659 ) ;
#56380 = PLANE ( 'NONE',  #186711 ) ;
#56383 = CARTESIAN_POINT ( 'NONE',  ( 18.59999999999999076, 10.25000000001115552, -91.75000000000005684 ) ) ;
#56384 = CIRCLE ( 'NONE', #89714, 0.09999999999999939493 ) ;
#56385 = CARTESIAN_POINT ( 'NONE',  ( -23.15000000000000213, 87.48912529308779540, -72.62310748452422615 ) ) ;
#56386 = CARTESIAN_POINT ( 'NONE',  ( 21.05000000000000071, 30.84068117814317134, -252.2514754752610031 ) ) ;
#56388 = ORIENTED_EDGE ( 'NONE', *, *, #243120, .F. ) ;
#56387 = VECTOR ( 'NONE', #183720, 1000.000000000000000 ) ;
#56389 = DIRECTION ( 'NONE',  ( 0.000000000000000000, -0.9947597004326452774, 0.1022405907414166287 ) ) ;
#56390 = AXIS2_PLACEMENT_3D ( 'NONE', #24851, #185175, #106910 ) ;
#56392 = ORIENTED_EDGE ( 'NONE', *, *, #119424, .F. ) ;
#56391 = FACE_OUTER_BOUND ( 'NONE', #18143, .T. ) ;
#56393 = DIRECTION ( 'NONE',  ( 0.000000000000000000, 0.9274965247785529332, 0.3738317757009255171 ) ) ;
#56394 = LINE ( 'NONE', #60254, #219872 ) ;
#56396 = DIRECTION ( 'NONE',  ( 0.000000000000000000, 0.000000000000000000, -1.000000000000000000 ) ) ;
#56395 = LINE ( 'NONE', #215482, #113559 ) ;
#56398 = VERTEX_POINT ( 'NONE', #71013 ) ;
#56397 = CARTESIAN_POINT ( 'NONE',  ( -21.44999999999999929, 7.150000000011155876, -121.6500000000000341 ) ) ;
#56400 = FACE_OUTER_BOUND ( 'NONE', #125496, .T. ) ;
#56399 = DIRECTION ( 'NONE',  ( 0.000000000000000000, -0.2128009952263603677, 0.9770955615653313941 ) ) ;
#56401 = CARTESIAN_POINT ( 'NONE',  ( -21.05000000000000071, 77.36087058720393372, -94.95010955743333625 ) ) ;
#56402 = DIRECTION ( 'NONE',  ( 1.000000000000000000, 0.000000000000000000, 0.000000000000000000 ) ) ;
#56403 = LINE ( 'NONE', #135940, #215868 ) ;
#56404 = CARTESIAN_POINT ( 'NONE',  ( 21.05000000000000426, 65.43724016256129516, -162.5662935266058184 ) ) ;
#56405 = ORIENTED_EDGE ( 'NONE', *, *, #189513, .F. ) ;
#56406 = CARTESIAN_POINT ( 'NONE',  ( -18.50000000000000000, 9.350000000011156942, -146.3500000000000227 ) ) ;
#56407 = ORIENTED_EDGE ( 'NONE', *, *, #183202, .T. ) ;
#56408 = EDGE_CURVE ( 'NONE', #135166, #202789, #29332, .T. ) ;
#56409 = DIRECTION ( 'NONE',  ( -0.000000000000000000, 1.000000000000000000, 6.982962677686266711E-15 ) ) ;
#56410 = ORIENTED_EDGE ( 'NONE', *, *, #114639, .F. ) ;
#56411 = DIRECTION ( 'NONE',  ( 0.000000000000000000, 0.000000000000000000, -1.000000000000000000 ) ) ;
#56412 = AXIS2_PLACEMENT_3D ( 'NONE', #199271, #59723, #1023 ) ;
#56413 = VERTEX_POINT ( 'NONE', #193518 ) ;
#56414 = LINE ( 'NONE', #173870, #26785 ) ;
#56416 = LINE ( 'NONE', #215506, #54202 ) ;
#56415 = AXIS2_PLACEMENT_3D ( 'NONE', #204652, #185107, #145969 ) ;
#56417 = ADVANCED_FACE ( 'NONE', ( #14888 ), #189654, .F. ) ;
#56418 = CARTESIAN_POINT ( 'NONE',  ( -21.29999999999995808, 1.148907358139439339E-11, -201.0000000000015064 ) ) ;
#56420 = EDGE_LOOP ( 'NONE', ( #19271, #183801, #183093, #164249 ) ) ;
#56419 = AXIS2_PLACEMENT_3D ( 'NONE', #215802, #213245, #232842 ) ;
#56421 = VECTOR ( 'NONE', #50680, 1000.000000000000000 ) ;
#56422 = ADVANCED_FACE ( 'NONE', ( #250893 ), #89632, .F. ) ;
#56423 = CIRCLE ( 'NONE', #39895, 0.1000000000000008937 ) ;
#56425 = CARTESIAN_POINT ( 'NONE',  ( -21.76363531954647357, -1.395625584870292979, -194.1266231281565524 ) ) ;
#56424 = AXIS2_PLACEMENT_3D ( 'NONE', #237484, #58810, #96646 ) ;
#56426 = DIRECTION ( 'NONE',  ( 1.000000000000000000, -0.000000000000000000, -0.000000000000000000 ) ) ;
#56427 = CARTESIAN_POINT ( 'NONE',  ( -21.05000000000000071, 4.193200906077805712, -212.0298262072164164 ) ) ;
#56428 = CYLINDRICAL_SURFACE ( 'NONE', #128805, 0.09999999999999939493 ) ;
#56429 = CARTESIAN_POINT ( 'NONE',  ( 21.05000000000000071, -3.770473190032740174, -225.9805569534692324 ) ) ;
#56430 = VERTEX_POINT ( 'NONE', #90534 ) ;
#56431 = CARTESIAN_POINT ( 'NONE',  ( 20.04999999999999716, 8.750000000011173285, -113.1500000000000483 ) ) ;
#56432 = ORIENTED_EDGE ( 'NONE', *, *, #105227, .T. ) ;
#56434 = VERTEX_POINT ( 'NONE', #74877 ) ;
#56433 = DIRECTION ( 'NONE',  ( -0.7071067811865389130, 0.000000000000000000, 0.7071067811865561215 ) ) ;
#56435 = ADVANCED_FACE ( 'NONE', ( #52694 ), #31255, .T. ) ;
#56436 = VECTOR ( 'NONE', #248337, 1000.000000000000000 ) ;
#56437 = ORIENTED_EDGE ( 'NONE', *, *, #207806, .F. ) ;
#56438 = CARTESIAN_POINT ( 'NONE',  ( 21.07016717457011623, 1.115539956314190190E-11, -60.67905916189912574 ) ) ;
#56439 = EDGE_CURVE ( 'NONE', #218249, #129969, #77171, .T. ) ;
#56440 = CYLINDRICAL_SURFACE ( 'NONE', #184128, 0.1000000000000038219 ) ;
#56441 = AXIS2_PLACEMENT_3D ( 'NONE', #201648, #125952, #202931 ) ;
#56442 = CARTESIAN_POINT ( 'NONE',  ( -23.15000000000000213, 64.25000000001195133, -103.0231074845244024 ) ) ;
#56443 = DIRECTION ( 'NONE',  ( -0.000000000000000000, -0.1298341882520022694, -0.9915357197604853789 ) ) ;
#56444 = EDGE_LOOP ( 'NONE', ( #18727, #142381, #39869, #19324 ) ) ;
#56445 = AXIS2_PLACEMENT_3D ( 'NONE', #257787, #196577, #178334 ) ;
#56446 = DIRECTION ( 'NONE',  ( 1.000000000000000000, 0.000000000000000000, 0.000000000000000000 ) ) ;
#56447 = DIRECTION ( 'NONE',  ( 0.000000000000000000, 0.000000000000000000, -1.000000000000000000 ) ) ;
#56448 = CIRCLE ( 'NONE', #10677, 0.09999999999999080458 ) ;
#56449 = ORIENTED_EDGE ( 'NONE', *, *, #61390, .F. ) ;
#56451 = ORIENTED_EDGE ( 'NONE', *, *, #163634, .T. ) ;
#56450 = DIRECTION ( 'NONE',  ( 0.000000000000000000, -7.116814260417668513E-15, 1.000000000000000000 ) ) ;
#56452 = LINE ( 'NONE', #197261, #39995 ) ;
#56453 = CARTESIAN_POINT ( 'NONE',  ( 21.05000000000000071, -11.64999999998883595, -97.60000000000005116 ) ) ;
#56454 = EDGE_CURVE ( 'NONE', #114896, #33295, #2152, .T. ) ;
#56455 = FACE_OUTER_BOUND ( 'NONE', #172999, .T. ) ;
#56456 = ORIENTED_EDGE ( 'NONE', *, *, #247698, .T. ) ;
#56457 = DIRECTION ( 'NONE',  ( 0.000000000000000000, 0.000000000000000000, 1.000000000000000000 ) ) ;
#56458 = EDGE_CURVE ( 'NONE', #189583, #144252, #251961, .T. ) ;
#56459 = CARTESIAN_POINT ( 'NONE',  ( 23.14999999999999858, 76.00000000001190870, -103.0231074845243029 ) ) ;
#56460 = CARTESIAN_POINT ( 'NONE',  ( 20.94999999999999574, -11.64999999998883595, -170.3999999999999773 ) ) ;
#56461 = B_SPLINE_CURVE_WITH_KNOTS ( 'NONE', 3,
 ( #181893, #243139, #43666, #85325, #162344, #164897, #61945, #120653, #1942, #141470 ),
 .UNSPECIFIED., .F., .F.,
 ( 4, 2, 2, 2, 4 ),
 ( 0.000000000000000000, 3.990160268013063079E-05, 7.980320536026126157E-05, 0.0001596064107205095669, 0.0003192128214409942514 ),
 .UNSPECIFIED. ) ;
#56462 = AXIS2_PLACEMENT_3D ( 'NONE', #32810, #133158, #13221 ) ;
#56463 = EDGE_CURVE ( 'NONE', #56104, #30748, #143625, .T. ) ;
#56464 = AXIS2_PLACEMENT_3D ( 'NONE', #167235, #129357, #30276 ) ;
#56465 = VECTOR ( 'NONE', #197625, 1000.000000000000000 ) ;
#56466 = EDGE_CURVE ( 'NONE', #73461, #256381, #18735, .T. ) ;
#56467 = VERTEX_POINT ( 'NONE', #11014 ) ;
#56468 = VECTOR ( 'NONE', #246418, 1000.000000000000000 ) ;
#56469 = ORIENTED_EDGE ( 'NONE', *, *, #116428, .F. ) ;
#56470 = CARTESIAN_POINT ( 'NONE',  ( -16.94107738177415712, 12.45552124806248706, -211.1315092113344463 ) ) ;
#56471 = CARTESIAN_POINT ( 'NONE',  ( -22.50485643085239928, -0.07878633906603055292, -21.75020506082759653 ) ) ;
#56473 = ORIENTED_EDGE ( 'NONE', *, *, #167381, .T. ) ;
#56472 = DIRECTION ( 'NONE',  ( 1.000000000000000000, 0.000000000000000000, 0.000000000000000000 ) ) ;
#56475 = EDGE_CURVE ( 'NONE', #85681, #154033, #206178, .T. ) ;
#56474 = LINE ( 'NONE', #215563, #195083 ) ;
#56476 = CARTESIAN_POINT ( 'NONE',  ( 21.13461538461538325, 67.11458296203814200, -191.1731074845244223 ) ) ;
#56477 = PLANE ( 'NONE',  #181127 ) ;
#56479 = CARTESIAN_POINT ( 'NONE',  ( 21.07946286933444568, 75.92331615675561807, -109.3521448035320560 ) ) ;
#56478 = AXIS2_PLACEMENT_3D ( 'NONE', #164397, #142251, #182687 ) ;
#56480 = CARTESIAN_POINT ( 'NONE',  ( 21.05000000000000071, 6.258847123090218290, -33.46824164694449877 ) ) ;
#56481 = EDGE_CURVE ( 'NONE', #86831, #79296, #148103, .T. ) ;
#56482 = AXIS2_PLACEMENT_3D ( 'NONE', #218605, #40027, #101200 ) ;
#56483 = DIRECTION ( 'NONE',  ( 0.000000000000000000, -1.000000000000000000, -6.982962677686265922E-15 ) ) ;
#56484 = LINE ( 'NONE', #90484, #219580 ) ;
#56486 = VERTEX_POINT ( 'NONE', #138629 ) ;
#56485 = DIRECTION ( 'NONE',  ( 0.000000000000000000, 0.4088369013363281623, -0.9126074666063771490 ) ) ;
#56487 = AXIS2_PLACEMENT_3D ( 'NONE', #50591, #187581, #169319 ) ;
#56488 = CARTESIAN_POINT ( 'NONE',  ( -18.50000000000000000, 68.00366762990590530, -224.2307594727497815 ) ) ;
#56489 = CIRCLE ( 'NONE', #202269, 0.09999999999999939493 ) ;
#56490 = DIRECTION ( 'NONE',  ( 0.000000000000000000, 0.000000000000000000, -1.000000000000000000 ) ) ;
#56491 = CARTESIAN_POINT ( 'NONE',  ( -18.40000000000000213, 85.51932773110506503, -196.5501311079650009 ) ) ;
#56492 = EDGE_LOOP ( 'NONE', ( #14340, #133213, #16528, #157885 ) ) ;
#56493 = DIRECTION ( 'NONE',  ( 0.000000000000000000, 0.000000000000000000, 1.000000000000000000 ) ) ;
#56494 = CARTESIAN_POINT ( 'NONE',  ( 20.94999999999999929, 76.00000000001142553, -36.02310748452432421 ) ) ;
#56495 = CARTESIAN_POINT ( 'NONE',  ( -18.49999999999997158, 85.32100840337291459, -62.28716923544639172 ) ) ;
#56496 = ORIENTED_EDGE ( 'NONE', *, *, #211998, .F. ) ;
#56498 = EDGE_CURVE ( 'NONE', #233103, #81229, #48137, .T. ) ;
#56497 = LINE ( 'NONE', #61660, #68780 ) ;
#56499 = CIRCLE ( 'NONE', #223122, 0.1000000000000000472 ) ;
#56500 = AXIS2_PLACEMENT_3D ( 'NONE', #204517, #49301, #168011 ) ;
#56501 = CARTESIAN_POINT ( 'NONE',  ( -16.94445028196808778, 66.00793639031486748, -190.9157773061059800 ) ) ;
#56502 = VERTEX_POINT ( 'NONE', #218174 ) ;
#56503 = CARTESIAN_POINT ( 'NONE',  ( -18.38204789744325396, 11.47950103717623982, -124.7500000000000284 ) ) ;
#56504 = ORIENTED_EDGE ( 'NONE', *, *, #191577, .T. ) ;
#56505 = DIRECTION ( 'NONE',  ( -0.000000000000000000, 0.000000000000000000, 1.000000000000000000 ) ) ;
#56507 = ORIENTED_EDGE ( 'NONE', *, *, #120309, .F. ) ;
#56506 = DIRECTION ( 'NONE',  ( 1.000000000000000000, 0.000000000000000000, 0.000000000000000000 ) ) ;
#56508 = DIRECTION ( 'NONE',  ( 1.000000000000000000, 0.000000000000000000, 0.000000000000000000 ) ) ;
#56509 = ORIENTED_EDGE ( 'NONE', *, *, #226988, .T. ) ;
#56510 = CARTESIAN_POINT ( 'NONE',  ( 20.94999999999999929, 10.29270135741298731, -105.9573618871519756 ) ) ;
#56511 = ORIENTED_EDGE ( 'NONE', *, *, #73226, .T. ) ;
#56513 = ORIENTED_EDGE ( 'NONE', *, *, #182966, .T. ) ;
#56512 = ORIENTED_EDGE ( 'NONE', *, *, #120084, .F. ) ;
#56514 = FACE_OUTER_BOUND ( 'NONE', #106979, .T. ) ;
#56515 = ORIENTED_EDGE ( 'NONE', *, *, #190425, .T. ) ;
#56516 = ADVANCED_FACE ( 'NONE', ( #119111 ), #79935, .F. ) ;
#56517 = CARTESIAN_POINT ( 'NONE',  ( -23.15000000000000213, 2.600000000011154278, -120.7753780772379315 ) ) ;
#56518 = VECTOR ( 'NONE', #13365, 1000.000000000000000 ) ;
#56519 = EDGE_LOOP ( 'NONE', ( #153802, #6839, #13264, #77785 ) ) ;
#56520 = CONICAL_SURFACE ( 'NONE', #177207, 4.299999999999956302, 0.7853981633974466137 ) ;
#56521 = EDGE_LOOP ( 'NONE', ( #129747, #206877, #121433 ) ) ;
#56522 = CARTESIAN_POINT ( 'NONE',  ( 16.27683809663749770, 9.349999999999983658, -9.250000000000005329 ) ) ;
#56523 = CARTESIAN_POINT ( 'NONE',  ( -20.94999999999999929, 1.115600667400684642E-11, -167.5000000000000284 ) ) ;
#56524 = FACE_OUTER_BOUND ( 'NONE', #147970, .T. ) ;
#56525 = ORIENTED_EDGE ( 'NONE', *, *, #39648, .F. ) ;
#56526 = CARTESIAN_POINT ( 'NONE',  ( -18.59999999999999787, 76.00000000001170974, -69.52310748452431710 ) ) ;
#56527 = CARTESIAN_POINT ( 'NONE',  ( -18.46093223321774701, -9.480682968263366206, -74.08455051392672885 ) ) ;
#56528 = CARTESIAN_POINT ( 'NONE',  ( 21.05000000000000071, -8.730841121484166578, -90.90192528101570701 ) ) ;
#56529 = EDGE_LOOP ( 'NONE', ( #250358, #72252, #67200, #188205, #238764 ) ) ;
#56530 = LINE ( 'NONE', #215623, #250207 ) ;
#56531 = DIRECTION ( 'NONE',  ( -1.000000000000000000, 0.000000000000000000, -0.000000000000000000 ) ) ;
#56532 = CARTESIAN_POINT ( 'NONE',  ( -21.05000000000000071, 5.850000000011156942, -190.8675027757220448 ) ) ;
#56533 = ORIENTED_EDGE ( 'NONE', *, *, #79664, .T. ) ;
#56534 = CARTESIAN_POINT ( 'NONE',  ( 21.05000000000000071, 4.850467289730776344, -54.96573259099832143 ) ) ;
#56535 = ORIENTED_EDGE ( 'NONE', *, *, #55285, .F. ) ;
#56536 = VERTEX_POINT ( 'NONE', #155692 ) ;
#56537 = AXIS2_PLACEMENT_3D ( 'NONE', #78691, #194837, #16197 ) ;
#56538 = CIRCLE ( 'NONE', #160657, 0.1000000000000028644 ) ;
#56539 = DIRECTION ( 'NONE',  ( 0.000000000000000000, 0.000000000000000000, -1.000000000000000000 ) ) ;
#56540 = VERTEX_POINT ( 'NONE', #143472 ) ;
#56541 = VERTEX_POINT ( 'NONE', #77389 ) ;
#56542 = DIRECTION ( 'NONE',  ( 0.000000000000000000, -6.982962677686266711E-15, 1.000000000000000000 ) ) ;
#56543 = ORIENTED_EDGE ( 'NONE', *, *, #87986, .T. ) ;
#56544 = ORIENTED_EDGE ( 'NONE', *, *, #199176, .F. ) ;
#56545 = CARTESIAN_POINT ( 'NONE',  ( -21.14999999999999858, -11.64999999998884483, -36.39999999999999858 ) ) ;
#56546 = DIRECTION ( 'NONE',  ( 1.000000000000000000, 7.304098846218134667E-16, 0.000000000000000000 ) ) ;
#56547 = ORIENTED_EDGE ( 'NONE', *, *, #81364, .F. ) ;
#56548 = EDGE_CURVE ( 'NONE', #132612, #163978, #239052, .T. ) ;
#56549 = AXIS2_PLACEMENT_3D ( 'NONE', #121404, #84761, #2682 ) ;
#56550 = ORIENTED_EDGE ( 'NONE', *, *, #117449, .T. ) ;
#56551 = CIRCLE ( 'NONE', #19176, 0.09999999999998898659 ) ;
#56552 = CIRCLE ( 'NONE', #69264, 0.1000000000000028644 ) ;
#56553 = FACE_OUTER_BOUND ( 'NONE', #169773, .T. ) ;
#56554 = MECHANICAL_DESIGN_GEOMETRIC_PRESENTATION_REPRESENTATION (  '', ( #52482 ), #164920 ) ;
#56555 = EDGE_CURVE ( 'NONE', #185405, #81280, #156512, .T. ) ;
#56556 = DIRECTION ( 'NONE',  ( 0.000000000000000000, 6.982962677686266711E-15, -1.000000000000000000 ) ) ;
#56557 = EDGE_CURVE ( 'NONE', #188914, #238533, #177356, .T. ) ;
#56558 = CARTESIAN_POINT ( 'NONE',  ( -18.39999999999999858, 37.95493834378066111, -261.2294694241335264 ) ) ;
#56559 = DIRECTION ( 'NONE',  ( 0.000000000000000000, 0.000000000000000000, -1.000000000000000000 ) ) ;
#56560 = CARTESIAN_POINT ( 'NONE',  ( 20.99999999999999645, 41.11438369982452912, -236.8714985644722617 ) ) ;
#56561 = CARTESIAN_POINT ( 'NONE',  ( 20.94999999999999929, 9.374458193048763377, -220.5475659691911119 ) ) ;
#56562 = DIRECTION ( 'NONE',  ( 0.000000000000000000, 0.8814952561688432775, -0.4721928772777342354 ) ) ;
#56564 = DIRECTION ( 'NONE',  ( 0.000000000000000000, 0.9998779222360102414, 0.01562499999996356907 ) ) ;
#56563 = CARTESIAN_POINT ( 'NONE',  ( 21.07954640115298162, 75.93399229287204832, -75.85239518054815733 ) ) ;
#56565 = DIRECTION ( 'NONE',  ( 0.000000000000000000, 1.000000000000000000, 0.000000000000000000 ) ) ;
#56566 = CARTESIAN_POINT ( 'NONE',  ( -16.84981964351493744, 23.15621314347246340, -231.0675665507066867 ) ) ;
#56567 = EDGE_CURVE ( 'NONE', #234900, #68838, #143987, .T. ) ;
#56568 = DIRECTION ( 'NONE',  ( 0.000000000000000000, 0.8103668758649578141, -0.5859227990963213895 ) ) ;
#56569 = CARTESIAN_POINT ( 'NONE',  ( 21.05281448260627641, 44.18064746791630881, -236.5651106086473021 ) ) ;
#56570 = AXIS2_PLACEMENT_3D ( 'NONE', #132565, #93419, #114276 ) ;
#56571 =( BOUNDED_SURFACE ( )  B_SPLINE_SURFACE ( 3, 2, ( 
 ( #127971, #6728, #185370 ),
 ( #2863, #242762, #64145 ),
 ( #207520, #101949, #181538 ),
 ( #143668, #223198, #203652 ),
 ( #184083, #165831, #5416 ),
 ( #84947, #164538, #244047 ) ),
 .UNSPECIFIED., .F., .F., .F. ) 
 B_SPLINE_SURFACE_WITH_KNOTS ( ( 4, 2, 4 ),
 ( 3, 3 ),
 ( 1.570796326794897668, 2.356194490192346169, 3.141592653589794448 ),
 ( 0.000000000000000000, 1.000000000000000000 ),
 .UNSPECIFIED. ) 
 GEOMETRIC_REPRESENTATION_ITEM ( )  RATIONAL_B_SPLINE_SURFACE ( (
 ( 1.000000000000000000, 0.7071067811865341390, 1.000000000000000000),
 ( 1.000000000000000000, 0.6611148371781488953, 1.000000000000000000),
 ( 1.000000000000000000, 0.6092287576690736950, 1.000000000000000000),
 ( 1.000000000000000000, 0.5278258667062413201, 1.000000000000000000),
 ( 1.000000000000000000, 0.4993418825330954713, 1.000000000000000000),
 ( 1.000000000000000000, 0.4999999999999439337, 1.000000000000000000) ) ) 
 REPRESENTATION_ITEM ( '' )  SURFACE ( )  );
#56572 = EDGE_LOOP ( 'NONE', ( #194, #73275, #195619, #233594 ) ) ;
#56573 =( GEOMETRIC_REPRESENTATION_CONTEXT ( 3 ) GLOBAL_UNCERTAINTY_ASSIGNED_CONTEXT ( ( #167788 ) ) GLOBAL_UNIT_ASSIGNED_CONTEXT ( ( #231420, #95726, #211856 ) ) REPRESENTATION_CONTEXT ( 'NONE', 'WORKASPACE' ) );
#56574 = AXIS2_PLACEMENT_3D ( 'NONE', #15151, #73869, #54255 ) ;
#56576 = ORIENTED_EDGE ( 'NONE', *, *, #72005, .F. ) ;
#56575 = CARTESIAN_POINT ( 'NONE',  ( -18.59999999999999787, -1.687074390080403941, -20.68542703345834965 ) ) ;
#56577 = CIRCLE ( 'NONE', #181539, 0.1000000000000011990 ) ;
#56578 = ADVANCED_FACE ( 'NONE', ( #39604 ), #16176, .T. ) ;
#56579 = CARTESIAN_POINT ( 'NONE',  ( -20.64999999999999858, 67.23127455305835554, -235.8551265064784559 ) ) ;
#56580 = AXIS2_PLACEMENT_3D ( 'NONE', #188618, #27017, #106490 ) ;
#56581 = AXIS2_PLACEMENT_3D ( 'NONE', #95091, #174684, #36432 ) ;
#56582 = LINE ( 'NONE', #198694, #53006 ) ;
#56583 = VERTEX_POINT ( 'NONE', #59086 ) ;
#56584 = LINE ( 'NONE', #136125, #216351 ) ;
#56585 = CARTESIAN_POINT ( 'NONE',  ( -16.94107738177415712, 65.98576071487568129, -157.4731074845244336 ) ) ;
#56586 = ORIENTED_EDGE ( 'NONE', *, *, #256226, .T. ) ;
#56588 = PLANE ( 'NONE',  #17367 ) ;
#56587 = VECTOR ( 'NONE', #97587, 1000.000000000000000 ) ;
#56589 = DIRECTION ( 'NONE',  ( 0.000000000000000000, 0.9126074666063769270, 0.4088369013363282733 ) ) ;
#56590 = CIRCLE ( 'NONE', #235688, 7.791421356237338003 ) ;
#56591 = CARTESIAN_POINT ( 'NONE',  ( 20.02499999999999858, 9.750000000011153745, -88.15000000000004832 ) ) ;
#56593 = ORIENTED_EDGE ( 'NONE', *, *, #6370, .F. ) ;
#56592 = CARTESIAN_POINT ( 'NONE',  ( -18.50000000000000000, -1.835859311432484375, -212.5044391687984842 ) ) ;
#56594 = AXIS2_PLACEMENT_3D ( 'NONE', #78233, #237326, #108088 ) ;
#56595 = AXIS2_PLACEMENT_3D ( 'NONE', #151351, #230888, #87484 ) ;
#56597 = ORIENTED_EDGE ( 'NONE', *, *, #253795, .F. ) ;
#56596 = CARTESIAN_POINT ( 'NONE',  ( -18.44232395690051618, 85.55228255706090579, -96.18085549971709725 ) ) ;
#56598 = CARTESIAN_POINT ( 'NONE',  ( 21.08750232978087524, 10.72486338601016520, -12.22885817299956912 ) ) ;
#56599 = CARTESIAN_POINT ( 'NONE',  ( 18.39999999999999503, 11.75000000001113953, -46.15000000000000568 ) ) ;
#56600 = CARTESIAN_POINT ( 'NONE',  ( -22.50000000000000000, 55.96443555106008461, -232.8914797391818752 ) ) ;
#56602 = CARTESIAN_POINT ( 'NONE',  ( 23.15000000000000213, -11.48912529306489994, -197.8999999999999773 ) ) ;
#56601 = CARTESIAN_POINT ( 'NONE',  ( 19.75857864376268935, 16.67126802362266247, -222.8016931105129004 ) ) ;
#56603 = DIRECTION ( 'NONE',  ( 4.408576920032446739E-17, 0.1350103645451945777, -0.9908441862701590219 ) ) ;
#56604 = LINE ( 'NONE', #177894, #20502 ) ;
#56605 = DIRECTION ( 'NONE',  ( -0.000000000000000000, 1.000000000000000000, -0.000000000000000000 ) ) ;
#56606 = DIRECTION ( 'NONE',  ( 0.000000000000000000, 0.000000000000000000, 1.000000000000000000 ) ) ;
#56607 = EDGE_LOOP ( 'NONE', ( #18734, #52930, #107882, #191933 ) ) ;
#56608 = EDGE_CURVE ( 'NONE', #257242, #121380, #197973, .T. ) ;
#56609 = DIRECTION ( 'NONE',  ( -1.836970198721029934E-16, -1.000000000000000000, -6.982962677686266711E-15 ) ) ;
#56610 = ORIENTED_EDGE ( 'NONE', *, *, #63862, .T. ) ;
#56611 = VERTEX_POINT ( 'NONE', #159528 ) ;
#56612 = SPHERICAL_SURFACE ( 'NONE', #94304, 0.1000000000000000056 ) ;
#56613 = FACE_OUTER_BOUND ( 'NONE', #216068, .T. ) ;
#56614 = VERTEX_POINT ( 'NONE', #17429 ) ;
#56616 = EDGE_CURVE ( 'NONE', #130365, #209310, #181437, .T. ) ;
#56615 =( BOUNDED_SURFACE ( )  B_SPLINE_SURFACE ( 3, 2, ( 
 ( #55407, #1865, #97095 ),
 ( #197512, #218347, #119285 ),
 ( #154581, #16346, #196231 ),
 ( #35909, #115412, #176697 ),
 ( #194983, #17587, #98375 ),
 ( #177977, #257438, #243064 ),
 ( #244344, #3153, #85244 ),
 ( #43594, #126978, #166147 ) ),
 .UNSPECIFIED., .F., .F., .F. ) 
 B_SPLINE_SURFACE_WITH_KNOTS ( ( 4, 2, 2, 4 ),
 ( 3, 3 ),
 ( 0.0001723339234021440737, 0.0002782939632049864602, 0.0003842540030078289010, 0.0005961740826135137825 ),
 ( 0.000000000000000000, 1.000000000000000000 ),
 .UNSPECIFIED. ) 
 GEOMETRIC_REPRESENTATION_ITEM ( )  RATIONAL_B_SPLINE_SURFACE ( (
 ( 1.000000000000000000, 0.9504532311154547664, 1.000000000000000000),
 ( 1.000000000000000000, 0.9506023220708359478, 1.000000000000000000),
 ( 1.000000000000000000, 0.9395774818183325605, 1.000000000000000000),
 ( 1.000000000000000000, 0.9079328464646000407, 1.000000000000000000),
 ( 1.000000000000000000, 0.8875702416213150370, 1.000000000000000000),
 ( 1.000000000000000000, 0.8205919608026237544, 1.000000000000000000),
 ( 1.000000000000000000, 0.7666842783609403300, 1.000000000000000000),
 ( 1.000000000000000000, 0.7071067811864569785, 1.000000000000000000) ) ) 
 REPRESENTATION_ITEM ( '' )  SURFACE ( )  );
#56617 = AXIS2_PLACEMENT_3D ( 'NONE', #42724, #24477, #101360 ) ;
#56618 = VECTOR ( 'NONE', #242433, 1000.000000000000000 ) ;
#56619 = VERTEX_POINT ( 'NONE', #179114 ) ;
#56620 = FACE_OUTER_BOUND ( 'NONE', #133201, .T. ) ;
#56621 = SURFACE_STYLE_FILL_AREA ( #114054 ) ;
#56623 = EDGE_CURVE ( 'NONE', #73311, #98112, #31609, .T. ) ;
#56622 = AXIS2_PLACEMENT_3D ( 'NONE', #107949, #110510, #85779 ) ;
#56624 = AXIS2_PLACEMENT_3D ( 'NONE', #37000, #156947, #136043 ) ;
#56626 = ORIENTED_EDGE ( 'NONE', *, *, #166909, .T. ) ;
#56625 = B_SPLINE_CURVE_WITH_KNOTS ( 'NONE', 3,
 ( #135646, #218317, #117956, #77519, #154557, #194954, #155827 ),
 .UNSPECIFIED., .F., .F.,
 ( 4, 3, 4 ),
 ( 0.000000000000000000, 0.0007844235214594269838, 0.001767853679404345069 ),
 .UNSPECIFIED. ) ;
#56627 = VERTEX_POINT ( 'NONE', #24848 ) ;
#56628 = AXIS2_PLACEMENT_3D ( 'NONE', #83133, #181009, #41504 ) ;
#56629 = CARTESIAN_POINT ( 'NONE',  ( 20.94999999999999929, 77.34915357198813979, -128.7356101489344837 ) ) ;
#56630 = CARTESIAN_POINT ( 'NONE',  ( 22.47071067811865319, 7.720074744509199505, -66.90090754529744288 ) ) ;
#56631 = CARTESIAN_POINT ( 'NONE',  ( -18.59999999999999787, 7.021664781911246322, -204.8335654018972605 ) ) ;
#56632 = CARTESIAN_POINT ( 'NONE',  ( 23.14999999999999503, 69.45000000001222418, -148.7731074845244166 ) ) ;
#56633 = DIRECTION ( 'NONE',  ( 0.000000000000000000, 0.000000000000000000, -1.000000000000000000 ) ) ;
#56634 = EDGE_CURVE ( 'NONE', #186373, #204719, #56489, .T. ) ;
#56635 = FACE_OUTER_BOUND ( 'NONE', #158677, .T. ) ;
#56636 = CARTESIAN_POINT ( 'NONE',  ( 21.04999999999999716, 76.01454569058356014, -143.0201252709570667 ) ) ;
#56638 = ORIENTED_EDGE ( 'NONE', *, *, #168909, .T. ) ;
#56637 = CYLINDRICAL_SURFACE ( 'NONE', #250677, 0.1000000000000028644 ) ;
#56640 = DIRECTION ( 'NONE',  ( 1.000000000000000000, 0.000000000000000000, 0.000000000000000000 ) ) ;
#56639 = CARTESIAN_POINT ( 'NONE',  ( 22.50497660315936699, 76.07871793023775808, -148.2729029894197197 ) ) ;
#56641 = CARTESIAN_POINT ( 'NONE',  ( 23.14999999999999858, 70.05000000001177796, -79.82880978955917328 ) ) ;
#56642 = AXIS2_PLACEMENT_3D ( 'NONE', #144805, #241371, #84813 ) ;
#56643 = ORIENTED_EDGE ( 'NONE', *, *, #240221, .T. ) ;
#56644 = CARTESIAN_POINT ( 'NONE',  ( -18.46856557590794168, 8.915543251359052235, -245.4376850085415356 ) ) ;
#56646 = ADVANCED_FACE ( 'NONE', ( #5220 ), #14847, .F. ) ;
#56645 = DIRECTION ( 'NONE',  ( 0.000000000000000000, 0.000000000000000000, -1.000000000000000000 ) ) ;
#56647 = ORIENTED_EDGE ( 'NONE', *, *, #103038, .T. ) ;
#56648 = CIRCLE ( 'NONE', #148261, 0.09999999999998898659 ) ;
#56649 = CARTESIAN_POINT ( 'NONE',  ( -20.64999999999999858, 71.65000000001253966, -182.3731074845244109 ) ) ;
#56650 = CARTESIAN_POINT ( 'NONE',  ( -21.05000000000000071, 1.750000000011155743, -112.1695115579016857 ) ) ;
#56651 = CARTESIAN_POINT ( 'NONE',  ( 22.49999999999999645, 64.35012909624747124, -69.60562737539740397 ) ) ;
#56652 = VERTEX_POINT ( 'NONE', #76116 ) ;
#56653 = EDGE_LOOP ( 'NONE', ( #81500, #142920, #22603, #158494 ) ) ;
#56654 = EDGE_CURVE ( 'NONE', #190492, #47603, #55239, .T. ) ;
#56655 = CARTESIAN_POINT ( 'NONE',  ( 22.49999999999999645, 64.05844819680035584, -247.1686437718134641 ) ) ;
#56656 = CARTESIAN_POINT ( 'NONE',  ( -20.64999999999999858, 76.00000000001259082, -190.5481074845243654 ) ) ;
#56657 = VECTOR ( 'NONE', #126153, 1000.000000000000000 ) ;
#56658 = CARTESIAN_POINT ( 'NONE',  ( -20.94999999999999929, 11.70000000001115126, -60.24500185048138690 ) ) ;
#56660 = EDGE_CURVE ( 'NONE', #11590, #217175, #115249, .T. ) ;
#56659 = CARTESIAN_POINT ( 'NONE',  ( -20.54999999999999716, 76.00000000001199396, -115.8981074845243029 ) ) ;
#56661 = ORIENTED_EDGE ( 'NONE', *, *, #65029, .F. ) ;
#56662 = EDGE_CURVE ( 'NONE', #120700, #127391, #96931, .T. ) ;
#56663 = CARTESIAN_POINT ( 'NONE',  ( -15.75000000000000355, 9.350000000011140955, -117.2500000000000284 ) ) ;
#56664 = DIRECTION ( 'NONE',  ( -7.304098846217948299E-16, -1.000000000000000000, 0.000000000000000000 ) ) ;
#56665 = LINE ( 'NONE', #214488, #78468 ) ;
#56666 = AXIS2_PLACEMENT_3D ( 'NONE', #161228, #144200, #3408 ) ;
#56667 = CIRCLE ( 'NONE', #19106, 7.900000000000003908 ) ;
#56668 = VECTOR ( 'NONE', #230971, 1000.000000000000114 ) ;
#56669 = AXIS2_PLACEMENT_3D ( 'NONE', #93837, #95127, #212531 ) ;
#56670 = DIRECTION ( 'NONE',  ( -1.000000000000000000, 1.652117596168391700E-15, 0.000000000000000000 ) ) ;
#56672 = ORIENTED_EDGE ( 'NONE', *, *, #231325, .T. ) ;
#56671 = CARTESIAN_POINT ( 'NONE',  ( -14.00000000000000178, 66.15000000001228386, -153.2731074845244166 ) ) ;
#56673 = FACE_OUTER_BOUND ( 'NONE', #148054, .T. ) ;
#56675 = EDGE_CURVE ( 'NONE', #253099, #155361, #231321, .T. ) ;
#56674 = DIRECTION ( 'NONE',  ( 0.000000000000000000, -0.9126074666063769270, -0.4088369013363280513 ) ) ;
#56676 = CARTESIAN_POINT ( 'NONE',  ( -18.59999999999999787, 1.115600667400684642E-11, -134.0000000000000000 ) ) ;
#56677 = DIRECTION ( 'NONE',  ( 0.000000000000000000, 0.2128009952263603122, -0.9770955615653315052 ) ) ;
#56678 = ADVANCED_FACE ( 'NONE', ( #147325 ), #254290, .T. ) ;
#56679 = CARTESIAN_POINT ( 'NONE',  ( 20.95595624212409547, 10.62389120310530366, -175.1296329141266312 ) ) ;
#56681 = ORIENTED_EDGE ( 'NONE', *, *, #32420, .F. ) ;
#56680 = DIRECTION ( 'NONE',  ( 0.000000000000000000, -0.2128009952263603954, 0.9770955615653315052 ) ) ;
#56682 = CARTESIAN_POINT ( 'NONE',  ( 22.49999999999999645, 64.35023708198045256, -170.1119174609113713 ) ) ;
#56683 = CARTESIAN_POINT ( 'NONE',  ( 20.85000000000000142, 7.128833340094563376, -233.7327013124401276 ) ) ;
#56684 = CARTESIAN_POINT ( 'NONE',  ( 20.94999999999999929, -1.135018845910178431, -41.21697688343231647 ) ) ;
#56685 = ORIENTED_EDGE ( 'NONE', *, *, #25433, .F. ) ;
#56686 = DIRECTION ( 'NONE',  ( -1.000000000000000000, -2.952720810173289112E-16, 0.000000000000000000 ) ) ;
#56687 = FACE_OUTER_BOUND ( 'NONE', #239468, .T. ) ;
#56688 = DIRECTION ( 'NONE',  ( 0.000000000000000000, 0.000000000000000000, -1.000000000000000000 ) ) ;
#56689 = DIRECTION ( 'NONE',  ( -0.000000000000000000, 0.9126074666063771490, 0.4088369013363281623 ) ) ;
#56690 = EDGE_CURVE ( 'NONE', #160449, #62992, #10398, .T. ) ;
#56691 = CIRCLE ( 'NONE', #44271, 4.049999999999998046 ) ;
#56692 = VECTOR ( 'NONE', #131719, 1000.000000000000000 ) ;
#56693 = LINE ( 'NONE', #215786, #967 ) ;
#56694 = CARTESIAN_POINT ( 'NONE',  ( -16.87683809663752399, 66.15000000001157332, -56.12074346632808641 ) ) ;
#56695 = ORIENTED_EDGE ( 'NONE', *, *, #186012, .T. ) ;
#56696 = ORIENTED_EDGE ( 'NONE', *, *, #102169, .F. ) ;
#56698 = CARTESIAN_POINT ( 'NONE',  ( 21.53699400386439677, -1.444431824881390991, -194.3677569336561533 ) ) ;
#56697 = CIRCLE ( 'NONE', #90043, 1.899999999999996136 ) ;
#56699 = CARTESIAN_POINT ( 'NONE',  ( -22.50000000000000000, 31.89597452117651244, -238.9192857152811769 ) ) ;
#56700 = CYLINDRICAL_SURFACE ( 'NONE', #24634, 0.09999999999999939493 ) ;
#56701 = DIRECTION ( 'NONE',  ( 0.000000000000000000, 1.000000000000000000, 2.891205793294679805E-16 ) ) ;
#56702 = VERTEX_POINT ( 'NONE', #249017 ) ;
#56703 = DIRECTION ( 'NONE',  ( 0.000000000000000000, -0.9594490217226104845, -0.2818822000686205809 ) ) ;
#56704 = EDGE_CURVE ( 'NONE', #99187, #169705, #227201, .T. ) ;
#56705 = CARTESIAN_POINT ( 'NONE',  ( 20.59588692710267921, 11.75683769346106011, -206.2576375686336405 ) ) ;
#56706 = DIRECTION ( 'NONE',  ( 1.000000000000000000, 0.000000000000000000, 0.000000000000000000 ) ) ;
#56707 = EDGE_CURVE ( 'NONE', #151273, #59542, #243854, .T. ) ;
#56708 = DIRECTION ( 'NONE',  ( 0.000000000000000000, 0.000000000000000000, -1.000000000000000000 ) ) ;
#56709 = EDGE_LOOP ( 'NONE', ( #78093, #254427, #242639, #93009 ) ) ;
#56710 = DIRECTION ( 'NONE',  ( -1.000000000000000000, -0.000000000000000000, -0.000000000000000000 ) ) ;
#56711 = ADVANCED_FACE ( 'NONE', ( #11686 ), #87336, .F. ) ;
#56712 = ORIENTED_EDGE ( 'NONE', *, *, #23220, .F. ) ;
#56713 = ADVANCED_FACE ( 'NONE', ( #86035 ), #130317, .F. ) ;
#56714 = VERTEX_POINT ( 'NONE', #164340 ) ;
#56715 = FACE_OUTER_BOUND ( 'NONE', #145978, .T. ) ;
#56716 = LINE ( 'NONE', #77573, #6009 ) ;
#56717 = CYLINDRICAL_SURFACE ( 'NONE', #195576, 0.5000000000000004441 ) ;
#56718 = VERTEX_POINT ( 'NONE', #66514 ) ;
#56719 = FACE_OUTER_BOUND ( 'NONE', #85103, .T. ) ;
#56721 = ADVANCED_FACE ( 'NONE', ( #146034 ), #23224, .T. ) ;
#56720 = CARTESIAN_POINT ( 'NONE',  ( -20.94999999999999929, 67.23127455305835554, -235.8551265064784559 ) ) ;
#56722 = LINE ( 'NONE', #217094, #216268 ) ;
#56723 = ORIENTED_EDGE ( 'NONE', *, *, #244451, .F. ) ;
#56724 = CARTESIAN_POINT ( 'NONE',  ( -22.20000000000000284, 11.75000000000000000, 32.89999999999999858 ) ) ;
#56726 = EDGE_LOOP ( 'NONE', ( #156111, #22171, #6513, #90564, #164317 ) ) ;
#56725 = DIRECTION ( 'NONE',  ( -1.000000000000000000, 0.000000000000000000, 0.000000000000000000 ) ) ;
#56727 = CARTESIAN_POINT ( 'NONE',  ( 20.94999999999999574, 1.162701749949165642, -75.10000000000003695 ) ) ;
#56728 = CARTESIAN_POINT ( 'NONE',  ( -22.39999999999999858, 75.90000000001170122, -77.31388708289772183 ) ) ;
#56729 = VECTOR ( 'NONE', #229608, 1000.000000000000000 ) ;
#56730 = B_SPLINE_CURVE_WITH_KNOTS ( 'NONE', 3,
 ( #35775, #194852, #17467, #179145, #96964, #159560, #175298 ),
 .UNSPECIFIED., .F., .F.,
 ( 4, 3, 4 ),
 ( 0.000000000000000000, 1.860045280646151707E-05, 5.251155757305330614E-05 ),
 .UNSPECIFIED. ) ;
#56731 = AXIS2_PLACEMENT_3D ( 'NONE', #149430, #68596, #245951 ) ;
#56732 = CIRCLE ( 'NONE', #81856, 0.09999999999999918676 ) ;
#56733 = EDGE_CURVE ( 'NONE', #157687, #151159, #65218, .T. ) ;
#56734 = ADVANCED_FACE ( 'NONE', ( #15549 ), #96318, .F. ) ;
#56735 = ORIENTED_EDGE ( 'NONE', *, *, #23842, .F. ) ;
#56736 = CARTESIAN_POINT ( 'NONE',  ( -20.64999999999999858, 68.75000000001205080, -124.1731074845243370 ) ) ;
#56737 = DIRECTION ( 'NONE',  ( 0.000000000000000000, -7.086529944415894657E-15, 1.000000000000000000 ) ) ;
#56738 = VERTEX_POINT ( 'NONE', #54635 ) ;
#56739 = DIRECTION ( 'NONE',  ( 0.000000000000000000, -6.982962677686266711E-15, 1.000000000000000000 ) ) ;
#56740 = EDGE_CURVE ( 'NONE', #68386, #133700, #102267, .T. ) ;
#56741 = DIRECTION ( 'NONE',  ( 0.000000000000000000, 0.000000000000000000, 1.000000000000000000 ) ) ;
#56742 = CYLINDRICAL_SURFACE ( 'NONE', #188967, 0.09999999999999939493 ) ;
#56743 = ORIENTED_EDGE ( 'NONE', *, *, #183288, .F. ) ;
#56744 = CARTESIAN_POINT ( 'NONE',  ( 21.05000000000000071, 8.776282895303630482, -42.05862899514094977 ) ) ;
#56745 = VERTEX_POINT ( 'NONE', #194179 ) ;
#56746 = EDGE_CURVE ( 'NONE', #138742, #104053, #69013, .T. ) ;
#56747 = AXIS2_PLACEMENT_3D ( 'NONE', #33199, #213067, #249647 ) ;
#56748 = CIRCLE ( 'NONE', #115236, 11.75000000000000533 ) ;
#56749 = ADVANCED_FACE ( 'NONE', ( #117192 ), #18908, .T. ) ;
#56750 = EDGE_LOOP ( 'NONE', ( #169294, #252716, #10128 ) ) ;
#56751 = CIRCLE ( 'NONE', #152511, 0.09999999999999799327 ) ;
#56752 = CARTESIAN_POINT ( 'NONE',  ( 20.04142135623730070, 11.75000000000000355, -24.65000000000000213 ) ) ;
#56753 = CARTESIAN_POINT ( 'NONE',  ( -17.71734398241073549, 65.15764277154798378, -180.2979692315188345 ) ) ;
#56755 = ORIENTED_EDGE ( 'NONE', *, *, #719, .F. ) ;
#56754 = DIRECTION ( 'NONE',  ( 0.000000000000000000, 0.000000000000000000, 1.000000000000000000 ) ) ;
#56756 = ADVANCED_FACE ( 'NONE', ( #250281 ), #172064, .T. ) ;
#56757 = CARTESIAN_POINT ( 'NONE',  ( 18.54999999999999716, 8.750000000000024869, -9.250000000000001776 ) ) ;
#56759 = VECTOR ( 'NONE', #192480, 1000.000000000000114 ) ;
#56758 = FACE_OUTER_BOUND ( 'NONE', #13116, .T. ) ;
#56760 = DIRECTION ( 'NONE',  ( 2.952720810173289112E-16, 1.000000000000000000, 9.912705577010238578E-15 ) ) ;
#56761 = CIRCLE ( 'NONE', #102558, 7.720710678118663850 ) ;
#56762 = CARTESIAN_POINT ( 'NONE',  ( -23.25000000000000000, 78.47509609352879068, -238.9045489380306435 ) ) ;
#56763 = ADVANCED_FACE ( 'NONE', ( #135451 ), #233310, .F. ) ;
#56764 = CARTESIAN_POINT ( 'NONE',  ( 18.59999999999999787, -11.75000000000000000, 5.900000000000001243 ) ) ;
#56765 = DIRECTION ( 'NONE',  ( 1.000000000000000000, 0.000000000000000000, 0.000000000000000000 ) ) ;
#56766 = DIRECTION ( 'NONE',  ( 0.000000000000000000, -0.8496786552930224445, -0.5273008465187981608 ) ) ;
#56768 = VERTEX_POINT ( 'NONE', #255354 ) ;
#56767 = CARTESIAN_POINT ( 'NONE',  ( -22.94999999999999929, -1.212568896937008089, -8.000000000000000000 ) ) ;
#56769 = ORIENTED_EDGE ( 'NONE', *, *, #158034, .F. ) ;
#56771 = CARTESIAN_POINT ( 'NONE',  ( -16.87333278164162920, 51.20547199152485973, -232.2055066581121991 ) ) ;
#56770 = DIRECTION ( 'NONE',  ( -0.7070776581709311559, 4.937903618720164857E-15, -0.7071359030027479786 ) ) ;
#56773 = ORIENTED_EDGE ( 'NONE', *, *, #169361, .T. ) ;
#56772 = LINE ( 'NONE', #193755, #163592 ) ;
#56774 = ORIENTED_EDGE ( 'NONE', *, *, #176082, .T. ) ;
#56775 = DIRECTION ( 'NONE',  ( 3.265361837132813093E-16, 1.000000000000000000, 6.982962677686266711E-15 ) ) ;
#56776 = DIRECTION ( 'NONE',  ( 0.000000000000000000, 0.000000000000000000, -1.000000000000000000 ) ) ;
#56777 = AXIS2_PLACEMENT_3D ( 'NONE', #195159, #196403, #138968 ) ;
#56778 = CIRCLE ( 'NONE', #77634, 0.3999999999999926392 ) ;
#56779 = CIRCLE ( 'NONE', #40098, 0.1999999999999987899 ) ;
#56780 = CARTESIAN_POINT ( 'NONE',  ( -20.64999999999999858, 72.62993014539878800, -215.9492192728129965 ) ) ;
#56781 = CARTESIAN_POINT ( 'NONE',  ( -21.05000000000000071, 76.00000000001193712, -107.0231074845243029 ) ) ;
#56782 = ADVANCED_FACE ( 'NONE', ( #134172 ), #152493, .F. ) ;
#56783 = DIRECTION ( 'NONE',  ( 0.000000000000000000, -0.2128009952263603954, 0.9770955615653315052 ) ) ;
#56784 = AXIS2_PLACEMENT_3D ( 'NONE', #16492, #12644, #92155 ) ;
#56785 = DIRECTION ( 'NONE',  ( 0.000000000000000000, 0.9126074666063770380, 0.4088369013363282178 ) ) ;
#56786 = CARTESIAN_POINT ( 'NONE',  ( -16.92989507731676113, 66.05000000001201954, -115.9056085539141492 ) ) ;
#56787 = EDGE_CURVE ( 'NONE', #174960, #160821, #139701, .T. ) ;
#56788 = ORIENTED_EDGE ( 'NONE', *, *, #94184, .F. ) ;
#56789 = VERTEX_POINT ( 'NONE', #55899 ) ;
#56790 = CARTESIAN_POINT ( 'NONE',  ( 21.05000000000000071, 30.93396944080688016, -252.0807926308514766 ) ) ;
#56791 = AXIS2_PLACEMENT_3D ( 'NONE', #62058, #28084, #124598 ) ;
#56792 = VERTEX_POINT ( 'NONE', #35125 ) ;
#56793 = DIRECTION ( 'NONE',  ( 1.000000000000000000, 0.000000000000000000, -0.000000000000000000 ) ) ;
#56794 = LINE ( 'NONE', #18974, #72648 ) ;
#56795 = DIRECTION ( 'NONE',  ( 1.000000000000000000, 0.000000000000000000, 0.000000000000000000 ) ) ;
#56796 = CARTESIAN_POINT ( 'NONE',  ( -22.00356870069503046, -1.543709994182673739, -193.9119119858162037 ) ) ;
#56797 = EDGE_LOOP ( 'NONE', ( #202475, #87911, #44709, #129207, #68887 ) ) ;
#56798 = EDGE_CURVE ( 'NONE', #218130, #225579, #173087, .T. ) ;
#56799 = DIRECTION ( 'NONE',  ( -2.840903330521631775E-16, 0.8700118002898321601, -0.4930308989875230030 ) ) ;
#56800 = ORIENTED_EDGE ( 'NONE', *, *, #1645, .T. ) ;
#56801 = CARTESIAN_POINT ( 'NONE',  ( -17.27223548804936826, 10.34539739143179560, -89.13360617919259710 ) ) ;
#56802 = VERTEX_POINT ( 'NONE', #151189 ) ;
#56803 = AXIS2_PLACEMENT_3D ( 'NONE', #146941, #128695, #68713 ) ;
#56804 = FACE_OUTER_BOUND ( 'NONE', #155410, .T. ) ;
#56805 = AXIS2_PLACEMENT_3D ( 'NONE', #164207, #106773, #24715 ) ;
#56806 = CARTESIAN_POINT ( 'NONE',  ( -16.86379686415369861, 9.975217759264314310, -113.0666101109097497 ) ) ;
#56807 = AXIS2_PLACEMENT_3D ( 'NONE', #228564, #90306, #68195 ) ;
#56808 = TOROIDAL_SURFACE ( 'NONE', #227528, 12.97499999999999787, 0.1000000000000000056 ) ;
#56809 = ORIENTED_EDGE ( 'NONE', *, *, #152054, .F. ) ;
#56810 = DIRECTION ( 'NONE',  ( 0.000000000000000000, -0.5907332058517320572, 0.8068669527896995541 ) ) ;
#56812 = ORIENTED_EDGE ( 'NONE', *, *, #39483, .F. ) ;
#56811 = DIRECTION ( 'NONE',  ( 1.000000000000000000, -7.304098846218134667E-16, 0.000000000000000000 ) ) ;
#56813 = EDGE_CURVE ( 'NONE', #134685, #213031, #110683, .T. ) ;
#56814 = FACE_OUTER_BOUND ( 'NONE', #248820, .T. ) ;
#56815 = VERTEX_POINT ( 'NONE', #72961 ) ;
#56816 = CIRCLE ( 'NONE', #86039, 11.90000000000000391 ) ;
#56817 = ORIENTED_EDGE ( 'NONE', *, *, #44734, .F. ) ;
#56818 = CARTESIAN_POINT ( 'NONE',  ( 21.93340585898732442, -5.963111948670274387E-16, 7.324147022127360351 ) ) ;
#56819 = EDGE_LOOP ( 'NONE', ( #193390, #253903, #172400, #184265 ) ) ;
#56820 = CARTESIAN_POINT ( 'NONE',  ( 18.59999999999999076, 1.835341550235567887, -45.05515129256298223 ) ) ;
#56821 = CARTESIAN_POINT ( 'NONE',  ( 21.05000000000000071, 69.45934304831041572, -69.42310748452436542 ) ) ;
#56822 = AXIS2_PLACEMENT_3D ( 'NONE', #191044, #51471, #54064 ) ;
#56823 = LINE ( 'NONE', #136359, #53598 ) ;
#56824 = CARTESIAN_POINT ( 'NONE',  ( 18.50016250449482413, 67.49429988484645548, -195.5441618131978316 ) ) ;
#56825 = CIRCLE ( 'NONE', #227543, 0.1000000000000028644 ) ;
#56826 = DIRECTION ( 'NONE',  ( -1.000000000000000000, 0.000000000000000000, 0.000000000000000000 ) ) ;
#56827 = AXIS2_PLACEMENT_3D ( 'NONE', #105767, #185335, #124091 ) ;
#56828 = VERTEX_POINT ( 'NONE', #155064 ) ;
#56829 = DIRECTION ( 'NONE',  ( 1.000000000000000000, 0.000000000000000000, 0.000000000000000000 ) ) ;
#56830 = CARTESIAN_POINT ( 'NONE',  ( 20.94999999999999929, 60.06173988932782493, -221.3217724115915814 ) ) ;
#56831 = CARTESIAN_POINT ( 'NONE',  ( 18.58222699835054570, 10.33200063080772324, -139.5931674956643462 ) ) ;
#56832 = ORIENTED_EDGE ( 'NONE', *, *, #120629, .F. ) ;
#56833 = DIRECTION ( 'NONE',  ( 1.000000000000000000, 0.000000000000000000, 0.000000000000000000 ) ) ;
#56834 = VERTEX_POINT ( 'NONE', #53362 ) ;
#56835 = ORIENTED_EDGE ( 'NONE', *, *, #183317, .F. ) ;
#56836 = LINE ( 'NONE', #176844, #101720 ) ;
#56837 = DIRECTION ( 'NONE',  ( 0.7071067811865475727, -0.7071067811865475727, -4.937700262164531476E-15 ) ) ;
#56838 = CIRCLE ( 'NONE', #140061, 0.1000000000000013933 ) ;
#56840 = ORIENTED_EDGE ( 'NONE', *, *, #52932, .T. ) ;
#56839 = DIRECTION ( 'NONE',  ( 0.000000000000000000, 0.000000000000000000, 1.000000000000000000 ) ) ;
#56841 = DIRECTION ( 'NONE',  ( -0.000000000000000000, -0.2617529984165031243, -0.9651348961777157509 ) ) ;
#56842 = EDGE_LOOP ( 'NONE', ( #48545, #210768, #62987, #238345 ) ) ;
#56843 = DIRECTION ( 'NONE',  ( 0.000000000000000000, 0.000000000000000000, 1.000000000000000000 ) ) ;
#56844 = EDGE_CURVE ( 'NONE', #113969, #248271, #248050, .T. ) ;
#56845 = CARTESIAN_POINT ( 'NONE',  ( -21.65000000000000213, 9.775875410973588586, -211.8174516384118817 ) ) ;
#56846 = ORIENTED_EDGE ( 'NONE', *, *, #43507, .F. ) ;
#56847 = VERTEX_POINT ( 'NONE', #37675 ) ;
#56848 = CARTESIAN_POINT ( 'NONE',  ( -22.00411653889213071, 0.09903810579707936212, -126.7465571323596123 ) ) ;
#56849 = CARTESIAN_POINT ( 'NONE',  ( -21.05315837717337857, 11.75000001535411798, -194.1583560218909099 ) ) ;
#56850 = ORIENTED_EDGE ( 'NONE', *, *, #133450, .F. ) ;
#56851 = DIRECTION ( 'NONE',  ( 0.000000000000000000, 1.000000000000000000, 0.000000000000000000 ) ) ;
#56852 = VECTOR ( 'NONE', #95488, 1000.000000000000000 ) ;
#56853 = CIRCLE ( 'NONE', #190186, 11.75000000000001066 ) ;
#56854 = AXIS2_PLACEMENT_3D ( 'NONE', #121928, #64513, #46222 ) ;
#56855 = CIRCLE ( 'NONE', #165042, 0.5000000000000014433 ) ;
#56856 = ORIENTED_EDGE ( 'NONE', *, *, #38474, .F. ) ;
#56857 = CARTESIAN_POINT ( 'NONE',  ( -18.59999999999999787, 1.148907358139439339E-11, -201.0000000000015064 ) ) ;
#56858 = EDGE_CURVE ( 'NONE', #173723, #178019, #127253, .T. ) ;
#56859 = EDGE_CURVE ( 'NONE', #118769, #28763, #177170, .T. ) ;
#56861 = ORIENTED_EDGE ( 'NONE', *, *, #224395, .T. ) ;
#56860 = CARTESIAN_POINT ( 'NONE',  ( -20.64999999999999858, 4.350000000011156054, -155.2500000000000284 ) ) ;
#56862 = FACE_OUTER_BOUND ( 'NONE', #163376, .T. ) ;
#56863 = DIRECTION ( 'NONE',  ( 0.000000000000000000, -0.8814952561688430555, 0.4721928772777346239 ) ) ;
#56864 = CARTESIAN_POINT ( 'NONE',  ( -16.83199318825828428, 63.07236900629889220, -213.2508343276289793 ) ) ;
#56865 = AXIS2_PLACEMENT_3D ( 'NONE', #165086, #5995, #69859 ) ;
#56867 = CARTESIAN_POINT ( 'NONE',  ( -22.42253884134832020, 75.99806764887715360, -181.6727131818727798 ) ) ;
#56866 = DIRECTION ( 'NONE',  ( 0.000000000000000000, 0.2128009952263568982, -0.9770955615653323934 ) ) ;
#56868 = DIRECTION ( 'NONE',  ( 1.000000000000000000, 0.000000000000000000, 0.000000000000000000 ) ) ;
#56869 = LINE ( 'NONE', #179442, #190124 ) ;
#56870 = AXIS2_PLACEMENT_3D ( 'NONE', #144540, #222790, #1171 ) ;
#56871 = AXIS2_PLACEMENT_3D ( 'NONE', #143427, #164293, #80869 ) ;
#56872 = EDGE_CURVE ( 'NONE', #126698, #93991, #139881, .T. ) ;
#56873 = DIRECTION ( 'NONE',  ( -0.000000000000000000, -0.1618390714546045217, 0.9868171638914230437 ) ) ;
#56874 = CARTESIAN_POINT ( 'NONE',  ( 22.50927854361890113, -3.275978807471259913, -228.2735453177909335 ) ) ;
#56875 = ORIENTED_EDGE ( 'NONE', *, *, #86116, .T. ) ;
#56876 = ORIENTED_EDGE ( 'NONE', *, *, #217989, .T. ) ;
#56877 = EDGE_CURVE ( 'NONE', #30860, #207476, #231499, .T. ) ;
#56878 = CARTESIAN_POINT ( 'NONE',  ( 18.41356215285960829, 85.50000000001232081, -162.9910380878246485 ) ) ;
#56879 = AXIS2_PLACEMENT_3D ( 'NONE', #171972, #93672, #195367 ) ;
#56881 = ORIENTED_EDGE ( 'NONE', *, *, #107374, .F. ) ;
#56880 = CARTESIAN_POINT ( 'NONE',  ( -13.40000000000000213, -8.250000000000005329, 10.95857864376269042 ) ) ;
#56882 = VERTEX_POINT ( 'NONE', #239709 ) ;
#56883 = DIRECTION ( 'NONE',  ( 0.000000000000000000, 0.8660254037844384856, -0.5000000000000003331 ) ) ;
#56884 = ORIENTED_EDGE ( 'NONE', *, *, #212301, .F. ) ;
#56885 = DIRECTION ( 'NONE',  ( 1.000000000000000000, 0.000000000000000000, 0.000000000000000000 ) ) ;
#56886 = EDGE_CURVE ( 'NONE', #52785, #100962, #119066, .T. ) ;
#56887 = ORIENTED_EDGE ( 'NONE', *, *, #81238, .F. ) ;
#56888 = ADVANCED_FACE ( 'NONE', ( #238417 ), #169158, .T. ) ;
#56891 = VERTEX_POINT ( 'NONE', #161470 ) ;
#56890 = ORIENTED_EDGE ( 'NONE', *, *, #38774, .T. ) ;
#56889 = VECTOR ( 'NONE', #157683, 1000.000000000000000 ) ;
#56892 = ORIENTED_EDGE ( 'NONE', *, *, #32475, .F. ) ;
#56893 = EDGE_LOOP ( 'NONE', ( #101737, #51750, #57218, #158533 ) ) ;
#56894 = VERTEX_POINT ( 'NONE', #240992 ) ;
#56895 = CARTESIAN_POINT ( 'NONE',  ( 21.05000000000000071, 1.115600667400684642E-11, -204.9999999999999716 ) ) ;
#56896 = LINE ( 'NONE', #79031, #112951 ) ;
#56898 = ORIENTED_EDGE ( 'NONE', *, *, #235289, .T. ) ;
#56897 = CARTESIAN_POINT ( 'NONE',  ( -20.94999999999999929, 87.48912529308817909, -133.4231074845242233 ) ) ;
#56899 = CARTESIAN_POINT ( 'NONE',  ( 23.15000000000000213, 87.65000000001238334, -170.0231074845242745 ) ) ;
#56900 = CARTESIAN_POINT ( 'NONE',  ( 14.77516762759920610, 12.45018385075468181, -213.8211107588515461 ) ) ;
#56902 = VERTEX_POINT ( 'NONE', #119781 ) ;
#56901 = CARTESIAN_POINT ( 'NONE',  ( -21.14999999999999858, 1.627786319807485116, -244.0021210468063089 ) ) ;
#56903 = DIRECTION ( 'NONE',  ( 0.000000000000000000, 1.000000000000000000, 0.000000000000000000 ) ) ;
#56904 = ORIENTED_EDGE ( 'NONE', *, *, #108069, .F. ) ;
#56906 = CARTESIAN_POINT ( 'NONE',  ( -18.50000000000000000, 77.36242903720516040, -95.13422623660308375 ) ) ;
#56905 = AXIS2_PLACEMENT_3D ( 'NONE', #99326, #81051, #216727 ) ;
#56909 = ADVANCED_FACE ( 'NONE', ( #61054 ), #80597, .T. ) ;
#56908 = VERTEX_POINT ( 'NONE', #59749 ) ;
#56907 = DIRECTION ( 'NONE',  ( 0.000000000000000000, -0.5774316882803290918, -0.8164390028469542537 ) ) ;
#56910 = DIRECTION ( 'NONE',  ( -0.000000000000000000, -0.000000000000000000, 1.000000000000000000 ) ) ;
#56911 = CARTESIAN_POINT ( 'NONE',  ( -16.91049119928362998, 9.950000000011138823, -87.88172039319088924 ) ) ;
#56912 = CIRCLE ( 'NONE', #11163, 0.09999999999999671652 ) ;
#56913 = ORIENTED_EDGE ( 'NONE', *, *, #160261, .F. ) ;
#56915 = DIRECTION ( 'NONE',  ( 0.000000000000000000, 0.2128009952263603677, -0.9770955615653313941 ) ) ;
#56914 = CARTESIAN_POINT ( 'NONE',  ( -20.94999999999999929, 68.20313450767837082, -227.8297066677462794 ) ) ;
#56916 = CARTESIAN_POINT ( 'NONE',  ( 21.07928932188134397, 6.328516656404459262, -133.9011048543456184 ) ) ;
#56917 = AXIS2_PLACEMENT_3D ( 'NONE', #10439, #229487, #166977 ) ;
#56918 = AXIS2_PLACEMENT_3D ( 'NONE', #72331, #227524, #28080 ) ;
#56919 = DIRECTION ( 'NONE',  ( -3.469446951953635015E-14, -1.000000000000000000, 0.000000000000000000 ) ) ;
#56920 = DIRECTION ( 'NONE',  ( 1.000000000000000000, 0.000000000000000000, 0.000000000000000000 ) ) ;
#56921 = ORIENTED_EDGE ( 'NONE', *, *, #232590, .F. ) ;
#56922 = ORIENTED_EDGE ( 'NONE', *, *, #624, .F. ) ;
#56923 = EDGE_CURVE ( 'NONE', #67212, #224490, #202448, .T. ) ;
#56924 = CARTESIAN_POINT ( 'NONE',  ( -23.15000000000000213, 64.35000000001254250, -182.2731074845244450 ) ) ;
#56925 = LINE ( 'NONE', #97335, #244098 ) ;
#56926 = VERTEX_POINT ( 'NONE', #44072 ) ;
#56927 = ORIENTED_EDGE ( 'NONE', *, *, #105832, .T. ) ;
#56928 = DIRECTION ( 'NONE',  ( 0.000000000000000000, -1.000000000000000000, 0.000000000000000000 ) ) ;
#56929 = CARTESIAN_POINT ( 'NONE',  ( -22.47007471830799830, 76.00000000001244871, -177.7438181364508694 ) ) ;
#56930 = ORIENTED_EDGE ( 'NONE', *, *, #139206, .F. ) ;
#56931 = CARTESIAN_POINT ( 'NONE',  ( 18.79999999999999716, 5.586869315528661062, 16.41686199900910736 ) ) ;
#56933 = B_SPLINE_CURVE_WITH_KNOTS ( 'NONE', 3,
 ( #133680, #85863, #48047, #66341, #145857, #46756, #27244, #99659 ),
 .UNSPECIFIED., .F., .F.,
 ( 4, 2, 2, 4 ),
 ( 0.000000000000000000, 6.534141206311790389E-05, 0.0001306828241262358078, 0.0002613656482524339937 ),
 .UNSPECIFIED. ) ;
#56932 = SHAPE_REPRESENTATION_RELATIONSHIP ( 'NONE' , 'NONE' ,  #45219, #228621 ) ;
#56934 = ADVANCED_FACE ( 'NONE', ( #101420 ), #222683, .F. ) ;
#56935 = VECTOR ( 'NONE', #113801, 1000.000000000000000 ) ;
#56936 = EDGE_CURVE ( 'NONE', #157661, #248851, #131529, .T. ) ;
#56937 = EDGE_LOOP ( 'NONE', ( #145202, #179397 ) ) ;
#56938 = EDGE_LOOP ( 'NONE', ( #253881, #88453, #99022, #173525, #59059, #32923, #233563 ) ) ;
#56939 = VECTOR ( 'NONE', #255008, 1000.000000000000000 ) ;
#56940 = VERTEX_POINT ( 'NONE', #3647 ) ;
#56942 = LINE ( 'NONE', #233076, #200712 ) ;
#56941 = CIRCLE ( 'NONE', #140350, 0.09999999999999763245 ) ;
#56943 = CARTESIAN_POINT ( 'NONE',  ( -22.39999999999999858, 75.90000000001219860, -144.3138870828977076 ) ) ;
#56944 = CARTESIAN_POINT ( 'NONE',  ( -23.15000000000000213, 32.96286418198891255, -251.2069521516576174 ) ) ;
#56945 = DIRECTION ( 'NONE',  ( 0.000000000000000000, 0.8814952561688476074, -0.4721928772777262417 ) ) ;
#56946 = LINE ( 'NONE', #137784, #5228 ) ;
#56948 = EDGE_CURVE ( 'NONE', #95948, #131701, #98168, .T. ) ;
#56947 =( BOUNDED_CURVE ( )  B_SPLINE_CURVE ( 3, ( #248071, #46010, #27776, #26471 ),
 .UNSPECIFIED., .F., .F. ) 
 B_SPLINE_CURVE_WITH_KNOTS ( ( 4, 4 ),
 ( 4.937700262164173333E-15, 1.570796326794912323 ),
 .UNSPECIFIED. ) 
 CURVE ( )  GEOMETRIC_REPRESENTATION_ITEM ( )  RATIONAL_B_SPLINE_CURVE ( ( 1.000000000000000000, 0.8047378541243623840, 0.8047378541243623840, 1.000000000000000000 ) ) 
 REPRESENTATION_ITEM ( '' )  );
#56950 = DIRECTION ( 'NONE',  ( 1.000000000000000000, 0.000000000000000000, 0.000000000000000000 ) ) ;
#56949 = DIRECTION ( 'NONE',  ( 0.000000000000000000, -0.000000000000000000, 1.000000000000000000 ) ) ;
#56951 = CARTESIAN_POINT ( 'NONE',  ( 22.50000000000000000, 59.72530380783945247, -233.9230542583682393 ) ) ;
#56953 = VERTEX_POINT ( 'NONE', #1059 ) ;
#56952 = DIRECTION ( 'NONE',  ( 0.000000000000000000, 0.000000000000000000, -1.000000000000000000 ) ) ;
#56954 = CARTESIAN_POINT ( 'NONE',  ( -20.64999999999999858, 11.48697431424113446, -220.1440440112397994 ) ) ;
#56955 = VERTEX_POINT ( 'NONE', #58469 ) ;
#56956 = AXIS2_PLACEMENT_3D ( 'NONE', #86929, #189913, #243458 ) ;
#56957 = CARTESIAN_POINT ( 'NONE',  ( -18.59999999999999787, 11.75000000001115197, -155.7499999999999716 ) ) ;
#56958 = AXIS2_PLACEMENT_3D ( 'NONE', #39349, #159287, #176288 ) ;
#56959 = EDGE_LOOP ( 'NONE', ( #42411, #63999, #122757, #43107 ) ) ;
#56960 = ORIENTED_EDGE ( 'NONE', *, *, #213269, .T. ) ;
#56961 = DIRECTION ( 'NONE',  ( -0.000000000000000000, -0.8700118002898321601, 0.4930308989875230030 ) ) ;
#56962 = CARTESIAN_POINT ( 'NONE',  ( -20.94999999999999929, 76.00000000001126921, -203.5231074845248997 ) ) ;
#56964 = EDGE_CURVE ( 'NONE', #15255, #89874, #220796, .T. ) ;
#56963 = DIRECTION ( 'NONE',  ( 1.000000000000000000, 0.000000000000000000, 0.000000000000000000 ) ) ;
#56966 = EDGE_CURVE ( 'NONE', #254732, #80617, #90011, .T. ) ;
#56965 = VERTEX_POINT ( 'NONE', #42786 ) ;
#56967 = CARTESIAN_POINT ( 'NONE',  ( 20.95159278453404283, 8.907896337960206523, -75.48472018510929615 ) ) ;
#56968 = AXIS2_PLACEMENT_3D ( 'NONE', #4310, #104672, #61734 ) ;
#56969 = DIRECTION ( 'NONE',  ( -1.000000000000000000, 0.000000000000000000, -0.000000000000000000 ) ) ;
#56971 = ORIENTED_EDGE ( 'NONE', *, *, #61310, .T. ) ;
#56970 = AXIS2_PLACEMENT_3D ( 'NONE', #97022, #194908, #117902 ) ;
#56972 = VERTEX_POINT ( 'NONE', #182312 ) ;
#56973 = CIRCLE ( 'NONE', #90301, 4.000000000000003553 ) ;
#56974 = ADVANCED_FACE ( 'NONE', ( #19377 ), #178474, .F. ) ;
#56975 = CARTESIAN_POINT ( 'NONE',  ( -15.75000000000000355, 48.12247445990688988, -234.1702647910923361 ) ) ;
#56976 = VERTEX_POINT ( 'NONE', #2354 ) ;
#56977 = CARTESIAN_POINT ( 'NONE',  ( -16.93302609847409457, 60.87765233411752774, -221.0909021287161806 ) ) ;
#56978 = DIRECTION ( 'NONE',  ( 1.000000000000000000, 0.000000000000000000, 0.000000000000000000 ) ) ;
#56979 = EDGE_LOOP ( 'NONE', ( #58632, #214193, #179751 ) ) ;
#56980 = DIRECTION ( 'NONE',  ( 1.000000000000000000, 0.000000000000000000, 0.000000000000000000 ) ) ;
#56981 = CYLINDRICAL_SURFACE ( 'NONE', #88503, 0.1000000000000013933 ) ;
#56982 = ORIENTED_EDGE ( 'NONE', *, *, #244234, .F. ) ;
#56983 = SPHERICAL_SURFACE ( 'NONE', #212763, 0.1000000000000000056 ) ;
#56984 = DIRECTION ( 'NONE',  ( 0.000000000000000000, 1.000000000000000000, 0.000000000000000000 ) ) ;
#56985 = AXIS2_PLACEMENT_3D ( 'NONE', #151884, #9767, #89297 ) ;
#56986 = FACE_OUTER_BOUND ( 'NONE', #110739, .T. ) ;
#56987 = ORIENTED_EDGE ( 'NONE', *, *, #50623, .F. ) ;
#56988 = CARTESIAN_POINT ( 'NONE',  ( 20.95000000000005258, 65.19115966511134275, -30.02310748452479316 ) ) ;
#56989 = ORIENTED_EDGE ( 'NONE', *, *, #253131, .F. ) ;
#56990 = EDGE_CURVE ( 'NONE', #182741, #12734, #242256, .T. ) ;
#56991 = CARTESIAN_POINT ( 'NONE',  ( -23.25000000000000000, 1.115600667400684642E-11, -146.7750000000000057 ) ) ;
#56992 = ADVANCED_FACE ( 'NONE', ( #18080 ), #94105, .T. ) ;
#56993 = CARTESIAN_POINT ( 'NONE',  ( 12.25000000000000000, 12.70026017068886937, -215.3766613508543628 ) ) ;
#56994 = DIRECTION ( 'NONE',  ( 0.000000000000000000, 1.000000000000000000, 0.000000000000000000 ) ) ;
#56996 = VECTOR ( 'NONE', #3269, 1000.000000000000000 ) ;
#56995 = CARTESIAN_POINT ( 'NONE',  ( 21.13461538461538325, 67.11458296203814200, -191.1731074845244223 ) ) ;
#56997 = CARTESIAN_POINT ( 'NONE',  ( -23.15000000000000213, 35.97645343225767789, -235.9694016464868298 ) ) ;
#56998 = FACE_OUTER_BOUND ( 'NONE', #217008, .T. ) ;
#57000 = ORIENTED_EDGE ( 'NONE', *, *, #232314, .T. ) ;
#56999 = VECTOR ( 'NONE', #142793, 1000.000000000000000 ) ;
#57001 = DIRECTION ( 'NONE',  ( 0.000000000000000000, 0.000000000000000000, -1.000000000000000000 ) ) ;
#57002 = FACE_OUTER_BOUND ( 'NONE', #118403, .T. ) ;
#57003 = AXIS2_PLACEMENT_3D ( 'NONE', #161881, #82284, #103144 ) ;
#57004 = VECTOR ( 'NONE', #15310, 1000.000000000000000 ) ;
#57005 = DIRECTION ( 'NONE',  ( 1.000000000000000000, 0.000000000000000000, 0.000000000000000000 ) ) ;
#57006 = EDGE_CURVE ( 'NONE', #12588, #133509, #257925, .T. ) ;
#57007 = CARTESIAN_POINT ( 'NONE',  ( 20.30531438145591139, 65.90309893892023752, -61.72708967725128559 ) ) ;
#57008 = AXIS2_PLACEMENT_3D ( 'NONE', #40276, #237167, #37703 ) ;
#57009 = ORIENTED_EDGE ( 'NONE', *, *, #28596, .T. ) ;
#57010 = ORIENTED_EDGE ( 'NONE', *, *, #70581, .F. ) ;
#57011 = DIRECTION ( 'NONE',  ( 0.000000000000000000, 0.2617529984165152257, 0.9651348961777124202 ) ) ;
#57012 = CARTESIAN_POINT ( 'NONE',  ( -20.64999999999999858, 71.65000000001228386, -157.6731074845243938 ) ) ;
#57013 = LINE ( 'NONE', #158744, #160160 ) ;
#57014 = CARTESIAN_POINT ( 'NONE',  ( -20.64999999999999858, 68.70534379447684614, -223.0647885566232560 ) ) ;
#57015 = CARTESIAN_POINT ( 'NONE',  ( -18.59999999999999787, 9.250000000011157297, -155.2500000000000284 ) ) ;
#57016 = CIRCLE ( 'NONE', #202783, 0.1000000000000014488 ) ;
#57017 = ORIENTED_EDGE ( 'NONE', *, *, #160949, .T. ) ;
#57018 = DIRECTION ( 'NONE',  ( 1.000000000000000000, -0.000000000000000000, -0.000000000000000000 ) ) ;
#57019 = DIRECTION ( 'NONE',  ( -1.000000000000000000, -0.000000000000000000, 0.000000000000000000 ) ) ;
#57020 = AXIS2_PLACEMENT_3D ( 'NONE', #236006, #195631, #256800 ) ;
#57021 = ORIENTED_EDGE ( 'NONE', *, *, #205198, .T. ) ;
#57022 = CARTESIAN_POINT ( 'NONE',  ( 23.14999999999999858, 76.00000000001237765, -170.0231074845243597 ) ) ;
#57023 = PLANE ( 'NONE',  #199286 ) ;
#57024 = EDGE_CURVE ( 'NONE', #110447, #188240, #148278, .T. ) ;
#57025 = TOROIDAL_SURFACE ( 'NONE', #219535, 0.9750000000000019762, 0.1000000000000000056 ) ;
#57026 = ORIENTED_EDGE ( 'NONE', *, *, #13305, .F. ) ;
#57027 = ADVANCED_FACE ( 'NONE', ( #106584 ), #64902, .F. ) ;
#57028 = ORIENTED_EDGE ( 'NONE', *, *, #4631, .T. ) ;
#57029 = CARTESIAN_POINT ( 'NONE',  ( 19.97071067811864609, 64.27928932189311695, -78.27310748452438816 ) ) ;
#57030 = DIRECTION ( 'NONE',  ( -0.000000000000000000, 1.000000000000000000, -0.000000000000000000 ) ) ;
#57031 = DIRECTION ( 'NONE',  ( -1.000000000000000000, -0.000000000000000000, 0.000000000000000000 ) ) ;
#57032 = CARTESIAN_POINT ( 'NONE',  ( 21.05000000000000071, 5.500000000011153745, -121.5947339810869465 ) ) ;
#57033 = FACE_BOUND ( 'NONE', #152455, .T. ) ;
#57035 = EDGE_CURVE ( 'NONE', #207360, #18233, #8796, .T. ) ;
#57034 = CARTESIAN_POINT ( 'NONE',  ( 21.05000000000000071, 67.18454772081477699, -161.6027149319101568 ) ) ;
#57036 = CYLINDRICAL_SURFACE ( 'NONE', #49700, 0.09999999999999609201 ) ;
#57037 = DIRECTION ( 'NONE',  ( 0.000000000000000000, 1.000000000000000000, 0.000000000000000000 ) ) ;
#57038 = DIRECTION ( 'NONE',  ( 0.000000000000000000, -0.1335171055202901691, 0.9910465087640861759 ) ) ;
#57039 = CARTESIAN_POINT ( 'NONE',  ( 18.39999999999999858, -7.785976468740638090, -209.8926132507865816 ) ) ;
#57040 = EDGE_CURVE ( 'NONE', #157934, #104851, #45350, .T. ) ;
#57041 = CARTESIAN_POINT ( 'NONE',  ( 21.04105312098486635, 22.18722240147778280, -231.7305707818096323 ) ) ;
#57042 = CARTESIAN_POINT ( 'NONE',  ( 18.79999999999999716, 11.49641995933507843, 1.885425182446133441 ) ) ;
#57043 = CARTESIAN_POINT ( 'NONE',  ( 18.55121869061587958, 10.32747123227773400, -206.5774032850248716 ) ) ;
#57044 = CIRCLE ( 'NONE', #202815, 0.09999999999999817368 ) ;
#57045 = CIRCLE ( 'NONE', #86084, 11.74999999999999645 ) ;
#57046 = AXIS2_PLACEMENT_3D ( 'NONE', #173938, #176476, #14843 ) ;
#57047 = CIRCLE ( 'NONE', #90387, 0.1000000000000089567 ) ;
#57048 = CARTESIAN_POINT ( 'NONE',  ( 21.04116576186320486, 10.62466307876251115, -79.32858176862818311 ) ) ;
#57049 = CARTESIAN_POINT ( 'NONE',  ( 20.94999999999999929, 56.24810294282597312, -228.0242159533278823 ) ) ;
#57050 = EDGE_CURVE ( 'NONE', #179995, #21528, #144420, .T. ) ;
#57052 = EDGE_CURVE ( 'NONE', #137039, #65850, #6626, .T. ) ;
#57051 = EDGE_CURVE ( 'NONE', #95316, #86438, #110869, .T. ) ;
#57053 = ORIENTED_EDGE ( 'NONE', *, *, #132475, .T. ) ;
#57054 =( BOUNDED_SURFACE ( )  B_SPLINE_SURFACE ( 3, 2, ( 
 ( #92444, #117162, #97555 ),
 ( #156317, #256603, #233280 ),
 ( #54604, #177159, #213684 ),
 ( #72931, #128055, #78015 ),
 ( #172036, #132880, #16792 ),
 ( #114591, #255323, #55864 ),
 ( #157608, #135420, #211124 ),
 ( #112035, #113302, #14230 ) ),
 .UNSPECIFIED., .F., .F., .T. ) 
 B_SPLINE_SURFACE_WITH_KNOTS ( ( 4, 2, 2, 4 ),
 ( 3, 3 ),
 ( 0.0001704874539069910233, 0.0003809798300636651949, 0.0004862260181420022536, 0.0005914722062203393122 ),
 ( 0.000000000000000000, 1.000000000000000000 ),
 .UNSPECIFIED. ) 
 GEOMETRIC_REPRESENTATION_ITEM ( )  RATIONAL_B_SPLINE_SURFACE ( (
 ( 1.000000000000000000, 0.7071067811864942820, 1.000000000000000000),
 ( 1.000000000000000000, 0.7670648383577298723, 1.000000000000000000),
 ( 1.000000000000000000, 0.8204820770251111117, 1.000000000000000000),
 ( 1.000000000000000000, 0.8877218296114299800, 1.000000000000000000),
 ( 1.000000000000000000, 0.9080815932667398727, 1.000000000000000000),
 ( 1.000000000000000000, 0.9395541505860036668, 1.000000000000000000),
 ( 1.000000000000000000, 0.9506520335380280740, 1.000000000000000000),
 ( 1.000000000000000000, 0.9504532311154628710, 1.000000000000000000) ) ) 
 REPRESENTATION_ITEM ( '' )  SURFACE ( )  );
#57055 = CARTESIAN_POINT ( 'NONE',  ( 21.05000000000000071, 6.304516329264039598, -0.02110330805900034398 ) ) ;
#57056 = DIRECTION ( 'NONE',  ( -0.000000000000000000, 1.000000000000000000, 1.445602896647339410E-16 ) ) ;
#57057 = CARTESIAN_POINT ( 'NONE',  ( 23.15000000000000213, -11.74999999998883560, -63.89999999999999858 ) ) ;
#57058 = ORIENTED_EDGE ( 'NONE', *, *, #101597, .F. ) ;
#57059 = DIRECTION ( 'NONE',  ( -0.9880948137434723000, -0.1538461538461483591, -1.074301950413233512E-15 ) ) ;
#57060 = DIRECTION ( 'NONE',  ( -0.7071067811865456854, 0.3338907855510742650, 0.6233112732207634066 ) ) ;
#57061 = CIRCLE ( 'NONE', #235578, 0.1000000000000026146 ) ;
#57062 = ORIENTED_EDGE ( 'NONE', *, *, #112133, .F. ) ;
#57063 = FACE_OUTER_BOUND ( 'NONE', #75084, .T. ) ;
#57064 = DIRECTION ( 'NONE',  ( 0.000000000000000000, 0.4088369013363281623, -0.9126074666063771490 ) ) ;
#57065 = CIRCLE ( 'NONE', #89835, 11.64999999999998970 ) ;
#57066 = AXIS2_PLACEMENT_3D ( 'NONE', #177665, #18565, #257114 ) ;
#57067 = ORIENTED_EDGE ( 'NONE', *, *, #85243, .T. ) ;
#57068 = ADVANCED_FACE ( 'NONE', ( #148307 ), #204410, .T. ) ;
#57069 = EDGE_CURVE ( 'NONE', #209893, #110094, #235752, .T. ) ;
#57070 = AXIS2_PLACEMENT_3D ( 'NONE', #17660, #51634, #131197 ) ;
#57071 = ORIENTED_EDGE ( 'NONE', *, *, #254640, .F. ) ;
#57072 = DIRECTION ( 'NONE',  ( 0.000000000000000000, -0.4930308989874653269, -0.8700118002898649117 ) ) ;
#57073 = EDGE_CURVE ( 'NONE', #87114, #13008, #123335, .T. ) ;
#57074 = ORIENTED_EDGE ( 'NONE', *, *, #26488, .T. ) ;
#57075 = CARTESIAN_POINT ( 'NONE',  ( -23.25000000000000000, 1.115600667400684642E-11, -167.5000000000000284 ) ) ;
#57076 = CARTESIAN_POINT ( 'NONE',  ( 18.59999999999999076, 64.35000000001220144, -145.2731074845244450 ) ) ;
#57077 = CARTESIAN_POINT ( 'NONE',  ( 23.14999999999999858, 5.500000000011153745, -88.09473398108696074 ) ) ;
#57078 = DIRECTION ( 'NONE',  ( 1.000000000000000000, 0.000000000000000000, 0.000000000000000000 ) ) ;
#57079 = CARTESIAN_POINT ( 'NONE',  ( -20.54999999999999716, -9.499999999988846255, -124.1060308773475924 ) ) ;
#57080 = EDGE_CURVE ( 'NONE', #139128, #51091, #39972, .T. ) ;
#57081 = DIRECTION ( 'NONE',  ( -1.000000000000000000, 0.000000000000000000, 0.000000000000000000 ) ) ;
#57082 = DIRECTION ( 'NONE',  ( -1.073024830501117725E-15, -6.982962677686266711E-15, 1.000000000000000000 ) ) ;
#57083 = DIRECTION ( 'NONE',  ( 1.000000000000000000, 0.000000000000000000, 0.000000000000000000 ) ) ;
#57086 = ORIENTED_EDGE ( 'NONE', *, *, #72256, .F. ) ;
#57085 = EDGE_CURVE ( 'NONE', #94400, #61015, #156691, .T. ) ;
#57084 = CARTESIAN_POINT ( 'NONE',  ( 21.05000000000001492, 69.45934304831069994, -103.0231074845243597 ) ) ;
#57087 = VERTEX_POINT ( 'NONE', #29670 ) ;
#57089 = DIRECTION ( 'NONE',  ( -1.000000000000000000, 0.000000000000000000, -0.000000000000000000 ) ) ;
#57088 = DIRECTION ( 'NONE',  ( 0.000000000000000000, 1.000000000000000000, -6.308085367188393199E-16 ) ) ;
#57091 = EDGE_LOOP ( 'NONE', ( #215270, #136259, #102258, #166209 ) ) ;
#57090 = CARTESIAN_POINT ( 'NONE',  ( 23.24999999999999289, 69.55000000001260219, -191.1731074845243938 ) ) ;
#57092 = VECTOR ( 'NONE', #192001, 1000.000000000000114 ) ;
#57093 = EDGE_LOOP ( 'NONE', ( #23402, #108347, #71005, #13399 ) ) ;
#57094 = FACE_BOUND ( 'NONE', #224891, .T. ) ;
#57095 = CARTESIAN_POINT ( 'NONE',  ( 20.97217846901851956, 8.875441724720829484, -176.0012276839371737 ) ) ;
#57096 = DIRECTION ( 'NONE',  ( 0.000000000000000000, 1.000000000000000000, 0.000000000000000000 ) ) ;
#57097 = DIRECTION ( 'NONE',  ( 1.000000000000000000, 0.000000000000000000, -0.000000000000000000 ) ) ;
#57098 = DIRECTION ( 'NONE',  ( 1.000000000000000000, 3.265361837132813093E-16, -0.000000000000000000 ) ) ;
#57099 = EDGE_CURVE ( 'NONE', #31295, #12012, #165298, .T. ) ;
#57100 = DIRECTION ( 'NONE',  ( 1.000000000000000000, 0.000000000000000000, 0.000000000000000000 ) ) ;
#57101 = CARTESIAN_POINT ( 'NONE',  ( -18.79999999999999716, -2.462484827400500453, -15.77971343137458682 ) ) ;
#57103 = CIRCLE ( 'NONE', #102899, 0.1000000000000028644 ) ;
#57102 = DIRECTION ( 'NONE',  ( -3.265361837132813093E-16, 1.000000000000000000, 0.000000000000000000 ) ) ;
#57104 = EDGE_CURVE ( 'NONE', #176398, #202160, #73301, .T. ) ;
#57105 = VERTEX_POINT ( 'NONE', #187445 ) ;
#57106 = VERTEX_POINT ( 'NONE', #7504 ) ;
#57107 = DIRECTION ( 'NONE',  ( -0.000000000000000000, -6.982962677686266711E-15, 1.000000000000000000 ) ) ;
#57108 = VECTOR ( 'NONE', #56785, 1000.000000000000114 ) ;
#57109 = AXIS2_PLACEMENT_3D ( 'NONE', #123007, #184246, #120462 ) ;
#57110 = ORIENTED_EDGE ( 'NONE', *, *, #230723, .F. ) ;
#57111 = CARTESIAN_POINT ( 'NONE',  ( -22.50000000000000000, 76.00000000001195133, -103.0231074845243171 ) ) ;
#57112 = VERTEX_POINT ( 'NONE', #87016 ) ;
#57113 = CIRCLE ( 'NONE', #20684, 0.09999999999999739653 ) ;
#57114 = VECTOR ( 'NONE', #81898, 1000.000000000000000 ) ;
#57115 = CARTESIAN_POINT ( 'NONE',  ( -15.73854595235692244, 48.33210975535352105, -234.0748017065895681 ) ) ;
#57116 = CARTESIAN_POINT ( 'NONE',  ( -23.25000000000000355, 30.16539832223782369, -234.6716761914553899 ) ) ;
#57117 = EDGE_CURVE ( 'NONE', #167556, #11331, #206996, .T. ) ;
#57118 = AXIS2_PLACEMENT_3D ( 'NONE', #65990, #67272, #26897 ) ;
#57120 = ORIENTED_EDGE ( 'NONE', *, *, #9755, .F. ) ;
#57119 = CARTESIAN_POINT ( 'NONE',  ( -21.05000000000000071, 46.53760404070597900, -243.0973507280067167 ) ) ;
#57121 = CARTESIAN_POINT ( 'NONE',  ( -21.05000000000000071, -10.60885044396467336, -206.2784744251879090 ) ) ;
#57122 = ORIENTED_EDGE ( 'NONE', *, *, #253432, .T. ) ;
#57123 = CARTESIAN_POINT ( 'NONE',  ( -21.04999999999999716, 11.74999999999999645, -6.783865662978152855 ) ) ;
#57124 = DIRECTION ( 'NONE',  ( -1.000000000000000000, 0.000000000000000000, 0.000000000000000000 ) ) ;
#57125 = DIRECTION ( 'NONE',  ( -1.000000000000000000, -1.040834085586090568E-13, 0.000000000000000000 ) ) ;
#57126 = DIRECTION ( 'NONE',  ( -0.000000000000000000, 0.000000000000000000, 1.000000000000000000 ) ) ;
#57127 = DIRECTION ( 'NONE',  ( 1.000000000000000000, 0.000000000000000000, 0.000000000000000000 ) ) ;
#57128 = ORIENTED_EDGE ( 'NONE', *, *, #98543, .T. ) ;
#57129 = DIRECTION ( 'NONE',  ( 0.000000000000000000, 0.8814952561688416122, -0.4721928772777371219 ) ) ;
#57130 = CIRCLE ( 'NONE', #252778, 0.6000000000000015321 ) ;
#57131 = ORIENTED_EDGE ( 'NONE', *, *, #225381, .F. ) ;
#57134 = ORIENTED_EDGE ( 'NONE', *, *, #45744, .T. ) ;
#57133 = FACE_OUTER_BOUND ( 'NONE', #185787, .T. ) ;
#57132 = CARTESIAN_POINT ( 'NONE',  ( 23.14999999999998437, 4.050000000011155343, -100.5000000000000284 ) ) ;
#57135 = CARTESIAN_POINT ( 'NONE',  ( -21.30740335185486245, 0.09893452578700702438, -160.9433420779719768 ) ) ;
#57136 = CIRCLE ( 'NONE', #202899, 0.1000000000000090677 ) ;
#57137 = CIRCLE ( 'NONE', #44703, 0.1000000000000028644 ) ;
#57138 = CARTESIAN_POINT ( 'NONE',  ( -18.50000000000000000, 11.75000000001115197, -88.75000000000004263 ) ) ;
#57139 = EDGE_LOOP ( 'NONE', ( #101826, #119471, #215333, #247889 ) ) ;
#57140 = CARTESIAN_POINT ( 'NONE',  ( -23.15000000000000213, 11.65000000001115588, -160.4851942293460638 ) ) ;
#57141 = AXIS2_PLACEMENT_3D ( 'NONE', #26360, #245409, #109722 ) ;
#57142 = DIRECTION ( 'NONE',  ( 2.952720810173289112E-16, -0.9770955615653316162, -0.2128009952263604232 ) ) ;
#57143 = AXIS2_PLACEMENT_3D ( 'NONE', #18356, #138278, #70974 ) ;
#57144 = CARTESIAN_POINT ( 'NONE',  ( -16.91049119928364419, 9.949999999999983302, -12.61827960680916405 ) ) ;
#57145 = UNCERTAINTY_MEASURE_WITH_UNIT (LENGTH_MEASURE( 1.000000000000000082E-05 ), #185580, 'distance_accuracy_value', 'NONE');
#57146 = ORIENTED_EDGE ( 'NONE', *, *, #95023, .T. ) ;
#57147 = DIRECTION ( 'NONE',  ( 3.469446951953635015E-14, 6.982962677686266711E-15, -1.000000000000000000 ) ) ;
#57148 = ORIENTED_EDGE ( 'NONE', *, *, #32053, .T. ) ;
#57149 = DIRECTION ( 'NONE',  ( 0.000000000000000000, 0.000000000000000000, -1.000000000000000000 ) ) ;
#57150 = DIRECTION ( 'NONE',  ( -1.000000000000000000, -0.000000000000000000, -0.000000000000000000 ) ) ;
#57151 = CARTESIAN_POINT ( 'NONE',  ( 23.24999999999999645, 11.75000000001113953, -46.15000000000001279 ) ) ;
#57152 = TOROIDAL_SURFACE ( 'NONE', #123833, 0.2000000000000000111, 0.1000000000000000056 ) ;
#57153 = ORIENTED_EDGE ( 'NONE', *, *, #216228, .F. ) ;
#57154 = LINE ( 'NONE', #178444, #13478 ) ;
#57156 = ORIENTED_EDGE ( 'NONE', *, *, #122612, .F. ) ;
#57155 = VECTOR ( 'NONE', #113510, 1000.000000000000000 ) ;
#57158 = VECTOR ( 'NONE', #204521, 1000.000000000000227 ) ;
#57157 = CARTESIAN_POINT ( 'NONE',  ( -18.40000000000000213, 59.45845889640172288, -220.6830127366588101 ) ) ;
#57159 = DIRECTION ( 'NONE',  ( -1.000000000000000000, 0.000000000000000000, 0.000000000000000000 ) ) ;
#57160 = DIRECTION ( 'NONE',  ( 0.000000000000000000, 0.000000000000000000, 1.000000000000000000 ) ) ;
#57161 = ORIENTED_EDGE ( 'NONE', *, *, #121374, .F. ) ;
#57162 = DIRECTION ( 'NONE',  ( 0.000000000000000000, 0.000000000000000000, 1.000000000000000000 ) ) ;
#57163 = DIRECTION ( 'NONE',  ( 0.000000000000000000, 0.000000000000000000, 1.000000000000000000 ) ) ;
#57164 = VECTOR ( 'NONE', #168302, 1000.000000000000000 ) ;
#57165 = EDGE_CURVE ( 'NONE', #130365, #171995, #189974, .T. ) ;
#57166 = CARTESIAN_POINT ( 'NONE',  ( -23.15000000000000213, -6.388372595096676321, -212.0629706944429813 ) ) ;
#57167 = EDGE_LOOP ( 'NONE', ( #187514, #107209, #10683, #78764 ) ) ;
#57168 = CARTESIAN_POINT ( 'NONE',  ( -20.00857864376270001, 9.150000000011157653, -121.6500000000000341 ) ) ;
#57169 = LINE ( 'NONE', #216256, #164998 ) ;
#57170 = PLANE ( 'NONE',  #227906 ) ;
#57171 = VERTEX_POINT ( 'NONE', #169182 ) ;
#57172 = PLANE ( 'NONE',  #191606 ) ;
#57173 = ORIENTED_EDGE ( 'NONE', *, *, #73873, .T. ) ;
#57175 = ORIENTED_EDGE ( 'NONE', *, *, #9110, .T. ) ;
#57174 = FACE_OUTER_BOUND ( 'NONE', #34433, .T. ) ;
#57176 = EDGE_CURVE ( 'NONE', #108484, #52356, #219002, .T. ) ;
#57177 = AXIS2_PLACEMENT_3D ( 'NONE', #225852, #169812, #145060 ) ;
#57178 = EDGE_CURVE ( 'NONE', #106961, #161837, #252312, .T. ) ;
#57179 = AXIS2_PLACEMENT_3D ( 'NONE', #39608, #193523, #176533 ) ;
#57182 = ORIENTED_EDGE ( 'NONE', *, *, #137398, .T. ) ;
#57181 = ORIENTED_EDGE ( 'NONE', *, *, #135379, .F. ) ;
#57180 = DIRECTION ( 'NONE',  ( -1.000000000000000000, -0.000000000000000000, -0.000000000000000000 ) ) ;
#57183 = DIRECTION ( 'NONE',  ( 0.000000000000000000, -0.6855225566104692358, -0.7280513885559494192 ) ) ;
#57184 = CIRCLE ( 'NONE', #74004, 0.09999999999999939493 ) ;
#57185 = CARTESIAN_POINT ( 'NONE',  ( -20.94999999999999929, 65.70729864260954400, -30.56574559737245877 ) ) ;
#57186 = CIRCLE ( 'NONE', #123868, 0.1000000000000013933 ) ;
#57187 = DIRECTION ( 'NONE',  ( 0.000000000000000000, 0.000000000000000000, -1.000000000000000000 ) ) ;
#57188 = CARTESIAN_POINT ( 'NONE',  ( 20.84999999999998721, 46.46967969402478360, -243.0849751855955674 ) ) ;
#57189 = CARTESIAN_POINT ( 'NONE',  ( 21.14261333020286671, 10.71569264926606202, -112.7500000000002558 ) ) ;
#57190 = LINE ( 'NONE', #96322, #122444 ) ;
#57191 = CIRCLE ( 'NONE', #227914, 0.09999999999999895084 ) ;
#57192 = CARTESIAN_POINT ( 'NONE',  ( -18.34374000495060386, 11.47316190337362585, -143.2500000000000284 ) ) ;
#57193 = ORIENTED_EDGE ( 'NONE', *, *, #197179, .T. ) ;
#57194 = ORIENTED_EDGE ( 'NONE', *, *, #82121, .T. ) ;
#57195 = VERTEX_POINT ( 'NONE', #53046 ) ;
#57196 = ADVANCED_FACE ( 'NONE', ( #156028 ), #73932, .F. ) ;
#57197 = DIRECTION ( 'NONE',  ( 1.000000000000000000, 0.000000000000000000, 0.000000000000000000 ) ) ;
#57200 = VERTEX_POINT ( 'NONE', #90890 ) ;
#57199 = EDGE_CURVE ( 'NONE', #31018, #64899, #77512, .T. ) ;
#57198 = LINE ( 'NONE', #59763, #3670 ) ;
#57201 = CARTESIAN_POINT ( 'NONE',  ( -16.87036670365549895, 60.86740053880574663, -221.1564527318009254 ) ) ;
#57202 = ORIENTED_EDGE ( 'NONE', *, *, #182328, .T. ) ;
#57203 = DIRECTION ( 'NONE',  ( 2.952720810173289112E-16, -1.000000000000000000, -0.000000000000000000 ) ) ;
#57204 = ORIENTED_EDGE ( 'NONE', *, *, #193127, .T. ) ;
#57205 = CARTESIAN_POINT ( 'NONE',  ( 20.84999999999998721, -4.352039508298082282, -236.2331130063498676 ) ) ;
#57206 = EDGE_CURVE ( 'NONE', #25862, #74935, #144152, .T. ) ;
#57207 = AXIS2_PLACEMENT_3D ( 'NONE', #197852, #195324, #19225 ) ;
#57208 = ORIENTED_EDGE ( 'NONE', *, *, #152927, .T. ) ;
#57209 = ADVANCED_FACE ( 'NONE', ( #114306 ), #110453, .F. ) ;
#57210 = DIRECTION ( 'NONE',  ( -0.000000000000000000, -6.982962677686266711E-15, 1.000000000000000000 ) ) ;
#57211 = CARTESIAN_POINT ( 'NONE',  ( -18.59999999999999787, -1.835341550213255957, -179.0551512925629538 ) ) ;
#57212 = AXIS2_PLACEMENT_3D ( 'NONE', #18617, #28935, #48437 ) ;
#57214 = ORIENTED_EDGE ( 'NONE', *, *, #173074, .F. ) ;
#57213 = EDGE_LOOP ( 'NONE', ( #236800, #194544, #49479, #117201 ) ) ;
#57215 = EDGE_LOOP ( 'NONE', ( #159577, #22699, #87044 ) ) ;
#57216 = DIRECTION ( 'NONE',  ( 1.000000000000000000, 0.000000000000000000, 0.000000000000000000 ) ) ;
#57218 = ORIENTED_EDGE ( 'NONE', *, *, #53591, .F. ) ;
#57217 = EDGE_CURVE ( 'NONE', #101654, #1640, #247454, .T. ) ;
#57219 = EDGE_LOOP ( 'NONE', ( #161484, #158274, #60469, #74424 ) ) ;
#57220 = CARTESIAN_POINT ( 'NONE',  ( 18.50000000000000000, 85.50000000001173817, -81.27310748452426026 ) ) ;
#57222 = ORIENTED_EDGE ( 'NONE', *, *, #65527, .T. ) ;
#57221 = DIRECTION ( 'NONE',  ( 0.000000000000000000, 0.9126074666063771490, 0.4088369013363281623 ) ) ;
#57224 = DIRECTION ( 'NONE',  ( 1.000000000000000000, 0.000000000000000000, 0.000000000000000000 ) ) ;
#57223 = DIRECTION ( 'NONE',  ( 1.000000000000000000, 0.000000000000000000, 0.000000000000000000 ) ) ;
#57225 = CARTESIAN_POINT ( 'NONE',  ( -21.44999999999999929, 68.75000000001158185, -57.17310748452437252 ) ) ;
#57226 = CARTESIAN_POINT ( 'NONE',  ( -18.40000000000000213, 11.48667500176882328, -42.75000000000000000 ) ) ;
#57227 = DIRECTION ( 'NONE',  ( -1.000000000000000000, -0.000000000000000000, -0.000000000000000000 ) ) ;
#57229 = ORIENTED_EDGE ( 'NONE', *, *, #53851, .T. ) ;
#57228 = B_SPLINE_CURVE_WITH_KNOTS ( 'NONE', 3,
 ( #226772, #127690, #26024, #207232 ),
 .UNSPECIFIED., .F., .F.,
 ( 4, 4 ),
 ( 0.000000000000000000, 0.001767853679387128589 ),
 .UNSPECIFIED. ) ;
#57231 = EDGE_CURVE ( 'NONE', #100350, #94397, #98342, .T. ) ;
#57230 = ORIENTED_EDGE ( 'NONE', *, *, #154202, .F. ) ;
#57232 = DIRECTION ( 'NONE',  ( 0.000000000000000000, 0.000000000000000000, -1.000000000000000000 ) ) ;
#57233 = DIRECTION ( 'NONE',  ( 0.000000000000000000, 1.000000000000000000, 6.982962677686266711E-15 ) ) ;
#57234 = CYLINDRICAL_SURFACE ( 'NONE', #12314, 0.1000000000000024342 ) ;
#57235 = ORIENTED_EDGE ( 'NONE', *, *, #178725, .F. ) ;
#57236 = CIRCLE ( 'NONE', #52963, 0.2000000000000057288 ) ;
#57237 = AXIS2_PLACEMENT_3D ( 'NONE', #46725, #164133, #125007 ) ;
#57238 = PLANE ( 'NONE',  #65501 ) ;
#57239 = B_SPLINE_CURVE_WITH_KNOTS ( 'NONE', 3,
 ( #193816, #16476, #219771, #58118, #75170, #235488, #215914, #95970, #195118, #17713, #116837, #97224, #15184, #154710, #175551, #55535, #254992, #76408, #137658 ),
 .UNSPECIFIED., .F., .F.,
 ( 4, 3, 3, 3, 3, 3, 4 ),
 ( 0.000000000000000000, 1.655171619026035414E-05, 2.773500582848695921E-05, 5.941817267378355548E-05, 0.0001114174635873587483, 0.0001914169455916365928, 0.0002627181070750677803 ),
 .UNSPECIFIED. ) ;
#57240 = VECTOR ( 'NONE', #93885, 1000.000000000000000 ) ;
#57241 = DIRECTION ( 'NONE',  ( 0.000000000000000000, 1.224646799142015331E-16, 1.000000000000000000 ) ) ;
#57242 = DIRECTION ( 'NONE',  ( -1.000000000000000000, 0.000000000000000000, -0.000000000000000000 ) ) ;
#57243 = VERTEX_POINT ( 'NONE', #94739 ) ;
#57244 = VERTEX_POINT ( 'NONE', #191316 ) ;
#57245 = CARTESIAN_POINT ( 'NONE',  ( -21.05000000000000071, 1.162701749949165642, -108.5000000000000426 ) ) ;
#57246 = CARTESIAN_POINT ( 'NONE',  ( 18.59999999999999787, 76.00000000001213607, -136.5231074845242745 ) ) ;
#57247 = VERTEX_POINT ( 'NONE', #174336 ) ;
#57248 = DIRECTION ( 'NONE',  ( 0.000000000000000000, 0.9770955615653313941, 0.2128009952263603677 ) ) ;
#57249 = ORIENTED_EDGE ( 'NONE', *, *, #161959, .T. ) ;
#57250 = CARTESIAN_POINT ( 'NONE',  ( -23.15000000000000213, 2.600000000011154278, -187.7753780772378889 ) ) ;
#57251 = CARTESIAN_POINT ( 'NONE',  ( -23.25000000000000000, 11.75000000000000000, 0.000000000000000000 ) ) ;
#57253 = CARTESIAN_POINT ( 'NONE',  ( -20.88420186297724612, 68.10670728244119232, -224.1434476749765565 ) ) ;
#57252 = DIRECTION ( 'NONE',  ( 0.000000000000000000, 0.9908441862701791170, -0.1350103645450472789 ) ) ;
#57254 = CARTESIAN_POINT ( 'NONE',  ( -20.94999999999999929, -11.48912529306490349, -137.1000000000000227 ) ) ;
#57255 = DIRECTION ( 'NONE',  ( 1.000000000000000000, -2.849773892568378313E-16, 7.728835255496647986E-17 ) ) ;
#57256 = AXIS2_PLACEMENT_3D ( 'NONE', #108150, #67733, #243801 ) ;
#57257 = AXIS2_PLACEMENT_3D ( 'NONE', #162289, #44896, #222215 ) ;
#57258 = CARTESIAN_POINT ( 'NONE',  ( -19.89999999999999858, 4.513204987021263825, 22.00000000000000355 ) ) ;
#57259 = ADVANCED_FACE ( 'NONE', ( #55579 ), #54321, .T. ) ;
#57261 = ORIENTED_EDGE ( 'NONE', *, *, #147704, .F. ) ;
#57260 = VERTEX_POINT ( 'NONE', #76455 ) ;
#57262 = CIRCLE ( 'NONE', #90586, 0.09999999999999982514 ) ;
#57263 = VERTEX_POINT ( 'NONE', #133868 ) ;
#57264 = FACE_OUTER_BOUND ( 'NONE', #177900, .T. ) ;
#57265 = CARTESIAN_POINT ( 'NONE',  ( -20.54999999999999716, 68.75000000001260503, -191.2731074845244166 ) ) ;
#57266 = DIRECTION ( 'NONE',  ( -1.000000000000000000, -0.000000000000000000, -0.000000000000000000 ) ) ;
#57267 = DIRECTION ( 'NONE',  ( 1.000000000000000000, 0.000000000000000000, 0.000000000000000000 ) ) ;
#57268 = EDGE_CURVE ( 'NONE', #242867, #97885, #212141, .T. ) ;
#57269 = EDGE_CURVE ( 'NONE', #108506, #99810, #123520, .T. ) ;
#57271 = DIRECTION ( 'NONE',  ( 0.000000000000000000, 0.2558827019434435912, -0.9667078373770033872 ) ) ;
#57270 = CARTESIAN_POINT ( 'NONE',  ( 20.74625933824092172, 8.882913521084280006, -8.555171024121042578 ) ) ;
#57272 = CARTESIAN_POINT ( 'NONE',  ( 22.39999999999999503, 65.19201463318205469, -243.3742797652979277 ) ) ;
#57273 = ORIENTED_EDGE ( 'NONE', *, *, #6371, .F. ) ;
#57274 = CARTESIAN_POINT ( 'NONE',  ( 23.15000000000000213, -11.65000000000000036, 3.469446951953614189E-15 ) ) ;
#57275 = ORIENTED_EDGE ( 'NONE', *, *, #65245, .F. ) ;
#57276 = ORIENTED_EDGE ( 'NONE', *, *, #131840, .T. ) ;
#57277 = CARTESIAN_POINT ( 'NONE',  ( -21.05000000000000071, 69.74218538953013535, -69.62089777583359762 ) ) ;
#57278 = DIRECTION ( 'NONE',  ( 0.000000000000000000, 0.000000000000000000, 1.000000000000000000 ) ) ;
#57280 = EDGE_CURVE ( 'NONE', #223147, #216520, #90179, .T. ) ;
#57279 = DIRECTION ( 'NONE',  ( 0.000000000000000000, 1.000000000000000000, 0.000000000000000000 ) ) ;
#57281 = EDGE_CURVE ( 'NONE', #83518, #92740, #22621, .T. ) ;
#57282 = CARTESIAN_POINT ( 'NONE',  ( 20.94999999999999574, 10.47338541492405994, -175.0786544642485012 ) ) ;
#57283 = EDGE_CURVE ( 'NONE', #11139, #209575, #85885, .T. ) ;
#57284 = CIRCLE ( 'NONE', #207343, 0.5000000000000004441 ) ;
#57285 = EDGE_CURVE ( 'NONE', #64016, #201514, #73489, .T. ) ;
#57286 = AXIS2_PLACEMENT_3D ( 'NONE', #197642, #138920, #99802 ) ;
#57287 = CARTESIAN_POINT ( 'NONE',  ( 22.59999954896768770, -0.008828232232978959135, -155.7494913259319844 ) ) ;
#57288 = ORIENTED_EDGE ( 'NONE', *, *, #123444, .F. ) ;
#57289 = ORIENTED_EDGE ( 'NONE', *, *, #156021, .T. ) ;
#57290 = EDGE_CURVE ( 'NONE', #168032, #187034, #119252, .T. ) ;
#57291 = DIRECTION ( 'NONE',  ( 0.000000000000000000, 0.2617529984165031243, 0.9651348961777157509 ) ) ;
#57292 = VERTEX_POINT ( 'NONE', #59428 ) ;
#57293 = CARTESIAN_POINT ( 'NONE',  ( -17.11825945287482753, 23.02528674727019364, -230.8469138855057281 ) ) ;
#57294 = VECTOR ( 'NONE', #115405, 1000.000000000000000 ) ;
#57295 = CARTESIAN_POINT ( 'NONE',  ( 20.85000000000000142, -1.835859311432481045, -212.5044391687984842 ) ) ;
#57296 = CARTESIAN_POINT ( 'NONE',  ( -20.54999999999999716, 2.000000000011154189, -120.7753780772379315 ) ) ;
#57297 = FACE_OUTER_BOUND ( 'NONE', #134683, .T. ) ;
#57299 = LINE ( 'NONE', #37783, #187266 ) ;
#57298 = CARTESIAN_POINT ( 'NONE',  ( -22.49917693094574389, 0.08522996422167167241, 11.64979578453066367 ) ) ;
#57300 = DIRECTION ( 'NONE',  ( 0.000000000000000000, 0.000000000000000000, 1.000000000000000000 ) ) ;
#57301 = VECTOR ( 'NONE', #88821, 1000.000000000000000 ) ;
#57302 = DIRECTION ( 'NONE',  ( 1.000000000000000000, 0.000000000000000000, 0.000000000000000000 ) ) ;
#57303 = CARTESIAN_POINT ( 'NONE',  ( -22.48660254037843131, 11.65000000001115588, -133.9500000000000455 ) ) ;
#57304 = DIRECTION ( 'NONE',  ( 0.000000000000000000, 0.8814952561688476074, -0.4721928772777262417 ) ) ;
#57305 = AXIS2_PLACEMENT_3D ( 'NONE', #166227, #248295, #149218 ) ;
#57307 = VERTEX_POINT ( 'NONE', #176875 ) ;
#57306 = CARTESIAN_POINT ( 'NONE',  ( 18.69999999999999929, 1.250000000000000000, 16.60000000000000142 ) ) ;
#57308 = VECTOR ( 'NONE', #137593, 1000.000000000000000 ) ;
#57309 = EDGE_CURVE ( 'NONE', #67356, #85130, #19284, .T. ) ;
#57310 = AXIS2_PLACEMENT_3D ( 'NONE', #124300, #159572, #99559 ) ;
#57311 = LINE ( 'NONE', #78165, #3767 ) ;
#57312 = AXIS2_PLACEMENT_3D ( 'NONE', #129795, #234027, #192346 ) ;
#57313 = ORIENTED_EDGE ( 'NONE', *, *, #196851, .T. ) ;
#57314 = EDGE_CURVE ( 'NONE', #48905, #82676, #31958, .T. ) ;
#57315 = EDGE_CURVE ( 'NONE', #146245, #46505, #148470, .T. ) ;
#57316 = DIRECTION ( 'NONE',  ( 1.000000000000000000, 0.000000000000000000, 0.000000000000000000 ) ) ;
#57317 = CARTESIAN_POINT ( 'NONE',  ( 23.14999999999999858, 68.05808644172607558, -213.7045301755741491 ) ) ;
#57318 = EDGE_LOOP ( 'NONE', ( #18609, #88398, #233558, #147293 ) ) ;
#57319 = DIRECTION ( 'NONE',  ( 0.000000000000000000, 0.1350103645451974088, -0.9908441862701587999 ) ) ;
#57320 = CARTESIAN_POINT ( 'NONE',  ( 15.07585980824113925, 9.417632963117448242, -85.14894846573231746 ) ) ;
#57321 = DIRECTION ( 'NONE',  ( -2.578261006436900068E-14, 0.1350103645451904977, -0.9908441862701597991 ) ) ;
#57322 = CIRCLE ( 'NONE', #11573, 2.000000000000001776 ) ;
#57323 = DIRECTION ( 'NONE',  ( 0.000000000000000000, -1.000000000000000000, -6.982962677686266711E-15 ) ) ;
#57324 = FACE_OUTER_BOUND ( 'NONE', #10407, .T. ) ;
#57325 = CARTESIAN_POINT ( 'NONE',  ( 20.94999999999999929, 65.27628289530447603, -115.2731074845243739 ) ) ;
#57326 = CIRCLE ( 'NONE', #90647, 0.1000000000000106498 ) ;
#57327 = VERTEX_POINT ( 'NONE', #3325 ) ;
#57328 = DIRECTION ( 'NONE',  ( 0.000000000000000000, -0.2128009952263403282, 0.9770955615653358350 ) ) ;
#57331 = ORIENTED_EDGE ( 'NONE', *, *, #186388, .F. ) ;
#57330 = CARTESIAN_POINT ( 'NONE',  ( 18.39999999999998082, 20.70020979027691510, -227.9869476361872103 ) ) ;
#57329 = VECTOR ( 'NONE', #219093, 1000.000000000000000 ) ;
#57332 = CYLINDRICAL_SURFACE ( 'NONE', #167498, 0.09999999999998898659 ) ;
#57333 = CARTESIAN_POINT ( 'NONE',  ( 21.08489834409762054, 23.03108543700951216, -230.2007552241209680 ) ) ;
#57334 = AXIS2_PLACEMENT_3D ( 'NONE', #209508, #225202, #8752 ) ;
#57335 = FACE_OUTER_BOUND ( 'NONE', #109251, .T. ) ;
#57336 = ORIENTED_EDGE ( 'NONE', *, *, #160720, .T. ) ;
#57337 = FACE_OUTER_BOUND ( 'NONE', #49845, .T. ) ;
#57338 = PRODUCT_CONTEXT ( 'NONE', #12422, 'mechanical' ) ;
#57339 = DIRECTION ( 'NONE',  ( 0.7071067811865462405, 0.6824534298470383842, -0.1850873201762212872 ) ) ;
#57340 = CARTESIAN_POINT ( 'NONE',  ( -18.58693740092120805, 85.40643215026499036, -95.89829102802303851 ) ) ;
#57341 = ORIENTED_EDGE ( 'NONE', *, *, #4620, .T. ) ;
#57342 = DIRECTION ( 'NONE',  ( -1.000000000000000000, 0.000000000000000000, 0.000000000000000000 ) ) ;
#57343 = LINE ( 'NONE', #113485, #117487 ) ;
#57344 = CIRCLE ( 'NONE', #99029, 1.999999999999997335 ) ;
#57345 = AXIS2_PLACEMENT_3D ( 'NONE', #138678, #171785, #150901 ) ;
#57346 = AXIS2_PLACEMENT_3D ( 'NONE', #204211, #245923, #105076 ) ;
#57347 = DIRECTION ( 'NONE',  ( 0.000000000000000000, 0.000000000000000000, -1.000000000000000000 ) ) ;
#57348 = EDGE_LOOP ( 'NONE', ( #134459, #253713, #20717, #228497 ) ) ;
#57349 = ORIENTED_EDGE ( 'NONE', *, *, #145479, .T. ) ;
#57350 = DIRECTION ( 'NONE',  ( 0.000000000000000000, 0.000000000000000000, -1.000000000000000000 ) ) ;
#57351 = DIRECTION ( 'NONE',  ( 1.000000000000000000, 0.000000000000000000, 0.000000000000000000 ) ) ;
#57352 = DIRECTION ( 'NONE',  ( 1.000000000000000000, -0.000000000000000000, -0.000000000000000000 ) ) ;
#57354 = AXIS2_PLACEMENT_3D ( 'NONE', #26187, #147407, #9179 ) ;
#57353 = CARTESIAN_POINT ( 'NONE',  ( 18.39999999999999858, 85.50000000001209344, -129.6084491415546154 ) ) ;
#57355 = EDGE_CURVE ( 'NONE', #152046, #107540, #219182, .T. ) ;
#57356 = CARTESIAN_POINT ( 'NONE',  ( -23.25000000000000000, 77.83585931145570669, -124.9186683157258244 ) ) ;
#57357 = AXIS2_PLACEMENT_3D ( 'NONE', #57254, #172138, #138083 ) ;
#57359 = CARTESIAN_POINT ( 'NONE',  ( -20.00857864376270001, 9.150000000011157653, -179.7499999999999716 ) ) ;
#57358 = DIRECTION ( 'NONE',  ( 1.000000000000000000, 0.000000000000000000, 0.000000000000000000 ) ) ;
#57360 = DIRECTION ( 'NONE',  ( 0.000000000000000000, 0.4599910535713788717, -0.8879235499941945386 ) ) ;
#57361 = ADVANCED_FACE ( 'NONE', ( #17754 ), #169351, .T. ) ;
#57362 = CIRCLE ( 'NONE', #207247, 0.1000000000000028644 ) ;
#57363 = CARTESIAN_POINT ( 'NONE',  ( 20.94999999999999929, 77.83534155023701828, -191.9679561919613491 ) ) ;
#57364 = DIRECTION ( 'NONE',  ( 0.000000000000000000, 0.000000000000000000, 1.000000000000000000 ) ) ;
#57365 = CARTESIAN_POINT ( 'NONE',  ( -18.59999999999999787, 9.350000000011156942, -121.6500000000000341 ) ) ;
#57366 = ORIENTED_EDGE ( 'NONE', *, *, #177505, .T. ) ;
#57367 = ORIENTED_EDGE ( 'NONE', *, *, #247528, .T. ) ;
#57368 = DIRECTION ( 'NONE',  ( 0.000000000000000000, -0.9908441862701610203, 0.1350103645451807555 ) ) ;
#57369 = DIRECTION ( 'NONE',  ( -1.000000000000000000, 0.000000000000000000, 0.000000000000000000 ) ) ;
#57371 = SPHERICAL_SURFACE ( 'NONE', #57782, 0.1000000000000000056 ) ;
#57370 = CARTESIAN_POINT ( 'NONE',  ( 21.08035267497491105, 69.66829316022864305, -69.60579610930049910 ) ) ;
#57372 = AXIS2_PLACEMENT_3D ( 'NONE', #177855, #120464, #57864 ) ;
#57373 = EDGE_CURVE ( 'NONE', #217175, #55402, #190168, .T. ) ;
#57374 = EDGE_CURVE ( 'NONE', #53868, #42338, #223457, .T. ) ;
#57375 = LINE ( 'NONE', #233489, #231057 ) ;
#57376 = DIRECTION ( 'NONE',  ( 0.000000000000000000, 0.000000000000000000, 1.000000000000000000 ) ) ;
#57377 = CARTESIAN_POINT ( 'NONE',  ( -23.25000000000000000, 11.65000000001115588, -67.00000000000004263 ) ) ;
#57378 = VERTEX_POINT ( 'NONE', #39935 ) ;
#57379 = CIRCLE ( 'NONE', #203130, 0.09999999999999990841 ) ;
#57380 = VERTEX_POINT ( 'NONE', #137701 ) ;
#57381 = AXIS2_PLACEMENT_3D ( 'NONE', #119566, #183379, #240783 ) ;
#57382 = TOROIDAL_SURFACE ( 'NONE', #203137, 7.800000000000000711, 0.1000000000000000056 ) ;
#57383 = CARTESIAN_POINT ( 'NONE',  ( -21.05000000000000071, 64.37928932189323916, -96.15469083218333424 ) ) ;
#57384 = CIRCLE ( 'NONE', #7505, 11.75000000000000000 ) ;
#57385 = ORIENTED_EDGE ( 'NONE', *, *, #195818, .T. ) ;
#57386 = DIRECTION ( 'NONE',  ( 1.000000000000000000, -0.000000000000000000, -0.000000000000000000 ) ) ;
#57387 = AXIS2_PLACEMENT_3D ( 'NONE', #5913, #224959, #62067 ) ;
#57388 = EDGE_CURVE ( 'NONE', #50778, #135659, #140842, .T. ) ;
#57389 = EDGE_CURVE ( 'NONE', #131644, #81419, #206715, .T. ) ;
#57390 = CARTESIAN_POINT ( 'NONE',  ( 18.39999999999999858, 85.68240343348776378, -29.36626410711146207 ) ) ;
#57391 = VERTEX_POINT ( 'NONE', #81564 ) ;
#57392 = CARTESIAN_POINT ( 'NONE',  ( -20.54999999999999716, 68.85000000001254250, -182.3731074845244109 ) ) ;
#57393 = ORIENTED_EDGE ( 'NONE', *, *, #23845, .T. ) ;
#57394 = CARTESIAN_POINT ( 'NONE',  ( 18.59999999999999787, -11.74999999998883737, -155.3500000000000227 ) ) ;
#57395 = DIRECTION ( 'NONE',  ( 0.000000000000000000, 0.1350103645451876666, -0.9908441862701600211 ) ) ;
#57397 = CIRCLE ( 'NONE', #178053, 0.3999999999999975797 ) ;
#57396 = DIRECTION ( 'NONE',  ( 1.000000000000000000, -2.952720810173289112E-16, -2.061873921506763405E-30 ) ) ;
#57398 = DIRECTION ( 'NONE',  ( -1.020425574104003999E-15, 0.8814952561688430555, -0.4721928772777346239 ) ) ;
#57399 = CARTESIAN_POINT ( 'NONE',  ( 21.05000000000000071, 65.61575147395463148, -242.1939180743342774 ) ) ;
#57400 = EDGE_CURVE ( 'NONE', #116784, #79014, #181785, .T. ) ;
#57402 = DIRECTION ( 'NONE',  ( 0.000000000000000000, -0.4930308989875324399, -0.8700118002898268310 ) ) ;
#57401 = DIRECTION ( 'NONE',  ( 7.304098846218135653E-16, -0.9770955615653315052, -0.2128009952263603954 ) ) ;
#57403 = FACE_OUTER_BOUND ( 'NONE', #86454, .T. ) ;
#57405 = EDGE_LOOP ( 'NONE', ( #181267, #115335, #209461, #70136 ) ) ;
#57404 = EDGE_CURVE ( 'NONE', #88284, #39258, #42467, .T. ) ;
#57407 = DIRECTION ( 'NONE',  ( 0.000000000000000000, 0.9126074666063770380, 0.4088369013363281068 ) ) ;
#57406 = CARTESIAN_POINT ( 'NONE',  ( -18.39999999999999858, 37.95493834378066111, -261.2294694241335264 ) ) ;
#57408 = EDGE_LOOP ( 'NONE', ( #249292, #201026, #218870, #246694, #13302, #213857, #45734, #74082, #224916, #179729, #57349, #223633, #124118, #36085, #69944, #90191, #9122, #115714, #178445, #236465, #209402, #74686, #40595, #238656, #78378, #136754, #230305, #24226, #137248 ) ) ;
#57410 = VERTEX_POINT ( 'NONE', #22941 ) ;
#57409 = DIRECTION ( 'NONE',  ( -1.000000000000000000, 0.000000000000000000, 0.000000000000000000 ) ) ;
#57411 = CIRCLE ( 'NONE', #236303, 0.09999999999999470424 ) ;
#57412 = VERTEX_POINT ( 'NONE', #215957 ) ;
#57413 = CARTESIAN_POINT ( 'NONE',  ( 20.94999999999997442, 74.95904887477786360, -233.7774272632847783 ) ) ;
#57414 = CARTESIAN_POINT ( 'NONE',  ( 21.14999999999999503, 11.65000000001116298, -67.00000000000004263 ) ) ;
#57415 = LINE ( 'NONE', #196935, #126627 ) ;
#57416 = LINE ( 'NONE', #113558, #171026 ) ;
#57417 = ORIENTED_EDGE ( 'NONE', *, *, #112714, .T. ) ;
#57418 = DIRECTION ( 'NONE',  ( -0.000000000000000000, 0.9651348961777155289, -0.2617529984165036794 ) ) ;
#57419 =( LENGTH_UNIT ( ) NAMED_UNIT ( * ) SI_UNIT ( .MILLI., .METRE. ) );
#57420 = FACE_OUTER_BOUND ( 'NONE', #138198, .T. ) ;
#57421 = EDGE_CURVE ( 'NONE', #106155, #96682, #44424, .T. ) ;
#57422 = VERTEX_POINT ( 'NONE', #9761 ) ;
#57423 = EDGE_CURVE ( 'NONE', #155438, #161400, #102637, .T. ) ;
#57424 = DIRECTION ( 'NONE',  ( 0.000000000000000000, -7.056502275159890832E-15, 1.000000000000000000 ) ) ;
#57425 = CARTESIAN_POINT ( 'NONE',  ( -18.50000000000000000, 78.48087866980282001, -232.8271061603568910 ) ) ;
#57426 = EDGE_CURVE ( 'NONE', #200563, #70381, #183274, .T. ) ;
#57427 = VECTOR ( 'NONE', #93601, 1000.000000000000114 ) ;
#57428 = ORIENTED_EDGE ( 'NONE', *, *, #117544, .T. ) ;
#57430 = ORIENTED_EDGE ( 'NONE', *, *, #188916, .T. ) ;
#57429 = AXIS2_PLACEMENT_3D ( 'NONE', #42277, #142630, #81359 ) ;
#57431 = CYLINDRICAL_SURFACE ( 'NONE', #39683, 0.09999999999999939493 ) ;
#57432 = VECTOR ( 'NONE', #4723, 1000.000000000000000 ) ;
#57433 = ORIENTED_EDGE ( 'NONE', *, *, #96116, .F. ) ;
#57434 = CARTESIAN_POINT ( 'NONE',  ( 21.14999999999999858, 64.35000000001258513, -191.3731074845244393 ) ) ;
#57435 = ORIENTED_EDGE ( 'NONE', *, *, #189707, .T. ) ;
#57436 = DIRECTION ( 'NONE',  ( 0.000000000000000000, 0.000000000000000000, -1.000000000000000000 ) ) ;
#57437 = LINE ( 'NONE', #134399, #123091 ) ;
#57438 = DIRECTION ( 'NONE',  ( -4.801466763864313332E-15, -0.2605042016806672911, -0.9654727137038716656 ) ) ;
#57439 = ADVANCED_FACE ( 'NONE', ( #106275 ), #79130, .T. ) ;
#57440 = DIRECTION ( 'NONE',  ( 0.000000000000000000, 1.000000000000000000, 0.000000000000000000 ) ) ;
#57441 = B_SPLINE_CURVE_WITH_KNOTS ( 'NONE', 3,
 ( #185356, #249191, #211343, #32743, #49695, #152682, #110954 ),
 .UNSPECIFIED., .F., .F.,
 ( 4, 3, 4 ),
 ( 0.000000000000000000, 3.357501770814691602E-05, 5.199112466349472097E-05 ),
 .UNSPECIFIED. ) ;
#57442 = EDGE_CURVE ( 'NONE', #97847, #76842, #23605, .T. ) ;
#57443 = AXIS2_PLACEMENT_3D ( 'NONE', #63558, #145661, #222618 ) ;
#57445 = CIRCLE ( 'NONE', #199117, 0.09999999999999939493 ) ;
#57444 = DIRECTION ( 'NONE',  ( -1.000000000000000000, 0.000000000000000000, 0.000000000000000000 ) ) ;
#57446 = LINE ( 'NONE', #99134, #144566 ) ;
#57447 = CARTESIAN_POINT ( 'NONE',  ( 20.84999999999999787, 56.11297552314564285, -227.9607914937811017 ) ) ;
#57448 = ORIENTED_EDGE ( 'NONE', *, *, #56258, .F. ) ;
#57450 = CARTESIAN_POINT ( 'NONE',  ( -22.16821283564876666, 7.558973340791935058, -33.50000000000000000 ) ) ;
#57449 = LINE ( 'NONE', #54880, #203943 ) ;
#57451 = ORIENTED_EDGE ( 'NONE', *, *, #10764, .T. ) ;
#57454 = ORIENTED_EDGE ( 'NONE', *, *, #194739, .T. ) ;
#57453 = DIRECTION ( 'NONE',  ( -1.000000000000000000, -0.000000000000000000, 0.000000000000000000 ) ) ;
#57452 = DIRECTION ( 'NONE',  ( -1.000000000000000000, 0.000000000000000000, 0.000000000000000000 ) ) ;
#57455 = ORIENTED_EDGE ( 'NONE', *, *, #149586, .F. ) ;
#57456 = VECTOR ( 'NONE', #132956, 1000.000000000000000 ) ;
#57457 = DIRECTION ( 'NONE',  ( 0.000000000000000000, 0.000000000000000000, 1.000000000000000000 ) ) ;
#57458 = CARTESIAN_POINT ( 'NONE',  ( 21.05000000000000071, -0.02138556592644301479, -60.69503888731549068 ) ) ;
#57459 = LINE ( 'NONE', #138274, #211046 ) ;
#57460 = CARTESIAN_POINT ( 'NONE',  ( -16.87372386987899020, 9.880600233647912845, -113.6492698718664514 ) ) ;
#57461 = VERTEX_POINT ( 'NONE', #125848 ) ;
#57462 = CARTESIAN_POINT ( 'NONE',  ( 20.95224633520496127, 67.09947783345539563, -195.0298310366031558 ) ) ;
#57463 = DIRECTION ( 'NONE',  ( 1.000000000000000000, 0.000000000000000000, 0.000000000000000000 ) ) ;
#57465 = CARTESIAN_POINT ( 'NONE',  ( 20.95545211741311320, 10.58641331154394472, -7.586146859588289715 ) ) ;
#57464 = CARTESIAN_POINT ( 'NONE',  ( -21.05000000000000071, 77.16270174994961906, -61.42310748452431568 ) ) ;
#57467 = VERTEX_POINT ( 'NONE', #185834 ) ;
#57466 = DIRECTION ( 'NONE',  ( 0.000000000000000000, -0.1480365673253065395, 0.9889818879709274535 ) ) ;
#57468 = EDGE_LOOP ( 'NONE', ( #190805, #42456, #161203, #105145 ) ) ;
#57469 = CIRCLE ( 'NONE', #74271, 11.80000000000000071 ) ;
#57470 = CARTESIAN_POINT ( 'NONE',  ( 20.95561247346651967, 11.96829920165036043, -206.1652233253646216 ) ) ;
#57471 = DIRECTION ( 'NONE',  ( 1.000000000000000000, 0.000000000000000000, 0.000000000000000000 ) ) ;
#57472 = ORIENTED_EDGE ( 'NONE', *, *, #200961, .T. ) ;
#57473 = DIRECTION ( 'NONE',  ( 0.000000000000000000, 0.9770955615653316162, 0.2128009952263604232 ) ) ;
#57474 = ORIENTED_EDGE ( 'NONE', *, *, #113779, .F. ) ;
#57475 = DIRECTION ( 'NONE',  ( -1.000000000000000000, 0.000000000000000000, 0.000000000000000000 ) ) ;
#57476 = CARTESIAN_POINT ( 'NONE',  ( 21.56666275994539816, 30.30957806568256885, -252.3955916421750203 ) ) ;
#57477 = FACE_OUTER_BOUND ( 'NONE', #224965, .T. ) ;
#57478 = TOROIDAL_SURFACE ( 'NONE', #74282, 0.4000000000000010214, 0.1000000000000000056 ) ;
#57479 = ORIENTED_EDGE ( 'NONE', *, *, #13001, .T. ) ;
#57480 = DIRECTION ( 'NONE',  ( 0.000000000000000000, -0.2617529984164955192, -0.9651348961777178603 ) ) ;
#57481 = ADVANCED_FACE ( 'NONE', ( #187146 ), #123305, .F. ) ;
#57482 = AXIS2_PLACEMENT_3D ( 'NONE', #203731, #244126, #204987 ) ;
#57483 = CIRCLE ( 'NONE', #74111, 0.09999999999999939493 ) ;
#57484 = LINE ( 'NONE', #99173, #48108 ) ;
#57485 = AXIS2_PLACEMENT_3D ( 'NONE', #256204, #75108, #154643 ) ;
#57486 = ORIENTED_EDGE ( 'NONE', *, *, #222303, .F. ) ;
#57487 = ORIENTED_EDGE ( 'NONE', *, *, #241067, .T. ) ;
#57489 = CARTESIAN_POINT ( 'NONE',  ( -16.97683810757273193, 44.69543639514680677, -235.0480788047526914 ) ) ;
#57488 = VECTOR ( 'NONE', #240189, 1000.000000000000000 ) ;
#57490 = ORIENTED_EDGE ( 'NONE', *, *, #137902, .T. ) ;
#57492 = ADVANCED_FACE ( 'NONE', ( #107574 ), #243229, .F. ) ;
#57491 = VERTEX_POINT ( 'NONE', #86708 ) ;
#57494 = ORIENTED_EDGE ( 'NONE', *, *, #34455, .F. ) ;
#57493 = LINE ( 'NONE', #134460, #17814 ) ;
#57495 = ORIENTED_EDGE ( 'NONE', *, *, #42989, .T. ) ;
#57496 = EDGE_CURVE ( 'NONE', #204227, #129114, #67177, .T. ) ;
#57497 = CYLINDRICAL_SURFACE ( 'NONE', #14317, 12.87499999999999822 ) ;
#57498 = EDGE_CURVE ( 'NONE', #101051, #238500, #211009, .T. ) ;
#57501 = ORIENTED_EDGE ( 'NONE', *, *, #170186, .F. ) ;
#57500 = ORIENTED_EDGE ( 'NONE', *, *, #182195, .F. ) ;
#57499 = DIRECTION ( 'NONE',  ( -0.000000000000000000, 1.000000000000000000, -1.224646799147352961E-16 ) ) ;
#57503 = ORIENTED_EDGE ( 'NONE', *, *, #37358, .T. ) ;
#57502 = AXIS2_PLACEMENT_3D ( 'NONE', #133418, #124750, #34343 ) ;
#57504 = CARTESIAN_POINT ( 'NONE',  ( -18.59999999999999787, 61.38756220455727686, -221.6813469827248184 ) ) ;
#57505 = AXIS2_PLACEMENT_3D ( 'NONE', #42162, #139942, #121707 ) ;
#57506 = CYLINDRICAL_SURFACE ( 'NONE', #172192, 0.09999999999999939493 ) ;
#57507 = CIRCLE ( 'NONE', #120107, 0.1000000000000028644 ) ;
#57508 = CARTESIAN_POINT ( 'NONE',  ( -16.89155683852576217, 14.02549623409718471, -218.6420703064984821 ) ) ;
#57509 = EDGE_LOOP ( 'NONE', ( #13300, #219566 ) ) ;
#57510 = VECTOR ( 'NONE', #77993, 1000.000000000000000 ) ;
#57511 = ADVANCED_FACE ( 'NONE', ( #45042 ), #68468, .F. ) ;
#57512 = CARTESIAN_POINT ( 'NONE',  ( -16.94132844910802760, 9.992436755191501874, -154.8962017559823323 ) ) ;
#57514 = VERTEX_POINT ( 'NONE', #245818 ) ;
#57513 = FACE_OUTER_BOUND ( 'NONE', #170441, .T. ) ;
#57515 = CARTESIAN_POINT ( 'NONE',  ( -20.64999999999999858, 71.65000000001222702, -148.8731074845244109 ) ) ;
#57517 = VERTEX_POINT ( 'NONE', #7180 ) ;
#57516 = CARTESIAN_POINT ( 'NONE',  ( -23.15000000000000213, 76.00000000001237765, -170.0231074845243597 ) ) ;
#57518 = AXIS2_PLACEMENT_3D ( 'NONE', #253330, #156840, #214223 ) ;
#57519 = EDGE_LOOP ( 'NONE', ( #55812, #239740, #196543, #31020, #90900 ) ) ;
#57520 = LINE ( 'NONE', #155393, #157197 ) ;
#57521 = CARTESIAN_POINT ( 'NONE',  ( 18.59999999999996945, 18.41524492703432614, -237.0006385043383546 ) ) ;
#57522 = EDGE_LOOP ( 'NONE', ( #88828, #49566, #43617, #129288 ) ) ;
#57523 = EDGE_LOOP ( 'NONE', ( #196108, #130298, #104611, #207614 ) ) ;
#57524 = CARTESIAN_POINT ( 'NONE',  ( -16.94180778212363592, 9.992443055743303049, -180.1041835705331948 ) ) ;
#57525 = CYLINDRICAL_SURFACE ( 'NONE', #152935, 0.09999999999999939493 ) ;
#57526 = VECTOR ( 'NONE', #8111, 1000.000000000000000 ) ;
#57527 = AXIS2_PLACEMENT_3D ( 'NONE', #142631, #107369, #145207 ) ;
#57529 = ORIENTED_EDGE ( 'NONE', *, *, #56634, .T. ) ;
#57528 = ORIENTED_EDGE ( 'NONE', *, *, #221459, .T. ) ;
#57531 = ORIENTED_EDGE ( 'NONE', *, *, #239703, .T. ) ;
#57530 = CLOSED_SHELL ( 'NONE', ( #29935, #33391, #105727, #99563, #235712, #248815, #175774, #48181, #17199, #68512, #52585, #188533, #45610, #120662, #73512, #60017, #18704, #232403, #108749, #150100, #67771, #27669, #130238, #159018, #234690, #227478, #253767, #192839, #88051, #208931, #252134, #222385, #135111, #89385, #136859, #113049, #125881, #218149, #41777, #197119, #127993, #33017, #69073, #240685, #8982, #122495, #248275, #146505, #47889, #248332, #183656, #48347, #221663, #471, #61495, #39424, #105591, #105135, #252456, #61095, #182136, #148828, #166582, #215958, #200470, #74081, #186372, #183342, #257066, #61161, #222687, #116860, #173382, #201884, #177015, #133339, #145999, #248142, #83216, #168104, #105597, #159208, #250722, #39203, #122258, #237983, #97967, #112604, #9528, #120051, #200121, #116865, #224528, #48445, #185079, #226709, #72700, #53825, #183633, #231391, #253287, #218334, #172727, #202737, #20991, #244700, #24687, #1154, #237938, #191266, #199510, #189687, #119095, #103886, #46033, #205112, #98, #117117, #201089, #158576, #51739, #107164, #240267, #177101, #241924, #8755, #228628, #131853, #4868, #203436, #26368, #234011, #110641, #199343, #177695, #242982, #9962, #190281, #143567, #54048, #220893, #196858, #171351, #109506, #44742, #81979, #58349, #58236, #245344, #187134, #24722, #32096, #158492, #41646, #35307, #243081, #231317, #174291, #22583, #68094, #197756, #218532, #230331, #132517, #213015, #31204, #128301, #56417, #65552, #57743, #88459, #124364, #71566, #161568, #154996, #240469, #153320, #202892, #208835, #208424, #227392, #233849, #70278, #100137, #79206, #25609, #65023, #65997, #76221, #250571, #58848, #239777, #82083, #230481, #86522, #8751, #155257, #236136, #225124, #75228, #158286, #71959, #149543, #160842, #191948, #146817, #79656, #248986, #192996, #206910, #119155, #122586, #42641, #181520, #255945, #249587, #5155, #7952, #17792, #81071, #51219, #253983, #7870, #139983, #243326, #39694, #147806, #53850, #34118, #6580, #208112, #78287, #99969, #149045, #122978, #172792, #180211, #249209, #20110, #190962, #30542, #202294, #176324, #35673, #209371, #89478, #87708, #151149, #208569, #221932, #164633, #80455, #226593, #79921, #151688, #201252, #170194, #207980, #41080, #191041, #175021, #72608, #138518, #230962, #11172, #211224, #227840, #189801, #38697, #104774, #70232, #95254, #130988, #7293, #86908, #86152, #63581, #140974, #26602, #236854, #180519, #205095, #6923, #192396, #65080, #37974, #176560, #199650, #106420, #83013, #144077, #29057, #143565, #117939, #125567, #12785, #23562, #150063, #191627, #78092, #189317, #20667, #60611, #92761, #120452, #130279, #116724, #98776, #170842, #106578, #222607, #171548, #33902, #126228, #257389, #19003, #254723, #74629, #121517, #189592, #127650, #126476, #117121, #235372, #156597, #244900, #42799, #73236, #186588, #128057, #15262, #182823, #211250, #235078, #43992, #234044, #167553, #96813, #73157, #12645, #7976, #194656, #161668, #30773, #75701, #20550, #234553, #187485, #1172, #188546, #62667, #76050, #161621, #97775, #77014, #61148, #44740, #1372, #192210, #99693, #127823, #148747, #189477, #167644, #30069, #119228, #62943, #167253, #79752, #253346, #158248, #43651, #131578, #242553, #185895, #192222, #107724, #86153, #98531, #219517, #167687, #189805, #115581, #168762, #110299, #175718, #131657, #170717, #135808, #147755, #244542, #179390, #200416, #28498, #245063, #99839, #74405, #48629, #109674, #252711, #82230, #19097, #162122, #44606, #47474, #240970, #248658, #105722, #99170, #92605, #174418, #4084, #228391, #185913, #108008, #104708, #190323, #20786, #230426, #202780, #93648, #109940, #163129, #21786, #224271, #31122, #231315, #51653, #136380, #246598, #78813, #118286, #186564, #157429, #119242, #122033, #240106, #44769, #41059, #200790, #132037, #214601, #1732, #176994, #87821, #39014, #43181, #128852, #27652, #177908, #46516, #15177, #21448, #141579, #82306, #7353, #84256, #228581, #191534, #231408, #188588, #14275, #27499, #156003, #50400, #37546, #159258, #28809, #247523, #156651, #164921, #79279, #168897, #62950, #117375, #101333, #48035, #121899 ) ) ;
#57532 = CARTESIAN_POINT ( 'NONE',  ( 21.05000000000000071, 49.36776662947724503, -253.7196102226803021 ) ) ;
#57534 = ORIENTED_EDGE ( 'NONE', *, *, #46193, .F. ) ;
#57533 = EDGE_CURVE ( 'NONE', #196293, #175979, #127619, .T. ) ;
#57535 = ORIENTED_EDGE ( 'NONE', *, *, #77891, .F. ) ;
#57536 = DIRECTION ( 'NONE',  ( -1.000000000000000000, 0.000000000000000000, -0.000000000000000000 ) ) ;
#57537 = VERTEX_POINT ( 'NONE', #207990 ) ;
#57538 = CARTESIAN_POINT ( 'NONE',  ( -23.25000000000000000, 6.933893972137497030, -204.7856458343735255 ) ) ;
#57540 = CARTESIAN_POINT ( 'NONE',  ( 23.15000000000000213, 87.65000000001172964, -72.62310748452422615 ) ) ;
#57539 = CARTESIAN_POINT ( 'NONE',  ( 21.05000000000005400, 65.15000000001120384, -4.423107484524790856 ) ) ;
#57541 = EDGE_LOOP ( 'NONE', ( #175933, #198333, #141946, #78087, #209189 ) ) ;
#57542 = CIRCLE ( 'NONE', #20157, 0.1000000000000002554 ) ;
#57543 = VECTOR ( 'NONE', #250247, 1000.000000000000000 ) ;
#57545 = ADVANCED_FACE ( 'NONE', ( #29376 ), #52598, .F. ) ;
#57544 = ORIENTED_EDGE ( 'NONE', *, *, #228203, .F. ) ;
#57546 = CARTESIAN_POINT ( 'NONE',  ( -21.14999999999999858, -11.64999999998884483, -136.9000000000000341 ) ) ;
#57547 = VECTOR ( 'NONE', #237627, 1000.000000000000114 ) ;
#57548 = VERTEX_POINT ( 'NONE', #63308 ) ;
#57549 = CIRCLE ( 'NONE', #115833, 0.09999999999999939493 ) ;
#57550 = CARTESIAN_POINT ( 'NONE',  ( -21.59142135623730852, 68.15000000001228386, -157.6731074845243938 ) ) ;
#57551 = ORIENTED_EDGE ( 'NONE', *, *, #4107, .F. ) ;
#57552 = ORIENTED_EDGE ( 'NONE', *, *, #95506, .T. ) ;
#57553 = FACE_OUTER_BOUND ( 'NONE', #58055, .T. ) ;
#57554 = ORIENTED_EDGE ( 'NONE', *, *, #205642, .F. ) ;
#57555 = DIRECTION ( 'NONE',  ( 0.000000000000000000, -1.000000000000000000, -7.272083257015735086E-15 ) ) ;
#57556 = DIRECTION ( 'NONE',  ( 0.000000000000000000, 0.9126074666063660468, 0.4088369013363524762 ) ) ;
#57557 = ORIENTED_EDGE ( 'NONE', *, *, #178552, .F. ) ;
#57558 = CIRCLE ( 'NONE', #236629, 0.1000000000000043771 ) ;
#57559 = DIRECTION ( 'NONE',  ( 1.000000000000000000, 4.095934188116521533E-15, 3.985178720521109717E-14 ) ) ;
#57560 = CARTESIAN_POINT ( 'NONE',  ( -18.59999999999999787, 11.75000000001115197, -174.5148057706539930 ) ) ;
#57561 = CARTESIAN_POINT ( 'NONE',  ( -21.05000000000000071, 56.02567683926420727, -227.9999002286038774 ) ) ;
#57562 = DIRECTION ( 'NONE',  ( 1.000000000000000000, -0.000000000000000000, -0.000000000000000000 ) ) ;
#57563 = EDGE_CURVE ( 'NONE', #209310, #82517, #152599, .T. ) ;
#57564 = DIRECTION ( 'NONE',  ( 0.000000000000000000, -0.000000000000000000, 1.000000000000000000 ) ) ;
#57566 = AXIS2_PLACEMENT_3D ( 'NONE', #111537, #35869, #97059 ) ;
#57565 = CARTESIAN_POINT ( 'NONE',  ( -16.97048361161167307, 62.95718135765960000, -213.6016144441782387 ) ) ;
#57567 = CIRCLE ( 'NONE', #199243, 0.1000000000000028644 ) ;
#57568 = CARTESIAN_POINT ( 'NONE',  ( -16.79140778683511215, 66.05505840115770866, -149.1933702507536736 ) ) ;
#57569 = CARTESIAN_POINT ( 'NONE',  ( 22.41477678272288188, 75.99917613424928220, -148.1726927690397133 ) ) ;
#57570 = CIRCLE ( 'NONE', #195163, 0.09999999999999062417 ) ;
#57572 = ORIENTED_EDGE ( 'NONE', *, *, #73307, .T. ) ;
#57571 = AXIS2_PLACEMENT_3D ( 'NONE', #149923, #130322, #31278 ) ;
#57573 = EDGE_CURVE ( 'NONE', #97655, #10791, #145416, .T. ) ;
#57575 = ORIENTED_EDGE ( 'NONE', *, *, #54497, .T. ) ;
#57574 = VERTEX_POINT ( 'NONE', #14922 ) ;
#57576 = ORIENTED_EDGE ( 'NONE', *, *, #37276, .F. ) ;
#57578 = VERTEX_POINT ( 'NONE', #213100 ) ;
#57577 = EDGE_CURVE ( 'NONE', #17846, #58858, #252495, .T. ) ;
#57579 = CARTESIAN_POINT ( 'NONE',  ( 21.10257677756356998, 75.97504925044474078, -209.9214892270570942 ) ) ;
#57580 = CARTESIAN_POINT ( 'NONE',  ( 21.05000000000000071, 67.23127455305835554, -235.8551265064784559 ) ) ;
#57581 = EDGE_CURVE ( 'NONE', #86057, #125245, #56838, .T. ) ;
#57582 = EDGE_CURVE ( 'NONE', #80890, #55172, #171452, .T. ) ;
#57584 = FACE_OUTER_BOUND ( 'NONE', #87149, .T. ) ;
#57583 = DIRECTION ( 'NONE',  ( 2.952720810173289112E-16, 0.4088369013363287729, -0.9126074666063767049 ) ) ;
#57585 = ORIENTED_EDGE ( 'NONE', *, *, #48641, .T. ) ;
#57586 = AXIS2_PLACEMENT_3D ( 'NONE', #68329, #155271, #76973 ) ;
#57587 = CARTESIAN_POINT ( 'NONE',  ( -20.94999999999994600, 66.15000000001120384, -4.623107484524796362 ) ) ;
#57588 = DIRECTION ( 'NONE',  ( -0.7071067811865474617, -0.7071067811865474617, -0.000000000000000000 ) ) ;
#57589 = CARTESIAN_POINT ( 'NONE',  ( -16.88560720703333473, 9.950564843760847822, -180.1481119208636983 ) ) ;
#57590 = ADVANCED_FACE ( 'NONE', ( #134821 ), #170178, .F. ) ;
#57591 = DIRECTION ( 'NONE',  ( -1.000000000000000000, 0.000000000000000000, 0.000000000000000000 ) ) ;
#57592 = EDGE_LOOP ( 'NONE', ( #46307, #224875, #176720, #170437 ) ) ;
#57593 = EDGE_CURVE ( 'NONE', #99483, #198203, #48502, .T. ) ;
#57595 = ADVANCED_FACE ( 'NONE', ( #33228 ), #189694, .F. ) ;
#57594 = ADVANCED_FACE ( 'NONE', ( #94433 ), #227556, .T. ) ;
#57596 = DIRECTION ( 'NONE',  ( -1.444674012291107001E-15, 0.1332476588733650935, 0.9910827722268042983 ) ) ;
#57597 = VERTEX_POINT ( 'NONE', #191001 ) ;
#57598 = DIRECTION ( 'NONE',  ( -1.000000000000000000, 0.000000000000000000, 0.000000000000000000 ) ) ;
#57599 = CARTESIAN_POINT ( 'NONE',  ( -18.59999999999999787, 9.250000000011157297, -179.8499999999999943 ) ) ;
#57600 = DIRECTION ( 'NONE',  ( -1.000000000000000000, -0.000000000000000000, 0.000000000000000000 ) ) ;
#57601 = DIRECTION ( 'NONE',  ( 1.000000000000000000, 0.000000000000000000, 0.000000000000000000 ) ) ;
#57602 = DIRECTION ( 'NONE',  ( 0.000000000000000000, 1.000000000000000000, 0.000000000000000000 ) ) ;
#57603 = CARTESIAN_POINT ( 'NONE',  ( 20.94999999999999929, 8.776282895303632259, -45.65000000000000568 ) ) ;
#57604 = ORIENTED_EDGE ( 'NONE', *, *, #204221, .T. ) ;
#57605 = CARTESIAN_POINT ( 'NONE',  ( -23.25000000000000000, 64.25000000001237765, -170.0231074845244166 ) ) ;
#57606 = CARTESIAN_POINT ( 'NONE',  ( 20.94999999999999574, 77.83534155023646406, -124.8679561919613121 ) ) ;
#57607 = DIRECTION ( 'NONE',  ( -0.7071067811865301422, 0.7071067811865648922, 0.000000000000000000 ) ) ;
#57608 = EDGE_CURVE ( 'NONE', #146363, #118755, #165992, .T. ) ;
#57610 = PLANE ( 'NONE',  #24596 ) ;
#57609 = CARTESIAN_POINT ( 'NONE',  ( 23.14999999999999503, 69.35000000001156195, -57.27310748452436684 ) ) ;
#57611 = DIRECTION ( 'NONE',  ( -0.000000000000000000, 1.000000000000000000, 1.626303258728266709E-15 ) ) ;
#57612 = CARTESIAN_POINT ( 'NONE',  ( -16.94275863006528482, 9.989496048678669027, -121.3916973820766145 ) ) ;
#57613 = AXIS2_PLACEMENT_3D ( 'NONE', #104497, #158132, #202344 ) ;
#57614 = AXIS2_PLACEMENT_3D ( 'NONE', #94224, #176361, #173826 ) ;
#57615 = AXIS2_PLACEMENT_3D ( 'NONE', #174023, #52732, #196115 ) ;
#57616 = DIRECTION ( 'NONE',  ( 1.000000000000000000, 0.000000000000000000, 0.000000000000000000 ) ) ;
#57617 = CARTESIAN_POINT ( 'NONE',  ( -23.15000000000000213, 71.65000000001180069, -81.87310748452433984 ) ) ;
#57618 = ADVANCED_FACE ( 'NONE', ( #253502 ), #12364, .T. ) ;
#57619 = AXIS2_PLACEMENT_3D ( 'NONE', #116673, #157110, #138766 ) ;
#57620 = EDGE_CURVE ( 'NONE', #184847, #185482, #27316, .T. ) ;
#57621 = ORIENTED_EDGE ( 'NONE', *, *, #18151, .F. ) ;
#57622 = EDGE_LOOP ( 'NONE', ( #20481, #207753, #51056, #212449, #187895 ) ) ;
#57623 = EDGE_CURVE ( 'NONE', #161165, #27184, #210542, .T. ) ;
#57624 = CARTESIAN_POINT ( 'NONE',  ( 23.40000000000005542, 83.80000000001119531, -34.86056257560453986 ) ) ;
#57625 = ORIENTED_EDGE ( 'NONE', *, *, #63236, .T. ) ;
#57626 = DIRECTION ( 'NONE',  ( 0.000000000000000000, 0.000000000000000000, -1.000000000000000000 ) ) ;
#57627 = ADVANCED_FACE ( 'NONE', ( #13626 ), #18893, .T. ) ;
#57628 = AXIS2_PLACEMENT_3D ( 'NONE', #245622, #168702, #205188 ) ;
#57629 = CIRCLE ( 'NONE', #211777, 0.9750000000000036415 ) ;
#57630 = DIRECTION ( 'NONE',  ( 0.000000000000000000, 1.000000000000000000, 7.272083257015735086E-15 ) ) ;
#57631 = VERTEX_POINT ( 'NONE', #31928 ) ;
#57632 = AXIS2_PLACEMENT_3D ( 'NONE', #208336, #213437, #132634 ) ;
#57633 = CARTESIAN_POINT ( 'NONE',  ( 20.12500000000000000, 66.25000000001263345, -195.4113362024101548 ) ) ;
#57634 = DIRECTION ( 'NONE',  ( -1.000000000000000000, 0.000000000000000000, -0.000000000000000000 ) ) ;
#57635 = CARTESIAN_POINT ( 'NONE',  ( -22.59999999999999787, 75.89914163091376054, -181.7726746080137445 ) ) ;
#57636 = FACE_OUTER_BOUND ( 'NONE', #147692, .T. ) ;
#57638 = ORIENTED_EDGE ( 'NONE', *, *, #66168, .F. ) ;
#57637 = CARTESIAN_POINT ( 'NONE',  ( -20.54999999999999716, 76.00000000001149658, -48.89810748452431710 ) ) ;
#57640 = CARTESIAN_POINT ( 'NONE',  ( 20.04142135623731136, 11.75000000001116263, -192.1499999999999488 ) ) ;
#57639 = DIRECTION ( 'NONE',  ( 1.000000000000000000, 0.000000000000000000, 0.000000000000000000 ) ) ;
#57641 = CARTESIAN_POINT ( 'NONE',  ( 19.97071067811864609, 64.27928932189283273, -44.87310748452440379 ) ) ;
#57642 = CARTESIAN_POINT ( 'NONE',  ( 23.25000000000000000, -8.596261682231828516, -191.5498724828496790 ) ) ;
#57643 = DIRECTION ( 'NONE',  ( -1.000000000000000000, -2.952720810173289112E-16, 0.000000000000000000 ) ) ;
#57644 = FACE_OUTER_BOUND ( 'NONE', #202084, .T. ) ;
#57645 = EDGE_LOOP ( 'NONE', ( #43125, #256949, #132557 ) ) ;
#57646 = CARTESIAN_POINT ( 'NONE',  ( 0.000000000000000000, 0.000000000000000000, 0.000000000000000000 ) ) ;
#57647 = DIRECTION ( 'NONE',  ( -1.000000000000000000, 0.000000000000000000, 0.000000000000000000 ) ) ;
#57648 = EDGE_LOOP ( 'NONE', ( #4890, #58769, #28012 ) ) ;
#57649 = TOROIDAL_SURFACE ( 'NONE', #24369, 0.6000000000000017542, 0.1000000000000000056 ) ;
#57650 = CARTESIAN_POINT ( 'NONE',  ( -16.89081410710458542, 66.04868147016543389, -182.6687015646880639 ) ) ;
#57651 = VERTEX_POINT ( 'NONE', #174025 ) ;
#57652 = CIRCLE ( 'NONE', #199329, 0.09999999999998898659 ) ;
#57653 = AXIS2_PLACEMENT_3D ( 'NONE', #148150, #192421, #247238 ) ;
#57654 = CARTESIAN_POINT ( 'NONE',  ( -18.59999999999999787, 61.63293978347611812, -221.5406706031726003 ) ) ;
#57655 = DIRECTION ( 'NONE',  ( 7.304098846218134667E-16, -1.000000000000000000, -6.982962677686267499E-15 ) ) ;
#57656 = CARTESIAN_POINT ( 'NONE',  ( -18.50000000000000000, 77.68707439010360360, -115.8376804510659497 ) ) ;
#57657 = EDGE_LOOP ( 'NONE', ( #49969, #235828, #144503 ) ) ;
#57658 = ORIENTED_EDGE ( 'NONE', *, *, #157746, .T. ) ;
#57659 = CARTESIAN_POINT ( 'NONE',  ( -20.00857864376270001, 63.86602797976523505, -212.9247947273492514 ) ) ;
#57660 = LINE ( 'NONE', #158113, #252481 ) ;
#57661 = EDGE_CURVE ( 'NONE', #106961, #45697, #39781, .T. ) ;
#57662 = FACE_OUTER_BOUND ( 'NONE', #33484, .T. ) ;
#57663 = FACE_OUTER_BOUND ( 'NONE', #237216, .T. ) ;
#57665 = DIRECTION ( 'NONE',  ( -1.000000000000000000, 3.265361837132813093E-16, 2.280189983783949500E-30 ) ) ;
#57664 = DIRECTION ( 'NONE',  ( -3.469446951953515108E-14, -1.000000000000000000, 0.000000000000000000 ) ) ;
#57666 = AXIS2_PLACEMENT_3D ( 'NONE', #254989, #76405, #157271 ) ;
#57668 = CARTESIAN_POINT ( 'NONE',  ( -18.39999999999999858, -9.682403433476396870, -40.15684337741279109 ) ) ;
#57667 = AXIS2_PLACEMENT_3D ( 'NONE', #77181, #215412, #135858 ) ;
#57669 = ADVANCED_FACE ( 'NONE', ( #16216 ), #149305, .T. ) ;
#57670 = CARTESIAN_POINT ( 'NONE',  ( 21.04116576186320486, 65.37533692126049800, -90.69452571589661716 ) ) ;
#57671 = CARTESIAN_POINT ( 'NONE',  ( -21.05000000000000071, 74.63912941281984104, -94.95010955743335046 ) ) ;
#57672 = AXIS2_PLACEMENT_3D ( 'NONE', #59323, #60628, #42371 ) ;
#57673 = ORIENTED_EDGE ( 'NONE', *, *, #39955, .F. ) ;
#57674 = DIRECTION ( 'NONE',  ( 0.000000000000000000, 8.881784197002011602E-16, -1.000000000000000000 ) ) ;
#57676 = EDGE_LOOP ( 'NONE', ( #18873, #247296, #31964, #254448 ) ) ;
#57675 = CARTESIAN_POINT ( 'NONE',  ( 20.84999999999999432, -1.164121893230052995, -74.91484808557160591 ) ) ;
#57677 = CARTESIAN_POINT ( 'NONE',  ( 21.15000000000005542, 87.50449464844290048, -34.18759587077607165 ) ) ;
#57678 = VECTOR ( 'NONE', #80119, 1000.000000000000000 ) ;
#57679 = CARTESIAN_POINT ( 'NONE',  ( 21.14999999999999858, 42.94327155031035659, -233.8606566173841372 ) ) ;
#57681 = CARTESIAN_POINT ( 'NONE',  ( -18.50000000000000000, 44.10700160683882132, -235.9691471569721841 ) ) ;
#57680 = CARTESIAN_POINT ( 'NONE',  ( 23.40000000000005542, 74.16448838626247664, -47.52760213295649550 ) ) ;
#57682 = EDGE_CURVE ( 'NONE', #222338, #251965, #210456, .T. ) ;
#57683 = ADVANCED_FACE ( 'NONE', ( #196118 ), #248028, .T. ) ;
#57684 = ORIENTED_EDGE ( 'NONE', *, *, #237235, .T. ) ;
#57686 = CARTESIAN_POINT ( 'NONE',  ( -18.40000000000000213, 11.47867410001105881, -57.72530678365939849 ) ) ;
#57685 = DIRECTION ( 'NONE',  ( -3.265361837132813093E-16, 1.000000000000000000, 0.000000000000000000 ) ) ;
#57687 = LINE ( 'NONE', #218037, #96894 ) ;
#57688 = CYLINDRICAL_SURFACE ( 'NONE', #165853, 12.87499999999999822 ) ;
#57689 = CARTESIAN_POINT ( 'NONE',  ( -18.39999999999999858, 85.68240343348826116, -96.36626410711143365 ) ) ;
#57690 = ORIENTED_EDGE ( 'NONE', *, *, #9755, .T. ) ;
#57691 = CARTESIAN_POINT ( 'NONE',  ( -33.72168855820452649, 52.34166666667894674, -153.2731074845245303 ) ) ;
#57692 = AXIS2_PLACEMENT_3D ( 'NONE', #66678, #148788, #245316 ) ;
#57693 = ORIENTED_EDGE ( 'NONE', *, *, #22280, .F. ) ;
#57694 = DIRECTION ( 'NONE',  ( -1.000000000000000000, -2.952720810173289112E-16, 0.000000000000000000 ) ) ;
#57695 = AXIS2_PLACEMENT_3D ( 'NONE', #95256, #216486, #193088 ) ;
#57696 = ORIENTED_EDGE ( 'NONE', *, *, #69932, .F. ) ;
#57697 = CARTESIAN_POINT ( 'NONE',  ( -17.01473183483381391, 9.950000000011138823, -154.7500000000000284 ) ) ;
#57698 = VERTEX_POINT ( 'NONE', #137406 ) ;
#57699 = ADVANCED_FACE ( 'NONE', ( #256024 ), #77421, .F. ) ;
#57700 = CIRCLE ( 'NONE', #124186, 0.09999999999999939493 ) ;
#57701 = DIRECTION ( 'NONE',  ( -3.469446951953605354E-14, 1.000000000000000000, 0.000000000000000000 ) ) ;
#57702 = CIRCLE ( 'NONE', #203467, 0.09999999999999939493 ) ;
#57703 = AXIS2_PLACEMENT_3D ( 'NONE', #142254, #2730, #41903 ) ;
#57704 = AXIS2_PLACEMENT_3D ( 'NONE', #29190, #44853, #10871 ) ;
#57705 =( BOUNDED_CURVE ( )  B_SPLINE_CURVE ( 3, ( #140440, #200430, #126013, #202989 ),
 .UNSPECIFIED., .F., .F. ) 
 B_SPLINE_CURVE_WITH_KNOTS ( ( 4, 4 ),
 ( 3.141592653589793116, 4.712388980384689674 ),
 .UNSPECIFIED. ) 
 CURVE ( )  GEOMETRIC_REPRESENTATION_ITEM ( )  RATIONAL_B_SPLINE_CURVE ( ( 1.000000000000000000, 0.8047378541243649375, 0.8047378541243649375, 1.000000000000000000 ) ) 
 REPRESENTATION_ITEM ( '' )  );
#57706 = DIRECTION ( 'NONE',  ( -1.000000000000000000, 0.000000000000000000, 0.000000000000000000 ) ) ;
#57707 = ORIENTED_EDGE ( 'NONE', *, *, #78535, .F. ) ;
#57708 = AXIS2_PLACEMENT_3D ( 'NONE', #199808, #180236, #100649 ) ;
#57709 = CARTESIAN_POINT ( 'NONE',  ( -18.44448725179913851, -9.490081715472173940, -174.1289602940624945 ) ) ;
#57710 = CARTESIAN_POINT ( 'NONE',  ( -22.50000000000000000, 0.09770955616802273758, -200.9787199004788931 ) ) ;
#57711 = DIRECTION ( 'NONE',  ( 2.694716079187272946E-16, -1.000000000000000000, 0.000000000000000000 ) ) ;
#57712 = CARTESIAN_POINT ( 'NONE',  ( 20.85000000000000142, 8.788681102860174121, -241.3540466926497174 ) ) ;
#57713 = DIRECTION ( 'NONE',  ( 6.423964682151766729E-15, 0.1575546449569727725, 0.9875102702516478370 ) ) ;
#57714 = CARTESIAN_POINT ( 'NONE',  ( 12.60053434924910754, 62.27203542310181916, -218.2690822304508913 ) ) ;
#57715 = B_SPLINE_CURVE_WITH_KNOTS ( 'NONE', 3,
 ( #10805, #12110, #150327, #129469, #206430, #49921, #207736, #146435, #68209, #91623 ),
 .UNSPECIFIED., .F., .F.,
 ( 4, 3, 3, 4 ),
 ( -2.000561356209491534E-06, 0.000000000000000000, 1.787822682428948123E-05, 4.206475347090216207E-05 ),
 .UNSPECIFIED. ) ;
#57717 = ORIENTED_EDGE ( 'NONE', *, *, #51315, .T. ) ;
#57716 = EDGE_CURVE ( 'NONE', #123921, #199924, #135593, .T. ) ;
#57718 = DIRECTION ( 'NONE',  ( 0.000000000000000000, -0.4856429311786292224, -0.8741572761215394838 ) ) ;
#57719 = CIRCLE ( 'NONE', #257576, 0.5000000000000004441 ) ;
#57720 = ORIENTED_EDGE ( 'NONE', *, *, #132375, .T. ) ;
#57722 = EDGE_LOOP ( 'NONE', ( #101029, #147603, #75963, #184301 ) ) ;
#57721 = CYLINDRICAL_SURFACE ( 'NONE', #77271, 0.1000000000000038219 ) ;
#57723 = ORIENTED_EDGE ( 'NONE', *, *, #71685, .T. ) ;
#57724 = DIRECTION ( 'NONE',  ( 0.000000000000000000, -0.2617529984165035128, -0.9651348961777155289 ) ) ;
#57725 = CARTESIAN_POINT ( 'NONE',  ( -18.39999999999999858, 85.51932773110404185, -62.55013110796492271 ) ) ;
#57726 = CARTESIAN_POINT ( 'NONE',  ( 22.57320508075687115, 11.75000000000000000, 0.000000000000000000 ) ) ;
#57727 = CARTESIAN_POINT ( 'NONE',  ( -21.05000000000000071, 69.60000000001157616, -59.59268285446279378 ) ) ;
#57728 = ORIENTED_EDGE ( 'NONE', *, *, #170804, .T. ) ;
#57729 = DIRECTION ( 'NONE',  ( 0.000000000000000000, 0.000000000000000000, -1.000000000000000000 ) ) ;
#57730 = CARTESIAN_POINT ( 'NONE',  ( 18.59999999999999076, 69.35000000001200249, -115.3731074845243398 ) ) ;
#57731 = EDGE_CURVE ( 'NONE', #177411, #140135, #87513, .T. ) ;
#57732 = EDGE_LOOP ( 'NONE', ( #111295, #135680, #243451, #19735 ) ) ;
#57733 = AXIS2_PLACEMENT_3D ( 'NONE', #125629, #22707, #223431 ) ;
#57735 = ORIENTED_EDGE ( 'NONE', *, *, #34875, .F. ) ;
#57734 = FACE_OUTER_BOUND ( 'NONE', #103121, .T. ) ;
#57736 = EDGE_CURVE ( 'NONE', #212150, #182680, #81268, .T. ) ;
#57737 = AXIS2_PLACEMENT_3D ( 'NONE', #66762, #143715, #25089 ) ;
#57738 = CARTESIAN_POINT ( 'NONE',  ( -23.15000000000000213, 11.60000000001115517, -60.07179676972450011 ) ) ;
#57739 = CIRCLE ( 'NONE', #220063, 11.64999999999999325 ) ;
#57740 = DIRECTION ( 'NONE',  ( 1.000000000000000000, 3.469446951953704435E-14, -2.003086131649669752E-14 ) ) ;
#57741 = ORIENTED_EDGE ( 'NONE', *, *, #254736, .T. ) ;
#57742 = VECTOR ( 'NONE', #66585, 999.9999999999998863 ) ;
#57743 = ADVANCED_FACE ( 'NONE', ( #116576 ), #158305, .F. ) ;
#57744 = CARTESIAN_POINT ( 'NONE',  ( 20.94999999999999929, 64.36312671090750825, -109.8448666978492270 ) ) ;
#57745 = ORIENTED_EDGE ( 'NONE', *, *, #101940, .T. ) ;
#57746 = DIRECTION ( 'NONE',  ( 0.000000000000000000, 0.000000000000000000, -1.000000000000000000 ) ) ;
#57747 = EDGE_CURVE ( 'NONE', #53590, #161202, #40920, .T. ) ;
#57748 = CARTESIAN_POINT ( 'NONE',  ( -18.50000000000000000, -1.135018845899022466, -175.2169768834323520 ) ) ;
#57749 = CARTESIAN_POINT ( 'NONE',  ( 12.60873083341396139, 66.61042836546511126, -51.70546677215522635 ) ) ;
#57750 = AXIS2_PLACEMENT_3D ( 'NONE', #66595, #126563, #31351 ) ;
#57751 = EDGE_CURVE ( 'NONE', #220457, #10283, #175299, .T. ) ;
#57752 = CYLINDRICAL_SURFACE ( 'NONE', #171952, 0.1000000000000028644 ) ;
#57753 = AXIS2_PLACEMENT_3D ( 'NONE', #167380, #184331, #14408 ) ;
#57754 = AXIS2_PLACEMENT_3D ( 'NONE', #1200, #61200, #146811 ) ;
#57755 = EDGE_CURVE ( 'NONE', #200940, #182384, #136101, .T. ) ;
#57756 = AXIS2_PLACEMENT_3D ( 'NONE', #252170, #214345, #211787 ) ;
#57757 = VERTEX_POINT ( 'NONE', #237808 ) ;
#57758 = DIRECTION ( 'NONE',  ( 0.000000000000000000, 6.982962677686267499E-15, -1.000000000000000000 ) ) ;
#57759 = ORIENTED_EDGE ( 'NONE', *, *, #222976, .F. ) ;
#57760 = CARTESIAN_POINT ( 'NONE',  ( -18.79999999999999716, 5.488301202077012775, 16.50000000000000000 ) ) ;
#57762 = EDGE_CURVE ( 'NONE', #60411, #41111, #40360, .T. ) ;
#57761 = DIRECTION ( 'NONE',  ( -1.000000000000000000, -0.000000000000000000, 0.000000000000000000 ) ) ;
#57764 = ORIENTED_EDGE ( 'NONE', *, *, #78740, .F. ) ;
#57763 = LINE ( 'NONE', #194751, #237470 ) ;
#57765 = LINE ( 'NONE', #38232, #149474 ) ;
#57766 = CARTESIAN_POINT ( 'NONE',  ( 21.00000000000000000, -1.885425182446133885, -11.49641995933507843 ) ) ;
#57767 = CARTESIAN_POINT ( 'NONE',  ( 21.14999999999999503, -0.09999999998884338825, -122.3504291924552234 ) ) ;
#57769 = CARTESIAN_POINT ( 'NONE',  ( -21.05000000000000071, 64.25000000001146816, -43.03791325517834565 ) ) ;
#57768 =( BOUNDED_CURVE ( )  B_SPLINE_CURVE ( 3, ( #193086, #93963, #195667, #131811 ),
 .UNSPECIFIED., .F., .F. ) 
 B_SPLINE_CURVE_WITH_KNOTS ( ( 4, 4 ),
 ( 0.5235987755983007030, 1.570796326794896558 ),
 .UNSPECIFIED. ) 
 CURVE ( )  GEOMETRIC_REPRESENTATION_ITEM ( )  RATIONAL_B_SPLINE_CURVE ( ( 1.000000000000000000, 0.9106836025229594345, 0.9106836025229594345, 1.000000000000000000 ) ) 
 REPRESENTATION_ITEM ( '' )  );
#57770 = CARTESIAN_POINT ( 'NONE',  ( 20.94999999999999929, 1.115600667400684642E-11, -205.0999999999999375 ) ) ;
#57771 = AXIS2_PLACEMENT_3D ( 'NONE', #126044, #45243, #123500 ) ;
#57772 = CARTESIAN_POINT ( 'NONE',  ( -22.39999999999999858, 11.65000000001115588, -100.4000000000000483 ) ) ;
#57773 = CARTESIAN_POINT ( 'NONE',  ( -18.58693740092131108, 85.40643215026497614, -129.3982910280227543 ) ) ;
#57775 = EDGE_LOOP ( 'NONE', ( #131917, #202586, #35547, #69045 ) ) ;
#57774 = CARTESIAN_POINT ( 'NONE',  ( 15.74999999999999645, 66.15000000001185754, -86.27310748452437394 ) ) ;
#57776 = CARTESIAN_POINT ( 'NONE',  ( 18.59999999999999076, 68.92903212821327941, -132.7765432626560766 ) ) ;
#57777 = CARTESIAN_POINT ( 'NONE',  ( -18.36527282682033402, 85.50000060001060831, -62.60095852002528716 ) ) ;
#57778 = CARTESIAN_POINT ( 'NONE',  ( -18.59999996769639097, 85.36327376984304749, -196.3416135690586088 ) ) ;
#57779 = ORIENTED_EDGE ( 'NONE', *, *, #199633, .F. ) ;
#57780 = CARTESIAN_POINT ( 'NONE',  ( 23.04999999999999716, 67.17743825834517679, -56.87310748452437537 ) ) ;
#57781 = FILL_AREA_STYLE_COLOUR ( '', #257224 ) ;
#57782 = AXIS2_PLACEMENT_3D ( 'NONE', #173545, #251742, #35306 ) ;
#57783 = AXIS2_PLACEMENT_3D ( 'NONE', #128137, #29068, #108567 ) ;
#57784 = EDGE_LOOP ( 'NONE', ( #164355, #10617, #230839, #230418 ) ) ;
#57785 = AXIS2_PLACEMENT_3D ( 'NONE', #109944, #128242, #129522 ) ;
#57786 = DIRECTION ( 'NONE',  ( 0.000000000000000000, 0.9126074666063770380, 0.4088369013363281068 ) ) ;
#57787 =( BOUNDED_CURVE ( )  B_SPLINE_CURVE ( 3, ( #132792, #117060, #200443, #101282 ),
 .UNSPECIFIED., .F., .F. ) 
 B_SPLINE_CURVE_WITH_KNOTS ( ( 4, 4 ),
 ( 0.000000000000000000, 1.570796326794908992 ),
 .UNSPECIFIED. ) 
 CURVE ( )  GEOMETRIC_REPRESENTATION_ITEM ( )  RATIONAL_B_SPLINE_CURVE ( ( 1.000000000000000000, 0.8047378541243619399, 0.8047378541243619399, 1.000000000000000000 ) ) 
 REPRESENTATION_ITEM ( '' )  );
#57788 = FACE_OUTER_BOUND ( 'NONE', #77603, .T. ) ;
#57789 = ORIENTED_EDGE ( 'NONE', *, *, #75902, .F. ) ;
#57790 = AXIS2_PLACEMENT_3D ( 'NONE', #225983, #163482, #104752 ) ;
#57791 = DIRECTION ( 'NONE',  ( -1.000000000000000000, -0.000000000000000000, -0.000000000000000000 ) ) ;
#57792 = ORIENTED_EDGE ( 'NONE', *, *, #203808, .F. ) ;
#57793 = DIRECTION ( 'NONE',  ( -1.000000000000000000, 0.000000000000000000, 0.000000000000000000 ) ) ;
#57794 = EDGE_CURVE ( 'NONE', #170273, #179549, #127238, .T. ) ;
#57796 = ORIENTED_EDGE ( 'NONE', *, *, #159730, .F. ) ;
#57795 = CARTESIAN_POINT ( 'NONE',  ( 21.07928932188134397, 6.328516656404468144, -133.9011048543456184 ) ) ;
#57797 = FACE_OUTER_BOUND ( 'NONE', #91538, .T. ) ;
#57798 = ORIENTED_EDGE ( 'NONE', *, *, #42473, .F. ) ;
#57799 = EDGE_CURVE ( 'NONE', #213303, #42728, #34256, .T. ) ;
#57800 = CARTESIAN_POINT ( 'NONE',  ( -0.8999999999999993561, -9.650000000000003908, 28.60000000000000142 ) ) ;
#57801 = AXIS2_PLACEMENT_3D ( 'NONE', #215618, #190959, #91832 ) ;
#57803 = EDGE_CURVE ( 'NONE', #99200, #37772, #201234, .T. ) ;
#57802 = TOROIDAL_SURFACE ( 'NONE', #70335, 0.2000000000000000111, 0.1000000000000000056 ) ;
#57804 = ORIENTED_EDGE ( 'NONE', *, *, #153466, .T. ) ;
#57806 = EDGE_LOOP ( 'NONE', ( #13489, #101538, #44009, #89502, #75432 ) ) ;
#57805 = ORIENTED_EDGE ( 'NONE', *, *, #175363, .T. ) ;
#57808 = CARTESIAN_POINT ( 'NONE',  ( 18.40000000000000213, 85.51932773110452501, -129.5501311079648872 ) ) ;
#57807 = AXIS2_PLACEMENT_3D ( 'NONE', #257827, #200482, #255260 ) ;
#57809 = ORIENTED_EDGE ( 'NONE', *, *, #223630, .F. ) ;
#57810 = CARTESIAN_POINT ( 'NONE',  ( -18.59999999999999787, 74.83729825007431202, -161.9231074845243654 ) ) ;
#57811 = ORIENTED_EDGE ( 'NONE', *, *, #59122, .F. ) ;
#57812 = AXIS2_PLACEMENT_3D ( 'NONE', #119181, #237836, #17495 ) ;
#57813 = EDGE_LOOP ( 'NONE', ( #169787, #242135, #215971, #77380 ) ) ;
#57814 = EDGE_CURVE ( 'NONE', #231239, #100947, #141272, .T. ) ;
#57815 = CARTESIAN_POINT ( 'NONE',  ( 20.90000000000000213, 6.356682116888462630, 11.91686199900910381 ) ) ;
#57816 = DIRECTION ( 'NONE',  ( 0.000000000000000000, 0.000000000000000000, -1.000000000000000000 ) ) ;
#57817 = CARTESIAN_POINT ( 'NONE',  ( -18.59999999999999787, 9.150000000011157653, -21.75000000000000355 ) ) ;
#57818 = LINE ( 'NONE', #61695, #2265 ) ;
#57819 = VERTEX_POINT ( 'NONE', #121729 ) ;
#57820 = DIRECTION ( 'NONE',  ( -6.938893903907222067E-15, -1.000000000000000000, -6.982962677686266711E-15 ) ) ;
#57821 = CARTESIAN_POINT ( 'NONE',  ( -20.54999999999999716, 67.23127455305835554, -235.8551265064784559 ) ) ;
#57822 = CARTESIAN_POINT ( 'NONE',  ( 23.14999999999999503, 21.17283678855157802, -243.7231193059830048 ) ) ;
#57823 = ORIENTED_EDGE ( 'NONE', *, *, #241839, .F. ) ;
#57824 = DIRECTION ( 'NONE',  ( 0.000000000000000000, 1.069579021796875354E-15, 1.000000000000000000 ) ) ;
#57825 = DIRECTION ( 'NONE',  ( -0.000000000000000000, -6.982962677686266711E-15, 1.000000000000000000 ) ) ;
#57826 = CARTESIAN_POINT ( 'NONE',  ( -21.65000000000000213, 44.22674245267958781, -235.2580479164738279 ) ) ;
#57827 = ORIENTED_EDGE ( 'NONE', *, *, #243074, .F. ) ;
#57828 = FACE_OUTER_BOUND ( 'NONE', #127829, .T. ) ;
#57829 = EDGE_LOOP ( 'NONE', ( #75891, #20434, #253818, #11311 ) ) ;
#57830 = VECTOR ( 'NONE', #83169, 1000.000000000000227 ) ;
#57831 = ORIENTED_EDGE ( 'NONE', *, *, #4317, .F. ) ;
#57832 = DIRECTION ( 'NONE',  ( 1.000000000000000000, -0.000000000000000000, 0.000000000000000000 ) ) ;
#57833 = ORIENTED_EDGE ( 'NONE', *, *, #120516, .F. ) ;
#57834 = ORIENTED_EDGE ( 'NONE', *, *, #23072, .T. ) ;
#57835 = CARTESIAN_POINT ( 'NONE',  ( -14.00000000000000178, 9.850000000011133849, -50.25000000000000711 ) ) ;
#57836 = EDGE_CURVE ( 'NONE', #143460, #31770, #50947, .T. ) ;
#57837 = DIRECTION ( 'NONE',  ( -1.000000000000000000, 0.000000000000000000, 0.000000000000000000 ) ) ;
#57838 = ORIENTED_EDGE ( 'NONE', *, *, #165335, .F. ) ;
#57839 = EDGE_CURVE ( 'NONE', #89812, #44396, #76150, .T. ) ;
#57840 = AXIS2_PLACEMENT_3D ( 'NONE', #70121, #113071, #252562 ) ;
#57841 = ORIENTED_EDGE ( 'NONE', *, *, #24617, .T. ) ;
#57842 = CARTESIAN_POINT ( 'NONE',  ( 18.69999999999999929, -10.74999999999999289, 32.89999999999999858 ) ) ;
#57843 = CARTESIAN_POINT ( 'NONE',  ( -21.05000000000000071, 13.60254931771583387, -238.7443143987590304 ) ) ;
#57844 = ORIENTED_EDGE ( 'NONE', *, *, #153022, .F. ) ;
#57846 = ADVANCED_FACE ( 'NONE', ( #164693 ), #223362, .T. ) ;
#57845 = VERTEX_POINT ( 'NONE', #206388 ) ;
#57847 = AXIS2_PLACEMENT_3D ( 'NONE', #38283, #255982, #215616 ) ;
#57848 = CIRCLE ( 'NONE', #74485, 2.000000000000001776 ) ;
#57850 = VERTEX_POINT ( 'NONE', #203809 ) ;
#57849 = AXIS2_PLACEMENT_3D ( 'NONE', #87274, #166869, #169440 ) ;
#57852 = DIRECTION ( 'NONE',  ( -1.000000000000000000, 0.000000000000000000, 0.000000000000000000 ) ) ;
#57851 = AXIS2_PLACEMENT_3D ( 'NONE', #27929, #106122, #68314 ) ;
#57853 = DIRECTION ( 'NONE',  ( 2.940209281316622495E-16, -1.000000000000000000, -2.352167425053297996E-15 ) ) ;
#57854 = CARTESIAN_POINT ( 'NONE',  ( -20.94999999999999929, 77.16270174994961906, -61.42310748452431568 ) ) ;
#57855 = DIRECTION ( 'NONE',  ( 1.000000000000000000, -0.000000000000000000, 0.000000000000000000 ) ) ;
#57856 = CIRCLE ( 'NONE', #149675, 0.09999999999999939493 ) ;
#57858 = AXIS2_PLACEMENT_3D ( 'NONE', #8959, #185025, #6386 ) ;
#57857 = DIRECTION ( 'NONE',  ( 1.000000000000000000, 0.000000000000000000, 0.000000000000000000 ) ) ;
#57859 = DIRECTION ( 'NONE',  ( -1.000000000000000000, -1.836970198721029934E-16, 0.000000000000000000 ) ) ;
#57861 = EDGE_CURVE ( 'NONE', #654, #135929, #82544, .T. ) ;
#57860 = CARTESIAN_POINT ( 'NONE',  ( 20.12500000000000355, 9.258049272917324046, -8.363338837142434201 ) ) ;
#57863 = CARTESIAN_POINT ( 'NONE',  ( -21.14999999999999858, 60.94483358488582070, -234.0465764481390636 ) ) ;
#57862 = DIRECTION ( 'NONE',  ( 0.000000000000000000, 1.265107689135680095E-16, -1.000000000000000000 ) ) ;
#57864 = DIRECTION ( 'NONE',  ( 0.000000000000000000, -0.9126074666063772600, -0.4088369013363274407 ) ) ;
#57865 = CARTESIAN_POINT ( 'NONE',  ( -15.75000000000000355, 66.15000000001155911, -52.77310748452439526 ) ) ;
#57866 = AXIS2_PLACEMENT_3D ( 'NONE', #228049, #211054, #166822 ) ;
#57867 = DIRECTION ( 'NONE',  ( -1.000000000000000000, -0.000000000000000000, -0.000000000000000000 ) ) ;
#57868 = LINE ( 'NONE', #464, #196803 ) ;
#57869 = ORIENTED_EDGE ( 'NONE', *, *, #177064, .F. ) ;
#57870 = AXIS2_PLACEMENT_3D ( 'NONE', #160586, #240099, #57583 ) ;
#57871 = CIRCLE ( 'NONE', #37079, 2.000000000000002665 ) ;
#57872 = PRESENTATION_LAYER_ASSIGNMENT (  '', '', ( #137011 ) ) ;
#57873 = EDGE_CURVE ( 'NONE', #142401, #21983, #73654, .T. ) ;
#57875 = ORIENTED_EDGE ( 'NONE', *, *, #124284, .T. ) ;
#57874 = DIRECTION ( 'NONE',  ( 0.000000000000000000, 0.5000000000000078826, -0.8660254037844340447 ) ) ;
#57876 = CIRCLE ( 'NONE', #37084, 0.09999999999999939493 ) ;
#57877 = DIRECTION ( 'NONE',  ( -3.265361837132813093E-16, 1.000000000000000000, 0.000000000000000000 ) ) ;
#57878 = EDGE_CURVE ( 'NONE', #214666, #21932, #19482, .T. ) ;
#57879 = ADVANCED_FACE ( 'NONE', ( #227223 ), #218795, .F. ) ;
#57880 = DIRECTION ( 'NONE',  ( -1.000000000000000000, 0.000000000000000000, 0.000000000000000000 ) ) ;
#57881 = ORIENTED_EDGE ( 'NONE', *, *, #22593, .T. ) ;
#57882 = CARTESIAN_POINT ( 'NONE',  ( 22.60000000000000142, 76.00000000001165290, -69.52310748452431710 ) ) ;
#57883 = CARTESIAN_POINT ( 'NONE',  ( -16.88005004766534967, 9.950100503321044343, -20.85033611194876002 ) ) ;
#57884 = CIRCLE ( 'NONE', #166279, 0.9750000000000036415 ) ;
#57885 = ORIENTED_EDGE ( 'NONE', *, *, #44065, .F. ) ;
#57887 = ADVANCED_FACE ( 'NONE', ( #26475 ), #123006, .F. ) ;
#57886 = EDGE_CURVE ( 'NONE', #182465, #242065, #185538, .T. ) ;
#57888 = CARTESIAN_POINT ( 'NONE',  ( -18.50000324121759121, 10.29307482169070909, -206.4586421466939896 ) ) ;
#57889 = LINE ( 'NONE', #253529, #63045 ) ;
#57890 = EDGE_CURVE ( 'NONE', #128969, #24871, #231305, .T. ) ;
#57891 = CARTESIAN_POINT ( 'NONE',  ( -20.94999999999999929, 0.000000000000000000, 0.000000000000000000 ) ) ;
#57892 = LINE ( 'NONE', #136133, #103592 ) ;
#57894 = EDGE_LOOP ( 'NONE', ( #129407, #172917, #61254, #131328 ) ) ;
#57893 = DIRECTION ( 'NONE',  ( -1.000000000000000000, -0.000000000000000000, 0.000000000000000000 ) ) ;
#57895 = EDGE_CURVE ( 'NONE', #59389, #152420, #185498, .T. ) ;
#57897 = ORIENTED_EDGE ( 'NONE', *, *, #10066, .T. ) ;
#57896 = DIRECTION ( 'NONE',  ( -0.000000000000000000, 6.982962677686266711E-15, -1.000000000000000000 ) ) ;
#57898 = AXIS2_PLACEMENT_3D ( 'NONE', #48033, #128874, #209684 ) ;
#57899 = DIRECTION ( 'NONE',  ( 1.000000000000000000, 0.000000000000000000, 0.000000000000000000 ) ) ;
#57900 = CARTESIAN_POINT ( 'NONE',  ( 21.05000000000000071, 10.72371710470752149, -12.15000000000000036 ) ) ;
#57901 = DIRECTION ( 'NONE',  ( -1.000000000000000000, 0.000000000000000000, -0.000000000000000000 ) ) ;
#57902 = CIRCLE ( 'NONE', #137213, 7.900000000000002132 ) ;
#57903 = EDGE_CURVE ( 'NONE', #3992, #160216, #125559, .T. ) ;
#57905 = LINE ( 'NONE', #14966, #66656 ) ;
#57904 = CARTESIAN_POINT ( 'NONE',  ( -16.83233564386398839, 9.930221796595855466, -154.7245206634761132 ) ) ;
#57906 = CARTESIAN_POINT ( 'NONE',  ( -16.94275863009466576, 66.01050395135021631, -190.9148048665655324 ) ) ;
#57907 = CIRCLE ( 'NONE', #212067, 0.2000000000000005107 ) ;
#57908 = CARTESIAN_POINT ( 'NONE',  ( 22.57856590037848576, -0.004128330053175016841, -155.7499415373246165 ) ) ;
#57909 = CARTESIAN_POINT ( 'NONE',  ( 18.59999999999999076, 69.35000000001151932, -48.27310748452436684 ) ) ;
#57910 = CARTESIAN_POINT ( 'NONE',  ( 21.12642695952774119, 0.09890328320052040045, -161.1243400779648027 ) ) ;
#57911 = CARTESIAN_POINT ( 'NONE',  ( 21.09316766718127667, 10.10216385852922194, -228.0989014875141265 ) ) ;
#57912 = EDGE_CURVE ( 'NONE', #48255, #138529, #202699, .T. ) ;
#57913 = EDGE_CURVE ( 'NONE', #223699, #45489, #243752, .T. ) ;
#57915 = VERTEX_POINT ( 'NONE', #48584 ) ;
#57914 = AXIS2_PLACEMENT_3D ( 'NONE', #11104, #211886, #213145 ) ;
#57916 = CARTESIAN_POINT ( 'NONE',  ( -21.05000000000000071, 1.115600667400684642E-11, -100.5000000000000284 ) ) ;
#57917 = VERTEX_POINT ( 'NONE', #104673 ) ;
#57918 = ORIENTED_EDGE ( 'NONE', *, *, #115872, .T. ) ;
#57919 = EDGE_CURVE ( 'NONE', #199102, #82775, #152204, .T. ) ;
#57920 = DIRECTION ( 'NONE',  ( -0.000000000000000000, -0.000000000000000000, 1.000000000000000000 ) ) ;
#57921 = CARTESIAN_POINT ( 'NONE',  ( 23.14999999999999503, 64.35000000001176090, -76.53791325517833855 ) ) ;
#57922 = ORIENTED_EDGE ( 'NONE', *, *, #44395, .F. ) ;
#57923 = EDGE_CURVE ( 'NONE', #204353, #55259, #22631, .T. ) ;
#57924 = AXIS2_PLACEMENT_3D ( 'NONE', #227318, #186943, #108659 ) ;
#57925 = EDGE_CURVE ( 'NONE', #56502, #187906, #4311, .T. ) ;
#57926 = EDGE_LOOP ( 'NONE', ( #112584, #193582, #154192, #345 ) ) ;
#57927 = TOROIDAL_SURFACE ( 'NONE', #170247, 0.6000000000000006439, 0.1000000000000000056 ) ;
#57928 = EDGE_CURVE ( 'NONE', #53442, #114232, #14837, .T. ) ;
#57929 = ORIENTED_EDGE ( 'NONE', *, *, #117338, .T. ) ;
#57930 = AXIS2_PLACEMENT_3D ( 'NONE', #45071, #124616, #185862 ) ;
#57931 = VERTEX_POINT ( 'NONE', #129412 ) ;
#57932 = CARTESIAN_POINT ( 'NONE',  ( -23.15000000000000213, 0.000000000000000000, -33.50000000000000000 ) ) ;
#57933 = SPHERICAL_SURFACE ( 'NONE', #86931, 0.1000000000000000056 ) ;
#57934 = DIRECTION ( 'NONE',  ( 0.000000000000000000, -1.000000000000000000, 0.000000000000000000 ) ) ;
#57935 = CARTESIAN_POINT ( 'NONE',  ( -23.25000000000000000, 1.999999999999998224, -13.22462192276210224 ) ) ;
#57936 = CARTESIAN_POINT ( 'NONE',  ( 14.87567385445977486, 9.430764995422318719, -15.23053739475045809 ) ) ;
#57937 = PLANE ( 'NONE',  #137533 ) ;
#57939 = ORIENTED_EDGE ( 'NONE', *, *, #45729, .F. ) ;
#57938 = DIRECTION ( 'NONE',  ( -1.000000000000000000, -2.952720810173289112E-16, 0.000000000000000000 ) ) ;
#57941 = DIRECTION ( 'NONE',  ( -1.000000000000000000, 0.000000000000000000, 0.000000000000000000 ) ) ;
#57940 = LINE ( 'NONE', #197463, #254557 ) ;
#57942 = EDGE_CURVE ( 'NONE', #176041, #110939, #160585, .T. ) ;
#57943 = CARTESIAN_POINT ( 'NONE',  ( 21.05000000000000071, 64.35000000001237197, -169.9231074845244507 ) ) ;
#57944 = ADVANCED_FACE ( 'NONE', ( #171159 ), #32929, .F. ) ;
#57945 = VERTEX_POINT ( 'NONE', #130689 ) ;
#57946 = DIRECTION ( 'NONE',  ( 0.000000000000000000, 1.000000000000000000, 0.000000000000000000 ) ) ;
#57947 = CARTESIAN_POINT ( 'NONE',  ( -23.25000000000000000, 5.950000000011167245, -90.19429769496522908 ) ) ;
#57948 = ORIENTED_EDGE ( 'NONE', *, *, #72787, .T. ) ;
#57950 = FACE_OUTER_BOUND ( 'NONE', #162349, .T. ) ;
#57949 = DIRECTION ( 'NONE',  ( 0.000000000000000000, 0.000000000000000000, -1.000000000000000000 ) ) ;
#57951 = VECTOR ( 'NONE', #14164, 1000.000000000000000 ) ;
#57952 = DIRECTION ( 'NONE',  ( 0.000000000000000000, 0.000000000000000000, -1.000000000000000000 ) ) ;
#57953 = CARTESIAN_POINT ( 'NONE',  ( -17.11825945287481332, 65.95000000001152785, -48.77310748452439526 ) ) ;
#57954 = ORIENTED_EDGE ( 'NONE', *, *, #133036, .T. ) ;
#57955 = EDGE_LOOP ( 'NONE', ( #143602, #12772, #107182, #174390 ) ) ;
#57956 = CARTESIAN_POINT ( 'NONE',  ( 23.15000000000000213, -11.64999999998883595, -122.2500000000000284 ) ) ;
#57957 = CARTESIAN_POINT ( 'NONE',  ( -18.44232395690005433, -0.7486215172606220936, -242.4509705927298171 ) ) ;
#57958 = DIRECTION ( 'NONE',  ( 1.000000000000000000, 0.000000000000000000, 0.000000000000000000 ) ) ;
#57959 = LINE ( 'NONE', #97062, #151081 ) ;
#57960 = VERTEX_POINT ( 'NONE', #250631 ) ;
#57961 = DIRECTION ( 'NONE',  ( 0.000000000000000000, 0.5000000000000078826, -0.8660254037844340447 ) ) ;
#57962 = CIRCLE ( 'NONE', #3826, 2.000000000000002665 ) ;
#57963 = EDGE_CURVE ( 'NONE', #51689, #20074, #91575, .T. ) ;
#57964 = DIRECTION ( 'NONE',  ( 0.000000000000000000, -6.982962677686266711E-15, 1.000000000000000000 ) ) ;
#57965 = AXIS2_PLACEMENT_3D ( 'NONE', #152868, #232390, #133268 ) ;
#57966 = AXIS2_PLACEMENT_3D ( 'NONE', #11209, #33374, #95853 ) ;
#57967 = VECTOR ( 'NONE', #166345, 1000.000000000000000 ) ;
#57968 = FACE_OUTER_BOUND ( 'NONE', #228042, .T. ) ;
#57969 = EDGE_CURVE ( 'NONE', #75011, #202644, #193875, .T. ) ;
#57970 = DIRECTION ( 'NONE',  ( -1.652117596168391700E-15, -1.000000000000000000, 0.000000000000000000 ) ) ;
#57972 = ORIENTED_EDGE ( 'NONE', *, *, #111590, .T. ) ;
#57971 = CARTESIAN_POINT ( 'NONE',  ( -20.94999999999999929, -1.162701749926853712, -75.10000000000003695 ) ) ;
#57973 = VECTOR ( 'NONE', #194630, 1000.000000000000000 ) ;
#57974 = CARTESIAN_POINT ( 'NONE',  ( -20.94999999999999929, 87.29603075034673054, -39.07100664418810965 ) ) ;
#57975 = DIRECTION ( 'NONE',  ( 1.000000000000000000, 0.000000000000000000, 0.000000000000000000 ) ) ;
#57976 = CARTESIAN_POINT ( 'NONE',  ( 18.54286124688533377, 77.31795877665247474, -241.8819332742536972 ) ) ;
#57977 = LINE ( 'NONE', #137515, #97009 ) ;
#57978 = CARTESIAN_POINT ( 'NONE',  ( -21.05000000000000071, 1.162701749949165642, -175.5999999999999659 ) ) ;
#57980 = ORIENTED_EDGE ( 'NONE', *, *, #44030, .F. ) ;
#57979 = DIRECTION ( 'NONE',  ( 0.000000000000000000, 1.000000000000000000, 6.982962677686266711E-15 ) ) ;
#57981 = CARTESIAN_POINT ( 'NONE',  ( -20.64999999999999858, 85.00000000001149658, -45.91707660717669626 ) ) ;
#57982 = CARTESIAN_POINT ( 'NONE',  ( -18.40000000000000213, 11.47316190336247388, -12.55000000000000249 ) ) ;
#57983 = CARTESIAN_POINT ( 'NONE',  ( 20.94999675878240808, 67.49461024981995649, -195.5605382655040216 ) ) ;
#57984 = EDGE_LOOP ( 'NONE', ( #213048, #129397, #145971, #150721 ) ) ;
#57985 = DIRECTION ( 'NONE',  ( 1.000000000000000000, -0.000000000000000000, -0.000000000000000000 ) ) ;
#57986 = FACE_OUTER_BOUND ( 'NONE', #205361, .T. ) ;
#57987 = DIRECTION ( 'NONE',  ( -0.000000000000000000, -0.4088369013363281068, 0.9126074666063770380 ) ) ;
#57988 = CIRCLE ( 'NONE', #107884, 0.5000000000000004441 ) ;
#57989 = AXIS2_PLACEMENT_3D ( 'NONE', #65330, #234684, #131729 ) ;
#57990 = CARTESIAN_POINT ( 'NONE',  ( 23.14999999999999503, 6.550000000000000711, -21.25000000000000000 ) ) ;
#57991 = VECTOR ( 'NONE', #188607, 1000.000000000000000 ) ;
#57992 = ADVANCED_FACE ( 'NONE', ( #72023 ), #154161, .T. ) ;
#57993 = CARTESIAN_POINT ( 'NONE',  ( -18.50000000000000000, 66.65000000001157332, -57.17310748452438673 ) ) ;
#57994 = DIRECTION ( 'NONE',  ( 3.265361837132812600E-16, -0.4721928772777346239, -0.8814952561688430555 ) ) ;
#57995 = AXIS2_PLACEMENT_3D ( 'NONE', #75898, #251958, #96706 ) ;
#57996 = ORIENTED_EDGE ( 'NONE', *, *, #85520, .T. ) ;
#57997 = ORIENTED_EDGE ( 'NONE', *, *, #44138, .F. ) ;
#57998 = CARTESIAN_POINT ( 'NONE',  ( 20.94999999999999574, 2.923777413779037548, -208.5507632484912222 ) ) ;
#57999 = CARTESIAN_POINT ( 'NONE',  ( -23.15000000000000213, 4.150000000011156764, -155.1500000000000057 ) ) ;
#58000 = DIRECTION ( 'NONE',  ( -1.000000000000000000, -0.000000000000000000, -0.000000000000000000 ) ) ;
#58001 = VERTEX_POINT ( 'NONE', #73329 ) ;
#58002 = DIRECTION ( 'NONE',  ( 1.000000000000000000, -0.000000000000000000, -0.000000000000000000 ) ) ;
#58003 = CARTESIAN_POINT ( 'NONE',  ( 18.59999999999999787, 45.93315328338058379, -256.6017782078560003 ) ) ;
#58004 = B_SPLINE_CURVE_WITH_KNOTS ( 'NONE', 3,
 ( #145102, #109827, #10750, #190696, #130683, #147690 ),
 .UNSPECIFIED., .F., .F.,
 ( 4, 2, 4 ),
 ( 1.138412281109779656E-18, 0.0001569047307838639788, 0.0003138094615677267650 ),
 .UNSPECIFIED. ) ;
#58005 = CARTESIAN_POINT ( 'NONE',  ( -16.79814274880124358, 9.949272542677302766, -12.65243303704799693 ) ) ;
#58007 = CARTESIAN_POINT ( 'NONE',  ( -20.85000000000000142, 65.66751761918619934, -30.42826094061123854 ) ) ;
#58006 = AXIS2_PLACEMENT_3D ( 'NONE', #38837, #21834, #119659 ) ;
#58008 = ORIENTED_EDGE ( 'NONE', *, *, #16433, .F. ) ;
#58009 = DIRECTION ( 'NONE',  ( 0.000000000000000000, 3.469446951953995998E-14, 1.000000000000000000 ) ) ;
#58010 = EDGE_LOOP ( 'NONE', ( #170531, #141891, #220498, #147487 ) ) ;
#58011 = ORIENTED_EDGE ( 'NONE', *, *, #90939, .T. ) ;
#58012 = DIRECTION ( 'NONE',  ( 2.259780016855444047E-14, 0.6052030477779081208, 0.7960711469211347868 ) ) ;
#58013 = CARTESIAN_POINT ( 'NONE',  ( -21.05000000000000071, 6.440770893673045450, -100.5175971870084908 ) ) ;
#58014 = FACE_OUTER_BOUND ( 'NONE', #212031, .T. ) ;
#58015 = CIRCLE ( 'NONE', #253838, 0.1000000000000028644 ) ;
#58016 = ORIENTED_EDGE ( 'NONE', *, *, #194843, .F. ) ;
#58017 = DIRECTION ( 'NONE',  ( -0.000000000000000000, 0.2128009952263597848, -0.9770955615653316162 ) ) ;
#58018 = CARTESIAN_POINT ( 'NONE',  ( 23.14999999999999858, 5.600000000011153389, -155.0947339810869323 ) ) ;
#58019 = CARTESIAN_POINT ( 'NONE',  ( -20.85000000000000142, -11.74999999998884448, -200.9999999999999432 ) ) ;
#58020 = EDGE_CURVE ( 'NONE', #126808, #60368, #181422, .T. ) ;
#58021 = ORIENTED_EDGE ( 'NONE', *, *, #101947, .T. ) ;
#58022 = DIRECTION ( 'NONE',  ( 0.000000000000000000, 0.000000000000000000, -1.000000000000000000 ) ) ;
#58024 = ORIENTED_EDGE ( 'NONE', *, *, #122478, .F. ) ;
#58023 = CARTESIAN_POINT ( 'NONE',  ( 18.49999999999999289, 65.76093837589073132, -145.2687100499267387 ) ) ;
#58026 = EDGE_CURVE ( 'NONE', #161169, #67174, #68760, .T. ) ;
#58025 = DIRECTION ( 'NONE',  ( 0.000000000000000000, 1.776356839400310418E-15, -1.000000000000000000 ) ) ;
#58027 = DIRECTION ( 'NONE',  ( -1.000000000000000000, -2.885090398161910739E-16, -6.283419270304611573E-17 ) ) ;
#58028 = CIRCLE ( 'NONE', #124701, 0.09999999999999938105 ) ;
#58029 = CONICAL_SURFACE ( 'NONE', #32983, 4.000000000000000000, 0.7853981633974489451 ) ;
#58030 = CIRCLE ( 'NONE', #120622, 0.09999999999999108213 ) ;
#58031 = ORIENTED_EDGE ( 'NONE', *, *, #219934, .T. ) ;
#58032 = DIRECTION ( 'NONE',  ( 1.000000000000000000, 0.000000000000000000, 0.000000000000000000 ) ) ;
#58034 = EDGE_CURVE ( 'NONE', #253110, #200640, #77590, .T. ) ;
#58033 = DIRECTION ( 'NONE',  ( 0.000000000000000000, 0.000000000000000000, 1.000000000000000000 ) ) ;
#58035 = DIRECTION ( 'NONE',  ( 1.000000000000000000, 0.000000000000000000, -0.000000000000000000 ) ) ;
#58036 = ORIENTED_EDGE ( 'NONE', *, *, #48729, .T. ) ;
#58037 = CARTESIAN_POINT ( 'NONE',  ( 21.05000000000000071, 5.399999999999998579, -21.09473398108690390 ) ) ;
#58039 = EDGE_CURVE ( 'NONE', #184752, #177157, #172438, .T. ) ;
#58038 = CARTESIAN_POINT ( 'NONE',  ( 13.77030915526558275, 49.66582466164801701, -233.3627041834999432 ) ) ;
#58040 = DIRECTION ( 'NONE',  ( -1.000000000000000000, 0.000000000000000000, 0.000000000000000000 ) ) ;
#58041 = AXIS2_PLACEMENT_3D ( 'NONE', #35229, #156465, #78153 ) ;
#58042 = VECTOR ( 'NONE', #221257, 1000.000000000000000 ) ;
#58043 = ORIENTED_EDGE ( 'NONE', *, *, #132402, .F. ) ;
#58044 = EDGE_CURVE ( 'NONE', #125708, #117495, #133271, .T. ) ;
#58045 = ORIENTED_EDGE ( 'NONE', *, *, #165306, .T. ) ;
#58046 = AXIS2_PLACEMENT_3D ( 'NONE', #147082, #67561, #184942 ) ;
#58047 = VECTOR ( 'NONE', #55750, 1000.000000000000000 ) ;
#58048 = CIRCLE ( 'NONE', #82983, 0.1000000000000054040 ) ;
#58049 = ORIENTED_EDGE ( 'NONE', *, *, #222285, .F. ) ;
#58050 = FACE_OUTER_BOUND ( 'NONE', #38912, .T. ) ;
#58051 = AXIS2_PLACEMENT_3D ( 'NONE', #13330, #233665, #134530 ) ;
#58053 = EDGE_CURVE ( 'NONE', #177294, #145739, #81579, .T. ) ;
#58052 = CARTESIAN_POINT ( 'NONE',  ( 21.06277459767431992, 8.872862438279399910, -45.70399919235632069 ) ) ;
#58055 = EDGE_LOOP ( 'NONE', ( #129352, #224284, #14573, #156041 ) ) ;
#58054 = LINE ( 'NONE', #115476, #75175 ) ;
#58056 = LINE ( 'NONE', #13820, #107382 ) ;
#58057 = LINE ( 'NONE', #41113, #94807 ) ;
#58058 = FACE_OUTER_BOUND ( 'NONE', #127759, .T. ) ;
#58059 = CARTESIAN_POINT ( 'NONE',  ( -18.39999999999999858, 64.52683809664961245, -127.1971614177164156 ) ) ;
#58060 = DIRECTION ( 'NONE',  ( 0.000000000000000000, 0.8814952561688429444, -0.4721928772777345684 ) ) ;
#58061 = CARTESIAN_POINT ( 'NONE',  ( 18.59999999999999076, 69.45000000001149942, -48.27310748452436684 ) ) ;
#58063 = ORIENTED_EDGE ( 'NONE', *, *, #79868, .T. ) ;
#58062 = CARTESIAN_POINT ( 'NONE',  ( -20.64999999999999858, 85.00000000001222134, -146.4170766071767389 ) ) ;
#58065 = ORIENTED_EDGE ( 'NONE', *, *, #219234, .T. ) ;
#58064 = CARTESIAN_POINT ( 'NONE',  ( -18.50000000000000000, -1.835341550213255957, -112.0551512925630107 ) ) ;
#58067 = CARTESIAN_POINT ( 'NONE',  ( -16.77431908686106610, 51.60765445881215641, -231.9560861657696194 ) ) ;
#58066 = CARTESIAN_POINT ( 'NONE',  ( -16.94878442675512176, 60.88907946405466731, -221.0676920639221805 ) ) ;
#58069 = ORIENTED_EDGE ( 'NONE', *, *, #93472, .F. ) ;
#58068 = DIRECTION ( 'NONE',  ( -1.000000000000000000, -0.000000000000000000, -0.000000000000000000 ) ) ;
#58070 = VERTEX_POINT ( 'NONE', #54987 ) ;
#58071 = DIRECTION ( 'NONE',  ( 1.000000000000000000, 0.000000000000000000, 0.000000000000000000 ) ) ;
#58072 = VECTOR ( 'NONE', #89971, 1000.000000000000000 ) ;
#58073 = DIRECTION ( 'NONE',  ( 1.000000000000000000, 0.000000000000000000, 0.000000000000000000 ) ) ;
#58074 = DIRECTION ( 'NONE',  ( -1.000000000000000000, 0.000000000000000000, 0.000000000000000000 ) ) ;
#58075 = DIRECTION ( 'NONE',  ( 0.000000000000000000, -0.000000000000000000, -1.000000000000000000 ) ) ;
#58076 = DIRECTION ( 'NONE',  ( 0.000000000000000000, 1.000000000000000000, 0.000000000000000000 ) ) ;
#58077 = CARTESIAN_POINT ( 'NONE',  ( -15.55912972643741199, 67.50912972644972854, -157.4731074845244336 ) ) ;
#58078 = AXIS2_PLACEMENT_3D ( 'NONE', #226460, #252139, #206928 ) ;
#58079 = FACE_OUTER_BOUND ( 'NONE', #84319, .T. ) ;
#58080 = EDGE_LOOP ( 'NONE', ( #211951, #119044, #212154, #157284, #183470, #81090, #193201, #190199, #132479, #137600 ) ) ;
#58081 = ORIENTED_EDGE ( 'NONE', *, *, #114941, .F. ) ;
#58082 = CARTESIAN_POINT ( 'NONE',  ( -23.15000000000000213, 61.57587952878036219, -212.2000740415318774 ) ) ;
#58083 = AXIS2_PLACEMENT_3D ( 'NONE', #34663, #54191, #72500 ) ;
#58084 = ORIENTED_EDGE ( 'NONE', *, *, #81939, .T. ) ;
#58085 = CARTESIAN_POINT ( 'NONE',  ( -21.05000000000000071, 70.47363787294415260, -228.3418745167492432 ) ) ;
#58086 = CARTESIAN_POINT ( 'NONE',  ( -23.25000000000000000, 69.01799029515598249, -166.3269553662681233 ) ) ;
#58087 = VECTOR ( 'NONE', #164448, 1000.000000000000000 ) ;
#58089 = EDGE_CURVE ( 'NONE', #244818, #226285, #14627, .T. ) ;
#58088 = CARTESIAN_POINT ( 'NONE',  ( 21.53699400383916185, 76.00000000001243450, -176.8108192777720831 ) ) ;
#58090 = CYLINDRICAL_SURFACE ( 'NONE', #22114, 0.09999999999999939493 ) ;
#58091 = VERTEX_POINT ( 'NONE', #207682 ) ;
#58092 = CARTESIAN_POINT ( 'NONE',  ( -12.26136940704871670, 66.64859682587037071, -119.5435770476859005 ) ) ;
#58093 = ORIENTED_EDGE ( 'NONE', *, *, #181263, .F. ) ;
#58095 = EDGE_CURVE ( 'NONE', #173897, #172048, #218989, .T. ) ;
#58094 = CARTESIAN_POINT ( 'NONE',  ( 18.49999999999999645, 1.835341550224411922, -11.55515129256298046 ) ) ;
#58096 = ORIENTED_EDGE ( 'NONE', *, *, #107757, .F. ) ;
#58097 = AXIS2_PLACEMENT_3D ( 'NONE', #153639, #194012, #15375 ) ;
#58098 = DIRECTION ( 'NONE',  ( 0.000000000000000000, 0.000000000000000000, 1.000000000000000000 ) ) ;
#58099 = CARTESIAN_POINT ( 'NONE',  ( 18.40000000000000213, 8.812905490826908661, -245.4119551738195071 ) ) ;
#58100 = CIRCLE ( 'NONE', #45480, 0.1999999999999996503 ) ;
#58101 = EDGE_CURVE ( 'NONE', #211497, #30659, #227369, .T. ) ;
#58102 = DIRECTION ( 'NONE',  ( -0.7071067811865475727, -0.7071067811865475727, -0.000000000000000000 ) ) ;
#58103 = ADVANCED_FACE ( 'NONE', ( #114986 ), #120167, .T. ) ;
#58104 = ORIENTED_EDGE ( 'NONE', *, *, #53136, .F. ) ;
#58105 = CARTESIAN_POINT ( 'NONE',  ( -20.64999999999999858, 76.00000000001213607, -136.5231074845243313 ) ) ;
#58107 = ORIENTED_EDGE ( 'NONE', *, *, #49348, .T. ) ;
#58106 = CARTESIAN_POINT ( 'NONE',  ( -18.59999999999999787, 7.021664781911246322, -171.3335654018973173 ) ) ;
#58108 = CARTESIAN_POINT ( 'NONE',  ( 20.90000000000000213, 7.900000000000000355, 1.212568896937007867 ) ) ;
#58109 = ORIENTED_EDGE ( 'NONE', *, *, #176439, .T. ) ;
#58110 = CARTESIAN_POINT ( 'NONE',  ( -20.94999999999999929, 56.27731819600170837, -227.9967441372480721 ) ) ;
#58111 = ORIENTED_EDGE ( 'NONE', *, *, #164378, .F. ) ;
#58112 = ADVANCED_FACE ( 'NONE', ( #78418 ), #236213, .T. ) ;
#58113 = DIRECTION ( 'NONE',  ( -1.000000000000000000, 0.000000000000000000, 0.000000000000000000 ) ) ;
#58114 = CARTESIAN_POINT ( 'NONE',  ( 21.05000000000000071, 69.45934304831041572, -69.52310748452437394 ) ) ;
#58115 = DIRECTION ( 'NONE',  ( 0.000000000000000000, -6.982962677686266711E-15, 1.000000000000000000 ) ) ;
#58116 = CARTESIAN_POINT ( 'NONE',  ( -16.94309007106720344, 66.00777380744158052, -56.91731620196888741 ) ) ;
#58117 = EDGE_CURVE ( 'NONE', #182617, #132760, #148257, .T. ) ;
#58118 = CARTESIAN_POINT ( 'NONE',  ( -21.08035267497491816, 0.08268862478717949049, -60.66829316021700436 ) ) ;
#58119 = ORIENTED_EDGE ( 'NONE', *, *, #222955, .F. ) ;
#58120 = CARTESIAN_POINT ( 'NONE',  ( -13.39999999999994351, 67.65000000001118963, -16.98168612828748181 ) ) ;
#58121 = LINE ( 'NONE', #709, #207782 ) ;
#58122 = TOROIDAL_SURFACE ( 'NONE', #133177, 11.65000000000000036, 0.1000000000000000056 ) ;
#58123 = DIRECTION ( 'NONE',  ( 0.000000000000000000, -6.982962677686266711E-15, 1.000000000000000000 ) ) ;
#58124 = ORIENTED_EDGE ( 'NONE', *, *, #70060, .F. ) ;
#58125 = CARTESIAN_POINT ( 'NONE',  ( -18.59999999999999787, 64.35000000001190301, -96.00830171387039513 ) ) ;
#58126 = VERTEX_POINT ( 'NONE', #96671 ) ;
#58127 = CARTESIAN_POINT ( 'NONE',  ( 20.85000000000000142, 11.75000000001115907, -100.5000000000000426 ) ) ;
#58128 = ORIENTED_EDGE ( 'NONE', *, *, #113249, .T. ) ;
#58129 = DIRECTION ( 'NONE',  ( 0.000000000000000000, 0.8777080977375655291, -0.4791956752370622463 ) ) ;
#58130 = LINE ( 'NONE', #173022, #189502 ) ;
#58131 = ADVANCED_FACE ( 'NONE', ( #195837 ), #216654, .T. ) ;
#58133 = EDGE_LOOP ( 'NONE', ( #206701, #227972, #44438, #251496 ) ) ;
#58132 = CARTESIAN_POINT ( 'NONE',  ( 21.72449340488910607, 10.28395627750227703, -109.7500000000000426 ) ) ;
#58134 = EDGE_CURVE ( 'NONE', #170630, #179524, #110660, .T. ) ;
#58135 = DIRECTION ( 'NONE',  ( 0.000000000000000000, 0.000000000000000000, 1.000000000000000000 ) ) ;
#58136 = VERTEX_POINT ( 'NONE', #79694 ) ;
#58137 = ADVANCED_FACE ( 'NONE', ( #160562 ), #73285, .T. ) ;
#58138 = LINE ( 'NONE', #198951, #148421 ) ;
#58139 = CARTESIAN_POINT ( 'NONE',  ( 23.15000000000000213, 28.50120599808395028, -258.2149742250584268 ) ) ;
#58140 = EDGE_LOOP ( 'NONE', ( #148620, #95803, #92289 ) ) ;
#58141 = ORIENTED_EDGE ( 'NONE', *, *, #124089, .F. ) ;
#58142 = VECTOR ( 'NONE', #120608, 1000.000000000000114 ) ;
#58144 = VECTOR ( 'NONE', #79388, 1000.000000000000000 ) ;
#58143 = DIRECTION ( 'NONE',  ( 0.000000000000000000, -1.000000000000000000, -6.982962677686265922E-15 ) ) ;
#58145 = CARTESIAN_POINT ( 'NONE',  ( 23.14999999999999503, 14.10000000001115694, -195.3997023888606179 ) ) ;
#58146 = ORIENTED_EDGE ( 'NONE', *, *, #56660, .T. ) ;
#58147 = CIRCLE ( 'NONE', #208037, 0.1000000000000054040 ) ;
#58149 = LINE ( 'NONE', #178145, #228101 ) ;
#58148 = CIRCLE ( 'NONE', #12409, 0.09999999999999976963 ) ;
#58150 = ORIENTED_EDGE ( 'NONE', *, *, #145802, .T. ) ;
#58151 = ORIENTED_EDGE ( 'NONE', *, *, #22070, .F. ) ;
#58152 = DIRECTION ( 'NONE',  ( 0.000000000000000000, -0.9908441862701610203, 0.1350103645451807555 ) ) ;
#58153 = CIRCLE ( 'NONE', #158192, 0.5000000000000004441 ) ;
#58154 = CARTESIAN_POINT ( 'NONE',  ( -18.59999999999999787, 1.261786168576181755, -41.58649896354548048 ) ) ;
#58156 = VERTEX_POINT ( 'NONE', #137125 ) ;
#58155 = DIRECTION ( 'NONE',  ( 0.000000000000000000, -0.000000000000000000, -1.000000000000000000 ) ) ;
#58157 = DIRECTION ( 'NONE',  ( 0.000000000000000000, -0.2128009952263603954, 0.9770955615653315052 ) ) ;
#58158 = VECTOR ( 'NONE', #5026, 1000.000000000000000 ) ;
#58159 = FACE_OUTER_BOUND ( 'NONE', #211760, .T. ) ;
#58161 = ADVANCED_FACE ( 'NONE', ( #194557 ), #38047, .T. ) ;
#58160 = CARTESIAN_POINT ( 'NONE',  ( -16.81931177881022776, 63.07818495933808833, -213.2051305120939446 ) ) ;
#58162 = CIRCLE ( 'NONE', #4029, 0.5000000000000004441 ) ;
#58164 = CARTESIAN_POINT ( 'NONE',  ( 20.27550659511089037, 66.78395627750369101, -182.6731074845244223 ) ) ;
#58163 = CARTESIAN_POINT ( 'NONE',  ( 18.59999999999999076, 1.835341550235567887, -179.0551512925629538 ) ) ;
#58165 = DIRECTION ( 'NONE',  ( -0.5932847527679298016, 0.8049926720990051576, 0.000000000000000000 ) ) ;
#58166 = DIRECTION ( 'NONE',  ( 0.000000000000000000, -0.06430067914209719460, 0.9979305700607958851 ) ) ;
#58167 = DIRECTION ( 'NONE',  ( -1.000000000000000000, 6.938893903907270030E-14, 0.000000000000000000 ) ) ;
#58168 = DIRECTION ( 'NONE',  ( -0.000000000000000000, -6.982962677686266711E-15, 1.000000000000000000 ) ) ;
#58169 = VECTOR ( 'NONE', #187859, 1000.000000000000000 ) ;
#58170 = EDGE_LOOP ( 'NONE', ( #192955, #17772, #1752, #9079, #153877 ) ) ;
#58171 = ORIENTED_EDGE ( 'NONE', *, *, #24580, .F. ) ;
#58172 = DIRECTION ( 'NONE',  ( 0.000000000000000000, -0.2617529984165022361, -0.9651348961777160840 ) ) ;
#58174 = ORIENTED_EDGE ( 'NONE', *, *, #111020, .T. ) ;
#58173 = DIRECTION ( 'NONE',  ( -0.000000000000000000, 0.8103668758649578141, -0.5859227990963212784 ) ) ;
#58175 = EDGE_LOOP ( 'NONE', ( #109414, #75260 ) ) ;
#58176 = ADVANCED_FACE ( 'NONE', ( #177572 ), #235547, .T. ) ;
#58177 = CARTESIAN_POINT ( 'NONE',  ( 18.59999999999999076, 1.835341550235567887, -112.0551512925630249 ) ) ;
#58178 = VERTEX_POINT ( 'NONE', #17192 ) ;
#58179 = DIRECTION ( 'NONE',  ( 1.000000000000000000, 0.000000000000000000, 0.000000000000000000 ) ) ;
#58180 = ADVANCED_FACE ( 'NONE', ( #159271 ), #58837, .F. ) ;
#58181 = ORIENTED_EDGE ( 'NONE', *, *, #61408, .F. ) ;
#58183 = EDGE_CURVE ( 'NONE', #65123, #87825, #35486, .T. ) ;
#58182 = CYLINDRICAL_SURFACE ( 'NONE', #186603, 0.09999999999999939493 ) ;
#58184 = CIRCLE ( 'NONE', #87432, 7.791421356237341556 ) ;
#58186 = ORIENTED_EDGE ( 'NONE', *, *, #121612, .F. ) ;
#58185 = VERTEX_POINT ( 'NONE', #175015 ) ;
#58187 = VERTEX_POINT ( 'NONE', #198375 ) ;
#58188 = ORIENTED_EDGE ( 'NONE', *, *, #217165, .T. ) ;
#58189 = ORIENTED_EDGE ( 'NONE', *, *, #49932, .F. ) ;
#58190 = ADVANCED_FACE ( 'NONE', ( #60135 ), #36777, .F. ) ;
#58191 = FACE_OUTER_BOUND ( 'NONE', #153195, .T. ) ;
#58192 = CARTESIAN_POINT ( 'NONE',  ( 22.39999999999999503, 75.90000000001219860, -144.3138870828976792 ) ) ;
#58195 = EDGE_CURVE ( 'NONE', #88325, #93493, #116289, .T. ) ;
#58194 = ORIENTED_EDGE ( 'NONE', *, *, #71457, .F. ) ;
#58193 = CARTESIAN_POINT ( 'NONE',  ( -18.40000000000000213, 64.25000000001179501, -78.77310748452438816 ) ) ;
#58196 = AXIS2_PLACEMENT_3D ( 'NONE', #112462, #32953, #210275 ) ;
#58197 = CARTESIAN_POINT ( 'NONE',  ( 21.00000000000000000, 9.750000000011153745, -79.35000000000005116 ) ) ;
#58198 = CARTESIAN_POINT ( 'NONE',  ( 14.22821877134046353, 12.43384112479209413, -213.6551227491177372 ) ) ;
#58200 = VERTEX_POINT ( 'NONE', #75862 ) ;
#58199 = CARTESIAN_POINT ( 'NONE',  ( -22.39999999999999858, 7.790779598384560245, -100.4000000000000341 ) ) ;
#58201 = DIRECTION ( 'NONE',  ( 0.000000000000000000, 0.000000000000000000, 1.000000000000000000 ) ) ;
#58202 = ORIENTED_EDGE ( 'NONE', *, *, #95806, .T. ) ;
#58203 = DIRECTION ( 'NONE',  ( -1.000000000000000000, 0.000000000000000000, 0.000000000000000000 ) ) ;
#58205 = EDGE_LOOP ( 'NONE', ( #210021, #12744, #134562, #9658 ) ) ;
#58204 = CYLINDRICAL_SURFACE ( 'NONE', #18759, 0.1000000000000008105 ) ;
#58206 = LINE ( 'NONE', #21679, #206092 ) ;
#58207 = CARTESIAN_POINT ( 'NONE',  ( 20.94999999999999929, 5.399999999999998579, -21.09473398108690390 ) ) ;
#58208 = CARTESIAN_POINT ( 'NONE',  ( -18.59999999999999787, 59.50933445848280456, -243.9217804674669310 ) ) ;
#58209 = VERTEX_POINT ( 'NONE', #176274 ) ;
#58211 = CARTESIAN_POINT ( 'NONE',  ( 20.94999999999999574, 87.65000000001191438, -99.92310748452422331 ) ) ;
#58210 = CARTESIAN_POINT ( 'NONE',  ( -16.85697194749129579, 9.908543714134824043, -46.43500426761385569 ) ) ;
#58212 = CARTESIAN_POINT ( 'NONE',  ( -15.51798037960204724, 66.62334006147830223, -85.39491493630713137 ) ) ;
#58213 = DIRECTION ( 'NONE',  ( 0.000000000000000000, -0.9770955615653316162, -0.2128009952263604232 ) ) ;
#58214 = ADVANCED_FACE ( 'NONE', ( #255736 ), #98154, .F. ) ;
#58215 = CARTESIAN_POINT ( 'NONE',  ( 23.24999999999999645, 70.40000000001157332, -57.11784146561127073 ) ) ;
#58216 = CARTESIAN_POINT ( 'NONE',  ( 22.10000000000000497, -11.75000000000000000, -15.00000000000000000 ) ) ;
#58218 = EDGE_CURVE ( 'NONE', #234494, #105159, #27510, .T. ) ;
#58217 = AXIS2_PLACEMENT_3D ( 'NONE', #92376, #14162, #229346 ) ;
#58219 = ORIENTED_EDGE ( 'NONE', *, *, #80637, .T. ) ;
#58220 = ORIENTED_EDGE ( 'NONE', *, *, #19344, .T. ) ;
#58221 = EDGE_LOOP ( 'NONE', ( #146090, #190715, #30536, #177692 ) ) ;
#58222 = CARTESIAN_POINT ( 'NONE',  ( -21.05000000000000071, -0.02110330804822888387, -127.6954836707355270 ) ) ;
#58223 = CARTESIAN_POINT ( 'NONE',  ( -23.25000000000000000, 1.115600667400684642E-11, -71.05000000000003979 ) ) ;
#58224 = EDGE_LOOP ( 'NONE', ( #57336, #210919, #155205, #69408 ) ) ;
#58226 = CARTESIAN_POINT ( 'NONE',  ( 23.24999999999999645, 11.75000000001113953, -79.65000000000004832 ) ) ;
#58225 = VECTOR ( 'NONE', #234030, 1000.000000000000000 ) ;
#58227 = ORIENTED_EDGE ( 'NONE', *, *, #110515, .T. ) ;
#58228 = EDGE_CURVE ( 'NONE', #5557, #4296, #131503, .T. ) ;
#58229 = DIRECTION ( 'NONE',  ( 0.000000000000000000, 0.7071067811865473507, -0.7071067811865477948 ) ) ;
#58230 = LINE ( 'NONE', #20426, #121079 ) ;
#58231 = VECTOR ( 'NONE', #218303, 1000.000000000000000 ) ;
#58232 = AXIS2_PLACEMENT_3D ( 'NONE', #207525, #9304, #28922 ) ;
#58233 = ADVANCED_FACE ( 'NONE', ( #26176 ), #163124, .T. ) ;
#58234 = ORIENTED_EDGE ( 'NONE', *, *, #254583, .F. ) ;
#58235 = CARTESIAN_POINT ( 'NONE',  ( -21.10000000000000142, 6.223900101154156594, 12.00000000000000000 ) ) ;
#58236 = ADVANCED_FACE ( 'NONE', ( #64004 ), #123992, .T. ) ;
#58238 = ORIENTED_EDGE ( 'NONE', *, *, #254840, .F. ) ;
#58237 = AXIS2_PLACEMENT_3D ( 'NONE', #141652, #101197, #242033 ) ;
#58239 = VERTEX_POINT ( 'NONE', #243913 ) ;
#58240 = CIRCLE ( 'NONE', #203997, 0.1000000000000028644 ) ;
#58241 = AXIS2_PLACEMENT_3D ( 'NONE', #216701, #95467, #156761 ) ;
#58242 = ORIENTED_EDGE ( 'NONE', *, *, #134470, .F. ) ;
#58243 = AXIS2_PLACEMENT_3D ( 'NONE', #114027, #33259, #137436 ) ;
#58244 = AXIS2_PLACEMENT_3D ( 'NONE', #103920, #141779, #204318 ) ;
#58245 = ADVANCED_FACE ( 'NONE', ( #122718 ), #245222, .T. ) ;
#58246 = DIRECTION ( 'NONE',  ( -1.000000000000000000, 0.000000000000000000, 0.000000000000000000 ) ) ;
#58247 = DIRECTION ( 'NONE',  ( -1.000000000000000000, -3.348484323767863974E-14, 9.081381425208614860E-15 ) ) ;
#58248 = FACE_OUTER_BOUND ( 'NONE', #132302, .T. ) ;
#58249 = DIRECTION ( 'NONE',  ( 1.000000000000000000, 0.000000000000000000, 0.000000000000000000 ) ) ;
#58250 = VECTOR ( 'NONE', #254788, 1000.000000000000000 ) ;
#58252 = LINE ( 'NONE', #74022, #236529 ) ;
#58251 = CARTESIAN_POINT ( 'NONE',  ( 21.09107601085556638, 0.03930716472845496856, -161.1361220246400592 ) ) ;
#58253 = DIRECTION ( 'NONE',  ( 1.000000000000000000, 0.000000000000000000, 0.000000000000000000 ) ) ;
#58255 = ORIENTED_EDGE ( 'NONE', *, *, #181365, .F. ) ;
#58254 = DIRECTION ( 'NONE',  ( 1.000000000000000000, 0.000000000000000000, 0.000000000000000000 ) ) ;
#58256 = CARTESIAN_POINT ( 'NONE',  ( 23.14999999999998437, 7.128833340093095217, -233.7327013124392749 ) ) ;
#58257 = ORIENTED_EDGE ( 'NONE', *, *, #222051, .T. ) ;
#58258 = CARTESIAN_POINT ( 'NONE',  ( 20.95512820512820440, 8.876151316288115822, -8.558628995140949769 ) ) ;
#58259 = EDGE_CURVE ( 'NONE', #152420, #60849, #146102, .T. ) ;
#58260 = ORIENTED_EDGE ( 'NONE', *, *, #208727, .F. ) ;
#58261 = VERTEX_POINT ( 'NONE', #202235 ) ;
#58262 = FACE_OUTER_BOUND ( 'NONE', #3291, .T. ) ;
#58263 = DIRECTION ( 'NONE',  ( 0.000000000000000000, -0.008583690987135041833, 0.9999631594459055250 ) ) ;
#58264 = DIRECTION ( 'NONE',  ( 0.000000000000000000, 0.9126074666063132002, 0.4088369013364708815 ) ) ;
#58265 = ORIENTED_EDGE ( 'NONE', *, *, #63923, .T. ) ;
#58266 = ORIENTED_EDGE ( 'NONE', *, *, #175392, .T. ) ;
#58267 = ORIENTED_EDGE ( 'NONE', *, *, #41505, .T. ) ;
#58268 = DIRECTION ( 'NONE',  ( 0.000000000000000000, -0.9770955615653315052, -0.2128009952263603954 ) ) ;
#58269 = ORIENTED_EDGE ( 'NONE', *, *, #202572, .F. ) ;
#58270 = CARTESIAN_POINT ( 'NONE',  ( -16.94445028196808778, 60.88759175473954599, -221.0718995934454938 ) ) ;
#58271 = PLANE ( 'NONE',  #173682 ) ;
#58272 = ORIENTED_EDGE ( 'NONE', *, *, #75114, .T. ) ;
#58273 = DIRECTION ( 'NONE',  ( 2.952720810173290098E-16, -0.4721928772777359007, -0.8814952561688425003 ) ) ;
#58274 = LINE ( 'NONE', #62151, #15709 ) ;
#58275 = DIRECTION ( 'NONE',  ( 0.000000000000000000, 0.000000000000000000, -1.000000000000000000 ) ) ;
#58276 = EDGE_LOOP ( 'NONE', ( #13506, #118121, #141212, #79142 ) ) ;
#58277 = AXIS2_PLACEMENT_3D ( 'NONE', #235164, #34420, #113918 ) ;
#58278 = DIRECTION ( 'NONE',  ( 0.000000000000000000, -1.000000000000000000, -6.982962677686266711E-15 ) ) ;
#58279 = DIRECTION ( 'NONE',  ( 0.000000000000000000, -1.000000000000000000, 0.000000000000000000 ) ) ;
#58280 = VECTOR ( 'NONE', #166922, 1000.000000000000000 ) ;
#58281 = CARTESIAN_POINT ( 'NONE',  ( -20.64999999999999858, 76.00000000001169553, -67.52310748452430289 ) ) ;
#58282 = AXIS2_PLACEMENT_3D ( 'NONE', #216390, #256753, #160305 ) ;
#58283 = ORIENTED_EDGE ( 'NONE', *, *, #257107, .T. ) ;
#58285 = EDGE_CURVE ( 'NONE', #97978, #100999, #60753, .T. ) ;
#58284 = PLANE ( 'NONE',  #246022 ) ;
#58286 = ORIENTED_EDGE ( 'NONE', *, *, #39354, .F. ) ;
#58287 = CARTESIAN_POINT ( 'NONE',  ( 21.08489247129321242, 67.12232480914198618, -124.1731074845243654 ) ) ;
#58288 = CARTESIAN_POINT ( 'NONE',  ( -16.87683809663752399, 13.90118822005493371, -218.5412211127979845 ) ) ;
#58289 = FACE_OUTER_BOUND ( 'NONE', #120966, .T. ) ;
#58290 = DIRECTION ( 'NONE',  ( 0.000000000000000000, 0.000000000000000000, 1.000000000000000000 ) ) ;
#58291 = DIRECTION ( 'NONE',  ( -1.000000000000000000, 0.000000000000000000, 0.000000000000000000 ) ) ;
#58292 = VERTEX_POINT ( 'NONE', #143532 ) ;
#58293 = LINE ( 'NONE', #256445, #100876 ) ;
#58294 = CIRCLE ( 'NONE', #49933, 0.09999999999999939493 ) ;
#58295 = CARTESIAN_POINT ( 'NONE',  ( -16.78055652883087134, 9.946776916136505164, -146.6607918375924555 ) ) ;
#58296 = CARTESIAN_POINT ( 'NONE',  ( -22.50000000000094147, 0.09999999999989445110, 11.64957080754481744 ) ) ;
#58297 = DIRECTION ( 'NONE',  ( 1.000000000000000000, 0.000000000000000000, 0.000000000000000000 ) ) ;
#58298 = EDGE_CURVE ( 'NONE', #67930, #123629, #7904, .T. ) ;
#58299 = CIRCLE ( 'NONE', #191632, 0.09999999999999971412 ) ;
#58300 = CARTESIAN_POINT ( 'NONE',  ( 20.58091095332318332, 66.98152984665915710, -61.10445730236583017 ) ) ;
#58301 = EDGE_LOOP ( 'NONE', ( #54717, #189372, #85805, #128461 ) ) ;
#58302 = ORIENTED_EDGE ( 'NONE', *, *, #191502, .T. ) ;
#58303 = CARTESIAN_POINT ( 'NONE',  ( 23.14999999999999858, 76.00000000001170974, -69.52310748452431710 ) ) ;
#58304 = FACE_OUTER_BOUND ( 'NONE', #135195, .T. ) ;
#58305 = CARTESIAN_POINT ( 'NONE',  ( -21.05000000000000071, 11.65000000001115232, -174.2838656629781156 ) ) ;
#58306 = CARTESIAN_POINT ( 'NONE',  ( 22.19999999999999929, -11.75000000000000000, 32.89999999999999858 ) ) ;
#58307 = DIRECTION ( 'NONE',  ( -1.000000000000000000, -0.000000000000000000, -0.000000000000000000 ) ) ;
#58308 = ORIENTED_EDGE ( 'NONE', *, *, #45309, .T. ) ;
#58309 = CARTESIAN_POINT ( 'NONE',  ( -18.39999999999999858, 46.96039402156217335, -255.3459641718773128 ) ) ;
#58310 = CARTESIAN_POINT ( 'NONE',  ( -20.54999999999999716, -8.999999999988844479, -57.10603087734755690 ) ) ;
#58311 = ORIENTED_EDGE ( 'NONE', *, *, #94519, .T. ) ;
#58312 = DIRECTION ( 'NONE',  ( 0.000000000000000000, 6.982962677686266711E-15, -1.000000000000000000 ) ) ;
#58313 = CIRCLE ( 'NONE', #154071, 0.1000000000000001305 ) ;
#58314 = ORIENTED_EDGE ( 'NONE', *, *, #255960, .T. ) ;
#58315 = CARTESIAN_POINT ( 'NONE',  ( 18.49999999999999645, 74.93036000061670165, -233.6816308724374949 ) ) ;
#58316 = EDGE_LOOP ( 'NONE', ( #12149, #110208, #116999, #148118 ) ) ;
#58317 = LINE ( 'NONE', #139131, #189195 ) ;
#58318 = CARTESIAN_POINT ( 'NONE',  ( -13.40000000000000213, -9.650000000000005684, 15.00000000000000355 ) ) ;
#58319 = DIRECTION ( 'NONE',  ( 1.000000000000000000, 0.000000000000000000, 0.000000000000000000 ) ) ;
#58320 = CARTESIAN_POINT ( 'NONE',  ( -20.64999999999999858, 21.39147882631411335, -233.2615922652120730 ) ) ;
#58321 = CARTESIAN_POINT ( 'NONE',  ( -22.50000000000000000, 1.115600667400684642E-11, -94.25000000000002842 ) ) ;
#58322 = CARTESIAN_POINT ( 'NONE',  ( 21.05000000000000071, 18.68960778496915509, -227.9427670361891956 ) ) ;
#58323 = DIRECTION ( 'NONE',  ( 0.000000000000000000, 0.9126074666063545004, 0.4088369013363783999 ) ) ;
#58324 = ADVANCED_FACE ( 'NONE', ( #62726 ), #6590, .T. ) ;
#58325 = CARTESIAN_POINT ( 'NONE',  ( -18.54270223418606633, -9.624105502871746154, -107.2409350504074723 ) ) ;
#58326 = DIRECTION ( 'NONE',  ( 1.000000000000000000, -0.000000000000000000, -0.000000000000000000 ) ) ;
#58327 = CARTESIAN_POINT ( 'NONE',  ( -23.15000000000000213, -8.999999999988846255, -110.3939691226524786 ) ) ;
#58328 = AXIS2_PLACEMENT_3D ( 'NONE', #119189, #494, #208986 ) ;
#58330 = EDGE_CURVE ( 'NONE', #236182, #63493, #102425, .T. ) ;
#58329 = CARTESIAN_POINT ( 'NONE',  ( -18.59999999999999787, 1.115600667400684642E-11, -67.00000000000004263 ) ) ;
#58332 = CYLINDRICAL_SURFACE ( 'NONE', #68950, 0.09999999999999939493 ) ;
#58331 = AXIS2_PLACEMENT_3D ( 'NONE', #63341, #183312, #184582 ) ;
#58333 = DIRECTION ( 'NONE',  ( -1.000000000000000000, 0.000000000000000000, 0.000000000000000000 ) ) ;
#58334 = DIRECTION ( 'NONE',  ( 0.000000000000000000, 0.000000000000000000, -1.000000000000000000 ) ) ;
#58335 = CIRCLE ( 'NONE', #154090, 4.299999999999970512 ) ;
#58336 = EDGE_LOOP ( 'NONE', ( #51818, #222756, #251620, #160544 ) ) ;
#58337 = CARTESIAN_POINT ( 'NONE',  ( 21.05000000000000071, 6.258847123079377184, 0.03175835305537381276 ) ) ;
#58339 = EDGE_CURVE ( 'NONE', #128522, #65850, #6607, .T. ) ;
#58338 = DIRECTION ( 'NONE',  ( 1.000000000000000000, 0.000000000000000000, 0.000000000000000000 ) ) ;
#58340 = DIRECTION ( 'NONE',  ( 0.000000000000000000, 0.000000000000000000, 1.000000000000000000 ) ) ;
#58341 = VERTEX_POINT ( 'NONE', #23632 ) ;
#58343 = ADVANCED_FACE ( 'NONE', ( #104386 ), #221762, .F. ) ;
#58342 = CARTESIAN_POINT ( 'NONE',  ( 16.87683809663749557, 51.61886293219124155, -231.9464690156495692 ) ) ;
#58345 = VECTOR ( 'NONE', #99881, 1000.000000000000000 ) ;
#58344 = DIRECTION ( 'NONE',  ( 0.000000000000000000, -7.026728003956686545E-15, 1.000000000000000000 ) ) ;
#58346 = ORIENTED_EDGE ( 'NONE', *, *, #167776, .F. ) ;
#58347 = PLANE ( 'NONE',  #142109 ) ;
#58348 = DIRECTION ( 'NONE',  ( 0.000000000000000000, -6.982962677686266711E-15, 1.000000000000000000 ) ) ;
#58349 = ADVANCED_FACE ( 'NONE', ( #43165, #86099 ), #4024, .T. ) ;
#58350 = ORIENTED_EDGE ( 'NONE', *, *, #201833, .F. ) ;
#58351 = EDGE_LOOP ( 'NONE', ( #101131, #114919, #43399, #3914, #196161, #180728, #165251 ) ) ;
#58352 = DIRECTION ( 'NONE',  ( 1.000000000000000000, 0.000000000000000000, 0.000000000000000000 ) ) ;
#58353 = VERTEX_POINT ( 'NONE', #45723 ) ;
#58354 = ADVANCED_FACE ( 'NONE', ( #27493 ), #104259, .T. ) ;
#58355 = DIRECTION ( 'NONE',  ( -6.938893903907219700E-15, 0.4721928772777345684, 0.8814952561688429444 ) ) ;
#58356 = CARTESIAN_POINT ( 'NONE',  ( 21.04105312098505109, 67.12466737696844632, -124.1946007373119585 ) ) ;
#58358 = DIRECTION ( 'NONE',  ( -1.000000000000000000, -0.000000000000000000, -0.000000000000000000 ) ) ;
#58357 = UNCERTAINTY_MEASURE_WITH_UNIT (LENGTH_MEASURE( 1.000000000000000082E-05 ), #175355, 'distance_accuracy_value', 'NONE');
#58359 = LINE ( 'NONE', #178365, #79448 ) ;
#58360 = DIRECTION ( 'NONE',  ( 0.000000000000000000, -0.4105728183244014562, -0.9118278131605539460 ) ) ;
#58361 = CARTESIAN_POINT ( 'NONE',  ( 22.39999999999999503, 11.75000000001116263, -134.1000000000000227 ) ) ;
#58362 = LINE ( 'NONE', #154958, #42987 ) ;
#58363 = CARTESIAN_POINT ( 'NONE',  ( 21.53752568622139307, 1.193029429790094298, -230.4407734565393469 ) ) ;
#58365 = ORIENTED_EDGE ( 'NONE', *, *, #44155, .T. ) ;
#58364 = CARTESIAN_POINT ( 'NONE',  ( 18.48197441911570138, -0.7048741502111930401, -242.4905267791219785 ) ) ;
#58366 = ORIENTED_EDGE ( 'NONE', *, *, #54959, .F. ) ;
#58368 = DIRECTION ( 'NONE',  ( -1.000000000000000000, -0.000000000000000000, 0.000000000000000000 ) ) ;
#58367 = CARTESIAN_POINT ( 'NONE',  ( 21.00000000000000000, 63.35728523183471594, -212.8904317177587870 ) ) ;
#58370 = ORIENTED_EDGE ( 'NONE', *, *, #62942, .T. ) ;
#58369 = FACE_OUTER_BOUND ( 'NONE', #122510, .T. ) ;
#58371 = TOROIDAL_SURFACE ( 'NONE', #170704, 0.2000000000000000111, 0.1000000000000000056 ) ;
#58372 = ORIENTED_EDGE ( 'NONE', *, *, #44975, .F. ) ;
#58373 = CARTESIAN_POINT ( 'NONE',  ( 23.14999999999999858, -2.099999999988846344, -200.9999999999999432 ) ) ;
#58374 = CARTESIAN_POINT ( 'NONE',  ( 20.21494484322224849, 9.303170737879936425, -175.8402651917702428 ) ) ;
#58375 = DIRECTION ( 'NONE',  ( 0.000000000000000000, 0.000000000000000000, 1.000000000000000000 ) ) ;
#58376 = LINE ( 'NONE', #55805, #139200 ) ;
#58377 = AXIS2_PLACEMENT_3D ( 'NONE', #22049, #63719, #181125 ) ;
#58378 = CARTESIAN_POINT ( 'NONE',  ( 20.12500000000000355, 9.258049272928479567, -108.8633388371424644 ) ) ;
#58379 = LINE ( 'NONE', #36302, #127062 ) ;
#58380 = DIRECTION ( 'NONE',  ( 0.000000000000000000, 0.000000000000000000, -1.000000000000000000 ) ) ;
#58381 = EDGE_CURVE ( 'NONE', #218153, #218718, #44025, .T. ) ;
#58382 = DIRECTION ( 'NONE',  ( 1.000000000000000000, 3.265361837132813093E-16, -0.000000000000000000 ) ) ;
#58383 = ORIENTED_EDGE ( 'NONE', *, *, #250428, .F. ) ;
#58384 = VERTEX_POINT ( 'NONE', #189093 ) ;
#58385 = DIRECTION ( 'NONE',  ( 0.000000000000000000, -0.000000000000000000, 1.000000000000000000 ) ) ;
#58386 = AXIS2_PLACEMENT_3D ( 'NONE', #181214, #126354, #186344 ) ;
#58387 = ORIENTED_EDGE ( 'NONE', *, *, #71789, .F. ) ;
#58388 = LINE ( 'NONE', #134095, #213376 ) ;
#58390 = ORIENTED_EDGE ( 'NONE', *, *, #22460, .T. ) ;
#58389 = AXIS2_PLACEMENT_3D ( 'NONE', #256208, #195049, #236704 ) ;
#58391 = CARTESIAN_POINT ( 'NONE',  ( 18.59999999999999787, 74.14897176987101091, -91.36919421510182815 ) ) ;
#58392 = EDGE_CURVE ( 'NONE', #83237, #63710, #76499, .T. ) ;
#58393 = AXIS2_PLACEMENT_3D ( 'NONE', #65665, #121809, #42266 ) ;
#58394 = DIRECTION ( 'NONE',  ( 1.000000000000000000, 0.000000000000000000, 0.000000000000000000 ) ) ;
#58395 = DIRECTION ( 'NONE',  ( 0.000000000000000000, 0.000000000000000000, -1.000000000000000000 ) ) ;
#58397 = EDGE_LOOP ( 'NONE', ( #44165, #145829, #208081, #205535 ) ) ;
#58396 = DIRECTION ( 'NONE',  ( 1.000000000000000000, 2.952720810173289112E-16, -0.000000000000000000 ) ) ;
#58398 = DIRECTION ( 'NONE',  ( -0.000000000000000000, -0.000000000000000000, 1.000000000000000000 ) ) ;
#58399 = VERTEX_POINT ( 'NONE', #28782 ) ;
#58400 = CIRCLE ( 'NONE', #50221, 4.300000000000033573 ) ;
#58403 = EDGE_CURVE ( 'NONE', #26537, #158092, #249082, .T. ) ;
#58402 = CIRCLE ( 'NONE', #183344, 0.6000000000000015321 ) ;
#58401 = DIRECTION ( 'NONE',  ( -1.000000000000000000, 0.000000000000000000, 0.000000000000000000 ) ) ;
#58404 = CARTESIAN_POINT ( 'NONE',  ( -20.94999999999999929, 76.00000000001190870, -103.0231074845243029 ) ) ;
#58405 = CARTESIAN_POINT ( 'NONE',  ( 18.39999999999999503, 59.20211495293902004, -220.5705723384363921 ) ) ;
#58406 = FACE_OUTER_BOUND ( 'NONE', #153043, .T. ) ;
#58407 = CARTESIAN_POINT ( 'NONE',  ( 15.74999999999999645, 9.850000000011137402, -83.75000000000004263 ) ) ;
#58408 = EDGE_CURVE ( 'NONE', #200518, #204167, #256335, .T. ) ;
#58409 = ORIENTED_EDGE ( 'NONE', *, *, #64092, .F. ) ;
#58410 = DIRECTION ( 'NONE',  ( 0.000000000000000000, -0.2617529984164955192, -0.9651348961777178603 ) ) ;
#58412 = ORIENTED_EDGE ( 'NONE', *, *, #240140, .F. ) ;
#58411 = B_SPLINE_CURVE_WITH_KNOTS ( 'NONE', 3,
 ( #198425, #40684, #254520, #36826, #155490, #98012, #61491, #156763, #117608, #60190, #120216, #21106, #255789, #217, #176321, #197131 ),
 .UNSPECIFIED., .F., .F.,
 ( 4, 3, 3, 3, 3, 4 ),
 ( 0.000000000000000000, 2.209833635978094077E-05, 5.595056164119021838E-05, 8.979992002654949078E-05, 0.0001236482757198866932, 0.0001574984039362965229 ),
 .UNSPECIFIED. ) ;
#58415 = ORIENTED_EDGE ( 'NONE', *, *, #8072, .F. ) ;
#58414 = DIRECTION ( 'NONE',  ( 1.000000000000000000, 0.000000000000000000, 0.000000000000000000 ) ) ;
#58413 = DIRECTION ( 'NONE',  ( 0.000000000000000000, 0.000000000000000000, -1.000000000000000000 ) ) ;
#58416 = CIRCLE ( 'NONE', #204166, 0.09999999999999963085 ) ;
#58417 = DIRECTION ( 'NONE',  ( 0.000000000000000000, 0.1350103645451876666, -0.9908441862701600211 ) ) ;
#58418 = AXIS2_PLACEMENT_3D ( 'NONE', #122547, #82089, #62564 ) ;
#58419 = AXIS2_PLACEMENT_3D ( 'NONE', #49313, #169307, #229250 ) ;
#58420 = CIRCLE ( 'NONE', #245892, 0.1999999999999987899 ) ;
#58421 = VECTOR ( 'NONE', #4067, 1000.000000000000000 ) ;
#58422 = FACE_OUTER_BOUND ( 'NONE', #187783, .T. ) ;
#58423 = ORIENTED_EDGE ( 'NONE', *, *, #4302, .F. ) ;
#58424 = CARTESIAN_POINT ( 'NONE',  ( 18.48413544395640074, 85.66430403364005031, -129.8400024914862456 ) ) ;
#58426 = EDGE_CURVE ( 'NONE', #231702, #47601, #235573, .T. ) ;
#58425 = CARTESIAN_POINT ( 'NONE',  ( -16.77683809663752257, 23.65833333334447985, -117.2500000000000284 ) ) ;
#58427 = CARTESIAN_POINT ( 'NONE',  ( -22.49756042579671700, -3.103614433689099616, -228.1629205807172980 ) ) ;
#58429 = VERTEX_POINT ( 'NONE', #49579 ) ;
#58428 = CARTESIAN_POINT ( 'NONE',  ( -18.39999999999999858, 8.780520186313291120, -245.4165333277510115 ) ) ;
#58430 = ADVANCED_FACE ( 'NONE', ( #89972 ), #95884, .T. ) ;
#58431 = EDGE_CURVE ( 'NONE', #87934, #121241, #177344, .T. ) ;
#58432 = VECTOR ( 'NONE', #153823, 1000.000000000000000 ) ;
#58433 = ORIENTED_EDGE ( 'NONE', *, *, #215935, .T. ) ;
#58434 = CARTESIAN_POINT ( 'NONE',  ( 18.49999999999999289, 11.75000000001115907, -122.2500000000000284 ) ) ;
#58435 = DIRECTION ( 'NONE',  ( 0.000000000000000000, 0.000000000000000000, -1.000000000000000000 ) ) ;
#58436 = CARTESIAN_POINT ( 'NONE',  ( 21.05000000000000071, 76.00000000001165290, -69.52310748452431710 ) ) ;
#58437 = ORIENTED_EDGE ( 'NONE', *, *, #72415, .T. ) ;
#58438 = DIRECTION ( 'NONE',  ( 0.000000000000000000, 0.000000000000000000, -1.000000000000000000 ) ) ;
#58439 = EDGE_LOOP ( 'NONE', ( #235205, #20204, #77339, #212753 ) ) ;
#58440 = CARTESIAN_POINT ( 'NONE',  ( -21.64999999999999858, 9.350000000011133849, -54.35000000000000142 ) ) ;
#58441 = EDGE_CURVE ( 'NONE', #29274, #24822, #52576, .T. ) ;
#58442 = DIRECTION ( 'NONE',  ( 1.000000000000000000, 0.000000000000000000, 0.000000000000000000 ) ) ;
#58443 = DIRECTION ( 'NONE',  ( 0.000000000000000000, 0.000000000000000000, 1.000000000000000000 ) ) ;
#58444 = ORIENTED_EDGE ( 'NONE', *, *, #166199, .T. ) ;
#58445 = EDGE_CURVE ( 'NONE', #6262, #219222, #170869, .T. ) ;
#58446 = CARTESIAN_POINT ( 'NONE',  ( 20.94999999999999929, -11.64999999998883595, -198.0999999999999659 ) ) ;
#58447 = EDGE_CURVE ( 'NONE', #24249, #39149, #85874, .T. ) ;
#58448 = AXIS2_PLACEMENT_3D ( 'NONE', #5507, #206310, #242855 ) ;
#58449 = CARTESIAN_POINT ( 'NONE',  ( 23.24999999999999289, 6.649999999999999467, -12.35000000000000320 ) ) ;
#58450 = CIRCLE ( 'NONE', #25185, 0.1000000000000124678 ) ;
#58451 = VERTEX_POINT ( 'NONE', #69165 ) ;
#58452 = CARTESIAN_POINT ( 'NONE',  ( 23.14999999999999503, 11.65000000001116298, -121.7500000000000426 ) ) ;
#58453 = DIRECTION ( 'NONE',  ( 1.000000000000000000, 0.000000000000000000, 0.000000000000000000 ) ) ;
#58454 = FACE_OUTER_BOUND ( 'NONE', #168574, .T. ) ;
#58455 = AXIS2_PLACEMENT_3D ( 'NONE', #184499, #185797, #123258 ) ;
#58456 = ORIENTED_EDGE ( 'NONE', *, *, #50521, .T. ) ;
#58457 = DIRECTION ( 'NONE',  ( 1.000000000000000000, 0.000000000000000000, 0.000000000000000000 ) ) ;
#58458 = ORIENTED_EDGE ( 'NONE', *, *, #211675, .T. ) ;
#58460 = ORIENTED_EDGE ( 'NONE', *, *, #195161, .T. ) ;
#58459 = CARTESIAN_POINT ( 'NONE',  ( 20.84999999999999432, 68.97833521811233481, -166.1895420826271277 ) ) ;
#58461 = EDGE_CURVE ( 'NONE', #208327, #105004, #148695, .T. ) ;
#58462 = EDGE_CURVE ( 'NONE', #181640, #106717, #249364, .T. ) ;
#58465 = ORIENTED_EDGE ( 'NONE', *, *, #21564, .F. ) ;
#58464 = ORIENTED_EDGE ( 'NONE', *, *, #91405, .T. ) ;
#58463 = CARTESIAN_POINT ( 'NONE',  ( -21.11927991906891222, 0.009083679473871926827, 6.448493118491512632 ) ) ;
#58466 = CIRCLE ( 'NONE', #4312, 11.90000000000000746 ) ;
#58467 = CARTESIAN_POINT ( 'NONE',  ( 20.95595624212461416, 65.37610879691773391, -95.39347457039747269 ) ) ;
#58468 = DIRECTION ( 'NONE',  ( 0.000000000000000000, 6.982962677686266711E-15, -1.000000000000000000 ) ) ;
#58470 = ADVANCED_FACE ( 'NONE', ( #256364 ), #81604, .T. ) ;
#58469 = CARTESIAN_POINT ( 'NONE',  ( -20.00857864376270001, 9.350000000000001421, -12.25000000000000000 ) ) ;
#58471 = CARTESIAN_POINT ( 'NONE',  ( -18.34374000495060386, 11.47316190336247033, -9.249999999999998224 ) ) ;
#58472 = CARTESIAN_POINT ( 'NONE',  ( -20.64999999999999858, 2.000000000011154189, -113.7246219227621395 ) ) ;
#58473 = AXIS2_PLACEMENT_3D ( 'NONE', #104409, #160592, #79714 ) ;
#58474 = CARTESIAN_POINT ( 'NONE',  ( 21.05000000000000071, 65.52661458509972192, -195.9444530202758870 ) ) ;
#58475 = CIRCLE ( 'NONE', #204242, 0.2000000000000000944 ) ;
#58476 = DIRECTION ( 'NONE',  ( 1.000000000000000000, 0.000000000000000000, 0.000000000000000000 ) ) ;
#58478 = DIRECTION ( 'NONE',  ( 0.000000000000000000, -0.1350103645451904977, -0.9908441862701596881 ) ) ;
#58477 = LINE ( 'NONE', #200579, #217696 ) ;
#58479 = ORIENTED_EDGE ( 'NONE', *, *, #215022, .F. ) ;
#58481 = ORIENTED_EDGE ( 'NONE', *, *, #124650, .T. ) ;
#58480 = AXIS2_PLACEMENT_3D ( 'NONE', #224642, #9456, #6885 ) ;
#58482 = VERTEX_POINT ( 'NONE', #98594 ) ;
#58483 = CARTESIAN_POINT ( 'NONE',  ( -23.25000000000000000, -0.1008583690875562017, -21.75043287651061164 ) ) ;
#58485 = ORIENTED_EDGE ( 'NONE', *, *, #142432, .T. ) ;
#58484 = CARTESIAN_POINT ( 'NONE',  ( 23.24999999999999645, 7.128833340093095217, -233.7327013124392749 ) ) ;
#58486 = DIRECTION ( 'NONE',  ( -0.000000000000000000, -0.1350103645451807555, -0.9908441862701610203 ) ) ;
#58487 = ORIENTED_EDGE ( 'NONE', *, *, #136539, .T. ) ;
#58488 = CARTESIAN_POINT ( 'NONE',  ( 20.94999999999999574, 87.65000000001235492, -167.0231074845242460 ) ) ;
#58489 =( BOUNDED_CURVE ( )  B_SPLINE_CURVE ( 3, ( #161215, #77799, #196472, #58235 ),
 .UNSPECIFIED., .F., .F. ) 
 B_SPLINE_CURVE_WITH_KNOTS ( ( 4, 4 ),
 ( 4.712388980384687009, 6.283185307179586232 ),
 .UNSPECIFIED. ) 
 CURVE ( )  GEOMETRIC_REPRESENTATION_ITEM ( )  RATIONAL_B_SPLINE_CURVE ( ( 1.000000000000000000, 0.8047378541243643824, 0.8047378541243643824, 1.000000000000000000 ) ) 
 REPRESENTATION_ITEM ( '' )  );
#58490 = ORIENTED_EDGE ( 'NONE', *, *, #66800, .F. ) ;
#58491 = CARTESIAN_POINT ( 'NONE',  ( -18.50000000000000000, -1.835859311443640340, -45.00443916879852679 ) ) ;
#58492 = ADVANCED_FACE ( 'NONE', ( #42510 ), #192629, .T. ) ;
#58493 = ORIENTED_EDGE ( 'NONE', *, *, #54254, .T. ) ;
#58494 = CIRCLE ( 'NONE', #241679, 0.1000000000000055844 ) ;
#58495 = AXIS2_PLACEMENT_3D ( 'NONE', #15817, #233562, #255625 ) ;
#58496 = CARTESIAN_POINT ( 'NONE',  ( -20.54999999999999716, 76.00000000001237765, -170.0231074845243597 ) ) ;
#58498 = EDGE_CURVE ( 'NONE', #154676, #130397, #157369, .T. ) ;
#58497 = CARTESIAN_POINT ( 'NONE',  ( 18.49999999999999289, 65.50857864377445594, -78.17310748452437963 ) ) ;
#58500 = ORIENTED_EDGE ( 'NONE', *, *, #28885, .F. ) ;
#58499 = ORIENTED_EDGE ( 'NONE', *, *, #106316, .T. ) ;
#58501 = VERTEX_POINT ( 'NONE', #122062 ) ;
#58502 = DIRECTION ( 'NONE',  ( -0.000000000000000000, 7.272083257015735086E-15, -1.000000000000000000 ) ) ;
#58503 = EDGE_LOOP ( 'NONE', ( #20666, #238247, #186577, #65355 ) ) ;
#58504 = VERTEX_POINT ( 'NONE', #176926 ) ;
#58505 = DIRECTION ( 'NONE',  ( 0.000000000000000000, -0.9654727137038715545, 0.2605042016806676242 ) ) ;
#58508 = EDGE_CURVE ( 'NONE', #154967, #10263, #227540, .T. ) ;
#58507 = ORIENTED_EDGE ( 'NONE', *, *, #15226, .T. ) ;
#58506 = DIRECTION ( 'NONE',  ( 0.000000000000000000, 0.000000000000000000, -1.000000000000000000 ) ) ;
#58510 = CARTESIAN_POINT ( 'NONE',  ( 20.94999999999999929, -8.999999999988844479, -76.89396912265249284 ) ) ;
#58509 = CARTESIAN_POINT ( 'NONE',  ( 13.99999999999999822, 9.850000000011137402, -50.24999999999999289 ) ) ;
#58511 = CARTESIAN_POINT ( 'NONE',  ( 18.54999999999999716, 10.51799536955200232, -208.1761252362501864 ) ) ;
#58512 = LINE ( 'NONE', #24567, #6597 ) ;
#58513 = DIRECTION ( 'NONE',  ( 1.000000000000000000, 0.000000000000000000, -0.000000000000000000 ) ) ;
#58514 = ORIENTED_EDGE ( 'NONE', *, *, #240748, .T. ) ;
#58515 = ADVANCED_FACE ( 'NONE', ( #39985 ), #60782, .F. ) ;
#58516 = ORIENTED_EDGE ( 'NONE', *, *, #100831, .F. ) ;
#58517 = DIRECTION ( 'NONE',  ( 1.836970198721029934E-16, 1.000000000000000000, 6.982962677686266711E-15 ) ) ;
#58519 = AXIS2_PLACEMENT_3D ( 'NONE', #130547, #190553, #52280 ) ;
#58518 = DIRECTION ( 'NONE',  ( -2.812466655313719426E-14, -0.1350103645451835865, -0.9908441862701605762 ) ) ;
#58520 = DIRECTION ( 'NONE',  ( 0.000000000000000000, -0.9875102702516471709, 0.1575546449569757979 ) ) ;
#58521 = CIRCLE ( 'NONE', #100016, 0.09999999999999939493 ) ;
#58522 = ADVANCED_FACE ( 'NONE', ( #158646 ), #180753, .F. ) ;
#58523 = CIRCLE ( 'NONE', #100207, 0.09999999999998898659 ) ;
#58524 = EDGE_LOOP ( 'NONE', ( #206739, #215376, #200682, #131279 ) ) ;
#58525 = CARTESIAN_POINT ( 'NONE',  ( 21.05000000000000071, -9.499999999988844479, -124.1060308773475924 ) ) ;
#58526 = EDGE_CURVE ( 'NONE', #39812, #135828, #2684, .T. ) ;
#58527 = CARTESIAN_POINT ( 'NONE',  ( -16.94107738177414291, 51.68386028857255354, -231.8469600742508021 ) ) ;
#58528 = DIRECTION ( 'NONE',  ( -0.000000000000000000, 6.982962677686266711E-15, -1.000000000000000000 ) ) ;
#58530 = EDGE_CURVE ( 'NONE', #66231, #19454, #148461, .T. ) ;
#58529 = EDGE_CURVE ( 'NONE', #32374, #51098, #119236, .T. ) ;
#58531 = EDGE_LOOP ( 'NONE', ( #144779, #177939, #201186, #226738 ) ) ;
#58532 = ORIENTED_EDGE ( 'NONE', *, *, #55160, .T. ) ;
#58533 = DIRECTION ( 'NONE',  ( 0.000000000000000000, 0.000000000000000000, -1.000000000000000000 ) ) ;
#58534 = CARTESIAN_POINT ( 'NONE',  ( -16.81744102076749314, 66.05000000001207638, -123.8731074845243683 ) ) ;
#58535 = ORIENTED_EDGE ( 'NONE', *, *, #167746, .T. ) ;
#58536 = DIRECTION ( 'NONE',  ( -0.7070776581708965169, -0.7071359030027827286, -0.000000000000000000 ) ) ;
#58537 = EDGE_LOOP ( 'NONE', ( #80991, #253234, #86993, #94416 ) ) ;
#58538 = DIRECTION ( 'NONE',  ( 0.000000000000000000, 0.000000000000000000, -1.000000000000000000 ) ) ;
#58539 = CARTESIAN_POINT ( 'NONE',  ( -18.50000000000000000, 9.350000000011156942, -155.1500000000000057 ) ) ;
#58541 = CARTESIAN_POINT ( 'NONE',  ( -22.59999985501179154, 55.87389454177475301, -232.8428744225222431 ) ) ;
#58540 = DIRECTION ( 'NONE',  ( 0.7071067811865463515, -0.7071067811865487940, -5.696443396193425170E-15 ) ) ;
#58542 = CIRCLE ( 'NONE', #8495, 11.80000000000000426 ) ;
#58543 = LINE ( 'NONE', #118561, #203117 ) ;
#58544 = LINE ( 'NONE', #138084, #99389 ) ;
#58545 = DIRECTION ( 'NONE',  ( 0.000000000000000000, 1.000000000000000000, 0.000000000000000000 ) ) ;
#58546 = EDGE_CURVE ( 'NONE', #35900, #96396, #22988, .T. ) ;
#58547 = EDGE_CURVE ( 'NONE', #73365, #124582, #94274, .T. ) ;
#58549 = ORIENTED_EDGE ( 'NONE', *, *, #119360, .T. ) ;
#58548 = ORIENTED_EDGE ( 'NONE', *, *, #230450, .T. ) ;
#58550 = ORIENTED_EDGE ( 'NONE', *, *, #14435, .T. ) ;
#58551 = EDGE_CURVE ( 'NONE', #20245, #169080, #90165, .T. ) ;
#58552 = DIRECTION ( 'NONE',  ( 0.000000000000000000, 1.000000000000000000, 0.000000000000000000 ) ) ;
#58553 = CARTESIAN_POINT ( 'NONE',  ( -18.45068461519106151, -7.764980607745699537, -209.9256088280441759 ) ) ;
#58554 = CARTESIAN_POINT ( 'NONE',  ( 18.59999999999999076, 11.65000000001115943, -55.25000000000004974 ) ) ;
#58555 = DIRECTION ( 'NONE',  ( 1.000000000000000000, -0.000000000000000000, -0.000000000000000000 ) ) ;
#58556 = AXIS2_PLACEMENT_3D ( 'NONE', #93279, #252345, #75044 ) ;
#58558 = DIRECTION ( 'NONE',  ( 0.000000000000000000, -1.000000000000000000, 0.000000000000000000 ) ) ;
#58557 = CARTESIAN_POINT ( 'NONE',  ( 20.58091095332318332, 9.018470153352529550, -8.418650182158506468 ) ) ;
#58559 = EDGE_CURVE ( 'NONE', #128415, #22177, #149349, .T. ) ;
#58560 = DIRECTION ( 'NONE',  ( 0.000000000000000000, -1.000000000000000000, 0.000000000000000000 ) ) ;
#58561 = ORIENTED_EDGE ( 'NONE', *, *, #216838, .F. ) ;
#58562 = FACE_OUTER_BOUND ( 'NONE', #167473, .T. ) ;
#58563 = ADVANCED_FACE ( 'NONE', ( #84152 ), #65936, .F. ) ;
#58564 = ORIENTED_EDGE ( 'NONE', *, *, #160054, .F. ) ;
#58565 = ORIENTED_EDGE ( 'NONE', *, *, #128023, .T. ) ;
#58566 = CARTESIAN_POINT ( 'NONE',  ( -21.05000000000000426, 69.50298221357934381, -69.50856179395341883 ) ) ;
#58567 = DIRECTION ( 'NONE',  ( 0.000000000000000000, 0.2617529984165034018, 0.9651348961777157509 ) ) ;
#58568 = CARTESIAN_POINT ( 'NONE',  ( -16.87683809663752044, 66.05000000001153637, -49.42547150272070411 ) ) ;
#58569 = CARTESIAN_POINT ( 'NONE',  ( 12.25000000000000000, 9.350000000011139178, -83.52151937182513564 ) ) ;
#58570 = AXIS2_PLACEMENT_3D ( 'NONE', #36970, #176466, #198564 ) ;
#58571 = CARTESIAN_POINT ( 'NONE',  ( -23.25000000000000000, 76.00000000001142553, -36.02310748452432421 ) ) ;
#58572 = ORIENTED_EDGE ( 'NONE', *, *, #202223, .T. ) ;
#58573 = ORIENTED_EDGE ( 'NONE', *, *, #191285, .T. ) ;
#58574 = CARTESIAN_POINT ( 'NONE',  ( -21.03922262424672951, 11.62390063401586460, -40.35920804289344233 ) ) ;
#58575 = CIRCLE ( 'NONE', #179238, 0.1000000000000096922 ) ;
#58576 = CARTESIAN_POINT ( 'NONE',  ( 19.75857864376268935, 62.46583972339646351, -208.9186153945276487 ) ) ;
#58578 = EDGE_CURVE ( 'NONE', #17335, #14833, #198325, .T. ) ;
#58577 = EDGE_LOOP ( 'NONE', ( #130661, #229871, #125360, #73650, #60938, #29970 ) ) ;
#58579 = CARTESIAN_POINT ( 'NONE',  ( -20.54999999999999716, 4.662003332185090443, -213.0075696128765514 ) ) ;
#58580 = DIRECTION ( 'NONE',  ( -1.000000000000000000, -0.000000000000000000, -0.000000000000000000 ) ) ;
#58581 = CARTESIAN_POINT ( 'NONE',  ( -20.94999999999999929, 68.00366762990589109, -224.2307594727497815 ) ) ;
#58582 = FACE_OUTER_BOUND ( 'NONE', #217248, .T. ) ;
#58583 = CARTESIAN_POINT ( 'NONE',  ( -16.77902162784673834, 66.05358074280401581, -90.36111624045503277 ) ) ;
#58584 = DIRECTION ( 'NONE',  ( -1.000000000000000000, 0.000000000000000000, 0.000000000000000000 ) ) ;
#58586 = FACE_OUTER_BOUND ( 'NONE', #102394, .T. ) ;
#58585 = CARTESIAN_POINT ( 'NONE',  ( -20.64999999999999858, 1.115600667400684642E-11, -100.5000000000000284 ) ) ;
#58587 = DIRECTION ( 'NONE',  ( -0.000000000000000000, 0.2128009952263603677, -0.9770955615653313941 ) ) ;
#58589 = EDGE_CURVE ( 'NONE', #248782, #145377, #125893, .T. ) ;
#58588 = DIRECTION ( 'NONE',  ( 1.000000000000000000, 1.836970198721029934E-16, 0.000000000000000000 ) ) ;
#58590 = CARTESIAN_POINT ( 'NONE',  ( -22.48660254037843131, 11.75000000001115374, -133.9500000000000171 ) ) ;
#58591 = DIRECTION ( 'NONE',  ( 1.000000000000000000, -3.265361837132813093E-16, -2.280189983783949500E-30 ) ) ;
#58592 = AXIS2_PLACEMENT_3D ( 'NONE', #100030, #19238, #154934 ) ;
#58594 = VERTEX_POINT ( 'NONE', #26836 ) ;
#58593 = DIRECTION ( 'NONE',  ( -1.073024830501117725E-15, -0.000000000000000000, -1.000000000000000000 ) ) ;
#58595 = CIRCLE ( 'NONE', #154342, 0.4000000000000045186 ) ;
#58596 = AXIS2_PLACEMENT_3D ( 'NONE', #5461, #86282, #165868 ) ;
#58597 = MECHANICAL_DESIGN_GEOMETRIC_PRESENTATION_REPRESENTATION (  '', ( #33530 ), #29427 ) ;
#58599 = ADVANCED_FACE ( 'NONE', ( #187184 ), #102612, .T. ) ;
#58598 = DIRECTION ( 'NONE',  ( 0.000000000000000000, 0.2617529984165050116, 0.9651348961777153068 ) ) ;
#58600 = ORIENTED_EDGE ( 'NONE', *, *, #243122, .F. ) ;
#58601 = AXIS2_PLACEMENT_3D ( 'NONE', #243439, #169084, #9969 ) ;
#58602 = LINE ( 'NONE', #152941, #254068 ) ;
#58603 = FACE_OUTER_BOUND ( 'NONE', #102769, .T. ) ;
#58604 = ORIENTED_EDGE ( 'NONE', *, *, #59562, .T. ) ;
#58605 = CARTESIAN_POINT ( 'NONE',  ( -21.05000000000000071, 6.540656951701240729, -0.09999999999999939493 ) ) ;
#58606 = CARTESIAN_POINT ( 'NONE',  ( -20.94999999999999929, 77.16412189325305349, -95.10825939895268277 ) ) ;
#58607 = DIRECTION ( 'NONE',  ( 0.000000000000000000, 0.4930308989875230585, 0.8700118002898322711 ) ) ;
#58608 = EDGE_CURVE ( 'NONE', #46173, #138239, #177317, .T. ) ;
#58609 = VECTOR ( 'NONE', #205833, 1000.000000000000000 ) ;
#58610 = DIRECTION ( 'NONE',  ( 4.336808689942128177E-15, 0.8660254037844330455, -0.5000000000000096589 ) ) ;
#58611 = VECTOR ( 'NONE', #131871, 1000.000000000000000 ) ;
#58612 = CARTESIAN_POINT ( 'NONE',  ( 18.56308993302899069, 10.38069115532423581, -24.73922263893877371 ) ) ;
#58613 = DIRECTION ( 'NONE',  ( 0.000000000000000000, -0.2617529984164915779, -0.9651348961777189706 ) ) ;
#58614 = CIRCLE ( 'NONE', #91937, 0.2000000000000057288 ) ;
#58615 = VECTOR ( 'NONE', #41633, 1000.000000000000000 ) ;
#58616 = EDGE_LOOP ( 'NONE', ( #51262, #68377, #39924, #155165 ) ) ;
#58617 = DIRECTION ( 'NONE',  ( 1.000000000000000000, 0.000000000000000000, 0.000000000000000000 ) ) ;
#58619 = ORIENTED_EDGE ( 'NONE', *, *, #154936, .T. ) ;
#58618 = CYLINDRICAL_SURFACE ( 'NONE', #113679, 0.09999999999999781286 ) ;
#58620 = CARTESIAN_POINT ( 'NONE',  ( 20.94999999999999929, 10.72371710471867701, -54.75000000000000000 ) ) ;
#58621 = DIRECTION ( 'NONE',  ( 0.000000000000000000, 0.2617529984165152257, 0.9651348961777124202 ) ) ;
#58622 = CARTESIAN_POINT ( 'NONE',  ( 20.85000000000000142, 36.65892442174935439, -249.5511627012433848 ) ) ;
#58623 = ORIENTED_EDGE ( 'NONE', *, *, #124509, .T. ) ;
#58624 = CARTESIAN_POINT ( 'NONE',  ( -22.48479450179659977, 75.95300841882533405, -148.1731059307759324 ) ) ;
#58625 = APPLICATION_PROTOCOL_DEFINITION ( 'draft international standard', 'automotive_design', 1998, #230605 ) ;
#58626 = AXIS2_PLACEMENT_3D ( 'NONE', #199322, #237162, #140609 ) ;
#58627 = DIRECTION ( 'NONE',  ( -0.000000000000000000, -0.000000000000000000, -1.000000000000000000 ) ) ;
#58628 = ORIENTED_EDGE ( 'NONE', *, *, #205032, .F. ) ;
#58629 = DIRECTION ( 'NONE',  ( 0.000000000000000000, 0.000000000000000000, -1.000000000000000000 ) ) ;
#58630 = LINE ( 'NONE', #73118, #30028 ) ;
#58631 = CARTESIAN_POINT ( 'NONE',  ( -18.50000000000000000, 64.25000000001152500, -48.17310748452440805 ) ) ;
#58632 = ORIENTED_EDGE ( 'NONE', *, *, #102474, .F. ) ;
#58633 = EDGE_LOOP ( 'NONE', ( #161866, #103797, #139598, #213744 ) ) ;
#58634 = DIRECTION ( 'NONE',  ( -1.000000000000000000, -0.000000000000000000, -0.000000000000000000 ) ) ;
#58635 = FACE_OUTER_BOUND ( 'NONE', #60171, .T. ) ;
#58636 = VECTOR ( 'NONE', #192864, 1000.000000000000227 ) ;
#58637 = CARTESIAN_POINT ( 'NONE',  ( 22.48660254037844197, 64.35000000001267040, -203.5731074845244564 ) ) ;
#58638 = CARTESIAN_POINT ( 'NONE',  ( 21.14999999999999858, 64.25000000001227818, -157.8731074845244393 ) ) ;
#58639 = EDGE_CURVE ( 'NONE', #236062, #147420, #252475, .T. ) ;
#58640 = CYLINDRICAL_SURFACE ( 'NONE', #203447, 0.09999999999999939493 ) ;
#58641 = DIRECTION ( 'NONE',  ( 0.000000000000000000, 0.000000000000000000, 1.000000000000000000 ) ) ;
#58642 = CARTESIAN_POINT ( 'NONE',  ( -23.25000000000000000, 6.307392164054360428, -220.9841382799134522 ) ) ;
#58643 = DIRECTION ( 'NONE',  ( -1.000000000000000000, 0.000000000000000000, 0.000000000000000000 ) ) ;
#58644 = CARTESIAN_POINT ( 'NONE',  ( 23.24999999999999289, 11.65000000001116298, -55.25000000000004974 ) ) ;
#58645 = ORIENTED_EDGE ( 'NONE', *, *, #36143, .F. ) ;
#58646 = AXIS2_PLACEMENT_3D ( 'NONE', #142123, #84679, #245079 ) ;
#58647 = EDGE_LOOP ( 'NONE', ( #232283, #127420, #184316, #172510 ) ) ;
#58648 = FACE_OUTER_BOUND ( 'NONE', #111194, .T. ) ;
#58650 = CARTESIAN_POINT ( 'NONE',  ( -21.14999999999999858, -11.74999999998884448, -167.4999999999999432 ) ) ;
#58649 = CARTESIAN_POINT ( 'NONE',  ( 21.08884785362045378, 69.64280663258641368, -69.57289057959120271 ) ) ;
#58651 = AXIS2_PLACEMENT_3D ( 'NONE', #200344, #120836, #219901 ) ;
#58652 = DIRECTION ( 'NONE',  ( 0.000000000000000000, -1.000000000000000000, -6.982962677686265922E-15 ) ) ;
#58654 = EDGE_CURVE ( 'NONE', #210647, #86355, #248395, .T. ) ;
#58653 = DIRECTION ( 'NONE',  ( 1.000000000000000000, -0.000000000000000000, -0.000000000000000000 ) ) ;
#58655 = CARTESIAN_POINT ( 'NONE',  ( 23.25000000000000000, -8.777002227904191045, -238.5420042644097975 ) ) ;
#58656 = ORIENTED_EDGE ( 'NONE', *, *, #187662, .F. ) ;
#58657 = ORIENTED_EDGE ( 'NONE', *, *, #65821, .T. ) ;
#58658 = EDGE_CURVE ( 'NONE', #39875, #188830, #107620, .T. ) ;
#58659 = AXIS2_PLACEMENT_3D ( 'NONE', #61428, #121434, #237502 ) ;
#58660 = DIRECTION ( 'NONE',  ( -1.000000000000000000, -0.000000000000000000, -0.000000000000000000 ) ) ;
#58661 = VERTEX_POINT ( 'NONE', #88033 ) ;
#58662 = DIRECTION ( 'NONE',  ( 0.000000000000000000, 0.2128009952263601456, -0.9770955615653316162 ) ) ;
#58663 = AXIS2_PLACEMENT_3D ( 'NONE', #53140, #252615, #233093 ) ;
#58664 = EDGE_CURVE ( 'NONE', #210119, #103572, #214671, .T. ) ;
#58665 = TOROIDAL_SURFACE ( 'NONE', #100162, 0.6000000000000013101, 0.1000000000000000056 ) ;
#58666 = CARTESIAN_POINT ( 'NONE',  ( 23.24999999999999289, 11.65000000001116298, -45.65000000000000568 ) ) ;
#58667 = CIRCLE ( 'NONE', #204419, 0.1000000000000000472 ) ;
#58668 = EDGE_CURVE ( 'NONE', #86653, #67751, #29414, .T. ) ;
#58669 = ADVANCED_FACE ( 'NONE', ( #4653 ), #168934, .T. ) ;
#58670 = ORIENTED_EDGE ( 'NONE', *, *, #53724, .F. ) ;
#58671 = DIRECTION ( 'NONE',  ( 0.000000000000000000, 0.000000000000000000, 1.000000000000000000 ) ) ;
#58672 = VERTEX_POINT ( 'NONE', #163760 ) ;
#58673 = EDGE_CURVE ( 'NONE', #94393, #55154, #256523, .T. ) ;
#58674 = FACE_OUTER_BOUND ( 'NONE', #109755, .T. ) ;
#58675 = CARTESIAN_POINT ( 'NONE',  ( 21.04999999999999716, -0.08561306079281309767, -27.08624026618970859 ) ) ;
#58676 = LINE ( 'NONE', #22164, #257274 ) ;
#58677 = CARTESIAN_POINT ( 'NONE',  ( 20.94999999999999574, 87.75000000001234923, -166.9231074845242802 ) ) ;
#58679 = CARTESIAN_POINT ( 'NONE',  ( -21.65000000000000213, 7.708578643773852157, -45.75000000000000000 ) ) ;
#58678 = DIRECTION ( 'NONE',  ( -1.000000000000000000, 0.000000000000000000, -0.000000000000000000 ) ) ;
#58680 = ADVANCED_FACE ( 'NONE', ( #31967 ), #249709, .T. ) ;
#58681 = AXIS2_PLACEMENT_3D ( 'NONE', #30909, #214325, #16152 ) ;
#58682 = DIRECTION ( 'NONE',  ( 0.7071067811865214825, -0.7071067811865735520, 0.000000000000000000 ) ) ;
#58683 = ORIENTED_EDGE ( 'NONE', *, *, #52524, .T. ) ;
#58685 = DIRECTION ( 'NONE',  ( 0.000000000000000000, 0.000000000000000000, -1.000000000000000000 ) ) ;
#58684 = CARTESIAN_POINT ( 'NONE',  ( -17.01825945287482966, 10.05000000001113847, -180.1499999999999773 ) ) ;
#58686 = ORIENTED_EDGE ( 'NONE', *, *, #69170, .F. ) ;
#58688 = VERTEX_POINT ( 'NONE', #111480 ) ;
#58687 = DIRECTION ( 'NONE',  ( -6.938893903907222856E-15, 0.4721928772777346239, 0.8814952561688430555 ) ) ;
#58689 = ORIENTED_EDGE ( 'NONE', *, *, #37856, .F. ) ;
#58690 = FACE_OUTER_BOUND ( 'NONE', #11568, .T. ) ;
#58691 = DIRECTION ( 'NONE',  ( -0.000000000000000000, 1.000000000000000000, 1.445602896647339410E-16 ) ) ;
#58692 = FACE_OUTER_BOUND ( 'NONE', #83802, .T. ) ;
#58693 = CARTESIAN_POINT ( 'NONE',  ( -23.15000000000000213, 2.000000000011154189, -46.22462192276210402 ) ) ;
#58694 = EDGE_LOOP ( 'NONE', ( #87938, #177841, #206295, #150242 ) ) ;
#58695 = LINE ( 'NONE', #255584, #21399 ) ;
#58696 = EDGE_CURVE ( 'NONE', #17708, #164109, #112197, .T. ) ;
#58697 = CARTESIAN_POINT ( 'NONE',  ( 21.09546886439552438, 8.878553113026075749, -112.7370938505550413 ) ) ;
#58698 = DIRECTION ( 'NONE',  ( 1.000000000000000000, 0.000000000000000000, 0.000000000000000000 ) ) ;
#58699 = ORIENTED_EDGE ( 'NONE', *, *, #97333, .F. ) ;
#58701 = ADVANCED_FACE ( 'NONE', ( #34534 ), #72372, .T. ) ;
#58700 = CARTESIAN_POINT ( 'NONE',  ( -18.50016250449483124, 46.34703458179508573, -243.0587802416268346 ) ) ;
#58702 = VECTOR ( 'NONE', #234137, 1000.000000000000000 ) ;
#58703 = CIRCLE ( 'NONE', #92034, 0.09999999999999939493 ) ;
#58704 = DIRECTION ( 'NONE',  ( 0.000000000000000000, 0.000000000000000000, -1.000000000000000000 ) ) ;
#58705 = ORIENTED_EDGE ( 'NONE', *, *, #32828, .T. ) ;
#58706 = VERTEX_POINT ( 'NONE', #175333 ) ;
#58707 = CARTESIAN_POINT ( 'NONE',  ( -16.89797118371800977, 9.976380722656529088, -188.4372933675600166 ) ) ;
#58708 = ORIENTED_EDGE ( 'NONE', *, *, #79931, .F. ) ;
#58709 = CARTESIAN_POINT ( 'NONE',  ( -17.78241384943093095, 10.85557575278284226, -10.24903767247034914 ) ) ;
#58710 = ORIENTED_EDGE ( 'NONE', *, *, #249108, .F. ) ;
#58711 = EDGE_CURVE ( 'NONE', #136982, #245093, #16260, .T. ) ;
#58712 = PLANE ( 'NONE',  #252235 ) ;
#58713 = CARTESIAN_POINT ( 'NONE',  ( 21.05000000000000071, 60.90953975616409366, -225.2728109422286877 ) ) ;
#58714 = CARTESIAN_POINT ( 'NONE',  ( 20.95083306685154056, 60.84428375453579463, -225.3393541664412112 ) ) ;
#58715 = AXIS2_PLACEMENT_3D ( 'NONE', #255511, #117344, #196864 ) ;
#58716 = DIRECTION ( 'NONE',  ( -1.000000000000000000, -0.000000000000000000, -0.000000000000000000 ) ) ;
#58717 = CARTESIAN_POINT ( 'NONE',  ( -21.08884785362073089, 0.04978309507788075683, -27.14280663257438420 ) ) ;
#58718 = CARTESIAN_POINT ( 'NONE',  ( 21.05000000000000071, 56.02567683926420727, -227.9999002286038774 ) ) ;
#58719 = VERTEX_POINT ( 'NONE', #12401 ) ;
#58721 = CARTESIAN_POINT ( 'NONE',  ( -21.55000000000000426, 68.25000000001260503, -191.1731074845243938 ) ) ;
#58720 = CARTESIAN_POINT ( 'NONE',  ( -21.30740335185486245, 75.90106547423657446, -176.5797654065523545 ) ) ;
#58722 = VERTEX_POINT ( 'NONE', #254786 ) ;
#58725 = ORIENTED_EDGE ( 'NONE', *, *, #210895, .F. ) ;
#58724 = CARTESIAN_POINT ( 'NONE',  ( 23.14999999999999503, 11.65000000000000746, -26.58519422934605814 ) ) ;
#58723 = DIRECTION ( 'NONE',  ( 0.000000000000000000, 1.156482317317873105E-15, 1.000000000000000000 ) ) ;
#58726 = EDGE_CURVE ( 'NONE', #146605, #107898, #169339, .T. ) ;
#58727 = EDGE_LOOP ( 'NONE', ( #180588, #141308, #83476, #106988 ) ) ;
#58728 = FACE_OUTER_BOUND ( 'NONE', #230681, .T. ) ;
#58729 = CARTESIAN_POINT ( 'NONE',  ( 21.05000000000000071, 0.09779029132038050132, -60.74218538951851798 ) ) ;
#58730 = LINE ( 'NONE', #114883, #173501 ) ;
#58731 = DIRECTION ( 'NONE',  ( -1.000000000000000000, -7.304098846218134667E-16, 0.000000000000000000 ) ) ;
#58732 = ORIENTED_EDGE ( 'NONE', *, *, #14692, .T. ) ;
#58733 = LINE ( 'NONE', #120054, #176098 ) ;
#58735 = EDGE_CURVE ( 'NONE', #1640, #237421, #130927, .T. ) ;
#58734 = DIRECTION ( 'NONE',  ( 0.000000000000000000, 1.000000000000000000, 6.982962677686266711E-15 ) ) ;
#58737 = CARTESIAN_POINT ( 'NONE',  ( 20.95566103547454517, 10.61824765094706358, -7.631840192980594573 ) ) ;
#58736 = DIRECTION ( 'NONE',  ( 0.000000000000000000, 0.000000000000000000, 1.000000000000000000 ) ) ;
#58739 = VERTEX_POINT ( 'NONE', #250971 ) ;
#58738 = CARTESIAN_POINT ( 'NONE',  ( -16.93301857435212909, 9.976309354746611291, -54.38577557116142458 ) ) ;
#58740 = AXIS2_PLACEMENT_3D ( 'NONE', #136212, #3133, #77528 ) ;
#58741 = EDGE_CURVE ( 'NONE', #253923, #200518, #89990, .T. ) ;
#58742 = EDGE_CURVE ( 'NONE', #208213, #2508, #177526, .T. ) ;
#58743 = ORIENTED_EDGE ( 'NONE', *, *, #193878, .F. ) ;
#58744 = AXIS2_PLACEMENT_3D ( 'NONE', #45919, #23823, #145003 ) ;
#58745 = EDGE_CURVE ( 'NONE', #2197, #16537, #156675, .T. ) ;
#58746 = B_SPLINE_CURVE_WITH_KNOTS ( 'NONE', 3,
 ( #58808, #138348, #15893, #155411, #217886, #92817, #39302, #73300, #251898, #14605 ),
 .UNSPECIFIED., .F., .F.,
 ( 4, 3, 3, 4 ),
 ( 0.000000000000000000, 3.394313611811087942E-05, 6.779740500699110782E-05, 0.0001049857339142587780 ),
 .UNSPECIFIED. ) ;
#58747 = CARTESIAN_POINT ( 'NONE',  ( 21.05000000000000071, 76.00000000001246292, -171.9231074845243938 ) ) ;
#58749 = ORIENTED_EDGE ( 'NONE', *, *, #137570, .T. ) ;
#58748 = TOROIDAL_SURFACE ( 'NONE', #183688, 0.4000000000000009104, 0.1000000000000000056 ) ;
#58750 = FACE_OUTER_BOUND ( 'NONE', #66508, .T. ) ;
#58751 = EDGE_LOOP ( 'NONE', ( #229747, #41710, #234577, #157481, #41067 ) ) ;
#58752 = EDGE_CURVE ( 'NONE', #23868, #214700, #44227, .T. ) ;
#58753 = LINE ( 'NONE', #97872, #5806 ) ;
#58754 = CIRCLE ( 'NONE', #100264, 0.1000000000000076522 ) ;
#58755 = B_SPLINE_CURVE_WITH_KNOTS ( 'NONE', 3,
 ( #254900, #78870, #253663, #237958, #59286, #155896, #138826, #154614, #235391, #218385, #3188, #141433, #5754, #181855, #202691, #162304, #4482, #241819, #64481, #20219, #24086, #119313, #198838, #63171, #200135, #100974, #44915, #201404, #103569, #140133 ),
 .UNSPECIFIED., .F., .F.,
 ( 4, 2, 2, 2, 2, 2, 2, 2, 2, 2, 2, 2, 2, 2, 4 ),
 ( 0.000000000000000000, 0.0003422764154113111176, 0.0006845528308226222353, 0.001026829246233933353, 0.001369105661645244471, 0.002053658492467925253, 0.002738211323290606469, 0.003080487738701950112, 0.003422764154113292889, 0.003765040569524635665, 0.004107316984935978008, 0.004449593400347320350, 0.004791869815758663560, 0.005134146231170005903, 0.005476422646581349113 ),
 .UNSPECIFIED. ) ;
#58756 = DIRECTION ( 'NONE',  ( 1.000000000000000000, 0.000000000000000000, 0.000000000000000000 ) ) ;
#58757 = CARTESIAN_POINT ( 'NONE',  ( 23.14999999999999858, 1.115600667400684642E-11, -167.5000000000000284 ) ) ;
#58758 = EDGE_LOOP ( 'NONE', ( #55250, #132871, #186621, #74923 ) ) ;
#58759 = CARTESIAN_POINT ( 'NONE',  ( 20.94999999999999929, 5.000000000011153745, -79.40526601891313874 ) ) ;
#58760 = AXIS2_PLACEMENT_3D ( 'NONE', #187316, #90747, #71224 ) ;
#58761 = DIRECTION ( 'NONE',  ( -0.000000000000000000, 7.272083257015735086E-15, -1.000000000000000000 ) ) ;
#58762 = AXIS2_PLACEMENT_3D ( 'NONE', #100413, #138259, #1318 ) ;
#58763 = ADVANCED_FACE ( 'NONE', ( #170226 ), #150613, .F. ) ;
#58764 = VERTEX_POINT ( 'NONE', #134862 ) ;
#58765 = EDGE_LOOP ( 'NONE', ( #73256, #214693, #52589, #99949 ) ) ;
#58766 = CIRCLE ( 'NONE', #175347, 0.1000000000000028644 ) ;
#58767 = EDGE_LOOP ( 'NONE', ( #254394, #68720, #238674, #146747 ) ) ;
#58768 = CARTESIAN_POINT ( 'NONE',  ( -21.10000000000000142, 6.322468214605804882, 12.11686199900910310 ) ) ;
#58769 = ORIENTED_EDGE ( 'NONE', *, *, #8078, .T. ) ;
#58771 = ORIENTED_EDGE ( 'NONE', *, *, #74002, .F. ) ;
#58770 = CARTESIAN_POINT ( 'NONE',  ( 20.73486653747088582, 68.75000000001229239, -160.7731074845244166 ) ) ;
#58772 = EDGE_CURVE ( 'NONE', #11922, #247736, #19259, .T. ) ;
#58773 = EDGE_CURVE ( 'NONE', #218485, #124985, #185849, .T. ) ;
#58774 = AXIS2_PLACEMENT_3D ( 'NONE', #229588, #210033, #7975 ) ;
#58775 = VECTOR ( 'NONE', #192180, 1000.000000000000000 ) ;
#58776 = ORIENTED_EDGE ( 'NONE', *, *, #237264, .T. ) ;
#58779 = ORIENTED_EDGE ( 'NONE', *, *, #97333, .T. ) ;
#58778 = VERTEX_POINT ( 'NONE', #153207 ) ;
#58777 = CARTESIAN_POINT ( 'NONE',  ( 18.39999999999999503, 11.75000000001113953, -188.3499999999999659 ) ) ;
#58780 = EDGE_LOOP ( 'NONE', ( #156868, #140983, #140869, #115238 ) ) ;
#58781 = CARTESIAN_POINT ( 'NONE',  ( 18.59999999999997655, -1.164121893230052995, -74.91484808557160591 ) ) ;
#58782 = AXIS2_PLACEMENT_3D ( 'NONE', #228945, #149424, #132409 ) ;
#58783 = AXIS2_PLACEMENT_3D ( 'NONE', #251502, #247663, #72911 ) ;
#58784 = AXIS2_PLACEMENT_3D ( 'NONE', #111542, #174128, #192365 ) ;
#58785 = DIRECTION ( 'NONE',  ( 1.836970198721029934E-16, -0.9770955615653316162, -0.2128009952263604232 ) ) ;
#58786 = CIRCLE ( 'NONE', #75412, 0.09999999999998898659 ) ;
#58787 = CARTESIAN_POINT ( 'NONE',  ( -16.87401514999227103, 14.14410934721911239, -219.1866934472504624 ) ) ;
#58788 = EDGE_LOOP ( 'NONE', ( #90132, #166833, #129797, #124235 ) ) ;
#58789 = DIRECTION ( 'NONE',  ( -1.000000000000000000, 2.952720810173289112E-16, 2.061873921506763405E-30 ) ) ;
#58791 = ORIENTED_EDGE ( 'NONE', *, *, #211893, .F. ) ;
#58790 = FACE_OUTER_BOUND ( 'NONE', #97730, .T. ) ;
#58792 = FACE_OUTER_BOUND ( 'NONE', #241326, .T. ) ;
#58794 = ORIENTED_EDGE ( 'NONE', *, *, #112790, .F. ) ;
#58793 = DIRECTION ( 'NONE',  ( 0.000000000000000000, -0.8660254037844420383, 0.4999999999999943379 ) ) ;
#58795 = EDGE_LOOP ( 'NONE', ( #6000, #217118, #104046, #37449, #75145 ) ) ;
#58796 = CARTESIAN_POINT ( 'NONE',  ( -20.54999999999999361, 31.44980407958351165, -233.5445995079518866 ) ) ;
#58797 = EDGE_CURVE ( 'NONE', #193670, #168409, #223443, .T. ) ;
#58798 = ORIENTED_EDGE ( 'NONE', *, *, #188916, .F. ) ;
#58799 = ORIENTED_EDGE ( 'NONE', *, *, #136539, .F. ) ;
#58800 = DIRECTION ( 'NONE',  ( -1.000000000000000000, 4.624352451196580357E-15, 3.439547145395922042E-14 ) ) ;
#58801 = DIRECTION ( 'NONE',  ( 1.000000000000000000, 0.000000000000000000, 0.000000000000000000 ) ) ;
#58803 = ORIENTED_EDGE ( 'NONE', *, *, #189526, .T. ) ;
#58802 = ORIENTED_EDGE ( 'NONE', *, *, #34323, .F. ) ;
#58804 = VERTEX_POINT ( 'NONE', #94469 ) ;
#58805 = DIRECTION ( 'NONE',  ( 0.000000000000000000, 0.000000000000000000, 1.000000000000000000 ) ) ;
#58806 = ORIENTED_EDGE ( 'NONE', *, *, #204273, .F. ) ;
#58807 = ORIENTED_EDGE ( 'NONE', *, *, #212165, .T. ) ;
#58808 = CARTESIAN_POINT ( 'NONE',  ( 20.94999999999999574, 18.81166555858608902, -229.8642012822692777 ) ) ;
#58809 = VERTEX_POINT ( 'NONE', #37105 ) ;
#58810 = DIRECTION ( 'NONE',  ( 0.000000000000000000, -1.000000000000000000, -6.982962677686265922E-15 ) ) ;
#58812 = CARTESIAN_POINT ( 'NONE',  ( 21.56666275994539461, 76.00000000001169553, -76.48047589141765457 ) ) ;
#58811 = FACE_OUTER_BOUND ( 'NONE', #152812, .T. ) ;
#58813 = AXIS2_PLACEMENT_3D ( 'NONE', #216249, #155039, #78026 ) ;
#58814 = VERTEX_POINT ( 'NONE', #21393 ) ;
#58815 = EDGE_CURVE ( 'NONE', #185762, #85685, #36227, .T. ) ;
#58817 = ORIENTED_EDGE ( 'NONE', *, *, #243117, .F. ) ;
#58816 = ORIENTED_EDGE ( 'NONE', *, *, #81626, .T. ) ;
#58818 = CARTESIAN_POINT ( 'NONE',  ( -18.59999999999999787, 76.00000000001237765, -170.0231074845243597 ) ) ;
#58819 = CARTESIAN_POINT ( 'NONE',  ( 23.14999999999999503, 11.65000000001116298, -160.4851942293460922 ) ) ;
#58820 = EDGE_CURVE ( 'NONE', #124226, #113211, #160896, .T. ) ;
#58821 = ORIENTED_EDGE ( 'NONE', *, *, #152482, .F. ) ;
#58822 = EDGE_CURVE ( 'NONE', #20388, #186519, #200009, .T. ) ;
#58823 = CIRCLE ( 'NONE', #217229, 0.1000000000000028644 ) ;
#58824 = CARTESIAN_POINT ( 'NONE',  ( 18.59999999999999076, 43.24695311518262031, -245.0026972281755491 ) ) ;
#58825 = ADVANCED_FACE ( 'NONE', ( #18786 ), #194451, .T. ) ;
#58826 = EDGE_LOOP ( 'NONE', ( #89905, #133014, #257254, #198901 ) ) ;
#58827 = EDGE_LOOP ( 'NONE', ( #106461, #246756, #145868, #152654 ) ) ;
#58828 = DIRECTION ( 'NONE',  ( -1.000000000000000000, 0.000000000000000000, -0.000000000000000000 ) ) ;
#58829 = ORIENTED_EDGE ( 'NONE', *, *, #150042, .T. ) ;
#58830 = CARTESIAN_POINT ( 'NONE',  ( -18.59999999999999787, 77.83585931145498193, -24.51866831572578675 ) ) ;
#58831 = DIRECTION ( 'NONE',  ( 0.000000000000000000, 0.000000000000000000, -1.000000000000000000 ) ) ;
#58832 = ORIENTED_EDGE ( 'NONE', *, *, #30338, .F. ) ;
#58833 = DIRECTION ( 'NONE',  ( 0.000000000000000000, 0.5000000000000209832, -0.8660254037844264952 ) ) ;
#58834 = CARTESIAN_POINT ( 'NONE',  ( 18.58719872626880942, 85.56664439761073027, -129.7006292881272884 ) ) ;
#58836 = CARTESIAN_POINT ( 'NONE',  ( -16.87333278164152972, 9.882609784590000501, -120.8668321938465482 ) ) ;
#58835 = CARTESIAN_POINT ( 'NONE',  ( 20.85000000000000142, 74.83412143252222393, -233.7087995678629966 ) ) ;
#58837 = CYLINDRICAL_SURFACE ( 'NONE', #202433, 2.000000000000003109 ) ;
#58838 = LINE ( 'NONE', #1450, #253694 ) ;
#58839 = CARTESIAN_POINT ( 'NONE',  ( -16.94226253665225457, 63.00806118293792224, -213.4140105000608116 ) ) ;
#58840 = FACE_OUTER_BOUND ( 'NONE', #152852, .T. ) ;
#58841 = DIRECTION ( 'NONE',  ( 0.000000000000000000, -1.000000000000000000, 0.000000000000000000 ) ) ;
#58842 = DIRECTION ( 'NONE',  ( 0.000000000000000000, -6.982962677686266711E-15, 1.000000000000000000 ) ) ;
#58843 = AXIS2_PLACEMENT_3D ( 'NONE', #123391, #38725, #142921 ) ;
#58844 = B_SPLINE_CURVE_WITH_KNOTS ( 'NONE', 3,
 ( #204084, #25476, #104956, #85393, #73610, #71033, #34484, #230085, #93133, #130984, #30625, #14909, #29358, #33212, #110131, #151860, #94415, #150555, #168871 ),
 .UNSPECIFIED., .F., .F.,
 ( 4, 3, 3, 3, 3, 3, 4 ),
 ( 0.000000000000000000, 2.646747978908424136E-05, 5.271166642127926225E-05, 9.008788829883960267E-05, 0.0001426648776560873473, 0.0001897378458659781616, 0.0001917382627806208306 ),
 .UNSPECIFIED. ) ;
#58845 = EDGE_LOOP ( 'NONE', ( #130493, #218182, #222, #105647 ) ) ;
#58846 = VECTOR ( 'NONE', #205411, 1000.000000000000000 ) ;
#58847 = EDGE_CURVE ( 'NONE', #13912, #134549, #236548, .T. ) ;
#58848 = ADVANCED_FACE ( 'NONE', ( #197424 ), #216978, .T. ) ;
#58849 = AXIS2_PLACEMENT_3D ( 'NONE', #40434, #104203, #142054 ) ;
#58851 = ORIENTED_EDGE ( 'NONE', *, *, #12293, .T. ) ;
#58850 = VERTEX_POINT ( 'NONE', #59165 ) ;
#58852 = VERTEX_POINT ( 'NONE', #177888 ) ;
#58853 = ORIENTED_EDGE ( 'NONE', *, *, #215764, .T. ) ;
#58854 = CARTESIAN_POINT ( 'NONE',  ( -21.05000000000000071, 0.4810385098657082859, -209.0827657365571213 ) ) ;
#58855 = LINE ( 'NONE', #219229, #7092 ) ;
#58857 = DIRECTION ( 'NONE',  ( 1.000000000000000000, -0.000000000000000000, -0.000000000000000000 ) ) ;
#58856 = DIRECTION ( 'NONE',  ( 0.000000000000000000, 0.3970902486047482305, -0.9177795674686920480 ) ) ;
#58858 = VERTEX_POINT ( 'NONE', #20093 ) ;
#58859 = CARTESIAN_POINT ( 'NONE',  ( 20.94999999999999574, 77.16270174995010223, -128.4231074845242802 ) ) ;
#58860 =( LENGTH_UNIT ( ) NAMED_UNIT ( * ) SI_UNIT ( .MILLI., .METRE. ) );
#58861 = EDGE_CURVE ( 'NONE', #258063, #21929, #257343, .T. ) ;
#58862 = DIRECTION ( 'NONE',  ( -1.000000000000000000, -0.000000000000000000, -0.000000000000000000 ) ) ;
#58864 = AXIS2_PLACEMENT_3D ( 'NONE', #76090, #209503, #10027 ) ;
#58863 = CARTESIAN_POINT ( 'NONE',  ( 20.85000000000000142, 77.83585931145600512, -158.5186683157258187 ) ) ;
#58865 = EDGE_CURVE ( 'NONE', #211037, #76531, #94449, .T. ) ;
#58866 = CARTESIAN_POINT ( 'NONE',  ( 21.05000000000000071, 5.000000000011153745, -112.9052660189131245 ) ) ;
#58867 = ORIENTED_EDGE ( 'NONE', *, *, #64439, .F. ) ;
#58868 = CARTESIAN_POINT ( 'NONE',  ( -18.59999999999999787, 23.38726701055792745, -229.1122755113798632 ) ) ;
#58869 = CARTESIAN_POINT ( 'NONE',  ( -21.09096482362058111, 0.03944827878523731596, -94.13645563459554921 ) ) ;
#58870 = ORIENTED_EDGE ( 'NONE', *, *, #159592, .F. ) ;
#58871 = CARTESIAN_POINT ( 'NONE',  ( -21.05000000000000071, -11.48912529306490349, -70.10000000000005116 ) ) ;
#58872 = SPHERICAL_SURFACE ( 'NONE', #27845, 0.1000000000000000056 ) ;
#58873 = EDGE_CURVE ( 'NONE', #58482, #169346, #227146, .T. ) ;
#58874 = DIRECTION ( 'NONE',  ( 6.938893903907499746E-14, -0.9126074666063545004, -0.4088369013363783999 ) ) ;
#58875 = CARTESIAN_POINT ( 'NONE',  ( -20.64999999999999858, -9.399999999988850163, -110.3939691226524786 ) ) ;
#58876 = CARTESIAN_POINT ( 'NONE',  ( 20.94999999999999929, 1.115600667400684642E-11, -100.5000000000000284 ) ) ;
#58877 = EDGE_LOOP ( 'NONE', ( #221359, #16842, #63293 ) ) ;
#58878 = CYLINDRICAL_SURFACE ( 'NONE', #136056, 0.09999999999999939493 ) ;
#58879 = DIRECTION ( 'NONE',  ( 1.000000000000000000, -0.000000000000000000, -0.000000000000000000 ) ) ;
#58880 = DIRECTION ( 'NONE',  ( 0.000000000000000000, 0.000000000000000000, -1.000000000000000000 ) ) ;
#58883 = CARTESIAN_POINT ( 'NONE',  ( -23.15000000000000213, 11.65000000001115588, -167.4999999999999716 ) ) ;
#58882 = AXIS2_PLACEMENT_3D ( 'NONE', #29330, #205333, #230059 ) ;
#58881 = DIRECTION ( 'NONE',  ( 0.000000000000000000, 0.000000000000000000, -1.000000000000000000 ) ) ;
#58885 = CARTESIAN_POINT ( 'NONE',  ( 18.49999999999999645, 1.115600667400684642E-11, -167.4999999999999716 ) ) ;
#58884 = AXIS2_PLACEMENT_3D ( 'NONE', #203012, #24408, #103894 ) ;
#58886 = AXIS2_PLACEMENT_3D ( 'NONE', #68590, #150689, #226345 ) ;
#58888 = EDGE_CURVE ( 'NONE', #174034, #33900, #231857, .T. ) ;
#58887 = DIRECTION ( 'NONE',  ( 0.000000000000000000, -7.116814260417668513E-15, 1.000000000000000000 ) ) ;
#58889 = FACE_OUTER_BOUND ( 'NONE', #197846, .T. ) ;
#58890 = DIRECTION ( 'NONE',  ( 1.000000000000000000, 0.000000000000000000, 0.000000000000000000 ) ) ;
#58891 = EDGE_LOOP ( 'NONE', ( #77121, #194800, #181038, #22546, #241813 ) ) ;
#58892 = EDGE_LOOP ( 'NONE', ( #2082, #229861, #224542, #146085 ) ) ;
#58893 = ORIENTED_EDGE ( 'NONE', *, *, #201559, .F. ) ;
#58894 = ADVANCED_FACE ( 'NONE', ( #97008 ), #176609, .F. ) ;
#58895 = CARTESIAN_POINT ( 'NONE',  ( -23.15000000000000213, -9.499999999988848032, -76.89396912265249284 ) ) ;
#58896 = AXIS2_PLACEMENT_3D ( 'NONE', #63459, #81710, #118325 ) ;
#58897 = CARTESIAN_POINT ( 'NONE',  ( -18.41799967126724979, -9.499999999988851584, -174.5320698132565269 ) ) ;
#58898 = LINE ( 'NONE', #38101, #12827 ) ;
#58899 = VERTEX_POINT ( 'NONE', #83861 ) ;
#58900 = CARTESIAN_POINT ( 'NONE',  ( 23.15000000000000213, -8.663551401858002876, -43.02410111806730697 ) ) ;
#58901 = CARTESIAN_POINT ( 'NONE',  ( -13.77083647240106501, 9.457410930301318075, -51.99991590874629566 ) ) ;
#58902 = CARTESIAN_POINT ( 'NONE',  ( 21.05000000000000071, 5.850000000011105428, -177.6324972242779268 ) ) ;
#58903 = DIRECTION ( 'NONE',  ( 1.000000000000000000, 7.304098846218105085E-16, 4.217023435051677501E-16 ) ) ;
#58905 = ORIENTED_EDGE ( 'NONE', *, *, #200030, .F. ) ;
#58904 = DIRECTION ( 'NONE',  ( -1.000000000000000000, 1.646408749285563322E-14, -1.073024830501002749E-15 ) ) ;
#58907 = DIRECTION ( 'NONE',  ( 1.000000000000000000, 0.000000000000000000, 0.000000000000000000 ) ) ;
#58906 = DIRECTION ( 'NONE',  ( 0.000000000000000000, -6.982962677686266711E-15, 1.000000000000000000 ) ) ;
#58909 = CARTESIAN_POINT ( 'NONE',  ( 19.97071067811865319, 64.27928932189281852, -44.81452884076170307 ) ) ;
#58908 = AXIS2_PLACEMENT_3D ( 'NONE', #233619, #95380, #254424 ) ;
#58910 = CARTESIAN_POINT ( 'NONE',  ( 18.59999999999999787, -10.80884033489985363, 6.100000000000002309 ) ) ;
#58911 = CARTESIAN_POINT ( 'NONE',  ( -20.00889983613310008, 5.561941060815491333, 16.56258203121810268 ) ) ;
#58912 = DIRECTION ( 'NONE',  ( -1.000000000000000000, 3.151514657663852580E-16, -8.547182517843351137E-17 ) ) ;
#58913 = ORIENTED_EDGE ( 'NONE', *, *, #87942, .T. ) ;
#58914 = CIRCLE ( 'NONE', #225515, 0.1000000000000052097 ) ;
#58915 =( LENGTH_UNIT ( ) NAMED_UNIT ( * ) SI_UNIT ( .MILLI., .METRE. ) );
#58916 = DIRECTION ( 'NONE',  ( 0.000000000000000000, 0.8814952561688437216, -0.4721928772777334582 ) ) ;
#58917 = EDGE_LOOP ( 'NONE', ( #157509, #252853, #16875, #13193 ) ) ;
#58918 = CIRCLE ( 'NONE', #212898, 0.09999999999999939493 ) ;
#58919 = CARTESIAN_POINT ( 'NONE',  ( -16.87665923198281348, 66.05000000001255955, -182.6731074845244223 ) ) ;
#58920 = EDGE_LOOP ( 'NONE', ( #32432, #71990, #159264, #170936 ) ) ;
#58921 = DIRECTION ( 'NONE',  ( -1.000000000000000000, 7.510212038922847255E-17, -1.676432719286211941E-16 ) ) ;
#58922 = AXIS2_PLACEMENT_3D ( 'NONE', #178928, #158093, #242 ) ;
#58924 = CARTESIAN_POINT ( 'NONE',  ( -16.94052228080551714, 9.986279733098838207, -20.89037550266942134 ) ) ;
#58923 = CIRCLE ( 'NONE', #204692, 1.900000000000012790 ) ;
#58925 = CARTESIAN_POINT ( 'NONE',  ( -21.05000000000000071, 44.47083028126616000, -247.4212268238128161 ) ) ;
#58926 = ORIENTED_EDGE ( 'NONE', *, *, #109214, .T. ) ;
#58927 = EDGE_LOOP ( 'NONE', ( #147936, #241178, #47656, #50358 ) ) ;
#58928 = AXIS2_PLACEMENT_3D ( 'NONE', #124313, #103432, #82571 ) ;
#58929 = CYLINDRICAL_SURFACE ( 'NONE', #256640, 0.1000000000000098310 ) ;
#58930 = CARTESIAN_POINT ( 'NONE',  ( -21.44999999999999929, 7.350000000011155166, -188.7499999999999716 ) ) ;
#58931 = DIRECTION ( 'NONE',  ( 1.000000000000000000, 0.000000000000000000, 0.000000000000000000 ) ) ;
#58932 = CARTESIAN_POINT ( 'NONE',  ( 16.87683809663749557, 66.05000000001183480, -82.17310748452439384 ) ) ;
#58933 = EDGE_CURVE ( 'NONE', #184831, #211733, #65233, .T. ) ;
#58935 = CARTESIAN_POINT ( 'NONE',  ( 20.94999999999999929, 1.115600667400684642E-11, -200.9999999999999432 ) ) ;
#58934 = CARTESIAN_POINT ( 'NONE',  ( -21.05000000000000071, 44.52640028187936849, -247.3006740988509193 ) ) ;
#58936 = TOROIDAL_SURFACE ( 'NONE', #213086, 0.2000000000000000111, 0.1000000000000000056 ) ;
#58937 = DIRECTION ( 'NONE',  ( -1.000000000000000000, 0.000000000000000000, 0.000000000000000000 ) ) ;
#58938 = DIRECTION ( 'NONE',  ( 0.000000000000000000, 0.000000000000000000, 1.000000000000000000 ) ) ;
#58940 = FACE_OUTER_BOUND ( 'NONE', #207884, .T. ) ;
#58939 = VECTOR ( 'NONE', #161724, 999.9999999999998863 ) ;
#58941 = ORIENTED_EDGE ( 'NONE', *, *, #17861, .F. ) ;
#58942 = DIRECTION ( 'NONE',  ( 1.000000000000000000, -7.304098846218133681E-16, 4.217023435051677994E-16 ) ) ;
#58944 = ORIENTED_EDGE ( 'NONE', *, *, #86680, .F. ) ;
#58943 = CARTESIAN_POINT ( 'NONE',  ( 20.09999999999999787, 66.25000000001156764, -48.67310748452440095 ) ) ;
#58945 = DIRECTION ( 'NONE',  ( 0.000000000000000000, 0.9999631594459055250, 0.008583690987131395445 ) ) ;
#58947 = CARTESIAN_POINT ( 'NONE',  ( -20.54999999999999716, 1.940186915899009490, -46.32911921105333164 ) ) ;
#58946 = CARTESIAN_POINT ( 'NONE',  ( 20.27550659511088682, 9.216043722520002035, -176.7499999999999716 ) ) ;
#58948 = AXIS2_PLACEMENT_3D ( 'NONE', #167718, #149431, #50287 ) ;
#58949 = EDGE_CURVE ( 'NONE', #224430, #70177, #5624, .T. ) ;
#58950 = ORIENTED_EDGE ( 'NONE', *, *, #177076, .T. ) ;
#58952 = CARTESIAN_POINT ( 'NONE',  ( -22.94999999999999929, 11.50977166988710820, 1.786320531569725478 ) ) ;
#58951 = CARTESIAN_POINT ( 'NONE',  ( -21.05000000000000071, 76.00000000001173817, -73.52310748452431710 ) ) ;
#58953 = CARTESIAN_POINT ( 'NONE',  ( -18.50000000000000000, 65.70729864261004138, -97.56574559737242680 ) ) ;
#58954 = LINE ( 'NONE', #138494, #138770 ) ;
#58955 = DIRECTION ( 'NONE',  ( -1.073024830501117725E-15, 0.000000000000000000, 1.000000000000000000 ) ) ;
#58957 = CARTESIAN_POINT ( 'NONE',  ( -18.54270223418607699, 85.62410550289477840, -96.28217243411681636 ) ) ;
#58956 = CIRCLE ( 'NONE', #254745, 0.09999999999999982514 ) ;
#58958 = ORIENTED_EDGE ( 'NONE', *, *, #221345, .T. ) ;
#58959 = CARTESIAN_POINT ( 'NONE',  ( -22.49436431346200038, 31.83493791481901880, -238.9466831125989756 ) ) ;
#58961 = ADVANCED_FACE ( 'NONE', ( #44786 ), #68203, .F. ) ;
#58960 = VERTEX_POINT ( 'NONE', #244248 ) ;
#58962 = CARTESIAN_POINT ( 'NONE',  ( 22.50000000000000000, 75.95437663941648054, -215.1736118230719512 ) ) ;
#58963 = ORIENTED_EDGE ( 'NONE', *, *, #15009, .F. ) ;
#58965 = DIRECTION ( 'NONE',  ( -0.000000000000000000, -0.000000000000000000, -1.000000000000000000 ) ) ;
#58964 = VECTOR ( 'NONE', #237336, 1000.000000000000000 ) ;
#58966 = AXIS2_PLACEMENT_3D ( 'NONE', #50913, #30119, #88763 ) ;
#58967 = ORIENTED_EDGE ( 'NONE', *, *, #118194, .F. ) ;
#58968 = CIRCLE ( 'NONE', #163074, 0.09999999999999939493 ) ;
#58969 = CYLINDRICAL_SURFACE ( 'NONE', #126720, 1.749999999999999778 ) ;
#58970 = CIRCLE ( 'NONE', #246438, 0.09999999999999939493 ) ;
#58971 = EDGE_CURVE ( 'NONE', #217875, #78646, #41090, .T. ) ;
#58973 = EDGE_CURVE ( 'NONE', #120817, #155038, #102812, .T. ) ;
#58972 = CARTESIAN_POINT ( 'NONE',  ( 20.85000000000000142, -1.835859311432481045, -112.0044391687985694 ) ) ;
#58974 = ORIENTED_EDGE ( 'NONE', *, *, #208638, .F. ) ;
#58975 = EDGE_CURVE ( 'NONE', #108203, #87151, #8236, .T. ) ;
#58976 = DIRECTION ( 'NONE',  ( 1.000000000000000000, 0.000000000000000000, 0.000000000000000000 ) ) ;
#58977 = CARTESIAN_POINT ( 'NONE',  ( 23.15000000000000213, -8.663551401869154844, -23.97589888193268948 ) ) ;
#58978 = DIRECTION ( 'NONE',  ( 1.000000000000000000, 0.000000000000000000, 0.000000000000000000 ) ) ;
#58980 = DIRECTION ( 'NONE',  ( -1.000000000000000000, -2.952720810173289112E-16, 0.000000000000000000 ) ) ;
#58979 = B_SPLINE_CURVE_WITH_KNOTS ( 'NONE', 3,
 ( #215129, #156475, #76891, #39082, #255485, #238539, #79450, #195590, #20801, #159035 ),
 .UNSPECIFIED., .F., .F.,
 ( 4, 3, 3, 4 ),
 ( 0.000000000000000000, 0.0002000000000002884074, 0.001000000000045107602, 0.001967863649472132576 ),
 .UNSPECIFIED. ) ;
#58981 = LINE ( 'NONE', #36923, #212011 ) ;
#58982 = CARTESIAN_POINT ( 'NONE',  ( 19.90621891164687440, 62.38985952047473660, -208.8167298195660635 ) ) ;
#58983 = ORIENTED_EDGE ( 'NONE', *, *, #113980, .F. ) ;
#58984 = AXIS2_PLACEMENT_3D ( 'NONE', #134550, #35511, #215388 ) ;
#58985 = CARTESIAN_POINT ( 'NONE',  ( -20.94999999999999929, -11.64999999998884306, -63.89999999999999858 ) ) ;
#58986 = ORIENTED_EDGE ( 'NONE', *, *, #36762, .F. ) ;
#58988 = ORIENTED_EDGE ( 'NONE', *, *, #57581, .F. ) ;
#58987 = DIRECTION ( 'NONE',  ( 0.000000000000000000, -0.9908441862701610203, 0.1350103645451807555 ) ) ;
#58989 = ORIENTED_EDGE ( 'NONE', *, *, #201246, .F. ) ;
#58990 = DIRECTION ( 'NONE',  ( 1.000000000000000000, 0.000000000000000000, 0.000000000000000000 ) ) ;
#58992 = ADVANCED_FACE ( 'NONE', ( #64352 ), #125597, .T. ) ;
#58991 = DIRECTION ( 'NONE',  ( 0.000000000000000000, 0.2128009952263628102, -0.9770955615653308390 ) ) ;
#58993 = LINE ( 'NONE', #81138, #129950 ) ;
#58994 = DIRECTION ( 'NONE',  ( 1.000000000000000000, 0.000000000000000000, 0.000000000000000000 ) ) ;
#58995 = DIRECTION ( 'NONE',  ( 0.000000000000000000, 0.9908441862701697911, -0.1350103645451153911 ) ) ;
#58996 = EDGE_LOOP ( 'NONE', ( #19828, #222336, #36164, #177293, #236019, #231280, #253436, #126980, #234292, #4625, #101438, #39228, #24076, #155294 ) ) ;
#58997 = CARTESIAN_POINT ( 'NONE',  ( -16.86132326855786090, 9.950000000011137047, -146.6986357846683688 ) ) ;
#58998 = DIRECTION ( 'NONE',  ( 1.000000000000000000, -2.952720810173289112E-16, -2.061873921506763405E-30 ) ) ;
#58999 = EDGE_LOOP ( 'NONE', ( #181965, #209421, #20166, #224001 ) ) ;
#59001 = VERTEX_POINT ( 'NONE', #9499 ) ;
#59000 = CARTESIAN_POINT ( 'NONE',  ( -20.65000000000000568, 68.75000000001161027, -60.27310748452437394 ) ) ;
#59003 = EDGE_CURVE ( 'NONE', #65541, #210276, #69541, .T. ) ;
#59002 = FACE_OUTER_BOUND ( 'NONE', #82920, .T. ) ;
#59004 = CARTESIAN_POINT ( 'NONE',  ( -16.80891096016346253, 9.950000000011137047, -79.63233719273293332 ) ) ;
#59005 = ORIENTED_EDGE ( 'NONE', *, *, #241713, .T. ) ;
#59006 = CIRCLE ( 'NONE', #109090, 0.09999999999998714084 ) ;
#59007 = DIRECTION ( 'NONE',  ( 0.000000000000000000, 0.1335171055202867274, -0.9910465087640866200 ) ) ;
#59008 = ORIENTED_EDGE ( 'NONE', *, *, #26907, .F. ) ;
#59009 = DIRECTION ( 'NONE',  ( 1.000000000000000000, 0.000000000000000000, 0.000000000000000000 ) ) ;
#59010 = CYLINDRICAL_SURFACE ( 'NONE', #143737, 0.09999999999999681366 ) ;
#59011 = CARTESIAN_POINT ( 'NONE',  ( 20.87155475150661132, 64.25000000001249134, -176.9275209553668162 ) ) ;
#59012 = DIRECTION ( 'NONE',  ( -1.000000000000000000, 0.000000000000000000, 0.000000000000000000 ) ) ;
#59013 = CIRCLE ( 'NONE', #175782, 0.09999999999999982514 ) ;
#59014 = AXIS2_PLACEMENT_3D ( 'NONE', #167309, #143851, #85137 ) ;
#59016 = ORIENTED_EDGE ( 'NONE', *, *, #233725, .T. ) ;
#59015 = VECTOR ( 'NONE', #38198, 1000.000000000000000 ) ;
#59017 = CARTESIAN_POINT ( 'NONE',  ( 21.05000000000000071, 67.12338541492448485, -61.13802700567971016 ) ) ;
#59018 = ADVANCED_FACE ( 'NONE', ( #48626 ), #222103, .T. ) ;
#59019 = ADVANCED_FACE ( 'NONE', ( #166040 ), #126892, .F. ) ;
#59020 = VERTEX_POINT ( 'NONE', #202573 ) ;
#59021 = DIRECTION ( 'NONE',  ( 0.000000000000000000, 0.8814952561688513821, -0.4721928772777189698 ) ) ;
#59022 = CARTESIAN_POINT ( 'NONE',  ( -23.25000000000000000, 87.75000000001143974, -39.12310748452424747 ) ) ;
#59024 = ORIENTED_EDGE ( 'NONE', *, *, #52353, .T. ) ;
#59023 = DIRECTION ( 'NONE',  ( 1.000000000000000000, 2.952720810173289112E-16, -0.000000000000000000 ) ) ;
#59025 = CARTESIAN_POINT ( 'NONE',  ( 21.09787244211745971, 67.22462929267425125, -57.28385410020680268 ) ) ;
#59026 = CARTESIAN_POINT ( 'NONE',  ( 23.24999999999999289, 12.62988036037870998, -223.4632815780722410 ) ) ;
#59028 = ADVANCED_FACE ( 'NONE', ( #26520 ), #65619, .T. ) ;
#59027 = CARTESIAN_POINT ( 'NONE',  ( 20.27550659511089037, 9.216043722519994930, -54.35000000000000142 ) ) ;
#59030 = EDGE_CURVE ( 'NONE', #66328, #43089, #188152, .T. ) ;
#59029 = CARTESIAN_POINT ( 'NONE',  ( -18.40000000000000213, 70.35000000001201670, -115.6731074845243370 ) ) ;
#59031 = CARTESIAN_POINT ( 'NONE',  ( 20.94999999999999929, 71.14953271029297355, -191.4888400755227167 ) ) ;
#59032 = FACE_OUTER_BOUND ( 'NONE', #28009, .T. ) ;
#59033 = CARTESIAN_POINT ( 'NONE',  ( 21.07933241753356768, 6.328645948390905218, -66.90662040958073931 ) ) ;
#59035 = ORIENTED_EDGE ( 'NONE', *, *, #238325, .F. ) ;
#59034 = CARTESIAN_POINT ( 'NONE',  ( 20.94999999999999929, 0.000000000000000000, 0.000000000000000000 ) ) ;
#59036 = TOROIDAL_SURFACE ( 'NONE', #175604, 0.2000000000000000111, 0.1000000000000000056 ) ;
#59037 = ADVANCED_FACE ( 'NONE', ( #124326 ), #103446, .F. ) ;
#59038 = EDGE_CURVE ( 'NONE', #23492, #94251, #98501, .T. ) ;
#59040 = ADVANCED_FACE ( 'NONE', ( #10798 ), #190748, .F. ) ;
#59039 = ADVANCED_FACE ( 'NONE', ( #46055 ), #14678, .F. ) ;
#59041 = FACE_OUTER_BOUND ( 'NONE', #9092, .T. ) ;
#59042 = ORIENTED_EDGE ( 'NONE', *, *, #193195, .T. ) ;
#59043 = EDGE_LOOP ( 'NONE', ( #246244, #193355, #75596, #145820 ) ) ;
#59044 = CARTESIAN_POINT ( 'NONE',  ( -18.43634282235120736, 85.67978719993963921, -62.86245559907034419 ) ) ;
#59045 = CARTESIAN_POINT ( 'NONE',  ( -18.48550754432078236, 85.46339977857238068, -196.4743177321096823 ) ) ;
#59046 = ORIENTED_EDGE ( 'NONE', *, *, #117563, .T. ) ;
#59047 = DIRECTION ( 'NONE',  ( 0.000000000000000000, 0.000000000000000000, -1.000000000000000000 ) ) ;
#59048 = EDGE_CURVE ( 'NONE', #127649, #82517, #2865, .T. ) ;
#59049 = AXIS2_PLACEMENT_3D ( 'NONE', #181577, #23803, #83695 ) ;
#59050 = AXIS2_PLACEMENT_3D ( 'NONE', #249798, #169018, #30777 ) ;
#59051 = CARTESIAN_POINT ( 'NONE',  ( -18.49346865148326202, 85.44307379853647433, -62.33791122920943906 ) ) ;
#59052 = AXIS2_PLACEMENT_3D ( 'NONE', #3145, #125679, #21469 ) ;
#59053 = VERTEX_POINT ( 'NONE', #232434 ) ;
#59054 = ADVANCED_FACE ( 'NONE', ( #112478, #12104 ), #34243, .F. ) ;
#59055 = EDGE_CURVE ( 'NONE', #232170, #7325, #72066, .T. ) ;
#59056 = DIRECTION ( 'NONE',  ( 0.000000000000000000, 1.000000000000000000, 2.891205793294679805E-16 ) ) ;
#59057 = FACE_OUTER_BOUND ( 'NONE', #244461, .T. ) ;
#59058 = EDGE_CURVE ( 'NONE', #95600, #62294, #177705, .T. ) ;
#59059 = ORIENTED_EDGE ( 'NONE', *, *, #238403, .F. ) ;
#59060 = CARTESIAN_POINT ( 'NONE',  ( -23.15000000000000213, 20.02211948220868365, -235.8179285081017156 ) ) ;
#59061 = ORIENTED_EDGE ( 'NONE', *, *, #52727, .T. ) ;
#59062 = CARTESIAN_POINT ( 'NONE',  ( -21.56666275994539816, 76.00000000001242029, -176.9804758914176830 ) ) ;
#59064 = VERTEX_POINT ( 'NONE', #49913 ) ;
#59063 = CARTESIAN_POINT ( 'NONE',  ( 21.04999999999999716, 6.441084688482184184, -134.0177194333088835 ) ) ;
#59065 = EDGE_CURVE ( 'NONE', #246301, #158894, #57016, .T. ) ;
#59066 = FACE_OUTER_BOUND ( 'NONE', #21488, .T. ) ;
#59067 = ORIENTED_EDGE ( 'NONE', *, *, #203394, .T. ) ;
#59068 = DIRECTION ( 'NONE',  ( 1.000000000000000000, -3.469446951953718318E-14, 2.003086131649645455E-14 ) ) ;
#59069 = EDGE_LOOP ( 'NONE', ( #49477, #92003, #36239, #127699 ) ) ;
#59071 = ORIENTED_EDGE ( 'NONE', *, *, #87330, .F. ) ;
#59070 = VERTEX_POINT ( 'NONE', #151619 ) ;
#59072 = CARTESIAN_POINT ( 'NONE',  ( -20.94999999999999929, 74.16465844978745281, -91.46795619196133487 ) ) ;
#59073 = ORIENTED_EDGE ( 'NONE', *, *, #10618, .T. ) ;
#59074 = DIRECTION ( 'NONE',  ( 0.000000000000000000, -0.9126074666063660468, -0.4088369013363524762 ) ) ;
#59075 = VERTEX_POINT ( 'NONE', #189440 ) ;
#59076 = ORIENTED_EDGE ( 'NONE', *, *, #214510, .T. ) ;
#59077 = CARTESIAN_POINT ( 'NONE',  ( -21.05000000000000071, 26.25728039895700761, -243.9792867493661106 ) ) ;
#59079 = CYLINDRICAL_SURFACE ( 'NONE', #105624, 0.1000000000000028644 ) ;
#59078 = VECTOR ( 'NONE', #256655, 1000.000000000000000 ) ;
#59081 = ORIENTED_EDGE ( 'NONE', *, *, #38786, .F. ) ;
#59080 = DIRECTION ( 'NONE',  ( -1.000000000000000000, 0.000000000000000000, 0.000000000000000000 ) ) ;
#59082 = FACE_OUTER_BOUND ( 'NONE', #201557, .T. ) ;
#59083 = ORIENTED_EDGE ( 'NONE', *, *, #158042, .F. ) ;
#59084 = FACE_OUTER_BOUND ( 'NONE', #221977, .T. ) ;
#59085 = CARTESIAN_POINT ( 'NONE',  ( -20.94999999999994600, 67.85000000001119247, -25.49719488170504533 ) ) ;
#59086 = CARTESIAN_POINT ( 'NONE',  ( 23.14999999999999503, 69.45000000001186891, -90.67310748452435121 ) ) ;
#59087 = VECTOR ( 'NONE', #88409, 1000.000000000000000 ) ;
#59088 = ORIENTED_EDGE ( 'NONE', *, *, #27307, .T. ) ;
#59089 = DIRECTION ( 'NONE',  ( 0.000000000000000000, 0.2617529984165152257, 0.9651348961777124202 ) ) ;
#59090 = CARTESIAN_POINT ( 'NONE',  ( -18.39999999999999858, 37.95493834378067532, -261.2294694241335264 ) ) ;
#59091 = CARTESIAN_POINT ( 'NONE',  ( -21.05000000000000071, 76.00000000001170974, -69.52310748452431710 ) ) ;
#59092 = CIRCLE ( 'NONE', #34222, 0.09999999999999939493 ) ;
#59093 = VECTOR ( 'NONE', #243169, 1000.000000000000000 ) ;
#59095 = ORIENTED_EDGE ( 'NONE', *, *, #250769, .F. ) ;
#59094 = AXIS2_PLACEMENT_3D ( 'NONE', #196396, #125537, #77720 ) ;
#59096 = CARTESIAN_POINT ( 'NONE',  ( -18.50000000000000000, 11.75000000001115552, -79.15000000000003411 ) ) ;
#59097 = ORIENTED_EDGE ( 'NONE', *, *, #123963, .F. ) ;
#59098 = ORIENTED_EDGE ( 'NONE', *, *, #5983, .F. ) ;
#59099 = AXIS2_PLACEMENT_3D ( 'NONE', #258074, #41665, #196850 ) ;
#59100 = CARTESIAN_POINT ( 'NONE',  ( -17.11825945287482753, 65.95000000001159890, -56.87310748452438958 ) ) ;
#59101 = VERTEX_POINT ( 'NONE', #90312 ) ;
#59102 = VECTOR ( 'NONE', #168043, 1000.000000000000000 ) ;
#59103 = ORIENTED_EDGE ( 'NONE', *, *, #154802, .T. ) ;
#59104 = FACE_OUTER_BOUND ( 'NONE', #193306, .T. ) ;
#59105 = LINE ( 'NONE', #55257, #158447 ) ;
#59106 = ORIENTED_EDGE ( 'NONE', *, *, #130936, .F. ) ;
#59107 = ORIENTED_EDGE ( 'NONE', *, *, #19615, .T. ) ;
#59108 = CARTESIAN_POINT ( 'NONE',  ( 20.02499999999999858, 9.750000000011153745, -188.6499999999999488 ) ) ;
#59109 = AXIS2_PLACEMENT_3D ( 'NONE', #224675, #125583, #206411 ) ;
#59110 = CARTESIAN_POINT ( 'NONE',  ( -18.40000000000000213, 10.58889512527366428, -208.1606840254082158 ) ) ;
#59112 = VERTEX_POINT ( 'NONE', #32974 ) ;
#59111 = AXIS2_PLACEMENT_3D ( 'NONE', #160929, #222138, #22715 ) ;
#59113 = EDGE_CURVE ( 'NONE', #203476, #32613, #236115, .T. ) ;
#59114 = ORIENTED_EDGE ( 'NONE', *, *, #118288, .T. ) ;
#59115 = CIRCLE ( 'NONE', #250683, 0.1000000000000106498 ) ;
#59116 = ADVANCED_FACE ( 'NONE', ( #15964 ), #169917, .F. ) ;
#59117 = VECTOR ( 'NONE', #71296, 1000.000000000000000 ) ;
#59118 = EDGE_LOOP ( 'NONE', ( #104916, #60491, #177355, #208383 ) ) ;
#59119 = AXIS2_PLACEMENT_3D ( 'NONE', #74600, #12797, #149741 ) ;
#59120 = EDGE_CURVE ( 'NONE', #172421, #81295, #134570, .T. ) ;
#59121 = CYLINDRICAL_SURFACE ( 'NONE', #93000, 0.1000000000000028644 ) ;
#59122 = EDGE_CURVE ( 'NONE', #109066, #225500, #251968, .T. ) ;
#59123 = AXIS2_PLACEMENT_3D ( 'NONE', #188644, #169124, #20160 ) ;
#59124 = CARTESIAN_POINT ( 'NONE',  ( -16.79363873026997922, 14.15705967318782399, -219.2515591053820003 ) ) ;
#59125 = LINE ( 'NONE', #179142, #39277 ) ;
#59126 = CARTESIAN_POINT ( 'NONE',  ( 21.05000000000000071, 65.45624872451672616, -162.4667196758603893 ) ) ;
#59127 = CARTESIAN_POINT ( 'NONE',  ( -21.05000000000000071, 64.35000000001166143, -69.42310748452440805 ) ) ;
#59128 = CARTESIAN_POINT ( 'NONE',  ( 18.59999999999998366, 7.021664781911246322, -137.8335654018973457 ) ) ;
#59130 = DIRECTION ( 'NONE',  ( -1.000000000000000000, 0.000000000000000000, 0.000000000000000000 ) ) ;
#59129 = CARTESIAN_POINT ( 'NONE',  ( -23.15000000000000213, 73.40000000001222702, -148.2731074845243313 ) ) ;
#59131 = CARTESIAN_POINT ( 'NONE',  ( 21.00000000000000000, 1.212568896937007645, -8.000000000000000000 ) ) ;
#59132 = CARTESIAN_POINT ( 'NONE',  ( -16.93710578446436088, 23.21501689610121844, -231.0619907376567710 ) ) ;
#59133 = DIRECTION ( 'NONE',  ( 0.000000000000000000, 0.000000000000000000, -1.000000000000000000 ) ) ;
#59134 = AXIS2_PLACEMENT_3D ( 'NONE', #179321, #222245, #201419 ) ;
#59135 = CARTESIAN_POINT ( 'NONE',  ( 21.05095171578076574, 44.17356502458446244, -236.5680974831273033 ) ) ;
#59136 = AXIS2_PLACEMENT_3D ( 'NONE', #12819, #31115, #190162 ) ;
#59138 = VERTEX_POINT ( 'NONE', #109877 ) ;
#59137 = AXIS2_PLACEMENT_3D ( 'NONE', #249546, #206553, #7059 ) ;
#59139 = ADVANCED_FACE ( 'NONE', ( #154209 ), #133317, .F. ) ;
#59140 = AXIS2_PLACEMENT_3D ( 'NONE', #55673, #149711, #229234 ) ;
#59141 = EDGE_CURVE ( 'NONE', #212963, #120605, #35533, .T. ) ;
#59142 = ORIENTED_EDGE ( 'NONE', *, *, #8112, .F. ) ;
#59143 = CARTESIAN_POINT ( 'NONE',  ( -20.15000000000000568, 66.70857864377420299, -48.27310748452438816 ) ) ;
#59144 = DIRECTION ( 'NONE',  ( 1.000000000000000000, 0.000000000000000000, 0.000000000000000000 ) ) ;
#59145 = VERTEX_POINT ( 'NONE', #95462 ) ;
#59146 =( NAMED_UNIT ( * ) SI_UNIT ( $, .STERADIAN. ) SOLID_ANGLE_UNIT ( ) );
#59147 = EDGE_CURVE ( 'NONE', #210574, #51994, #190157, .T. ) ;
#59148 = DIRECTION ( 'NONE',  ( 0.000000000000000000, 6.769652589177784668E-15, -1.000000000000000000 ) ) ;
#59149 = EDGE_CURVE ( 'NONE', #28188, #27371, #54333, .T. ) ;
#59150 = CARTESIAN_POINT ( 'NONE',  ( -16.89146115310546037, 9.951443245656456327, -20.85482241895421751 ) ) ;
#59151 = AXIS2_PLACEMENT_3D ( 'NONE', #67568, #207089, #148398 ) ;
#59152 = ORIENTED_EDGE ( 'NONE', *, *, #43926, .T. ) ;
#59153 = CARTESIAN_POINT ( 'NONE',  ( -18.54148534481894117, 10.32532329027886497, -206.5699343018359286 ) ) ;
#59154 = DIRECTION ( 'NONE',  ( -0.000000000000000000, 0.000000000000000000, 1.000000000000000000 ) ) ;
#59155 = CARTESIAN_POINT ( 'NONE',  ( 18.59999999999999432, -1.102499207903924860, -187.8171010361417643 ) ) ;
#59157 = ORIENTED_EDGE ( 'NONE', *, *, #37427, .F. ) ;
#59156 = CARTESIAN_POINT ( 'NONE',  ( -20.94999999999999574, 64.37928932189329601, -109.8915241368653284 ) ) ;
#59158 = EDGE_CURVE ( 'NONE', #232621, #12655, #100566, .T. ) ;
#59160 = ORIENTED_EDGE ( 'NONE', *, *, #91757, .T. ) ;
#59159 = CARTESIAN_POINT ( 'NONE',  ( -18.50000000000000000, 85.42129027953527043, -96.19922530549789030 ) ) ;
#59161 = CARTESIAN_POINT ( 'NONE',  ( -22.49231231312463208, 11.64998490368843953, -167.4389471123986084 ) ) ;
#59162 = DIRECTION ( 'NONE',  ( -1.000000000000000000, -8.673617379884087537E-15, 0.000000000000000000 ) ) ;
#59163 = FACE_OUTER_BOUND ( 'NONE', #136615, .T. ) ;
#59164 = ADVANCED_FACE ( 'NONE', ( #238834 ), #61482, .T. ) ;
#59165 = CARTESIAN_POINT ( 'NONE',  ( 21.05000000000000071, 69.74218538953655866, -203.6208977758331855 ) ) ;
#59167 = DIRECTION ( 'NONE',  ( 5.421010862427554711E-16, -1.000000000000000000, -3.252606517456533024E-15 ) ) ;
#59166 = CARTESIAN_POINT ( 'NONE',  ( 18.45068634130097607, 8.880467395992003077, -245.4328382399599491 ) ) ;
#59168 = DIRECTION ( 'NONE',  ( -1.000000000000000000, 0.000000000000000000, 0.000000000000000000 ) ) ;
#59169 = DIRECTION ( 'NONE',  ( -1.000000000000000000, -0.000000000000000000, -0.000000000000000000 ) ) ;
#59171 = EDGE_CURVE ( 'NONE', #146439, #61685, #125103, .T. ) ;
#59170 = CARTESIAN_POINT ( 'NONE',  ( 18.59999999999999076, 65.79142135624907439, -78.37310748452438247 ) ) ;
#59172 = DIRECTION ( 'NONE',  ( 1.000000000000000000, 0.000000000000000000, 0.000000000000000000 ) ) ;
#59173 = DIRECTION ( 'NONE',  ( -0.000000000000000000, -1.000000000000000000, -6.982962677686266711E-15 ) ) ;
#59174 = ORIENTED_EDGE ( 'NONE', *, *, #15881, .F. ) ;
#59176 = VECTOR ( 'NONE', #104176, 1000.000000000000000 ) ;
#59175 = CARTESIAN_POINT ( 'NONE',  ( 21.05000000000000071, -0.08559286335111412902, -94.08633726513041040 ) ) ;
#59177 = EDGE_LOOP ( 'NONE', ( #7544, #102784, #209342, #102625, #88682, #216914, #62985, #198009, #62850, #185487, #145004, #31981 ) ) ;
#59178 = EDGE_LOOP ( 'NONE', ( #160985, #113885, #107660, #169795 ) ) ;
#59179 = DIRECTION ( 'NONE',  ( 0.000000000000000000, -0.7899159663865552572, -0.6132151058540507016 ) ) ;
#59180 = FACE_BOUND ( 'NONE', #95813, .T. ) ;
#59181 = ORIENTED_EDGE ( 'NONE', *, *, #236971, .T. ) ;
#59182 =( REPRESENTATION_RELATIONSHIP ('NONE','NONE', #36900, #205135 ) REPRESENTATION_RELATIONSHIP_WITH_TRANSFORMATION ( #127611 )SHAPE_REPRESENTATION_RELATIONSHIP( ) );
#59183 = EDGE_CURVE ( 'NONE', #8870, #229103, #179282, .T. ) ;
#59184 = EDGE_LOOP ( 'NONE', ( #159497, #149700, #110904, #242025 ) ) ;
#59185 = ADVANCED_FACE ( 'NONE', ( #197124 ), #40676, .F. ) ;
#59186 = AXIS2_PLACEMENT_3D ( 'NONE', #43890, #123428, #243363 ) ;
#59187 = ORIENTED_EDGE ( 'NONE', *, *, #146902, .F. ) ;
#59188 = ORIENTED_EDGE ( 'NONE', *, *, #14679, .T. ) ;
#59189 = AXIS2_PLACEMENT_3D ( 'NONE', #110991, #169723, #91433 ) ;
#59190 = DIRECTION ( 'NONE',  ( 0.000000000000000000, 0.2617529984165152257, 0.9651348961777124202 ) ) ;
#59191 = FACE_OUTER_BOUND ( 'NONE', #252490, .T. ) ;
#59192 = LINE ( 'NONE', #38394, #151106 ) ;
#59193 = DIRECTION ( 'NONE',  ( 1.000000000000000000, 0.000000000000000000, 0.000000000000000000 ) ) ;
#59194 = CARTESIAN_POINT ( 'NONE',  ( 18.49999999999999645, 0.6656436123793491033, -212.6810495496487476 ) ) ;
#59195 = AXIS2_PLACEMENT_3D ( 'NONE', #51824, #131380, #197771 ) ;
#59196 =( BOUNDED_CURVE ( )  B_SPLINE_CURVE ( 3, ( #235667, #194007, #93604, #94877 ),
 .UNSPECIFIED., .F., .F. ) 
 B_SPLINE_CURVE_WITH_KNOTS ( ( 4, 4 ),
 ( 1.570796326794895448, 3.141592653589791784 ),
 .UNSPECIFIED. ) 
 CURVE ( )  GEOMETRIC_REPRESENTATION_ITEM ( )  RATIONAL_B_SPLINE_CURVE ( ( 1.000000000000000000, 0.8047378541243650485, 0.8047378541243650485, 1.000000000000000000 ) ) 
 REPRESENTATION_ITEM ( '' )  );
#59197 = CARTESIAN_POINT ( 'NONE',  ( -23.15000000000000213, 87.48912529308798014, -106.1231074845242262 ) ) ;
#59198 = CARTESIAN_POINT ( 'NONE',  ( 21.05000000000000071, 76.02138556595014052, -142.8280685972092954 ) ) ;
#59200 = VERTEX_POINT ( 'NONE', #180156 ) ;
#59199 = FACE_OUTER_BOUND ( 'NONE', #214823, .T. ) ;
#59202 = DIRECTION ( 'NONE',  ( -0.000000000000000000, 6.982962677686266711E-15, -1.000000000000000000 ) ) ;
#59201 = DIRECTION ( 'NONE',  ( 0.000000000000000000, -0.9126074666063844765, -0.4088369013363114535 ) ) ;
#59203 = DIRECTION ( 'NONE',  ( 0.000000000000000000, -1.000000000000000000, 0.000000000000000000 ) ) ;
#59204 = VERTEX_POINT ( 'NONE', #19802 ) ;
#59205 = DIRECTION ( 'NONE',  ( 0.000000000000000000, 1.000000000000000000, 0.000000000000000000 ) ) ;
#59206 = FACE_OUTER_BOUND ( 'NONE', #205100, .T. ) ;
#59207 = EDGE_LOOP ( 'NONE', ( #118183, #145339, #158865, #248056 ) ) ;
#59208 = VECTOR ( 'NONE', #226533, 1000.000000000000000 ) ;
#59211 = DIRECTION ( 'NONE',  ( 0.000000000000000000, -0.8814952561688444987, 0.4721928772777320149 ) ) ;
#59210 = VECTOR ( 'NONE', #75492, 999.9999999999998863 ) ;
#59209 = DIRECTION ( 'NONE',  ( 0.000000000000000000, 0.000000000000000000, 1.000000000000000000 ) ) ;
#59212 = CARTESIAN_POINT ( 'NONE',  ( -21.95218792049438861, 75.90097156021208491, -110.2246150457710030 ) ) ;
#59213 = CARTESIAN_POINT ( 'NONE',  ( 20.04142135623731136, 16.75134856811735062, -222.6994677643232876 ) ) ;
#59214 = VERTEX_POINT ( 'NONE', #216696 ) ;
#59215 = CARTESIAN_POINT ( 'NONE',  ( 18.49999999999999645, 67.23127455305835554, -235.8551265064784559 ) ) ;
#59216 = CARTESIAN_POINT ( 'NONE',  ( -18.37151313414604203, -0.7723694306740864768, -242.4299537170358292 ) ) ;
#59217 = SPHERICAL_SURFACE ( 'NONE', #157350, 0.1000000000000000056 ) ;
#59218 = DIRECTION ( 'NONE',  ( 0.000000000000000000, 1.000000000000000000, 0.000000000000000000 ) ) ;
#59219 = ORIENTED_EDGE ( 'NONE', *, *, #229025, .T. ) ;
#59220 = CARTESIAN_POINT ( 'NONE',  ( 21.13461538461538325, 8.885417037985616773, -179.8499999999999943 ) ) ;
#59221 = AXIS2_PLACEMENT_3D ( 'NONE', #145961, #161712, #224215 ) ;
#59222 = AXIS2_PLACEMENT_3D ( 'NONE', #104805, #163537, #4447 ) ;
#59223 = AXIS2_PLACEMENT_3D ( 'NONE', #43282, #19878, #23746 ) ;
#59224 = DIRECTION ( 'NONE',  ( -1.073024830501117725E-15, -0.000000000000000000, -1.000000000000000000 ) ) ;
#59225 = CARTESIAN_POINT ( 'NONE',  ( 20.94999999999999574, 70.10000000001163301, -59.30400771986794695 ) ) ;
#59226 = DIRECTION ( 'NONE',  ( 1.000000000000000000, -0.000000000000000000, 0.000000000000000000 ) ) ;
#59227 = CARTESIAN_POINT ( 'NONE',  ( -18.50000000000000000, 85.40000000001232650, -162.7258477248610120 ) ) ;
#59229 = ORIENTED_EDGE ( 'NONE', *, *, #22375, .T. ) ;
#59228 = DIRECTION ( 'NONE',  ( -1.000000000000000000, -9.012599976027990443E-15, -6.882867235861669241E-14 ) ) ;
#59230 = FACE_OUTER_BOUND ( 'NONE', #229083, .T. ) ;
#59231 = FACE_OUTER_BOUND ( 'NONE', #182988, .T. ) ;
#59232 = CARTESIAN_POINT ( 'NONE',  ( 20.94999999999999929, 7.128833340094563376, -233.7327013124401276 ) ) ;
#59233 = DIRECTION ( 'NONE',  ( -1.000000000000000000, 1.145314911736513911E-16, -3.106193895438251633E-17 ) ) ;
#59234 = ADVANCED_FACE ( 'NONE', ( #178898 ), #1492, .F. ) ;
#59235 = CARTESIAN_POINT ( 'NONE',  ( 20.85000000000000142, -1.835859311443637010, -45.00443916879852679 ) ) ;
#59237 = ORIENTED_EDGE ( 'NONE', *, *, #145049, .F. ) ;
#59236 = CARTESIAN_POINT ( 'NONE',  ( 21.13920837816993270, 67.21675294989165650, -57.27310748452438105 ) ) ;
#59238 = DIRECTION ( 'NONE',  ( 0.000000000000000000, 1.000000000000000000, 6.982962677686266711E-15 ) ) ;
#59239 = DIRECTION ( 'NONE',  ( 0.000000000000000000, 0.2128009952263604232, -0.9770955615653316162 ) ) ;
#59240 = FACE_BOUND ( 'NONE', #107613, .T. ) ;
#59241 = AXIS2_PLACEMENT_3D ( 'NONE', #245657, #82689, #181832 ) ;
#59242 = ORIENTED_EDGE ( 'NONE', *, *, #246609, .T. ) ;
#59243 = DIRECTION ( 'NONE',  ( 0.000000000000000000, -0.000000000000000000, -1.000000000000000000 ) ) ;
#59244 = CARTESIAN_POINT ( 'NONE',  ( 18.59999999999999076, -1.851617760457748618, -112.1031897196037050 ) ) ;
#59246 = EDGE_CURVE ( 'NONE', #42405, #130839, #208306, .T. ) ;
#59245 = CARTESIAN_POINT ( 'NONE',  ( -5.899999999999938183, 64.75000000001119815, -22.12310748452479103 ) ) ;
#59247 = EDGE_CURVE ( 'NONE', #221150, #222371, #112620, .T. ) ;
#59248 = CARTESIAN_POINT ( 'NONE',  ( 21.14999999999998082, -11.74999999998884448, -167.4999999999999432 ) ) ;
#59249 = DIRECTION ( 'NONE',  ( -0.000000000000000000, 0.2493442905258256848, 0.9684149032218436481 ) ) ;
#59250 = B_SPLINE_CURVE_WITH_KNOTS ( 'NONE', 3,
 ( #201958, #162845, #64998, #39044, #41618, #24629 ),
 .UNSPECIFIED., .F., .F.,
 ( 4, 2, 4 ),
 ( 0.000000000000000000, 0.0001895189928937444739, 0.0003790379857874889478 ),
 .UNSPECIFIED. ) ;
#59251 = TOROIDAL_SURFACE ( 'NONE', #121855, 4.149999999999999467, 0.1000000000000000056 ) ;
#59252 = CARTESIAN_POINT ( 'NONE',  ( -18.59999999999999787, 1.115600667400684642E-11, -200.9999999999999432 ) ) ;
#59253 = EDGE_LOOP ( 'NONE', ( #111021, #244834, #148512, #172121, #33862, #142947 ) ) ;
#59254 = ORIENTED_EDGE ( 'NONE', *, *, #140940, .F. ) ;
#59255 = CARTESIAN_POINT ( 'NONE',  ( -18.34374000495060386, 64.52683809664983983, -160.7731074845244450 ) ) ;
#59256 = CARTESIAN_POINT ( 'NONE',  ( -20.85000000000000142, 77.73670573947964613, -125.0056848969006182 ) ) ;
#59257 = ADVANCED_FACE ( 'NONE', ( #138416 ), #18507, .F. ) ;
#59258 = AXIS2_PLACEMENT_3D ( 'NONE', #232681, #54021, #133561 ) ;
#59259 = FACE_OUTER_BOUND ( 'NONE', #188078, .T. ) ;
#59260 = CARTESIAN_POINT ( 'NONE',  ( -20.94999999999999929, 7.031312794766356511, -104.1091509382273586 ) ) ;
#59261 = EDGE_LOOP ( 'NONE', ( #43725, #111150, #62687, #79509 ) ) ;
#59262 = CARTESIAN_POINT ( 'NONE',  ( 20.95035502843362707, 10.47763832678762164, -175.0762997087363431 ) ) ;
#59263 = VECTOR ( 'NONE', #154551, 1000.000000000000000 ) ;
#59264 = CARTESIAN_POINT ( 'NONE',  ( 20.54374330479332400, 11.90843211854532235, -206.3132545399801074 ) ) ;
#59265 = CIRCLE ( 'NONE', #155216, 4.000000000000006217 ) ;
#59266 = DIRECTION ( 'NONE',  ( -0.000000000000000000, -0.000000000000000000, 1.000000000000000000 ) ) ;
#59267 = CIRCLE ( 'NONE', #200786, 0.09999999999999939493 ) ;
#59268 = CARTESIAN_POINT ( 'NONE',  ( -16.97683809663752186, 9.949999999999983302, -20.09763598180368405 ) ) ;
#59269 = AXIS2_PLACEMENT_3D ( 'NONE', #185976, #85549, #182135 ) ;
#59270 = ORIENTED_EDGE ( 'NONE', *, *, #159405, .F. ) ;
#59271 = CARTESIAN_POINT ( 'NONE',  ( -21.05000000000000071, 1.115600667400684642E-11, -100.5000000000000426 ) ) ;
#59272 = CIRCLE ( 'NONE', #67703, 0.09999999999998898659 ) ;
#59273 = ORIENTED_EDGE ( 'NONE', *, *, #241537, .F. ) ;
#59274 = CARTESIAN_POINT ( 'NONE',  ( -21.05000000000000071, 11.75000000001115197, -93.48519422934609224 ) ) ;
#59275 = VERTEX_POINT ( 'NONE', #198418 ) ;
#59276 = EDGE_CURVE ( 'NONE', #113536, #227353, #99294, .T. ) ;
#59277 = DIRECTION ( 'NONE',  ( 1.000000000000000000, -0.000000000000000000, 0.000000000000000000 ) ) ;
#59278 = CARTESIAN_POINT ( 'NONE',  ( 21.14999999999999858, 23.34004772283015683, -229.2004250369967338 ) ) ;
#59279 = EDGE_CURVE ( 'NONE', #115133, #183380, #187458, .T. ) ;
#59280 = CARTESIAN_POINT ( 'NONE',  ( -21.05000000000000071, 7.128833340094563376, -233.7327013124401276 ) ) ;
#59281 = ORIENTED_EDGE ( 'NONE', *, *, #104438, .T. ) ;
#59282 = FACE_OUTER_BOUND ( 'NONE', #184899, .T. ) ;
#59283 = DIRECTION ( 'NONE',  ( 0.000000000000000000, 0.2128009952263604232, -0.9770955615653316162 ) ) ;
#59284 = AXIS2_PLACEMENT_3D ( 'NONE', #193939, #58247, #40021 ) ;
#59285 = ORIENTED_EDGE ( 'NONE', *, *, #141402, .F. ) ;
#59286 = CARTESIAN_POINT ( 'NONE',  ( -12.33960340485503870, 9.360749169926261715, -151.3145701406073158 ) ) ;
#59287 = AXIS2_PLACEMENT_3D ( 'NONE', #66652, #245291, #225680 ) ;
#59289 = VERTEX_POINT ( 'NONE', #137160 ) ;
#59288 = DIRECTION ( 'NONE',  ( 0.000000000000000000, -0.8700118002898356018, 0.4930308989875170078 ) ) ;
#59290 = LINE ( 'NONE', #102275, #239913 ) ;
#59291 = B_SPLINE_CURVE_WITH_KNOTS ( 'NONE', 3,
 ( #128429, #207984, #189688, #170172, #108860, #249667, #25488, #256020 ),
 .UNSPECIFIED., .F., .F.,
 ( 4, 2, 2, 4 ),
 ( 0.000000000000000000, 6.534141206311282169E-05, 0.0001306828241262256434, 0.0002613656482524638093 ),
 .UNSPECIFIED. ) ;
#59293 = ADVANCED_FACE ( 'NONE', ( #22374 ), #199729, .F. ) ;
#59292 = CARTESIAN_POINT ( 'NONE',  ( 20.85000000000000142, 0.000000000000000000, -33.50000000000000000 ) ) ;
#59294 = CIRCLE ( 'NONE', #167509, 0.1000000000000028644 ) ;
#59295 = CIRCLE ( 'NONE', #26033, 0.09999999999999939493 ) ;
#59296 = CIRCLE ( 'NONE', #221634, 12.77499999999999503 ) ;
#59297 = CIRCLE ( 'NONE', #176455, 0.2000000000000111688 ) ;
#59298 = ORIENTED_EDGE ( 'NONE', *, *, #73456, .F. ) ;
#59300 =( BOUNDED_CURVE ( )  B_SPLINE_CURVE ( 3, ( #188220, #228653, #109958, #169988 ),
 .UNSPECIFIED., .F., .F. ) 
 B_SPLINE_CURVE_WITH_KNOTS ( ( 4, 4 ),
 ( 1.570796326794901665, 3.141592653589802886 ),
 .UNSPECIFIED. ) 
 CURVE ( )  GEOMETRIC_REPRESENTATION_ITEM ( )  RATIONAL_B_SPLINE_CURVE ( ( 1.000000000000000000, 0.8047378541243639383, 0.8047378541243639383, 1.000000000000000000 ) ) 
 REPRESENTATION_ITEM ( '' )  );
#59299 = AXIS2_PLACEMENT_3D ( 'NONE', #174149, #237922, #99669 ) ;
#59301 = DIRECTION ( 'NONE',  ( 1.000000000000000000, 0.000000000000000000, 0.000000000000000000 ) ) ;
#59302 = DIRECTION ( 'NONE',  ( 1.000000000000000000, 0.000000000000000000, 0.000000000000000000 ) ) ;
#59303 = DIRECTION ( 'NONE',  ( 0.000000000000000000, 0.9126074666063660468, 0.4088369013363524762 ) ) ;
#59304 = VERTEX_POINT ( 'NONE', #160610 ) ;
#59305 = DIRECTION ( 'NONE',  ( 0.000000000000000000, 1.000000000000000000, 0.000000000000000000 ) ) ;
#59306 = CIRCLE ( 'NONE', #105098, 0.1000000000000060701 ) ;
#59307 = CARTESIAN_POINT ( 'NONE',  ( 12.48201962039795454, 48.91301996986817358, -233.7868972119375712 ) ) ;
#59308 = DIRECTION ( 'NONE',  ( -0.7070776581709311559, -0.1850949428989308032, -0.6824815363280924974 ) ) ;
#59309 = ADVANCED_FACE ( 'NONE', ( #156757 ), #236259, .F. ) ;
#59310 = ORIENTED_EDGE ( 'NONE', *, *, #191929, .T. ) ;
#59311 = ORIENTED_EDGE ( 'NONE', *, *, #36276, .T. ) ;
#59312 = AXIS2_PLACEMENT_3D ( 'NONE', #63457, #185983, #125999 ) ;
#59313 = AXIS2_PLACEMENT_3D ( 'NONE', #203356, #105496, #257177 ) ;
#59314 = CIRCLE ( 'NONE', #21959, 0.09999999999999939493 ) ;
#59315 = VERTEX_POINT ( 'NONE', #78458 ) ;
#59316 = ADVANCED_FACE ( 'NONE', ( #41939 ), #158060, .T. ) ;
#59317 = EDGE_CURVE ( 'NONE', #204714, #143764, #135857, .T. ) ;
#59318 = ORIENTED_EDGE ( 'NONE', *, *, #40186, .F. ) ;
#59319 = DIRECTION ( 'NONE',  ( -4.336808689941751890E-15, -0.8660254037844445918, -0.4999999999999897304 ) ) ;
#59320 = DIRECTION ( 'NONE',  ( 0.000000000000000000, -0.8814952561688429444, 0.4721928772777345684 ) ) ;
#59322 = EDGE_LOOP ( 'NONE', ( #159822, #181528, #186984, #240541, #153190 ) ) ;
#59321 = CARTESIAN_POINT ( 'NONE',  ( 21.05000000000000071, -8.999999999988842703, -124.1060308773475924 ) ) ;
#59323 = CARTESIAN_POINT ( 'NONE',  ( 21.14999999999999858, -0.09999999998884338825, -160.9593430482987344 ) ) ;
#59324 = LINE ( 'NONE', #138860, #244650 ) ;
#59325 = ADVANCED_FACE ( 'NONE', ( #223109 ), #144853, .F. ) ;
#59327 = EDGE_CURVE ( 'NONE', #50892, #70706, #146142, .T. ) ;
#59326 = CARTESIAN_POINT ( 'NONE',  ( -21.05000000000000071, 56.16603649944111254, -228.1013850343386764 ) ) ;
#59328 = CARTESIAN_POINT ( 'NONE',  ( 18.59999999999999432, 77.16270174994990327, -95.02310748452430289 ) ) ;
#59329 = SPHERICAL_SURFACE ( 'NONE', #100279, 0.1000000000000000056 ) ;
#59330 = CYLINDRICAL_SURFACE ( 'NONE', #72217, 1.749999999999998002 ) ;
#59332 = ORIENTED_EDGE ( 'NONE', *, *, #36342, .F. ) ;
#59331 = CARTESIAN_POINT ( 'NONE',  ( -16.94878442675510399, 66.00827089702154638, -182.6348879088865829 ) ) ;
#59334 = ORIENTED_EDGE ( 'NONE', *, *, #23010, .T. ) ;
#59333 = PLANE ( 'NONE',  #94480 ) ;
#59335 = CARTESIAN_POINT ( 'NONE',  ( -21.05000000000000071, 5.900000000011102586, -110.7190997646564483 ) ) ;
#59336 = ORIENTED_EDGE ( 'NONE', *, *, #37158, .T. ) ;
#59337 = VERTEX_POINT ( 'NONE', #242674 ) ;
#59338 = CARTESIAN_POINT ( 'NONE',  ( -21.04999999999994387, 66.15000000001120384, -5.923107484524795296 ) ) ;
#59339 = VECTOR ( 'NONE', #90623, 1000.000000000000000 ) ;
#59340 = DIRECTION ( 'NONE',  ( -0.000000000000000000, -0.000000000000000000, 1.000000000000000000 ) ) ;
#59341 = EDGE_CURVE ( 'NONE', #227337, #216161, #41716, .T. ) ;
#59342 = EDGE_CURVE ( 'NONE', #9358, #65920, #225011, .T. ) ;
#59343 = CARTESIAN_POINT ( 'NONE',  ( -21.05000000000000071, 5.849999999999949019, -10.13249722427796762 ) ) ;
#59344 = CARTESIAN_POINT ( 'NONE',  ( -18.40000000000000213, 61.62651781180419874, -212.6889521952982420 ) ) ;
#59345 = LINE ( 'NONE', #200188, #22123 ) ;
#59346 = EDGE_CURVE ( 'NONE', #4064, #224664, #127880, .T. ) ;
#59347 = LINE ( 'NONE', #61964, #128244 ) ;
#59348 = FACE_OUTER_BOUND ( 'NONE', #240364, .T. ) ;
#59350 = ORIENTED_EDGE ( 'NONE', *, *, #134950, .T. ) ;
#59349 = EDGE_CURVE ( 'NONE', #8739, #186134, #87472, .T. ) ;
#59351 = ORIENTED_EDGE ( 'NONE', *, *, #243676, .F. ) ;
#59352 = DIRECTION ( 'NONE',  ( 0.000000000000000000, 0.2128009952263603677, -0.9770955615653313941 ) ) ;
#59353 = ORIENTED_EDGE ( 'NONE', *, *, #54827, .T. ) ;
#59354 = ADVANCED_FACE ( 'NONE', ( #185284 ), #174391, .T. ) ;
#59355 = CARTESIAN_POINT ( 'NONE',  ( 21.14999999999999858, 6.650000000011155876, -45.65000000000000568 ) ) ;
#59356 = ADVANCED_FACE ( 'NONE', ( #45762 ), #114175, .F. ) ;
#59357 = DIRECTION ( 'NONE',  ( -0.000000000000000000, 6.982962677686266711E-15, -1.000000000000000000 ) ) ;
#59358 = CARTESIAN_POINT ( 'NONE',  ( 22.47007471830799474, 76.00000000001243450, -177.7438181364508694 ) ) ;
#59359 = DIRECTION ( 'NONE',  ( -1.000000000000000000, 0.000000000000000000, 0.000000000000000000 ) ) ;
#59360 = EDGE_CURVE ( 'NONE', #189932, #122006, #108346, .T. ) ;
#59361 = ORIENTED_EDGE ( 'NONE', *, *, #183289, .F. ) ;
#59362 = DIRECTION ( 'NONE',  ( 0.000000000000000000, -0.8705263436746263350, -0.4921218192363414623 ) ) ;
#59363 = VERTEX_POINT ( 'NONE', #52173 ) ;
#59364 = DIRECTION ( 'NONE',  ( 1.000000000000000000, 0.000000000000000000, -0.000000000000000000 ) ) ;
#59365 = VERTEX_POINT ( 'NONE', #69210 ) ;
#59366 = ADVANCED_FACE ( 'NONE', ( #170907 ), #195848, .T. ) ;
#59367 = DIRECTION ( 'NONE',  ( -0.000000000000000000, -6.982962677686266711E-15, 1.000000000000000000 ) ) ;
#59368 = EDGE_CURVE ( 'NONE', #148681, #195613, #33551, .T. ) ;
#59369 = CARTESIAN_POINT ( 'NONE',  ( 18.43579564894475453, 8.780520514393622022, -245.4165332813718976 ) ) ;
#59370 = DIRECTION ( 'NONE',  ( -0.000000000000000000, 0.2617529984165031243, 0.9651348961777157509 ) ) ;
#59372 = EDGE_LOOP ( 'NONE', ( #196440, #78440, #74436, #43124 ) ) ;
#59371 = ADVANCED_FACE ( 'NONE', ( #130434 ), #212589, .T. ) ;
#59374 = CARTESIAN_POINT ( 'NONE',  ( 20.04142135623730070, 64.25000000001196554, -111.8731074845243825 ) ) ;
#59373 = AXIS2_PLACEMENT_3D ( 'NONE', #198796, #218342, #121848 ) ;
#59375 = VERTEX_POINT ( 'NONE', #109578 ) ;
#59376 = DIRECTION ( 'NONE',  ( -0.000000000000000000, -0.000000000000000000, 1.000000000000000000 ) ) ;
#59377 = ORIENTED_EDGE ( 'NONE', *, *, #234440, .T. ) ;
#59378 = CIRCLE ( 'NONE', #192707, 0.09999999999999939493 ) ;
#59379 = VECTOR ( 'NONE', #99307, 1000.000000000000000 ) ;
#59380 = CARTESIAN_POINT ( 'NONE',  ( -16.81744102076749314, 66.05000000001261640, -190.8731074845244393 ) ) ;
#59381 = ORIENTED_EDGE ( 'NONE', *, *, #207472, .F. ) ;
#59382 = EDGE_CURVE ( 'NONE', #70494, #53791, #83360, .T. ) ;
#59383 = CARTESIAN_POINT ( 'NONE',  ( -20.94999999999999929, 1.115600667400684642E-11, -134.0000000000000284 ) ) ;
#59384 = CARTESIAN_POINT ( 'NONE',  ( 22.48508240969612615, 26.00811813615022317, -254.2718847878610688 ) ) ;
#59385 = CARTESIAN_POINT ( 'NONE',  ( 23.25000000000000000, 87.48912529308798014, -106.1231074845242262 ) ) ;
#59386 = CARTESIAN_POINT ( 'NONE',  ( 18.39999999999999503, 64.52683809664958403, -123.8731074845243683 ) ) ;
#59387 = LINE ( 'NONE', #214643, #60351 ) ;
#59388 = AXIS2_PLACEMENT_3D ( 'NONE', #67185, #45049, #166323 ) ;
#59389 = VERTEX_POINT ( 'NONE', #110878 ) ;
#59390 = VECTOR ( 'NONE', #143114, 1000.000000000000000 ) ;
#59391 = CARTESIAN_POINT ( 'NONE',  ( -18.59999999999999787, 85.40000000001167280, -62.64106563635157698 ) ) ;
#59392 = CARTESIAN_POINT ( 'NONE',  ( -18.34374000495060386, 40.40989152675300033, -235.2989281452919954 ) ) ;
#59393 = DIRECTION ( 'NONE',  ( 0.000000000000000000, 0.000000000000000000, -1.000000000000000000 ) ) ;
#59394 = ORIENTED_EDGE ( 'NONE', *, *, #200460, .F. ) ;
#59395 = CARTESIAN_POINT ( 'NONE',  ( 22.40000000000000568, 7.612336166715867769, -199.3421143478784359 ) ) ;
#59396 = VERTEX_POINT ( 'NONE', #189131 ) ;
#59397 = DIRECTION ( 'NONE',  ( 1.073024830501117725E-15, 6.982962677686266711E-15, -1.000000000000000000 ) ) ;
#59398 = ORIENTED_EDGE ( 'NONE', *, *, #86287, .F. ) ;
#59399 = FACE_OUTER_BOUND ( 'NONE', #24559, .T. ) ;
#59400 = LINE ( 'NONE', #138940, #18792 ) ;
#59401 = VECTOR ( 'NONE', #32796, 1000.000000000000000 ) ;
#59403 = ORIENTED_EDGE ( 'NONE', *, *, #178712, .T. ) ;
#59402 = CARTESIAN_POINT ( 'NONE',  ( -23.25000000000000000, 55.89093952297024970, -232.7795287750844579 ) ) ;
#59404 = FACE_OUTER_BOUND ( 'NONE', #82174, .T. ) ;
#59405 = ORIENTED_EDGE ( 'NONE', *, *, #221080, .F. ) ;
#59406 = CARTESIAN_POINT ( 'NONE',  ( -23.25000000000000000, 87.65000000001192859, -99.92310748452422331 ) ) ;
#59407 = AXIS2_PLACEMENT_3D ( 'NONE', #91978, #132400, #97071 ) ;
#59408 = VECTOR ( 'NONE', #246049, 1000.000000000000000 ) ;
#59409 = CARTESIAN_POINT ( 'NONE',  ( 20.94999999999999574, 70.62381305392328557, -228.5002045501660746 ) ) ;
#59410 = ORIENTED_EDGE ( 'NONE', *, *, #196574, .T. ) ;
#59411 = AXIS2_PLACEMENT_3D ( 'NONE', #111791, #110492, #46654 ) ;
#59412 = ORIENTED_EDGE ( 'NONE', *, *, #236828, .F. ) ;
#59413 = EDGE_CURVE ( 'NONE', #240172, #191070, #74355, .T. ) ;
#59414 = CARTESIAN_POINT ( 'NONE',  ( 23.24999999999999645, 71.00000000001230660, -157.6178414656113205 ) ) ;
#59415 = CARTESIAN_POINT ( 'NONE',  ( -21.05000000000000071, 11.60000000001115339, -194.0717967697244717 ) ) ;
#59416 = VERTEX_POINT ( 'NONE', #252940 ) ;
#59417 = CARTESIAN_POINT ( 'NONE',  ( 21.14999999999999858, 75.90220970870363715, -176.2809220950004772 ) ) ;
#59418 = EDGE_CURVE ( 'NONE', #79677, #145985, #21067, .T. ) ;
#59419 = VERTEX_POINT ( 'NONE', #153910 ) ;
#59420 = VERTEX_POINT ( 'NONE', #93876 ) ;
#59421 = DIRECTION ( 'NONE',  ( 1.000000000000000000, 0.000000000000000000, 0.000000000000000000 ) ) ;
#59422 = EDGE_CURVE ( 'NONE', #86183, #206239, #8388, .T. ) ;
#59423 = EDGE_CURVE ( 'NONE', #177874, #69398, #90017, .T. ) ;
#59425 = EDGE_LOOP ( 'NONE', ( #92137, #203479, #41376 ) ) ;
#59424 = DIRECTION ( 'NONE',  ( 0.000000000000000000, 1.181088324069315448E-15, 1.000000000000000000 ) ) ;
#59426 = CARTESIAN_POINT ( 'NONE',  ( 23.24999999999999645, 1.115600667400684642E-11, -67.00000000000000000 ) ) ;
#59427 = FACE_OUTER_BOUND ( 'NONE', #132002, .T. ) ;
#59428 = CARTESIAN_POINT ( 'NONE',  ( -18.50000000000000000, 1.866714910068465239, -179.2526752462819672 ) ) ;
#59430 = CARTESIAN_POINT ( 'NONE',  ( -22.49756042579671700, 75.92195366299527848, -181.6729724456266979 ) ) ;
#59429 = DIRECTION ( 'NONE',  ( -1.000000000000000000, -0.000000000000000000, -0.000000000000000000 ) ) ;
#59431 = CARTESIAN_POINT ( 'NONE',  ( -18.40000000000000213, 11.47316190337310537, -158.2001707515343014 ) ) ;
#59432 = DIRECTION ( 'NONE',  ( 0.000000000000000000, 0.000000000000000000, -1.000000000000000000 ) ) ;
#59433 = VECTOR ( 'NONE', #176454, 1000.000000000000114 ) ;
#59434 = DIRECTION ( 'NONE',  ( 1.000000000000000000, 0.000000000000000000, 0.000000000000000000 ) ) ;
#59435 = DIRECTION ( 'NONE',  ( 1.000000000000000000, 0.000000000000000000, 0.000000000000000000 ) ) ;
#59436 = EDGE_LOOP ( 'NONE', ( #21984, #220060, #79930 ) ) ;
#59438 = ORIENTED_EDGE ( 'NONE', *, *, #140611, .T. ) ;
#59437 = CARTESIAN_POINT ( 'NONE',  ( -18.50000000000000000, 43.35377423437995503, -245.1717807829448930 ) ) ;
#59439 = VERTEX_POINT ( 'NONE', #211265 ) ;
#59441 = DIRECTION ( 'NONE',  ( 0.000000000000000000, 0.000000000000000000, 1.000000000000000000 ) ) ;
#59440 = AXIS2_PLACEMENT_3D ( 'NONE', #131975, #214084, #36769 ) ;
#59442 = EDGE_LOOP ( 'NONE', ( #169777, #217705, #255809, #246185 ) ) ;
#59443 = DIRECTION ( 'NONE',  ( 1.000000000000000000, -0.000000000000000000, -0.000000000000000000 ) ) ;
#59444 = VECTOR ( 'NONE', #227003, 1000.000000000000000 ) ;
#59445 = VERTEX_POINT ( 'NONE', #151308 ) ;
#59446 = CIRCLE ( 'NONE', #42743, 0.09999999999999939493 ) ;
#59447 = AXIS2_PLACEMENT_3D ( 'NONE', #11694, #31282, #232029 ) ;
#59448 = CARTESIAN_POINT ( 'NONE',  ( 21.05000000000000071, 67.23127455305841238, -235.8551265064783991 ) ) ;
#59449 = AXIS2_PLACEMENT_3D ( 'NONE', #164056, #244856, #124929 ) ;
#59451 = VERTEX_POINT ( 'NONE', #230849 ) ;
#59450 = ORIENTED_EDGE ( 'NONE', *, *, #71140, .F. ) ;
#59452 = EDGE_CURVE ( 'NONE', #114211, #46041, #201009, .T. ) ;
#59453 = ORIENTED_EDGE ( 'NONE', *, *, #205798, .T. ) ;
#59454 = ORIENTED_EDGE ( 'NONE', *, *, #158333, .T. ) ;
#59455 = CIRCLE ( 'NONE', #5497, 0.09999999999998898659 ) ;
#59456 = FACE_OUTER_BOUND ( 'NONE', #48952, .T. ) ;
#59457 = CARTESIAN_POINT ( 'NONE',  ( -16.86379686415369150, 30.29174399807271456, -234.8241917813125781 ) ) ;
#59459 = ORIENTED_EDGE ( 'NONE', *, *, #184251, .T. ) ;
#59458 = CARTESIAN_POINT ( 'NONE',  ( 21.05000000000000071, -11.29603075032412640, -197.9521008403361009 ) ) ;
#59460 = CARTESIAN_POINT ( 'NONE',  ( -20.94999999999999929, 67.49463558145296815, -195.5618716440587548 ) ) ;
#59461 = DIRECTION ( 'NONE',  ( 0.000000000000000000, -0.9752329468386645717, -0.2211802418851520069 ) ) ;
#59463 = ORIENTED_EDGE ( 'NONE', *, *, #199789, .F. ) ;
#59462 = CARTESIAN_POINT ( 'NONE',  ( -20.94999999999999929, 61.95000000001265050, -198.0094124137634708 ) ) ;
#59464 = CARTESIAN_POINT ( 'NONE',  ( 20.00000000000000355, 11.75000000001116263, -125.1500000000000341 ) ) ;
#59465 = ORIENTED_EDGE ( 'NONE', *, *, #154566, .F. ) ;
#59466 = CARTESIAN_POINT ( 'NONE',  ( -16.87036670365548474, 10.08494996326643189, -154.9500000000000455 ) ) ;
#59467 = AXIS2_PLACEMENT_3D ( 'NONE', #5652, #205146, #81331 ) ;
#59468 = ADVANCED_FACE ( 'NONE', ( #172185 ), #60860, .F. ) ;
#59470 = VERTEX_POINT ( 'NONE', #233417 ) ;
#59469 = CARTESIAN_POINT ( 'NONE',  ( -21.12230431290520016, 6.457566653304160909, -167.4947901483108978 ) ) ;
#59471 = AXIS2_PLACEMENT_3D ( 'NONE', #24676, #65052, #67617 ) ;
#59472 = DIRECTION ( 'NONE',  ( 1.000000000000000000, 2.952720810173289112E-16, -0.000000000000000000 ) ) ;
#59473 = DIRECTION ( 'NONE',  ( 0.000000000000000000, 0.8814952561688494947, -0.4721928772777226890 ) ) ;
#59474 = EDGE_CURVE ( 'NONE', #221017, #23701, #213828, .T. ) ;
#59475 = CARTESIAN_POINT ( 'NONE',  ( 21.02374657821572868, 11.60000000083170413, -60.07179677019824027 ) ) ;
#59476 = ORIENTED_EDGE ( 'NONE', *, *, #28171, .T. ) ;
#59477 = AXIS2_PLACEMENT_3D ( 'NONE', #69725, #86668, #168854 ) ;
#59479 = DIRECTION ( 'NONE',  ( 0.000000000000000000, -0.9999176327611369874, 0.01283462868041984617 ) ) ;
#59478 = CARTESIAN_POINT ( 'NONE',  ( 18.59999999999999076, -1.249999999988843369, -41.50000000000000000 ) ) ;
#59480 = FACE_OUTER_BOUND ( 'NONE', #148368, .T. ) ;
#59481 = CARTESIAN_POINT ( 'NONE',  ( 21.30740335185486245, 6.556657922039159203, -133.9010654742241684 ) ) ;
#59482 = CARTESIAN_POINT ( 'NONE',  ( 21.05000000000000071, 1.115600667400684642E-11, -134.0000000000000000 ) ) ;
#59483 = PLANE ( 'NONE',  #159358 ) ;
#59485 = ORIENTED_EDGE ( 'NONE', *, *, #41985, .T. ) ;
#59484 = VECTOR ( 'NONE', #1370, 1000.000000000000000 ) ;
#59486 = VERTEX_POINT ( 'NONE', #36503 ) ;
#59487 = CIRCLE ( 'NONE', #238596, 0.1000000000000028644 ) ;
#59489 = ORIENTED_EDGE ( 'NONE', *, *, #234867, .T. ) ;
#59488 = CIRCLE ( 'NONE', #251044, 0.1000000000000028644 ) ;
#59490 = ADVANCED_FACE ( 'NONE', ( #57297 ), #159022, .F. ) ;
#59491 = CARTESIAN_POINT ( 'NONE',  ( -23.49999999999994316, 64.35000000001120668, -36.02310748452479316 ) ) ;
#59492 = AXIS2_PLACEMENT_3D ( 'NONE', #75958, #35574, #53823 ) ;
#59493 = VERTEX_POINT ( 'NONE', #238521 ) ;
#59494 = LINE ( 'NONE', #219884, #122606 ) ;
#59495 = ORIENTED_EDGE ( 'NONE', *, *, #238093, .T. ) ;
#59496 = DIRECTION ( 'NONE',  ( 0.000000000000000000, -0.9770955615653315052, -0.2128009952263603954 ) ) ;
#59497 = DIRECTION ( 'NONE',  ( -1.000000000000000000, -2.885090398161910739E-16, -6.283419270304611573E-17 ) ) ;
#59498 = ADVANCED_FACE ( 'NONE', ( #61171 ), #256750, .F. ) ;
#59499 = EDGE_CURVE ( 'NONE', #158664, #241281, #229141, .T. ) ;
#59500 = VERTEX_POINT ( 'NONE', #37781 ) ;
#59501 = EDGE_CURVE ( 'NONE', #35607, #155655, #258040, .T. ) ;
#59502 = DIRECTION ( 'NONE',  ( 0.2834754621636358940, 0.2834754621636501049, -0.9161240771326873977 ) ) ;
#59503 = AXIS2_PLACEMENT_3D ( 'NONE', #7787, #6482, #49472 ) ;
#59504 = CIRCLE ( 'NONE', #205269, 0.1000000000000052097 ) ;
#59505 = ORIENTED_EDGE ( 'NONE', *, *, #249325, .F. ) ;
#59507 = ORIENTED_EDGE ( 'NONE', *, *, #129134, .F. ) ;
#59506 = CIRCLE ( 'NONE', #226106, 11.70000000000000817 ) ;
#59508 = VERTEX_POINT ( 'NONE', #96426 ) ;
#59509 = CARTESIAN_POINT ( 'NONE',  ( -18.50000000000000000, 7.021664781911246322, -137.8335654018973457 ) ) ;
#59510 = CARTESIAN_POINT ( 'NONE',  ( 22.49436431346199683, 75.93309647029050780, -215.1730584321778110 ) ) ;
#59511 = CARTESIAN_POINT ( 'NONE',  ( 20.12500000000000000, 9.750000000011153745, -142.1117712821142902 ) ) ;
#59512 = CARTESIAN_POINT ( 'NONE',  ( -23.15000000000000213, 1.115600667400684642E-11, -167.4999999999999716 ) ) ;
#59513 = DIRECTION ( 'NONE',  ( -3.265361837132813093E-16, -1.000000000000000000, 7.445645354460596589E-46 ) ) ;
#59514 = EDGE_CURVE ( 'NONE', #208323, #244309, #114733, .T. ) ;
#59516 = DIRECTION ( 'NONE',  ( 1.000000000000000000, -0.000000000000000000, 0.000000000000000000 ) ) ;
#59515 = DIRECTION ( 'NONE',  ( 0.000000000000000000, 0.000000000000000000, 1.000000000000000000 ) ) ;
#59517 = DIRECTION ( 'NONE',  ( -0.000000000000000000, 0.9651348961777155289, -0.2617529984165036794 ) ) ;
#59519 = ORIENTED_EDGE ( 'NONE', *, *, #32166, .F. ) ;
#59518 = DIRECTION ( 'NONE',  ( 0.000000000000000000, -1.224646799142185182E-16, 1.000000000000000000 ) ) ;
#59520 = CARTESIAN_POINT ( 'NONE',  ( 21.14999999999999858, 64.25000000001202238, -114.7731074845243882 ) ) ;
#59521 = ORIENTED_EDGE ( 'NONE', *, *, #63267, .T. ) ;
#59522 = CARTESIAN_POINT ( 'NONE',  ( -18.46946985241255490, -9.509317228700188807, -140.9866625654999552 ) ) ;
#59523 = VERTEX_POINT ( 'NONE', #255468 ) ;
#59524 = ORIENTED_EDGE ( 'NONE', *, *, #99413, .F. ) ;
#59525 = CARTESIAN_POINT ( 'NONE',  ( -23.15000000000000213, -4.756823075239758225, -233.1486023682345490 ) ) ;
#59526 = CARTESIAN_POINT ( 'NONE',  ( -22.59999999999999787, 64.35042919246758686, -170.1231074845244393 ) ) ;
#59527 = FACE_OUTER_BOUND ( 'NONE', #227231, .T. ) ;
#59528 = EDGE_LOOP ( 'NONE', ( #191332, #45662, #50366, #139906 ) ) ;
#59529 = AXIS2_PLACEMENT_3D ( 'NONE', #142281, #62754, #22364 ) ;
#59530 = DIRECTION ( 'NONE',  ( 1.000000000000000000, 0.000000000000000000, 0.000000000000000000 ) ) ;
#59531 = ORIENTED_EDGE ( 'NONE', *, *, #33898, .F. ) ;
#59532 = ORIENTED_EDGE ( 'NONE', *, *, #250118, .F. ) ;
#59533 = VECTOR ( 'NONE', #150448, 1000.000000000000000 ) ;
#59534 = DIRECTION ( 'NONE',  ( 0.000000000000000000, 0.6728971962616697722, -0.7397360091702875895 ) ) ;
#59535 = ORIENTED_EDGE ( 'NONE', *, *, #23788, .F. ) ;
#59536 = CARTESIAN_POINT ( 'NONE',  ( 20.00894256274686001, 5.586869314946281584, 16.41686200241345261 ) ) ;
#59537 = CARTESIAN_POINT ( 'NONE',  ( 20.04142135623730070, 11.65000000001115943, -88.35000000000003695 ) ) ;
#59538 = ORIENTED_EDGE ( 'NONE', *, *, #33799, .T. ) ;
#59539 = CARTESIAN_POINT ( 'NONE',  ( -20.64999999999999858, -8.730841121484171907, -143.5980747189843783 ) ) ;
#59540 = DIRECTION ( 'NONE',  ( 1.000000000000000000, -0.000000000000000000, -0.000000000000000000 ) ) ;
#59541 = FACE_OUTER_BOUND ( 'NONE', #217271, .T. ) ;
#59542 = VERTEX_POINT ( 'NONE', #156463 ) ;
#59543 = CARTESIAN_POINT ( 'NONE',  ( -20.94999999999999929, 76.00000000001190870, -103.0231074845243029 ) ) ;
#59544 = CYLINDRICAL_SURFACE ( 'NONE', #120757, 0.09999999999998898659 ) ;
#59545 = CARTESIAN_POINT ( 'NONE',  ( -23.15000000000000213, 7.128833340094563376, -233.7327013124401276 ) ) ;
#59546 = ADVANCED_FACE ( 'NONE', ( #218953 ), #117300, .F. ) ;
#59547 = ORIENTED_EDGE ( 'NONE', *, *, #218868, .F. ) ;
#59549 = ORIENTED_EDGE ( 'NONE', *, *, #234814, .T. ) ;
#59548 = CARTESIAN_POINT ( 'NONE',  ( -23.25000000000000000, 74.00000000001254818, -183.2477294072864709 ) ) ;
#59550 = VERTEX_POINT ( 'NONE', #40368 ) ;
#59551 = CYLINDRICAL_SURFACE ( 'NONE', #164028, 11.74999999999999645 ) ;
#59552 = ADVANCED_FACE ( 'NONE', ( #234677 ), #215111, .T. ) ;
#59553 = CARTESIAN_POINT ( 'NONE',  ( 20.94999999999999574, 47.95459712139159336, -246.5019368548292675 ) ) ;
#59554 = DIRECTION ( 'NONE',  ( 0.000000000000000000, 1.000000000000000000, 0.000000000000000000 ) ) ;
#59555 = DIRECTION ( 'NONE',  ( 0.000000000000000000, 0.9126074666064812879, 0.4088369013360954596 ) ) ;
#59556 = CARTESIAN_POINT ( 'NONE',  ( 20.94999999999999574, 77.73625713160970463, -158.4544551555068495 ) ) ;
#59557 = CARTESIAN_POINT ( 'NONE',  ( -16.87383368123029825, 66.05000000001207638, -123.8731074845243683 ) ) ;
#59558 = ORIENTED_EDGE ( 'NONE', *, *, #49985, .F. ) ;
#59559 = CARTESIAN_POINT ( 'NONE',  ( -16.92973740335330390, 63.05938405906327660, -213.0623915549271601 ) ) ;
#59560 = CARTESIAN_POINT ( 'NONE',  ( -15.55912972643741199, 8.490870273573719373, -79.65000000000004832 ) ) ;
#59561 = EDGE_CURVE ( 'NONE', #128403, #170879, #204173, .T. ) ;
#59562 = EDGE_CURVE ( 'NONE', #136985, #17846, #61785, .T. ) ;
#59563 = CARTESIAN_POINT ( 'NONE',  ( -21.05000000000000071, 74.92681270650359693, -207.4801605588535551 ) ) ;
#59564 = DIRECTION ( 'NONE',  ( 1.000000000000000000, 0.000000000000000000, 0.000000000000000000 ) ) ;
#59565 = VECTOR ( 'NONE', #209081, 1000.000000000000000 ) ;
#59567 = CARTESIAN_POINT ( 'NONE',  ( 20.19326291201647194, 65.84393901210765421, -61.76124567692164646 ) ) ;
#59566 = CIRCLE ( 'NONE', #134410, 0.1000000000000028644 ) ;
#59568 = ORIENTED_EDGE ( 'NONE', *, *, #223244, .T. ) ;
#59569 = EDGE_LOOP ( 'NONE', ( #133535, #90247, #60040, #247375 ) ) ;
#59570 = FACE_OUTER_BOUND ( 'NONE', #99062, .T. ) ;
#59572 = CARTESIAN_POINT ( 'NONE',  ( 20.94999999999999929, 5.850000000011105428, -110.6324972242780120 ) ) ;
#59571 = AXIS2_PLACEMENT_3D ( 'NONE', #192043, #251986, #35546 ) ;
#59573 = CARTESIAN_POINT ( 'NONE',  ( 23.14999999999999858, 1.115600667400684642E-11, -100.5000000000000284 ) ) ;
#59574 = LINE ( 'NONE', #139110, #197268 ) ;
#59575 = CARTESIAN_POINT ( 'NONE',  ( -20.94999999999999929, 1.162701749949165642, -142.1000000000000227 ) ) ;
#59576 = EDGE_CURVE ( 'NONE', #42291, #66731, #250174, .T. ) ;
#59577 = ORIENTED_EDGE ( 'NONE', *, *, #33971, .T. ) ;
#59578 = DIRECTION ( 'NONE',  ( 1.000000000000000000, 0.000000000000000000, 0.000000000000000000 ) ) ;
#59579 = ADVANCED_FACE ( 'NONE', ( #16923 ), #237247, .T. ) ;
#59580 = ITEM_DEFINED_TRANSFORMATION ( 'NONE', 'NONE', #148554,  #2425 ) ;
#59581 = CARTESIAN_POINT ( 'NONE',  ( -18.50000000000000000, 11.65000000001115232, -74.01480577065404987 ) ) ;
#59582 = AXIS2_PLACEMENT_3D ( 'NONE', #254164, #235888, #18138 ) ;
#59583 = AXIS2_PLACEMENT_3D ( 'NONE', #163681, #140233, #25461 ) ;
#59584 = DIRECTION ( 'NONE',  ( 0.000000000000000000, 0.000000000000000000, -1.000000000000000000 ) ) ;
#59585 = PRODUCT_RELATED_PRODUCT_CATEGORY ( 'part', '', ( #249281 ) ) ;
#59586 = CIRCLE ( 'NONE', #205344, 7.900000000000003908 ) ;
#59587 = B_SPLINE_CURVE_WITH_KNOTS ( 'NONE', 3,
 ( #197312, #39574, #98185, #78644, #6829, #85046, #86331, #29005, #108496, #4243 ),
 .UNSPECIFIED., .F., .F.,
 ( 4, 2, 2, 2, 4 ),
 ( 0.000000000000000000, 0.0003916577441626799445, 0.0005874866162440102674, 0.0006854010522846840483, 0.0007833154883253576123 ),
 .UNSPECIFIED. ) ;
#59588 = DIRECTION ( 'NONE',  ( 1.000000000000000000, 3.265361837132813093E-16, -0.000000000000000000 ) ) ;
#59589 = EDGE_LOOP ( 'NONE', ( #52891, #169898, #125948, #20037 ) ) ;
#59590 = DIRECTION ( 'NONE',  ( -4.448008912761039862E-16, -0.9651348961777161950, 0.2617529984165013479 ) ) ;
#59591 = EDGE_CURVE ( 'NONE', #179449, #139023, #138120, .T. ) ;
#59592 = CIRCLE ( 'NONE', #22054, 0.09999999999998898659 ) ;
#59593 = ORIENTED_EDGE ( 'NONE', *, *, #254803, .T. ) ;
#59594 = ADVANCED_FACE ( 'NONE', ( #176011 ), #208498, .T. ) ;
#59595 = DIRECTION ( 'NONE',  ( 1.000000000000000000, 0.000000000000000000, 0.000000000000000000 ) ) ;
#59596 = EDGE_CURVE ( 'NONE', #225545, #20026, #98979, .T. ) ;
#59597 = CARTESIAN_POINT ( 'NONE',  ( 21.05000000000000071, 69.45934304831114048, -170.0231074845243882 ) ) ;
#59598 = CARTESIAN_POINT ( 'NONE',  ( 20.94999999999999929, 6.650000000011155876, -177.5170271704400022 ) ) ;
#59599 = DIRECTION ( 'NONE',  ( 0.000000000000000000, 8.881784197002011602E-16, -1.000000000000000000 ) ) ;
#59601 = AXIS2_PLACEMENT_3D ( 'NONE', #42288, #4426, #241758 ) ;
#59600 = CARTESIAN_POINT ( 'NONE',  ( 20.94999999999999574, -10.86374996222470379, -206.3339888224507206 ) ) ;
#59602 = FACE_OUTER_BOUND ( 'NONE', #160322, .T. ) ;
#59604 = CARTESIAN_POINT ( 'NONE',  ( 21.14999999999999858, 52.81534179157632991, -244.1198638051726277 ) ) ;
#59603 = AXIS2_PLACEMENT_3D ( 'NONE', #147602, #671, #41143 ) ;
#59605 = TOROIDAL_SURFACE ( 'NONE', #84539, 0.9750000000000019762, 0.1000000000000000056 ) ;
#59606 = SPHERICAL_SURFACE ( 'NONE', #72746, 0.1000000000000000056 ) ;
#59608 = LINE ( 'NONE', #153669, #87289 ) ;
#59607 = AXIS2_PLACEMENT_3D ( 'NONE', #252333, #77533, #133683 ) ;
#59609 = DIRECTION ( 'NONE',  ( -0.000000000000000000, -6.982962677686266711E-15, 1.000000000000000000 ) ) ;
#59610 = DIRECTION ( 'NONE',  ( -1.000000000000000000, -0.000000000000000000, -0.000000000000000000 ) ) ;
#59611 = SPHERICAL_SURFACE ( 'NONE', #114729, 0.1000000000000000056 ) ;
#59612 = DIRECTION ( 'NONE',  ( 1.000000000000000000, -0.000000000000000000, -0.000000000000000000 ) ) ;
#59613 = CARTESIAN_POINT ( 'NONE',  ( 20.99749315643147440, 56.02567684099302880, -227.9999002278293858 ) ) ;
#59614 = ORIENTED_EDGE ( 'NONE', *, *, #109317, .F. ) ;
#59615 = DIRECTION ( 'NONE',  ( 0.000000000000000000, 0.1686199900910312910, -0.9856811345164826488 ) ) ;
#59616 = DIRECTION ( 'NONE',  ( 0.000000000000000000, 2.891205793294679805E-16, -1.000000000000000000 ) ) ;
#59617 = CARTESIAN_POINT ( 'NONE',  ( 20.22483756094572271, 9.501904678882469923, -41.63953912871468788 ) ) ;
#59618 = ORIENTED_EDGE ( 'NONE', *, *, #162, .F. ) ;
#59619 = CARTESIAN_POINT ( 'NONE',  ( -23.25000000000000000, 67.23127455305841238, -235.8551265064783991 ) ) ;
#59620 = EDGE_CURVE ( 'NONE', #232039, #217568, #54529, .T. ) ;
#59621 = DIRECTION ( 'NONE',  ( 1.000000000000000000, -0.000000000000000000, -0.000000000000000000 ) ) ;
#59622 = AXIS2_PLACEMENT_3D ( 'NONE', #56418, #39481, #116424 ) ;
#59623 = ORIENTED_EDGE ( 'NONE', *, *, #60027, .T. ) ;
#59624 = DIRECTION ( 'NONE',  ( 0.000000000000000000, -6.530723674265620862E-15, 1.000000000000000000 ) ) ;
#59625 = DIRECTION ( 'NONE',  ( 0.000000000000000000, 0.000000000000000000, -1.000000000000000000 ) ) ;
#59626 = AXIS2_PLACEMENT_3D ( 'NONE', #128167, #9488, #168628 ) ;
#59627 = ORIENTED_EDGE ( 'NONE', *, *, #104355, .F. ) ;
#59628 = ORIENTED_EDGE ( 'NONE', *, *, #77197, .T. ) ;
#59630 = CARTESIAN_POINT ( 'NONE',  ( -23.15000000000000213, 7.128833340093095217, -233.7327013124392749 ) ) ;
#59629 = AXIS2_PLACEMENT_3D ( 'NONE', #111416, #132255, #193530 ) ;
#59631 = EDGE_CURVE ( 'NONE', #213320, #132574, #121023, .T. ) ;
#59632 = TOROIDAL_SURFACE ( 'NONE', #130583, 0.6000000000000013101, 0.1000000000000000056 ) ;
#59633 = ORIENTED_EDGE ( 'NONE', *, *, #83583, .F. ) ;
#59634 = DIRECTION ( 'NONE',  ( 1.000000000000000000, 3.276496277610882853E-15, 6.116602059353118732E-15 ) ) ;
#59635 = DIRECTION ( 'NONE',  ( 0.000000000000000000, 0.000000000000000000, -1.000000000000000000 ) ) ;
#59637 = VECTOR ( 'NONE', #234392, 1000.000000000000000 ) ;
#59636 = DIRECTION ( 'NONE',  ( 1.000000000000000000, 0.000000000000000000, 0.000000000000000000 ) ) ;
#59638 = EDGE_CURVE ( 'NONE', #216543, #201537, #16957, .T. ) ;
#59639 = CARTESIAN_POINT ( 'NONE',  ( -20.54999999999999716, 4.350000000011156054, -117.2500000000000284 ) ) ;
#59640 = CARTESIAN_POINT ( 'NONE',  ( 22.50000000000000000, 76.00000000001195133, -103.0231074845243171 ) ) ;
#59641 = CIRCLE ( 'NONE', #51273, 11.75000000000001066 ) ;
#59642 = CARTESIAN_POINT ( 'NONE',  ( -20.94999999999994245, 67.65000000001118963, -3.123107484524795474 ) ) ;
#59644 = CARTESIAN_POINT ( 'NONE',  ( -16.87036670365548474, 66.01058118071016168, -82.04354736722233099 ) ) ;
#59643 = AXIS2_PLACEMENT_3D ( 'NONE', #213093, #37061, #55271 ) ;
#59645 = ADVANCED_FACE ( 'NONE', ( #63735 ), #242368, .T. ) ;
#59646 = VECTOR ( 'NONE', #147030, 1000.000000000000000 ) ;
#59648 = ORIENTED_EDGE ( 'NONE', *, *, #246900, .F. ) ;
#59647 = CARTESIAN_POINT ( 'NONE',  ( -18.48550754432022103, -9.463399778548794217, -40.54878975241538797 ) ) ;
#59649 = EDGE_LOOP ( 'NONE', ( #89685, #42363, #155791, #5141, #119840 ) ) ;
#59651 = CARTESIAN_POINT ( 'NONE',  ( 23.14999999999999503, 14.10000000000000142, -27.89970238886063925 ) ) ;
#59650 = CARTESIAN_POINT ( 'NONE',  ( 22.45380639572288928, 1.426688889968629469E-07, 11.75043289110677591 ) ) ;
#59652 = AXIS2_PLACEMENT_3D ( 'NONE', #35783, #57867, #257315 ) ;
#59655 = ORIENTED_EDGE ( 'NONE', *, *, #121343, .T. ) ;
#59654 = CARTESIAN_POINT ( 'NONE',  ( 21.08750232978087524, 10.72486338602132250, -146.2288581729995940 ) ) ;
#59653 = CYLINDRICAL_SURFACE ( 'NONE', #248519, 0.09999999999999939493 ) ;
#59656 = ORIENTED_EDGE ( 'NONE', *, *, #67871, .F. ) ;
#59657 = CARTESIAN_POINT ( 'NONE',  ( -21.05000000000000071, 61.95000000001265050, -198.0094124137634708 ) ) ;
#59658 = DIRECTION ( 'NONE',  ( 0.000000000000000000, 0.2128009952263775484, -0.9770955615653277304 ) ) ;
#59659 = VECTOR ( 'NONE', #3256, 1000.000000000000000 ) ;
#59660 = EDGE_CURVE ( 'NONE', #145413, #250736, #122439, .T. ) ;
#59661 = EDGE_CURVE ( 'NONE', #64710, #152450, #167007, .T. ) ;
#59662 = CARTESIAN_POINT ( 'NONE',  ( 18.69999999999999574, -8.262584272387851314, 10.47734830970188824 ) ) ;
#59663 = CARTESIAN_POINT ( 'NONE',  ( -23.15000000000000213, 1.115600667400684642E-11, -113.3750000000000284 ) ) ;
#59664 = CARTESIAN_POINT ( 'NONE',  ( 18.59999999999999432, -1.135018845899022466, -175.2169768834323520 ) ) ;
#59665 = CARTESIAN_POINT ( 'NONE',  ( -20.54999999999999716, -9.399999999988848387, -143.8939691226524644 ) ) ;
#59666 = DIRECTION ( 'NONE',  ( 0.000000000000000000, 0.000000000000000000, 1.000000000000000000 ) ) ;
#59667 = CIRCLE ( 'NONE', #159663, 4.299999999999970512 ) ;
#59668 = CARTESIAN_POINT ( 'NONE',  ( -21.14999999999999858, 11.75000000001115552, -73.78386566297820082 ) ) ;
#59669 = AXIS2_PLACEMENT_3D ( 'NONE', #44398, #207327, #165631 ) ;
#59670 = ORIENTED_EDGE ( 'NONE', *, *, #150001, .T. ) ;
#59671 = EDGE_LOOP ( 'NONE', ( #87670, #237479, #233538, #236491 ) ) ;
#59672 = LINE ( 'NONE', #45273, #189680 ) ;
#59673 = EDGE_CURVE ( 'NONE', #191682, #233644, #221508, .T. ) ;
#59674 = ORIENTED_EDGE ( 'NONE', *, *, #28244, .F. ) ;
#59675 = DIRECTION ( 'NONE',  ( 0.000000000000000000, 0.9667078373770114919, 0.2558827019434133931 ) ) ;
#59677 = EDGE_CURVE ( 'NONE', #156346, #204844, #46157, .T. ) ;
#59676 = ORIENTED_EDGE ( 'NONE', *, *, #247500, .F. ) ;
#59679 = AXIS2_PLACEMENT_3D ( 'NONE', #160186, #239700, #101411 ) ;
#59678 = CARTESIAN_POINT ( 'NONE',  ( -22.50000000000000000, 64.35023708198022518, -136.6119174609113145 ) ) ;
#59680 = AXIS2_PLACEMENT_3D ( 'NONE', #153664, #228341, #147512 ) ;
#59681 = VECTOR ( 'NONE', #240614, 1000.000000000000000 ) ;
#59682 = AXIS2_PLACEMENT_3D ( 'NONE', #163203, #238883, #240174 ) ;
#59683 = DIRECTION ( 'NONE',  ( -1.000000000000000000, 0.000000000000000000, 0.000000000000000000 ) ) ;
#59684 = FACE_OUTER_BOUND ( 'NONE', #17411, .T. ) ;
#59685 = EDGE_CURVE ( 'NONE', #86120, #77802, #44193, .T. ) ;
#59686 = DIRECTION ( 'NONE',  ( 0.000000000000000000, -6.982962677686266711E-15, 1.000000000000000000 ) ) ;
#59687 = FACE_OUTER_BOUND ( 'NONE', #147662, .T. ) ;
#59688 = ORIENTED_EDGE ( 'NONE', *, *, #112149, .T. ) ;
#59689 = DIRECTION ( 'NONE',  ( 0.000000000000000000, -0.1350103645451945777, 0.9908441862701591329 ) ) ;
#59690 = CYLINDRICAL_SURFACE ( 'NONE', #79976, 0.09999999999998898659 ) ;
#59691 = DIRECTION ( 'NONE',  ( -1.000000000000000000, -0.000000000000000000, -0.000000000000000000 ) ) ;
#59692 = ADVANCED_FACE ( 'NONE', ( #101546 ), #186268, .F. ) ;
#59693 = DIRECTION ( 'NONE',  ( 1.000000000000000000, 7.304098846218134667E-16, -0.000000000000000000 ) ) ;
#59694 = DIRECTION ( 'NONE',  ( 0.000000000000000000, 0.000000000000000000, -1.000000000000000000 ) ) ;
#59696 = ORIENTED_EDGE ( 'NONE', *, *, #211255, .T. ) ;
#59695 = ADVANCED_FACE ( 'NONE', ( #165419 ), #37814, .T. ) ;
#59697 = DIRECTION ( 'NONE',  ( -1.000000000000000000, 0.000000000000000000, 0.000000000000000000 ) ) ;
#59698 = CIRCLE ( 'NONE', #84622, 0.09999999999998898659 ) ;
#59699 = VERTEX_POINT ( 'NONE', #244940 ) ;
#59702 = EDGE_LOOP ( 'NONE', ( #157992, #135144, #142034, #220456 ) ) ;
#59701 = DIRECTION ( 'NONE',  ( 4.239556034732056743E-17, 0.9579639084728132081, 0.2868887416116073785 ) ) ;
#59700 = CARTESIAN_POINT ( 'NONE',  ( 21.05000000000000071, 5.400000000011154988, -179.9052660189130677 ) ) ;
#59703 = CIRCLE ( 'NONE', #30713, 0.09999999999998898659 ) ;
#59704 = AXIS2_PLACEMENT_3D ( 'NONE', #240939, #62293, #141819 ) ;
#59705 = DIRECTION ( 'NONE',  ( 1.000000000000000000, -3.151514657663852580E-16, 8.547182517843351137E-17 ) ) ;
#59706 = AXIS2_PLACEMENT_3D ( 'NONE', #197679, #157313, #19050 ) ;
#59707 = DIRECTION ( 'NONE',  ( 0.000000000000000000, 0.4721928772777346239, 0.8814952561688430555 ) ) ;
#59708 = VERTEX_POINT ( 'NONE', #166727 ) ;
#59709 = CARTESIAN_POINT ( 'NONE',  ( 18.31325810956293410, 85.53638847601938267, -129.6546672782193923 ) ) ;
#59710 = DIRECTION ( 'NONE',  ( -1.000000000000000000, 0.000000000000000000, 4.336808689942017736E-16 ) ) ;
#59711 = EDGE_CURVE ( 'NONE', #112125, #117495, #25340, .T. ) ;
#59712 = CARTESIAN_POINT ( 'NONE',  ( 20.94999999999999929, 76.00000000001139711, -32.02310748452432421 ) ) ;
#59713 = UNCERTAINTY_MEASURE_WITH_UNIT (LENGTH_MEASURE( 1.000000000000000082E-05 ), #192260, 'distance_accuracy_value', 'NONE');
#59714 = EDGE_CURVE ( 'NONE', #236598, #238413, #246235, .T. ) ;
#59716 = VERTEX_POINT ( 'NONE', #224084 ) ;
#59715 = CYLINDRICAL_SURFACE ( 'NONE', #35288, 0.1000000000000028644 ) ;
#59717 = DIRECTION ( 'NONE',  ( 1.000000000000000000, 0.000000000000000000, 0.000000000000000000 ) ) ;
#59718 = VERTEX_POINT ( 'NONE', #67591 ) ;
#59719 = DIRECTION ( 'NONE',  ( -0.000000000000000000, 0.2617529984165031243, 0.9651348961777157509 ) ) ;
#59720 = LINE ( 'NONE', #243512, #50464 ) ;
#59721 = EDGE_LOOP ( 'NONE', ( #187197, #135837, #78354, #66955 ) ) ;
#59722 = ORIENTED_EDGE ( 'NONE', *, *, #88836, .T. ) ;
#59723 = DIRECTION ( 'NONE',  ( -1.000000000000000000, 0.000000000000000000, 0.000000000000000000 ) ) ;
#59724 = CIRCLE ( 'NONE', #176481, 0.1000000000000028644 ) ;
#59725 = DIRECTION ( 'NONE',  ( 0.000000000000000000, 1.000000000000000000, 0.000000000000000000 ) ) ;
#59726 = CARTESIAN_POINT ( 'NONE',  ( -23.25000000000000000, 2.600000000011156054, -87.27537807723794572 ) ) ;
#59727 = ORIENTED_EDGE ( 'NONE', *, *, #83209, .T. ) ;
#59728 = CARTESIAN_POINT ( 'NONE',  ( -21.44999999999999929, 68.65000000001180069, -81.87310748452436826 ) ) ;
#59729 = CARTESIAN_POINT ( 'NONE',  ( -18.69999999999999929, 7.973296578895943121, -1.410778198689825791 ) ) ;
#59730 = CARTESIAN_POINT ( 'NONE',  ( -20.99551997958407412, 64.25000000001251976, -176.8714483468355922 ) ) ;
#59731 = ORIENTED_EDGE ( 'NONE', *, *, #242689, .F. ) ;
#59732 = DIRECTION ( 'NONE',  ( 1.000000000000000000, 0.000000000000000000, 0.000000000000000000 ) ) ;
#59733 = DIRECTION ( 'NONE',  ( 1.000000000000000000, 1.875376730785737719E-16, 0.000000000000000000 ) ) ;
#59735 = DIRECTION ( 'NONE',  ( 0.000000000000000000, -0.2617529984165031243, -0.9651348961777157509 ) ) ;
#59734 = CIRCLE ( 'NONE', #222236, 0.1000000000000028644 ) ;
#59736 = EDGE_CURVE ( 'NONE', #77760, #164498, #171109, .T. ) ;
#59737 = AXIS2_PLACEMENT_3D ( 'NONE', #37866, #97782, #176097 ) ;
#59738 = ORIENTED_EDGE ( 'NONE', *, *, #200247, .T. ) ;
#59739 = AXIS2_PLACEMENT_3D ( 'NONE', #251952, #77163, #152892 ) ;
#59740 = FACE_OUTER_BOUND ( 'NONE', #236715, .T. ) ;
#59741 = ORIENTED_EDGE ( 'NONE', *, *, #64092, .T. ) ;
#59743 = VERTEX_POINT ( 'NONE', #204524 ) ;
#59742 = CARTESIAN_POINT ( 'NONE',  ( -21.00857864376268935, 11.60000000001115161, -107.4282032302755852 ) ) ;
#59746 = ORIENTED_EDGE ( 'NONE', *, *, #232609, .T. ) ;
#59745 = EDGE_LOOP ( 'NONE', ( #100890, #203058, #238108, #98433 ) ) ;
#59744 = CARTESIAN_POINT ( 'NONE',  ( -21.09813707148783735, 0.03135149952943332152, 6.385062105736676763 ) ) ;
#59747 = DIRECTION ( 'NONE',  ( -0.000000000000000000, 0.2617529984165031243, 0.9651348961777157509 ) ) ;
#59748 = CARTESIAN_POINT ( 'NONE',  ( -21.11101077989000530, 0.01528526892543718291, -161.0763152652738484 ) ) ;
#59749 = CARTESIAN_POINT ( 'NONE',  ( 21.14999999999999503, 87.75000000001162448, -66.62310748452424036 ) ) ;
#59750 = CARTESIAN_POINT ( 'NONE',  ( -16.97683810757273193, 12.54460316225921446, -211.8424120337253385 ) ) ;
#59752 = EDGE_CURVE ( 'NONE', #4179, #153430, #23365, .T. ) ;
#59751 = CARTESIAN_POINT ( 'NONE',  ( -23.15000000000000213, 2.600000000011156054, -80.22462192276213955 ) ) ;
#59753 = CARTESIAN_POINT ( 'NONE',  ( -18.40000000000000213, 8.822561741677553471, -124.7500000000000284 ) ) ;
#59754 = AXIS2_PLACEMENT_3D ( 'NONE', #256222, #172955, #115495 ) ;
#59755 = CARTESIAN_POINT ( 'NONE',  ( -15.55912972643741199, 67.50912972644972854, -157.3731074845244109 ) ) ;
#59757 = CARTESIAN_POINT ( 'NONE',  ( -21.05000000000000071, 87.75000000001216449, -139.5231074845243029 ) ) ;
#59756 = DIRECTION ( 'NONE',  ( 0.000000000000000000, -0.9999991631930157387, 0.001293682058423061953 ) ) ;
#59758 = TOROIDAL_SURFACE ( 'NONE', #84698, 11.70000000000000639, 0.1000000000000000056 ) ;
#59759 = ORIENTED_EDGE ( 'NONE', *, *, #149560, .T. ) ;
#59760 = ORIENTED_EDGE ( 'NONE', *, *, #67121, .T. ) ;
#59761 = CIRCLE ( 'NONE', #113767, 0.1000000000000001860 ) ;
#59762 = CARTESIAN_POINT ( 'NONE',  ( 18.59999999999999432, 77.16270174995034381, -161.9231074845243370 ) ) ;
#59764 = ORIENTED_EDGE ( 'NONE', *, *, #31496, .T. ) ;
#59763 = CARTESIAN_POINT ( 'NONE',  ( -16.27683809663751191, 66.65000000001232650, -157.4731074845244336 ) ) ;
#59765 = CARTESIAN_POINT ( 'NONE',  ( 21.05000000000000071, 1.162701749949165642, -41.40000000000000568 ) ) ;
#59766 = ORIENTED_EDGE ( 'NONE', *, *, #234889, .T. ) ;
#59767 = CARTESIAN_POINT ( 'NONE',  ( -20.94999999999999929, 1.750000000011155743, -112.1695115579016857 ) ) ;
#59768 = ORIENTED_EDGE ( 'NONE', *, *, #243897, .F. ) ;
#59769 = DIRECTION ( 'NONE',  ( 1.000000000000000000, 0.000000000000000000, 0.000000000000000000 ) ) ;
#59770 = VECTOR ( 'NONE', #114365, 1000.000000000000000 ) ;
#59771 = AXIS2_PLACEMENT_3D ( 'NONE', #203778, #79945, #25171 ) ;
#59772 = ORIENTED_EDGE ( 'NONE', *, *, #161069, .T. ) ;
#59773 = CIRCLE ( 'NONE', #88820, 0.09999999999999939493 ) ;
#59774 = CARTESIAN_POINT ( 'NONE',  ( -16.94275863006528482, 66.01050395134429039, -82.13141010244780205 ) ) ;
#59775 = DIRECTION ( 'NONE',  ( -0.7071067811865474617, -0.3338907855510734324, -0.6233112732207618523 ) ) ;
#59777 = ORIENTED_EDGE ( 'NONE', *, *, #151325, .F. ) ;
#59776 = ORIENTED_EDGE ( 'NONE', *, *, #117730, .T. ) ;
#59778 = ORIENTED_EDGE ( 'NONE', *, *, #217551, .T. ) ;
#59779 = FACE_OUTER_BOUND ( 'NONE', #11838, .T. ) ;
#59780 = ORIENTED_EDGE ( 'NONE', *, *, #60614, .F. ) ;
#59781 = VERTEX_POINT ( 'NONE', #121185 ) ;
#59783 = DIRECTION ( 'NONE',  ( -1.000000000000000000, 0.000000000000000000, 0.000000000000000000 ) ) ;
#59782 = CIRCLE ( 'NONE', #126452, 0.5000000000000004441 ) ;
#59785 = VERTEX_POINT ( 'NONE', #200691 ) ;
#59784 = CARTESIAN_POINT ( 'NONE',  ( 21.00000000000000000, 9.749999999999998224, -12.35000000000000320 ) ) ;
#59787 = CARTESIAN_POINT ( 'NONE',  ( 20.95462737510932882, 65.44321804836857837, -162.4531574279621395 ) ) ;
#59786 = DIRECTION ( 'NONE',  ( 0.000000000000000000, 6.982962677686266711E-15, -1.000000000000000000 ) ) ;
#59788 = CARTESIAN_POINT ( 'NONE',  ( 23.14999999999999503, 64.35000000001218723, -143.4379132551783869 ) ) ;
#59789 = CARTESIAN_POINT ( 'NONE',  ( 23.25000000000000000, 87.65000000001214175, -136.5231074845242176 ) ) ;
#59790 = CARTESIAN_POINT ( 'NONE',  ( -23.15000000000000213, 1.115600667400684642E-11, -134.0000000000000000 ) ) ;
#59791 = ORIENTED_EDGE ( 'NONE', *, *, #146774, .T. ) ;
#59792 = AXIS2_PLACEMENT_3D ( 'NONE', #36580, #13137, #54803 ) ;
#59793 = CIRCLE ( 'NONE', #97180, 11.80000000000000426 ) ;
#59794 = AXIS2_PLACEMENT_3D ( 'NONE', #64782, #140463, #220012 ) ;
#59795 = ORIENTED_EDGE ( 'NONE', *, *, #33126, .F. ) ;
#59796 = CARTESIAN_POINT ( 'NONE',  ( -13.39999999999994529, 67.75000000001118394, -16.98168612828748181 ) ) ;
#59797 = CARTESIAN_POINT ( 'NONE',  ( 20.94999999999999574, -11.41227409413852989, -103.4000000000000341 ) ) ;
#59798 = CARTESIAN_POINT ( 'NONE',  ( -23.39999999999994529, 87.50449464844290048, -37.85861909827351468 ) ) ;
#59799 = ADVANCED_FACE ( 'NONE', ( #2467 ), #3766, .F. ) ;
#59800 = ORIENTED_EDGE ( 'NONE', *, *, #130400, .F. ) ;
#59801 = DIRECTION ( 'NONE',  ( -1.073024830501117725E-15, -6.982962677686266711E-15, 1.000000000000000000 ) ) ;
#59802 = CARTESIAN_POINT ( 'NONE',  ( -18.50000000000000000, 7.675662554762638479, -241.7139905447625381 ) ) ;
#59803 = CARTESIAN_POINT ( 'NONE',  ( -14.45443560709636266, 12.43810346549959611, -213.7002393734605903 ) ) ;
#59804 = ORIENTED_EDGE ( 'NONE', *, *, #205652, .F. ) ;
#59805 = ORIENTED_EDGE ( 'NONE', *, *, #36691, .T. ) ;
#59806 = EDGE_CURVE ( 'NONE', #244339, #53312, #62737, .T. ) ;
#59807 = DIRECTION ( 'NONE',  ( -0.000000000000000000, 0.9525900758537790836, -0.3042567129660269099 ) ) ;
#59808 = DIRECTION ( 'NONE',  ( 0.000000000000000000, 0.8855159391400395652, -0.4646089985449416981 ) ) ;
#59809 = ORIENTED_EDGE ( 'NONE', *, *, #97986, .F. ) ;
#59810 = CARTESIAN_POINT ( 'NONE',  ( 22.39999999999999503, 7.790779598384535376, -167.3999999999999773 ) ) ;
#59811 = ORIENTED_EDGE ( 'NONE', *, *, #49242, .F. ) ;
#59812 = CARTESIAN_POINT ( 'NONE',  ( 23.15000000000000213, -8.999999999988842703, -124.6060308773475924 ) ) ;
#59813 = CARTESIAN_POINT ( 'NONE',  ( -14.00000000000000178, 62.10905854918435409, -217.1108499610990918 ) ) ;
#59815 = CARTESIAN_POINT ( 'NONE',  ( -20.85000000000000142, 68.11287320386161070, -224.1382462126928488 ) ) ;
#59814 = DIRECTION ( 'NONE',  ( -0.000000000000000000, -0.000000000000000000, 1.000000000000000000 ) ) ;
#59816 = ADVANCED_FACE ( 'NONE', ( #71468 ), #108513, .F. ) ;
#59817 = DIRECTION ( 'NONE',  ( 2.827886303505249259E-16, 0.8660254037844377084, 0.5000000000000016653 ) ) ;
#59818 = CARTESIAN_POINT ( 'NONE',  ( 20.94999999999999929, 6.550000000011156231, -77.01702717044007329 ) ) ;
#59819 = TOROIDAL_SURFACE ( 'NONE', #205565, 11.65000000000000036, 0.1000000000000000056 ) ;
#59820 = AXIS2_PLACEMENT_3D ( 'NONE', #202265, #96703, #198 ) ;
#59821 = ORIENTED_EDGE ( 'NONE', *, *, #236787, .F. ) ;
#59822 = EDGE_CURVE ( 'NONE', #71927, #75205, #75222, .T. ) ;
#59823 = CARTESIAN_POINT ( 'NONE',  ( -23.15000000000000213, -8.596261682231835621, -76.45012751715033517 ) ) ;
#59824 = AXIS2_PLACEMENT_3D ( 'NONE', #148518, #186366, #66409 ) ;
#59826 = ORIENTED_EDGE ( 'NONE', *, *, #73547, .F. ) ;
#59825 = EDGE_LOOP ( 'NONE', ( #231626, #212806, #73133, #76166 ) ) ;
#59827 = VERTEX_POINT ( 'NONE', #89707 ) ;
#59828 = VECTOR ( 'NONE', #13218, 1000.000000000000000 ) ;
#59829 = DIRECTION ( 'NONE',  ( 1.000000000000000000, -3.469446951953718318E-14, 2.003086131649645455E-14 ) ) ;
#59830 = FACE_OUTER_BOUND ( 'NONE', #1441, .T. ) ;
#59831 = CIRCLE ( 'NONE', #118111, 0.09999999999998898659 ) ;
#59832 = DIRECTION ( 'NONE',  ( -1.000000000000000000, -8.720091142841976186E-15, -1.400634033999624291E-14 ) ) ;
#59833 = ADVANCED_FACE ( 'NONE', ( #191426 ), #50570, .T. ) ;
#59835 = CARTESIAN_POINT ( 'NONE',  ( -15.39946565075090312, 66.61046543766514105, -87.34829818013443514 ) ) ;
#59834 = CARTESIAN_POINT ( 'NONE',  ( 20.77766267348356166, 10.44904239061880702, -7.592708915877627973 ) ) ;
#59836 = ORIENTED_EDGE ( 'NONE', *, *, #219137, .F. ) ;
#59837 = DIRECTION ( 'NONE',  ( 0.000000000000000000, 0.000000000000000000, -1.000000000000000000 ) ) ;
#59838 = EDGE_LOOP ( 'NONE', ( #231248, #100282, #237191, #161304 ) ) ;
#59839 = CARTESIAN_POINT ( 'NONE',  ( 22.37643362114956247, 33.45079766894996709, -242.6323179357828792 ) ) ;
#59840 = ORIENTED_EDGE ( 'NONE', *, *, #217935, .T. ) ;
#59841 = ORIENTED_EDGE ( 'NONE', *, *, #31508, .F. ) ;
#59842 = DIRECTION ( 'NONE',  ( -0.000000000000000000, -6.982962677686266711E-15, 1.000000000000000000 ) ) ;
#59843 = AXIS2_PLACEMENT_3D ( 'NONE', #88938, #87656, #244162 ) ;
#59844 = CARTESIAN_POINT ( 'NONE',  ( -18.59999999999999787, 1.162701749949165642, -175.5999999999999659 ) ) ;
#59845 = CARTESIAN_POINT ( 'NONE',  ( -16.97683809663752186, 66.05000000001153637, -49.42547150272071121 ) ) ;
#59846 = VECTOR ( 'NONE', #159075, 1000.000000000000000 ) ;
#59847 = CARTESIAN_POINT ( 'NONE',  ( 18.50000000000000000, 85.50000000001209344, -129.4910380878245633 ) ) ;
#59848 = VECTOR ( 'NONE', #221368, 999.9999999999998863 ) ;
#59849 = CARTESIAN_POINT ( 'NONE',  ( 20.94999999999999574, 74.83729825007388570, -94.92310748452432279 ) ) ;
#59850 = ORIENTED_EDGE ( 'NONE', *, *, #84987, .T. ) ;
#59851 = EDGE_LOOP ( 'NONE', ( #100862, #150255, #148370, #157454 ) ) ;
#59852 = CARTESIAN_POINT ( 'NONE',  ( -20.95613430942416144, 11.75000000001115907, -40.35716264822026744 ) ) ;
#59853 = CARTESIAN_POINT ( 'NONE',  ( 23.24999999999999645, 62.02748777246247869, -221.3368380802343722 ) ) ;
#59854 = ORIENTED_EDGE ( 'NONE', *, *, #144943, .T. ) ;
#59855 = FACE_OUTER_BOUND ( 'NONE', #255300, .T. ) ;
#59856 = DIRECTION ( 'NONE',  ( 0.000000000000000000, 0.000000000000000000, -1.000000000000000000 ) ) ;
#59858 = AXIS2_PLACEMENT_3D ( 'NONE', #53499, #157784, #176038 ) ;
#59857 = FACE_OUTER_BOUND ( 'NONE', #47623, .T. ) ;
#59859 = CARTESIAN_POINT ( 'NONE',  ( -22.42357213249529480, 75.90091303601063544, -144.1960398708842206 ) ) ;
#59860 = DIRECTION ( 'NONE',  ( -1.000000000000000000, 0.000000000000000000, -0.000000000000000000 ) ) ;
#59861 = DIRECTION ( 'NONE',  ( 0.000000000000000000, 0.5341055959867045955, -0.8454177738465681324 ) ) ;
#59863 = DIRECTION ( 'NONE',  ( 0.000000000000000000, 0.000000000000000000, -1.000000000000000000 ) ) ;
#59862 = FACE_OUTER_BOUND ( 'NONE', #5893, .T. ) ;
#59864 = DIRECTION ( 'NONE',  ( 1.000000000000000000, 0.000000000000000000, 0.000000000000000000 ) ) ;
#59865 = CARTESIAN_POINT ( 'NONE',  ( -21.14999999999999858, 6.390846877240203838, -199.6081416912452653 ) ) ;
#59866 = CIRCLE ( 'NONE', #151494, 0.09999999999998898659 ) ;
#59867 = DIRECTION ( 'NONE',  ( -1.000000000000000000, 0.000000000000000000, 0.000000000000000000 ) ) ;
#59868 = CARTESIAN_POINT ( 'NONE',  ( 20.85000000000000142, 76.00000000001126921, -203.5231074845248997 ) ) ;
#59869 = AXIS2_PLACEMENT_3D ( 'NONE', #235519, #133861, #114298 ) ;
#59870 = AXIS2_PLACEMENT_3D ( 'NONE', #151511, #228471, #88923 ) ;
#59871 = ADVANCED_FACE ( 'NONE', ( #12778 ), #200104, .T. ) ;
#59872 = VERTEX_POINT ( 'NONE', #169304 ) ;
#59873 = AXIS2_PLACEMENT_3D ( 'NONE', #107721, #4744, #187285 ) ;
#59874 = CARTESIAN_POINT ( 'NONE',  ( 20.95539060131842746, 10.62386215766680131, -41.15373381365618854 ) ) ;
#59875 = VERTEX_POINT ( 'NONE', #187566 ) ;
#59876 = EDGE_CURVE ( 'NONE', #84708, #14612, #175207, .T. ) ;
#59877 = CYLINDRICAL_SURFACE ( 'NONE', #133279, 0.09999999999998898659 ) ;
#59878 = CARTESIAN_POINT ( 'NONE',  ( -18.37160782347004329, 11.47561641481354044, -109.7500000000000426 ) ) ;
#59879 =( LENGTH_UNIT ( ) NAMED_UNIT ( * ) SI_UNIT ( .MILLI., .METRE. ) );
#59880 = ORIENTED_EDGE ( 'NONE', *, *, #211407, .T. ) ;
#59881 = DIRECTION ( 'NONE',  ( 0.000000000000000000, -1.000000000000000000, -6.352154140967427193E-15 ) ) ;
#59882 = ADVANCED_FACE ( 'NONE', ( #130124 ), #31073, .F. ) ;
#59883 = CYLINDRICAL_SURFACE ( 'NONE', #177220, 0.09999999999999939493 ) ;
#59884 = CARTESIAN_POINT ( 'NONE',  ( 22.45301702632625762, 0.01521087972134078925, -21.85020777573961226 ) ) ;
#59885 = AXIS2_PLACEMENT_3D ( 'NONE', #191923, #34139, #113636 ) ;
#59886 = AXIS2_PLACEMENT_3D ( 'NONE', #228742, #187053, #108770 ) ;
#59887 = VECTOR ( 'NONE', #228774, 1000.000000000000000 ) ;
#59889 = DIRECTION ( 'NONE',  ( 7.304098846218132695E-16, -0.9770955615653315052, -0.2128009952263603954 ) ) ;
#59888 = AXIS2_PLACEMENT_3D ( 'NONE', #93142, #172740, #210538 ) ;
#59890 = CARTESIAN_POINT ( 'NONE',  ( -20.90000000000000213, 1.885425182446133885, -11.49641995933507843 ) ) ;
#59891 = CARTESIAN_POINT ( 'NONE',  ( 21.05000000000000071, 74.83729825007462466, -195.4231074845243654 ) ) ;
#59892 = ORIENTED_EDGE ( 'NONE', *, *, #15905, .T. ) ;
#59893 = CARTESIAN_POINT ( 'NONE',  ( 23.24999999999999645, 76.00000000001267608, -203.5231074845243597 ) ) ;
#59895 = ORIENTED_EDGE ( 'NONE', *, *, #217400, .F. ) ;
#59894 = CARTESIAN_POINT ( 'NONE',  ( -20.64999999999999858, -8.999999999988846255, -109.8939691226524786 ) ) ;
#59896 = CARTESIAN_POINT ( 'NONE',  ( -20.85000000000000142, 64.35000000001220144, -143.3069731475025321 ) ) ;
#59897 = EDGE_CURVE ( 'NONE', #252148, #97927, #96025, .T. ) ;
#59898 = CARTESIAN_POINT ( 'NONE',  ( -16.77683809663752257, 9.945835743215303282, -188.3360509808957488 ) ) ;
#59899 = DIRECTION ( 'NONE',  ( 0.000000000000000000, 0.1350103645451945777, -0.9908441862701589109 ) ) ;
#59900 = ORIENTED_EDGE ( 'NONE', *, *, #51968, .F. ) ;
#59901 = DIRECTION ( 'NONE',  ( 1.000000000000000000, 0.000000000000000000, 0.000000000000000000 ) ) ;
#59902 = ADVANCED_FACE ( 'NONE', ( #70189 ), #152290, .F. ) ;
#59903 = APPLICATION_PROTOCOL_DEFINITION ( 'draft international standard', 'automotive_design', 1998, #140721 ) ;
#59904 = ADVANCED_FACE ( 'NONE', ( #127570 ), #148426, .T. ) ;
#59905 = CARTESIAN_POINT ( 'NONE',  ( 22.50046968638675793, -2.456286045658393036, -189.5094708429525099 ) ) ;
#59906 = ORIENTED_EDGE ( 'NONE', *, *, #118891, .T. ) ;
#59907 = CYLINDRICAL_SURFACE ( 'NONE', #100411, 0.09999999999999939493 ) ;
#59908 = CARTESIAN_POINT ( 'NONE',  ( 15.39170923737819763, 9.389529397477893724, -185.3171079128936753 ) ) ;
#59909 = EDGE_CURVE ( 'NONE', #119976, #21421, #239140, .T. ) ;
#59910 = VECTOR ( 'NONE', #192797, 1000.000000000000000 ) ;
#59911 = DIRECTION ( 'NONE',  ( -1.000000000000000000, -9.012599976027990443E-15, -6.882867235861669241E-14 ) ) ;
#59912 = EDGE_LOOP ( 'NONE', ( #111998, #56203, #125994, #106609 ) ) ;
#59913 = ORIENTED_EDGE ( 'NONE', *, *, #179288, .F. ) ;
#59914 = EDGE_CURVE ( 'NONE', #145230, #170111, #67008, .T. ) ;
#59915 = FACE_OUTER_BOUND ( 'NONE', #62613, .T. ) ;
#59916 = EDGE_CURVE ( 'NONE', #8334, #163587, #183538, .T. ) ;
#59917 = DIRECTION ( 'NONE',  ( -6.938893903907222067E-15, 1.000000000000000000, 2.891205793294679805E-16 ) ) ;
#59918 = CARTESIAN_POINT ( 'NONE',  ( -22.94999999999999929, 0.000000000000000000, 0.000000000000000000 ) ) ;
#59919 = LINE ( 'NONE', #161638, #15380 ) ;
#59920 = DIRECTION ( 'NONE',  ( -1.836970198721029934E-16, 1.000000000000000000, 0.000000000000000000 ) ) ;
#59921 = CARTESIAN_POINT ( 'NONE',  ( 21.14999999999999858, 64.35000000001267040, -203.4231074845244507 ) ) ;
#59923 = CARTESIAN_POINT ( 'NONE',  ( -20.85000000000000142, 76.00000000001126921, -203.5231074845248997 ) ) ;
#59922 = CARTESIAN_POINT ( 'NONE',  ( -23.15000000000000213, 5.950000000000007283, -23.19429769496518645 ) ) ;
#59924 = CARTESIAN_POINT ( 'NONE',  ( -14.00000000000000178, 9.850000000011133849, -150.7500000000000284 ) ) ;
#59925 = CARTESIAN_POINT ( 'NONE',  ( -18.59999999999999787, 2.272311100394797556, -217.9150152700588876 ) ) ;
#59926 = CARTESIAN_POINT ( 'NONE',  ( 18.58222699835054570, 65.66799936921481162, -30.42993998886010232 ) ) ;
#59928 = CARTESIAN_POINT ( 'NONE',  ( -23.25000000000000000, 76.00000000001165290, -69.52310748452431710 ) ) ;
#59927 = AXIS2_PLACEMENT_3D ( 'NONE', #250553, #92759, #190608 ) ;
#59929 = EDGE_LOOP ( 'NONE', ( #57202, #99509, #53667, #3982 ) ) ;
#59930 = AXIS2_PLACEMENT_3D ( 'NONE', #87219, #247595, #190204 ) ;
#59931 = ORIENTED_EDGE ( 'NONE', *, *, #41565, .T. ) ;
#59932 = DIRECTION ( 'NONE',  ( 0.7070776581708965169, -0.6453375049857822399, -0.2891032514073239579 ) ) ;
#59935 = DIRECTION ( 'NONE',  ( 0.000000000000000000, -1.000000000000000000, 0.000000000000000000 ) ) ;
#59934 = CARTESIAN_POINT ( 'NONE',  ( 21.13498764882293557, 69.50438185653779044, -69.52476387925570123 ) ) ;
#59933 = AXIS2_PLACEMENT_3D ( 'NONE', #241396, #84835, #220542 ) ;
#59936 = EDGE_CURVE ( 'NONE', #120136, #237128, #150231, .T. ) ;
#59937 = CARTESIAN_POINT ( 'NONE',  ( -1.820710678118658388, 63.21415835242177650, -248.5348766565488461 ) ) ;
#59939 = EDGE_CURVE ( 'NONE', #14789, #38227, #133635, .T. ) ;
#59938 = CARTESIAN_POINT ( 'NONE',  ( -23.15000000000000213, -0.8831241301779060304, -196.9450534195053706 ) ) ;
#59940 = CARTESIAN_POINT ( 'NONE',  ( -23.15000000000000213, 2.000000000011154189, -53.77537807723790309 ) ) ;
#59941 = ORIENTED_EDGE ( 'NONE', *, *, #42695, .T. ) ;
#59942 = FACE_OUTER_BOUND ( 'NONE', #252779, .T. ) ;
#59943 = ORIENTED_EDGE ( 'NONE', *, *, #57268, .F. ) ;
#59944 = EDGE_CURVE ( 'NONE', #196305, #257282, #87653, .T. ) ;
#59946 = AXIS2_PLACEMENT_3D ( 'NONE', #61923, #164879, #102289 ) ;
#59945 = CARTESIAN_POINT ( 'NONE',  ( 21.05000000000000071, 67.22371710471982453, -157.8731074845244109 ) ) ;
#59947 = EDGE_LOOP ( 'NONE', ( #89236, #140196, #161879 ) ) ;
#59948 = CYLINDRICAL_SURFACE ( 'NONE', #155662, 0.1000000000000028644 ) ;
#59949 = VECTOR ( 'NONE', #212710, 1000.000000000000000 ) ;
#59951 = CARTESIAN_POINT ( 'NONE',  ( -21.64999999999999858, 22.69475173317577443, -231.4639605648239353 ) ) ;
#59950 = AXIS2_PLACEMENT_3D ( 'NONE', #136661, #98793, #197921 ) ;
#59952 = AXIS2_PLACEMENT_3D ( 'NONE', #139273, #3624, #200554 ) ;
#59953 = ORIENTED_EDGE ( 'NONE', *, *, #189260, .F. ) ;
#59954 = DIRECTION ( 'NONE',  ( 1.000000000000000000, -7.304098846218134667E-16, 0.000000000000000000 ) ) ;
#59955 = ORIENTED_EDGE ( 'NONE', *, *, #169932, .T. ) ;
#59956 = DIRECTION ( 'NONE',  ( 0.000000000000000000, 0.000000000000000000, 1.000000000000000000 ) ) ;
#59957 = DIRECTION ( 'NONE',  ( 0.000000000000000000, -0.4088369013363281068, 0.9126074666063770380 ) ) ;
#59958 = CARTESIAN_POINT ( 'NONE',  ( -23.25000000000000000, 76.00000000001216449, -140.5731074845242858 ) ) ;
#59959 = VECTOR ( 'NONE', #105018, 1000.000000000000000 ) ;
#59960 = EDGE_CURVE ( 'NONE', #2966, #200313, #5854, .T. ) ;
#59961 = DIRECTION ( 'NONE',  ( 0.000000000000000000, 0.000000000000000000, 1.000000000000000000 ) ) ;
#59962 = SPHERICAL_SURFACE ( 'NONE', #143023, 0.1000000000000000056 ) ;
#59964 = LINE ( 'NONE', #238629, #125099 ) ;
#59963 = DIRECTION ( 'NONE',  ( 0.000000000000000000, 6.505213034913742890E-15, -1.000000000000000000 ) ) ;
#59965 = DIRECTION ( 'NONE',  ( 1.000000000000000000, 0.000000000000000000, 0.000000000000000000 ) ) ;
#59966 = ADVANCED_FACE ( 'NONE', ( #201496 ), #145376, .T. ) ;
#59968 = ORIENTED_EDGE ( 'NONE', *, *, #161801, .F. ) ;
#59967 = CARTESIAN_POINT ( 'NONE',  ( 20.44999100639871514, 65.56028929680029194, -128.7640317585553476 ) ) ;
#59970 = LINE ( 'NONE', #120002, #184926 ) ;
#59969 = CARTESIAN_POINT ( 'NONE',  ( -18.43707690579160641, 37.95493834378067532, -261.2294694241335833 ) ) ;
#59971 = CIRCLE ( 'NONE', #143378, 0.09999999999999939493 ) ;
#59972 = EDGE_LOOP ( 'NONE', ( #50804, #191607, #60375 ) ) ;
#59974 = ORIENTED_EDGE ( 'NONE', *, *, #75148, .T. ) ;
#59973 = DIRECTION ( 'NONE',  ( -1.000000000000000000, 0.000000000000000000, 0.000000000000000000 ) ) ;
#59975 = ORIENTED_EDGE ( 'NONE', *, *, #120735, .F. ) ;
#59976 = CARTESIAN_POINT ( 'NONE',  ( 23.24999999999999645, 70.35000000001230092, -157.3731074845244109 ) ) ;
#59977 = DIRECTION ( 'NONE',  ( 0.000000000000000000, -0.000000000000000000, -1.000000000000000000 ) ) ;
#59978 = DIRECTION ( 'NONE',  ( 1.000000000000000000, 0.000000000000000000, 0.000000000000000000 ) ) ;
#59979 = ADVANCED_FACE ( 'NONE', ( #163671 ), #250356, .T. ) ;
#59980 = TOROIDAL_SURFACE ( 'NONE', #122361, 0.2000000000000000111, 0.1000000000000000056 ) ;
#59981 = EDGE_LOOP ( 'NONE', ( #109369, #184219, #167108, #107421 ) ) ;
#59982 = EDGE_CURVE ( 'NONE', #108203, #48993, #58786, .T. ) ;
#59983 = DIRECTION ( 'NONE',  ( 0.000000000000000000, 0.000000000000000000, -1.000000000000000000 ) ) ;
#59984 = DIRECTION ( 'NONE',  ( 0.000000000000000000, 0.1332476588733589318, 0.9910827722268049644 ) ) ;
#59985 = DIRECTION ( 'NONE',  ( -1.836970198721030427E-16, -0.4088369013363281623, 0.9126074666063771490 ) ) ;
#59986 = VECTOR ( 'NONE', #37630, 1000.000000000000000 ) ;
#59987 = EDGE_CURVE ( 'NONE', #237761, #40973, #47545, .T. ) ;
#59988 = CARTESIAN_POINT ( 'NONE',  ( 18.59999999999999432, 79.11538813396778380, -196.3722783875038544 ) ) ;
#59989 = CIRCLE ( 'NONE', #239078, 0.1000000000000046685 ) ;
#59990 = DIRECTION ( 'NONE',  ( 0.000000000000000000, 0.000000000000000000, -1.000000000000000000 ) ) ;
#59991 = AXIS2_PLACEMENT_3D ( 'NONE', #187296, #88141, #230249 ) ;
#59992 = LINE ( 'NONE', #253065, #168577 ) ;
#59993 = EDGE_LOOP ( 'NONE', ( #137477, #54404, #149338 ) ) ;
#59994 = VERTEX_POINT ( 'NONE', #144079 ) ;
#59995 = DIRECTION ( 'NONE',  ( -0.000000000000000000, -0.2617529984165031243, -0.9651348961777157509 ) ) ;
#59996 = B_SPLINE_CURVE_WITH_KNOTS ( 'NONE', 3,
 ( #135389, #97526, #237078, #255297, #233254, #174596 ),
 .UNSPECIFIED., .F., .F.,
 ( 4, 2, 4 ),
 ( 0.000000000000000000, 0.0001891491689349579291, 0.0003782983378699158582 ),
 .UNSPECIFIED. ) ;
#59997 = EDGE_CURVE ( 'NONE', #158566, #62919, #205335, .T. ) ;
#59998 = ORIENTED_EDGE ( 'NONE', *, *, #137352, .T. ) ;
#59999 = DIRECTION ( 'NONE',  ( 2.952720810173289112E-16, -0.9770955615653318382, -0.2128009952263588411 ) ) ;
#60001 = EDGE_CURVE ( 'NONE', #117118, #149981, #26746, .T. ) ;
#60000 = ORIENTED_EDGE ( 'NONE', *, *, #118488, .F. ) ;
#60002 = DIRECTION ( 'NONE',  ( -1.000000000000000000, 0.000000000000000000, -0.000000000000000000 ) ) ;
#60003 = DIRECTION ( 'NONE',  ( 0.000000000000000000, -0.8660254037844383745, 0.5000000000000003331 ) ) ;
#60004 = FACE_OUTER_BOUND ( 'NONE', #138295, .T. ) ;
#60005 = EDGE_CURVE ( 'NONE', #68838, #180003, #150423, .T. ) ;
#60006 = DIRECTION ( 'NONE',  ( 0.000000000000000000, -1.000000000000000000, 0.000000000000000000 ) ) ;
#60007 = CIRCLE ( 'NONE', #130939, 0.1000000000000028644 ) ;
#60008 = AXIS2_PLACEMENT_3D ( 'NONE', #215862, #244431, #162353 ) ;
#60009 = SPHERICAL_SURFACE ( 'NONE', #108676, 0.1000000000000000056 ) ;
#60010 = DIRECTION ( 'NONE',  ( -1.000000000000000000, -1.646408749285562691E-14, 1.073024830501117725E-15 ) ) ;
#60011 = DIRECTION ( 'NONE',  ( 0.000000000000000000, 0.000000000000000000, -1.000000000000000000 ) ) ;
#60012 = CIRCLE ( 'NONE', #247469, 7.900000000000013678 ) ;
#60014 = VERTEX_POINT ( 'NONE', #227477 ) ;
#60013 = ADVANCED_FACE ( 'NONE', ( #187105 ), #46268, .T. ) ;
#60017 = ADVANCED_FACE ( 'NONE', ( #183235 ), #200464, .F. ) ;
#60016 = DIRECTION ( 'NONE',  ( -1.000000000000000000, 0.000000000000000000, -0.000000000000000000 ) ) ;
#60015 = DIRECTION ( 'NONE',  ( -3.265361837132813093E-16, 1.000000000000000000, 0.000000000000000000 ) ) ;
#60018 = EDGE_LOOP ( 'NONE', ( #93564, #76226, #118653, #159220 ) ) ;
#60021 = ORIENTED_EDGE ( 'NONE', *, *, #11882, .T. ) ;
#60020 = DIRECTION ( 'NONE',  ( -0.000000000000000000, 1.000000000000000000, -0.000000000000000000 ) ) ;
#60019 = FACE_OUTER_BOUND ( 'NONE', #130857, .T. ) ;
#60022 = ORIENTED_EDGE ( 'NONE', *, *, #6358, .F. ) ;
#60023 = DIRECTION ( 'NONE',  ( 1.000000000000000000, -0.000000000000000000, 0.000000000000000000 ) ) ;
#60024 = DIRECTION ( 'NONE',  ( 0.000000000000000000, 6.938893903907222067E-15, -1.000000000000000000 ) ) ;
#60025 = CIRCLE ( 'NONE', #84944, 0.1999999999999987899 ) ;
#60026 = DIRECTION ( 'NONE',  ( -0.000000000000000000, 0.9118278131605244141, -0.4105728183244670704 ) ) ;
#60027 = EDGE_CURVE ( 'NONE', #63287, #157258, #28039, .T. ) ;
#60028 = CARTESIAN_POINT ( 'NONE',  ( -18.59999999999999787, 77.83585931145546510, -91.51866831572576189 ) ) ;
#60029 = CIRCLE ( 'NONE', #76604, 0.1000000000000002554 ) ;
#60030 = ORIENTED_EDGE ( 'NONE', *, *, #80591, .F. ) ;
#60031 = DIRECTION ( 'NONE',  ( 0.000000000000000000, 0.000000000000000000, -1.000000000000000000 ) ) ;
#60033 = DIRECTION ( 'NONE',  ( 1.000000000000000000, 0.000000000000000000, -0.000000000000000000 ) ) ;
#60032 =( BOUNDED_SURFACE ( )  B_SPLINE_SURFACE ( 3, 2, ( 
 ( #95154, #53462, #176000 ),
 ( #233407, #170895, #57287 ),
 ( #230837, #52159, #216375 ),
 ( #192982, #136838, #32658 ) ),
 .UNSPECIFIED., .F., .F., .F. ) 
 B_SPLINE_SURFACE_WITH_KNOTS ( ( 4, 4 ),
 ( 3, 3 ),
 ( -1.897353801849632760E-19, 0.0003124336600439506836 ),
 ( 0.000000000000000000, 1.000000000000000000 ),
 .UNSPECIFIED. ) 
 GEOMETRIC_REPRESENTATION_ITEM ( )  RATIONAL_B_SPLINE_SURFACE ( (
 ( 1.000000000000000000, 0.7071067811865475727, 1.000000000000000000),
 ( 1.000000000000000000, 0.7089187706049675519, 1.000000000000000000),
 ( 1.000000000000000000, 0.7039288185052250402, 1.000000000000000000),
 ( 1.000000000000000000, 0.7040654476015688612, 1.000000000000000000) ) ) 
 REPRESENTATION_ITEM ( '' )  SURFACE ( )  );
#60034 = EDGE_CURVE ( 'NONE', #107334, #98586, #67188, .T. ) ;
#60035 = CIRCLE ( 'NONE', #147345, 0.6000000000000008660 ) ;
#60037 = DIRECTION ( 'NONE',  ( 0.000000000000000000, 0.000000000000000000, -1.000000000000000000 ) ) ;
#60036 = CARTESIAN_POINT ( 'NONE',  ( 20.09999999999999787, 66.25000000001227818, -149.1731074845244223 ) ) ;
#60038 = EDGE_CURVE ( 'NONE', #182906, #187157, #106235, .T. ) ;
#60040 = ORIENTED_EDGE ( 'NONE', *, *, #255069, .F. ) ;
#60039 = DIRECTION ( 'NONE',  ( 0.000000000000000000, 0.000000000000000000, 1.000000000000000000 ) ) ;
#60041 = AXIS2_PLACEMENT_3D ( 'NONE', #62540, #202049, #20872 ) ;
#60042 = CIRCLE ( 'NONE', #80699, 0.1999999999999987899 ) ;
#60043 = AXIS2_PLACEMENT_3D ( 'NONE', #209612, #90941, #190051 ) ;
#60044 = PRODUCT_DEFINITION_SHAPE ( 'NONE', 'NONE',  #258129 ) ;
#60045 = ORIENTED_EDGE ( 'NONE', *, *, #153479, .F. ) ;
#60046 = AXIS2_PLACEMENT_3D ( 'NONE', #150838, #73905, #90858 ) ;
#60047 = DIRECTION ( 'NONE',  ( 0.000000000000000000, -1.000000000000000000, -6.860497997771531562E-15 ) ) ;
#60048 = ORIENTED_EDGE ( 'NONE', *, *, #81559, .T. ) ;
#60049 = CARTESIAN_POINT ( 'NONE',  ( 20.73486653747088582, 21.70314669089255943, -233.3151006027784717 ) ) ;
#60050 = ORIENTED_EDGE ( 'NONE', *, *, #193888, .F. ) ;
#60051 =( BOUNDED_CURVE ( )  B_SPLINE_CURVE ( 3, ( #33571, #193892, #73967, #115626 ),
 .UNSPECIFIED., .F., .F. ) 
 B_SPLINE_CURVE_WITH_KNOTS ( ( 4, 4 ),
 ( 5.731445031868798168, 5.983100554402348337 ),
 .UNSPECIFIED. ) 
 CURVE ( )  GEOMETRIC_REPRESENTATION_ITEM ( )  RATIONAL_B_SPLINE_CURVE ( ( 1.000000000000000000, 0.9947294176030464508, 0.9947294176030464508, 1.000000000000000000 ) ) 
 REPRESENTATION_ITEM ( '' )  );
#60052 = DIRECTION ( 'NONE',  ( 0.000000000000000000, 0.4088369013363281068, -0.9126074666063770380 ) ) ;
#60054 = ADVANCED_FACE ( 'NONE', ( #167545 ), #22897, .F. ) ;
#60053 = FACE_OUTER_BOUND ( 'NONE', #833, .T. ) ;
#60055 = DIRECTION ( 'NONE',  ( 1.000000000000000000, 0.000000000000000000, 0.000000000000000000 ) ) ;
#60056 = AXIS2_PLACEMENT_3D ( 'NONE', #147147, #93264, #125037 ) ;
#60057 = VERTEX_POINT ( 'NONE', #151053 ) ;
#60058 = DIRECTION ( 'NONE',  ( 1.000000000000000000, 0.000000000000000000, 0.000000000000000000 ) ) ;
#60059 = EDGE_CURVE ( 'NONE', #44660, #249154, #233612, .T. ) ;
#60060 = CIRCLE ( 'NONE', #18375, 0.1000000000000055705 ) ;
#60061 = CARTESIAN_POINT ( 'NONE',  ( -16.83794479845801106, 9.926357419362650703, -54.19644470422232274 ) ) ;
#60062 = VECTOR ( 'NONE', #7872, 1000.000000000000114 ) ;
#60063 =( BOUNDED_SURFACE ( )  B_SPLINE_SURFACE ( 3, 2, ( 
 ( #79693, #158013, #138377 ),
 ( #103106, #182686, #217913 ),
 ( #58836, #4023, #83531 ),
 ( #237514, #38046, #163123 ),
 ( #22337, #39329, #238795 ),
 ( #118858, #1448, #101811 ),
 ( #198374, #99257, #178852 ),
 ( #240081, #160, #200944 ),
 ( #60133, #220520, #139660 ),
 ( #219212, #40632, #120166 ) ),
 .UNSPECIFIED., .F., .F., .F. ) 
 B_SPLINE_SURFACE_WITH_KNOTS ( ( 4, 2, 2, 2, 4 ),
 ( 3, 3 ),
 ( 0.002161241639767248670, 0.002579950749615824400, 0.002789305304540112482, 0.002893982582002256523, 0.002998659859464400564 ),
 ( 0.000000000000000000, 1.000000000000000000 ),
 .UNSPECIFIED. ) 
 GEOMETRIC_REPRESENTATION_ITEM ( )  RATIONAL_B_SPLINE_SURFACE ( (
 ( 1.000000000000000000, 0.7071067811865536790, 1.000000000000000000),
 ( 1.000000000000000000, 0.7632447400664197357, 1.000000000000000000),
 ( 1.000000000000000000, 0.8158073005110335618, 1.000000000000000000),
 ( 1.000000000000000000, 0.8906973462395710861, 1.000000000000000000),
 ( 1.000000000000000000, 0.9149408947800710123, 1.000000000000000000),
 ( 1.000000000000000000, 0.9493368785275515531, 1.000000000000000000),
 ( 1.000000000000000000, 0.9605194247156906284, 1.000000000000000000),
 ( 1.000000000000000000, 0.9803630264781052484, 1.000000000000000000),
 ( 1.000000000000000000, 0.9900844824271277655, 1.000000000000000000),
 ( 1.000000000000000000, 0.9894588281429246290, 1.000000000000000000) ) ) 
 REPRESENTATION_ITEM ( '' )  SURFACE ( )  );
#60064 = CIRCLE ( 'NONE', #43341, 0.09999999999998898659 ) ;
#60065 = VERTEX_POINT ( 'NONE', #211020 ) ;
#60066 = AXIS2_PLACEMENT_3D ( 'NONE', #99388, #215505, #16055 ) ;
#60067 = EDGE_LOOP ( 'NONE', ( #240823, #180610, #74578, #210304 ) ) ;
#60068 = ORIENTED_EDGE ( 'NONE', *, *, #85021, .F. ) ;
#60069 = CARTESIAN_POINT ( 'NONE',  ( -20.94999999999999929, -11.41227409413852811, -131.1000000000000227 ) ) ;
#60070 = EDGE_CURVE ( 'NONE', #27375, #242008, #71309, .T. ) ;
#60071 = ORIENTED_EDGE ( 'NONE', *, *, #41774, .T. ) ;
#60073 = ORIENTED_EDGE ( 'NONE', *, *, #54655, .F. ) ;
#60072 = CARTESIAN_POINT ( 'NONE',  ( 15.73863059295127442, 66.64859682587091072, -186.5435770476858579 ) ) ;
#60074 = ORIENTED_EDGE ( 'NONE', *, *, #54994, .F. ) ;
#60077 = ORIENTED_EDGE ( 'NONE', *, *, #135403, .F. ) ;
#60076 = ORIENTED_EDGE ( 'NONE', *, *, #227461, .F. ) ;
#60075 = CARTESIAN_POINT ( 'NONE',  ( -20.94999999999999929, 74.83729825007360148, -61.42310748452432989 ) ) ;
#60078 = ORIENTED_EDGE ( 'NONE', *, *, #143009, .F. ) ;
#60079 = CARTESIAN_POINT ( 'NONE',  ( -23.15000000000000213, -8.999999999988844479, -90.60603087734760663 ) ) ;
#60080 = ADVANCED_FACE ( 'NONE', ( #251425 ), #229305, .T. ) ;
#60081 = VECTOR ( 'NONE', #8191, 1000.000000000000000 ) ;
#60082 = FACE_OUTER_BOUND ( 'NONE', #99176, .T. ) ;
#60083 = DIRECTION ( 'NONE',  ( -1.000000000000000000, 0.000000000000000000, 0.000000000000000000 ) ) ;
#60084 = VERTEX_POINT ( 'NONE', #11547 ) ;
#60085 = LINE ( 'NONE', #199637, #103892 ) ;
#60087 = ORIENTED_EDGE ( 'NONE', *, *, #226944, .F. ) ;
#60086 = SPHERICAL_SURFACE ( 'NONE', #132696, 0.1000000000000000056 ) ;
#60088 = PLANE ( 'NONE',  #163193 ) ;
#60090 = ORIENTED_EDGE ( 'NONE', *, *, #204308, .T. ) ;
#60089 = CARTESIAN_POINT ( 'NONE',  ( 18.59999999999999432, 43.57568952063339651, -245.1784935019914826 ) ) ;
#60091 = ORIENTED_EDGE ( 'NONE', *, *, #139438, .F. ) ;
#60092 = DIRECTION ( 'NONE',  ( 0.000000000000000000, 2.891205793294679805E-16, -1.000000000000000000 ) ) ;
#60093 = SURFACE_STYLE_FILL_AREA ( #155394 ) ;
#60094 = ORIENTED_EDGE ( 'NONE', *, *, #243010, .T. ) ;
#60095 = EDGE_LOOP ( 'NONE', ( #24856, #41401, #97332, #236826 ) ) ;
#60096 = CARTESIAN_POINT ( 'NONE',  ( -16.94445028196808778, 9.992063609708889516, -180.1073301784184366 ) ) ;
#60097 = CARTESIAN_POINT ( 'NONE',  ( -18.50000000000000000, 45.93315328338058379, -256.6017782078560003 ) ) ;
#60099 = VERTEX_POINT ( 'NONE', #108071 ) ;
#60098 = ORIENTED_EDGE ( 'NONE', *, *, #230450, .F. ) ;
#60100 = CIRCLE ( 'NONE', #55995, 0.2000000000000003997 ) ;
#60101 = ORIENTED_EDGE ( 'NONE', *, *, #206330, .F. ) ;
#60102 = CARTESIAN_POINT ( 'NONE',  ( 21.13736287352038445, 8.046642376395153562, -54.35000000000000142 ) ) ;
#60103 = ORIENTED_EDGE ( 'NONE', *, *, #79951, .F. ) ;
#60104 = ORIENTED_EDGE ( 'NONE', *, *, #5748, .T. ) ;
#60105 = DIRECTION ( 'NONE',  ( 1.000000000000000000, 0.000000000000000000, 0.000000000000000000 ) ) ;
#60106 = ORIENTED_EDGE ( 'NONE', *, *, #101715, .T. ) ;
#60107 = CARTESIAN_POINT ( 'NONE',  ( -16.93583594267724379, 12.45203240582405257, -211.1418800172411636 ) ) ;
#60109 = CARTESIAN_POINT ( 'NONE',  ( -20.94999999999999929, 1.750000000011155743, -78.66951155790169992 ) ) ;
#60108 = CARTESIAN_POINT ( 'NONE',  ( 21.00000000000000000, 0.000000000000000000, 0.000000000000000000 ) ) ;
#60110 = VERTEX_POINT ( 'NONE', #250145 ) ;
#60111 = ADVANCED_FACE ( 'NONE', ( #32413 ), #196179, .T. ) ;
#60113 = VERTEX_POINT ( 'NONE', #111935 ) ;
#60112 = ORIENTED_EDGE ( 'NONE', *, *, #105378, .F. ) ;
#60114 = DIRECTION ( 'NONE',  ( 0.000000000000000000, 0.9908441862701596881, 0.1350103645451904977 ) ) ;
#60115 = DIRECTION ( 'NONE',  ( 0.000000000000000000, 0.2128009952263485993, -0.9770955615653341697 ) ) ;
#60116 = CIRCLE ( 'NONE', #39312, 0.6000000000000015321 ) ;
#60117 = ORIENTED_EDGE ( 'NONE', *, *, #40547, .T. ) ;
#60118 = AXIS2_PLACEMENT_3D ( 'NONE', #249853, #7380, #25675 ) ;
#60119 = AXIS2_PLACEMENT_3D ( 'NONE', #50549, #169284, #84517 ) ;
#60120 = AXIS2_PLACEMENT_3D ( 'NONE', #227893, #104067, #222740 ) ;
#60121 = DIRECTION ( 'NONE',  ( -1.000000000000000000, -0.000000000000000000, -0.000000000000000000 ) ) ;
#60122 = ORIENTED_EDGE ( 'NONE', *, *, #190156, .T. ) ;
#60123 = VERTEX_POINT ( 'NONE', #10258 ) ;
#60124 = EDGE_CURVE ( 'NONE', #137732, #67859, #191485, .T. ) ;
#60125 = CARTESIAN_POINT ( 'NONE',  ( 20.27550659511088682, 11.69688800608038193, -211.3990755776034405 ) ) ;
#60126 = ORIENTED_EDGE ( 'NONE', *, *, #27347, .T. ) ;
#60127 = DIRECTION ( 'NONE',  ( -1.000000000000000000, 9.312479980434134033E-16, 4.171876297610248080E-16 ) ) ;
#60128 = DIRECTION ( 'NONE',  ( 0.000000000000000000, -0.8814952561688430555, 0.4721928772777346239 ) ) ;
#60129 = ORIENTED_EDGE ( 'NONE', *, *, #70209, .T. ) ;
#60130 = CARTESIAN_POINT ( 'NONE',  ( -21.59142135623730852, 68.15000000001187175, -90.77310748452437394 ) ) ;
#60131 = CARTESIAN_POINT ( 'NONE',  ( -16.91256925476570672, 9.985731158139333985, -46.03235751099471429 ) ) ;
#60133 = CARTESIAN_POINT ( 'NONE',  ( -16.79270642812318570, 9.946244216949072126, -121.3389332785620525 ) ) ;
#60132 = DIRECTION ( 'NONE',  ( 1.000000000000000000, 0.000000000000000000, 0.000000000000000000 ) ) ;
#60134 = EDGE_CURVE ( 'NONE', #78889, #107983, #175362, .T. ) ;
#60135 = FACE_OUTER_BOUND ( 'NONE', #146545, .T. ) ;
#60136 = DIRECTION ( 'NONE',  ( -1.000000000000000000, 0.000000000000000000, 0.000000000000000000 ) ) ;
#60137 = CARTESIAN_POINT ( 'NONE',  ( -18.59999999999999787, 51.38014393322265505, -230.1906178717505611 ) ) ;
#60138 = CIRCLE ( 'NONE', #68353, 0.09999999999999491240 ) ;
#60139 = DIRECTION ( 'NONE',  ( 0.000000000000000000, -0.9908441862701782288, -0.1350103645450542456 ) ) ;
#60140 = ADVANCED_FACE ( 'NONE', ( #8963 ), #70255, .F. ) ;
#60141 = AXIS2_PLACEMENT_3D ( 'NONE', #255404, #57233, #75567 ) ;
#60142 = ORIENTED_EDGE ( 'NONE', *, *, #199663, .T. ) ;
#60143 = CIRCLE ( 'NONE', #155858, 0.2000000000000000944 ) ;
#60144 = EDGE_CURVE ( 'NONE', #108480, #68656, #117080, .T. ) ;
#60146 = ORIENTED_EDGE ( 'NONE', *, *, #21652, .T. ) ;
#60145 = EDGE_LOOP ( 'NONE', ( #109109, #152905, #210735, #99904 ) ) ;
#60147 = EDGE_LOOP ( 'NONE', ( #251526, #210566, #114599, #244310 ) ) ;
#60148 = EDGE_LOOP ( 'NONE', ( #208226, #80676, #68858, #74259 ) ) ;
#60149 = EDGE_CURVE ( 'NONE', #53843, #202387, #155116, .T. ) ;
#60150 = CARTESIAN_POINT ( 'NONE',  ( 20.94999999999999929, 76.00000000001126921, -203.5231074845248997 ) ) ;
#60151 = CARTESIAN_POINT ( 'NONE',  ( -18.59999999999999787, -1.135018845899022466, -108.2169768834323662 ) ) ;
#60152 = ADVANCED_FACE ( 'NONE', ( #49378 ), #72819, .T. ) ;
#60154 = CYLINDRICAL_SURFACE ( 'NONE', #174046, 0.1000000000000028644 ) ;
#60153 = CARTESIAN_POINT ( 'NONE',  ( 18.59999999999999432, 23.98305617022077030, -253.3362246115443099 ) ) ;
#60155 = CARTESIAN_POINT ( 'NONE',  ( 18.59999999999999076, 33.89981536720673461, -236.1713368690715527 ) ) ;
#60156 = EDGE_LOOP ( 'NONE', ( #1123, #254123, #63713, #20352 ) ) ;
#60157 = LINE ( 'NONE', #220540, #79836 ) ;
#60159 = VECTOR ( 'NONE', #245691, 1000.000000000000000 ) ;
#60158 = FILL_AREA_STYLE ('',( #120191 ) ) ;
#60161 = AXIS2_PLACEMENT_3D ( 'NONE', #196294, #138855, #254926 ) ;
#60160 = DIRECTION ( 'NONE',  ( 3.469446951953498700E-14, -0.7899159663865300551, -0.6132151058540831201 ) ) ;
#60162 = EDGE_CURVE ( 'NONE', #173202, #98368, #37994, .T. ) ;
#60163 = CARTESIAN_POINT ( 'NONE',  ( -23.39999999999994529, 82.72707916847673459, -26.51159310135756897 ) ) ;
#60164 = B_SPLINE_CURVE_WITH_KNOTS ( 'NONE', 3,
 ( #50900, #150057, #147464, #226997, #129195, #229580, #228297, #48359, #90045, #130464 ),
 .UNSPECIFIED., .F., .F.,
 ( 4, 3, 3, 4 ),
 ( 0.000000000000000000, 4.874959354402676393E-05, 9.785140065120904985E-05, 0.0001360444631936179696 ),
 .UNSPECIFIED. ) ;
#60165 = CARTESIAN_POINT ( 'NONE',  ( -20.54999999999999716, 74.00000000001186606, -90.29848556176222019 ) ) ;
#60167 = EDGE_LOOP ( 'NONE', ( #189022, #42246, #201154, #24896 ) ) ;
#60166 = AXIS2_PLACEMENT_3D ( 'NONE', #61647, #181609, #45931 ) ;
#60168 = DIRECTION ( 'NONE',  ( -0.000000000000000000, 6.982962677686266711E-15, -1.000000000000000000 ) ) ;
#60169 = TOROIDAL_SURFACE ( 'NONE', #205925, 0.2000000000000000111, 0.1000000000000000056 ) ;
#60170 = CARTESIAN_POINT ( 'NONE',  ( 21.05000000000000071, 78.17003882911672008, -228.8770135013149911 ) ) ;
#60171 = EDGE_LOOP ( 'NONE', ( #152338, #107019, #130110, #235507 ) ) ;
#60172 = DIRECTION ( 'NONE',  ( 0.000000000000000000, -1.000000000000000000, 0.000000000000000000 ) ) ;
#60173 = DIRECTION ( 'NONE',  ( 0.000000000000000000, 0.000000000000000000, 1.000000000000000000 ) ) ;
#60174 = CARTESIAN_POINT ( 'NONE',  ( -17.04761207306817639, 10.02645087340892438, -121.3500000000000227 ) ) ;
#60175 = DIRECTION ( 'NONE',  ( 1.000000000000000000, 0.000000000000000000, 0.000000000000000000 ) ) ;
#60176 = VECTOR ( 'NONE', #229089, 1000.000000000000000 ) ;
#60177 = CARTESIAN_POINT ( 'NONE',  ( -20.94999999999999929, 76.00000000001165290, -69.52310748452431710 ) ) ;
#60179 = ORIENTED_EDGE ( 'NONE', *, *, #229230, .T. ) ;
#60178 = AXIS2_PLACEMENT_3D ( 'NONE', #84664, #43025, #220383 ) ;
#60180 = CARTESIAN_POINT ( 'NONE',  ( 18.44364597020195617, 46.98014916993328427, -255.3266904785022575 ) ) ;
#60181 = DIRECTION ( 'NONE',  ( -1.000000000000000000, 0.000000000000000000, 0.000000000000000000 ) ) ;
#60183 = EDGE_CURVE ( 'NONE', #80617, #254732, #167186, .T. ) ;
#60182 = CARTESIAN_POINT ( 'NONE',  ( -20.64999999999999858, 1.148907358139439339E-11, -201.0000000000015064 ) ) ;
#60184 = AXIS2_PLACEMENT_3D ( 'NONE', #83972, #164857, #120607 ) ;
#60186 = CARTESIAN_POINT ( 'NONE',  ( 18.59999999999999432, 1.637172712981537659, -112.0821533654720525 ) ) ;
#60185 = CARTESIAN_POINT ( 'NONE',  ( 20.94999999999999574, 65.52661458509869874, -61.94445302027585143 ) ) ;
#60187 = CARTESIAN_POINT ( 'NONE',  ( 18.59999999999999076, 11.65000000001115943, -158.7500000000000284 ) ) ;
#60188 = DIRECTION ( 'NONE',  ( 0.000000000000000000, -0.2617529984164506107, -0.9651348961777299618 ) ) ;
#60189 = CARTESIAN_POINT ( 'NONE',  ( -20.94999999999999929, 1.115600667400684642E-11, -100.5000000000000284 ) ) ;
#60190 = CARTESIAN_POINT ( 'NONE',  ( 22.47809213839789066, 75.96246293238351655, -114.6730808193121192 ) ) ;
#60191 = ORIENTED_EDGE ( 'NONE', *, *, #203595, .F. ) ;
#60192 = VERTEX_POINT ( 'NONE', #190180 ) ;
#60193 = EDGE_CURVE ( 'NONE', #244844, #86021, #208684, .T. ) ;
#60194 = VERTEX_POINT ( 'NONE', #166788 ) ;
#60195 = CARTESIAN_POINT ( 'NONE',  ( -21.05000000000000071, 1.162701749949165642, -175.3999999999999773 ) ) ;
#60196 =( NAMED_UNIT ( * ) PLANE_ANGLE_UNIT ( ) SI_UNIT ( $, .RADIAN. ) );
#60197 = AXIS2_PLACEMENT_3D ( 'NONE', #221609, #162967, #101650 ) ;
#60198 = AXIS2_PLACEMENT_3D ( 'NONE', #97849, #118750, #103002 ) ;
#60199 = CARTESIAN_POINT ( 'NONE',  ( -18.59999996769639097, -9.363273769819180359, -174.6814939154657793 ) ) ;
#60200 = B_SPLINE_CURVE_WITH_KNOTS ( 'NONE', 3,
 ( #172942, #154647, #157214, #54219, #193747, #236703, #252413 ),
 .UNSPECIFIED., .F., .F.,
 ( 4, 3, 4 ),
 ( 0.000000000000000000, 4.520325912680675046E-05, 5.794988040901435228E-05 ),
 .UNSPECIFIED. ) ;
#60201 = EDGE_CURVE ( 'NONE', #255700, #226146, #183726, .T. ) ;
#60202 = AXIS2_PLACEMENT_3D ( 'NONE', #65789, #145314, #46217 ) ;
#60203 = LINE ( 'NONE', #17252, #196140 ) ;
#60204 = ORIENTED_EDGE ( 'NONE', *, *, #196952, .F. ) ;
#60205 = EDGE_CURVE ( 'NONE', #105079, #131402, #96214, .T. ) ;
#60206 = CARTESIAN_POINT ( 'NONE',  ( -21.05000000000000071, 74.16465844978745281, -91.46795619196133487 ) ) ;
#60207 = CARTESIAN_POINT ( 'NONE',  ( -15.69373346032659100, 9.356790025057037496, -50.70482650861391960 ) ) ;
#60208 = DIRECTION ( 'NONE',  ( -1.000000000000000000, -0.000000000000000000, -0.000000000000000000 ) ) ;
#60209 = DIRECTION ( 'NONE',  ( 1.000000000000000000, 0.000000000000000000, 0.000000000000000000 ) ) ;
#60211 = VERTEX_POINT ( 'NONE', #253976 ) ;
#60210 = DIRECTION ( 'NONE',  ( 1.000000000000000000, 0.000000000000000000, 0.000000000000000000 ) ) ;
#60213 = DIRECTION ( 'NONE',  ( 0.000000000000000000, 0.000000000000000000, -1.000000000000000000 ) ) ;
#60212 = CARTESIAN_POINT ( 'NONE',  ( -18.59999999999999787, 64.35000000001222986, -148.2731074845243882 ) ) ;
#60214 = DIRECTION ( 'NONE',  ( 1.000000000000000000, 0.000000000000000000, 0.000000000000000000 ) ) ;
#60215 = EDGE_CURVE ( 'NONE', #197319, #4376, #237871, .T. ) ;
#60216 = CARTESIAN_POINT ( 'NONE',  ( 18.59999999999999432, 74.83729825007388570, -94.92310748452432279 ) ) ;
#60217 = ORIENTED_EDGE ( 'NONE', *, *, #144720, .F. ) ;
#60218 = AXIS2_PLACEMENT_3D ( 'NONE', #239436, #142861, #80315 ) ;
#60219 = EDGE_CURVE ( 'NONE', #62401, #235424, #158797, .T. ) ;
#60220 = FACE_OUTER_BOUND ( 'NONE', #53622, .T. ) ;
#60221 = EDGE_CURVE ( 'NONE', #73682, #184556, #46321, .T. ) ;
#60222 = AXIS2_PLACEMENT_3D ( 'NONE', #52901, #132447, #249831 ) ;
#60223 = DIRECTION ( 'NONE',  ( -0.000000000000000000, 1.000000000000000000, 6.982962677686266711E-15 ) ) ;
#60224 = AXIS2_PLACEMENT_3D ( 'NONE', #171493, #11105, #8536 ) ;
#60225 = ORIENTED_EDGE ( 'NONE', *, *, #20323, .F. ) ;
#60226 = DIRECTION ( 'NONE',  ( 0.000000000000000000, -0.9770955615653313941, -0.2128009952263603677 ) ) ;
#60227 = CARTESIAN_POINT ( 'NONE',  ( -16.87331047859649757, 66.05000000001255955, -182.6731074845244223 ) ) ;
#60228 = ORIENTED_EDGE ( 'NONE', *, *, #193434, .F. ) ;
#60229 = CARTESIAN_POINT ( 'NONE',  ( -18.59999999999999787, -1.835341550213255957, -45.05515129256298223 ) ) ;
#60230 = ADVANCED_FACE ( 'NONE', ( #238266 ), #50410, .T. ) ;
#60231 = CARTESIAN_POINT ( 'NONE',  ( -21.14999999999999858, 55.98745301258801987, -232.8057040749261262 ) ) ;
#60232 = CARTESIAN_POINT ( 'NONE',  ( -20.64999999999999858, 76.00000000001165290, -69.52310748452431710 ) ) ;
#60233 = ORIENTED_EDGE ( 'NONE', *, *, #94036, .T. ) ;
#60234 = AXIS2_PLACEMENT_3D ( 'NONE', #169682, #249185, #66689 ) ;
#60235 = EDGE_LOOP ( 'NONE', ( #113938, #90047, #35417, #238150 ) ) ;
#60236 = DIRECTION ( 'NONE',  ( 1.000000000000000000, 7.304098846218134667E-16, -0.000000000000000000 ) ) ;
#60238 = TOROIDAL_SURFACE ( 'NONE', #147168, 0.2000000000000000111, 0.1000000000000000056 ) ;
#60237 = CYLINDRICAL_SURFACE ( 'NONE', #102621, 0.1000000000000028644 ) ;
#60239 = CARTESIAN_POINT ( 'NONE',  ( -16.89935556175753106, 62.95755809683543447, -213.6002253325821698 ) ) ;
#60240 = CARTESIAN_POINT ( 'NONE',  ( -23.39999999999994529, 84.00000000001119815, -37.18565239344504647 ) ) ;
#60242 = CARTESIAN_POINT ( 'NONE',  ( 19.75857864376268935, 64.25000000001250555, -178.6731074845244507 ) ) ;
#60241 = DIRECTION ( 'NONE',  ( 0.000000000000000000, 1.000000000000000000, 0.000000000000000000 ) ) ;
#60243 = CARTESIAN_POINT ( 'NONE',  ( 18.39999999999999858, -9.499999999988842703, -174.1001893912220737 ) ) ;
#60244 = CARTESIAN_POINT ( 'NONE',  ( -16.87372386987899375, 66.11939976637481209, -56.37383761265798654 ) ) ;
#60245 = CARTESIAN_POINT ( 'NONE',  ( -22.49999999999999645, 64.25043287652275126, -136.6239658536231332 ) ) ;
#60246 = CIRCLE ( 'NONE', #226847, 12.87499999999999822 ) ;
#60247 = ORIENTED_EDGE ( 'NONE', *, *, #133750, .T. ) ;
#60248 = DIRECTION ( 'NONE',  ( -1.000000000000000000, -2.671448610905051031E-14, -6.406987848362951272E-14 ) ) ;
#60249 = TOROIDAL_SURFACE ( 'NONE', #206009, 0.2000000000000000111, 0.1000000000000000056 ) ;
#60251 = VERTEX_POINT ( 'NONE', #55752 ) ;
#60250 = DIRECTION ( 'NONE',  ( 0.000000000000000000, 0.000000000000000000, -1.000000000000000000 ) ) ;
#60252 = AXIS2_PLACEMENT_3D ( 'NONE', #165829, #71858, #151395 ) ;
#60253 = DIRECTION ( 'NONE',  ( 0.000000000000000000, 1.000000000000000000, 0.000000000000000000 ) ) ;
#60254 = CARTESIAN_POINT ( 'NONE',  ( 18.39999999999999503, 64.25000000001182343, -82.17310748452439384 ) ) ;
#60256 = CARTESIAN_POINT ( 'NONE',  ( -20.85000000000000142, 7.021664781911246322, -204.7335654018972662 ) ) ;
#60255 = LINE ( 'NONE', #58946, #187746 ) ;
#60257 = EDGE_CURVE ( 'NONE', #162766, #238178, #142015, .T. ) ;
#60258 = ORIENTED_EDGE ( 'NONE', *, *, #216881, .T. ) ;
#60260 = CARTESIAN_POINT ( 'NONE',  ( -17.11825945287482753, 23.02528674727019364, -230.8469138855057281 ) ) ;
#60259 = DIRECTION ( 'NONE',  ( 1.000000000000000000, -0.000000000000000000, 0.000000000000000000 ) ) ;
#60262 = EDGE_CURVE ( 'NONE', #8118, #220769, #79636, .T. ) ;
#60261 = DIRECTION ( 'NONE',  ( -0.000000000000000000, 6.982962677686266711E-15, -1.000000000000000000 ) ) ;
#60263 = CARTESIAN_POINT ( 'NONE',  ( -20.94999999999999929, -1.835341550213255957, -112.1551512925630192 ) ) ;
#60264 = DIRECTION ( 'NONE',  ( 0.000000000000000000, -0.8814952561688430555, 0.4721928772777346239 ) ) ;
#60265 = CARTESIAN_POINT ( 'NONE',  ( 21.14999999999999858, 64.27847795353595473, -247.1247091181747066 ) ) ;
#60266 = ORIENTED_EDGE ( 'NONE', *, *, #163278, .T. ) ;
#60267 = DIRECTION ( 'NONE',  ( 1.000000000000000000, 0.000000000000000000, 0.000000000000000000 ) ) ;
#60268 = ORIENTED_EDGE ( 'NONE', *, *, #73518, .T. ) ;
#60269 = EDGE_CURVE ( 'NONE', #139384, #62835, #54500, .T. ) ;
#60270 = FACE_OUTER_BOUND ( 'NONE', #4352, .T. ) ;
#60271 = ORIENTED_EDGE ( 'NONE', *, *, #113859, .F. ) ;
#60272 = CARTESIAN_POINT ( 'NONE',  ( -20.88420186297724257, 46.46179379974390855, -243.0832762246653260 ) ) ;
#60273 = TOROIDAL_SURFACE ( 'NONE', #110336, 0.6000000000000009770, 0.1000000000000000056 ) ;
#60274 = ORIENTED_EDGE ( 'NONE', *, *, #61366, .F. ) ;
#60275 = CARTESIAN_POINT ( 'NONE',  ( 20.85000000000000142, 87.65000000001244018, -170.0231074845242745 ) ) ;
#60276 = AXIS2_PLACEMENT_3D ( 'NONE', #31439, #88781, #107076 ) ;
#60277 = DIRECTION ( 'NONE',  ( 0.000000000000000000, 0.000000000000000000, -1.000000000000000000 ) ) ;
#60278 = ORIENTED_EDGE ( 'NONE', *, *, #213156, .T. ) ;
#60279 = CARTESIAN_POINT ( 'NONE',  ( -16.85312964099708211, 9.913604682078863917, -87.60281570643047644 ) ) ;
#60280 = CARTESIAN_POINT ( 'NONE',  ( -18.47690164073606667, -9.464844538001088381, -174.2013809398361559 ) ) ;
#60281 = DIRECTION ( 'NONE',  ( -0.000000000000000000, -6.982962677686266711E-15, 1.000000000000000000 ) ) ;
#60282 = CARTESIAN_POINT ( 'NONE',  ( -20.94999999999999929, 76.00000000001170974, -69.52310748452431710 ) ) ;
#60283 = DIRECTION ( 'NONE',  ( 0.000000000000000000, 0.000000000000000000, -1.000000000000000000 ) ) ;
#60284 = CARTESIAN_POINT ( 'NONE',  ( 12.84233041328157476, 62.18838770701750462, -218.4972640811180611 ) ) ;
#60285 = ADVANCED_FACE ( 'NONE', ( #217411 ), #15399, .F. ) ;
#60286 = ORIENTED_EDGE ( 'NONE', *, *, #208781, .F. ) ;
#60287 = DIRECTION ( 'NONE',  ( 0.000000000000000000, 0.000000000000000000, -1.000000000000000000 ) ) ;
#60288 = ORIENTED_EDGE ( 'NONE', *, *, #148181, .T. ) ;
#60290 = VERTEX_POINT ( 'NONE', #134032 ) ;
#60289 = DIRECTION ( 'NONE',  ( 0.000000000000000000, -7.109473446599835262E-15, 1.000000000000000000 ) ) ;
#60291 = CIRCLE ( 'NONE', #101966, 0.09999999999998898659 ) ;
#60292 = ORIENTED_EDGE ( 'NONE', *, *, #215887, .F. ) ;
#60293 = CIRCLE ( 'NONE', #164556, 0.5000000000000004441 ) ;
#60294 = CARTESIAN_POINT ( 'NONE',  ( -33.72168855820451938, 66.05000000001200533, -115.6731074845243228 ) ) ;
#60295 = DIRECTION ( 'NONE',  ( 1.000000000000000000, -2.952720810173289112E-16, -2.061873921506763405E-30 ) ) ;
#60296 = CARTESIAN_POINT ( 'NONE',  ( 12.29592348164038818, 66.64419340838244921, -187.2320049529782864 ) ) ;
#60297 = CARTESIAN_POINT ( 'NONE',  ( 20.97468175916167965, 60.18418091238081757, -221.2464335850836505 ) ) ;
#60298 = DIRECTION ( 'NONE',  ( 1.000000000000000000, 0.000000000000000000, 0.000000000000000000 ) ) ;
#60299 = EDGE_LOOP ( 'NONE', ( #130861, #189906, #224239, #77770 ) ) ;
#60300 = ADVANCED_FACE ( 'NONE', ( #114479 ), #234416, .T. ) ;
#60301 = FACE_OUTER_BOUND ( 'NONE', #222223, .T. ) ;
#60302 = DIRECTION ( 'NONE',  ( 0.000000000000000000, 0.1495327102803283015, 0.9887567792719397231 ) ) ;
#60303 = EDGE_CURVE ( 'NONE', #1348, #201739, #121214, .T. ) ;
#60305 = ORIENTED_EDGE ( 'NONE', *, *, #250739, .T. ) ;
#60304 = CARTESIAN_POINT ( 'NONE',  ( -23.15000000000000213, 1.115649653272650466E-11, -71.00000000000001421 ) ) ;
#60306 = DIRECTION ( 'NONE',  ( 1.000000000000000000, 0.000000000000000000, 0.000000000000000000 ) ) ;
#60307 = EDGE_CURVE ( 'NONE', #154129, #146487, #33661, .T. ) ;
#60309 = AXIS2_PLACEMENT_3D ( 'NONE', #156001, #56837, #154722 ) ;
#60308 = CARTESIAN_POINT ( 'NONE',  ( 21.51976009735019346, 6.910458441670357388, -100.5000000000000284 ) ) ;
#60310 = ORIENTED_EDGE ( 'NONE', *, *, #31490, .F. ) ;
#60311 = AXIS2_PLACEMENT_3D ( 'NONE', #78280, #35359, #36638 ) ;
#60312 = AXIS2_PLACEMENT_3D ( 'NONE', #174113, #51516, #33312 ) ;
#60313 = VECTOR ( 'NONE', #17633, 1000.000000000000000 ) ;
#60314 = EDGE_CURVE ( 'NONE', #64432, #241204, #136591, .T. ) ;
#60315 = CARTESIAN_POINT ( 'NONE',  ( 21.05315837517336419, 64.24999999299804188, -109.8647514757571315 ) ) ;
#60318 = EDGE_CURVE ( 'NONE', #211247, #66896, #50604, .T. ) ;
#60317 = EDGE_CURVE ( 'NONE', #121164, #156961, #104743, .T. ) ;
#60316 = ORIENTED_EDGE ( 'NONE', *, *, #201474, .F. ) ;
#60319 = CYLINDRICAL_SURFACE ( 'NONE', #171084, 0.1000000000000101225 ) ;
#60320 = CARTESIAN_POINT ( 'NONE',  ( -21.05000000000000071, 64.35000000001195986, -102.9231074845243938 ) ) ;
#60321 = CARTESIAN_POINT ( 'NONE',  ( -20.94999999999999929, -1.261786168565025568, -8.086498963545480478 ) ) ;
#60322 = DIRECTION ( 'NONE',  ( 0.000000000000000000, 0.9651348961777379554, -0.2617529984164210233 ) ) ;
#60323 = AXIS2_PLACEMENT_3D ( 'NONE', #31005, #192613, #191356 ) ;
#60324 = EDGE_CURVE ( 'NONE', #17273, #240326, #162603, .T. ) ;
#60325 = EDGE_CURVE ( 'NONE', #87242, #238381, #64766, .T. ) ;
#60326 = AXIS2_PLACEMENT_3D ( 'NONE', #161757, #23544, #83443 ) ;
#60327 = ORIENTED_EDGE ( 'NONE', *, *, #4800, .T. ) ;
#60328 = DIRECTION ( 'NONE',  ( 1.000000000000000000, -0.000000000000000000, -0.000000000000000000 ) ) ;
#60329 = AXIS2_PLACEMENT_3D ( 'NONE', #29361, #206673, #69745 ) ;
#60330 = AXIS2_PLACEMENT_3D ( 'NONE', #66386, #84613, #145904 ) ;
#60331 = VERTEX_POINT ( 'NONE', #244678 ) ;
#60332 = CARTESIAN_POINT ( 'NONE',  ( -17.01764560440361507, 9.950000000011138823, -188.2500000007888730 ) ) ;
#60333 = EDGE_CURVE ( 'NONE', #155916, #212250, #46500, .T. ) ;
#60334 = DIRECTION ( 'NONE',  ( 0.000000000000000000, 0.000000000000000000, -1.000000000000000000 ) ) ;
#60336 = ORIENTED_EDGE ( 'NONE', *, *, #25039, .T. ) ;
#60335 = DIRECTION ( 'NONE',  ( 0.000000000000000000, 0.000000000000000000, 1.000000000000000000 ) ) ;
#60337 = CARTESIAN_POINT ( 'NONE',  ( -17.04761207306818704, 10.02645087340892616, -54.35000000000000853 ) ) ;
#60338 = CARTESIAN_POINT ( 'NONE',  ( 20.94999999999999929, 23.45160524131172153, -253.2535058871250726 ) ) ;
#60339 = CARTESIAN_POINT ( 'NONE',  ( 21.05000000000000071, 71.14953271029217774, -81.55737489352601699 ) ) ;
#60340 = LINE ( 'NONE', #119055, #47725 ) ;
#60341 = CIRCLE ( 'NONE', #35269, 0.1000000000000106498 ) ;
#60342 = CARTESIAN_POINT ( 'NONE',  ( -18.40000000000000213, 64.52683809665005299, -182.5731074845244279 ) ) ;
#60344 = ADVANCED_FACE ( 'NONE', ( #219991 ), #105134, .T. ) ;
#60343 = DIRECTION ( 'NONE',  ( 7.304098846218134667E-16, -1.000000000000000000, 0.000000000000000000 ) ) ;
#60346 = VERTEX_POINT ( 'NONE', #139145 ) ;
#60345 = DIRECTION ( 'NONE',  ( 1.000000000000000000, 0.000000000000000000, 0.000000000000000000 ) ) ;
#60347 = CIRCLE ( 'NONE', #81184, 0.1000000000000028644 ) ;
#60348 = ADVANCED_FACE ( 'NONE', ( #179609 ), #85575, .F. ) ;
#60349 = VECTOR ( 'NONE', #198424, 1000.000000000000000 ) ;
#60350 = DIRECTION ( 'NONE',  ( 3.616040088954497272E-32, -1.224646799147352961E-16, 1.000000000000000000 ) ) ;
#60351 = VECTOR ( 'NONE', #136361, 1000.000000000000000 ) ;
#60352 = ORIENTED_EDGE ( 'NONE', *, *, #56341, .F. ) ;
#60353 = VERTEX_POINT ( 'NONE', #41388 ) ;
#60354 = AXIS2_PLACEMENT_3D ( 'NONE', #158764, #195326, #139138 ) ;
#60356 = ADVANCED_FACE ( 'NONE', ( #4769 ), #3502, .T. ) ;
#60355 = CARTESIAN_POINT ( 'NONE',  ( -18.40000000000000213, 85.68240343348806221, -62.86626410711146207 ) ) ;
#60357 = CARTESIAN_POINT ( 'NONE',  ( 21.07094088545303734, 69.67983277809545939, -103.1220011870765774 ) ) ;
#60358 = VECTOR ( 'NONE', #118117, 1000.000000000000000 ) ;
#60359 = B_SPLINE_CURVE_WITH_KNOTS ( 'NONE', 3,
 ( #119363, #198887, #20266, #179350, #234156, #60642, #140177, #254947 ),
 .UNSPECIFIED., .F., .F.,
 ( 4, 2, 2, 4 ),
 ( 0.000000000000000000, 9.550056980123377442E-05, 0.0001910011396024675488, 0.0003820022792049778695 ),
 .UNSPECIFIED. ) ;
#60360 = ORIENTED_EDGE ( 'NONE', *, *, #166781, .F. ) ;
#60361 = CARTESIAN_POINT ( 'NONE',  ( 21.05000000000000071, 2.761092913073515565, -213.6778149113116854 ) ) ;
#60362 = DIRECTION ( 'NONE',  ( 1.000000000000000000, 0.000000000000000000, 0.000000000000000000 ) ) ;
#60363 = ADVANCED_FACE ( 'NONE', ( #24386 ), #204724, .T. ) ;
#60364 = ORIENTED_EDGE ( 'NONE', *, *, #20635, .T. ) ;
#60365 = B_SPLINE_CURVE_WITH_KNOTS ( 'NONE', 3,
 ( #149722, #14052, #135248, #210958, #209669, #174446, #130121, #229244 ),
 .UNSPECIFIED., .F., .F.,
 ( 4, 2, 2, 4 ),
 ( 0.000000000000000000, 0.0001094981963948558640, 0.0002189963927897117281, 0.0004379927855794304493 ),
 .UNSPECIFIED. ) ;
#60366 = DIRECTION ( 'NONE',  ( 0.000000000000000000, 0.2128009952263601456, -0.9770955615653316162 ) ) ;
#60367 = CARTESIAN_POINT ( 'NONE',  ( -16.93226657140833069, 66.00045617728818570, -190.9443943735508071 ) ) ;
#60368 = VERTEX_POINT ( 'NONE', #180880 ) ;
#60369 = VERTEX_POINT ( 'NONE', #240852 ) ;
#60370 = FACE_OUTER_BOUND ( 'NONE', #172383, .T. ) ;
#60371 = ORIENTED_EDGE ( 'NONE', *, *, #147953, .T. ) ;
#60373 = ADVANCED_FACE ( 'NONE', ( #122195 ), #102582, .T. ) ;
#60372 = DIRECTION ( 'NONE',  ( 2.978066053179062821E-16, 0.4088369013363259419, -0.9126074666063780372 ) ) ;
#60375 = ORIENTED_EDGE ( 'NONE', *, *, #868, .F. ) ;
#60374 = FACE_OUTER_BOUND ( 'NONE', #26128, .T. ) ;
#60376 = DIRECTION ( 'NONE',  ( -0.000000000000000000, 1.000000000000000000, 6.982962677686266711E-15 ) ) ;
#60377 = ORIENTED_EDGE ( 'NONE', *, *, #177386, .T. ) ;
#60378 = AXIS2_PLACEMENT_3D ( 'NONE', #165203, #120969, #122232 ) ;
#60379 = CARTESIAN_POINT ( 'NONE',  ( 22.59999999999999432, 0.1008583691098678403, -88.75043287651062940 ) ) ;
#60380 = ORIENTED_EDGE ( 'NONE', *, *, #221047, .T. ) ;
#60381 = CIRCLE ( 'NONE', #106162, 0.09999999999998898659 ) ;
#60383 = VERTEX_POINT ( 'NONE', #45206 ) ;
#60382 = ORIENTED_EDGE ( 'NONE', *, *, #200956, .T. ) ;
#60384 = DIRECTION ( 'NONE',  ( 1.000000000000000000, -2.836875882374966742E-15, 6.332486386695204832E-15 ) ) ;
#60385 = ORIENTED_EDGE ( 'NONE', *, *, #59673, .T. ) ;
#60386 = CIRCLE ( 'NONE', #106164, 0.09999999999998898659 ) ;
#60387 = DIRECTION ( 'NONE',  ( 0.000000000000000000, -0.8660254037844445918, -0.4999999999999897304 ) ) ;
#60388 = VERTEX_POINT ( 'NONE', #124756 ) ;
#60389 = AXIS2_PLACEMENT_3D ( 'NONE', #25123, #147613, #5512 ) ;
#60390 = AXIS2_PLACEMENT_3D ( 'NONE', #150624, #191060, #177602 ) ;
#60391 = VERTEX_POINT ( 'NONE', #123467 ) ;
#60392 = DIRECTION ( 'NONE',  ( 6.938893903906840889E-14, -0.2128009952263485993, 0.9770955615653341697 ) ) ;
#60393 = FACE_OUTER_BOUND ( 'NONE', #78385, .T. ) ;
#60395 = ORIENTED_EDGE ( 'NONE', *, *, #13800, .T. ) ;
#60394 = DIRECTION ( 'NONE',  ( 1.000000000000000000, 0.000000000000000000, 0.000000000000000000 ) ) ;
#60396 = DIRECTION ( 'NONE',  ( 0.000000000000000000, 6.982962677686266711E-15, -1.000000000000000000 ) ) ;
#60397 = ORIENTED_EDGE ( 'NONE', *, *, #166871, .F. ) ;
#60398 = CYLINDRICAL_SURFACE ( 'NONE', #207685, 0.09999999999999939493 ) ;
#60399 = DIRECTION ( 'NONE',  ( 0.000000000000000000, -1.000000000000000000, 0.000000000000000000 ) ) ;
#60400 = DIRECTION ( 'NONE',  ( 0.000000000000000000, -1.000000000000000000, 0.000000000000000000 ) ) ;
#60401 = AXIS2_PLACEMENT_3D ( 'NONE', #159590, #21384, #216969 ) ;
#60402 = ORIENTED_EDGE ( 'NONE', *, *, #102395, .T. ) ;
#60403 = DIRECTION ( 'NONE',  ( 0.000000000000000000, 0.000000000000000000, -1.000000000000000000 ) ) ;
#60404 = CARTESIAN_POINT ( 'NONE',  ( 21.05000000000000071, 76.00000000001246292, -172.0231074845243597 ) ) ;
#60405 = B_SPLINE_CURVE_WITH_KNOTS ( 'NONE', 3,
 ( #194709, #172601, #76015, #117706, #192134, #252079, #14790, #236371, #212961, #176424, #33087, #53889, #115146, #91728, #153028, #255882 ),
 .UNSPECIFIED., .F., .F.,
 ( 4, 3, 3, 3, 3, 4 ),
 ( 0.000000000000000000, 2.372700795693547977E-05, 5.739057815866958510E-05, 9.073899019179559378E-05, 0.0001243544287365697066, 0.0001585386695601189160 ),
 .UNSPECIFIED. ) ;
#60406 = DIRECTION ( 'NONE',  ( -1.000000000000000000, 2.952720810173289112E-16, 2.061873921506763405E-30 ) ) ;
#60407 = VECTOR ( 'NONE', #205989, 1000.000000000000000 ) ;
#60408 = EDGE_LOOP ( 'NONE', ( #158610, #239021 ) ) ;
#60409 = DIRECTION ( 'NONE',  ( 0.000000000000000000, 0.000000000000000000, -1.000000000000000000 ) ) ;
#60410 = ORIENTED_EDGE ( 'NONE', *, *, #107069, .F. ) ;
#60411 = VERTEX_POINT ( 'NONE', #161325 ) ;
#60412 = CARTESIAN_POINT ( 'NONE',  ( -18.59999999999999787, 36.65892442174935439, -249.5511627012433848 ) ) ;
#60413 = ORIENTED_EDGE ( 'NONE', *, *, #230150, .F. ) ;
#60414 = EDGE_LOOP ( 'NONE', ( #17683, #48901, #206743, #143988 ) ) ;
#60415 = FACE_OUTER_BOUND ( 'NONE', #227442, .T. ) ;
#60416 = DIRECTION ( 'NONE',  ( 0.000000000000000000, 0.000000000000000000, 1.000000000000000000 ) ) ;
#60417 = EDGE_LOOP ( 'NONE', ( #105961, #52561, #116463, #194168 ) ) ;
#60418 = CIRCLE ( 'NONE', #85337, 5.000000000000000888 ) ;
#60419 = ORIENTED_EDGE ( 'NONE', *, *, #122687, .T. ) ;
#60420 = CARTESIAN_POINT ( 'NONE',  ( 20.93284271247462414, 62.82351852614502974, -207.2177435922979214 ) ) ;
#60421 = FACE_OUTER_BOUND ( 'NONE', #203744, .T. ) ;
#60422 = ORIENTED_EDGE ( 'NONE', *, *, #231976, .F. ) ;
#60423 = ADVANCED_FACE ( 'NONE', ( #242118 ), #63476, .F. ) ;
#60424 = ORIENTED_EDGE ( 'NONE', *, *, #148300, .F. ) ;
#60425 = VERTEX_POINT ( 'NONE', #80445 ) ;
#60426 = CIRCLE ( 'NONE', #135439, 0.09999999999999939493 ) ;
#60427 = AXIS2_PLACEMENT_3D ( 'NONE', #56728, #234112, #55446 ) ;
#60428 = CARTESIAN_POINT ( 'NONE',  ( 21.13422380239045850, 69.50667348520697431, -203.5231074845243882 ) ) ;
#60429 = DIRECTION ( 'NONE',  ( 0.000000000000000000, 1.000000000000000000, 6.982962677686266711E-15 ) ) ;
#60430 = DIRECTION ( 'NONE',  ( 0.000000000000000000, 0.000000000000000000, -1.000000000000000000 ) ) ;
#60431 = CARTESIAN_POINT ( 'NONE',  ( 20.94999999999999929, -1.835859311443637010, -45.00443916879852679 ) ) ;
#60432 = DIRECTION ( 'NONE',  ( -0.000000000000000000, -6.982962677686266711E-15, 1.000000000000000000 ) ) ;
#60433 = EDGE_CURVE ( 'NONE', #47818, #59075, #142197, .T. ) ;
#60434 = LINE ( 'NONE', #136100, #15328 ) ;
#60435 = ADVANCED_FACE ( 'NONE', ( #243404 ), #42640, .T. ) ;
#60436 = DIRECTION ( 'NONE',  ( -0.000000000000000000, -1.265107689135680095E-16, 1.000000000000000000 ) ) ;
#60438 = CARTESIAN_POINT ( 'NONE',  ( 21.05000000000000071, 34.07109384788311957, -243.8522760710328328 ) ) ;
#60437 = CARTESIAN_POINT ( 'NONE',  ( 20.94999999999999929, 76.00000000001142553, -36.02310748452432421 ) ) ;
#60439 = DIRECTION ( 'NONE',  ( -0.000000000000000000, -0.8700118002898356018, 0.4930308989875170078 ) ) ;
#60440 = CARTESIAN_POINT ( 'NONE',  ( -20.64999999999999858, -8.663551401858001100, -124.4758988819327215 ) ) ;
#60441 = DIRECTION ( 'NONE',  ( 0.000000000000000000, 0.4721928772777352346, 0.8814952561688428334 ) ) ;
#60442 = CARTESIAN_POINT ( 'NONE',  ( 21.15000000000005542, 82.74366731733570646, -26.36310895752070138 ) ) ;
#60443 = AXIS2_PLACEMENT_3D ( 'NONE', #230133, #132313, #48922 ) ;
#60444 = EDGE_LOOP ( 'NONE', ( #236780, #60087, #159257, #168914 ) ) ;
#60445 = EDGE_CURVE ( 'NONE', #227344, #96734, #34098, .T. ) ;
#60446 = AXIS2_PLACEMENT_3D ( 'NONE', #148481, #168085, #31136 ) ;
#60448 = ORIENTED_EDGE ( 'NONE', *, *, #195659, .F. ) ;
#60447 = DIRECTION ( 'NONE',  ( 2.978066053179067751E-16, -1.000000000000000000, 0.000000000000000000 ) ) ;
#60449 = ADVANCED_FACE ( 'NONE', ( #6070 ), #40113, .T. ) ;
#60450 = DIRECTION ( 'NONE',  ( 0.000000000000000000, 0.000000000000000000, 1.000000000000000000 ) ) ;
#60451 = CARTESIAN_POINT ( 'NONE',  ( -21.52071067811865746, 68.22071067813118361, -182.3731074845244109 ) ) ;
#60452 = EDGE_CURVE ( 'NONE', #22954, #208409, #79823, .T. ) ;
#60453 = CYLINDRICAL_SURFACE ( 'NONE', #223682, 0.1000000000000028644 ) ;
#60454 = VERTEX_POINT ( 'NONE', #188568 ) ;
#60455 = DIRECTION ( 'NONE',  ( 1.000000000000000000, 0.000000000000000000, 0.000000000000000000 ) ) ;
#60456 = EDGE_CURVE ( 'NONE', #40566, #247898, #29532, .T. ) ;
#60457 = CARTESIAN_POINT ( 'NONE',  ( -23.25000000000000355, 67.23581240663841641, -214.2531594801197627 ) ) ;
#60458 = ORIENTED_EDGE ( 'NONE', *, *, #204232, .F. ) ;
#60460 = CARTESIAN_POINT ( 'NONE',  ( -21.05000000000000071, 61.95000000001234497, -164.5094124137634708 ) ) ;
#60459 =( GEOMETRIC_REPRESENTATION_CONTEXT ( 3 ) GLOBAL_UNCERTAINTY_ASSIGNED_CONTEXT ( ( #59713 ) ) GLOBAL_UNIT_ASSIGNED_CONTEXT ( ( #192260, #210525, #190985 ) ) REPRESENTATION_CONTEXT ( 'NONE', 'WORKASPACE' ) );
#60461 = TOROIDAL_SURFACE ( 'NONE', #110548, 12.97499999999999609, 0.1000000000000000056 ) ;
#60462 = CARTESIAN_POINT ( 'NONE',  ( 21.51976009735019346, 69.08954155835245103, -69.52310748452435973 ) ) ;
#60463 = EDGE_CURVE ( 'NONE', #94787, #177719, #248542, .T. ) ;
#60464 = CARTESIAN_POINT ( 'NONE',  ( 23.24999999999999289, 64.25000000001244871, -181.7731074845244450 ) ) ;
#60465 = CARTESIAN_POINT ( 'NONE',  ( 22.50000000000000000, 76.00000000001165290, -69.52310748452431710 ) ) ;
#60467 = ORIENTED_EDGE ( 'NONE', *, *, #66022, .F. ) ;
#60466 = CARTESIAN_POINT ( 'NONE',  ( -20.94999675878240808, 67.49461024981995649, -195.5605382655040216 ) ) ;
#60469 = ORIENTED_EDGE ( 'NONE', *, *, #140315, .F. ) ;
#60468 = CARTESIAN_POINT ( 'NONE',  ( -18.48179518609121885, 85.51832530050704406, -96.13340190776337124 ) ) ;
#60470 = CYLINDRICAL_SURFACE ( 'NONE', #150052, 4.049999999999997158 ) ;
#60471 = DIRECTION ( 'NONE',  ( 1.000000000000000000, 0.000000000000000000, 0.000000000000000000 ) ) ;
#60472 = DIRECTION ( 'NONE',  ( 1.000000000000000000, 0.000000000000000000, 0.000000000000000000 ) ) ;
#60474 = EDGE_CURVE ( 'NONE', #236967, #66095, #66049, .T. ) ;
#60473 = CARTESIAN_POINT ( 'NONE',  ( -13.43673303185029688, 9.446648990640015953, -182.5891632959231288 ) ) ;
#60476 = LINE ( 'NONE', #5627, #153616 ) ;
#60475 = CARTESIAN_POINT ( 'NONE',  ( -16.93262454970419384, 63.05570051748338045, -213.0396161178616694 ) ) ;
#60477 = DIRECTION ( 'NONE',  ( -0.000000000000000000, -0.8660254037844420383, 0.4999999999999943379 ) ) ;
#60478 = CARTESIAN_POINT ( 'NONE',  ( 22.39999999999999858, 33.38250548509083870, -242.4821227592188961 ) ) ;
#60479 = CIRCLE ( 'NONE', #185579, 12.87500000000000000 ) ;
#60480 = LINE ( 'NONE', #76194, #178920 ) ;
#60481 = CARTESIAN_POINT ( 'NONE',  ( -18.40000000000000213, 5.650000000011139001, -46.15000000000000568 ) ) ;
#60482 = CARTESIAN_POINT ( 'NONE',  ( 21.08376601933332495, 10.06723741856825782, -228.1121902998345092 ) ) ;
#60483 = CIRCLE ( 'NONE', #218887, 0.1999999999999996503 ) ;
#60484 = VERTEX_POINT ( 'NONE', #26963 ) ;
#60485 = AXIS2_PLACEMENT_3D ( 'NONE', #49610, #144844, #44489 ) ;
#60486 = DIRECTION ( 'NONE',  ( -0.000000000000000000, -0.8814952561688432775, 0.4721928772777344019 ) ) ;
#60487 = EDGE_LOOP ( 'NONE', ( #28412, #108540, #137071, #160553 ) ) ;
#60488 = ORIENTED_EDGE ( 'NONE', *, *, #12267, .F. ) ;
#60489 = DIRECTION ( 'NONE',  ( 0.000000000000000000, 0.000000000000000000, -1.000000000000000000 ) ) ;
#60490 = DIRECTION ( 'NONE',  ( 1.000000000000000000, 0.000000000000000000, 0.000000000000000000 ) ) ;
#60491 = ORIENTED_EDGE ( 'NONE', *, *, #73530, .T. ) ;
#60492 = EDGE_LOOP ( 'NONE', ( #16773, #39822, #153465, #147624 ) ) ;
#60493 = ORIENTED_EDGE ( 'NONE', *, *, #220478, .F. ) ;
#60494 = CIRCLE ( 'NONE', #156423, 0.5999999999999894307 ) ;
#60495 = ORIENTED_EDGE ( 'NONE', *, *, #125824, .F. ) ;
#60496 = AXIS2_PLACEMENT_3D ( 'NONE', #254137, #36419, #235861 ) ;
#60497 = EDGE_CURVE ( 'NONE', #15176, #249034, #121582, .T. ) ;
#60498 = DIRECTION ( 'NONE',  ( 0.000000000000000000, -0.8814952561688476074, 0.4721928772777262417 ) ) ;
#60499 = CARTESIAN_POINT ( 'NONE',  ( -18.59999999999999787, 1.162701749949165642, -142.0000000000000284 ) ) ;
#60500 = DIRECTION ( 'NONE',  ( 0.000000000000000000, -0.9651348961777379554, 0.2617529984164210233 ) ) ;
#60502 = EDGE_CURVE ( 'NONE', #157963, #158625, #171462, .T. ) ;
#60501 = VECTOR ( 'NONE', #128617, 1000.000000000000000 ) ;
#60503 = CARTESIAN_POINT ( 'NONE',  ( 21.05000000000000071, 1.162701749949165642, -75.10000000000003695 ) ) ;
#60504 = DIRECTION ( 'NONE',  ( 0.000000000000000000, -6.938893903907222067E-15, 1.000000000000000000 ) ) ;
#60505 = DIRECTION ( 'NONE',  ( 1.000000000000000000, 0.000000000000000000, 0.000000000000000000 ) ) ;
#60506 = CARTESIAN_POINT ( 'NONE',  ( 21.11825140030062897, 75.99279637937912923, -142.9685150499435338 ) ) ;
#60508 = ORIENTED_EDGE ( 'NONE', *, *, #142596, .F. ) ;
#60507 = CARTESIAN_POINT ( 'NONE',  ( -21.14999999999999858, 11.65000000001115588, -134.1000000000000227 ) ) ;
#60510 = CARTESIAN_POINT ( 'NONE',  ( 20.94999999999999929, -9.399999999988844834, -124.1060308773475924 ) ) ;
#60509 = CARTESIAN_POINT ( 'NONE',  ( -16.89021194854739605, 66.05000000001224691, -149.2805393529200728 ) ) ;
#60511 = EDGE_CURVE ( 'NONE', #159037, #133646, #17325, .T. ) ;
#60512 = CARTESIAN_POINT ( 'NONE',  ( 20.85000000000000142, 11.65000000001115943, -134.0000000000000284 ) ) ;
#60513 = EDGE_CURVE ( 'NONE', #104499, #118363, #58968, .T. ) ;
#60514 = ORIENTED_EDGE ( 'NONE', *, *, #101106, .T. ) ;
#60515 = VECTOR ( 'NONE', #103268, 1000.000000000000000 ) ;
#60516 = CARTESIAN_POINT ( 'NONE',  ( -16.94165728009534888, 63.05992920170000104, -213.0780854433903642 ) ) ;
#60517 = DIRECTION ( 'NONE',  ( 1.000000000000000000, 0.000000000000000000, 0.000000000000000000 ) ) ;
#60518 = CIRCLE ( 'NONE', #135342, 0.09999999999999939493 ) ;
#60520 = EDGE_LOOP ( 'NONE', ( #160965, #250610, #23981, #24978 ) ) ;
#60519 = VECTOR ( 'NONE', #171434, 1000.000000000000000 ) ;
#60521 = EDGE_CURVE ( 'NONE', #68090, #80528, #107746, .T. ) ;
#60523 = DIRECTION ( 'NONE',  ( -1.000000000000000000, 2.849773892568378313E-16, -7.728835255496647986E-17 ) ) ;
#60522 = CARTESIAN_POINT ( 'NONE',  ( -20.65000000000000568, 68.75000000001256240, -182.6731074845244223 ) ) ;
#60524 = EDGE_CURVE ( 'NONE', #19453, #143109, #229696, .T. ) ;
#60525 = CARTESIAN_POINT ( 'NONE',  ( -16.97683810757273193, 66.05000000001182059, -82.78668419698475134 ) ) ;
#60526 = CARTESIAN_POINT ( 'NONE',  ( 22.59999985501178799, 64.25013020700868083, -69.58870615432387297 ) ) ;
#60527 = EDGE_CURVE ( 'NONE', #89909, #235335, #134004, .T. ) ;
#60528 = EDGE_LOOP ( 'NONE', ( #21286, #176872, #157680, #58913 ) ) ;
#60529 = AXIS2_PLACEMENT_3D ( 'NONE', #124549, #244476, #205334 ) ;
#60530 = LINE ( 'NONE', #120545, #76263 ) ;
#60531 = DIRECTION ( 'NONE',  ( 0.000000000000000000, -0.1568667991644355497, 0.9876197685951332295 ) ) ;
#60532 = AXIS2_PLACEMENT_3D ( 'NONE', #188066, #164656, #244165 ) ;
#60533 = ADVANCED_FACE ( 'NONE', ( #90738 ), #249835, .T. ) ;
#60534 = CARTESIAN_POINT ( 'NONE',  ( -22.57848426163148403, -0.004264329271961148776, -55.24994169310969738 ) ) ;
#60535 = CARTESIAN_POINT ( 'NONE',  ( 21.05000000000000071, 1.115600667400684642E-11, -200.9999999999999432 ) ) ;
#60536 = DIRECTION ( 'NONE',  ( 1.000000000000000000, 0.000000000000000000, 0.000000000000000000 ) ) ;
#60537 = ORIENTED_EDGE ( 'NONE', *, *, #102853, .T. ) ;
#60538 = AXIS2_PLACEMENT_3D ( 'NONE', #214600, #236725, #213314 ) ;
#60539 = CARTESIAN_POINT ( 'NONE',  ( -21.05000000000000071, -11.65000000000000036, -2.900000000000001688 ) ) ;
#60540 = EDGE_CURVE ( 'NONE', #153107, #85086, #71498, .T. ) ;
#60541 = CARTESIAN_POINT ( 'NONE',  ( 23.15000000000000213, -8.596261682231833845, -176.9501275171502641 ) ) ;
#60542 = DIRECTION ( 'NONE',  ( -3.469446951953433697E-14, 0.9908441862701605762, 0.1350103645451835310 ) ) ;
#60543 = CARTESIAN_POINT ( 'NONE',  ( -21.45000000000000284, 68.29142135624930177, -115.2731074845243455 ) ) ;
#60544 = EDGE_CURVE ( 'NONE', #126699, #216204, #217190, .T. ) ;
#60545 = DIRECTION ( 'NONE',  ( -0.4999999999999799050, 0.000000000000000000, -0.8660254037844502539 ) ) ;
#60546 = DIRECTION ( 'NONE',  ( 0.000000000000000000, -1.000000000000000000, -6.982962677686265922E-15 ) ) ;
#60547 = EDGE_CURVE ( 'NONE', #119770, #147057, #13228, .T. ) ;
#60549 = ORIENTED_EDGE ( 'NONE', *, *, #101843, .T. ) ;
#60548 = LINE ( 'NONE', #568, #125414 ) ;
#60550 = CARTESIAN_POINT ( 'NONE',  ( 23.24999999999999289, 6.650000000011155876, -79.35000000000005116 ) ) ;
#60551 = DIRECTION ( 'NONE',  ( 0.000000000000000000, 0.000000000000000000, 1.000000000000000000 ) ) ;
#60552 = FACE_BOUND ( 'NONE', #6866, .T. ) ;
#60553 = DIRECTION ( 'NONE',  ( 0.000000000000000000, 1.000000000000000000, 0.000000000000000000 ) ) ;
#60554 = CARTESIAN_POINT ( 'NONE',  ( 21.04999999999997584, 10.47338541492403863, -175.0786544642485012 ) ) ;
#60555 = ADVANCED_FACE ( 'NONE', ( #51593 ), #166474, .F. ) ;
#60557 = ORIENTED_EDGE ( 'NONE', *, *, #39746, .T. ) ;
#60556 = CARTESIAN_POINT ( 'NONE',  ( 21.07199075132371746, 67.22505500089548036, -57.30957532291152745 ) ) ;
#60558 = CARTESIAN_POINT ( 'NONE',  ( -23.25000000000000000, 65.66751761918648356, -63.92826094061123143 ) ) ;
#60559 = ADVANCED_FACE ( 'NONE', ( #131160 ), #210702, .T. ) ;
#60560 = DIRECTION ( 'NONE',  ( -1.000000000000000000, 1.836970198721029934E-16, 1.282749433769087582E-30 ) ) ;
#60561 = DIRECTION ( 'NONE',  ( -4.408576920032448588E-17, 0.1350103645451876666, -0.9908441862701600211 ) ) ;
#60562 = VERTEX_POINT ( 'NONE', #126019 ) ;
#60563 = CARTESIAN_POINT ( 'NONE',  ( -12.33960340485503870, 66.63925083009715422, -152.7085373439171576 ) ) ;
#60564 = AXIS2_PLACEMENT_3D ( 'NONE', #215259, #160452, #61323 ) ;
#60565 = DIRECTION ( 'NONE',  ( -1.000000000000000000, 7.304098846218134667E-16, 5.100424963727255829E-30 ) ) ;
#60566 = DIRECTION ( 'NONE',  ( 1.000000000000000000, 0.000000000000000000, 0.000000000000000000 ) ) ;
#60567 = AXIS2_PLACEMENT_3D ( 'NONE', #158535, #238035, #222297 ) ;
#60568 = DIRECTION ( 'NONE',  ( -0.000000000000000000, -0.8660254037844420383, 0.4999999999999943379 ) ) ;
#60569 = CARTESIAN_POINT ( 'NONE',  ( 20.94999999999999574, 76.00000000001267608, -203.5231074845243597 ) ) ;
#60570 = ORIENTED_EDGE ( 'NONE', *, *, #6348, .F. ) ;
#60571 = EDGE_LOOP ( 'NONE', ( #211809, #104784, #210136, #85687 ) ) ;
#60572 = AXIS2_PLACEMENT_3D ( 'NONE', #222985, #84729, #43086 ) ;
#60573 = DIRECTION ( 'NONE',  ( 1.000000000000000000, 0.000000000000000000, 0.000000000000000000 ) ) ;
#60574 = AXIS2_PLACEMENT_3D ( 'NONE', #151302, #15656, #131718 ) ;
#60575 = CARTESIAN_POINT ( 'NONE',  ( -21.05000000000000071, 76.00000000001142553, -36.02310748452432421 ) ) ;
#60576 = DIRECTION ( 'NONE',  ( -0.000000000000000000, 1.000000000000000000, 6.982962677686266711E-15 ) ) ;
#60577 = CYLINDRICAL_SURFACE ( 'NONE', #201493, 0.09999999999999939493 ) ;
#60578 = ORIENTED_EDGE ( 'NONE', *, *, #136023, .T. ) ;
#60579 = AXIS2_PLACEMENT_3D ( 'NONE', #113992, #153175, #192275 ) ;
#60581 = AXIS2_PLACEMENT_3D ( 'NONE', #250055, #71438, #51827 ) ;
#60580 = CARTESIAN_POINT ( 'NONE',  ( -21.56666275994539816, 76.00000000001200817, -109.9804758914176404 ) ) ;
#60582 = CARTESIAN_POINT ( 'NONE',  ( 20.52683494730048253, 10.58476304708173643, -207.3993787893872138 ) ) ;
#60583 = CARTESIAN_POINT ( 'NONE',  ( -16.78569801330231925, 9.947933733113496046, -12.65691290534750024 ) ) ;
#60584 = DIRECTION ( 'NONE',  ( -1.000000000000000000, -0.000000000000000000, -0.000000000000000000 ) ) ;
#60585 = DIRECTION ( 'NONE',  ( 0.000000000000000000, 0.000000000000000000, -1.000000000000000000 ) ) ;
#60586 = EDGE_LOOP ( 'NONE', ( #153524, #126120, #159048, #9233 ) ) ;
#60588 = ORIENTED_EDGE ( 'NONE', *, *, #156013, .F. ) ;
#60587 = DIRECTION ( 'NONE',  ( 0.000000000000000000, -0.9698110461157734008, -0.2438576117980102709 ) ) ;
#60589 = EDGE_LOOP ( 'NONE', ( #68404, #24230, #257560, #89543 ) ) ;
#60590 = DIRECTION ( 'NONE',  ( 1.713247197920696616E-14, -0.9876197685951263461, 0.1568667991644794590 ) ) ;
#60591 = ORIENTED_EDGE ( 'NONE', *, *, #255726, .F. ) ;
#60592 = CARTESIAN_POINT ( 'NONE',  ( -21.13422380239059706, 1.115527483754041871E-11, -27.00667348519442612 ) ) ;
#60593 = DIRECTION ( 'NONE',  ( -1.000000000000000000, 0.000000000000000000, 0.000000000000000000 ) ) ;
#60594 = CARTESIAN_POINT ( 'NONE',  ( 18.59999999999999432, -1.835859311432484375, -179.0044391687985410 ) ) ;
#60596 = VERTEX_POINT ( 'NONE', #205550 ) ;
#60595 = AXIS2_PLACEMENT_3D ( 'NONE', #32556, #92480, #251554 ) ;
#60597 = CARTESIAN_POINT ( 'NONE',  ( 21.05000000000000071, 17.01923898301590654, -224.3994341343041867 ) ) ;
#60598 = CARTESIAN_POINT ( 'NONE',  ( -22.50000000000000000, 12.54152817314149715, -223.4164406214577241 ) ) ;
#60599 = ORIENTED_EDGE ( 'NONE', *, *, #136914, .T. ) ;
#60600 = DIRECTION ( 'NONE',  ( -1.000000000000000000, -0.000000000000000000, -0.000000000000000000 ) ) ;
#60601 = EDGE_CURVE ( 'NONE', #202498, #37588, #7362, .T. ) ;
#60603 = ORIENTED_EDGE ( 'NONE', *, *, #23272, .F. ) ;
#60602 = CARTESIAN_POINT ( 'NONE',  ( -11.59999999999994458, 66.35000000001119247, -18.42310748452479174 ) ) ;
#60604 = CARTESIAN_POINT ( 'NONE',  ( 20.94999999999999929, 76.00000000001165290, -61.72310748452430573 ) ) ;
#60605 = CARTESIAN_POINT ( 'NONE',  ( 20.04142135623730070, 11.75000000000000355, -21.35000000000000142 ) ) ;
#60606 = EDGE_CURVE ( 'NONE', #86456, #95048, #200651, .T. ) ;
#60607 = AXIS2_PLACEMENT_3D ( 'NONE', #91444, #246646, #68021 ) ;
#60608 = VERTEX_POINT ( 'NONE', #196270 ) ;
#60609 = DIRECTION ( 'NONE',  ( 0.000000000000000000, 0.000000000000000000, -1.000000000000000000 ) ) ;
#60611 = ADVANCED_FACE ( 'NONE', ( #214547 ), #231560, .T. ) ;
#60610 = CARTESIAN_POINT ( 'NONE',  ( -15.75000000000000000, 66.65000000001204228, -120.0015881126992525 ) ) ;
#60612 = DIRECTION ( 'NONE',  ( 0.000000000000000000, 0.000000000000000000, 1.000000000000000000 ) ) ;
#60614 = EDGE_CURVE ( 'NONE', #179165, #232353, #75078, .T. ) ;
#60613 = ORIENTED_EDGE ( 'NONE', *, *, #65029, .T. ) ;
#60615 = CARTESIAN_POINT ( 'NONE',  ( 22.45305468355010703, 76.10085836911217427, -181.7726746080141140 ) ) ;
#60616 = LINE ( 'NONE', #80156, #93147 ) ;
#60617 = DIRECTION ( 'NONE',  ( 0.000000000000000000, 0.000000000000000000, 1.000000000000000000 ) ) ;
#60618 = VERTEX_POINT ( 'NONE', #172910 ) ;
#60619 = AXIS2_PLACEMENT_3D ( 'NONE', #166036, #63041, #21387 ) ;
#60620 = EDGE_CURVE ( 'NONE', #41664, #123927, #77583, .T. ) ;
#60621 = ORIENTED_EDGE ( 'NONE', *, *, #225357, .F. ) ;
#60622 = TOROIDAL_SURFACE ( 'NONE', #31643, 11.90000000000000213, 0.1000000000000000056 ) ;
#60623 = EDGE_LOOP ( 'NONE', ( #97802, #51940, #194671, #126054, #59453 ) ) ;
#60624 = DIRECTION ( 'NONE',  ( -0.000000000000000000, 1.000000000000000000, 6.982962677686266711E-15 ) ) ;
#60625 = DIRECTION ( 'NONE',  ( 0.000000000000000000, 1.000000000000000000, 6.982962677686266711E-15 ) ) ;
#60627 = VERTEX_POINT ( 'NONE', #254902 ) ;
#60626 = DIRECTION ( 'NONE',  ( 0.000000000000000000, 0.000000000000000000, 1.000000000000000000 ) ) ;
#60628 = DIRECTION ( 'NONE',  ( -0.000000000000000000, -0.000000000000000000, 1.000000000000000000 ) ) ;
#60629 = DIRECTION ( 'NONE',  ( 0.000000000000000000, -0.2617529984164856383, -0.9651348961777204138 ) ) ;
#60630 = FACE_OUTER_BOUND ( 'NONE', #4701, .T. ) ;
#60631 = CARTESIAN_POINT ( 'NONE',  ( -23.25000000000000000, 32.96286418198890544, -251.2069521516576174 ) ) ;
#60632 = CARTESIAN_POINT ( 'NONE',  ( 5.900000000000059863, 64.65000000001120384, -25.92310748452479174 ) ) ;
#60633 = DIRECTION ( 'NONE',  ( -1.000000000000000000, -0.000000000000000000, -0.000000000000000000 ) ) ;
#60636 = VERTEX_POINT ( 'NONE', #192430 ) ;
#60635 = ADVANCED_FACE ( 'NONE', ( #35938 ), #245936, .T. ) ;
#60634 = CARTESIAN_POINT ( 'NONE',  ( -16.86445178670600598, 66.03778837089669196, -182.6323300464076453 ) ) ;
#60637 = VERTEX_POINT ( 'NONE', #137564 ) ;
#60638 = CARTESIAN_POINT ( 'NONE',  ( -22.39999999999999858, 75.90000000001199965, -110.8138870828977218 ) ) ;
#60639 = EDGE_LOOP ( 'NONE', ( #57604, #184513, #234256, #140953 ) ) ;
#60640 = EDGE_LOOP ( 'NONE', ( #91527, #214672, #69975, #256077 ) ) ;
#60641 = ADVANCED_FACE ( 'NONE', ( #232857 ), #129892, .T. ) ;
#60642 = CARTESIAN_POINT ( 'NONE',  ( -21.05000000000000426, 6.413759733821437159, -167.5856130608038939 ) ) ;
#60643 = DIRECTION ( 'NONE',  ( -1.000000000000000000, -0.000000000000000000, -0.000000000000000000 ) ) ;
#60644 = CIRCLE ( 'NONE', #219056, 0.1000000000000013933 ) ;
#60645 = VECTOR ( 'NONE', #50597, 1000.000000000000000 ) ;
#60646 = CARTESIAN_POINT ( 'NONE',  ( -20.64999999999999858, -8.999999999988844479, -157.6060308773475924 ) ) ;
#60647 = DIRECTION ( 'NONE',  ( -0.000000000000000000, -0.9770955615653313941, -0.2128009952263603677 ) ) ;
#60648 = DIRECTION ( 'NONE',  ( 1.000000000000000000, 0.000000000000000000, 0.000000000000000000 ) ) ;
#60650 = EDGE_CURVE ( 'NONE', #128947, #231343, #154616, .T. ) ;
#60649 = CARTESIAN_POINT ( 'NONE',  ( -20.54999999999999716, 81.86853375790846599, -214.9828603846715964 ) ) ;
#60651 = EDGE_CURVE ( 'NONE', #10718, #209659, #197553, .T. ) ;
#60652 = DIRECTION ( 'NONE',  ( 0.000000000000000000, -0.1495327102803283015, -0.9887567792719397231 ) ) ;
#60653 = ORIENTED_EDGE ( 'NONE', *, *, #70480, .T. ) ;
#60654 = ORIENTED_EDGE ( 'NONE', *, *, #108537, .T. ) ;
#60655 =( LENGTH_UNIT ( ) NAMED_UNIT ( * ) SI_UNIT ( .MILLI., .METRE. ) );
#60656 = AXIS2_PLACEMENT_3D ( 'NONE', #50784, #69109, #32572 ) ;
#60657 = EDGE_CURVE ( 'NONE', #173700, #219131, #17476, .T. ) ;
#60658 = ORIENTED_EDGE ( 'NONE', *, *, #162057, .F. ) ;
#60659 = FACE_OUTER_BOUND ( 'NONE', #172580, .T. ) ;
#60660 = CARTESIAN_POINT ( 'NONE',  ( 18.50000972452444969, 68.00519115550227411, -224.2294631537214400 ) ) ;
#60661 = AXIS2_PLACEMENT_3D ( 'NONE', #49018, #227650, #106403 ) ;
#60662 = CIRCLE ( 'NONE', #143882, 0.1000000000000118433 ) ;
#60663 = CARTESIAN_POINT ( 'NONE',  ( -13.88555196119803625, 66.54256847116265305, -54.52319054662474684 ) ) ;
#60664 = CARTESIAN_POINT ( 'NONE',  ( -21.53699400386206264, -1.444431824880774817, -194.3677569336538227 ) ) ;
#60665 = VERTEX_POINT ( 'NONE', #76309 ) ;
#60666 = DIRECTION ( 'NONE',  ( 0.000000000000000000, 0.000000000000000000, 1.000000000000000000 ) ) ;
#60667 = ORIENTED_EDGE ( 'NONE', *, *, #194691, .T. ) ;
#60668 = EDGE_CURVE ( 'NONE', #195790, #167847, #221466, .T. ) ;
#60669 = CARTESIAN_POINT ( 'NONE',  ( 18.49999999999998934, 63.79085327820362039, -209.3815830819285395 ) ) ;
#60670 = VERTEX_POINT ( 'NONE', #98411 ) ;
#60671 = CARTESIAN_POINT ( 'NONE',  ( -20.94999999999999929, 69.29912324054878070, -228.2305608266744343 ) ) ;
#60672 = ADVANCED_FACE ( 'NONE', ( #251094 ), #54187, .T. ) ;
#60673 = ORIENTED_EDGE ( 'NONE', *, *, #64320, .F. ) ;
#60674 = CARTESIAN_POINT ( 'NONE',  ( -18.50000000000000000, -1.835341550213255957, -145.5551512925629822 ) ) ;
#60676 = ORIENTED_EDGE ( 'NONE', *, *, #225405, .T. ) ;
#60675 = CARTESIAN_POINT ( 'NONE',  ( -21.22070241538126112, 6.469946272880768845, -100.4010809694650135 ) ) ;
#60677 = B_SPLINE_CURVE_WITH_KNOTS ( 'NONE', 3,
 ( #235012, #73395, #135878, #237578, #17255, #75936, #212881, #118925 ),
 .UNSPECIFIED., .F., .F.,
 ( 4, 2, 2, 4 ),
 ( 0.000000000000000000, 0.0001306511400391344700, 0.0001959767100587032906, 0.0002613022800782720842 ),
 .UNSPECIFIED. ) ;
#60678 = CYLINDRICAL_SURFACE ( 'NONE', #68980, 0.1000000000000021844 ) ;
#60680 = ORIENTED_EDGE ( 'NONE', *, *, #174256, .F. ) ;
#60679 = AXIS2_PLACEMENT_3D ( 'NONE', #116847, #38596, #257575 ) ;
#60681 = STYLED_ITEM ( 'NONE', ( #73955 ), #132074 ) ;
#60682 = AXIS2_PLACEMENT_3D ( 'NONE', #175830, #213655, #97518 ) ;
#60683 = CARTESIAN_POINT ( 'NONE',  ( 18.59999999999999432, 1.736257131608553550, -179.0686523290174819 ) ) ;
#60684 = VERTEX_POINT ( 'NONE', #20220 ) ;
#60685 = VECTOR ( 'NONE', #156869, 1000.000000000000000 ) ;
#60686 = CARTESIAN_POINT ( 'NONE',  ( 18.59999999999999432, -1.736257131586239844, -112.0686523290175245 ) ) ;
#60687 = CARTESIAN_POINT ( 'NONE',  ( 19.83283456528358002, 64.25000000001250555, -178.6731074851066694 ) ) ;
#60688 = DIRECTION ( 'NONE',  ( 0.000000000000000000, 0.8814952561688439436, -0.4721928772777328476 ) ) ;
#60689 = CARTESIAN_POINT ( 'NONE',  ( -37.88850191057539973, -11.65000000000000036, 29.89999999999999858 ) ) ;
#60690 = AXIS2_PLACEMENT_3D ( 'NONE', #43021, #83387, #120016 ) ;
#60691 = VECTOR ( 'NONE', #48461, 1000.000000000000000 ) ;
#60692 = CIRCLE ( 'NONE', #43961, 0.1000000000000013933 ) ;
#60693 = CARTESIAN_POINT ( 'NONE',  ( 23.24999999999999645, -2.099999999988846344, -67.00000000000000000 ) ) ;
#60694 = ORIENTED_EDGE ( 'NONE', *, *, #62228, .F. ) ;
#60695 = CARTESIAN_POINT ( 'NONE',  ( -20.54999999999999716, 7.150000000011155876, -150.7500000000000284 ) ) ;
#60696 = CARTESIAN_POINT ( 'NONE',  ( 21.05000000000000071, 6.540656951712399803, -100.6000000000000512 ) ) ;
#60697 = DIRECTION ( 'NONE',  ( 0.000000000000000000, -0.1298341882520079038, -0.9915357197604846018 ) ) ;
#60698 = ORIENTED_EDGE ( 'NONE', *, *, #119766, .F. ) ;
#60699 = CARTESIAN_POINT ( 'NONE',  ( -21.05000000000000071, 75.96824164695651405, -109.2819546076052859 ) ) ;
#60700 = ORIENTED_EDGE ( 'NONE', *, *, #208004, .T. ) ;
#60701 = CARTESIAN_POINT ( 'NONE',  ( -20.54999999999999716, 74.00000000001156764, -56.29848556176223440 ) ) ;
#60702 = VERTEX_POINT ( 'NONE', #63172 ) ;
#60703 = AXIS2_PLACEMENT_3D ( 'NONE', #231065, #131939, #206353 ) ;
#60704 = AXIS2_PLACEMENT_3D ( 'NONE', #12825, #126652, #223172 ) ;
#60705 = CARTESIAN_POINT ( 'NONE',  ( -21.22070241538126112, 69.53005372714306986, -203.6220265150594173 ) ) ;
#60706 = CARTESIAN_POINT ( 'NONE',  ( -17.29838795457914102, 65.62845014207091765, -181.4183662019063377 ) ) ;
#60707 = ORIENTED_EDGE ( 'NONE', *, *, #4202, .T. ) ;
#60709 = EDGE_LOOP ( 'NONE', ( #186526, #17166, #126831, #137980 ) ) ;
#60708 = DIRECTION ( 'NONE',  ( -0.000000000000000000, -0.000000000000000000, -1.000000000000000000 ) ) ;
#60710 = CARTESIAN_POINT ( 'NONE',  ( -18.49346865148304886, 9.003597566524152995, -245.4495245630940587 ) ) ;
#60711 = ORIENTED_EDGE ( 'NONE', *, *, #170199, .T. ) ;
#60712 = CIRCLE ( 'NONE', #185639, 0.09999999999998898659 ) ;
#60713 = AXIS2_PLACEMENT_3D ( 'NONE', #184464, #89217, #127071 ) ;
#60714 = CARTESIAN_POINT ( 'NONE',  ( -21.65000000000000213, 66.05000000001187743, -90.27310748452438816 ) ) ;
#60715 = DIRECTION ( 'NONE',  ( 0.000000000000000000, 0.5859227990963362664, 0.8103668758649469339 ) ) ;
#60716 = ORIENTED_EDGE ( 'NONE', *, *, #60783, .F. ) ;
#60717 = ORIENTED_EDGE ( 'NONE', *, *, #61188, .F. ) ;
#60718 = CARTESIAN_POINT ( 'NONE',  ( -33.72168855820452649, 23.65833333334447985, -117.2500000000000284 ) ) ;
#60720 = ADVANCED_FACE ( 'NONE', ( #138828 ), #237959, .T. ) ;
#60719 = LINE ( 'NONE', #732, #115128 ) ;
#60721 = ORIENTED_EDGE ( 'NONE', *, *, #128761, .T. ) ;
#60722 = DIRECTION ( 'NONE',  ( 1.000000000000000000, 0.000000000000000000, 0.000000000000000000 ) ) ;
#60723 = VERTEX_POINT ( 'NONE', #60602 ) ;
#60724 = ORIENTED_EDGE ( 'NONE', *, *, #96091, .T. ) ;
#60725 = DIRECTION ( 'NONE',  ( -2.978066053179067751E-16, 1.000000000000000000, 0.000000000000000000 ) ) ;
#60726 = EDGE_CURVE ( 'NONE', #214744, #64899, #141434, .T. ) ;
#60728 = ORIENTED_EDGE ( 'NONE', *, *, #98240, .T. ) ;
#60727 = FACE_BOUND ( 'NONE', #240556, .T. ) ;
#60729 = AXIS2_PLACEMENT_3D ( 'NONE', #20619, #199249, #58410 ) ;
#60730 = ADVANCED_FACE ( 'NONE', ( #200136 ), #64482, .F. ) ;
#60731 = DIRECTION ( 'NONE',  ( 0.000000000000000000, 0.2128009952263603677, -0.9770955615653313941 ) ) ;
#60732 = ADVANCED_FACE ( 'NONE', ( #61906 ), #82711, .T. ) ;
#60733 = DIRECTION ( 'NONE',  ( 0.000000000000000000, -6.982962677686266711E-15, 1.000000000000000000 ) ) ;
#60734 = AXIS2_PLACEMENT_3D ( 'NONE', #79919, #115233, #236464 ) ;
#60735 = CARTESIAN_POINT ( 'NONE',  ( -18.59999999999999787, 1.115600667400684642E-11, -100.5000000000000284 ) ) ;
#60737 = CARTESIAN_POINT ( 'NONE',  ( -23.15000000000000213, 76.00000000001243450, -168.0231074845243597 ) ) ;
#60736 = CYLINDRICAL_SURFACE ( 'NONE', #152670, 0.1000000000000028644 ) ;
#60739 = AXIS2_PLACEMENT_3D ( 'NONE', #44110, #141914, #3688 ) ;
#60738 = DIRECTION ( 'NONE',  ( -1.000000000000000000, 0.000000000000000000, 0.000000000000000000 ) ) ;
#60740 = VECTOR ( 'NONE', #46252, 1000.000000000000114 ) ;
#60741 = DIRECTION ( 'NONE',  ( -1.000000000000000000, 7.304098846218134667E-16, 4.217023435051625732E-16 ) ) ;
#60742 = CYLINDRICAL_SURFACE ( 'NONE', #184977, 1.749999999999998002 ) ;
#60744 = ORIENTED_EDGE ( 'NONE', *, *, #132711, .T. ) ;
#60743 = AXIS2_PLACEMENT_3D ( 'NONE', #102709, #105265, #205675 ) ;
#60745 = B_SPLINE_CURVE_WITH_KNOTS ( 'NONE', 3,
 ( #153152, #193533, #172723, #113970, #194831, #176545, #14902 ),
 .UNSPECIFIED., .F., .F.,
 ( 4, 3, 4 ),
 ( 0.000000000000000000, 1.860045280644813734E-05, 5.251155757305090734E-05 ),
 .UNSPECIFIED. ) ;
#60746 = ORIENTED_EDGE ( 'NONE', *, *, #126864, .F. ) ;
#60747 = ORIENTED_EDGE ( 'NONE', *, *, #23159, .T. ) ;
#60748 = ADVANCED_FACE ( 'NONE', ( #222232 ), #43633, .T. ) ;
#60749 = CARTESIAN_POINT ( 'NONE',  ( -20.94999999999999929, 76.00000000001188027, -98.92310748452429436 ) ) ;
#60750 =( BOUNDED_SURFACE ( )  B_SPLINE_SURFACE ( 3, 2, ( 
 ( #106625, #164071, #166663 ),
 ( #246166, #123660, #147046 ),
 ( #187496, #226582, #127503 ),
 ( #8840, #247443, #109205 ),
 ( #128796, #64948, #208345 ),
 ( #29717, #188751, #144471 ) ),
 .UNSPECIFIED., .F., .F., .F. ) 
 B_SPLINE_SURFACE_WITH_KNOTS ( ( 4, 2, 4 ),
 ( 3, 3 ),
 ( 1.570796326794895448, 2.356194490192343505, 3.141592653589791784 ),
 ( 0.000000000000000000, 1.000000000000000000 ),
 .UNSPECIFIED. ) 
 GEOMETRIC_REPRESENTATION_ITEM ( )  RATIONAL_B_SPLINE_SURFACE ( (
 ( 1.000000000000000000, 0.7071067811865475727, 1.000000000000000000),
 ( 1.000000000000000000, 0.6611148371771847776, 1.000000000000000000),
 ( 1.000000000000000000, 0.6092287576706065799, 1.000000000000000000),
 ( 1.000000000000000000, 0.5278258667047666108, 1.000000000000000000),
 ( 1.000000000000000000, 0.4993418825338903910, 1.000000000000000000),
 ( 1.000000000000000000, 0.5000000000000048850, 1.000000000000000000) ) ) 
 REPRESENTATION_ITEM ( '' )  SURFACE ( )  );
#60751 = ORIENTED_EDGE ( 'NONE', *, *, #190956, .F. ) ;
#60752 = CARTESIAN_POINT ( 'NONE',  ( -23.39999999999994529, 76.00000000001119815, -31.97310748452479601 ) ) ;
#60753 = CIRCLE ( 'NONE', #85676, 0.09999999999999864553 ) ;
#60754 = CARTESIAN_POINT ( 'NONE',  ( -11.59999999999994458, 67.72071067812984779, -21.02310748452479316 ) ) ;
#60755 = CIRCLE ( 'NONE', #189780, 0.1000000000000028644 ) ;
#60756 = ORIENTED_EDGE ( 'NONE', *, *, #62914, .F. ) ;
#60757 = AXIS2_PLACEMENT_3D ( 'NONE', #38757, #43564, #123110 ) ;
#60758 =( NAMED_UNIT ( * ) PLANE_ANGLE_UNIT ( ) SI_UNIT ( $, .RADIAN. ) );
#60759 = DIRECTION ( 'NONE',  ( 0.000000000000000000, 0.000000000000000000, -1.000000000000000000 ) ) ;
#60761 = ORIENTED_EDGE ( 'NONE', *, *, #82603, .T. ) ;
#60760 = VERTEX_POINT ( 'NONE', #240544 ) ;
#60762 = EDGE_LOOP ( 'NONE', ( #38674, #30627, #106624, #222702 ) ) ;
#60763 = ORIENTED_EDGE ( 'NONE', *, *, #39591, .T. ) ;
#60764 = DIRECTION ( 'NONE',  ( -1.000000000000000000, 3.265361837132813093E-16, 2.280189983783949500E-30 ) ) ;
#60765 = CARTESIAN_POINT ( 'NONE',  ( -18.50000000000000000, 66.65000000001259650, -191.1731074845244223 ) ) ;
#60767 = VERTEX_POINT ( 'NONE', #121894 ) ;
#60766 = DIRECTION ( 'NONE',  ( -0.5932847527679310229, 0.8049926720990042694, -6.366092712777067056E-16 ) ) ;
#60768 = EDGE_CURVE ( 'NONE', #69456, #253194, #119314, .T. ) ;
#60769 = EDGE_CURVE ( 'NONE', #42519, #189870, #238236, .T. ) ;
#60770 = AXIS2_PLACEMENT_3D ( 'NONE', #181028, #81871, #20675 ) ;
#60771 = CARTESIAN_POINT ( 'NONE',  ( 20.87631937322886344, 39.29512351867782627, -236.8959183278824412 ) ) ;
#60772 = FACE_OUTER_BOUND ( 'NONE', #137266, .T. ) ;
#60774 = ORIENTED_EDGE ( 'NONE', *, *, #99353, .F. ) ;
#60773 = DIRECTION ( 'NONE',  ( 1.000000000000000000, 0.000000000000000000, 0.000000000000000000 ) ) ;
#60775 = FACE_OUTER_BOUND ( 'NONE', #73480, .T. ) ;
#60776 = ORIENTED_EDGE ( 'NONE', *, *, #6505, .T. ) ;
#60777 = DIRECTION ( 'NONE',  ( 0.000000000000000000, -0.9553114395363172529, -0.2956011730204217702 ) ) ;
#60779 = ORIENTED_EDGE ( 'NONE', *, *, #100979, .F. ) ;
#60778 = FACE_OUTER_BOUND ( 'NONE', #95441, .T. ) ;
#60780 = DIRECTION ( 'NONE',  ( 0.000000000000000000, -1.000000000000000000, 0.000000000000000000 ) ) ;
#60781 = CARTESIAN_POINT ( 'NONE',  ( -13.11924609551136278, 27.69551741609592810, -234.0500622709108143 ) ) ;
#60783 = EDGE_CURVE ( 'NONE', #75696, #208239, #80139, .T. ) ;
#60782 = CYLINDRICAL_SURFACE ( 'NONE', #60942, 0.1000000000000028644 ) ;
#60784 = ORIENTED_EDGE ( 'NONE', *, *, #255155, .F. ) ;
#60786 = CARTESIAN_POINT ( 'NONE',  ( 18.49999999999999289, 54.53338637621133955, -228.6684279704127789 ) ) ;
#60785 = DIRECTION ( 'NONE',  ( 0.000000000000000000, -7.429790795770644761E-15, 1.000000000000000000 ) ) ;
#60787 = CARTESIAN_POINT ( 'NONE',  ( -12.26136940704872025, 66.64859682587017176, -86.04357704768588633 ) ) ;
#60788 = DIRECTION ( 'NONE',  ( -1.000000000000000000, 0.000000000000000000, 0.000000000000000000 ) ) ;
#60789 = CIRCLE ( 'NONE', #206558, 0.5000000000000008882 ) ;
#60790 = DIRECTION ( 'NONE',  ( 0.000000000000000000, 1.897661533703519897E-16, -1.000000000000000000 ) ) ;
#60791 = VECTOR ( 'NONE', #162012, 1000.000000000000000 ) ;
#60793 = CARTESIAN_POINT ( 'NONE',  ( 22.39999999999999503, 0.1000000000111554016, -59.20922040162665922 ) ) ;
#60792 = AXIS2_PLACEMENT_3D ( 'NONE', #74319, #91288, #70473 ) ;
#60794 = ORIENTED_EDGE ( 'NONE', *, *, #176332, .F. ) ;
#60795 = EDGE_LOOP ( 'NONE', ( #115103, #109166, #190071, #138093 ) ) ;
#60796 = EDGE_LOOP ( 'NONE', ( #69292, #240156, #195503, #242403 ) ) ;
#60797 = CARTESIAN_POINT ( 'NONE',  ( -21.04999999999999716, 1.115177828553415134E-11, -127.4593430482987912 ) ) ;
#60798 = EDGE_LOOP ( 'NONE', ( #242246, #127804, #247245, #83292 ) ) ;
#60799 = CARTESIAN_POINT ( 'NONE',  ( -23.25000000000000000, -1.249999999988843369, -208.8004807544150481 ) ) ;
#60800 = ORIENTED_EDGE ( 'NONE', *, *, #139801, .F. ) ;
#60801 = DIRECTION ( 'NONE',  ( -1.000000000000000000, 0.000000000000000000, -0.000000000000000000 ) ) ;
#60802 = DIRECTION ( 'NONE',  ( -1.000000000000000000, -0.000000000000000000, -0.000000000000000000 ) ) ;
#60803 = ORIENTED_EDGE ( 'NONE', *, *, #238619, .T. ) ;
#60804 = AXIS2_PLACEMENT_3D ( 'NONE', #195882, #116340, #177615 ) ;
#60805 = DIRECTION ( 'NONE',  ( -0.5932847527679299127, -0.8049926720990051576, -6.257843056355997642E-15 ) ) ;
#60806 = CIRCLE ( 'NONE', #127655, 0.1000000000000028644 ) ;
#60807 = ORIENTED_EDGE ( 'NONE', *, *, #34730, .T. ) ;
#60808 = ORIENTED_EDGE ( 'NONE', *, *, #119706, .T. ) ;
#60809 = ORIENTED_EDGE ( 'NONE', *, *, #115866, .F. ) ;
#60810 = EDGE_CURVE ( 'NONE', #165845, #84743, #99714, .T. ) ;
#60811 = CARTESIAN_POINT ( 'NONE',  ( 5.899999999999995914, -11.34999999999999964, 10.10000000000000142 ) ) ;
#60812 = VECTOR ( 'NONE', #110317, 1000.000000000000000 ) ;
#60813 = CARTESIAN_POINT ( 'NONE',  ( -16.93658623642902583, 66.01961832835444000, -56.91120475539518964 ) ) ;
#60814 = EDGE_CURVE ( 'NONE', #70041, #136156, #201405, .T. ) ;
#60815 = DIRECTION ( 'NONE',  ( -0.000000000000000000, 0.9876197685951279004, -0.1568667991644694115 ) ) ;
#60816 = FACE_OUTER_BOUND ( 'NONE', #248941, .T. ) ;
#60817 = DIRECTION ( 'NONE',  ( 0.000000000000000000, 0.000000000000000000, -1.000000000000000000 ) ) ;
#60819 = CARTESIAN_POINT ( 'NONE',  ( -0.8999999999999437339, 66.35000000001119247, -10.02310748452479139 ) ) ;
#60818 = CARTESIAN_POINT ( 'NONE',  ( 23.24999999999999289, 63.99342642423710714, -222.3880800784493772 ) ) ;
#60820 = CARTESIAN_POINT ( 'NONE',  ( -21.44999999999999929, 7.350000000011155166, -179.8499999999999943 ) ) ;
#60822 = ORIENTED_EDGE ( 'NONE', *, *, #95880, .F. ) ;
#60821 = DIRECTION ( 'NONE',  ( 2.710505431213777355E-16, 1.000000000000000000, 6.982962677686266711E-15 ) ) ;
#60823 = CARTESIAN_POINT ( 'NONE',  ( -20.05000000000000426, 11.66622623553636018, -211.0987209794895421 ) ) ;
#60824 = EDGE_CURVE ( 'NONE', #166449, #48752, #84062, .T. ) ;
#60825 = CARTESIAN_POINT ( 'NONE',  ( -18.49719636458551975, -9.446365359216901680, -141.0716138698831230 ) ) ;
#60826 = EDGE_CURVE ( 'NONE', #91499, #245021, #229872, .T. ) ;
#60827 = ORIENTED_EDGE ( 'NONE', *, *, #61764, .T. ) ;
#60828 = ORIENTED_EDGE ( 'NONE', *, *, #9915, .T. ) ;
#60829 = DIRECTION ( 'NONE',  ( -1.000000000000000000, -0.000000000000000000, -0.000000000000000000 ) ) ;
#60830 = CARTESIAN_POINT ( 'NONE',  ( -21.05000000000000071, 14.05000000001115623, -173.0136950707609458 ) ) ;
#60831 = PLANE ( 'NONE',  #187836 ) ;
#60832 = ORIENTED_EDGE ( 'NONE', *, *, #120799, .T. ) ;
#60833 = EDGE_CURVE ( 'NONE', #17038, #109261, #171638, .T. ) ;
#60834 = EDGE_CURVE ( 'NONE', #101319, #2330, #163581, .T. ) ;
#60835 = VECTOR ( 'NONE', #39305, 1000.000000000000000 ) ;
#60836 = PLANE ( 'NONE',  #196722 ) ;
#60838 = EDGE_CURVE ( 'NONE', #175143, #8211, #150756, .T. ) ;
#60837 = EDGE_CURVE ( 'NONE', #160000, #44809, #180004, .T. ) ;
#60839 = ORIENTED_EDGE ( 'NONE', *, *, #103498, .F. ) ;
#60840 = EDGE_LOOP ( 'NONE', ( #239616, #9174, #196807, #47511, #85051, #103626 ) ) ;
#60841 = CARTESIAN_POINT ( 'NONE',  ( -23.15000000000000213, 84.66355140188123585, -126.9990063664569391 ) ) ;
#60842 = ORIENTED_EDGE ( 'NONE', *, *, #137452, .F. ) ;
#60843 = CARTESIAN_POINT ( 'NONE',  ( -23.25000000000000000, 6.878457983866232972, -212.1414458560986986 ) ) ;
#60844 = FACE_OUTER_BOUND ( 'NONE', #200029, .T. ) ;
#60845 = FACE_OUTER_BOUND ( 'NONE', #175638, .T. ) ;
#60846 = EDGE_CURVE ( 'NONE', #16570, #14025, #134176, .T. ) ;
#60847 = SPHERICAL_SURFACE ( 'NONE', #244792, 0.1000000000000000056 ) ;
#60848 = DIRECTION ( 'NONE',  ( 0.000000000000000000, -0.8814952561688476074, 0.4721928772777262417 ) ) ;
#60849 = VERTEX_POINT ( 'NONE', #150452 ) ;
#60850 = CARTESIAN_POINT ( 'NONE',  ( 21.05000000000000071, 12.10919762232931163, -206.2073353557311748 ) ) ;
#60851 = EDGE_CURVE ( 'NONE', #139023, #69456, #167535, .T. ) ;
#60852 = CARTESIAN_POINT ( 'NONE',  ( -20.54999999999999716, 2.500000000011154633, -187.7753780772378889 ) ) ;
#60853 = VECTOR ( 'NONE', #271, 1000.000000000000000 ) ;
#60854 = DIRECTION ( 'NONE',  ( 1.000000000000000000, 0.000000000000000000, 0.000000000000000000 ) ) ;
#60855 = EDGE_CURVE ( 'NONE', #31598, #82492, #104921, .T. ) ;
#60856 = ADVANCED_FACE ( 'NONE', ( #130862 ), #149171, .F. ) ;
#60857 = AXIS2_PLACEMENT_3D ( 'NONE', #61870, #100933, #141391 ) ;
#60858 = CIRCLE ( 'NONE', #239951, 0.09999999999999992228 ) ;
#60859 = ORIENTED_EDGE ( 'NONE', *, *, #113628, .T. ) ;
#60860 =( BOUNDED_SURFACE ( )  B_SPLINE_SURFACE ( 3, 2, ( 
 ( #92580, #229553, #31382 ),
 ( #11806, #113442, #173479 ),
 ( #131723, #133021, #32671 ),
 ( #212561, #192992, #14374 ) ),
 .UNSPECIFIED., .F., .F., .F. ) 
 B_SPLINE_SURFACE_WITH_KNOTS ( ( 4, 4 ),
 ( 3, 3 ),
 ( 0.04058434257139457990, 0.04256401539001584966 ),
 ( 0.000000000000000000, 1.000000000000000000 ),
 .UNSPECIFIED. ) 
 GEOMETRIC_REPRESENTATION_ITEM ( )  RATIONAL_B_SPLINE_SURFACE ( (
 ( 1.000000000000000000, 0.7103081912008052390, 1.000000000000000000),
 ( 1.000000000000000000, 0.7104998333555472279, 1.000000000000000000),
 ( 1.000000000000000000, 0.7107238315755474156, 1.000000000000000000),
 ( 1.000000000000000000, 0.7110073749539291832, 1.000000000000000000) ) ) 
 REPRESENTATION_ITEM ( '' )  SURFACE ( )  );
#60861 = EDGE_CURVE ( 'NONE', #22560, #171424, #188270, .T. ) ;
#60863 = VERTEX_POINT ( 'NONE', #70927 ) ;
#60862 = CARTESIAN_POINT ( 'NONE',  ( 18.50000000000000000, -9.399999999988843058, -141.2972597596633193 ) ) ;
#60864 = SPHERICAL_SURFACE ( 'NONE', #55842, 0.1000000000000000056 ) ;
#60865 = DIRECTION ( 'NONE',  ( 0.000000000000000000, 2.891205793294679805E-16, -1.000000000000000000 ) ) ;
#60866 = CARTESIAN_POINT ( 'NONE',  ( -21.64999999999999858, 53.04688186230822566, -234.1557136682916394 ) ) ;
#60867 = DIRECTION ( 'NONE',  ( -1.000000000000000000, -0.000000000000000000, -0.000000000000000000 ) ) ;
#60868 = EDGE_CURVE ( 'NONE', #206012, #19219, #67046, .T. ) ;
#60869 = CARTESIAN_POINT ( 'NONE',  ( -22.50000000000000000, 75.90000000001202807, -114.6726782920691221 ) ) ;
#60870 = LINE ( 'NONE', #101236, #161376 ) ;
#60871 = VERTEX_POINT ( 'NONE', #128313 ) ;
#60872 = FACE_OUTER_BOUND ( 'NONE', #89268, .T. ) ;
#60873 = CARTESIAN_POINT ( 'NONE',  ( -23.25000000000000000, -1.835859311432481045, -112.0044391687985694 ) ) ;
#60875 = EDGE_CURVE ( 'NONE', #219752, #69817, #250705, .T. ) ;
#60874 = CARTESIAN_POINT ( 'NONE',  ( -18.40904629823850769, 77.13860739149254186, -241.8264963902813065 ) ) ;
#60876 = DIRECTION ( 'NONE',  ( 1.186688945009010077E-16, -1.000000000000000000, -0.000000000000000000 ) ) ;
#60877 = AXIS2_PLACEMENT_3D ( 'NONE', #99648, #35878, #18855 ) ;
#60878 = CARTESIAN_POINT ( 'NONE',  ( 20.22483756094572271, 66.49809532113982868, -61.38356835580996318 ) ) ;
#60879 = TOROIDAL_SURFACE ( 'NONE', #73396, 4.099999999999999645, 0.1000000000000000056 ) ;
#60880 = ORIENTED_EDGE ( 'NONE', *, *, #94085, .F. ) ;
#60881 = ORIENTED_EDGE ( 'NONE', *, *, #9320, .F. ) ;
#60882 = DIRECTION ( 'NONE',  ( 0.000000000000000000, 0.000000000000000000, -1.000000000000000000 ) ) ;
#60883 = CARTESIAN_POINT ( 'NONE',  ( -20.94999999999999929, 80.82257920297074349, -192.8058055878823609 ) ) ;
#60884 = CARTESIAN_POINT ( 'NONE',  ( 23.24999999999999289, 70.05000000001221849, -146.8288097895591875 ) ) ;
#60885 = DIRECTION ( 'NONE',  ( -1.000000000000000000, 2.952720810173289112E-16, 2.061873921506763405E-30 ) ) ;
#60886 = CIRCLE ( 'NONE', #198267, 0.09999999999999939493 ) ;
#60887 = EDGE_CURVE ( 'NONE', #167022, #200406, #55055, .T. ) ;
#60888 = VERTEX_POINT ( 'NONE', #205249 ) ;
#60889 = CARTESIAN_POINT ( 'NONE',  ( -18.47653818581419571, 47.03188537331093499, -255.2758925175261311 ) ) ;
#60890 = AXIS2_PLACEMENT_3D ( 'NONE', #239623, #63529, #120980 ) ;
#60891 = AXIS2_PLACEMENT_3D ( 'NONE', #1417, #80951, #61407 ) ;
#60892 = DIRECTION ( 'NONE',  ( 0.000000000000000000, 0.4088369013363281623, -0.9126074666063771490 ) ) ;
#60893 = CARTESIAN_POINT ( 'NONE',  ( -20.54999999999999716, 76.00000000001170974, -69.52310748452431710 ) ) ;
#60894 = CARTESIAN_POINT ( 'NONE',  ( -18.59999999999999787, 22.33586458086958615, -231.4986017528744071 ) ) ;
#60895 = AXIS2_PLACEMENT_3D ( 'NONE', #34494, #71050, #132278 ) ;
#60896 = CIRCLE ( 'NONE', #144264, 0.1999999999999987899 ) ;
#60897 = VERTEX_POINT ( 'NONE', #228702 ) ;
#60899 = LINE ( 'NONE', #163869, #131833 ) ;
#60898 = VECTOR ( 'NONE', #90727, 1000.000000000000000 ) ;
#60900 = VERTEX_POINT ( 'NONE', #90441 ) ;
#60901 = CARTESIAN_POINT ( 'NONE',  ( -21.04999999999999716, 75.90156250001170690, -75.82233839461120795 ) ) ;
#60902 = CARTESIAN_POINT ( 'NONE',  ( 23.14999999999999503, 64.35000000001195986, -110.0379132551783243 ) ) ;
#60903 = FACE_BOUND ( 'NONE', #38401, .T. ) ;
#60904 = AXIS2_PLACEMENT_3D ( 'NONE', #183255, #224925, #207972 ) ;
#60905 = FACE_OUTER_BOUND ( 'NONE', #10920, .T. ) ;
#60906 = DIRECTION ( 'NONE',  ( -1.000000000000000000, -0.000000000000000000, -0.000000000000000000 ) ) ;
#60907 = DIRECTION ( 'NONE',  ( 1.000000000000000000, 0.000000000000000000, 0.000000000000000000 ) ) ;
#60908 = DIRECTION ( 'NONE',  ( -0.000000000000000000, 0.2128009952263603677, -0.9770955615653313941 ) ) ;
#60909 = CARTESIAN_POINT ( 'NONE',  ( 20.94999999999999929, 8.876614585098254295, -75.38508047884472774 ) ) ;
#60910 = ADVANCED_FACE ( 'NONE', ( #170045 ), #46690, .T. ) ;
#60911 = CARTESIAN_POINT ( 'NONE',  ( -21.05000000000000071, 76.00000000001195133, -103.0231074845243171 ) ) ;
#60912 = DIRECTION ( 'NONE',  ( 0.000000000000000000, 6.982962677686266711E-15, -1.000000000000000000 ) ) ;
#60913 = AXIS2_PLACEMENT_3D ( 'NONE', #177530, #116248, #157972 ) ;
#60914 = DIRECTION ( 'NONE',  ( 1.000000000000000000, 0.000000000000000000, -0.000000000000000000 ) ) ;
#60915 = ADVANCED_FACE ( 'NONE', ( #224817 ), #26654, .T. ) ;
#60916 = CARTESIAN_POINT ( 'NONE',  ( 23.24999999999999289, 11.65000000001116298, -88.35000000000003695 ) ) ;
#60917 = CARTESIAN_POINT ( 'NONE',  ( 21.02374657821576065, 56.16603649953788135, -228.1013850333971220 ) ) ;
#60918 = ORIENTED_EDGE ( 'NONE', *, *, #28805, .F. ) ;
#60919 = FACE_OUTER_BOUND ( 'NONE', #95560, .T. ) ;
#60921 = ADVANCED_FACE ( 'NONE', ( #106147 ), #8364, .F. ) ;
#60920 = CARTESIAN_POINT ( 'NONE',  ( -21.64999999999999858, 65.95000000001262208, -190.8731074845244393 ) ) ;
#60922 = DIRECTION ( 'NONE',  ( 1.000000000000000000, 0.000000000000000000, 0.000000000000000000 ) ) ;
#60923 = ADVANCED_FACE ( 'NONE', ( #85289 ), #88372, .T. ) ;
#60924 = ORIENTED_EDGE ( 'NONE', *, *, #226458, .F. ) ;
#60925 = CARTESIAN_POINT ( 'NONE',  ( -23.15000000000000213, -9.000000000000001776, -23.60603087734756045 ) ) ;
#60926 = AXIS2_PLACEMENT_3D ( 'NONE', #234182, #34741, #218464 ) ;
#60927 = EDGE_CURVE ( 'NONE', #107540, #74720, #129591, .T. ) ;
#60928 = VECTOR ( 'NONE', #122513, 1000.000000000000000 ) ;
#60929 = DIRECTION ( 'NONE',  ( 0.000000000000000000, 0.000000000000000000, -1.000000000000000000 ) ) ;
#60930 = ORIENTED_EDGE ( 'NONE', *, *, #222592, .T. ) ;
#60932 = AXIS2_PLACEMENT_3D ( 'NONE', #203194, #122383, #199365 ) ;
#60931 = DIRECTION ( 'NONE',  ( -0.000000000000000000, 0.5407049257165768008, -0.8412123295017919222 ) ) ;
#60933 = PLANE ( 'NONE',  #130867 ) ;
#60934 = AXIS2_PLACEMENT_3D ( 'NONE', #64243, #216882, #117792 ) ;
#60935 = ORIENTED_EDGE ( 'NONE', *, *, #24993, .T. ) ;
#60936 = AXIS2_PLACEMENT_3D ( 'NONE', #254435, #155401, #234911 ) ;
#60937 = ADVANCED_FACE ( 'NONE', ( #185711 ), #227394, .T. ) ;
#60938 = ORIENTED_EDGE ( 'NONE', *, *, #142725, .T. ) ;
#60939 = DIRECTION ( 'NONE',  ( 0.000000000000000000, 0.000000000000000000, 1.000000000000000000 ) ) ;
#60940 = ORIENTED_EDGE ( 'NONE', *, *, #189861, .F. ) ;
#60942 = AXIS2_PLACEMENT_3D ( 'NONE', #162484, #137748, #3371 ) ;
#60941 = DIRECTION ( 'NONE',  ( -3.265361837132813093E-16, -1.000000000000000000, 7.445645354460596589E-46 ) ) ;
#60943 = FACE_OUTER_BOUND ( 'NONE', #175256, .T. ) ;
#60945 = CARTESIAN_POINT ( 'NONE',  ( -21.64999999999999858, 10.05000000001113847, -46.15000000000000568 ) ) ;
#60944 = PRODUCT_DEFINITION_CONTEXT ( 'detailed design', #197444, 'design' ) ;
#60946 = DIRECTION ( 'NONE',  ( -1.000000000000000000, 0.000000000000000000, 0.000000000000000000 ) ) ;
#60947 = AXIS2_PLACEMENT_3D ( 'NONE', #25321, #164815, #246901 ) ;
#60948 = CARTESIAN_POINT ( 'NONE',  ( -16.89155683852408174, 66.05000000001230376, -156.7457356349848681 ) ) ;
#60949 = DIRECTION ( 'NONE',  ( 0.000000000000000000, 0.8741572761215280485, -0.4856429311786498171 ) ) ;
#60950 = AXIS2_PLACEMENT_3D ( 'NONE', #178953, #78513, #141077 ) ;
#60951 = CARTESIAN_POINT ( 'NONE',  ( -15.55912972643741199, 22.20092727007757460, -232.1740600553843876 ) ) ;
#60952 = CARTESIAN_POINT ( 'NONE',  ( 23.15000000000000213, 82.67551891922275331, -215.5849511313000164 ) ) ;
#60954 = VERTEX_POINT ( 'NONE', #9632 ) ;
#60953 = CARTESIAN_POINT ( 'NONE',  ( -18.43473496883417084, -9.494952410988139135, -40.54587157222824345 ) ) ;
#60955 = ORIENTED_EDGE ( 'NONE', *, *, #46420, .T. ) ;
#60957 = DIRECTION ( 'NONE',  ( -0.000000000000000000, 1.000000000000000000, 0.000000000000000000 ) ) ;
#60956 = CARTESIAN_POINT ( 'NONE',  ( 18.59999999999999076, 38.22825984020919066, -261.1961207961828677 ) ) ;
#60959 = ORIENTED_EDGE ( 'NONE', *, *, #104389, .T. ) ;
#60958 = CARTESIAN_POINT ( 'NONE',  ( 21.00000000000000000, 7.800000000000000711, 1.212568896937007867 ) ) ;
#60960 = ORIENTED_EDGE ( 'NONE', *, *, #233606, .F. ) ;
#60961 = EDGE_CURVE ( 'NONE', #138331, #182833, #42423, .T. ) ;
#60962 = DIRECTION ( 'NONE',  ( -3.265361837132813093E-16, -1.000000000000000000, -6.982962677686266711E-15 ) ) ;
#60963 = CARTESIAN_POINT ( 'NONE',  ( -21.44999999999999929, 68.65000000001253966, -182.2731074845244166 ) ) ;
#60964 = CARTESIAN_POINT ( 'NONE',  ( 23.24999999999999289, 11.65000000001116298, -167.5999999999999659 ) ) ;
#60965 = CARTESIAN_POINT ( 'NONE',  ( 21.05000000000000071, 6.650000000011155876, -112.6500000000000341 ) ) ;
#60967 = CARTESIAN_POINT ( 'NONE',  ( 20.94999999999999574, 87.41227409416205774, -167.1231074845242688 ) ) ;
#60966 = AXIS2_PLACEMENT_3D ( 'NONE', #52735, #111437, #250927 ) ;
#60968 = CARTESIAN_POINT ( 'NONE',  ( -14.00000000000000178, 13.18880795147152440, -215.2702608532411830 ) ) ;
#60970 = EDGE_CURVE ( 'NONE', #6953, #30427, #168769, .T. ) ;
#60969 = CARTESIAN_POINT ( 'NONE',  ( -23.25000000000000000, 6.982009704867601307, -104.1961521182563359 ) ) ;
#60971 = EDGE_CURVE ( 'NONE', #93175, #109469, #109046, .T. ) ;
#60972 = DIRECTION ( 'NONE',  ( 0.000000000000000000, -6.982962677686267499E-15, 1.000000000000000000 ) ) ;
#60973 = ORIENTED_EDGE ( 'NONE', *, *, #248881, .T. ) ;
#60974 = EDGE_LOOP ( 'NONE', ( #85160, #189381, #127104, #255279, #163358, #25826, #26344, #19913, #108439, #145119, #229710, #199222, #242386, #182046, #127061, #83139 ) ) ;
#60975 = FACE_OUTER_BOUND ( 'NONE', #78911, .T. ) ;
#60976 = AXIS2_PLACEMENT_3D ( 'NONE', #191062, #107638, #127212 ) ;
#60977 = VERTEX_POINT ( 'NONE', #214262 ) ;
#60978 = AXIS2_PLACEMENT_3D ( 'NONE', #150944, #248766, #173120 ) ;
#60979 = ORIENTED_EDGE ( 'NONE', *, *, #56567, .F. ) ;
#60980 = CARTESIAN_POINT ( 'NONE',  ( -18.39999999999999858, 40.45536607095846193, -235.2785561097531968 ) ) ;
#60981 = EDGE_CURVE ( 'NONE', #38706, #193905, #175910, .T. ) ;
#60982 = FACE_OUTER_BOUND ( 'NONE', #57215, .T. ) ;
#60983 = DIRECTION ( 'NONE',  ( 1.000000000000000000, 0.000000000000000000, -0.000000000000000000 ) ) ;
#60984 = CARTESIAN_POINT ( 'NONE',  ( 20.95512820512820440, 10.62384868372303615, -146.1500000000000341 ) ) ;
#60985 = ADVANCED_FACE ( 'NONE', ( #137275 ), #237564, .T. ) ;
#60986 = DIRECTION ( 'NONE',  ( 7.304098846218134667E-16, 1.000000000000000000, -0.000000000000000000 ) ) ;
#60987 = ORIENTED_EDGE ( 'NONE', *, *, #110695, .F. ) ;
#60988 = EDGE_CURVE ( 'NONE', #59315, #40380, #115159, .T. ) ;
#60989 = DIRECTION ( 'NONE',  ( 0.000000000000000000, -6.982962677686266711E-15, 1.000000000000000000 ) ) ;
#60990 = ORIENTED_EDGE ( 'NONE', *, *, #10143, .F. ) ;
#60991 = SPHERICAL_SURFACE ( 'NONE', #196528, 0.1000000000000000056 ) ;
#60992 = DIRECTION ( 'NONE',  ( 0.000000000000000000, -6.938893903907222067E-15, 1.000000000000000000 ) ) ;
#60993 = LINE ( 'NONE', #988, #233773 ) ;
#60994 = EDGE_CURVE ( 'NONE', #91127, #200635, #173896, .T. ) ;
#60995 = VECTOR ( 'NONE', #106372, 1000.000000000000000 ) ;
#60996 = DIRECTION ( 'NONE',  ( -1.000000000000000000, 0.000000000000000000, 0.000000000000000000 ) ) ;
#60997 = EDGE_LOOP ( 'NONE', ( #217850, #112664, #222458, #177660 ) ) ;
#60998 = AXIS2_PLACEMENT_3D ( 'NONE', #176008, #196816, #254214 ) ;
#60999 = FACE_OUTER_BOUND ( 'NONE', #62974, .T. ) ;
#61000 = ORIENTED_EDGE ( 'NONE', *, *, #144793, .T. ) ;
#61003 = VERTEX_POINT ( 'NONE', #113872 ) ;
#61002 = CARTESIAN_POINT ( 'NONE',  ( 18.47149038651511077, -9.671457157995551057, -107.1727863347384613 ) ) ;
#61001 = DIRECTION ( 'NONE',  ( 1.000000000000000000, 0.000000000000000000, 0.000000000000000000 ) ) ;
#61004 = CARTESIAN_POINT ( 'NONE',  ( -22.39999999999999858, 0.1000000000111554016, -159.7092204016265384 ) ) ;
#61005 = LINE ( 'NONE', #127413, #146002 ) ;
#61006 = AXIS2_PLACEMENT_3D ( 'NONE', #228057, #246334, #49416 ) ;
#61007 = VERTEX_POINT ( 'NONE', #112598 ) ;
#61008 = CARTESIAN_POINT ( 'NONE',  ( 18.59999996954842771, 85.52320413787039399, -129.6400657726071017 ) ) ;
#61009 = EDGE_CURVE ( 'NONE', #257282, #18100, #192150, .T. ) ;
#61010 = CARTESIAN_POINT ( 'NONE',  ( 23.14999999999999858, 11.65000000001116298, -160.4851942293460922 ) ) ;
#61011 = CARTESIAN_POINT ( 'NONE',  ( 20.90000000000000213, -1.300000000000000044, -7.800000000000000711 ) ) ;
#61013 = VERTEX_POINT ( 'NONE', #93021 ) ;
#61012 = CARTESIAN_POINT ( 'NONE',  ( 21.72449340488910607, 65.71604372252119219, -160.7731074845244166 ) ) ;
#61014 = DIRECTION ( 'NONE',  ( 0.000000000000000000, -0.4721928772777332917, -0.8814952561688437216 ) ) ;
#61015 = VERTEX_POINT ( 'NONE', #250805 ) ;
#61016 = DIRECTION ( 'NONE',  ( 1.000000000000000000, 0.000000000000000000, 0.000000000000000000 ) ) ;
#61017 = CARTESIAN_POINT ( 'NONE',  ( 22.39999999999999858, 59.71212129423884818, -233.8158665866020272 ) ) ;
#61018 = CARTESIAN_POINT ( 'NONE',  ( -20.85000000000000142, 77.16412189325258453, -28.20825939895270551 ) ) ;
#61019 = AXIS2_PLACEMENT_3D ( 'NONE', #178828, #214065, #136 ) ;
#61020 = VERTEX_POINT ( 'NONE', #76026 ) ;
#61021 = CARTESIAN_POINT ( 'NONE',  ( 20.94999999999999574, -10.72348020702289695, -206.5081278352411402 ) ) ;
#61022 = EDGE_LOOP ( 'NONE', ( #255349, #170517, #30678, #69424, #146403 ) ) ;
#61023 = LINE ( 'NONE', #136707, #177071 ) ;
#61024 = DIRECTION ( 'NONE',  ( 0.000000000000000000, 0.000000000000000000, 1.000000000000000000 ) ) ;
#61025 = CARTESIAN_POINT ( 'NONE',  ( 20.94999999999999574, -1.349084418615859482, -141.9864989635455004 ) ) ;
#61026 = VERTEX_POINT ( 'NONE', #252094 ) ;
#61027 = FACE_OUTER_BOUND ( 'NONE', #158404, .T. ) ;
#61028 = CIRCLE ( 'NONE', #74120, 11.70000000000001528 ) ;
#61029 = CARTESIAN_POINT ( 'NONE',  ( 22.39999999999999858, -1.560176095955058129, -193.3663837337745122 ) ) ;
#61030 = CARTESIAN_POINT ( 'NONE',  ( -20.94999999999999574, 11.62071067812980907, -93.63158334765908819 ) ) ;
#61031 = ORIENTED_EDGE ( 'NONE', *, *, #37035, .F. ) ;
#61032 = AXIS2_PLACEMENT_3D ( 'NONE', #161645, #142046, #44249 ) ;
#61033 = DIRECTION ( 'NONE',  ( -0.7071067811865463515, 0.7071067811865487940, 4.178957128135655137E-15 ) ) ;
#61034 = ORIENTED_EDGE ( 'NONE', *, *, #100871, .F. ) ;
#61035 = CYLINDRICAL_SURFACE ( 'NONE', #61500, 0.1000000000000054040 ) ;
#61036 = AXIS2_PLACEMENT_3D ( 'NONE', #30023, #45700, #27475 ) ;
#61037 = AXIS2_PLACEMENT_3D ( 'NONE', #166317, #150573, #245820 ) ;
#61038 = EDGE_CURVE ( 'NONE', #220134, #41279, #190875, .T. ) ;
#61039 = ORIENTED_EDGE ( 'NONE', *, *, #202551, .F. ) ;
#61040 = ORIENTED_EDGE ( 'NONE', *, *, #88298, .T. ) ;
#61041 = PRESENTATION_LAYER_ASSIGNMENT (  '', '', ( #148165 ) ) ;
#61042 = DIRECTION ( 'NONE',  ( 1.000000000000000000, 0.000000000000000000, 0.000000000000000000 ) ) ;
#61043 = VERTEX_POINT ( 'NONE', #94297 ) ;
#61045 = VERTEX_POINT ( 'NONE', #13499 ) ;
#61044 = DIRECTION ( 'NONE',  ( 1.000000000000000000, -6.696968647535681247E-15, 1.816276285041710114E-15 ) ) ;
#61046 = ADVANCED_FACE ( 'NONE', ( #153042 ), #96841, .T. ) ;
#61049 = ORIENTED_EDGE ( 'NONE', *, *, #195377, .T. ) ;
#61048 = VERTEX_POINT ( 'NONE', #155608 ) ;
#61047 = FACE_OUTER_BOUND ( 'NONE', #197719, .T. ) ;
#61050 = ADVANCED_FACE ( 'NONE', ( #233828 ), #111311, .F. ) ;
#61051 = CARTESIAN_POINT ( 'NONE',  ( -21.29999999999995808, 0.000000000000000000, 0.000000000000000000 ) ) ;
#61052 = EDGE_CURVE ( 'NONE', #85479, #37719, #88569, .T. ) ;
#61053 = DIRECTION ( 'NONE',  ( -2.827886303505248766E-16, -0.8660254037844377084, -0.5000000000000015543 ) ) ;
#61054 = FACE_OUTER_BOUND ( 'NONE', #57408, .T. ) ;
#61055 = CARTESIAN_POINT ( 'NONE',  ( -18.50000000000000000, 1.637172712981535883, -179.0821533654719815 ) ) ;
#61056 = DIRECTION ( 'NONE',  ( 1.000000000000000000, 0.000000000000000000, 0.000000000000000000 ) ) ;
#61057 = CIRCLE ( 'NONE', #15300, 2.100000000000004530 ) ;
#61058 = CARTESIAN_POINT ( 'NONE',  ( -18.59999999999999787, -1.835859311432481045, -145.5044391687985694 ) ) ;
#61059 = DIRECTION ( 'NONE',  ( 1.000000000000000000, 7.304098846218163263E-16, -4.217023435051627211E-16 ) ) ;
#61061 = DIRECTION ( 'NONE',  ( 0.000000000000000000, 1.000000000000000000, 6.982962677686266711E-15 ) ) ;
#61060 = DIRECTION ( 'NONE',  ( 3.697785493223492838E-32, -0.2128009952263605065, 0.9770955615653315052 ) ) ;
#61062 = AXIS2_PLACEMENT_3D ( 'NONE', #228764, #47520, #189632 ) ;
#61063 = ORIENTED_EDGE ( 'NONE', *, *, #50092, .F. ) ;
#61064 = EDGE_LOOP ( 'NONE', ( #36591, #32545, #91815, #144439 ) ) ;
#61066 = LINE ( 'NONE', #140602, #158146 ) ;
#61065 = VECTOR ( 'NONE', #77456, 1000.000000000000000 ) ;
#61068 = ORIENTED_EDGE ( 'NONE', *, *, #152796, .F. ) ;
#61067 = FACE_OUTER_BOUND ( 'NONE', #137510, .T. ) ;
#61070 = CARTESIAN_POINT ( 'NONE',  ( -23.49999999999994316, 83.80000000001119531, -37.18565239344504647 ) ) ;
#61069 = CIRCLE ( 'NONE', #148580, 0.1000000000000115796 ) ;
#61071 = EDGE_LOOP ( 'NONE', ( #97911, #77407, #221681, #137726 ) ) ;
#61072 = EDGE_CURVE ( 'NONE', #191279, #211462, #125990, .T. ) ;
#61073 = CARTESIAN_POINT ( 'NONE',  ( -16.79184697841823848, 12.41370493160941635, -211.2471998651527656 ) ) ;
#61074 = ORIENTED_EDGE ( 'NONE', *, *, #6699, .T. ) ;
#61075 = DIRECTION ( 'NONE',  ( 0.000000000000000000, -0.000000000000000000, 1.000000000000000000 ) ) ;
#61076 = B_SPLINE_CURVE_WITH_KNOTS ( 'NONE', 3,
 ( #159693, #20186, #140097, #41046, #236642, #99679 ),
 .UNSPECIFIED., .F., .F.,
 ( 4, 2, 4 ),
 ( 0.000000000000000000, 0.0001568709654583421050, 0.0003137419309166842099 ),
 .UNSPECIFIED. ) ;
#61077 = CIRCLE ( 'NONE', #190089, 0.1000000000000055844 ) ;
#61078 = TOROIDAL_SURFACE ( 'NONE', #177647, 12.77499999999999858, 0.1000000000000000056 ) ;
#61079 = ORIENTED_EDGE ( 'NONE', *, *, #166566, .T. ) ;
#61080 = DIRECTION ( 'NONE',  ( 0.000000000000000000, 1.000000000000000000, 0.000000000000000000 ) ) ;
#61081 = DIRECTION ( 'NONE',  ( 0.000000000000000000, 0.000000000000000000, -1.000000000000000000 ) ) ;
#61084 = ORIENTED_EDGE ( 'NONE', *, *, #49690, .T. ) ;
#61083 = ORIENTED_EDGE ( 'NONE', *, *, #97876, .T. ) ;
#61082 = VECTOR ( 'NONE', #172437, 1000.000000000000000 ) ;
#61085 = EDGE_LOOP ( 'NONE', ( #1071, #19129, #179621, #217251, #60101, #170799 ) ) ;
#61086 = CARTESIAN_POINT ( 'NONE',  ( -20.94999999999999929, 44.05869416168422958, -258.6139110589941197 ) ) ;
#61087 = AXIS2_PLACEMENT_3D ( 'NONE', #183039, #4375, #126911 ) ;
#61088 = ORIENTED_EDGE ( 'NONE', *, *, #32475, .T. ) ;
#61089 = TOROIDAL_SURFACE ( 'NONE', #236067, 12.97499999999999609, 0.1000000000000000056 ) ;
#61090 = ORIENTED_EDGE ( 'NONE', *, *, #81531, .F. ) ;
#61091 = FACE_OUTER_BOUND ( 'NONE', #64835, .T. ) ;
#61093 = VERTEX_POINT ( 'NONE', #236383 ) ;
#61092 = CARTESIAN_POINT ( 'NONE',  ( 18.58725287972303875, -9.566626910680497531, -107.3225048057656181 ) ) ;
#61094 = ADVANCED_FACE ( 'NONE', ( #57734 ), #12228, .F. ) ;
#61095 = ADVANCED_FACE ( 'NONE', ( #177732 ), #79851, .T. ) ;
#61097 = DIRECTION ( 'NONE',  ( 0.000000000000000000, -0.1575844902526687130, -0.9875055080513762684 ) ) ;
#61096 = DIRECTION ( 'NONE',  ( 0.000000000000000000, 1.000000000000000000, 0.000000000000000000 ) ) ;
#61098 = CARTESIAN_POINT ( 'NONE',  ( -16.81744102076748959, 51.61886293219124155, -231.9464690156495692 ) ) ;
#61099 = CARTESIAN_POINT ( 'NONE',  ( -20.54999999999999716, 4.350000000011156054, -45.85000000000000142 ) ) ;
#61100 = CARTESIAN_POINT ( 'NONE',  ( 23.24999999999999645, 76.00000000001142553, -36.02310748452432421 ) ) ;
#61101 = ORIENTED_EDGE ( 'NONE', *, *, #82859, .F. ) ;
#61102 = ORIENTED_EDGE ( 'NONE', *, *, #121372, .F. ) ;
#61103 = CARTESIAN_POINT ( 'NONE',  ( -17.11825945287481332, 66.05000000001182059, -82.27310748452437394 ) ) ;
#61104 = LINE ( 'NONE', #237188, #172637 ) ;
#61105 = CARTESIAN_POINT ( 'NONE',  ( -23.25000000000000000, 2.600000000011156054, -46.72462192276210402 ) ) ;
#61106 = AXIS2_PLACEMENT_3D ( 'NONE', #90895, #212146, #109161 ) ;
#61107 = EDGE_CURVE ( 'NONE', #207698, #210716, #213474, .T. ) ;
#61108 = VERTEX_POINT ( 'NONE', #60304 ) ;
#61109 = DIRECTION ( 'NONE',  ( 0.000000000000000000, 0.000000000000000000, 1.000000000000000000 ) ) ;
#61110 = DIRECTION ( 'NONE',  ( 0.000000000000000000, -0.1298341882520079038, -0.9915357197604846018 ) ) ;
#61111 = DIRECTION ( 'NONE',  ( 2.879366945564059217E-14, -0.9984213852963244040, -0.05616704890742151013 ) ) ;
#61112 = VERTEX_POINT ( 'NONE', #185069 ) ;
#61113 = ORIENTED_EDGE ( 'NONE', *, *, #58285, .T. ) ;
#61114 = FACE_OUTER_BOUND ( 'NONE', #238066, .T. ) ;
#61115 = LINE ( 'NONE', #98931, #35836 ) ;
#61116 = ORIENTED_EDGE ( 'NONE', *, *, #200275, .F. ) ;
#61117 = DIRECTION ( 'NONE',  ( 0.000000000000000000, -1.000000000000000000, -6.982962677686265922E-15 ) ) ;
#61118 = ORIENTED_EDGE ( 'NONE', *, *, #112693, .T. ) ;
#61119 = CARTESIAN_POINT ( 'NONE',  ( 21.30000000000002558, 76.00000000001267608, -203.5231074845243597 ) ) ;
#61120 = CARTESIAN_POINT ( 'NONE',  ( 20.94999999999999929, 87.48912529308822172, -139.5231074845243029 ) ) ;
#61122 = CARTESIAN_POINT ( 'NONE',  ( -21.05000000000000071, 1.360870587203197646, -175.5729979270909382 ) ) ;
#61121 = DIRECTION ( 'NONE',  ( 0.000000000000000000, 0.000000000000000000, -1.000000000000000000 ) ) ;
#61123 = VECTOR ( 'NONE', #68405, 1000.000000000000114 ) ;
#61124 = DIRECTION ( 'NONE',  ( 1.000000000000000000, 0.000000000000000000, -0.000000000000000000 ) ) ;
#61125 = AXIS2_PLACEMENT_3D ( 'NONE', #141526, #240634, #62012 ) ;
#61126 = EDGE_CURVE ( 'NONE', #100102, #50622, #197259, .T. ) ;
#61127 = CARTESIAN_POINT ( 'NONE',  ( -16.88219499860498374, 66.04979357458428524, -90.37379779441707228 ) ) ;
#61128 = VECTOR ( 'NONE', #36134, 1000.000000000000000 ) ;
#61129 = AXIS2_PLACEMENT_3D ( 'NONE', #162833, #87107, #64986 ) ;
#61130 = VERTEX_POINT ( 'NONE', #6427 ) ;
#61131 = CARTESIAN_POINT ( 'NONE',  ( -21.05000000000000071, -11.64999999998884483, -33.50000000000000000 ) ) ;
#61132 = AXIS2_PLACEMENT_3D ( 'NONE', #178495, #97618, #119802 ) ;
#61134 = VERTEX_POINT ( 'NONE', #159434 ) ;
#61133 = ORIENTED_EDGE ( 'NONE', *, *, #226880, .T. ) ;
#61135 = ORIENTED_EDGE ( 'NONE', *, *, #205024, .F. ) ;
#61136 = ORIENTED_EDGE ( 'NONE', *, *, #203269, .T. ) ;
#61137 = ADVANCED_FACE ( 'NONE', ( #125116 ), #205912, .F. ) ;
#61138 = CARTESIAN_POINT ( 'NONE',  ( 22.32929514600007792, 7.578647565387638174, -33.40092432188608740 ) ) ;
#61139 = DIRECTION ( 'NONE',  ( 0.000000000000000000, 1.000000000000000000, 6.982962677686266711E-15 ) ) ;
#61140 = CARTESIAN_POINT ( 'NONE',  ( -23.25000000000000355, 5.650000000011139001, -146.6500000000000341 ) ) ;
#61141 = DIRECTION ( 'NONE',  ( 3.697785493223492838E-32, -0.2128009952263605065, 0.9770955615653315052 ) ) ;
#61142 = DIRECTION ( 'NONE',  ( 0.000000000000000000, 0.000000000000000000, -1.000000000000000000 ) ) ;
#61143 = AXIS2_PLACEMENT_3D ( 'NONE', #242972, #248113, #27823 ) ;
#61144 = LINE ( 'NONE', #140679, #249624 ) ;
#61145 = ORIENTED_EDGE ( 'NONE', *, *, #13394, .F. ) ;
#61146 = FACE_OUTER_BOUND ( 'NONE', #197061, .T. ) ;
#61147 = EDGE_LOOP ( 'NONE', ( #117426, #145101, #253071, #90877 ) ) ;
#61148 = ADVANCED_FACE ( 'NONE', ( #26008 ), #78586, .T. ) ;
#61149 = CARTESIAN_POINT ( 'NONE',  ( -22.49544290803744317, 11.74987023786832552, -66.93468804074220202 ) ) ;
#61150 = EDGE_CURVE ( 'NONE', #41172, #77258, #183790, .T. ) ;
#61151 = VECTOR ( 'NONE', #16036, 1000.000000000000000 ) ;
#61152 = ORIENTED_EDGE ( 'NONE', *, *, #216778, .F. ) ;
#61153 = ORIENTED_EDGE ( 'NONE', *, *, #168542, .F. ) ;
#61154 = DIRECTION ( 'NONE',  ( 0.000000000000000000, 0.000000000000000000, 1.000000000000000000 ) ) ;
#61155 = CIRCLE ( 'NONE', #206891, 0.1000000000000028644 ) ;
#61156 = LINE ( 'NONE', #179838, #251680 ) ;
#61157 = DIRECTION ( 'NONE',  ( 6.938893903907030216E-14, 0.000000000000000000, 1.000000000000000000 ) ) ;
#61158 = DIRECTION ( 'NONE',  ( -1.000000000000000000, -0.000000000000000000, -0.000000000000000000 ) ) ;
#61159 = EDGE_CURVE ( 'NONE', #144129, #234461, #50962, .T. ) ;
#61160 = DIRECTION ( 'NONE',  ( -0.000000000000000000, -6.982962677686266711E-15, 1.000000000000000000 ) ) ;
#61161 = ADVANCED_FACE ( 'NONE', ( #164240 ), #27326, .F. ) ;
#61162 = ORIENTED_EDGE ( 'NONE', *, *, #156567, .T. ) ;
#61163 = ORIENTED_EDGE ( 'NONE', *, *, #155194, .T. ) ;
#61164 = DIRECTION ( 'NONE',  ( 0.000000000000000000, 0.000000000000000000, 1.000000000000000000 ) ) ;
#61165 = ORIENTED_EDGE ( 'NONE', *, *, #208727, .T. ) ;
#61166 = DIRECTION ( 'NONE',  ( 0.000000000000000000, -7.086529944415894657E-15, 1.000000000000000000 ) ) ;
#61167 = CARTESIAN_POINT ( 'NONE',  ( -20.00857864376270001, 66.85000000001200249, -115.2731074845243597 ) ) ;
#61168 = DIRECTION ( 'NONE',  ( 1.000000000000000000, 0.000000000000000000, 0.000000000000000000 ) ) ;
#61169 = DIRECTION ( 'NONE',  ( 0.000000000000000000, 0.000000000000000000, -1.000000000000000000 ) ) ;
#61170 = CARTESIAN_POINT ( 'NONE',  ( -16.77779411503079032, 66.05389855308774827, -90.36005006690454877 ) ) ;
#61171 = FACE_OUTER_BOUND ( 'NONE', #30295, .T. ) ;
#61172 = FACE_OUTER_BOUND ( 'NONE', #100247, .T. ) ;
#61173 = CARTESIAN_POINT ( 'NONE',  ( -20.94999999999999929, 61.95000000001210338, -131.0094124137634140 ) ) ;
#61174 = ADVANCED_FACE ( 'NONE', ( #65117 ), #66411, .F. ) ;
#61175 = CARTESIAN_POINT ( 'NONE',  ( 20.85000000000000142, -1.835859311432481045, -78.50443916879852679 ) ) ;
#61176 = CIRCLE ( 'NONE', #127824, 0.1000000000000028644 ) ;
#61178 = AXIS2_PLACEMENT_3D ( 'NONE', #137172, #34259, #135870 ) ;
#61177 = CARTESIAN_POINT ( 'NONE',  ( 20.94999999999999574, 76.00000000001195133, -103.0231074845243171 ) ) ;
#61180 = ADVANCED_FACE ( 'NONE', ( #67689 ), #45562, .T. ) ;
#61179 = AXIS2_PLACEMENT_3D ( 'NONE', #230647, #71586, #76348 ) ;
#61181 = CIRCLE ( 'NONE', #106954, 0.09999999999999949207 ) ;
#61182 = EDGE_CURVE ( 'NONE', #226069, #151518, #184253, .T. ) ;
#61183 = ORIENTED_EDGE ( 'NONE', *, *, #176614, .F. ) ;
#61184 = EDGE_CURVE ( 'NONE', #182355, #46904, #246788, .T. ) ;
#61185 = CARTESIAN_POINT ( 'NONE',  ( 20.95420533658165141, 10.54586447477073285, -41.06750602069324430 ) ) ;
#61186 = ORIENTED_EDGE ( 'NONE', *, *, #112189, .F. ) ;
#61187 = CARTESIAN_POINT ( 'NONE',  ( 20.95512820512820440, 58.98414156600839675, -225.6766266970810477 ) ) ;
#61188 = EDGE_CURVE ( 'NONE', #128969, #101017, #18624, .T. ) ;
#61189 = CARTESIAN_POINT ( 'NONE',  ( 23.14999999999999503, 6.450000000000001066, -12.35000000000000320 ) ) ;
#61190 = ADVANCED_FACE ( 'NONE', ( #98126 ), #119023, .T. ) ;
#61191 = ORIENTED_EDGE ( 'NONE', *, *, #14581, .F. ) ;
#61192 = CARTESIAN_POINT ( 'NONE',  ( 18.49999999999999645, 1.115600667400684642E-11, -134.0000000000000284 ) ) ;
#61193 = AXIS2_PLACEMENT_3D ( 'NONE', #3114, #98337, #82635 ) ;
#61195 = ADVANCED_FACE ( 'NONE', ( #179020 ), #332, .T. ) ;
#61194 = DIRECTION ( 'NONE',  ( 0.000000000000000000, 0.000000000000000000, -1.000000000000000000 ) ) ;
#61196 = CARTESIAN_POINT ( 'NONE',  ( -18.50000000000000000, -1.362429037182155023, -74.88888124792120493 ) ) ;
#61197 = CIRCLE ( 'NONE', #189810, 7.900000000000003908 ) ;
#61198 = CIRCLE ( 'NONE', #140272, 0.1999999999999987899 ) ;
#61199 = DIRECTION ( 'NONE',  ( 0.000000000000000000, 1.000000000000000000, 0.000000000000000000 ) ) ;
#61200 = DIRECTION ( 'NONE',  ( -0.000000000000000000, -0.4791956752371546169, -0.8777080977375152360 ) ) ;
#61201 = CARTESIAN_POINT ( 'NONE',  ( 21.05000000000000071, 87.39257802171759693, -106.0970570643561501 ) ) ;
#61202 = CIRCLE ( 'NONE', #206949, 0.6000000000000015321 ) ;
#61203 = ORIENTED_EDGE ( 'NONE', *, *, #11392, .T. ) ;
#61204 = DIRECTION ( 'NONE',  ( 0.000000000000000000, 0.000000000000000000, 1.000000000000000000 ) ) ;
#61206 = VERTEX_POINT ( 'NONE', #230629 ) ;
#61205 = DIRECTION ( 'NONE',  ( 1.000000000000000000, 0.000000000000000000, 0.000000000000000000 ) ) ;
#61207 = CARTESIAN_POINT ( 'NONE',  ( 20.85000000000000142, 1.115600667400684642E-11, -134.0000000000000284 ) ) ;
#61208 = FACE_OUTER_BOUND ( 'NONE', #240007, .T. ) ;
#61209 = ADVANCED_FACE ( 'NONE', ( #131512 ), #180181, .F. ) ;
#61210 = CARTESIAN_POINT ( 'NONE',  ( 20.90000000000000213, 11.49641995933507843, 1.885425182446133885 ) ) ;
#61211 = ORIENTED_EDGE ( 'NONE', *, *, #37225, .T. ) ;
#61212 = DIRECTION ( 'NONE',  ( 1.000000000000000000, 0.000000000000000000, 0.000000000000000000 ) ) ;
#61213 = EDGE_CURVE ( 'NONE', #49841, #6886, #31176, .T. ) ;
#61214 = SHAPE_DEFINITION_REPRESENTATION ( #47193, #213520 ) ;
#61215 = CYLINDRICAL_SURFACE ( 'NONE', #150581, 0.1000000000000118433 ) ;
#61216 = EDGE_LOOP ( 'NONE', ( #154658, #168750, #111665 ) ) ;
#61217 = CYLINDRICAL_SURFACE ( 'NONE', #79566, 0.5000000000000004441 ) ;
#61218 = CARTESIAN_POINT ( 'NONE',  ( 15.69410316191959254, 9.356746017089404788, -184.7033597213641656 ) ) ;
#61219 = CIRCLE ( 'NONE', #231928, 0.09999999999998898659 ) ;
#61220 = CARTESIAN_POINT ( 'NONE',  ( 23.15000000000000213, 48.89266972451527948, -253.5637804087949121 ) ) ;
#61221 = VERTEX_POINT ( 'NONE', #69000 ) ;
#61222 = ORIENTED_EDGE ( 'NONE', *, *, #23559, .T. ) ;
#61223 = DIRECTION ( 'NONE',  ( -1.000000000000000000, -0.000000000000000000, 0.000000000000000000 ) ) ;
#61224 = CIRCLE ( 'NONE', #144398, 0.1000000000000028644 ) ;
#61225 = DIRECTION ( 'NONE',  ( 0.000000000000000000, 0.000000000000000000, -1.000000000000000000 ) ) ;
#61226 = CARTESIAN_POINT ( 'NONE',  ( -18.39999999999999858, 85.60000000001137721, -29.32291809330221355 ) ) ;
#61227 = DIRECTION ( 'NONE',  ( 1.000000000000000000, 0.000000000000000000, 0.000000000000000000 ) ) ;
#61228 = CARTESIAN_POINT ( 'NONE',  ( 18.49999999999999289, 10.25000000263022670, -125.1871719496316615 ) ) ;
#61229 = DIRECTION ( 'NONE',  ( -1.000000000000000000, -0.000000000000000000, 0.000000000000000000 ) ) ;
#61232 = FACE_OUTER_BOUND ( 'NONE', #68410, .T. ) ;
#61231 = AXIS2_PLACEMENT_3D ( 'NONE', #27930, #109991, #67023 ) ;
#61230 = CARTESIAN_POINT ( 'NONE',  ( 21.05000000000000071, 87.75000000001216449, -139.6231074845242688 ) ) ;
#61233 = EDGE_CURVE ( 'NONE', #26247, #200341, #42792, .T. ) ;
#61234 = CARTESIAN_POINT ( 'NONE',  ( 21.15000000000004476, 77.16254490893143725, -44.02310748452479316 ) ) ;
#61235 = DIRECTION ( 'NONE',  ( 0.000000000000000000, -1.000000000000000000, -6.982962677686266711E-15 ) ) ;
#61236 = CARTESIAN_POINT ( 'NONE',  ( 18.51697539158856642, 65.68434038414308418, -30.48668807260655456 ) ) ;
#61237 = CARTESIAN_POINT ( 'NONE',  ( -16.89268316805466341, 9.951721813253341153, -146.6442475214544743 ) ) ;
#61238 = CIRCLE ( 'NONE', #44506, 0.1000000000000028644 ) ;
#61239 = ORIENTED_EDGE ( 'NONE', *, *, #112263, .F. ) ;
#61240 = CIRCLE ( 'NONE', #94536, 11.90000000000000213 ) ;
#61241 = EDGE_CURVE ( 'NONE', #21421, #5563, #71857, .T. ) ;
#61242 = ORIENTED_EDGE ( 'NONE', *, *, #197351, .F. ) ;
#61243 = CARTESIAN_POINT ( 'NONE',  ( -20.64999999999999858, 4.350000000011156054, -88.15000000000004832 ) ) ;
#61245 = DIRECTION ( 'NONE',  ( 0.000000000000000000, -6.853228547068871147E-15, 1.000000000000000000 ) ) ;
#61244 = DIRECTION ( 'NONE',  ( 0.000000000000000000, 0.000000000000000000, -1.000000000000000000 ) ) ;
#61246 = AXIS2_PLACEMENT_3D ( 'NONE', #61524, #160648, #121520 ) ;
#61247 = AXIS2_PLACEMENT_3D ( 'NONE', #104352, #183918, #84779 ) ;
#61248 = FACE_BOUND ( 'NONE', #9255, .T. ) ;
#61249 = DIRECTION ( 'NONE',  ( -0.000000000000000000, 1.000000000000000000, -0.000000000000000000 ) ) ;
#61250 = AXIS2_PLACEMENT_3D ( 'NONE', #83265, #24641, #147107 ) ;
#61251 = DIRECTION ( 'NONE',  ( 1.000000000000000000, 0.000000000000000000, 0.000000000000000000 ) ) ;
#61252 = ORIENTED_EDGE ( 'NONE', *, *, #169622, .F. ) ;
#61253 = DIRECTION ( 'NONE',  ( -1.000000000000000000, 0.000000000000000000, -0.000000000000000000 ) ) ;
#61254 = ORIENTED_EDGE ( 'NONE', *, *, #130369, .T. ) ;
#61255 = CARTESIAN_POINT ( 'NONE',  ( -23.25000000000000000, 37.95493834378066111, -261.2294694241335264 ) ) ;
#61256 = ORIENTED_EDGE ( 'NONE', *, *, #57404, .F. ) ;
#61257 = EDGE_CURVE ( 'NONE', #257053, #255448, #46877, .T. ) ;
#61258 = CARTESIAN_POINT ( 'NONE',  ( -20.64999999999999858, 68.75000000001179501, -81.77310748452435973 ) ) ;
#61259 = AXIS2_PLACEMENT_3D ( 'NONE', #180212, #81075, #160664 ) ;
#61260 = CIRCLE ( 'NONE', #144429, 0.09999999999998898659 ) ;
#61261 = DIRECTION ( 'NONE',  ( 1.000000000000000000, 0.000000000000000000, 0.000000000000000000 ) ) ;
#61262 = VECTOR ( 'NONE', #101782, 1000.000000000000000 ) ;
#61264 = ORIENTED_EDGE ( 'NONE', *, *, #242148, .F. ) ;
#61263 = AXIS2_PLACEMENT_3D ( 'NONE', #228729, #67069, #72220 ) ;
#61265 = DIRECTION ( 'NONE',  ( 1.000000000000000000, 7.304098846218134667E-16, -0.000000000000000000 ) ) ;
#61266 = ORIENTED_EDGE ( 'NONE', *, *, #23509, .T. ) ;
#61267 = CIRCLE ( 'NONE', #236047, 0.09999999999999939493 ) ;
#61268 = FACE_OUTER_BOUND ( 'NONE', #37092, .T. ) ;
#61269 = TOROIDAL_SURFACE ( 'NONE', #256842, 0.2000000000000000111, 0.1000000000000000056 ) ;
#61270 = CARTESIAN_POINT ( 'NONE',  ( -20.94999999999999929, 1.250000000011155299, -75.00000000000004263 ) ) ;
#61271 = DIRECTION ( 'NONE',  ( 1.000000000000000000, 0.000000000000000000, 0.000000000000000000 ) ) ;
#61272 = CARTESIAN_POINT ( 'NONE',  ( -18.46907102845852577, 77.19708304286818645, -241.7715114803566223 ) ) ;
#61273 = CARTESIAN_POINT ( 'NONE',  ( -21.98333005346336932, 1.115600667400684642E-11, -93.12592467094334836 ) ) ;
#61275 = CARTESIAN_POINT ( 'NONE',  ( 18.53317502108576775, 65.67736539654967487, -130.9625116876572406 ) ) ;
#61274 = DIRECTION ( 'NONE',  ( 0.000000000000000000, 0.000000000000000000, 1.000000000000000000 ) ) ;
#61276 = DIRECTION ( 'NONE',  ( 0.7071067811865487940, -4.937700262164522799E-15, 0.7071067811865463515 ) ) ;
#61278 = VERTEX_POINT ( 'NONE', #152395 ) ;
#61277 = CARTESIAN_POINT ( 'NONE',  ( 20.84451136049623798, 65.37985808520379294, -129.0291829250029707 ) ) ;
#61280 = CARTESIAN_POINT ( 'NONE',  ( -1.820710678118657944, -9.929289321870186313, -125.2500000000000284 ) ) ;
#61279 = CARTESIAN_POINT ( 'NONE',  ( -18.60000000000000142, 38.22824641643772736, -261.1961226904935529 ) ) ;
#61281 = EDGE_LOOP ( 'NONE', ( #150200, #182342, #66532, #182967 ) ) ;
#61283 = ORIENTED_EDGE ( 'NONE', *, *, #13878, .F. ) ;
#61282 = LINE ( 'NONE', #200795, #119162 ) ;
#61284 = TOROIDAL_SURFACE ( 'NONE', #132010, 7.800000000000000711, 0.1000000000000000056 ) ;
#61285 = ORIENTED_EDGE ( 'NONE', *, *, #194813, .T. ) ;
#61286 = DIRECTION ( 'NONE',  ( 0.000000000000000000, 0.000000000000000000, 1.000000000000000000 ) ) ;
#61287 = VECTOR ( 'NONE', #12775, 1000.000000000000000 ) ;
#61288 = CARTESIAN_POINT ( 'NONE',  ( -21.53551880898957904, 30.42660484565359980, -252.2347178754784522 ) ) ;
#61289 = DIRECTION ( 'NONE',  ( -1.000000000000000000, -0.000000000000000000, -0.000000000000000000 ) ) ;
#61290 = ORIENTED_EDGE ( 'NONE', *, *, #87589, .F. ) ;
#61291 = CARTESIAN_POINT ( 'NONE',  ( -16.87036670365548474, 66.01058118070987746, -48.54354736722234520 ) ) ;
#61292 = CARTESIAN_POINT ( 'NONE',  ( 21.05000000000000071, 74.83729825007360148, -61.42310748452432989 ) ) ;
#61293 = CARTESIAN_POINT ( 'NONE',  ( 18.45139536634706445, 38.03324368979225056, -261.0487010247114767 ) ) ;
#61294 = ORIENTED_EDGE ( 'NONE', *, *, #130194, .F. ) ;
#61295 = CARTESIAN_POINT ( 'NONE',  ( -18.51024323315077069, 46.39397692848788779, -243.0687461883537708 ) ) ;
#61296 = ADVANCED_FACE ( 'NONE', ( #12880 ), #192644, .T. ) ;
#61297 = VECTOR ( 'NONE', #149308, 999.9999999999998863 ) ;
#61298 = FACE_OUTER_BOUND ( 'NONE', #99143, .T. ) ;
#61299 = VERTEX_POINT ( 'NONE', #111970 ) ;
#61300 = ORIENTED_EDGE ( 'NONE', *, *, #165048, .F. ) ;
#61301 = CARTESIAN_POINT ( 'NONE',  ( -22.47071067811865319, 7.522163794833024220, -199.2603376134758832 ) ) ;
#61302 = ORIENTED_EDGE ( 'NONE', *, *, #81866, .T. ) ;
#61303 = DIRECTION ( 'NONE',  ( 2.940209281316621016E-16, 1.000000000000000000, 7.056502275159890832E-15 ) ) ;
#61304 = EDGE_LOOP ( 'NONE', ( #125214, #79659, #9365, #51225 ) ) ;
#61305 = CARTESIAN_POINT ( 'NONE',  ( 23.15000000000000213, 87.65000000001192859, -106.1231074845242262 ) ) ;
#61306 = AXIS2_PLACEMENT_3D ( 'NONE', #89600, #244827, #45354 ) ;
#61307 = EDGE_CURVE ( 'NONE', #6193, #56955, #230051, .T. ) ;
#61308 = CARTESIAN_POINT ( 'NONE',  ( -20.94999999999999929, 76.00000000001193712, -107.0231074845243029 ) ) ;
#61309 = CARTESIAN_POINT ( 'NONE',  ( 18.49999999999999645, 74.13328508995456900, -91.27043223824230722 ) ) ;
#61310 = EDGE_CURVE ( 'NONE', #131237, #88007, #14163, .T. ) ;
#61311 = CARTESIAN_POINT ( 'NONE',  ( -14.00000000000000178, 66.15000000001258229, -186.7731074845244166 ) ) ;
#61312 = VERTEX_POINT ( 'NONE', #192781 ) ;
#61313 = VECTOR ( 'NONE', #21933, 1000.000000000000000 ) ;
#61314 = AXIS2_PLACEMENT_3D ( 'NONE', #65542, #222027, #43423 ) ;
#61315 = VECTOR ( 'NONE', #129158, 1000.000000000000000 ) ;
#61316 = VECTOR ( 'NONE', #139373, 1000.000000000000000 ) ;
#61317 = DIRECTION ( 'NONE',  ( 0.000000000000000000, 0.2617529984165044010, 0.9651348961777154178 ) ) ;
#61318 = ADVANCED_FACE ( 'NONE', ( #190216 ), #188925, .F. ) ;
#61319 = FACE_OUTER_BOUND ( 'NONE', #37797, .T. ) ;
#61320 = CARTESIAN_POINT ( 'NONE',  ( -20.94999999999999929, 36.65892442174472876, -249.5511627012454596 ) ) ;
#61321 = ORIENTED_EDGE ( 'NONE', *, *, #16578, .T. ) ;
#61323 = DIRECTION ( 'NONE',  ( 1.000000000000000000, 0.000000000000000000, 0.000000000000000000 ) ) ;
#61322 = FACE_OUTER_BOUND ( 'NONE', #19786, .T. ) ;
#61324 = VERTEX_POINT ( 'NONE', #170696 ) ;
#61327 = ORIENTED_EDGE ( 'NONE', *, *, #253149, .F. ) ;
#61326 = CARTESIAN_POINT ( 'NONE',  ( -18.59999999999999787, 64.25000000001222134, -148.2731074845243882 ) ) ;
#61325 = DIRECTION ( 'NONE',  ( 0.000000000000000000, -0.4856429311786307768, -0.8741572761215385956 ) ) ;
#61328 = AXIS2_PLACEMENT_3D ( 'NONE', #244846, #6232, #204433 ) ;
#61329 = ORIENTED_EDGE ( 'NONE', *, *, #33667, .T. ) ;
#61330 = DIRECTION ( 'NONE',  ( -1.000000000000000000, 0.000000000000000000, 0.000000000000000000 ) ) ;
#61331 = FACE_OUTER_BOUND ( 'NONE', #223603, .T. ) ;
#61332 = DIRECTION ( 'NONE',  ( 0.000000000000000000, -0.1335171055202867274, -0.9910465087640866200 ) ) ;
#61333 = ORIENTED_EDGE ( 'NONE', *, *, #81052, .F. ) ;
#61334 = LINE ( 'NONE', #20953, #163601 ) ;
#61335 = EDGE_CURVE ( 'NONE', #173164, #27007, #211057, .T. ) ;
#61336 = CARTESIAN_POINT ( 'NONE',  ( 21.15000000000005187, 76.00000000001119815, -36.02310748452479316 ) ) ;
#61338 = PLANE ( 'NONE',  #171772 ) ;
#61337 = PLANE ( 'NONE',  #80339 ) ;
#61339 = TOROIDAL_SURFACE ( 'NONE', #194639, 0.4000000000000005773, 0.1000000000000000056 ) ;
#61341 = VERTEX_POINT ( 'NONE', #191521 ) ;
#61340 = CARTESIAN_POINT ( 'NONE',  ( 22.01447462590973458, 0.09903700005953483543, 7.263800201229913434 ) ) ;
#61342 = VECTOR ( 'NONE', #63471, 1000.000000000000000 ) ;
#61343 = ORIENTED_EDGE ( 'NONE', *, *, #138796, .T. ) ;
#61344 = CARTESIAN_POINT ( 'NONE',  ( 18.79999999999999716, 4.513204987021263825, 22.10000000000000142 ) ) ;
#61345 = ORIENTED_EDGE ( 'NONE', *, *, #83341, .F. ) ;
#61346 = DIRECTION ( 'NONE',  ( 0.000000000000000000, -0.8660254037844420383, 0.4999999999999942824 ) ) ;
#61347 = ORIENTED_EDGE ( 'NONE', *, *, #123348, .T. ) ;
#61348 = DIRECTION ( 'NONE',  ( 0.000000000000000000, -0.9126074666063769270, -0.4088369013363280513 ) ) ;
#61349 = DIRECTION ( 'NONE',  ( 0.000000000000000000, 1.000000000000000000, 0.000000000000000000 ) ) ;
#61350 = CARTESIAN_POINT ( 'NONE',  ( -21.05000000000000071, 0.09779029131994770863, -161.2421853895238542 ) ) ;
#61351 = ORIENTED_EDGE ( 'NONE', *, *, #175533, .F. ) ;
#61352 = CARTESIAN_POINT ( 'NONE',  ( 20.73486653747088582, 7.250000000011182166, -176.7499999999999716 ) ) ;
#61353 = AXIS2_PLACEMENT_3D ( 'NONE', #96451, #191760, #176040 ) ;
#61354 = VECTOR ( 'NONE', #10196, 1000.000000000000000 ) ;
#61355 = CYLINDRICAL_SURFACE ( 'NONE', #52373, 0.09999999999999939493 ) ;
#61356 = CIRCLE ( 'NONE', #207123, 0.09999999999999939493 ) ;
#61357 = CIRCLE ( 'NONE', #94663, 0.09999999999999939493 ) ;
#61358 = ADVANCED_FACE ( 'NONE', ( #173265 ), #171969, .F. ) ;
#61359 = ORIENTED_EDGE ( 'NONE', *, *, #158848, .T. ) ;
#61360 = VERTEX_POINT ( 'NONE', #70293 ) ;
#61361 = ORIENTED_EDGE ( 'NONE', *, *, #49123, .F. ) ;
#61362 = DIRECTION ( 'NONE',  ( 1.000000000000000000, 0.000000000000000000, 0.000000000000000000 ) ) ;
#61363 = VERTEX_POINT ( 'NONE', #88509 ) ;
#61365 = VERTEX_POINT ( 'NONE', #147224 ) ;
#61364 = CARTESIAN_POINT ( 'NONE',  ( 14.45963434102923451, 66.54845833862704296, -185.0692319856938184 ) ) ;
#61366 = EDGE_CURVE ( 'NONE', #23293, #189866, #122580, .T. ) ;
#61367 = EDGE_LOOP ( 'NONE', ( #151846, #142222, #196846, #44701 ) ) ;
#61370 = ORIENTED_EDGE ( 'NONE', *, *, #86631, .F. ) ;
#61369 = EDGE_LOOP ( 'NONE', ( #170454, #149947, #240223, #29059 ) ) ;
#61368 = CARTESIAN_POINT ( 'NONE',  ( -16.79184697841823493, 9.948761661669548673, -113.1541422706025486 ) ) ;
#61371 = ADVANCED_FACE ( 'NONE', ( #29879 ), #10305, .T. ) ;
#61372 = AXIS2_PLACEMENT_3D ( 'NONE', #245087, #134107, #190263 ) ;
#61373 = EDGE_CURVE ( 'NONE', #136156, #3432, #146827, .T. ) ;
#61374 = AXIS2_PLACEMENT_3D ( 'NONE', #212323, #109329, #89772 ) ;
#61375 = ORIENTED_EDGE ( 'NONE', *, *, #23048, .F. ) ;
#61376 = CARTESIAN_POINT ( 'NONE',  ( 18.59999999999999076, -1.149570369564537842, -175.3159124845019790 ) ) ;
#61377 = DIRECTION ( 'NONE',  ( 0.000000000000000000, 0.000000000000000000, -1.000000000000000000 ) ) ;
#61378 = CIRCLE ( 'NONE', #153007, 0.2000000000000000944 ) ;
#61379 = CARTESIAN_POINT ( 'NONE',  ( -16.96982749440682170, 14.05796827014931871, -218.7911686801608084 ) ) ;
#61380 = EDGE_LOOP ( 'NONE', ( #107937, #196635, #247728, #147132 ) ) ;
#61381 = DIRECTION ( 'NONE',  ( -1.000000000000000000, 0.000000000000000000, 0.000000000000000000 ) ) ;
#61382 = EDGE_CURVE ( 'NONE', #237152, #105632, #197894, .T. ) ;
#61384 = VERTEX_POINT ( 'NONE', #216171 ) ;
#61383 = CARTESIAN_POINT ( 'NONE',  ( 21.05000000000000071, 0.000000000000000000, -33.50000000000000000 ) ) ;
#61385 = CARTESIAN_POINT ( 'NONE',  ( -21.05000000000000071, 87.41227409416133298, -66.52310748452423184 ) ) ;
#61387 = EDGE_LOOP ( 'NONE', ( #66542, #218154, #176934, #240701 ) ) ;
#61386 = DIRECTION ( 'NONE',  ( -1.000000000000000000, 4.851622311275599093E-17, -1.082981191754466866E-16 ) ) ;
#61388 = ADVANCED_FACE ( 'NONE', ( #37565 ), #178369, .F. ) ;
#61389 = ORIENTED_EDGE ( 'NONE', *, *, #127897, .T. ) ;
#61390 = EDGE_CURVE ( 'NONE', #82222, #242287, #115805, .T. ) ;
#61391 = DIRECTION ( 'NONE',  ( 1.000000000000000000, 0.000000000000000000, 0.000000000000000000 ) ) ;
#61392 = CARTESIAN_POINT ( 'NONE',  ( 18.39999999999999858, 85.51932773110434027, -96.05013110796491560 ) ) ;
#61393 = ORIENTED_EDGE ( 'NONE', *, *, #30461, .F. ) ;
#61394 = ORIENTED_EDGE ( 'NONE', *, *, #104881, .F. ) ;
#61395 = CARTESIAN_POINT ( 'NONE',  ( -16.87683809663752754, 9.865889849342865503, -180.7674268070695121 ) ) ;
#61396 = CARTESIAN_POINT ( 'NONE',  ( -21.05000000000000071, 0.09843750001115457449, -161.2007690899130807 ) ) ;
#61397 = VECTOR ( 'NONE', #68176, 1000.000000000000000 ) ;
#61399 = ORIENTED_EDGE ( 'NONE', *, *, #67681, .T. ) ;
#61398 = ORIENTED_EDGE ( 'NONE', *, *, #211975, .T. ) ;
#61400 = ORIENTED_EDGE ( 'NONE', *, *, #97112, .T. ) ;
#61401 = CARTESIAN_POINT ( 'NONE',  ( -22.45354308602258087, 64.15556329907074939, -247.1958792766958481 ) ) ;
#61402 = ORIENTED_EDGE ( 'NONE', *, *, #122360, .F. ) ;
#61403 = ORIENTED_EDGE ( 'NONE', *, *, #79587, .F. ) ;
#61404 = EDGE_CURVE ( 'NONE', #84197, #183369, #92854, .T. ) ;
#61405 = ORIENTED_EDGE ( 'NONE', *, *, #224312, .F. ) ;
#61406 = ADVANCED_FACE ( 'NONE', ( #15437 ), #217444, .F. ) ;
#61407 = DIRECTION ( 'NONE',  ( 0.000000000000000000, 0.000000000000000000, -1.000000000000000000 ) ) ;
#61408 = EDGE_CURVE ( 'NONE', #253110, #118445, #58362, .T. ) ;
#61409 = TOROIDAL_SURFACE ( 'NONE', #186316, 0.4000000000000015210, 0.1000000000000000056 ) ;
#61411 = DIRECTION ( 'NONE',  ( -0.000000000000000000, -0.000000000000000000, 1.000000000000000000 ) ) ;
#61410 = DIRECTION ( 'NONE',  ( 0.000000000000000000, 0.6728971962616965286, -0.7397360091702632756 ) ) ;
#61412 = ORIENTED_EDGE ( 'NONE', *, *, #105742, .F. ) ;
#61414 = ORIENTED_EDGE ( 'NONE', *, *, #98880, .T. ) ;
#61413 = ORIENTED_EDGE ( 'NONE', *, *, #161407, .F. ) ;
#61415 = TOROIDAL_SURFACE ( 'NONE', #194532, 6.258578643762700899, 0.1000000000000000056 ) ;
#61416 = DIRECTION ( 'NONE',  ( 1.000000000000000000, -0.000000000000000000, 0.000000000000000000 ) ) ;
#61417 = CARTESIAN_POINT ( 'NONE',  ( 20.85000000000000142, -1.135018845910178431, -41.21697688343231647 ) ) ;
#61418 = ORIENTED_EDGE ( 'NONE', *, *, #120333, .T. ) ;
#61419 = AXIS2_PLACEMENT_3D ( 'NONE', #162658, #80506, #243461 ) ;
#61420 = VECTOR ( 'NONE', #141616, 1000.000000000000227 ) ;
#61421 = PRODUCT_DEFINITION_FORMATION_WITH_SPECIFIED_SOURCE ( 'ANY', '', #149326, .NOT_KNOWN. ) ;
#61422 = DIRECTION ( 'NONE',  ( 0.000000000000000000, -6.608470384673536824E-15, 1.000000000000000000 ) ) ;
#61423 = TOROIDAL_SURFACE ( 'NONE', #77975, 0.6000000000000017542, 0.1000000000000000056 ) ;
#61424 = ORIENTED_EDGE ( 'NONE', *, *, #65148, .T. ) ;
#61425 = EDGE_CURVE ( 'NONE', #176771, #235080, #139187, .T. ) ;
#61426 = ORIENTED_EDGE ( 'NONE', *, *, #236624, .F. ) ;
#61427 = ADVANCED_FACE ( 'NONE', ( #100056 ), #237035, .F. ) ;
#61428 = CARTESIAN_POINT ( 'NONE',  ( -18.59999999999999787, 9.150000000011157653, -155.1500000000000057 ) ) ;
#61429 = TOROIDAL_SURFACE ( 'NONE', #207194, 11.90000000000000213, 0.1000000000000000056 ) ;
#61430 = VERTEX_POINT ( 'NONE', #19268 ) ;
#61431 = CARTESIAN_POINT ( 'NONE',  ( -23.15000000000000213, 64.35000000001218723, -143.5379132551784096 ) ) ;
#61432 = DIRECTION ( 'NONE',  ( 0.000000000000000000, -6.417474130781257643E-15, 1.000000000000000000 ) ) ;
#61433 = ORIENTED_EDGE ( 'NONE', *, *, #121587, .F. ) ;
#61434 = DIRECTION ( 'NONE',  ( -2.827886303505249259E-16, -0.8660254037844378194, -0.5000000000000016653 ) ) ;
#61435 = CARTESIAN_POINT ( 'NONE',  ( 18.39999999999999858, 85.68240343348850274, -129.8662641071115047 ) ) ;
#61437 = DIRECTION ( 'NONE',  ( 0.000000000000000000, 0.000000000000000000, -1.000000000000000000 ) ) ;
#61436 = FACE_OUTER_BOUND ( 'NONE', #196132, .T. ) ;
#61438 = CARTESIAN_POINT ( 'NONE',  ( 19.75857864376268935, 11.75000000001116440, -91.75000000000004263 ) ) ;
#61439 = DIRECTION ( 'NONE',  ( 0.000000000000000000, 0.9126074666063763718, 0.4088369013363297166 ) ) ;
#61440 = CARTESIAN_POINT ( 'NONE',  ( -20.85000000000000142, 0.1610488207298751417, -66.71581015563977246 ) ) ;
#61441 = ADVANCED_FACE ( 'NONE', ( #218729 ), #98761, .T. ) ;
#61442 = CARTESIAN_POINT ( 'NONE',  ( 18.39999999999998082, 64.52683809664961245, -127.2731074845243882 ) ) ;
#61443 = PLANE ( 'NONE',  #114215 ) ;
#61444 = ORIENTED_EDGE ( 'NONE', *, *, #229803, .F. ) ;
#61445 = CIRCLE ( 'NONE', #153067, 0.2000000000000021205 ) ;
#61448 = ORIENTED_EDGE ( 'NONE', *, *, #157310, .F. ) ;
#61447 = ORIENTED_EDGE ( 'NONE', *, *, #114715, .F. ) ;
#61446 = AXIS2_PLACEMENT_3D ( 'NONE', #249054, #55939, #15587 ) ;
#61449 = ORIENTED_EDGE ( 'NONE', *, *, #248094, .F. ) ;
#61451 = EDGE_LOOP ( 'NONE', ( #120511, #64943, #66868, #96115 ) ) ;
#61450 = AXIS2_PLACEMENT_3D ( 'NONE', #82806, #2006, #99807 ) ;
#61452 = FACE_OUTER_BOUND ( 'NONE', #74348, .T. ) ;
#61453 = DIRECTION ( 'NONE',  ( -1.000000000000000000, 0.000000000000000000, 0.000000000000000000 ) ) ;
#61454 = AXIS2_PLACEMENT_3D ( 'NONE', #175855, #194140, #15502 ) ;
#61455 = CARTESIAN_POINT ( 'NONE',  ( 21.72449340488910252, 65.71604372252116377, -157.3731074845244393 ) ) ;
#61456 = LINE ( 'NONE', #191036, #24710 ) ;
#61457 = ORIENTED_EDGE ( 'NONE', *, *, #37238, .F. ) ;
#61458 = EDGE_CURVE ( 'NONE', #205408, #121571, #234452, .T. ) ;
#61459 = CARTESIAN_POINT ( 'NONE',  ( -20.85882249326303040, 10.33248238083634796, -106.0948465439131922 ) ) ;
#61460 = SURFACE_STYLE_USAGE ( .BOTH. , #117578 ) ;
#61461 = CARTESIAN_POINT ( 'NONE',  ( -18.40000000000000213, 70.35000000001230092, -157.3731074845244109 ) ) ;
#61462 = CARTESIAN_POINT ( 'NONE',  ( 20.94999999999999929, 7.300274141770061398, -211.7264450054621534 ) ) ;
#61463 = ADVANCED_FACE ( 'NONE', ( #97486 ), #20573, .T. ) ;
#61464 = CARTESIAN_POINT ( 'NONE',  ( -16.98495255085918032, 65.99443563401753465, -157.3884902783039195 ) ) ;
#61465 = ORIENTED_EDGE ( 'NONE', *, *, #84433, .T. ) ;
#61466 = AXIS2_PLACEMENT_3D ( 'NONE', #76835, #18148, #114685 ) ;
#61467 = CIRCLE ( 'NONE', #111352, 11.80000000000000426 ) ;
#61468 = AXIS2_PLACEMENT_3D ( 'NONE', #137810, #856, #217345 ) ;
#61469 = CARTESIAN_POINT ( 'NONE',  ( -20.94999999999999929, 64.40000000001161595, -62.59490425424885274 ) ) ;
#61470 = EDGE_CURVE ( 'NONE', #225548, #24943, #155451, .T. ) ;
#61471 = DIRECTION ( 'NONE',  ( -0.000000000000000000, -1.265107689135680095E-16, 1.000000000000000000 ) ) ;
#61472 = ADVANCED_FACE ( 'NONE', ( #238305 ), #196613, .F. ) ;
#61473 = ORIENTED_EDGE ( 'NONE', *, *, #186905, .T. ) ;
#61474 = CARTESIAN_POINT ( 'NONE',  ( 18.59999999999996945, 10.33248238083634440, -106.0948465439131922 ) ) ;
#61475 = CARTESIAN_POINT ( 'NONE',  ( 20.04142135623730070, 64.25000000001220712, -148.2731074845243882 ) ) ;
#61476 = LINE ( 'NONE', #163155, #89435 ) ;
#61477 = DIRECTION ( 'NONE',  ( 0.000000000000000000, 0.000000000000000000, 1.000000000000000000 ) ) ;
#61478 = ADVANCED_FACE ( 'NONE', ( #40149 ), #17972, .T. ) ;
#61479 = FACE_OUTER_BOUND ( 'NONE', #239974, .T. ) ;
#61480 = ORIENTED_EDGE ( 'NONE', *, *, #47512, .T. ) ;
#61481 = CYLINDRICAL_SURFACE ( 'NONE', #75711, 0.1000000000000028644 ) ;
#61482 = PLANE ( 'NONE',  #183354 ) ;
#61483 = AXIS2_PLACEMENT_3D ( 'NONE', #224051, #89670, #105360 ) ;
#61485 = DIRECTION ( 'NONE',  ( 0.000000000000000000, -0.9915357197604804940, 0.1298341882520397950 ) ) ;
#61484 = DIRECTION ( 'NONE',  ( 0.7071067811865127117, 0.7071067811865821007, 0.000000000000000000 ) ) ;
#61486 = CARTESIAN_POINT ( 'NONE',  ( 20.95512820512820440, 10.62384868372303615, -45.70016201942441825 ) ) ;
#61487 = AXIS2_PLACEMENT_3D ( 'NONE', #160566, #22339, #240084 ) ;
#61488 = CARTESIAN_POINT ( 'NONE',  ( 21.14999999999999503, 76.00000000001242029, -176.2731074845243597 ) ) ;
#61489 = DIRECTION ( 'NONE',  ( 0.000000000000000000, -0.000000000000000000, -1.000000000000000000 ) ) ;
#61491 = CARTESIAN_POINT ( 'NONE',  ( 22.45301702632625762, 75.98478912030185484, -114.6728997087847119 ) ) ;
#61490 = AXIS2_PLACEMENT_3D ( 'NONE', #201358, #80085, #239203 ) ;
#61493 = ORIENTED_EDGE ( 'NONE', *, *, #213032, .F. ) ;
#61492 = LINE ( 'NONE', #41947, #111250 ) ;
#61494 = EDGE_CURVE ( 'NONE', #217779, #7029, #74143, .T. ) ;
#61495 = ADVANCED_FACE ( 'NONE', ( #220036 ), #182202, .F. ) ;
#61496 = AXIS2_PLACEMENT_3D ( 'NONE', #192278, #74914, #13629 ) ;
#61497 = ORIENTED_EDGE ( 'NONE', *, *, #239153, .F. ) ;
#61498 = ADVANCED_FACE ( 'NONE', ( #21842 ), #117803, .F. ) ;
#61499 = DIRECTION ( 'NONE',  ( -0.000000000000000000, 0.1022405907414166287, 0.9947597004326451664 ) ) ;
#61500 = AXIS2_PLACEMENT_3D ( 'NONE', #16808, #76754, #181011 ) ;
#61501 = CARTESIAN_POINT ( 'NONE',  ( 20.73486653747088937, 68.25000000001178080, -82.17310748452437963 ) ) ;
#61502 = CIRCLE ( 'NONE', #223795, 0.09999999999999939493 ) ;
#61503 = AXIS2_PLACEMENT_3D ( 'NONE', #69840, #231475, #191074 ) ;
#61504 = FACE_OUTER_BOUND ( 'NONE', #89540, .T. ) ;
#61505 = AXIS2_PLACEMENT_3D ( 'NONE', #206583, #8397, #26685 ) ;
#61506 = EDGE_CURVE ( 'NONE', #207105, #239230, #200477, .T. ) ;
#61507 = CARTESIAN_POINT ( 'NONE',  ( -18.69999999999999929, -10.84999999999999076, -15.00000000000000000 ) ) ;
#61508 = ORIENTED_EDGE ( 'NONE', *, *, #96906, .F. ) ;
#61509 = AXIS2_PLACEMENT_3D ( 'NONE', #257626, #158621, #238117 ) ;
#61510 = LINE ( 'NONE', #159341, #55557 ) ;
#61511 = CARTESIAN_POINT ( 'NONE',  ( 23.14999999999999503, 59.07123845373075000, -221.0531397865252075 ) ) ;
#61512 = CARTESIAN_POINT ( 'NONE',  ( -18.59117750673696889, 65.66751761918668251, -97.42826094061121012 ) ) ;
#61513 = EDGE_CURVE ( 'NONE', #135372, #149012, #46513, .T. ) ;
#61514 = DIRECTION ( 'NONE',  ( 1.000000000000000000, -0.000000000000000000, -0.000000000000000000 ) ) ;
#61516 = VERTEX_POINT ( 'NONE', #23144 ) ;
#61515 = FACE_OUTER_BOUND ( 'NONE', #117497, .T. ) ;
#61518 = DIRECTION ( 'NONE',  ( 1.000000000000000000, 0.000000000000000000, 0.000000000000000000 ) ) ;
#61517 = CARTESIAN_POINT ( 'NONE',  ( 20.04142135623730070, 31.49702336731128582, -233.4564499823349877 ) ) ;
#61519 = CARTESIAN_POINT ( 'NONE',  ( -20.54999999999999716, 24.17260720300848931, -252.6908294531417027 ) ) ;
#61520 = DIRECTION ( 'NONE',  ( 0.000000000000000000, 0.000000000000000000, -1.000000000000000000 ) ) ;
#61521 = ORIENTED_EDGE ( 'NONE', *, *, #255682, .T. ) ;
#61522 = EDGE_CURVE ( 'NONE', #231817, #253110, #192837, .T. ) ;
#61523 = AXIS2_PLACEMENT_3D ( 'NONE', #4479, #42339, #103566 ) ;
#61524 = CARTESIAN_POINT ( 'NONE',  ( 0.000000000000000000, 0.000000000000000000, 0.000000000000000000 ) ) ;
#61525 = DIRECTION ( 'NONE',  ( -3.890533409366484652E-14, -0.1298341882520124002, -0.9915357197604841577 ) ) ;
#61526 = CYLINDRICAL_SURFACE ( 'NONE', #98123, 0.09999999999999939493 ) ;
#61527 = ORIENTED_EDGE ( 'NONE', *, *, #229803, .T. ) ;
#61528 = CARTESIAN_POINT ( 'NONE',  ( 18.39999999999999147, 10.58889512527366428, -208.1606840254082158 ) ) ;
#61529 = CARTESIAN_POINT ( 'NONE',  ( -22.59999999999999787, 1.115600667400684642E-11, -167.4999999999999716 ) ) ;
#61530 = ORIENTED_EDGE ( 'NONE', *, *, #61941, .T. ) ;
#61531 = CIRCLE ( 'NONE', #7349, 2.000000000000001776 ) ;
#61532 = DIRECTION ( 'NONE',  ( 0.000000000000000000, -0.9651348961777028723, 0.2617529984165503087 ) ) ;
#61533 = DIRECTION ( 'NONE',  ( 1.000000000000000000, 0.000000000000000000, 0.000000000000000000 ) ) ;
#61534 = CYLINDRICAL_SURFACE ( 'NONE', #70237, 7.899999999999990585 ) ;
#61535 = EDGE_CURVE ( 'NONE', #85165, #104826, #130270, .T. ) ;
#61536 = ORIENTED_EDGE ( 'NONE', *, *, #149282, .T. ) ;
#61537 = ORIENTED_EDGE ( 'NONE', *, *, #104245, .F. ) ;
#61538 = FACE_OUTER_BOUND ( 'NONE', #182205, .T. ) ;
#61539 = FACE_OUTER_BOUND ( 'NONE', #195804, .T. ) ;
#61540 = DIRECTION ( 'NONE',  ( 0.000000000000000000, 0.000000000000000000, 1.000000000000000000 ) ) ;
#61542 = CARTESIAN_POINT ( 'NONE',  ( 20.95512820512820795, 10.62384868371188240, -12.20016201942441647 ) ) ;
#61541 = DIRECTION ( 'NONE',  ( -1.000000000000000000, 0.000000000000000000, -0.000000000000000000 ) ) ;
#61543 = AXIS2_PLACEMENT_3D ( 'NONE', #234381, #151017, #110591 ) ;
#61544 = AXIS2_PLACEMENT_3D ( 'NONE', #83911, #241748, #245611 ) ;
#61545 = CARTESIAN_POINT ( 'NONE',  ( -18.59999999999999787, 2.272311100394797556, -217.9150152700588876 ) ) ;
#61546 = CARTESIAN_POINT ( 'NONE',  ( -23.30000000000000426, -11.79999999999999893, 33.00000000000000000 ) ) ;
#61547 = AXIS2_PLACEMENT_3D ( 'NONE', #79125, #42587, #140389 ) ;
#61548 = CARTESIAN_POINT ( 'NONE',  ( 22.50000000000000000, 75.95437663941591211, -148.1736118230718944 ) ) ;
#61549 = VERTEX_POINT ( 'NONE', #81771 ) ;
#61550 = PLANE ( 'NONE',  #6559 ) ;
#61552 = ORIENTED_EDGE ( 'NONE', *, *, #226747, .T. ) ;
#61551 = CARTESIAN_POINT ( 'NONE',  ( -21.05000000000000071, -11.48912529306490349, -36.60000000000000142 ) ) ;
#61553 = CARTESIAN_POINT ( 'NONE',  ( -21.05000000000000071, 68.35681244624936426, -231.7050464529142459 ) ) ;
#61554 = CARTESIAN_POINT ( 'NONE',  ( 23.14999999999999503, 59.16775194334852017, -221.0793150863668473 ) ) ;
#61556 = DIRECTION ( 'NONE',  ( -1.000000000000000000, -0.000000000000000000, -0.000000000000000000 ) ) ;
#61555 = CARTESIAN_POINT ( 'NONE',  ( 22.59080734064467677, 64.25000000001195133, -103.0538571926214644 ) ) ;
#61557 = EDGE_CURVE ( 'NONE', #155284, #218820, #17830, .T. ) ;
#61558 = EDGE_LOOP ( 'NONE', ( #115863, #168709, #34781 ) ) ;
#61560 = CARTESIAN_POINT ( 'NONE',  ( -21.05000000000000071, 76.00000000001195133, -103.0231074845243171 ) ) ;
#61559 = CARTESIAN_POINT ( 'NONE',  ( -16.96982749440684657, 66.05000000001157900, -56.39832907571204146 ) ) ;
#61561 = CARTESIAN_POINT ( 'NONE',  ( -21.04999999999994387, 66.15000000001120384, -6.023107484524794941 ) ) ;
#61562 = DIRECTION ( 'NONE',  ( 2.952720810173289112E-16, 1.000000000000000000, 6.530723674265620862E-15 ) ) ;
#61563 = CARTESIAN_POINT ( 'NONE',  ( -23.15000000000000213, 76.00000000001244871, -170.0231074845243597 ) ) ;
#61564 = FACE_OUTER_BOUND ( 'NONE', #71979, .T. ) ;
#61565 = EDGE_LOOP ( 'NONE', ( #36160, #4962, #141567, #218922 ) ) ;
#61566 = FACE_BOUND ( 'NONE', #78526, .T. ) ;
#61567 = ORIENTED_EDGE ( 'NONE', *, *, #142390, .T. ) ;
#61569 = AXIS2_PLACEMENT_3D ( 'NONE', #166162, #113854, #95571 ) ;
#61568 = DIRECTION ( 'NONE',  ( -0.000000000000000000, 1.000000000000000000, -0.000000000000000000 ) ) ;
#61570 = ORIENTED_EDGE ( 'NONE', *, *, #123444, .T. ) ;
#61571 = EDGE_CURVE ( 'NONE', #187669, #256381, #63513, .T. ) ;
#61572 = LINE ( 'NONE', #120301, #251098 ) ;
#61573 = EDGE_LOOP ( 'NONE', ( #156513, #252462, #207073, #43671 ) ) ;
#61575 = DIRECTION ( 'NONE',  ( 1.000000000000000000, 0.000000000000000000, 0.000000000000000000 ) ) ;
#61574 = VECTOR ( 'NONE', #108250, 1000.000000000000000 ) ;
#61576 = DIRECTION ( 'NONE',  ( 0.000000000000000000, 6.982962677686266711E-15, -1.000000000000000000 ) ) ;
#61577 = ORIENTED_EDGE ( 'NONE', *, *, #244798, .F. ) ;
#61578 =( BOUNDED_SURFACE ( )  B_SPLINE_SURFACE ( 3, 2, ( 
 ( #187384, #249912, #150806 ),
 ( #230334, #152118, #51677 ),
 ( #111680, #93392, #52980 ),
 ( #192505, #13869, #172981 ),
 ( #47832, #8736, #88237 ),
 ( #167836, #68711, #148238 ),
 ( #227771, #128692, #59369 ),
 ( #54261, #58099, #76383 ) ),
 .UNSPECIFIED., .F., .F., .F. ) 
 B_SPLINE_SURFACE_WITH_KNOTS ( ( 4, 2, 2, 4 ),
 ( 3, 3 ),
 ( 0.0001704874539069848162, 0.0003809798300636535939, 0.0004862260181419879963, 0.0005914722062203223987 ),
 ( 0.000000000000000000, 1.000000000000000000 ),
 .UNSPECIFIED. ) 
 GEOMETRIC_REPRESENTATION_ITEM ( )  RATIONAL_B_SPLINE_SURFACE ( (
 ( 1.000000000000000000, 0.7071067811864538699, 1.000000000000000000),
 ( 1.000000000000000000, 0.7670648383549212301, 1.000000000000000000),
 ( 1.000000000000000000, 0.8204820770288628884, 1.000000000000000000),
 ( 1.000000000000000000, 0.8877218296095996664, 1.000000000000000000),
 ( 1.000000000000000000, 0.9080815932668204749, 1.000000000000000000),
 ( 1.000000000000000000, 0.9395541505859124065, 1.000000000000000000),
 ( 1.000000000000000000, 0.9506520335380942432, 1.000000000000000000),
 ( 1.000000000000000000, 0.9504532311154588742, 1.000000000000000000) ) ) 
 REPRESENTATION_ITEM ( '' )  SURFACE ( )  );
#61579 = DIRECTION ( 'NONE',  ( 4.239556034732057360E-17, 0.1298341882519953860, 0.9915357197604862671 ) ) ;
#61580 = CARTESIAN_POINT ( 'NONE',  ( -21.14999999999999858, 33.98486250090727623, -243.5821103306120108 ) ) ;
#61581 = CARTESIAN_POINT ( 'NONE',  ( 20.94999999999999929, 11.63687328911507635, -160.6782407866756159 ) ) ;
#61582 = CARTESIAN_POINT ( 'NONE',  ( 21.05000000000000071, 33.13294339707397285, -247.6623911921324463 ) ) ;
#61583 = CARTESIAN_POINT ( 'NONE',  ( 23.14999999999999147, 1.148907358139439339E-11, -201.0000000000015064 ) ) ;
#61584 = CARTESIAN_POINT ( 'NONE',  ( 13.43443725621852813, 62.06390979127201746, -218.8186321886647931 ) ) ;
#61585 = CIRCLE ( 'NONE', #161566, 0.4000000000000097367 ) ;
#61586 = ORIENTED_EDGE ( 'NONE', *, *, #137323, .F. ) ;
#61587 = CYLINDRICAL_SURFACE ( 'NONE', #249018, 0.09999999999999939493 ) ;
#61589 = ORIENTED_EDGE ( 'NONE', *, *, #96563, .T. ) ;
#61588 = AXIS2_PLACEMENT_3D ( 'NONE', #158267, #201199, #240342 ) ;
#61591 = VERTEX_POINT ( 'NONE', #242157 ) ;
#61590 = DIRECTION ( 'NONE',  ( 1.000000000000000000, 0.000000000000000000, 0.000000000000000000 ) ) ;
#61592 = ORIENTED_EDGE ( 'NONE', *, *, #193360, .T. ) ;
#61593 = PLANE ( 'NONE',  #11471 ) ;
#61594 = DIRECTION ( 'NONE',  ( 0.000000000000000000, 0.8103668758649578141, -0.5859227990963213895 ) ) ;
#61595 =( BOUNDED_SURFACE ( )  B_SPLINE_SURFACE ( 3, 2, ( 
 ( #198585, #379, #255946 ),
 ( #19978, #116497, #99465 ),
 ( #96883, #176483, #77346 ),
 ( #60357, #120380, #199897 ) ),
 .UNSPECIFIED., .F., .F., .F. ) 
 B_SPLINE_SURFACE_WITH_KNOTS ( ( 4, 4 ),
 ( 3, 3 ),
 ( 0.04058434257139476031, 0.04256401539001599538 ),
 ( 0.000000000000000000, 1.000000000000000000 ),
 .UNSPECIFIED. ) 
 GEOMETRIC_REPRESENTATION_ITEM ( )  RATIONAL_B_SPLINE_SURFACE ( (
 ( 1.000000000000000000, 0.7103081912008298859, 1.000000000000000000),
 ( 1.000000000000000000, 0.7104998333555329060, 1.000000000000000000),
 ( 1.000000000000000000, 0.7107238315755145530, 1.000000000000000000),
 ( 1.000000000000000000, 0.7110073749539290722, 1.000000000000000000) ) ) 
 REPRESENTATION_ITEM ( '' )  SURFACE ( )  );
#61596 = CARTESIAN_POINT ( 'NONE',  ( -21.17356465864818560, 61.00651281073072596, -234.2694012202724423 ) ) ;
#61597 = VERTEX_POINT ( 'NONE', #240890 ) ;
#61598 = DIRECTION ( 'NONE',  ( 0.000000000000000000, 0.000000000000000000, -1.000000000000000000 ) ) ;
#61599 = VECTOR ( 'NONE', #248209, 1000.000000000000000 ) ;
#61600 = CARTESIAN_POINT ( 'NONE',  ( 18.49999999999999289, 6.846123162363745074, -204.7377262668498190 ) ) ;
#61601 = VERTEX_POINT ( 'NONE', #4808 ) ;
#61602 = EDGE_CURVE ( 'NONE', #89895, #245302, #230232, .T. ) ;
#61603 = DIRECTION ( 'NONE',  ( 0.000000000000000000, -0.9274965247785504907, -0.3738317757009320674 ) ) ;
#61604 = CIRCLE ( 'NONE', #228011, 0.09999999999998898659 ) ;
#61605 = CARTESIAN_POINT ( 'NONE',  ( -20.85000000000000142, 62.88396779178383156, -206.9948552354529170 ) ) ;
#61606 = AXIS2_PLACEMENT_3D ( 'NONE', #158514, #21557, #18964 ) ;
#61607 = ORIENTED_EDGE ( 'NONE', *, *, #216542, .T. ) ;
#61608 = VECTOR ( 'NONE', #46058, 1000.000000000000000 ) ;
#61609 = FACE_OUTER_BOUND ( 'NONE', #59043, .T. ) ;
#61610 = AXIS2_PLACEMENT_3D ( 'NONE', #132484, #33423, #95907 ) ;
#61611 =( BOUNDED_SURFACE ( )  B_SPLINE_SURFACE ( 3, 2, ( 
 ( #16440, #252441, #95935 ),
 ( #55502, #235446, #76372 ),
 ( #13857, #251154, #73855 ),
 ( #35995, #115504, #114233 ),
 ( #195078, #15141, #56790 ),
 ( #231627, #52962, #153404 ) ),
 .UNSPECIFIED., .F., .F., .F. ) 
 B_SPLINE_SURFACE_WITH_KNOTS ( ( 4, 2, 4 ),
 ( 3, 3 ),
 ( 0.0001300404313046471842, 0.0003183318589266437163, 0.0005066232865486402755 ),
 ( 0.000000000000000000, 1.000000000000000000 ),
 .UNSPECIFIED. ) 
 GEOMETRIC_REPRESENTATION_ITEM ( )  RATIONAL_B_SPLINE_SURFACE ( (
 ( 1.000000000000000000, 0.7071067811865402453, 1.000000000000000000),
 ( 1.000000000000000000, 0.7625113560538631097, 1.000000000000000000),
 ( 1.000000000000000000, 0.8126073484690463644, 1.000000000000000000),
 ( 1.000000000000000000, 0.8923049332730159655, 1.000000000000000000),
 ( 1.000000000000000000, 0.9231914937771280583, 1.000000000000000000),
 ( 1.000000000000000000, 0.9238795325112966195, 1.000000000000000000) ) ) 
 REPRESENTATION_ITEM ( '' )  SURFACE ( )  );
#61612 = CARTESIAN_POINT ( 'NONE',  ( 20.94999999999999929, 8.013878543493270001, -211.9507248933737458 ) ) ;
#61614 = VERTEX_POINT ( 'NONE', #222576 ) ;
#61613 = AXIS2_PLACEMENT_3D ( 'NONE', #88996, #128153, #227235 ) ;
#61615 = FACE_OUTER_BOUND ( 'NONE', #246592, .T. ) ;
#61616 = EDGE_CURVE ( 'NONE', #3181, #87379, #113711, .T. ) ;
#61617 = DIRECTION ( 'NONE',  ( 1.000000000000000000, -3.151514657663852580E-16, 8.547182517843351137E-17 ) ) ;
#61618 = DIRECTION ( 'NONE',  ( 1.000000000000000000, 0.000000000000000000, 0.000000000000000000 ) ) ;
#61619 = EDGE_CURVE ( 'NONE', #144450, #171778, #76281, .T. ) ;
#61620 = DIRECTION ( 'NONE',  ( 0.000000000000000000, 0.1298341882520022694, 0.9915357197604852679 ) ) ;
#61622 = ADVANCED_FACE ( 'NONE', ( #163918 ), #123506, .T. ) ;
#61621 = CIRCLE ( 'NONE', #140729, 0.09999999999998898659 ) ;
#61623 = FACE_OUTER_BOUND ( 'NONE', #86959, .T. ) ;
#61624 = TOROIDAL_SURFACE ( 'NONE', #240680, 4.900000000000003020, 0.1000000000000000056 ) ;
#61625 = ORIENTED_EDGE ( 'NONE', *, *, #203519, .T. ) ;
#61626 = DIRECTION ( 'NONE',  ( -1.000000000000000000, 0.000000000000000000, 0.000000000000000000 ) ) ;
#61627 = AXIS2_PLACEMENT_3D ( 'NONE', #139330, #119813, #199341 ) ;
#61628 = VECTOR ( 'NONE', #137370, 1000.000000000000000 ) ;
#61629 = VERTEX_POINT ( 'NONE', #145615 ) ;
#61630 = CIRCLE ( 'NONE', #15870, 4.299999999999956302 ) ;
#61631 = PLANE ( 'NONE',  #255939 ) ;
#61632 = DIRECTION ( 'NONE',  ( -1.000000000000000000, -0.000000000000000000, 0.000000000000000000 ) ) ;
#61634 = EDGE_LOOP ( 'NONE', ( #206164, #222653, #169851, #16748 ) ) ;
#61633 = CARTESIAN_POINT ( 'NONE',  ( 23.15000000000000213, 85.00000000001188027, -93.12913836187181005 ) ) ;
#61635 = DIRECTION ( 'NONE',  ( 1.000000000000000000, 0.000000000000000000, 0.000000000000000000 ) ) ;
#61636 = VECTOR ( 'NONE', #186105, 1000.000000000000000 ) ;
#61637 = EDGE_CURVE ( 'NONE', #208426, #251611, #64804, .T. ) ;
#61638 = SURFACE_STYLE_FILL_AREA ( #165899 ) ;
#61639 = DIRECTION ( 'NONE',  ( -1.000000000000000000, 0.000000000000000000, 0.000000000000000000 ) ) ;
#61640 = DIRECTION ( 'NONE',  ( 0.000000000000000000, 1.000000000000000000, 0.000000000000000000 ) ) ;
#61641 = DIRECTION ( 'NONE',  ( -0.000000000000000000, -0.9126074666063770380, -0.4088369013363281068 ) ) ;
#61643 = ORIENTED_EDGE ( 'NONE', *, *, #52250, .F. ) ;
#61642 = CARTESIAN_POINT ( 'NONE',  ( 21.13461538461538325, 67.11458296203782936, -157.7731074845244166 ) ) ;
#61644 = ADVANCED_FACE ( 'NONE', ( #45248 ), #105171, .F. ) ;
#61645 = VECTOR ( 'NONE', #188442, 1000.000000000000114 ) ;
#61646 = AXIS2_PLACEMENT_3D ( 'NONE', #212174, #30991, #253834 ) ;
#61647 = CARTESIAN_POINT ( 'NONE',  ( -20.94999999999999929, 19.68370618165487329, -225.3554403480446240 ) ) ;
#61648 = ORIENTED_EDGE ( 'NONE', *, *, #140716, .T. ) ;
#61649 = ORIENTED_EDGE ( 'NONE', *, *, #124374, .F. ) ;
#61650 = CARTESIAN_POINT ( 'NONE',  ( -18.41817142474039670, 85.49870306661377128, -62.91914199688723386 ) ) ;
#61651 = CARTESIAN_POINT ( 'NONE',  ( -18.52186455169011481, 85.48101848145532244, -196.4980910066099966 ) ) ;
#61652 = ORIENTED_EDGE ( 'NONE', *, *, #182148, .F. ) ;
#61653 = LINE ( 'NONE', #218136, #120870 ) ;
#61654 = EDGE_CURVE ( 'NONE', #148976, #219200, #225143, .T. ) ;
#61655 = AXIS2_PLACEMENT_3D ( 'NONE', #7260, #108931, #188472 ) ;
#61656 = AXIS2_PLACEMENT_3D ( 'NONE', #190066, #207065, #248761 ) ;
#61657 = CARTESIAN_POINT ( 'NONE',  ( -18.43473496883427032, 85.49495241101085696, -62.47723591229602391 ) ) ;
#61659 = ORIENTED_EDGE ( 'NONE', *, *, #177797, .F. ) ;
#61658 = AXIS2_PLACEMENT_3D ( 'NONE', #6706, #186647, #225731 ) ;
#61660 = CARTESIAN_POINT ( 'NONE',  ( 20.85000000000000142, 28.46617234522943463, -258.4921533293940570 ) ) ;
#61662 = CYLINDRICAL_SURFACE ( 'NONE', #5676, 0.09999999999999939493 ) ;
#61661 = AXIS2_PLACEMENT_3D ( 'NONE', #208953, #30332, #112437 ) ;
#61663 = ADVANCED_FACE ( 'NONE', ( #80483 ), #239608, .F. ) ;
#61664 = ORIENTED_EDGE ( 'NONE', *, *, #103433, .F. ) ;
#61665 = ORIENTED_EDGE ( 'NONE', *, *, #167048, .F. ) ;
#61666 = CARTESIAN_POINT ( 'NONE',  ( -18.50000000000000000, 72.08710075277916474, -192.0412845115134246 ) ) ;
#61667 = VERTEX_POINT ( 'NONE', #132489 ) ;
#61668 = DIRECTION ( 'NONE',  ( 1.000000000000000000, 0.000000000000000000, 0.000000000000000000 ) ) ;
#61669 = VERTEX_POINT ( 'NONE', #52941 ) ;
#61671 = ORIENTED_EDGE ( 'NONE', *, *, #85258, .F. ) ;
#61670 = DIRECTION ( 'NONE',  ( -0.000000000000000000, -1.000000000000000000, 4.336808689942043611E-14 ) ) ;
#61672 = AXIS2_PLACEMENT_3D ( 'NONE', #63612, #47888, #244809 ) ;
#61673 = EDGE_CURVE ( 'NONE', #39176, #110160, #59504, .T. ) ;
#61674 = CYLINDRICAL_SURFACE ( 'NONE', #40328, 0.09999999999999939493 ) ;
#61675 = ORIENTED_EDGE ( 'NONE', *, *, #77710, .F. ) ;
#61676 = VECTOR ( 'NONE', #114414, 1000.000000000000000 ) ;
#61677 = AXIS2_PLACEMENT_3D ( 'NONE', #60503, #77487, #198743 ) ;
#61678 = ORIENTED_EDGE ( 'NONE', *, *, #113581, .T. ) ;
#61680 = ORIENTED_EDGE ( 'NONE', *, *, #127346, .T. ) ;
#61679 = ORIENTED_EDGE ( 'NONE', *, *, #166301, .T. ) ;
#61681 = CARTESIAN_POINT ( 'NONE',  ( -21.55000000000000426, 52.88334710177370113, -233.7906706816490896 ) ) ;
#61682 = CIRCLE ( 'NONE', #207444, 0.09999999999998898659 ) ;
#61683 = EDGE_CURVE ( 'NONE', #115258, #96658, #238613, .T. ) ;
#61684 = CARTESIAN_POINT ( 'NONE',  ( -16.92563707711777710, 14.18410270801246753, -219.2810851154148963 ) ) ;
#61685 = VERTEX_POINT ( 'NONE', #111639 ) ;
#61686 = B_SPLINE_CURVE_WITH_KNOTS ( 'NONE', 3,
 ( #138127, #4705, #216396, #155185, #202923, #242047, #163814, #37788, #36512, #117307, #215117, #43861, #18204, #24313, #123396, #201641, #243329, #78159, #176021 ),
 .UNSPECIFIED., .F., .F.,
 ( 4, 3, 3, 3, 3, 3, 4 ),
 ( 0.000000000000000000, 7.110282409889155599E-05, 0.0001508797727291355647, 0.0002027344179858367663, 0.0002343294522348933582, 0.0002454816334821332082, 0.0002619873080085637876 ),
 .UNSPECIFIED. ) ;
#61687 = AXIS2_PLACEMENT_3D ( 'NONE', #88297, #223979, #67479 ) ;
#61688 = EDGE_CURVE ( 'NONE', #92142, #184550, #34625, .T. ) ;
#61689 = VERTEX_POINT ( 'NONE', #90775 ) ;
#61690 = CARTESIAN_POINT ( 'NONE',  ( 21.05000000000000071, 0.02128009953412425548, -201.0977095561580370 ) ) ;
#61691 = DIRECTION ( 'NONE',  ( 0.000000000000000000, -0.9947597004326491632, 0.1022405907413782566 ) ) ;
#61692 = EDGE_CURVE ( 'NONE', #132235, #41070, #128651, .T. ) ;
#61694 = ORIENTED_EDGE ( 'NONE', *, *, #220705, .F. ) ;
#61693 = CARTESIAN_POINT ( 'NONE',  ( -22.10000000000000497, 6.223900101154157483, 12.09999999999999787 ) ) ;
#61695 = CARTESIAN_POINT ( 'NONE',  ( 21.05000000000000071, 6.650000000011155876, -143.8438220896831297 ) ) ;
#61696 = VERTEX_POINT ( 'NONE', #49088 ) ;
#61697 = DIRECTION ( 'NONE',  ( 1.000000000000000000, 0.000000000000000000, 0.000000000000000000 ) ) ;
#61698 = CARTESIAN_POINT ( 'NONE',  ( 18.49999999999999289, 65.75000000001195133, -111.8731074845243825 ) ) ;
#61699 = VECTOR ( 'NONE', #122540, 1000.000000000000000 ) ;
#61701 = ORIENTED_EDGE ( 'NONE', *, *, #39771, .F. ) ;
#61700 = EDGE_CURVE ( 'NONE', #50700, #87387, #134537, .T. ) ;
#61703 = EDGE_CURVE ( 'NONE', #157963, #190865, #248583, .T. ) ;
#61702 = CYLINDRICAL_SURFACE ( 'NONE', #103358, 0.09999999999998898659 ) ;
#61704 = CARTESIAN_POINT ( 'NONE',  ( -1.820710678118658388, -9.929289321881341834, -24.65000000000000213 ) ) ;
#61705 = CARTESIAN_POINT ( 'NONE',  ( 23.14999999999999503, 64.35000000001197407, -115.1731074845243796 ) ) ;
#61706 = ORIENTED_EDGE ( 'NONE', *, *, #245953, .T. ) ;
#61707 = DIRECTION ( 'NONE',  ( 1.000000000000000000, 0.000000000000000000, 0.000000000000000000 ) ) ;
#61708 = EDGE_LOOP ( 'NONE', ( #115270, #44743, #117330, #165393, #185615, #113238, #168447, #199955, #131291, #29085 ) ) ;
#61710 = ORIENTED_EDGE ( 'NONE', *, *, #199134, .T. ) ;
#61709 = VECTOR ( 'NONE', #196933, 1000.000000000000000 ) ;
#61711 = EDGE_CURVE ( 'NONE', #126560, #107516, #109603, .T. ) ;
#61712 = ORIENTED_EDGE ( 'NONE', *, *, #42667, .T. ) ;
#61713 = ORIENTED_EDGE ( 'NONE', *, *, #97325, .T. ) ;
#61714 = LINE ( 'NONE', #120440, #53251 ) ;
#61715 = ORIENTED_EDGE ( 'NONE', *, *, #229780, .F. ) ;
#61716 = ORIENTED_EDGE ( 'NONE', *, *, #169887, .F. ) ;
#61717 = EDGE_CURVE ( 'NONE', #19541, #39176, #234508, .T. ) ;
#61718 = DIRECTION ( 'NONE',  ( -0.000000000000000000, 0.8660254037844383745, -0.5000000000000003331 ) ) ;
#61719 = EDGE_CURVE ( 'NONE', #160025, #155708, #152076, .T. ) ;
#61720 = FACE_OUTER_BOUND ( 'NONE', #198829, .T. ) ;
#61721 = ORIENTED_EDGE ( 'NONE', *, *, #54578, .T. ) ;
#61722 = ORIENTED_EDGE ( 'NONE', *, *, #153343, .T. ) ;
#61723 = AXIS2_PLACEMENT_3D ( 'NONE', #141097, #83639, #42009 ) ;
#61724 = AXIS2_PLACEMENT_3D ( 'NONE', #30425, #209047, #211625 ) ;
#61725 = CIRCLE ( 'NONE', #174769, 0.1000000000000024342 ) ;
#61726 = CIRCLE ( 'NONE', #136721, 0.1000000000000054040 ) ;
#61727 = ORIENTED_EDGE ( 'NONE', *, *, #62043, .T. ) ;
#61728 = CARTESIAN_POINT ( 'NONE',  ( 20.94999999999999929, 71.18691588786253988, -124.5815897280005089 ) ) ;
#61729 = EDGE_CURVE ( 'NONE', #215705, #95420, #146890, .T. ) ;
#61730 = EDGE_CURVE ( 'NONE', #17884, #33201, #109420, .T. ) ;
#61731 = CARTESIAN_POINT ( 'NONE',  ( 21.05000000000000071, 76.00000000001142553, -36.02310748452432421 ) ) ;
#61732 = CYLINDRICAL_SURFACE ( 'NONE', #31100, 0.09999999999999939493 ) ;
#61733 = DIRECTION ( 'NONE',  ( -0.000000000000000000, -2.891205793294679805E-16, 1.000000000000000000 ) ) ;
#61734 = DIRECTION ( 'NONE',  ( 0.000000000000000000, -2.211772431870365684E-13, -1.000000000000000000 ) ) ;
#61735 = DIRECTION ( 'NONE',  ( 1.000000000000000000, -0.000000000000000000, -0.000000000000000000 ) ) ;
#61738 = DIRECTION ( 'NONE',  ( 0.000000000000000000, 0.000000000000000000, -1.000000000000000000 ) ) ;
#61737 = CIRCLE ( 'NONE', #53361, 0.1000000000000055844 ) ;
#61736 = CARTESIAN_POINT ( 'NONE',  ( -23.15000000000000213, -11.48912529306489994, -164.5000000000000000 ) ) ;
#61739 = CARTESIAN_POINT ( 'NONE',  ( 23.25000000000000000, -11.64999999998883595, -21.75000000000000355 ) ) ;
#61740 = DIRECTION ( 'NONE',  ( -0.000000000000000000, 1.000000000000000000, -0.000000000000000000 ) ) ;
#61741 = ADVANCED_FACE ( 'NONE', ( #9973 ), #131195, .T. ) ;
#61742 = AXIS2_PLACEMENT_3D ( 'NONE', #230955, #190543, #113548 ) ;
#61743 = FACE_OUTER_BOUND ( 'NONE', #106342, .T. ) ;
#61744 = DIRECTION ( 'NONE',  ( 1.000000000000000000, -0.000000000000000000, 0.000000000000000000 ) ) ;
#61745 = ORIENTED_EDGE ( 'NONE', *, *, #4567, .F. ) ;
#61746 = VECTOR ( 'NONE', #25834, 1000.000000000000000 ) ;
#61748 = VERTEX_POINT ( 'NONE', #129906 ) ;
#61747 = CARTESIAN_POINT ( 'NONE',  ( 21.05000000000000071, 10.48443348965288990, -107.9568058014919245 ) ) ;
#61749 = CARTESIAN_POINT ( 'NONE',  ( 15.74999999999999645, 66.15000000001258229, -186.7731074845244450 ) ) ;
#61750 = FACE_OUTER_BOUND ( 'NONE', #62672, .T. ) ;
#61751 = CARTESIAN_POINT ( 'NONE',  ( -22.48479450179659977, 64.13649931337441501, -247.0866463600959833 ) ) ;
#61752 = ORIENTED_EDGE ( 'NONE', *, *, #76889, .T. ) ;
#61753 = EDGE_CURVE ( 'NONE', #168456, #140891, #69970, .T. ) ;
#61754 = FILL_AREA_STYLE_COLOUR ( '', #10826 ) ;
#61755 = DIRECTION ( 'NONE',  ( 1.000000000000000000, -0.000000000000000000, -0.000000000000000000 ) ) ;
#61756 = EDGE_CURVE ( 'NONE', #782, #95600, #184616, .T. ) ;
#61757 = CIRCLE ( 'NONE', #207529, 0.09999999999999939493 ) ;
#61758 = LINE ( 'NONE', #220826, #16369 ) ;
#61759 = ORIENTED_EDGE ( 'NONE', *, *, #236295, .T. ) ;
#61760 = TOROIDAL_SURFACE ( 'NONE', #203235, 11.70000000000000639, 0.1000000000000000056 ) ;
#61761 = CARTESIAN_POINT ( 'NONE',  ( -18.50000000000000000, 10.29270135741298375, -206.4573618871519045 ) ) ;
#61762 = DIRECTION ( 'NONE',  ( 0.000000000000000000, 0.2617529984165152257, 0.9651348961777124202 ) ) ;
#61763 = DIRECTION ( 'NONE',  ( 1.000000000000000000, 0.000000000000000000, -0.000000000000000000 ) ) ;
#61764 = EDGE_CURVE ( 'NONE', #103509, #12088, #86915, .T. ) ;
#61765 = LINE ( 'NONE', #205106, #241199 ) ;
#61767 = ORIENTED_EDGE ( 'NONE', *, *, #249816, .T. ) ;
#61766 = DIRECTION ( 'NONE',  ( 0.000000000000000000, -7.056502275159890832E-15, 1.000000000000000000 ) ) ;
#61768 = CIRCLE ( 'NONE', #207543, 0.09999999999999990841 ) ;
#61770 = ORIENTED_EDGE ( 'NONE', *, *, #170355, .T. ) ;
#61769 = FACE_OUTER_BOUND ( 'NONE', #139627, .T. ) ;
#61772 = EDGE_CURVE ( 'NONE', #116921, #83686, #113893, .T. ) ;
#61771 = CARTESIAN_POINT ( 'NONE',  ( -20.94999999999999929, 77.16270174994961906, -61.42310748452431568 ) ) ;
#61773 = DIRECTION ( 'NONE',  ( 0.000000000000000000, -0.9893560106964500722, 0.1455152366551550613 ) ) ;
#61774 = CARTESIAN_POINT ( 'NONE',  ( -16.93440969289730802, 66.00481482419834833, -157.4318732995136259 ) ) ;
#61775 = CARTESIAN_POINT ( 'NONE',  ( -13.12432614554022869, 9.430764995433474240, -182.7305373947504279 ) ) ;
#61777 = DIRECTION ( 'NONE',  ( -0.000000000000000000, 0.1290532225515619857, 0.9916376685811492120 ) ) ;
#61776 = CARTESIAN_POINT ( 'NONE',  ( -16.93415306273742260, 63.05742080263221538, -213.0577167727462040 ) ) ;
#61779 = EDGE_CURVE ( 'NONE', #22594, #181739, #247285, .T. ) ;
#61778 = LINE ( 'NONE', #141317, #62042 ) ;
#61780 = DIRECTION ( 'NONE',  ( 1.000000000000000000, 0.000000000000000000, 0.000000000000000000 ) ) ;
#61781 = SURFACE_SIDE_STYLE ('',( #44791 ) ) ;
#61782 = DIRECTION ( 'NONE',  ( -1.000000000000000000, -0.000000000000000000, -0.000000000000000000 ) ) ;
#61783 = CIRCLE ( 'NONE', #219995, 0.9000000000000014655 ) ;
#61785 = B_SPLINE_CURVE_WITH_KNOTS ( 'NONE', 3,
 ( #18196, #139403, #19491, #177306, #78151, #119891 ),
 .UNSPECIFIED., .F., .F.,
 ( 4, 2, 4 ),
 ( 0.000000000000000000, 0.0001891491689349584983, 0.0003782983378699169967 ),
 .UNSPECIFIED. ) ;
#61784 = CIRCLE ( 'NONE', #144976, 0.8750000000000007772 ) ;
#61786 = CARTESIAN_POINT ( 'NONE',  ( 21.07971444708685738, 10.04030013319147585, -228.1115500188630278 ) ) ;
#61787 = CIRCLE ( 'NONE', #228399, 0.09999999999998898659 ) ;
#61788 = ORIENTED_EDGE ( 'NONE', *, *, #3260, .F. ) ;
#61789 = EDGE_CURVE ( 'NONE', #18598, #217929, #188910, .T. ) ;
#61790 = DIRECTION ( 'NONE',  ( 0.000000000000000000, 0.000000000000000000, 1.000000000000000000 ) ) ;
#61793 = EDGE_CURVE ( 'NONE', #78009, #190986, #253704, .T. ) ;
#61792 = EDGE_CURVE ( 'NONE', #16790, #138899, #195050, .T. ) ;
#61791 = AXIS2_PLACEMENT_3D ( 'NONE', #18566, #199790, #236317 ) ;
#61794 = ORIENTED_EDGE ( 'NONE', *, *, #164123, .F. ) ;
#61795 = ORIENTED_EDGE ( 'NONE', *, *, #144813, .T. ) ;
#61796 = CARTESIAN_POINT ( 'NONE',  ( -20.94999999999999929, 0.000000000000000000, 0.000000000000000000 ) ) ;
#61797 = DIRECTION ( 'NONE',  ( -0.7071067811865389130, 0.000000000000000000, 0.7071067811865561215 ) ) ;
#61798 = VERTEX_POINT ( 'NONE', #76343 ) ;
#61799 = CIRCLE ( 'NONE', #78545, 0.09999999999999892308 ) ;
#61800 = EDGE_LOOP ( 'NONE', ( #165894, #26260, #106023 ) ) ;
#61801 = AXIS2_PLACEMENT_3D ( 'NONE', #204922, #64150, #223205 ) ;
#61802 = ORIENTED_EDGE ( 'NONE', *, *, #152705, .T. ) ;
#61803 = ADVANCED_FACE ( 'NONE', ( #256210 ), #13828, .T. ) ;
#61804 = DIRECTION ( 'NONE',  ( -1.000000000000000000, 0.000000000000000000, 0.000000000000000000 ) ) ;
#61806 = ADVANCED_FACE ( 'NONE', ( #112929 ), #155930, .T. ) ;
#61805 = AXIS2_PLACEMENT_3D ( 'NONE', #120135, #139629, #99222 ) ;
#61807 = VERTEX_POINT ( 'NONE', #118054 ) ;
#61809 = FACE_OUTER_BOUND ( 'NONE', #160071, .T. ) ;
#61808 = AXIS2_PLACEMENT_3D ( 'NONE', #58197, #235561, #114349 ) ;
#61810 = DIRECTION ( 'NONE',  ( 0.000000000000000000, 1.000000000000000000, 0.000000000000000000 ) ) ;
#61811 = CARTESIAN_POINT ( 'NONE',  ( -16.78270389226384296, 66.05262738339480677, -82.18190044761291801 ) ) ;
#61812 = AXIS2_PLACEMENT_3D ( 'NONE', #38008, #97918, #161804 ) ;
#61813 = VECTOR ( 'NONE', #148698, 1000.000000000000000 ) ;
#61814 = DIRECTION ( 'NONE',  ( -0.000000000000000000, 1.000000000000000000, -0.000000000000000000 ) ) ;
#61815 = DIRECTION ( 'NONE',  ( -1.000000000000000000, 0.000000000000000000, 0.000000000000000000 ) ) ;
#61816 = CIRCLE ( 'NONE', #74327, 0.09999999999999939493 ) ;
#61817 = ADVANCED_FACE ( 'NONE', ( #235421 ), #59330, .F. ) ;
#61818 = FACE_OUTER_BOUND ( 'NONE', #67772, .T. ) ;
#61819 = CARTESIAN_POINT ( 'NONE',  ( -23.25000000000000000, -8.596261682231835621, -109.9501275171503210 ) ) ;
#61821 = VERTEX_POINT ( 'NONE', #38529 ) ;
#61820 = CARTESIAN_POINT ( 'NONE',  ( -21.53551880898957904, 75.90103026544004194, -76.30790524594065971 ) ) ;
#61823 = CARTESIAN_POINT ( 'NONE',  ( 18.52351027002948669, 85.64216290470656645, -29.30806053401447286 ) ) ;
#61822 = CARTESIAN_POINT ( 'NONE',  ( 18.59999999999998721, 6.933893972137497030, -171.2856458343736108 ) ) ;
#61824 = CIRCLE ( 'NONE', #215909, 0.5999999999999969802 ) ;
#61825 = DIRECTION ( 'NONE',  ( 0.000000000000000000, 0.000000000000000000, 1.000000000000000000 ) ) ;
#61826 = EDGE_CURVE ( 'NONE', #98003, #60425, #154650, .T. ) ;
#61827 = EDGE_LOOP ( 'NONE', ( #149334, #48515, #252387, #19099 ) ) ;
#61828 = DIRECTION ( 'NONE',  ( 1.000000000000000000, 0.000000000000000000, 0.000000000000000000 ) ) ;
#61829 = DIRECTION ( 'NONE',  ( -1.000000000000000000, 0.000000000000000000, 0.000000000000000000 ) ) ;
#61830 = ORIENTED_EDGE ( 'NONE', *, *, #198988, .T. ) ;
#61831 = ADVANCED_FACE ( 'NONE', ( #55476 ), #17659, .T. ) ;
#61833 = CYLINDRICAL_SURFACE ( 'NONE', #220746, 0.1000000000000021844 ) ;
#61832 = DIRECTION ( 'NONE',  ( -1.073024830501117725E-15, -0.9126074666063770380, -0.4088369013363281068 ) ) ;
#61834 = CARTESIAN_POINT ( 'NONE',  ( -16.89155683852747813, 66.05000000001449223, -82.80047933406495986 ) ) ;
#61835 = CIRCLE ( 'NONE', #86737, 0.1000000000000001860 ) ;
#61837 = ORIENTED_EDGE ( 'NONE', *, *, #237754, .T. ) ;
#61836 = AXIS2_PLACEMENT_3D ( 'NONE', #122803, #163207, #242718 ) ;
#61838 = CARTESIAN_POINT ( 'NONE',  ( -18.79999999999999716, -11.65000000000000036, 32.89999999999999858 ) ) ;
#61839 = DIRECTION ( 'NONE',  ( -1.000000000000000000, -1.040834085586090568E-13, 0.000000000000000000 ) ) ;
#61840 = CARTESIAN_POINT ( 'NONE',  ( -18.36527282682003204, -0.6805348922791804034, -242.5179119244810977 ) ) ;
#61841 = DIRECTION ( 'NONE',  ( 0.000000000000000000, 0.8814952561688444987, -0.4721928772777320149 ) ) ;
#61842 = EDGE_CURVE ( 'NONE', #212015, #169097, #140848, .T. ) ;
#61843 = ORIENTED_EDGE ( 'NONE', *, *, #241883, .F. ) ;
#61844 = CIRCLE ( 'NONE', #103510, 0.1000000000000072220 ) ;
#61845 = CIRCLE ( 'NONE', #28579, 0.09999999999998712696 ) ;
#61847 = EDGE_CURVE ( 'NONE', #28813, #221229, #172211, .T. ) ;
#61846 = CARTESIAN_POINT ( 'NONE',  ( 20.95512828230159030, 67.12384868768657498, -90.82067721902097901 ) ) ;
#61848 = CARTESIAN_POINT ( 'NONE',  ( -23.25000000000000000, 4.150000000011156764, -112.8500000000000369 ) ) ;
#61849 = CARTESIAN_POINT ( 'NONE',  ( -18.59999999999999787, 74.95904887477786360, -233.7774272632847783 ) ) ;
#61850 = CIRCLE ( 'NONE', #186955, 0.2000000000000057288 ) ;
#61851 = CARTESIAN_POINT ( 'NONE',  ( 20.94999999999999929, 0.6656436123793473270, -212.6810495496487476 ) ) ;
#61852 = DIRECTION ( 'NONE',  ( 1.000000000000000000, 0.000000000000000000, 0.000000000000000000 ) ) ;
#61853 = AXIS2_PLACEMENT_3D ( 'NONE', #129121, #11763, #88676 ) ;
#61855 = ORIENTED_EDGE ( 'NONE', *, *, #232868, .F. ) ;
#61854 = DIRECTION ( 'NONE',  ( 1.000000000000000000, 0.000000000000000000, 0.000000000000000000 ) ) ;
#61856 = DIRECTION ( 'NONE',  ( -1.000000000000000000, -2.952720810173289112E-16, 0.000000000000000000 ) ) ;
#61857 = DIRECTION ( 'NONE',  ( -0.000000000000000000, 0.000000000000000000, 1.000000000000000000 ) ) ;
#61858 = LINE ( 'NONE', #157122, #245994 ) ;
#61859 = CARTESIAN_POINT ( 'NONE',  ( 21.05000000000000071, 6.257814610487280937, -167.4022097086911742 ) ) ;
#61860 = EDGE_CURVE ( 'NONE', #229115, #231485, #15118, .T. ) ;
#61861 = CARTESIAN_POINT ( 'NONE',  ( -18.59999999999999787, 77.85161776048025217, -24.41991776492064758 ) ) ;
#61863 = EDGE_LOOP ( 'NONE', ( #199403, #227172, #203157, #90559 ) ) ;
#61862 = CARTESIAN_POINT ( 'NONE',  ( -1.820710678118658388, -9.929289321870186313, -125.1500000000000341 ) ) ;
#61864 = FACE_OUTER_BOUND ( 'NONE', #3300, .T. ) ;
#61865 = TOROIDAL_SURFACE ( 'NONE', #211725, 4.099999999999999645, 0.1000000000000000056 ) ;
#61866 = DIRECTION ( 'NONE',  ( 0.000000000000000000, 1.000000000000000000, 0.000000000000000000 ) ) ;
#61867 = CARTESIAN_POINT ( 'NONE',  ( 20.94999999999999929, 67.49462292596868451, -195.5612049585272700 ) ) ;
#61868 = ORIENTED_EDGE ( 'NONE', *, *, #85730, .F. ) ;
#61869 = DIRECTION ( 'NONE',  ( 0.000000000000000000, -0.9930108503404180276, -0.1180230956474192239 ) ) ;
#61870 = CARTESIAN_POINT ( 'NONE',  ( 18.59999999999999432, -1.162701749926853712, -41.60000000000000142 ) ) ;
#61871 = AXIS2_PLACEMENT_3D ( 'NONE', #205488, #86815, #47693 ) ;
#61872 = AXIS2_PLACEMENT_3D ( 'NONE', #230872, #49640, #108343 ) ;
#61873 = CARTESIAN_POINT ( 'NONE',  ( 23.24999999999999289, 21.17283678855157802, -243.7231193059830048 ) ) ;
#61874 = AXIS2_PLACEMENT_3D ( 'NONE', #69714, #149254, #206637 ) ;
#61875 = CYLINDRICAL_SURFACE ( 'NONE', #88274, 0.09999999999999939493 ) ;
#61876 = AXIS2_PLACEMENT_3D ( 'NONE', #251238, #11367, #90894 ) ;
#61877 = CARTESIAN_POINT ( 'NONE',  ( -16.96982749440706328, 9.950000000011137047, -87.37522159118832121 ) ) ;
#61878 = ORIENTED_EDGE ( 'NONE', *, *, #4399, .T. ) ;
#61879 = ORIENTED_EDGE ( 'NONE', *, *, #124257, .T. ) ;
#61880 = LINE ( 'NONE', #205216, #168275 ) ;
#61881 = CARTESIAN_POINT ( 'NONE',  ( 18.39999999999999858, -9.599999999988842347, -107.5320693966997112 ) ) ;
#61882 = CARTESIAN_POINT ( 'NONE',  ( -22.39999999999999858, 76.00000000001271871, -209.7731074845243597 ) ) ;
#61883 = CARTESIAN_POINT ( 'NONE',  ( -21.05000000000000071, 76.00000000001237765, -170.0231074845243597 ) ) ;
#61884 = ORIENTED_EDGE ( 'NONE', *, *, #106254, .T. ) ;
#61885 = DIRECTION ( 'NONE',  ( 1.000000000000000000, 0.000000000000000000, 0.000000000000000000 ) ) ;
#61886 = CIRCLE ( 'NONE', #186799, 0.09999999999999938105 ) ;
#61887 = CARTESIAN_POINT ( 'NONE',  ( 20.21567752745037794, 11.64196147963353134, -206.5319045250219858 ) ) ;
#61888 = CARTESIAN_POINT ( 'NONE',  ( -16.81744102076749314, 9.949999999999986855, -12.65000000000000213 ) ) ;
#61889 = CARTESIAN_POINT ( 'NONE',  ( -20.65000000000000568, 5.650000000011139001, -54.35000000000000142 ) ) ;
#61890 = DIRECTION ( 'NONE',  ( -0.000000000000000000, 0.2617529984165031243, 0.9651348961777157509 ) ) ;
#61891 = DIRECTION ( 'NONE',  ( -1.000000000000000000, 0.000000000000000000, 0.000000000000000000 ) ) ;
#61892 = ORIENTED_EDGE ( 'NONE', *, *, #193302, .T. ) ;
#61894 = EDGE_LOOP ( 'NONE', ( #224425, #151281, #14659, #141332 ) ) ;
#61893 = LINE ( 'NONE', #99698, #52707 ) ;
#61895 = ORIENTED_EDGE ( 'NONE', *, *, #147259, .T. ) ;
#61896 = DIRECTION ( 'NONE',  ( -1.000000000000000000, 0.000000000000000000, 0.000000000000000000 ) ) ;
#61897 = ORIENTED_EDGE ( 'NONE', *, *, #33972, .T. ) ;
#61898 = CARTESIAN_POINT ( 'NONE',  ( -23.24999999999999645, 85.60000000001166143, -62.92291809330219365 ) ) ;
#61899 = DIRECTION ( 'NONE',  ( 0.000000000000000000, 0.000000000000000000, -1.000000000000000000 ) ) ;
#61900 = DIRECTION ( 'NONE',  ( -1.000000000000000000, -0.000000000000000000, -0.000000000000000000 ) ) ;
#61901 = ORIENTED_EDGE ( 'NONE', *, *, #127434, .F. ) ;
#61902 = CARTESIAN_POINT ( 'NONE',  ( -16.86445178670626888, 66.03778837089552667, -56.91388492264187704 ) ) ;
#61903 = DIRECTION ( 'NONE',  ( 1.000000000000000000, 0.000000000000000000, 0.000000000000000000 ) ) ;
#61904 = ORIENTED_EDGE ( 'NONE', *, *, #50299, .F. ) ;
#61905 = CARTESIAN_POINT ( 'NONE',  ( 22.49999999999999645, 11.64987090377453960, -100.4174801091270979 ) ) ;
#61907 = ORIENTED_EDGE ( 'NONE', *, *, #186327, .F. ) ;
#61906 = FACE_OUTER_BOUND ( 'NONE', #69822, .T. ) ;
#61908 = EDGE_CURVE ( 'NONE', #97513, #74229, #122275, .T. ) ;
#61909 = CYLINDRICAL_SURFACE ( 'NONE', #235795, 0.09999999999999867328 ) ;
#61910 = DIRECTION ( 'NONE',  ( 1.000000000000000000, 0.000000000000000000, 0.000000000000000000 ) ) ;
#61911 = CIRCLE ( 'NONE', #28643, 4.049999999999998046 ) ;
#61912 = CIRCLE ( 'NONE', #107689, 0.09999999999999520384 ) ;
#61913 = AXIS2_PLACEMENT_3D ( 'NONE', #25002, #201044, #22434 ) ;
#61914 = VERTEX_POINT ( 'NONE', #232899 ) ;
#61915 = DIRECTION ( 'NONE',  ( 0.000000000000000000, -1.000000000000000000, -0.000000000000000000 ) ) ;
#61916 = CARTESIAN_POINT ( 'NONE',  ( -18.39418127959864790, 11.48390560169813668, -24.25000000000000000 ) ) ;
#61917 = AXIS2_PLACEMENT_3D ( 'NONE', #198746, #538, #179219 ) ;
#61918 = DIRECTION ( 'NONE',  ( 0.000000000000000000, -0.9915357197604982575, 0.1298341882519033486 ) ) ;
#61919 = ORIENTED_EDGE ( 'NONE', *, *, #41500, .F. ) ;
#61920 = FACE_OUTER_BOUND ( 'NONE', #108433, .T. ) ;
#61921 = ADVANCED_FACE ( 'NONE', ( #37260 ), #234145, .T. ) ;
#61922 = CARTESIAN_POINT ( 'NONE',  ( 13.43663047529820176, 49.59862664907821994, -233.4030665626792995 ) ) ;
#61923 = CARTESIAN_POINT ( 'NONE',  ( -21.14999999999999858, 6.540656951712397138, -67.10000000000005116 ) ) ;
#61924 = ADVANCED_FACE ( 'NONE', ( #172944 ), #133764, .T. ) ;
#61925 = VERTEX_POINT ( 'NONE', #252415 ) ;
#61926 = CIRCLE ( 'NONE', #174403, 0.09999999999999939493 ) ;
#61927 = AXIS2_PLACEMENT_3D ( 'NONE', #157728, #155149, #218919 ) ;
#61928 = AXIS2_PLACEMENT_3D ( 'NONE', #43969, #205594, #206897 ) ;
#61929 = EDGE_CURVE ( 'NONE', #146220, #197879, #80541, .T. ) ;
#61930 = AXIS2_PLACEMENT_3D ( 'NONE', #134851, #39667, #216968 ) ;
#61931 = VERTEX_POINT ( 'NONE', #237995 ) ;
#61932 = EDGE_CURVE ( 'NONE', #249163, #130019, #143096, .T. ) ;
#61933 = VERTEX_POINT ( 'NONE', #184449 ) ;
#61934 = EDGE_CURVE ( 'NONE', #14875, #110943, #202729, .T. ) ;
#61935 = FACE_OUTER_BOUND ( 'NONE', #92774, .T. ) ;
#61936 = CARTESIAN_POINT ( 'NONE',  ( 18.54999999999999716, 67.25000000001259082, -194.2731074845244166 ) ) ;
#61938 = ORIENTED_EDGE ( 'NONE', *, *, #182288, .T. ) ;
#61937 = CYLINDRICAL_SURFACE ( 'NONE', #137664, 4.000000000000003553 ) ;
#61939 = DIRECTION ( 'NONE',  ( -0.000000000000000000, 0.000000000000000000, 1.000000000000000000 ) ) ;
#61940 = LINE ( 'NONE', #144026, #53118 ) ;
#61941 = EDGE_CURVE ( 'NONE', #246557, #171400, #59703, .T. ) ;
#61942 = B_SPLINE_CURVE_WITH_KNOTS ( 'NONE', 3,
 ( #98940, #179812, #123679, #2419, #181097, #183657, #40323, #243613, #83227, #203203, #139359, #198068, #41595, #178542, #24598, #84490 ),
 .UNSPECIFIED., .F., .F.,
 ( 4, 3, 3, 3, 3, 4 ),
 ( 0.000000000000000000, 2.209833635978076120E-05, 5.595056164119274593E-05, 8.979992002655373272E-05, 0.0001236482757198912469, 0.0001574984039362985829 ),
 .UNSPECIFIED. ) ;
#61943 = CARTESIAN_POINT ( 'NONE',  ( 18.59999999999999076, 64.35000000001177511, -78.17310748452437963 ) ) ;
#61944 = CARTESIAN_POINT ( 'NONE',  ( -16.88328101497759448, 51.61979511467394133, -231.9456647872781900 ) ) ;
#61945 = CARTESIAN_POINT ( 'NONE',  ( -18.47653818581420637, 85.46528038777508129, -129.3971466683843801 ) ) ;
#61946 = DIRECTION ( 'NONE',  ( 1.000000000000000000, 0.000000000000000000, 0.000000000000000000 ) ) ;
#61948 = VERTEX_POINT ( 'NONE', #20256 ) ;
#61947 = CARTESIAN_POINT ( 'NONE',  ( -16.92778301347286529, 65.99905508317719693, -182.5945893765574795 ) ) ;
#61950 = ORIENTED_EDGE ( 'NONE', *, *, #130681, .F. ) ;
#61949 = CARTESIAN_POINT ( 'NONE',  ( -16.27683809663751191, 11.80649599073814215, -211.2728599922799617 ) ) ;
#61951 = CARTESIAN_POINT ( 'NONE',  ( -18.59999999999999787, 11.65000000001115232, -146.1500000000000341 ) ) ;
#61952 = EDGE_CURVE ( 'NONE', #92370, #129641, #181894, .T. ) ;
#61953 = EDGE_LOOP ( 'NONE', ( #204421, #92150, #151564 ) ) ;
#61954 = AXIS2_PLACEMENT_3D ( 'NONE', #248464, #108936, #148080 ) ;
#61955 = VERTEX_POINT ( 'NONE', #44952 ) ;
#61956 = DIRECTION ( 'NONE',  ( -1.000000000000000000, 0.000000000000000000, 0.000000000000000000 ) ) ;
#61958 = CARTESIAN_POINT ( 'NONE',  ( 18.59999999999999787, 74.98773774893902555, -233.8732236541320333 ) ) ;
#61957 = AXIS2_PLACEMENT_3D ( 'NONE', #155078, #195484, #36407 ) ;
#61959 = EDGE_CURVE ( 'NONE', #118692, #148702, #209570, .T. ) ;
#61960 = DIRECTION ( 'NONE',  ( -1.000000000000000000, 0.000000000000000000, -0.000000000000000000 ) ) ;
#61961 = EDGE_CURVE ( 'NONE', #180734, #149751, #140169, .T. ) ;
#61963 = CARTESIAN_POINT ( 'NONE',  ( -21.05000000000000071, 1.115600667400684642E-11, -134.0000000000000000 ) ) ;
#61962 = CIRCLE ( 'NONE', #228563, 0.09999999999999961697 ) ;
#61964 = CARTESIAN_POINT ( 'NONE',  ( 20.94999999999999929, -9.499999999988848032, -177.3939691226524076 ) ) ;
#61965 = ADVANCED_FACE ( 'NONE', ( #3228 ), #41118, .F. ) ;
#61966 = DIRECTION ( 'NONE',  ( 0.000000000000000000, 6.982962677686267499E-15, -1.000000000000000000 ) ) ;
#61967 = ORIENTED_EDGE ( 'NONE', *, *, #138199, .F. ) ;
#61968 = ORIENTED_EDGE ( 'NONE', *, *, #129940, .F. ) ;
#61969 = CIRCLE ( 'NONE', #3505, 11.69999999999998863 ) ;
#61970 = VECTOR ( 'NONE', #250387, 1000.000000000000000 ) ;
#61971 = EDGE_LOOP ( 'NONE', ( #213406, #74581, #72085, #108327 ) ) ;
#61973 = SPHERICAL_SURFACE ( 'NONE', #255747, 0.1000000000000000056 ) ;
#61972 = AXIS2_PLACEMENT_3D ( 'NONE', #65998, #142944, #222481 ) ;
#61974 = CARTESIAN_POINT ( 'NONE',  ( -14.45443560709636266, 66.54940788787786232, -54.46691916571599990 ) ) ;
#61975 = CIRCLE ( 'NONE', #16205, 0.1000000000000076938 ) ;
#61976 = DIRECTION ( 'NONE',  ( -1.000000000000000000, -8.153259210133937167E-16, -2.158126701439427224E-16 ) ) ;
#61977 = EDGE_CURVE ( 'NONE', #209103, #46675, #142899, .T. ) ;
#61978 = ORIENTED_EDGE ( 'NONE', *, *, #25227, .F. ) ;
#61979 = DIRECTION ( 'NONE',  ( 0.000000000000000000, 0.2128009952263650861, -0.9770955615653305060 ) ) ;
#61980 = ORIENTED_EDGE ( 'NONE', *, *, #245231, .F. ) ;
#61982 = CARTESIAN_POINT ( 'NONE',  ( -23.15000000000000213, 17.11694853917243364, -224.3781540347815451 ) ) ;
#61981 = SHAPE_REPRESENTATION ( 'Injection Molded Chain Links 8', ( #2425 ), #110949 ) ;
#61983 = ORIENTED_EDGE ( 'NONE', *, *, #203192, .T. ) ;
#61984 = CIRCLE ( 'NONE', #254076, 0.09999999999998898659 ) ;
#61985 = AXIS2_PLACEMENT_3D ( 'NONE', #39123, #169359, #7688 ) ;
#61986 = CARTESIAN_POINT ( 'NONE',  ( 18.59999999999999076, 74.16465844978745281, -91.46795619196133487 ) ) ;
#61987 = CARTESIAN_POINT ( 'NONE',  ( 12.25000000000000000, 9.350000000011140955, -184.2499999999999716 ) ) ;
#61988 = ORIENTED_EDGE ( 'NONE', *, *, #114474, .F. ) ;
#61989 = DIRECTION ( 'NONE',  ( -1.000000000000000000, 2.849773892568378313E-16, -7.728835255496647986E-17 ) ) ;
#61990 = AXIS2_PLACEMENT_3D ( 'NONE', #24743, #104224, #245039 ) ;
#61992 = ORIENTED_EDGE ( 'NONE', *, *, #81559, .F. ) ;
#61991 = DIRECTION ( 'NONE',  ( 1.000000000000000000, -2.952720810173289112E-16, -2.061873921506763405E-30 ) ) ;
#61993 = CARTESIAN_POINT ( 'NONE',  ( 18.59999999999999076, 70.05000000001236060, -159.7174051794895320 ) ) ;
#61994 = ORIENTED_EDGE ( 'NONE', *, *, #92709, .F. ) ;
#61995 = EDGE_CURVE ( 'NONE', #8860, #57378, #93042, .T. ) ;
#61996 = CIRCLE ( 'NONE', #199383, 0.1000000000000028644 ) ;
#61997 = CIRCLE ( 'NONE', #28722, 0.09999999999999939493 ) ;
#61998 = AXIS2_PLACEMENT_3D ( 'NONE', #139360, #98941, #242327 ) ;
#61999 = CIRCLE ( 'NONE', #236969, 11.74999999999999112 ) ;
#62000 = DIRECTION ( 'NONE',  ( 0.000000000000000000, 0.000000000000000000, -1.000000000000000000 ) ) ;
#62001 = VERTEX_POINT ( 'NONE', #24123 ) ;
#62003 = AXIS2_PLACEMENT_3D ( 'NONE', #137127, #172439, #35489 ) ;
#62002 = CARTESIAN_POINT ( 'NONE',  ( 23.24999999999999289, 64.35000000001237197, -169.9231074845244507 ) ) ;
#62004 = CARTESIAN_POINT ( 'NONE',  ( 19.97071067811865674, 64.27928932189384170, -178.8731074845244393 ) ) ;
#62005 = EDGE_CURVE ( 'NONE', #60897, #82258, #76461, .T. ) ;
#62006 = DIRECTION ( 'NONE',  ( 0.000000000000000000, -1.000000000000000000, -6.982962677686265922E-15 ) ) ;
#62007 = DIRECTION ( 'NONE',  ( 0.000000000000000000, 0.000000000000000000, 1.000000000000000000 ) ) ;
#62008 = CARTESIAN_POINT ( 'NONE',  ( -15.15766958671844122, 66.58946139148370946, -188.0904194873835422 ) ) ;
#62010 = VERTEX_POINT ( 'NONE', #159764 ) ;
#62009 = EDGE_CURVE ( 'NONE', #248002, #135164, #163617, .T. ) ;
#62011 = ADVANCED_FACE ( 'NONE', ( #198878 ), #101011, .T. ) ;
#62012 = DIRECTION ( 'NONE',  ( 1.000000000000000000, 0.000000000000000000, 0.000000000000000000 ) ) ;
#62013 = CARTESIAN_POINT ( 'NONE',  ( -1.739115166359751170E-14, 11.65000000001114699, -88.35000000000003695 ) ) ;
#62014 = DIRECTION ( 'NONE',  ( 0.000000000000000000, -0.4088369013363280513, 0.9126074666063769270 ) ) ;
#62015 = ADVANCED_FACE ( 'NONE', ( #5793 ), #13945, .T. ) ;
#62016 = EDGE_LOOP ( 'NONE', ( #548, #96553, #93105, #1202 ) ) ;
#62017 = CARTESIAN_POINT ( 'NONE',  ( 18.50016250449482413, 10.29766095125182268, -105.9743663933279265 ) ) ;
#62020 = ADVANCED_FACE ( 'NONE', ( #244425 ), #145316, .F. ) ;
#62019 = ORIENTED_EDGE ( 'NONE', *, *, #189806, .F. ) ;
#62018 = VECTOR ( 'NONE', #254715, 1000.000000000000000 ) ;
#62021 = DIRECTION ( 'NONE',  ( 1.836970198721029934E-16, -1.000000000000000000, -0.000000000000000000 ) ) ;
#62022 = EDGE_LOOP ( 'NONE', ( #235621, #229857, #181496, #125256 ) ) ;
#62023 = CYLINDRICAL_SURFACE ( 'NONE', #47561, 12.87500000000000178 ) ;
#62024 = DIRECTION ( 'NONE',  ( -1.000000000000000000, -0.000000000000000000, 0.000000000000000000 ) ) ;
#62025 = EDGE_CURVE ( 'NONE', #200161, #252276, #97097, .T. ) ;
#62026 = VERTEX_POINT ( 'NONE', #219717 ) ;
#62027 = ORIENTED_EDGE ( 'NONE', *, *, #105806, .F. ) ;
#62028 = FACE_OUTER_BOUND ( 'NONE', #122574, .T. ) ;
#62029 = ORIENTED_EDGE ( 'NONE', *, *, #193302, .F. ) ;
#62030 = PLANE ( 'NONE',  #52529 ) ;
#62031 = CIRCLE ( 'NONE', #241117, 0.1000000000000028644 ) ;
#62032 = CARTESIAN_POINT ( 'NONE',  ( -20.00857864376270001, 22.38308386859736032, -231.4104522272575082 ) ) ;
#62033 = CIRCLE ( 'NONE', #107806, 11.80000000000000426 ) ;
#62034 = ORIENTED_EDGE ( 'NONE', *, *, #6136, .T. ) ;
#62035 = VERTEX_POINT ( 'NONE', #180607 ) ;
#62036 = CARTESIAN_POINT ( 'NONE',  ( 18.59999999999999787, 77.83534155023646406, -124.9679561919613064 ) ) ;
#62037 = CARTESIAN_POINT ( 'NONE',  ( 21.05000000000000071, 75.90220970870393558, -209.7809220950004772 ) ) ;
#62038 = TOROIDAL_SURFACE ( 'NONE', #207802, 12.77500000000000036, 0.1000000000000000056 ) ;
#62039 = FACE_OUTER_BOUND ( 'NONE', #253387, .T. ) ;
#62040 = VERTEX_POINT ( 'NONE', #240578 ) ;
#62041 = ORIENTED_EDGE ( 'NONE', *, *, #146236, .F. ) ;
#62042 = VECTOR ( 'NONE', #216981, 1000.000000000000227 ) ;
#62043 = EDGE_CURVE ( 'NONE', #44661, #126512, #1944, .T. ) ;
#62044 = CARTESIAN_POINT ( 'NONE',  ( -18.50000000000000000, 7.128833340094563376, -233.7327013124401276 ) ) ;
#62045 = ADVANCED_FACE ( 'NONE', ( #121925 ), #34812, .T. ) ;
#62046 = ADVANCED_FACE ( 'NONE', ( #46219 ), #189608, .F. ) ;
#62048 = ORIENTED_EDGE ( 'NONE', *, *, #184140, .T. ) ;
#62047 = CYLINDRICAL_SURFACE ( 'NONE', #10025, 0.1000000000000013933 ) ;
#62049 = DIRECTION ( 'NONE',  ( 0.000000000000000000, 1.072103779144465041E-14, -1.000000000000000000 ) ) ;
#62050 = AXIS2_PLACEMENT_3D ( 'NONE', #22100, #2499, #204564 ) ;
#62051 = DIRECTION ( 'NONE',  ( 0.000000000000000000, 0.000000000000000000, -1.000000000000000000 ) ) ;
#62052 = CIRCLE ( 'NONE', #11998, 0.09999999999999939493 ) ;
#62053 = CARTESIAN_POINT ( 'NONE',  ( 23.14999999999999858, 0.000000000000000000, -33.50000000000000000 ) ) ;
#62054 = CIRCLE ( 'NONE', #28787, 0.09999999999998898659 ) ;
#62056 = CARTESIAN_POINT ( 'NONE',  ( 22.88900146558018989, 22.38967017749599364, -232.0334904264913973 ) ) ;
#62055 = DIRECTION ( 'NONE',  ( 1.000000000000000000, 0.000000000000000000, 0.000000000000000000 ) ) ;
#62057 = DIRECTION ( 'NONE',  ( -1.000000000000000000, 0.000000000000000000, -0.000000000000000000 ) ) ;
#62058 = CARTESIAN_POINT ( 'NONE',  ( -20.95000000000000284, 17.01923898301589588, -224.3994341343041867 ) ) ;
#62059 = FACE_OUTER_BOUND ( 'NONE', #155097, .T. ) ;
#62060 = CARTESIAN_POINT ( 'NONE',  ( 22.40000000000010161, -3.229117512540232049, -228.1842305956910195 ) ) ;
#62061 = ORIENTED_EDGE ( 'NONE', *, *, #231595, .T. ) ;
#62062 = ORIENTED_EDGE ( 'NONE', *, *, #9101, .T. ) ;
#62063 = CARTESIAN_POINT ( 'NONE',  ( -20.64999999999999858, 7.150000000011155876, -54.65000000000000568 ) ) ;
#62064 = ORIENTED_EDGE ( 'NONE', *, *, #3202, .F. ) ;
#62065 = DIRECTION ( 'NONE',  ( 0.000000000000000000, -0.9553114395362733990, 0.2956011730205631016 ) ) ;
#62066 = EDGE_LOOP ( 'NONE', ( #130141, #46186, #220703, #170892 ) ) ;
#62067 = DIRECTION ( 'NONE',  ( 0.000000000000000000, 0.000000000000000000, -1.000000000000000000 ) ) ;
#62069 = VERTEX_POINT ( 'NONE', #128351 ) ;
#62068 = ORIENTED_EDGE ( 'NONE', *, *, #197, .F. ) ;
#62070 = ORIENTED_EDGE ( 'NONE', *, *, #207683, .F. ) ;
#62071 = ORIENTED_EDGE ( 'NONE', *, *, #82288, .T. ) ;
#62072 = DIRECTION ( 'NONE',  ( -1.000000000000000000, 0.000000000000000000, 0.000000000000000000 ) ) ;
#62073 = CARTESIAN_POINT ( 'NONE',  ( -16.81744102076749314, 9.950000000011142376, -46.15000000000000568 ) ) ;
#62075 = VERTEX_POINT ( 'NONE', #47494 ) ;
#62074 = CARTESIAN_POINT ( 'NONE',  ( -21.14999999999999858, 30.73075574124490572, -252.3164853687435709 ) ) ;
#62076 = CARTESIAN_POINT ( 'NONE',  ( 20.85882249326303040, 65.66751761918668251, -97.42826094061121012 ) ) ;
#62078 = ORIENTED_EDGE ( 'NONE', *, *, #185770, .F. ) ;
#62077 = CARTESIAN_POINT ( 'NONE',  ( -18.50000000000000000, -26.43935341558978891, -85.14150860750750383 ) ) ;
#62079 = DIRECTION ( 'NONE',  ( -0.000000000000000000, 0.9770955615653313941, 0.2128009952263603954 ) ) ;
#62080 = ORIENTED_EDGE ( 'NONE', *, *, #87330, .T. ) ;
#62081 = CARTESIAN_POINT ( 'NONE',  ( 20.85000000000000142, 76.00000000001142553, -36.02310748452432421 ) ) ;
#62083 = ORIENTED_EDGE ( 'NONE', *, *, #95603, .T. ) ;
#62082 = CARTESIAN_POINT ( 'NONE',  ( 6.000000000000060396, 64.35000000001120668, -25.92310748452479174 ) ) ;
#62084 = DIRECTION ( 'NONE',  ( -2.952720810173289112E-16, -1.000000000000000000, -6.982962677686266711E-15 ) ) ;
#62086 = EDGE_CURVE ( 'NONE', #234302, #216880, #117989, .T. ) ;
#62085 = CARTESIAN_POINT ( 'NONE',  ( 21.97500000000000497, 66.25000000001207923, -124.2731074845243597 ) ) ;
#62087 = CARTESIAN_POINT ( 'NONE',  ( 20.94999999999999929, 11.63687328911533392, -60.17824078667518961 ) ) ;
#62088 = ORIENTED_EDGE ( 'NONE', *, *, #63465, .T. ) ;
#62089 = CIRCLE ( 'NONE', #103744, 0.09999999999999939493 ) ;
#62092 = DIRECTION ( 'NONE',  ( 1.000000000000000000, 0.000000000000000000, 0.000000000000000000 ) ) ;
#62091 = AXIS2_PLACEMENT_3D ( 'NONE', #97959, #1446, #78415 ) ;
#62090 = CARTESIAN_POINT ( 'NONE',  ( -17.01764560440454588, 9.950000000011138823, -121.2500000007868408 ) ) ;
#62094 = ADVANCED_FACE ( 'NONE', ( #26692 ), #188304, .T. ) ;
#62093 = CARTESIAN_POINT ( 'NONE',  ( -12.33960340485503870, 66.63925083009671368, -85.70853734391708656 ) ) ;
#62095 = VECTOR ( 'NONE', #194024, 1000.000000000000000 ) ;
#62096 = AXIS2_PLACEMENT_3D ( 'NONE', #208023, #9799, #51465 ) ;
#62097 = CARTESIAN_POINT ( 'NONE',  ( -20.85000000000000142, 6.933893972137497030, -104.2856458343736250 ) ) ;
#62098 = DIRECTION ( 'NONE',  ( 1.000000000000000000, 0.000000000000000000, 0.000000000000000000 ) ) ;
#62099 = ORIENTED_EDGE ( 'NONE', *, *, #26350, .T. ) ;
#62100 = ORIENTED_EDGE ( 'NONE', *, *, #218095, .T. ) ;
#62101 = EDGE_LOOP ( 'NONE', ( #64753, #229174, #216647, #34550 ) ) ;
#62102 = EDGE_CURVE ( 'NONE', #135871, #52558, #214038, .T. ) ;
#62103 = DIRECTION ( 'NONE',  ( 2.694716079187273439E-16, 1.000000000000000000, 6.467318590049456648E-15 ) ) ;
#62104 = AXIS2_PLACEMENT_3D ( 'NONE', #8271, #87771, #68235 ) ;
#62105 = ADVANCED_FACE ( 'NONE', ( #27989 ), #227635, .T. ) ;
#62106 = VERTEX_POINT ( 'NONE', #170082 ) ;
#62107 = LINE ( 'NONE', #223722, #251759 ) ;
#62108 = ORIENTED_EDGE ( 'NONE', *, *, #16240, .F. ) ;
#62109 = CARTESIAN_POINT ( 'NONE',  ( 20.04142135623730070, 64.35000000001180354, -81.67310748452439384 ) ) ;
#62110 = FACE_OUTER_BOUND ( 'NONE', #107121, .T. ) ;
#62111 = CIRCLE ( 'NONE', #82914, 0.09999999999999939493 ) ;
#62112 = CIRCLE ( 'NONE', #253624, 0.1000000000000024342 ) ;
#62113 = ORIENTED_EDGE ( 'NONE', *, *, #71554, .T. ) ;
#62114 = CARTESIAN_POINT ( 'NONE',  ( 12.93279065517211635, 9.417690691074255938, -152.1416006967646695 ) ) ;
#62115 = PRESENTATION_STYLE_ASSIGNMENT (( #103770 ) ) ;
#62116 = ORIENTED_EDGE ( 'NONE', *, *, #201323, .T. ) ;
#62118 = ADVANCED_FACE ( 'NONE', ( #107485 ), #226120, .T. ) ;
#62117 = AXIS2_PLACEMENT_3D ( 'NONE', #17225, #138407, #194590 ) ;
#62119 = ORIENTED_EDGE ( 'NONE', *, *, #83397, .F. ) ;
#62120 = EDGE_CURVE ( 'NONE', #93493, #183016, #50078, .T. ) ;
#62121 = ORIENTED_EDGE ( 'NONE', *, *, #232868, .T. ) ;
#62122 = CARTESIAN_POINT ( 'NONE',  ( -23.25000000000000355, 9.950000000011138823, -176.7499999999999716 ) ) ;
#62123 = CARTESIAN_POINT ( 'NONE',  ( 22.47809213839789066, 75.96246293238424130, -215.1730808193121618 ) ) ;
#62124 = DIRECTION ( 'NONE',  ( 6.938893903907991995E-14, 0.000000000000000000, 1.000000000000000000 ) ) ;
#62125 = DIRECTION ( 'NONE',  ( 0.000000000000000000, 0.000000000000000000, 1.000000000000000000 ) ) ;
#62126 = CYLINDRICAL_SURFACE ( 'NONE', #35880, 0.1000000000000026007 ) ;
#62127 = PLANE ( 'NONE',  #155327 ) ;
#62129 = CARTESIAN_POINT ( 'NONE',  ( -20.54999999999999716, 76.00000000001244871, -170.0231074845243597 ) ) ;
#62128 = DIRECTION ( 'NONE',  ( 0.000000000000000000, 0.9651348961777157509, -0.2617529984165031243 ) ) ;
#62130 = DIRECTION ( 'NONE',  ( 0.000000000000000000, 0.1350103645451945777, -0.9908441862701589109 ) ) ;
#62132 = EDGE_LOOP ( 'NONE', ( #189944, #110259, #177218, #246173 ) ) ;
#62131 = DIRECTION ( 'NONE',  ( 0.000000000000000000, -6.938893903907222067E-15, 1.000000000000000000 ) ) ;
#62133 = DIRECTION ( 'NONE',  ( 0.000000000000000000, 0.000000000000000000, -1.000000000000000000 ) ) ;
#62134 = DIRECTION ( 'NONE',  ( 0.000000000000000000, 0.9908441862701782288, 0.1350103645450542456 ) ) ;
#62135 = VERTEX_POINT ( 'NONE', #227429 ) ;
#62136 = LINE ( 'NONE', #120854, #187882 ) ;
#62137 = CARTESIAN_POINT ( 'NONE',  ( -21.10257677756356642, 69.60161825747893261, -69.54805823409236609 ) ) ;
#62138 = CARTESIAN_POINT ( 'NONE',  ( -16.87683809663752399, 9.850000000011144508, -46.90236401819630885 ) ) ;
#62139 = ORIENTED_EDGE ( 'NONE', *, *, #177151, .T. ) ;
#62140 = EDGE_CURVE ( 'NONE', #59451, #246280, #122466, .T. ) ;
#62141 = EDGE_CURVE ( 'NONE', #45900, #64483, #230613, .T. ) ;
#62142 = AXIS2_PLACEMENT_3D ( 'NONE', #143671, #163259, #165833 ) ;
#62143 = CARTESIAN_POINT ( 'NONE',  ( 22.39999999999999503, -2.576749817950531707, -189.6385361693310756 ) ) ;
#62144 = ORIENTED_EDGE ( 'NONE', *, *, #119255, .T. ) ;
#62145 = EDGE_LOOP ( 'NONE', ( #122694, #193879, #250915, #2779, #196969 ) ) ;
#62146 = DIRECTION ( 'NONE',  ( -1.000000000000000000, -0.000000000000000000, -0.000000000000000000 ) ) ;
#62147 = VERTEX_POINT ( 'NONE', #210459 ) ;
#62148 = DIRECTION ( 'NONE',  ( 0.000000000000000000, 0.2128009952263237581, -0.9770955615653394988 ) ) ;
#62150 = DIRECTION ( 'NONE',  ( 1.000000000000000000, 0.000000000000000000, 0.000000000000000000 ) ) ;
#62149 = AXIS2_PLACEMENT_3D ( 'NONE', #32276, #213442, #251281 ) ;
#62151 = CARTESIAN_POINT ( 'NONE',  ( -23.25000000000000000, 74.44087353924872730, -232.6253149859214773 ) ) ;
#62153 = ADVANCED_FACE ( 'NONE', ( #48793 ), #234891, .T. ) ;
#62152 = LINE ( 'NONE', #139077, #146769 ) ;
#62154 = ORIENTED_EDGE ( 'NONE', *, *, #73750, .F. ) ;
#62155 = CARTESIAN_POINT ( 'NONE',  ( -23.15000000000000213, 87.39257802171759693, -106.0970570643561501 ) ) ;
#62156 = PLANE ( 'NONE',  #241372 ) ;
#62158 = EDGE_CURVE ( 'NONE', #248221, #253904, #114056, .T. ) ;
#62157 = CARTESIAN_POINT ( 'NONE',  ( 18.49999999999999289, 10.41716543472752399, -192.3499999994177472 ) ) ;
#62159 = CARTESIAN_POINT ( 'NONE',  ( 21.05000000000000071, 1.115600667400684642E-11, -169.5000000000000284 ) ) ;
#62160 = TOROIDAL_SURFACE ( 'NONE', #16381, 0.2000000000000000111, 0.1000000000000000056 ) ;
#62161 = VECTOR ( 'NONE', #70882, 1000.000000000000000 ) ;
#62162 = ORIENTED_EDGE ( 'NONE', *, *, #210439, .F. ) ;
#62163 = CIRCLE ( 'NONE', #37226, 11.64999999999999325 ) ;
#62165 = ORIENTED_EDGE ( 'NONE', *, *, #90000, .T. ) ;
#62164 = LINE ( 'NONE', #197807, #50354 ) ;
#62166 = DIRECTION ( 'NONE',  ( 0.000000000000000000, 0.000000000000000000, 1.000000000000000000 ) ) ;
#62167 = CARTESIAN_POINT ( 'NONE',  ( -21.05000000000000071, 34.10074028454091177, -243.7884649046354184 ) ) ;
#62168 = ADVANCED_FACE ( 'NONE', ( #230002 ), #130900, .F. ) ;
#62169 = CARTESIAN_POINT ( 'NONE',  ( 20.90000000000000213, -1.410778198689825347, -7.973296578895943121 ) ) ;
#62170 = DIRECTION ( 'NONE',  ( 0.000000000000000000, 0.000000000000000000, 1.000000000000000000 ) ) ;
#62171 = AXIS2_PLACEMENT_3D ( 'NONE', #158063, #175061, #137163 ) ;
#62172 = CARTESIAN_POINT ( 'NONE',  ( 18.50000000000000000, -10.35479209691423996, -94.25654098307380480 ) ) ;
#62173 = CARTESIAN_POINT ( 'NONE',  ( -20.64999999999999858, 71.75000000001186606, -90.67310748452433700 ) ) ;
#62174 = AXIS2_PLACEMENT_3D ( 'NONE', #200434, #80440, #41384 ) ;
#62175 = ORIENTED_EDGE ( 'NONE', *, *, #73337, .F. ) ;
#62176 = CARTESIAN_POINT ( 'NONE',  ( -16.86445178670725653, 63.08462010037012391, -213.0850694278881008 ) ) ;
#62177 = ADVANCED_FACE ( 'NONE', ( #153083 ), #36976, .T. ) ;
#62178 = CARTESIAN_POINT ( 'NONE',  ( -23.25000000000000000, -11.64999999998884483, -97.40000000000004832 ) ) ;
#62179 = CARTESIAN_POINT ( 'NONE',  ( -22.45437739390953880, -1.124859753953710850E-15, 11.64957081159447405 ) ) ;
#62180 = DIRECTION ( 'NONE',  ( -1.836970198721029934E-16, -1.000000000000000000, -6.982962677686266711E-15 ) ) ;
#62181 = DIRECTION ( 'NONE',  ( 0.000000000000000000, 1.000000000000000000, 1.387778780781444413E-14 ) ) ;
#62182 = CARTESIAN_POINT ( 'NONE',  ( 20.84451136049642272, 65.37985808520329556, -62.02918292499334285 ) ) ;
#62183 = TOROIDAL_SURFACE ( 'NONE', #141281, 4.099999999999999645, 0.1000000000000000056 ) ;
#62184 = AXIS2_PLACEMENT_3D ( 'NONE', #130178, #209735, #110627 ) ;
#62185 = ORIENTED_EDGE ( 'NONE', *, *, #94363, .T. ) ;
#62186 = ORIENTED_EDGE ( 'NONE', *, *, #168070, .T. ) ;
#62187 = DIRECTION ( 'NONE',  ( 0.000000000000000000, 6.982962677686266711E-15, -1.000000000000000000 ) ) ;
#62188 = CIRCLE ( 'NONE', #20506, 0.1000000000000046685 ) ;
#62189 = DIRECTION ( 'NONE',  ( 0.000000000000000000, 0.3848449534832868446, 0.9229812358755982160 ) ) ;
#62190 = DIRECTION ( 'NONE',  ( -1.000000000000000000, 1.836970198721029934E-16, 1.282749433769087582E-30 ) ) ;
#62191 = DIRECTION ( 'NONE',  ( 0.000000000000000000, 0.000000000000000000, -1.000000000000000000 ) ) ;
#62192 = CIRCLE ( 'NONE', #132932, 0.3999999999999975797 ) ;
#62193 = VERTEX_POINT ( 'NONE', #112632 ) ;
#62194 = CARTESIAN_POINT ( 'NONE',  ( -18.45068461519104375, 46.98837717972348571, -255.3186424377302899 ) ) ;
#62195 = DIRECTION ( 'NONE',  ( -0.000000000000000000, 1.000000000000000000, -0.000000000000000000 ) ) ;
#62196 = DIRECTION ( 'NONE',  ( 1.000000000000000000, 0.000000000000000000, 0.000000000000000000 ) ) ;
#62197 = PRODUCT_DEFINITION_SHAPE ( 'NONE', 'NONE',  #258136 ) ;
#62198 = CARTESIAN_POINT ( 'NONE',  ( -20.00857864376270001, 9.250000000011157297, -54.75000000000000000 ) ) ;
#62199 = VECTOR ( 'NONE', #124430, 1000.000000000000227 ) ;
#62200 = ORIENTED_EDGE ( 'NONE', *, *, #23443, .T. ) ;
#62201 = DIRECTION ( 'NONE',  ( 0.000000000000000000, 0.000000000000000000, 1.000000000000000000 ) ) ;
#62202 = VERTEX_POINT ( 'NONE', #194759 ) ;
#62203 = DIRECTION ( 'NONE',  ( -1.000000000000000000, -0.000000000000000000, -0.000000000000000000 ) ) ;
#62204 = LINE ( 'NONE', #100005, #104819 ) ;
#62205 = CARTESIAN_POINT ( 'NONE',  ( -21.05000000000045546, 10.18563131712793357, -228.0635015899710254 ) ) ;
#62206 = CARTESIAN_POINT ( 'NONE',  ( 20.94999999999999929, 6.550000000011156231, -144.0170271704400307 ) ) ;
#62207 = CARTESIAN_POINT ( 'NONE',  ( 20.94999999999999929, 64.32322888843472697, -213.0487915999076449 ) ) ;
#62208 = CARTESIAN_POINT ( 'NONE',  ( 20.95262331984796234, 18.75370877634653155, -228.0435341303648897 ) ) ;
#62209 = DIRECTION ( 'NONE',  ( 0.000000000000000000, -6.982962677686266711E-15, 1.000000000000000000 ) ) ;
#62210 = CARTESIAN_POINT ( 'NONE',  ( 21.00000000000000000, 9.750000000011153745, -155.2500000000000284 ) ) ;
#62211 = CIRCLE ( 'NONE', #53831, 0.09999999999999939493 ) ;
#62212 = CARTESIAN_POINT ( 'NONE',  ( -22.47007471830798764, 7.720710651937634061, -67.00000000000004263 ) ) ;
#62213 = DIRECTION ( 'NONE',  ( 0.000000000000000000, 0.000000000000000000, 1.000000000000000000 ) ) ;
#62214 = ADVANCED_FACE ( 'NONE', ( #98159 ), #232604, .T. ) ;
#62215 = AXIS2_PLACEMENT_3D ( 'NONE', #188137, #234647, #246810 ) ;
#62216 = DIRECTION ( 'NONE',  ( -1.000000000000000000, 1.836970198721029934E-16, 1.601412966608202925E-30 ) ) ;
#62217 = DIRECTION ( 'NONE',  ( -0.000000000000000000, 0.9126074666063769270, 0.4088369013363280513 ) ) ;
#62218 = CYLINDRICAL_SURFACE ( 'NONE', #220272, 0.09999999999999939493 ) ;
#62219 = CARTESIAN_POINT ( 'NONE',  ( 20.96077737575334865, 56.21923056145944742, -228.0513653586724274 ) ) ;
#62220 = AXIS2_PLACEMENT_3D ( 'NONE', #133320, #193301, #52469 ) ;
#62221 = EDGE_LOOP ( 'NONE', ( #24769, #80841, #95971, #181342, #66476 ) ) ;
#62222 = DIRECTION ( 'NONE',  ( 0.000000000000000000, 1.000000000000000000, 6.982962677686266711E-15 ) ) ;
#62223 = DIRECTION ( 'NONE',  ( -0.000000000000000000, -6.982962677686266711E-15, 1.000000000000000000 ) ) ;
#62224 = ADVANCED_FACE ( 'NONE', ( #172655 ), #193465, .T. ) ;
#62225 = ORIENTED_EDGE ( 'NONE', *, *, #207196, .T. ) ;
#62226 = FACE_OUTER_BOUND ( 'NONE', #28031, .T. ) ;
#62228 = EDGE_CURVE ( 'NONE', #103673, #136601, #13537, .T. ) ;
#62227 = CIRCLE ( 'NONE', #116412, 0.1000000000000028644 ) ;
#62229 = CARTESIAN_POINT ( 'NONE',  ( -17.80356949364000130, 10.87673139701363745, -190.7130730242347738 ) ) ;
#62230 = CIRCLE ( 'NONE', #124594, 0.09999999999999939493 ) ;
#62231 = ORIENTED_EDGE ( 'NONE', *, *, #182163, .T. ) ;
#62232 = CARTESIAN_POINT ( 'NONE',  ( -18.59999999999999787, 11.65000000001115232, -107.5148057706540357 ) ) ;
#62233 = DIRECTION ( 'NONE',  ( 0.000000000000000000, 0.000000000000000000, -1.000000000000000000 ) ) ;
#62234 = ORIENTED_EDGE ( 'NONE', *, *, #131124, .F. ) ;
#62235 = AXIS2_PLACEMENT_3D ( 'NONE', #204129, #224967, #85441 ) ;
#62236 = EDGE_LOOP ( 'NONE', ( #10394, #77926, #224262, #115489 ) ) ;
#62237 = DIRECTION ( 'NONE',  ( 0.000000000000000000, -0.2128009952263403282, 0.9770955615653358350 ) ) ;
#62238 = EDGE_CURVE ( 'NONE', #5593, #141892, #35011, .T. ) ;
#62239 = ORIENTED_EDGE ( 'NONE', *, *, #195812, .T. ) ;
#62240 = ADVANCED_FACE ( 'NONE', ( #115196 ), #176474, .T. ) ;
#62241 = LINE ( 'NONE', #144307, #158220 ) ;
#62242 = DIRECTION ( 'NONE',  ( 0.000000000000000000, 0.9770955615653316162, 0.2128009952263604232 ) ) ;
#62243 = CARTESIAN_POINT ( 'NONE',  ( 23.25000000000000000, 73.42097182497056451, -249.7082903213649558 ) ) ;
#62244 = CARTESIAN_POINT ( 'NONE',  ( 18.49999999999999645, 76.00000000001244871, -170.0231074845243597 ) ) ;
#62245 = CARTESIAN_POINT ( 'NONE',  ( -16.84981964351479533, 66.08268176591360543, -157.1535058705049153 ) ) ;
#62246 = DIRECTION ( 'NONE',  ( 1.000000000000000000, 0.000000000000000000, 0.000000000000000000 ) ) ;
#62247 = DIRECTION ( 'NONE',  ( 1.000000000000000000, 0.000000000000000000, 0.000000000000000000 ) ) ;
#62248 = DIRECTION ( 'NONE',  ( 0.000000000000000000, -6.517943393102682774E-15, 1.000000000000000000 ) ) ;
#62250 = ORIENTED_EDGE ( 'NONE', *, *, #36675, .F. ) ;
#62249 = CARTESIAN_POINT ( 'NONE',  ( -18.60000000000000142, -9.321008403350132809, -40.73593824907788274 ) ) ;
#62251 = ORIENTED_EDGE ( 'NONE', *, *, #159213, .F. ) ;
#62253 = CARTESIAN_POINT ( 'NONE',  ( 18.59999999999997655, -1.164121893230052995, -108.4148480855716485 ) ) ;
#62252 = AXIS2_PLACEMENT_3D ( 'NONE', #91105, #213611, #251457 ) ;
#62255 = VERTEX_POINT ( 'NONE', #175219 ) ;
#62254 = DIRECTION ( 'NONE',  ( 0.000000000000000000, 0.000000000000000000, 1.000000000000000000 ) ) ;
#62256 = ORIENTED_EDGE ( 'NONE', *, *, #173338, .F. ) ;
#62257 = DIRECTION ( 'NONE',  ( 1.000000000000000000, 0.000000000000000000, 0.000000000000000000 ) ) ;
#62258 = LINE ( 'NONE', #162652, #180245 ) ;
#62259 = EDGE_CURVE ( 'NONE', #231766, #24249, #55180, .T. ) ;
#62260 = CARTESIAN_POINT ( 'NONE',  ( -23.15000000000000213, 71.85000000001151932, -48.37310748452435405 ) ) ;
#62261 = DIRECTION ( 'NONE',  ( 0.000000000000000000, 0.000000000000000000, 1.000000000000000000 ) ) ;
#62262 = CARTESIAN_POINT ( 'NONE',  ( 20.94999999999999929, 76.00000000001142553, -36.02310748452432421 ) ) ;
#62263 = DIRECTION ( 'NONE',  ( 0.000000000000000000, -1.000000000000000000, 0.000000000000000000 ) ) ;
#62264 = ADVANCED_FACE ( 'NONE', ( #116485 ), #173936, .T. ) ;
#62265 = CARTESIAN_POINT ( 'NONE',  ( -18.50000000000000000, 12.76524917372336532, -223.4223513401831553 ) ) ;
#62266 = CIRCLE ( 'NONE', #108070, 0.1000000000000001305 ) ;
#62267 = ORIENTED_EDGE ( 'NONE', *, *, #114152, .T. ) ;
#62268 = ORIENTED_EDGE ( 'NONE', *, *, #106080, .T. ) ;
#62269 = VECTOR ( 'NONE', #140656, 1000.000000000000000 ) ;
#62270 = CIRCLE ( 'NONE', #141372, 1.900000000000012790 ) ;
#62271 = TOROIDAL_SURFACE ( 'NONE', #78987, 11.65000000000000036, 0.1000000000000000056 ) ;
#62272 = ORIENTED_EDGE ( 'NONE', *, *, #226404, .T. ) ;
#62273 = CARTESIAN_POINT ( 'NONE',  ( 21.05000000000000071, -0.08559286335111393473, -27.08633726513048856 ) ) ;
#62274 = ORIENTED_EDGE ( 'NONE', *, *, #197223, .F. ) ;
#62275 = CARTESIAN_POINT ( 'NONE',  ( -13.39999999999999858, -8.279289321881348584, 11.02928932188134503 ) ) ;
#62276 = AXIS2_PLACEMENT_3D ( 'NONE', #113467, #58617, #213858 ) ;
#62277 = CARTESIAN_POINT ( 'NONE',  ( -15.75000000000001066, 48.22675593180858300, -234.1235479764714853 ) ) ;
#62278 = DIRECTION ( 'NONE',  ( -1.000000000000000000, 0.000000000000000000, 0.000000000000000000 ) ) ;
#62279 = ORIENTED_EDGE ( 'NONE', *, *, #10938, .F. ) ;
#62280 = DIRECTION ( 'NONE',  ( 0.000000000000000000, -6.982962677686266711E-15, 1.000000000000000000 ) ) ;
#62281 = ORIENTED_EDGE ( 'NONE', *, *, #201541, .F. ) ;
#62283 = FACE_OUTER_BOUND ( 'NONE', #250825, .T. ) ;
#62282 = CIRCLE ( 'NONE', #244876, 0.09999999999998898659 ) ;
#62284 = VECTOR ( 'NONE', #174450, 1000.000000000000000 ) ;
#62285 = DIRECTION ( 'NONE',  ( 0.000000000000000000, -0.9667078373770112698, -0.2558827019434132821 ) ) ;
#62287 = CIRCLE ( 'NONE', #170678, 0.09999999999999939493 ) ;
#62286 = CARTESIAN_POINT ( 'NONE',  ( -14.00000000000000178, 66.15000000001228386, -153.2731074845244166 ) ) ;
#62288 = LINE ( 'NONE', #20617, #69949 ) ;
#62289 = ORIENTED_EDGE ( 'NONE', *, *, #52345, .T. ) ;
#62290 = CYLINDRICAL_SURFACE ( 'NONE', #144293, 0.09999999999999939493 ) ;
#62291 = EDGE_LOOP ( 'NONE', ( #20664, #85539, #231077, #146394 ) ) ;
#62294 = VERTEX_POINT ( 'NONE', #18662 ) ;
#62293 = DIRECTION ( 'NONE',  ( 1.000000000000000000, -0.000000000000000000, -0.000000000000000000 ) ) ;
#62292 = CYLINDRICAL_SURFACE ( 'NONE', #240686, 0.1000000000000101225 ) ;
#62295 = AXIS2_PLACEMENT_3D ( 'NONE', #118244, #238174, #211253 ) ;
#62296 = DIRECTION ( 'NONE',  ( -2.952720810173288126E-16, 0.9770955615653313941, 0.2128009952263603677 ) ) ;
#62297 = VERTEX_POINT ( 'NONE', #93056 ) ;
#62298 = ADVANCED_FACE ( 'NONE', ( #17383 ), #254661, .F. ) ;
#62299 = DIRECTION ( 'NONE',  ( -1.000000000000000000, 0.000000000000000000, -0.000000000000000000 ) ) ;
#62300 = ORIENTED_EDGE ( 'NONE', *, *, #140414, .T. ) ;
#62302 = ADVANCED_FACE ( 'NONE', ( #151780 ), #155793, .T. ) ;
#62301 = CARTESIAN_POINT ( 'NONE',  ( -23.15000000000000213, 67.23127455305835554, -235.8551265064784559 ) ) ;
#62304 = CARTESIAN_POINT ( 'NONE',  ( -16.93353400591625757, 10.00461239618409515, -54.43268447020540890 ) ) ;
#62303 =( BOUNDED_SURFACE ( )  B_SPLINE_SURFACE ( 3, 2, ( 
 ( #62643, #198287, #78 ),
 ( #39247, #200861, #22243 ),
 ( #239998, #181318, #221683 ),
 ( #180029, #41813, #2646 ) ),
 .UNSPECIFIED., .F., .F., .F. ) 
 B_SPLINE_SURFACE_WITH_KNOTS ( ( 4, 4 ),
 ( 3, 3 ),
 ( 3.550762114890027021E-18, 0.0003124336600439677055 ),
 ( 0.000000000000000000, 1.000000000000000000 ),
 .UNSPECIFIED. ) 
 GEOMETRIC_REPRESENTATION_ITEM ( )  RATIONAL_B_SPLINE_SURFACE ( (
 ( 1.000000000000000000, 0.7071067811865475727, 1.000000000000000000),
 ( 1.000000000000000000, 0.7089187706049929760, 1.000000000000000000),
 ( 1.000000000000000000, 0.7039288185051876257, 1.000000000000000000),
 ( 1.000000000000000000, 0.7040654476015342222, 1.000000000000000000) ) ) 
 REPRESENTATION_ITEM ( '' )  SURFACE ( )  );
#62305 = EDGE_CURVE ( 'NONE', #243146, #159674, #109972, .T. ) ;
#62306 = CARTESIAN_POINT ( 'NONE',  ( 20.85000000000000142, 77.26327546522911405, -95.12124281777788326 ) ) ;
#62307 = EDGE_CURVE ( 'NONE', #62686, #17722, #159884, .T. ) ;
#62308 = UNCERTAINTY_MEASURE_WITH_UNIT (LENGTH_MEASURE( 1.000000000000000082E-05 ), #137322, 'distance_accuracy_value', 'NONE');
#62309 = ORIENTED_EDGE ( 'NONE', *, *, #14549, .T. ) ;
#62310 = LINE ( 'NONE', #105235, #47692 ) ;
#62312 = EDGE_LOOP ( 'NONE', ( #71898, #188173, #96314, #46335 ) ) ;
#62311 = EDGE_CURVE ( 'NONE', #80704, #124622, #156920, .T. ) ;
#62313 = DIRECTION ( 'NONE',  ( 1.000000000000000000, 0.000000000000000000, 0.000000000000000000 ) ) ;
#62314 = CARTESIAN_POINT ( 'NONE',  ( -16.94275863006528482, 9.989496048678669027, -188.3916973820765293 ) ) ;
#62315 = CARTESIAN_POINT ( 'NONE',  ( -14.23072895065543975, 66.54401276639954688, -155.0115763176265489 ) ) ;
#62316 = AXIS2_PLACEMENT_3D ( 'NONE', #225450, #222894, #168118 ) ;
#62317 = EDGE_CURVE ( 'NONE', #238459, #14749, #68298, .T. ) ;
#62318 = EDGE_LOOP ( 'NONE', ( #169794, #219290, #112345, #12538, #67977 ) ) ;
#62319 = DIRECTION ( 'NONE',  ( 0.000000000000000000, -0.000000000000000000, 1.000000000000000000 ) ) ;
#62322 = EDGE_CURVE ( 'NONE', #11158, #214793, #255675, .T. ) ;
#62321 = EDGE_CURVE ( 'NONE', #235986, #246004, #163319, .T. ) ;
#62320 = ORIENTED_EDGE ( 'NONE', *, *, #104652, .F. ) ;
#62323 = CARTESIAN_POINT ( 'NONE',  ( -20.94999999999999929, 10.29270135741298731, -172.9573618871519614 ) ) ;
#62324 = DIRECTION ( 'NONE',  ( 0.000000000000000000, 0.000000000000000000, 1.000000000000000000 ) ) ;
#62325 = DIRECTION ( 'NONE',  ( 0.000000000000000000, 1.000000000000000000, 0.000000000000000000 ) ) ;
#62326 = VECTOR ( 'NONE', #147725, 1000.000000000000000 ) ;
#62328 = VERTEX_POINT ( 'NONE', #162046 ) ;
#62327 = DIRECTION ( 'NONE',  ( -0.8049926720990043805, 0.5725998182664988612, -0.1552940629517997051 ) ) ;
#62329 = CARTESIAN_POINT ( 'NONE',  ( 20.46382478191414833, 11.98971155215881801, -206.2465614625865271 ) ) ;
#62330 = DIRECTION ( 'NONE',  ( -1.000000000000000000, -0.000000000000000000, -0.000000000000000000 ) ) ;
#62331 = EDGE_CURVE ( 'NONE', #121939, #162201, #218105, .T. ) ;
#62332 = DIRECTION ( 'NONE',  ( 1.000000000000000000, 0.000000000000000000, 0.000000000000000000 ) ) ;
#62333 = VERTEX_POINT ( 'NONE', #240289 ) ;
#62334 = LINE ( 'NONE', #178457, #205708 ) ;
#62335 = FACE_OUTER_BOUND ( 'NONE', #245494, .T. ) ;
#62337 = ORIENTED_EDGE ( 'NONE', *, *, #220248, .F. ) ;
#62336 = EDGE_CURVE ( 'NONE', #231733, #173596, #138976, .T. ) ;
#62339 = EDGE_CURVE ( 'NONE', #114911, #114550, #47422, .T. ) ;
#62338 = DIRECTION ( 'NONE',  ( 1.000000000000000000, -0.000000000000000000, -0.000000000000000000 ) ) ;
#62340 = CIRCLE ( 'NONE', #95637, 0.1000000000000055844 ) ;
#62341 = AXIS2_PLACEMENT_3D ( 'NONE', #202377, #161992, #223208 ) ;
#62342 = EDGE_LOOP ( 'NONE', ( #122418, #227657, #152881, #7809 ) ) ;
#62343 = EDGE_CURVE ( 'NONE', #155708, #215605, #139873, .T. ) ;
#62344 = CARTESIAN_POINT ( 'NONE',  ( -21.05000000000000071, 74.83729825007431202, -161.9231074845243654 ) ) ;
#62345 = VERTEX_POINT ( 'NONE', #104586 ) ;
#62347 = ORIENTED_EDGE ( 'NONE', *, *, #140288, .T. ) ;
#62346 = DIRECTION ( 'NONE',  ( -1.000000000000000000, 0.000000000000000000, 0.000000000000000000 ) ) ;
#62348 = CIRCLE ( 'NONE', #221110, 0.09999999999999939493 ) ;
#62349 = EDGE_CURVE ( 'NONE', #210574, #45940, #179055, .T. ) ;
#62350 = CIRCLE ( 'NONE', #4082, 4.099999999999999645 ) ;
#62353 = ORIENTED_EDGE ( 'NONE', *, *, #167206, .F. ) ;
#62352 = ORIENTED_EDGE ( 'NONE', *, *, #77474, .T. ) ;
#62351 = DIRECTION ( 'NONE',  ( 0.000000000000000000, 0.000000000000000000, 1.000000000000000000 ) ) ;
#62354 = CYLINDRICAL_SURFACE ( 'NONE', #207885, 0.1000000000000018374 ) ;
#62355 = CARTESIAN_POINT ( 'NONE',  ( -20.85000000000000142, 65.66751761918619934, -30.42826094061123854 ) ) ;
#62357 = CARTESIAN_POINT ( 'NONE',  ( -16.92778301347278358, 10.00094491683526066, -20.92851810796845413 ) ) ;
#62356 = CARTESIAN_POINT ( 'NONE',  ( 20.93302460841142931, 46.41023286455059349, -243.0722154975327385 ) ) ;
#62358 = CARTESIAN_POINT ( 'NONE',  ( 23.25000000000000000, 87.75000000001186606, -90.87310748452424036 ) ) ;
#62359 = FACE_OUTER_BOUND ( 'NONE', #205625, .T. ) ;
#62360 = CIRCLE ( 'NONE', #174839, 4.300000000000025580 ) ;
#62361 = FACE_OUTER_BOUND ( 'NONE', #58751, .T. ) ;
#62363 = CARTESIAN_POINT ( 'NONE',  ( -18.50000000000000000, -26.43935341558978891, -152.1415086075074896 ) ) ;
#62362 = DIRECTION ( 'NONE',  ( 1.000000000000000000, 0.000000000000000000, 0.000000000000000000 ) ) ;
#62364 = VECTOR ( 'NONE', #58326, 1000.000000000000000 ) ;
#62365 = ORIENTED_EDGE ( 'NONE', *, *, #58508, .F. ) ;
#62366 = COLOUR_RGB ( '', 0.66274510, 0.83137255, 0.94901961) ;
#62368 = ORIENTED_EDGE ( 'NONE', *, *, #158967, .F. ) ;
#62367 = CIRCLE ( 'NONE', #216477, 0.09999999999999939493 ) ;
#62369 = DIRECTION ( 'NONE',  ( 1.000000000000000000, -0.000000000000000000, 0.000000000000000000 ) ) ;
#62371 = VERTEX_POINT ( 'NONE', #180306 ) ;
#62370 = DIRECTION ( 'NONE',  ( 0.000000000000000000, -1.000000000000000000, -8.609265936414504429E-15 ) ) ;
#62372 = EDGE_LOOP ( 'NONE', ( #139940, #23893, #210272, #124538 ) ) ;
#62373 = CARTESIAN_POINT ( 'NONE',  ( 21.07094088545303734, 6.320167221927647461, -100.4011062974478250 ) ) ;
#62374 = EDGE_LOOP ( 'NONE', ( #255997, #35912, #255613, #84098 ) ) ;
#62375 = CARTESIAN_POINT ( 'NONE',  ( 21.14999999999999858, 11.65000000001115943, -146.1500000000000341 ) ) ;
#62376 = ORIENTED_EDGE ( 'NONE', *, *, #55043, .T. ) ;
#62377 = CARTESIAN_POINT ( 'NONE',  ( -23.25000000000000000, 1.115600667400684642E-11, -134.0000000000000000 ) ) ;
#62378 = LINE ( 'NONE', #122353, #90524 ) ;
#62380 = ORIENTED_EDGE ( 'NONE', *, *, #185638, .F. ) ;
#62379 = ORIENTED_EDGE ( 'NONE', *, *, #4821, .F. ) ;
#62381 = ORIENTED_EDGE ( 'NONE', *, *, #195711, .F. ) ;
#62382 = CARTESIAN_POINT ( 'NONE',  ( 23.24999999999999645, 5.600000000011153389, -88.09473398108696074 ) ) ;
#62383 = EDGE_LOOP ( 'NONE', ( #54085, #95269, #174163, #218546 ) ) ;
#62384 = ORIENTED_EDGE ( 'NONE', *, *, #16983, .F. ) ;
#62385 = DIRECTION ( 'NONE',  ( 0.000000000000000000, 1.000000000000000000, 6.982962677686266711E-15 ) ) ;
#62387 = ORIENTED_EDGE ( 'NONE', *, *, #198553, .T. ) ;
#62386 = LINE ( 'NONE', #201893, #89281 ) ;
#62389 = CARTESIAN_POINT ( 'NONE',  ( 20.95568717954149562, 65.39800594612050588, -162.4205991162557723 ) ) ;
#62388 = FACE_OUTER_BOUND ( 'NONE', #143027, .T. ) ;
#62390 = DIRECTION ( 'NONE',  ( 1.000000000000000000, 0.000000000000000000, 0.000000000000000000 ) ) ;
#62391 = CARTESIAN_POINT ( 'NONE',  ( -23.25000000000000355, 65.95000000001260787, -190.7731074845244166 ) ) ;
#62392 = DIRECTION ( 'NONE',  ( 0.000000000000000000, 1.000000000000000000, 0.000000000000000000 ) ) ;
#62393 = ORIENTED_EDGE ( 'NONE', *, *, #112189, .T. ) ;
#62394 = AXIS2_PLACEMENT_3D ( 'NONE', #981, #194116, #115839 ) ;
#62395 = VERTEX_POINT ( 'NONE', #103314 ) ;
#62396 = PLANE ( 'NONE',  #12373 ) ;
#62397 = CARTESIAN_POINT ( 'NONE',  ( 20.04999999999999716, 44.62608598762253109, -236.3940605665350745 ) ) ;
#62399 = ADVANCED_FACE ( 'NONE', ( #59032 ), #160773, .T. ) ;
#62398 = FACE_OUTER_BOUND ( 'NONE', #29464, .T. ) ;
#62400 = AXIS2_PLACEMENT_3D ( 'NONE', #147313, #105592, #6517 ) ;
#62401 = VERTEX_POINT ( 'NONE', #199887 ) ;
#62402 = DIRECTION ( 'NONE',  ( 0.000000000000000000, -0.9651348961777157509, 0.2617529984165031243 ) ) ;
#62403 = ADVANCED_FACE ( 'NONE', ( #220714 ), #81179, .T. ) ;
#62404 = AXIS2_PLACEMENT_3D ( 'NONE', #178588, #1182, #80716 ) ;
#62405 = LINE ( 'NONE', #79375, #92928 ) ;
#62406 = CARTESIAN_POINT ( 'NONE',  ( 23.14999999999999858, 70.40000000001157332, -57.11784146561127073 ) ) ;
#62407 = ORIENTED_EDGE ( 'NONE', *, *, #112003, .F. ) ;
#62408 = ORIENTED_EDGE ( 'NONE', *, *, #56243, .F. ) ;
#62409 =( BOUNDED_SURFACE ( )  B_SPLINE_SURFACE ( 3, 2, ( 
 ( #252117, #70958, #87884 ),
 ( #167478, #147902, #227418 ),
 ( #60332, #238992, #139863 ),
 ( #155632, #255921, #55168 ) ),
 .UNSPECIFIED., .F., .F., .T. ) 
 B_SPLINE_SURFACE_WITH_KNOTS ( ( 4, 4 ),
 ( 3, 3 ),
 ( 3.658908243880901523, 4.712388980384689674 ),
 ( 0.000000000000000000, 1.000000000000000000 ),
 .UNSPECIFIED. ) 
 GEOMETRIC_REPRESENTATION_ITEM ( )  RATIONAL_B_SPLINE_SURFACE ( (
 ( 1.000000000000000000, 0.8984936768950646524, 1.000000000000000000),
 ( 1.000000000000000000, 0.8646876308616670004, 1.000000000000000000),
 ( 1.000000000000000000, 0.7953136715911841570, 1.000000000000000000),
 ( 1.000000000000000000, 0.7071067811866457165, 1.000000000000000000) ) ) 
 REPRESENTATION_ITEM ( '' )  SURFACE ( )  );
#62410 = EDGE_CURVE ( 'NONE', #68443, #42929, #101569, .T. ) ;
#62411 = DIRECTION ( 'NONE',  ( -1.000000000000000000, 7.510212038922847255E-17, -1.676432719286211941E-16 ) ) ;
#62413 = EDGE_CURVE ( 'NONE', #180058, #24563, #64193, .T. ) ;
#62412 = CARTESIAN_POINT ( 'NONE',  ( 21.05000000000000071, 7.128833340094563376, -233.7327013124401276 ) ) ;
#62414 = ORIENTED_EDGE ( 'NONE', *, *, #72962, .T. ) ;
#62415 = FACE_OUTER_BOUND ( 'NONE', #220157, .T. ) ;
#62416 = ORIENTED_EDGE ( 'NONE', *, *, #212572, .F. ) ;
#62417 = CARTESIAN_POINT ( 'NONE',  ( -22.57320508075687115, 11.75000000001115552, -67.00000000000004263 ) ) ;
#62418 = DIRECTION ( 'NONE',  ( 1.000000000000000000, -0.000000000000000000, -0.000000000000000000 ) ) ;
#62420 = CARTESIAN_POINT ( 'NONE',  ( -20.93302460841143287, 68.06642993404715014, -224.1774859612004036 ) ) ;
#62419 = PLANE ( 'NONE',  #165532 ) ;
#62421 = CIRCLE ( 'NONE', #208170, 0.1000000000000028644 ) ;
#62422 = CARTESIAN_POINT ( 'NONE',  ( -20.94999999999999929, 1.115600667400684642E-11, -100.5000000000000426 ) ) ;
#62423 = CARTESIAN_POINT ( 'NONE',  ( -16.87487986503753845, 66.04999244492626076, -90.37313274483764758 ) ) ;
#62424 = AXIS2_PLACEMENT_3D ( 'NONE', #40260, #217560, #119791 ) ;
#62425 = ORIENTED_EDGE ( 'NONE', *, *, #103898, .F. ) ;
#62426 = CARTESIAN_POINT ( 'NONE',  ( -21.44999999999999929, 7.350000000011155166, -146.2500000000000284 ) ) ;
#62427 = CIRCLE ( 'NONE', #41599, 0.1000000000000055844 ) ;
#62428 = EDGE_CURVE ( 'NONE', #183793, #182847, #176457, .T. ) ;
#62430 = ORIENTED_EDGE ( 'NONE', *, *, #145545, .T. ) ;
#62429 = ORIENTED_EDGE ( 'NONE', *, *, #151567, .T. ) ;
#62431 = ORIENTED_EDGE ( 'NONE', *, *, #64214, .T. ) ;
#62432 = EDGE_CURVE ( 'NONE', #198388, #201923, #64211, .T. ) ;
#62433 = VERTEX_POINT ( 'NONE', #44652 ) ;
#62434 = CARTESIAN_POINT ( 'NONE',  ( 20.94999999999999574, 44.18518595211054389, -258.7688298343402380 ) ) ;
#62435 = CARTESIAN_POINT ( 'NONE',  ( 20.85000000000000142, -1.835859311432481045, -112.0044391687985694 ) ) ;
#62436 = CARTESIAN_POINT ( 'NONE',  ( -33.72168855820451938, 66.05000000001206217, -123.8731074845244251 ) ) ;
#62437 = DIRECTION ( 'NONE',  ( -0.000000000000000000, 0.000000000000000000, 1.000000000000000000 ) ) ;
#62439 = DIRECTION ( 'NONE',  ( 0.000000000000000000, 0.000000000000000000, -1.000000000000000000 ) ) ;
#62438 = CARTESIAN_POINT ( 'NONE',  ( -21.05000000000000071, 76.00000000001190870, -103.0231074845243029 ) ) ;
#62441 = ORIENTED_EDGE ( 'NONE', *, *, #28737, .F. ) ;
#62440 = CARTESIAN_POINT ( 'NONE',  ( 18.33683296300631227, 77.42198378243760715, -241.7117649660008567 ) ) ;
#62442 = DIRECTION ( 'NONE',  ( -1.000000000000000000, -0.000000000000000000, -0.000000000000000000 ) ) ;
#62443 = ORIENTED_EDGE ( 'NONE', *, *, #150887, .T. ) ;
#62444 = CARTESIAN_POINT ( 'NONE',  ( -20.94999999999999929, 79.37986612816742138, -196.2658927859692142 ) ) ;
#62445 = ORIENTED_EDGE ( 'NONE', *, *, #165970, .T. ) ;
#62446 = ORIENTED_EDGE ( 'NONE', *, *, #125154, .T. ) ;
#62447 = FACE_OUTER_BOUND ( 'NONE', #192112, .T. ) ;
#62448 = DIRECTION ( 'NONE',  ( 0.000000000000000000, 0.000000000000000000, -1.000000000000000000 ) ) ;
#62449 = CARTESIAN_POINT ( 'NONE',  ( 18.59999999999999432, 46.50671693017397246, -243.2369495081682942 ) ) ;
#62450 = EDGE_CURVE ( 'NONE', #148169, #226006, #124198, .T. ) ;
#62451 = CARTESIAN_POINT ( 'NONE',  ( 21.05000000000000426, 65.27628289530510131, -195.9286900929113244 ) ) ;
#62452 = AXIS2_PLACEMENT_3D ( 'NONE', #251130, #72534, #152077 ) ;
#62453 = CIRCLE ( 'NONE', #70846, 0.1000000000000028644 ) ;
#62454 = EDGE_CURVE ( 'NONE', #85330, #18319, #202519, .T. ) ;
#62455 = DIRECTION ( 'NONE',  ( 1.000000000000000000, 0.000000000000000000, 0.000000000000000000 ) ) ;
#62456 = VERTEX_POINT ( 'NONE', #158216 ) ;
#62457 = VERTEX_POINT ( 'NONE', #198573 ) ;
#62458 = CARTESIAN_POINT ( 'NONE',  ( 20.94999999999999929, 40.88152484246180052, -238.0427780438910474 ) ) ;
#62459 = ORIENTED_EDGE ( 'NONE', *, *, #190454, .T. ) ;
#62460 = CYLINDRICAL_SURFACE ( 'NONE', #102069, 0.09999999999998898659 ) ;
#62461 = CARTESIAN_POINT ( 'NONE',  ( -21.05000000000000071, 70.10000000001163301, -59.30400771986794695 ) ) ;
#62462 = CARTESIAN_POINT ( 'NONE',  ( 20.94999999999999574, -11.48912529306490349, -103.6000000000000369 ) ) ;
#62463 = CARTESIAN_POINT ( 'NONE',  ( -22.37643362114956602, 75.90091862633082087, -144.1488974784826951 ) ) ;
#62465 = ADVANCED_FACE ( 'NONE', ( #99457 ), #39090, .T. ) ;
#62464 = CARTESIAN_POINT ( 'NONE',  ( 21.12642695952774119, 0.09890328320052040045, -60.62434007796486668 ) ) ;
#62466 = DIRECTION ( 'NONE',  ( 1.000000000000000000, 0.000000000000000000, -0.000000000000000000 ) ) ;
#62467 = CYLINDRICAL_SURFACE ( 'NONE', #95823, 0.09999999999999939493 ) ;
#62468 = CARTESIAN_POINT ( 'NONE',  ( -20.94999999999999929, -1.162701749926853712, -108.4000000000000341 ) ) ;
#62469 = EDGE_CURVE ( 'NONE', #9149, #223523, #239001, .T. ) ;
#62470 = CARTESIAN_POINT ( 'NONE',  ( -21.04999999999953531, 6.144922128657323235, -199.6090117692627928 ) ) ;
#62471 = AXIS2_PLACEMENT_3D ( 'NONE', #189564, #33093, #168760 ) ;
#62472 = CIRCLE ( 'NONE', #91674, 0.1000000000000017958 ) ;
#62473 = DIRECTION ( 'NONE',  ( -0.000000000000000000, 6.982962677686266711E-15, -1.000000000000000000 ) ) ;
#62474 = TOROIDAL_SURFACE ( 'NONE', #41640, 0.4000000000000009104, 0.1000000000000000056 ) ;
#62475 = VECTOR ( 'NONE', #76542, 1000.000000000000000 ) ;
#62476 = EDGE_CURVE ( 'NONE', #215011, #6262, #128041, .T. ) ;
#62477 = CYLINDRICAL_SURFACE ( 'NONE', #148865, 0.1000000000000054040 ) ;
#62478 = ORIENTED_EDGE ( 'NONE', *, *, #251257, .F. ) ;
#62479 = TOROIDAL_SURFACE ( 'NONE', #108262, 4.099999999999999645, 0.1000000000000000056 ) ;
#62480 = CARTESIAN_POINT ( 'NONE',  ( 20.95132126680579887, 10.48994987015794322, -41.07032453843452657 ) ) ;
#62481 = ORIENTED_EDGE ( 'NONE', *, *, #184738, .T. ) ;
#62482 = EDGE_CURVE ( 'NONE', #46223, #234522, #18396, .T. ) ;
#62483 = CARTESIAN_POINT ( 'NONE',  ( 20.73486653747088582, 7.250000000011182166, -113.1500000000000483 ) ) ;
#62484 = DIRECTION ( 'NONE',  ( 0.000000000000000000, 1.000000000000000000, 7.272083257015735086E-15 ) ) ;
#62485 = DIRECTION ( 'NONE',  ( 2.694716079187272946E-16, -1.000000000000000000, 0.000000000000000000 ) ) ;
#62486 = CIRCLE ( 'NONE', #154102, 0.1000000000000000472 ) ;
#62487 = ORIENTED_EDGE ( 'NONE', *, *, #130674, .T. ) ;
#62489 = AXIS2_PLACEMENT_3D ( 'NONE', #14518, #37928, #207905 ) ;
#62488 = FACE_OUTER_BOUND ( 'NONE', #136159, .T. ) ;
#62490 = EDGE_CURVE ( 'NONE', #126467, #124845, #63616, .T. ) ;
#62491 = FACE_OUTER_BOUND ( 'NONE', #73950, .T. ) ;
#62492 = DIRECTION ( 'NONE',  ( 0.000000000000000000, 0.2617529984165031243, 0.9651348961777157509 ) ) ;
#62493 = CARTESIAN_POINT ( 'NONE',  ( -20.64999999999999858, 82.09643798151613225, -215.4278993322501208 ) ) ;
#62494 = CARTESIAN_POINT ( 'NONE',  ( -18.39999999999999858, 85.40000000001204228, -114.7731074845242460 ) ) ;
#62495 = DIRECTION ( 'NONE',  ( 0.000000000000000000, 6.982962677686266711E-15, -1.000000000000000000 ) ) ;
#62496 = ORIENTED_EDGE ( 'NONE', *, *, #191736, .F. ) ;
#62497 = CARTESIAN_POINT ( 'NONE',  ( 18.59999999999999076, 11.65000000001115943, -125.3500000000000512 ) ) ;
#62499 = VERTEX_POINT ( 'NONE', #45926 ) ;
#62498 = DIRECTION ( 'NONE',  ( -1.000000000000000000, -0.000000000000000000, -0.000000000000000000 ) ) ;
#62500 = DIRECTION ( 'NONE',  ( -1.000000000000000000, -0.000000000000000000, -0.000000000000000000 ) ) ;
#62501 = ADVANCED_FACE ( 'NONE', ( #107175 ), #227120, .T. ) ;
#62502 = FACE_OUTER_BOUND ( 'NONE', #67566, .T. ) ;
#62503 = DIRECTION ( 'NONE',  ( -0.000000000000000000, 0.9651348961777157509, -0.2617529984165031243 ) ) ;
#62504 = VERTEX_POINT ( 'NONE', #86306 ) ;
#62505 = CARTESIAN_POINT ( 'NONE',  ( 22.59999999999999432, 11.74956712350054566, -33.39914163090129762 ) ) ;
#62506 = DIRECTION ( 'NONE',  ( -1.000000000000000000, 0.000000000000000000, 0.000000000000000000 ) ) ;
#62507 = VERTEX_POINT ( 'NONE', #28981 ) ;
#62508 = DIRECTION ( 'NONE',  ( 1.000000000000000000, 0.000000000000000000, 0.000000000000000000 ) ) ;
#62509 = CARTESIAN_POINT ( 'NONE',  ( 20.94999999999999929, 1.835341550235569663, -45.05515129256298223 ) ) ;
#62510 = AXIS2_PLACEMENT_3D ( 'NONE', #141758, #201741, #28282 ) ;
#62511 = CARTESIAN_POINT ( 'NONE',  ( -23.49999999999994316, 74.16448838626247664, -47.62760213295649692 ) ) ;
#62512 = EDGE_LOOP ( 'NONE', ( #60578, #40152, #136325, #256919 ) ) ;
#62513 = TOROIDAL_SURFACE ( 'NONE', #129157, 11.65000000000000036, 0.1000000000000000056 ) ;
#62514 = ORIENTED_EDGE ( 'NONE', *, *, #214449, .F. ) ;
#62515 = CARTESIAN_POINT ( 'NONE',  ( 21.05000000000000071, 10.50253167713781544, -74.55882981707586055 ) ) ;
#62516 = FACE_OUTER_BOUND ( 'NONE', #39962, .T. ) ;
#62517 = CARTESIAN_POINT ( 'NONE',  ( 18.49999999999999289, 69.35000000001200249, -115.1731074845243512 ) ) ;
#62518 = CARTESIAN_POINT ( 'NONE',  ( 21.05000000000000071, -12.41227409413852811, -131.0000000000000284 ) ) ;
#62519 = CARTESIAN_POINT ( 'NONE',  ( 22.60000000000000142, -3.180729737797944434, -228.0957332317254895 ) ) ;
#62521 = CARTESIAN_POINT ( 'NONE',  ( -23.15000000000000213, 1.115600667400684642E-11, -33.50000000000000000 ) ) ;
#62520 = LINE ( 'NONE', #122502, #220200 ) ;
#62522 = DIRECTION ( 'NONE',  ( 1.000000000000000000, 0.000000000000000000, -0.000000000000000000 ) ) ;
#62523 = CARTESIAN_POINT ( 'NONE',  ( 18.59999999999999076, 10.49142135624846439, -192.2499999999999716 ) ) ;
#62524 = CARTESIAN_POINT ( 'NONE',  ( 22.44352723754029810, 0.009277095054436634847, -155.8502786546512482 ) ) ;
#62525 = DIRECTION ( 'NONE',  ( 0.000000000000000000, 0.9654727137038715545, 0.2605042016806676242 ) ) ;
#62526 = TOROIDAL_SURFACE ( 'NONE', #112415, 12.97499999999999609, 0.1000000000000000056 ) ;
#62527 = ORIENTED_EDGE ( 'NONE', *, *, #235512, .F. ) ;
#62528 = ORIENTED_EDGE ( 'NONE', *, *, #203986, .T. ) ;
#62529 = DIRECTION ( 'NONE',  ( 2.952720810173289112E-16, -1.000000000000000000, -0.000000000000000000 ) ) ;
#62530 = CIRCLE ( 'NONE', #220735, 0.09999999999999939493 ) ;
#62531 = CARTESIAN_POINT ( 'NONE',  ( -22.47071067811865319, 75.90090754530983475, -177.7431822290224090 ) ) ;
#62533 = DIRECTION ( 'NONE',  ( 0.000000000000000000, 0.000000000000000000, -1.000000000000000000 ) ) ;
#62532 = CYLINDRICAL_SURFACE ( 'NONE', #229746, 12.87500000000000355 ) ;
#62534 = AXIS2_PLACEMENT_3D ( 'NONE', #154246, #172533, #252006 ) ;
#62535 = LINE ( 'NONE', #99059, #185250 ) ;
#62536 = CARTESIAN_POINT ( 'NONE',  ( 20.94999999999999929, -1.362429037182151470, -108.3888812479212476 ) ) ;
#62538 = EDGE_CURVE ( 'NONE', #199002, #125361, #206291, .T. ) ;
#62537 = DIRECTION ( 'NONE',  ( -1.000000000000000000, 0.000000000000000000, 0.000000000000000000 ) ) ;
#62539 = ORIENTED_EDGE ( 'NONE', *, *, #90052, .F. ) ;
#62540 = CARTESIAN_POINT ( 'NONE',  ( -23.25000000000000000, 76.00000000001244871, -170.0231074845243597 ) ) ;
#62541 = AXIS2_PLACEMENT_3D ( 'NONE', #136628, #37562, #216167 ) ;
#62542 = ORIENTED_EDGE ( 'NONE', *, *, #23673, .T. ) ;
#62543 = EDGE_CURVE ( 'NONE', #152420, #247434, #24335, .T. ) ;
#62544 = EDGE_CURVE ( 'NONE', #22307, #248393, #224554, .T. ) ;
#62545 = DIRECTION ( 'NONE',  ( 0.000000000000000000, -7.189901751995755791E-15, 1.000000000000000000 ) ) ;
#62546 = EDGE_LOOP ( 'NONE', ( #78553, #57735, #151724, #112281 ) ) ;
#62547 = DIRECTION ( 'NONE',  ( 1.000000000000000000, 0.000000000000000000, 0.000000000000000000 ) ) ;
#62548 = AXIS2_PLACEMENT_3D ( 'NONE', #185611, #23991, #120529 ) ;
#62549 = AXIS2_PLACEMENT_3D ( 'NONE', #215213, #39170, #200784 ) ;
#62550 = DIRECTION ( 'NONE',  ( -1.000000000000000000, -0.000000000000000000, -0.000000000000000000 ) ) ;
#62551 = TOROIDAL_SURFACE ( 'NONE', #108345, 12.77499999999999858, 0.1000000000000000056 ) ;
#62552 = AXIS2_PLACEMENT_3D ( 'NONE', #251667, #148734, #250386 ) ;
#62553 = EDGE_LOOP ( 'NONE', ( #225533, #243826, #1402, #129807 ) ) ;
#62554 = DIRECTION ( 'NONE',  ( 0.000000000000000000, -6.938893903907222067E-15, 1.000000000000000000 ) ) ;
#62555 = EDGE_CURVE ( 'NONE', #52663, #89722, #117783, .T. ) ;
#62556 = ORIENTED_EDGE ( 'NONE', *, *, #177913, .T. ) ;
#62557 = CARTESIAN_POINT ( 'NONE',  ( -16.77683809663752257, 52.34166666667851331, -86.27310748452447342 ) ) ;
#62558 = CARTESIAN_POINT ( 'NONE',  ( -18.40000000000000213, 11.41458325961093756, -46.14999999999999858 ) ) ;
#62559 = FACE_OUTER_BOUND ( 'NONE', #7739, .T. ) ;
#62560 = DIRECTION ( 'NONE',  ( 0.000000000000000000, -0.8660254037844412611, -0.4999999999999956701 ) ) ;
#62561 = DIRECTION ( 'NONE',  ( 1.186688945009010077E-16, -1.000000000000000000, -0.000000000000000000 ) ) ;
#62562 = VECTOR ( 'NONE', #156005, 1000.000000000000000 ) ;
#62564 = DIRECTION ( 'NONE',  ( 0.000000000000000000, -0.4088369013363783999, 0.9126074666063545004 ) ) ;
#62563 = DIRECTION ( 'NONE',  ( 1.000000000000000000, 0.000000000000000000, 0.000000000000000000 ) ) ;
#62565 = DIRECTION ( 'NONE',  ( -0.7071067811865795472, 0.3338907855511005218, 0.6233112732207110041 ) ) ;
#62567 = ORIENTED_EDGE ( 'NONE', *, *, #222631, .T. ) ;
#62566 = CARTESIAN_POINT ( 'NONE',  ( 20.22894356738409627, 66.72150177717436748, -128.2545845782748586 ) ) ;
#62569 = CARTESIAN_POINT ( 'NONE',  ( 21.14999999999999858, 30.73075574124490217, -252.3164853687435709 ) ) ;
#62568 = LINE ( 'NONE', #58684, #219960 ) ;
#62570 = EDGE_LOOP ( 'NONE', ( #79022, #191964, #15887, #171427 ) ) ;
#62572 = ORIENTED_EDGE ( 'NONE', *, *, #123221, .T. ) ;
#62571 = DIRECTION ( 'NONE',  ( 0.000000000000000000, 0.000000000000000000, 1.000000000000000000 ) ) ;
#62573 = ORIENTED_EDGE ( 'NONE', *, *, #5178, .F. ) ;
#62574 = DIRECTION ( 'NONE',  ( 1.000000000000000000, -0.000000000000000000, -0.000000000000000000 ) ) ;
#62575 = CARTESIAN_POINT ( 'NONE',  ( -20.85000000000000142, 56.23643450586806836, -227.9054833905874204 ) ) ;
#62576 = CARTESIAN_POINT ( 'NONE',  ( -22.94999999999999929, -1.800000000000000044, -11.61130914238355771 ) ) ;
#62577 = ORIENTED_EDGE ( 'NONE', *, *, #117671, .F. ) ;
#62578 = EDGE_CURVE ( 'NONE', #93118, #220499, #111036, .T. ) ;
#62580 = ADVANCED_FACE ( 'NONE', ( #249277 ), #245425, .F. ) ;
#62579 = CARTESIAN_POINT ( 'NONE',  ( 22.57320508075688537, 11.65000000000000036, 0.000000000000000000 ) ) ;
#62581 = CARTESIAN_POINT ( 'NONE',  ( -20.54999999999999716, 76.00000000001253397, -182.8981074845243597 ) ) ;
#62582 = CARTESIAN_POINT ( 'NONE',  ( 21.05000000000000071, 76.10000000001276987, -215.1726782920691505 ) ) ;
#62583 = B_SPLINE_CURVE_WITH_KNOTS ( 'NONE', 3,
 ( #132025, #55034, #233710, #35534, #137162, #115034, #254512, #75910, #211572, #176316, #255784, #216697, #203560, #104429 ),
 .UNSPECIFIED., .F., .F.,
 ( 4, 2, 2, 2, 2, 2, 4 ),
 ( 0.000000000000000000, 2.389617747640127089E-05, 4.779235495280254178E-05, 9.558470990564673048E-05, 0.0001911694198113693551, 0.0003823388396228073944, 0.0007646776792456835272 ),
 .UNSPECIFIED. ) ;
#62584 = ORIENTED_EDGE ( 'NONE', *, *, #128872, .F. ) ;
#62585 = CIRCLE ( 'NONE', #208343, 0.09999999999999939493 ) ;
#62586 = CARTESIAN_POINT ( 'NONE',  ( -20.64999999999999858, 2.000000000011154189, -80.22462192276213955 ) ) ;
#62587 = CIRCLE ( 'NONE', #75258, 0.1000000000000052097 ) ;
#62588 = EDGE_CURVE ( 'NONE', #237540, #74012, #149232, .T. ) ;
#62589 = VERTEX_POINT ( 'NONE', #109735 ) ;
#62590 = EDGE_LOOP ( 'NONE', ( #24568, #240254, #237496, #99875 ) ) ;
#62591 = CYLINDRICAL_SURFACE ( 'NONE', #139583, 0.09999999999999939493 ) ;
#62592 = VECTOR ( 'NONE', #227954, 1000.000000000000000 ) ;
#62593 = EDGE_LOOP ( 'NONE', ( #209428, #235897, #842, #117613, #159003, #6275, #27041, #101623 ) ) ;
#62594 = CARTESIAN_POINT ( 'NONE',  ( -18.59999999999999787, 18.81339837015603322, -226.7756228984618190 ) ) ;
#62595 = ORIENTED_EDGE ( 'NONE', *, *, #115559, .T. ) ;
#62596 = LINE ( 'NONE', #49443, #113617 ) ;
#62597 = CARTESIAN_POINT ( 'NONE',  ( -21.05000000000000071, 5.900000000000005684, -23.28090023534363340 ) ) ;
#62598 = CYLINDRICAL_SURFACE ( 'NONE', #176322, 0.1000000000000000472 ) ;
#62599 = CARTESIAN_POINT ( 'NONE',  ( -21.07971444708686093, 30.84640344441752902, -252.0588669582742227 ) ) ;
#62600 = CARTESIAN_POINT ( 'NONE',  ( 20.97468175916176847, 10.62526516438217605, -179.7547614354127745 ) ) ;
#62601 = ORIENTED_EDGE ( 'NONE', *, *, #217978, .F. ) ;
#62602 = AXIS2_PLACEMENT_3D ( 'NONE', #113837, #13468, #53875 ) ;
#62603 = ADVANCED_FACE ( 'NONE', ( #146303 ), #150180, .T. ) ;
#62604 = LINE ( 'NONE', #24787, #53412 ) ;
#62605 = CIRCLE ( 'NONE', #208367, 0.09999999999998898659 ) ;
#62606 = DIRECTION ( 'NONE',  ( -0.7071067811865475727, -0.7071067811865475727, 0.000000000000000000 ) ) ;
#62607 = DIRECTION ( 'NONE',  ( -1.000000000000000000, -0.000000000000000000, -0.000000000000000000 ) ) ;
#62608 = CARTESIAN_POINT ( 'NONE',  ( -23.25000000000000000, -1.835859311432481045, -212.6044391687984785 ) ) ;
#62609 = EDGE_LOOP ( 'NONE', ( #74643, #252735, #23568, #24325 ) ) ;
#62612 = DIRECTION ( 'NONE',  ( -0.000000000000000000, 1.000000000000000000, 6.982962677686266711E-15 ) ) ;
#62611 = PLANE ( 'NONE',  #220699 ) ;
#62610 = CIRCLE ( 'NONE', #124970, 0.09999999999999939493 ) ;
#62613 = EDGE_LOOP ( 'NONE', ( #212349, #117313, #221771, #212177, #85660, #35659, #121503, #204609, #38301, #135165, #257172, #230106 ) ) ;
#62616 = ORIENTED_EDGE ( 'NONE', *, *, #121216, .T. ) ;
#62615 = CARTESIAN_POINT ( 'NONE',  ( -20.54999999999999716, 9.350000000011156942, -188.6499999999999488 ) ) ;
#62614 = CARTESIAN_POINT ( 'NONE',  ( -20.94999999999999929, 76.00000000001142553, -36.02310748452432421 ) ) ;
#62617 = AXIS2_PLACEMENT_3D ( 'NONE', #1127, #255424, #80667 ) ;
#62618 = ORIENTED_EDGE ( 'NONE', *, *, #231316, .T. ) ;
#62619 = DIRECTION ( 'NONE',  ( 1.000000000000000000, -0.000000000000000000, -0.000000000000000000 ) ) ;
#62620 = CARTESIAN_POINT ( 'NONE',  ( -21.14999999999999858, 7.128833340093095217, -233.7327013124392749 ) ) ;
#62621 = ADVANCED_FACE ( 'NONE', ( #229706 ), #188016, .T. ) ;
#62622 = DIRECTION ( 'NONE',  ( 1.000000000000000000, 0.000000000000000000, 0.000000000000000000 ) ) ;
#62623 = ORIENTED_EDGE ( 'NONE', *, *, #4967, .F. ) ;
#62624 = CARTESIAN_POINT ( 'NONE',  ( 20.04142135391667168, 16.73759089399622013, -222.6362981240360739 ) ) ;
#62625 = LINE ( 'NONE', #142148, #44528 ) ;
#62626 = EDGE_CURVE ( 'NONE', #172615, #209763, #244117, .T. ) ;
#62628 = DIRECTION ( 'NONE',  ( 0.000000000000000000, -1.000000000000000000, -6.982962677686265922E-15 ) ) ;
#62627 = CARTESIAN_POINT ( 'NONE',  ( -18.50000000000000000, 7.021664781911246322, -104.1335654018973287 ) ) ;
#62629 = EDGE_CURVE ( 'NONE', #138653, #60369, #38687, .T. ) ;
#62631 = ORIENTED_EDGE ( 'NONE', *, *, #165140, .T. ) ;
#62630 = DIRECTION ( 'NONE',  ( 0.000000000000000000, -0.9770955615653318382, -0.2128009952263588411 ) ) ;
#62632 = CIRCLE ( 'NONE', #183429, 0.1000000000000028644 ) ;
#62633 = AXIS2_PLACEMENT_3D ( 'NONE', #117462, #237403, #97852 ) ;
#62634 = ORIENTED_EDGE ( 'NONE', *, *, #139703, .T. ) ;
#62635 = CARTESIAN_POINT ( 'NONE',  ( -2.995603634470891112E-16, 87.75000000001186606, -90.77310748452423184 ) ) ;
#62636 = EDGE_CURVE ( 'NONE', #8746, #146536, #72011, .T. ) ;
#62637 = DIRECTION ( 'NONE',  ( 0.000000000000000000, -5.551115123125777653E-14, 1.000000000000000000 ) ) ;
#62639 = EDGE_CURVE ( 'NONE', #180867, #90288, #105273, .T. ) ;
#62638 = VERTEX_POINT ( 'NONE', #171063 ) ;
#62640 = DIRECTION ( 'NONE',  ( 0.000000000000000000, -6.982962677686266711E-15, 1.000000000000000000 ) ) ;
#62641 = ORIENTED_EDGE ( 'NONE', *, *, #69806, .T. ) ;
#62642 = DIRECTION ( 'NONE',  ( -1.836970198721029934E-16, -1.000000000000000000, -6.982962677686266711E-15 ) ) ;
#62643 = CARTESIAN_POINT ( 'NONE',  ( 22.49999999999999645, 75.90000000001202807, -114.6726782920691221 ) ) ;
#62644 = CARTESIAN_POINT ( 'NONE',  ( 22.39999999999999503, 11.65000000001116298, -167.4999999999999716 ) ) ;
#62645 = EDGE_CURVE ( 'NONE', #124622, #146995, #59488, .T. ) ;
#62646 = ORIENTED_EDGE ( 'NONE', *, *, #18814, .F. ) ;
#62647 = CARTESIAN_POINT ( 'NONE',  ( -21.65000000000000213, 62.98412863812492901, -221.9071248009556712 ) ) ;
#62648 = AXIS2_PLACEMENT_3D ( 'NONE', #154023, #15777, #176125 ) ;
#62649 = ADVANCED_FACE ( 'NONE', ( #56180 ), #72583, .T. ) ;
#62650 = AXIS2_PLACEMENT_3D ( 'NONE', #73364, #98002, #95458 ) ;
#62651 = AXIS2_PLACEMENT_3D ( 'NONE', #76228, #194927, #117923 ) ;
#62652 = DIRECTION ( 'NONE',  ( 0.000000000000000000, 1.000000000000000000, 6.982962677686266711E-15 ) ) ;
#62653 = EDGE_CURVE ( 'NONE', #38302, #204155, #190595, .T. ) ;
#62654 = EDGE_CURVE ( 'NONE', #218397, #227951, #139170, .T. ) ;
#62655 = VERTEX_POINT ( 'NONE', #32829 ) ;
#62656 = AXIS2_PLACEMENT_3D ( 'NONE', #29200, #69578, #49996 ) ;
#62657 = ORIENTED_EDGE ( 'NONE', *, *, #41876, .F. ) ;
#62658 = ORIENTED_EDGE ( 'NONE', *, *, #169463, .T. ) ;
#62659 = ADVANCED_FACE ( 'NONE', ( #172347 ), #231008, .F. ) ;
#62660 = FACE_OUTER_BOUND ( 'NONE', #43587, .T. ) ;
#62661 = ORIENTED_EDGE ( 'NONE', *, *, #15413, .T. ) ;
#62663 = ORIENTED_EDGE ( 'NONE', *, *, #100459, .T. ) ;
#62662 = CARTESIAN_POINT ( 'NONE',  ( 13.43663047529819998, 66.55335465531732098, -185.1123010284242412 ) ) ;
#62665 = EDGE_CURVE ( 'NONE', #57698, #168032, #238597, .T. ) ;
#62664 = ORIENTED_EDGE ( 'NONE', *, *, #206301, .T. ) ;
#62666 = AXIS2_PLACEMENT_3D ( 'NONE', #230203, #111545, #172853 ) ;
#62667 = ADVANCED_FACE ( 'NONE', ( #74527 ), #34110, .T. ) ;
#62670 = ORIENTED_EDGE ( 'NONE', *, *, #30050, .T. ) ;
#62669 = ORIENTED_EDGE ( 'NONE', *, *, #246560, .T. ) ;
#62668 = DIRECTION ( 'NONE',  ( 0.000000000000000000, 0.000000000000000000, 1.000000000000000000 ) ) ;
#62671 = EDGE_CURVE ( 'NONE', #27654, #200535, #126143, .T. ) ;
#62672 = EDGE_LOOP ( 'NONE', ( #40408, #37239, #165348, #223868 ) ) ;
#62673 = DIRECTION ( 'NONE',  ( 0.000000000000000000, 0.9126074666063771490, 0.4088369013363281623 ) ) ;
#62674 = CARTESIAN_POINT ( 'NONE',  ( -20.85000000000000142, 11.65000000001115232, -167.5000000000000284 ) ) ;
#62675 = LINE ( 'NONE', #37995, #80117 ) ;
#62676 = ORIENTED_EDGE ( 'NONE', *, *, #232101, .F. ) ;
#62677 = CARTESIAN_POINT ( 'NONE',  ( -21.29999999999995808, 1.115600667400684642E-11, -167.4999999999999716 ) ) ;
#62679 = ORIENTED_EDGE ( 'NONE', *, *, #209811, .F. ) ;
#62678 = DIRECTION ( 'NONE',  ( 1.000000000000000000, -0.000000000000000000, -0.000000000000000000 ) ) ;
#62680 = CARTESIAN_POINT ( 'NONE',  ( -16.88460203013674743, 14.16703338188093575, -219.2695876520766092 ) ) ;
#62682 = ORIENTED_EDGE ( 'NONE', *, *, #80160, .F. ) ;
#62681 = DIRECTION ( 'NONE',  ( -1.000000000000000000, 1.387778780781454006E-13, 0.000000000000000000 ) ) ;
#62683 = ADVANCED_FACE ( 'NONE', ( #15823 ), #95327, .T. ) ;
#62684 = VERTEX_POINT ( 'NONE', #14533 ) ;
#62685 = CARTESIAN_POINT ( 'NONE',  ( -20.64999999999999858, 84.66355140188147743, -160.4990063664569959 ) ) ;
#62686 = VERTEX_POINT ( 'NONE', #253100 ) ;
#62687 = ORIENTED_EDGE ( 'NONE', *, *, #239385, .F. ) ;
#62689 = AXIS2_PLACEMENT_3D ( 'NONE', #172647, #89192, #27981 ) ;
#62688 = CARTESIAN_POINT ( 'NONE',  ( -16.87683809663752399, 9.850000000011123191, -180.9023640181964652 ) ) ;
#62690 = DIRECTION ( 'NONE',  ( 0.000000000000000000, 0.000000000000000000, -1.000000000000000000 ) ) ;
#62692 = ORIENTED_EDGE ( 'NONE', *, *, #182672, .F. ) ;
#62691 = VERTEX_POINT ( 'NONE', #36671 ) ;
#62693 = ORIENTED_EDGE ( 'NONE', *, *, #94707, .F. ) ;
#62694 = CARTESIAN_POINT ( 'NONE',  ( -18.79999999999999716, 11.50977166988710820, -1.786320531569725478 ) ) ;
#62695 = VERTEX_POINT ( 'NONE', #233567 ) ;
#62696 = EDGE_LOOP ( 'NONE', ( #192711, #86312, #256500 ) ) ;
#62697 = CARTESIAN_POINT ( 'NONE',  ( -1.739115166359751170E-14, 43.07541598710463404, -233.9110336739111631 ) ) ;
#62699 = ORIENTED_EDGE ( 'NONE', *, *, #128120, .F. ) ;
#62698 = CARTESIAN_POINT ( 'NONE',  ( 13.99999999999999822, 47.91805600923871822, -233.7139610577891631 ) ) ;
#62700 = CARTESIAN_POINT ( 'NONE',  ( -20.85000000000000142, -1.835859311432481045, -179.0044391687985410 ) ) ;
#62702 = CARTESIAN_POINT ( 'NONE',  ( 18.40000000000000213, -9.499999999988844479, -107.5320693966997112 ) ) ;
#62701 = CARTESIAN_POINT ( 'NONE',  ( -18.40000000000000213, 11.75000000001113953, -124.7500000000000426 ) ) ;
#62703 = EDGE_LOOP ( 'NONE', ( #232554, #21061, #152402, #71679 ) ) ;
#62705 = VERTEX_POINT ( 'NONE', #54898 ) ;
#62704 = ORIENTED_EDGE ( 'NONE', *, *, #96656, .T. ) ;
#62706 = CARTESIAN_POINT ( 'NONE',  ( 20.85000000000000142, 77.83585931145526615, -58.01866831572577610 ) ) ;
#62708 = ADVANCED_FACE ( 'NONE', ( #213997 ), #96581, .T. ) ;
#62707 = CARTESIAN_POINT ( 'NONE',  ( 21.14999999999999503, 76.00000000001195133, -103.0231074845243171 ) ) ;
#62710 = ORIENTED_EDGE ( 'NONE', *, *, #184880, .F. ) ;
#62709 = VECTOR ( 'NONE', #194052, 1000.000000000000000 ) ;
#62711 = EDGE_CURVE ( 'NONE', #81280, #16906, #110691, .T. ) ;
#62712 = CIRCLE ( 'NONE', #45947, 4.000000000000003553 ) ;
#62713 = DIRECTION ( 'NONE',  ( -1.000000000000000000, 0.000000000000000000, 0.000000000000000000 ) ) ;
#62714 = ORIENTED_EDGE ( 'NONE', *, *, #196070, .F. ) ;
#62715 = ORIENTED_EDGE ( 'NONE', *, *, #252576, .F. ) ;
#62716 = LINE ( 'NONE', #241363, #254298 ) ;
#62717 = EDGE_LOOP ( 'NONE', ( #84340, #151630, #138347, #55910 ) ) ;
#62718 = CARTESIAN_POINT ( 'NONE',  ( -23.15000000000000213, 70.60814576644823148, -215.7631455941064189 ) ) ;
#62719 = VERTEX_POINT ( 'NONE', #174922 ) ;
#62720 = AXIS2_PLACEMENT_3D ( 'NONE', #111225, #172536, #12151 ) ;
#62721 = DIRECTION ( 'NONE',  ( -0.000000000000000000, 1.000000000000000000, -0.000000000000000000 ) ) ;
#62723 = TOROIDAL_SURFACE ( 'NONE', #241774, 4.099999999999999645, 0.1000000000000000056 ) ;
#62722 = CARTESIAN_POINT ( 'NONE',  ( -18.41431012584568450, 11.48747202921932598, -42.72676398689832666 ) ) ;
#62725 = DIRECTION ( 'NONE',  ( 0.000000000000000000, -1.000000000000000000, -6.982962677686265922E-15 ) ) ;
#62724 = DIRECTION ( 'NONE',  ( 0.000000000000000000, 0.9651348961777379554, -0.2617529984164210233 ) ) ;
#62726 = FACE_OUTER_BOUND ( 'NONE', #150542, .T. ) ;
#62727 = DIRECTION ( 'NONE',  ( 0.000000000000000000, 0.9126074666063804797, 0.4088369013363203908 ) ) ;
#62728 = CARTESIAN_POINT ( 'NONE',  ( 18.39999999999999503, 33.92263863280957992, -235.0698407953532012 ) ) ;
#62729 = CARTESIAN_POINT ( 'NONE',  ( -2.995603634470891112E-16, 69.35000000001180354, -81.77310748452435973 ) ) ;
#62730 = CARTESIAN_POINT ( 'NONE',  ( 18.49999999999999289, 67.49463558145296815, -195.5618716440587548 ) ) ;
#62731 = EDGE_CURVE ( 'NONE', #14025, #13648, #157920, .T. ) ;
#62732 = ORIENTED_EDGE ( 'NONE', *, *, #139046, .T. ) ;
#62733 = AXIS2_PLACEMENT_3D ( 'NONE', #68914, #105410, #48036 ) ;
#62734 = AXIS2_PLACEMENT_3D ( 'NONE', #233770, #91679, #14738 ) ;
#62735 = AXIS2_PLACEMENT_3D ( 'NONE', #139082, #161263, #4717 ) ;
#62736 = CIRCLE ( 'NONE', #154356, 0.1000000000000028644 ) ;
#62737 = CIRCLE ( 'NONE', #225198, 0.1000000000000002554 ) ;
#62739 = EDGE_LOOP ( 'NONE', ( #237463, #51398, #199847, #237970 ) ) ;
#62738 = EDGE_LOOP ( 'NONE', ( #25584, #246883, #243198 ) ) ;
#62740 = EDGE_LOOP ( 'NONE', ( #96365, #61399 ) ) ;
#62741 = CARTESIAN_POINT ( 'NONE',  ( 21.14999999999999858, 1.115600667400684642E-11, -179.6499999999999773 ) ) ;
#62742 = CARTESIAN_POINT ( 'NONE',  ( -18.50000000000000000, 70.08587962373172786, -198.1273832143211848 ) ) ;
#62744 = CARTESIAN_POINT ( 'NONE',  ( -12.25000000000000178, 9.349999999999980105, -16.51856895740264264 ) ) ;
#62743 = CYLINDRICAL_SURFACE ( 'NONE', #232696, 0.1000000000000028644 ) ;
#62745 = CARTESIAN_POINT ( 'NONE',  ( 18.59999999999999432, 1.736257131608553550, -45.06865232901750318 ) ) ;
#62746 = ORIENTED_EDGE ( 'NONE', *, *, #32541, .F. ) ;
#62747 = CYLINDRICAL_SURFACE ( 'NONE', #25701, 0.09999999999999939493 ) ;
#62748 = VECTOR ( 'NONE', #119127, 1000.000000000000000 ) ;
#62749 = FACE_OUTER_BOUND ( 'NONE', #230472, .T. ) ;
#62750 = CARTESIAN_POINT ( 'NONE',  ( 20.94999999999999574, -11.41227409413852989, -170.4999999999999716 ) ) ;
#62751 = DIRECTION ( 'NONE',  ( 1.000000000000000000, 0.000000000000000000, 0.000000000000000000 ) ) ;
#62752 = ORIENTED_EDGE ( 'NONE', *, *, #154307, .T. ) ;
#62753 = CARTESIAN_POINT ( 'NONE',  ( -21.05000000000000071, 64.37928932189296916, -62.65469083218336266 ) ) ;
#62754 = DIRECTION ( 'NONE',  ( -1.836970198721029934E-16, -1.000000000000000000, -6.982962677686266711E-15 ) ) ;
#62755 = ORIENTED_EDGE ( 'NONE', *, *, #138338, .T. ) ;
#62756 = CARTESIAN_POINT ( 'NONE',  ( 18.59999999999999076, 11.75000000001115907, -122.2500000000000284 ) ) ;
#62757 = DIRECTION ( 'NONE',  ( 0.000000000000000000, -0.1298341882520022694, -0.9915357197604853789 ) ) ;
#62758 = FACE_OUTER_BOUND ( 'NONE', #1121, .T. ) ;
#62759 = CYLINDRICAL_SURFACE ( 'NONE', #119284, 0.1000000000000000472 ) ;
#62760 = B_SPLINE_CURVE_WITH_KNOTS ( 'NONE', 3,
 ( #236719, #159778, #239310, #213309, #193763, #15133, #174243 ),
 .UNSPECIFIED., .F., .F.,
 ( 4, 3, 4 ),
 ( 0.000000000000000000, 1.860045280644891661E-05, 5.251155757304066840E-05 ),
 .UNSPECIFIED. ) ;
#62761 = CARTESIAN_POINT ( 'NONE',  ( 22.39999999999999858, 65.09550114356429162, -243.3481044654562879 ) ) ;
#62762 = VERTEX_POINT ( 'NONE', #62627 ) ;
#62763 = CARTESIAN_POINT ( 'NONE',  ( 23.24999999999999289, 11.75000000001116263, -179.6499999999999773 ) ) ;
#62765 = ADVANCED_FACE ( 'NONE', ( #80876 ), #97859, .F. ) ;
#62764 = FACE_OUTER_BOUND ( 'NONE', #151225, .T. ) ;
#62766 = CARTESIAN_POINT ( 'NONE',  ( 21.05000000000242721, 11.87050359475319716, -206.1507498716061946 ) ) ;
#62768 = DIRECTION ( 'NONE',  ( 0.000000000000000000, 0.000000000000000000, 1.000000000000000000 ) ) ;
#62767 = FACE_OUTER_BOUND ( 'NONE', #238155, .T. ) ;
#62769 = LINE ( 'NONE', #45766, #120683 ) ;
#62770 = EDGE_CURVE ( 'NONE', #101205, #226140, #177465, .T. ) ;
#62771 = DIRECTION ( 'NONE',  ( 0.5932847527679299127, -0.8049926720990051576, 6.366092712777055223E-16 ) ) ;
#62772 = CARTESIAN_POINT ( 'NONE',  ( -18.59999999999999787, 6.440012694424540385, -187.5719980452876712 ) ) ;
#62775 = VERTEX_POINT ( 'NONE', #161746 ) ;
#62774 = CIRCLE ( 'NONE', #58646, 0.09999999999999939493 ) ;
#62773 = DIRECTION ( 'NONE',  ( -0.000000000000000000, 0.000000000000000000, 1.000000000000000000 ) ) ;
#62776 = ORIENTED_EDGE ( 'NONE', *, *, #236360, .F. ) ;
#62777 = ADVANCED_FACE ( 'NONE', ( #1339, #43062, #138279, #20955 ), #163023, .T. ) ;
#62778 = AXIS2_PLACEMENT_3D ( 'NONE', #204485, #88377, #205778 ) ;
#62779 = ADVANCED_FACE ( 'NONE', ( #241276 ), #142149, .F. ) ;
#62780 = EDGE_CURVE ( 'NONE', #64013, #31307, #222963, .T. ) ;
#62781 = DIRECTION ( 'NONE',  ( 0.000000000000000000, 7.026728003956683390E-15, -1.000000000000000000 ) ) ;
#62782 = CIRCLE ( 'NONE', #208545, 0.5000000000000004441 ) ;
#62783 = DIRECTION ( 'NONE',  ( -0.7071067811865474617, -0.7071067811865474617, -0.000000000000000000 ) ) ;
#62784 = ADVANCED_FACE ( 'NONE', ( #39232 ), #61337, .T. ) ;
#62785 = CARTESIAN_POINT ( 'NONE',  ( 15.70340296795548163, 9.355888454513701546, -150.2886428967780148 ) ) ;
#62786 = VECTOR ( 'NONE', #27516, 1000.000000000000000 ) ;
#62787 = VERTEX_POINT ( 'NONE', #159181 ) ;
#62788 = DIRECTION ( 'NONE',  ( -0.000000000000000000, -1.000000000000000000, -1.734723475976807292E-15 ) ) ;
#62789 = CYLINDRICAL_SURFACE ( 'NONE', #120171, 0.09999999999999939493 ) ;
#62791 = CARTESIAN_POINT ( 'NONE',  ( -21.46681500597874148, 76.00000000001200817, -109.8806186439521611 ) ) ;
#62790 = AXIS2_PLACEMENT_3D ( 'NONE', #145734, #8811, #46622 ) ;
#62792 = EDGE_LOOP ( 'NONE', ( #78969, #20459, #72634, #138316 ) ) ;
#62793 = CARTESIAN_POINT ( 'NONE',  ( 23.15000000000000213, 69.09936979046463534, -247.6075824278584889 ) ) ;
#62795 = ORIENTED_EDGE ( 'NONE', *, *, #150679, .T. ) ;
#62794 = CARTESIAN_POINT ( 'NONE',  ( -23.25000000000000000, 75.45031870333662027, -205.5498907664980948 ) ) ;
#62796 = CYLINDRICAL_SURFACE ( 'NONE', #25636, 0.09999999999999939493 ) ;
#62797 = EDGE_CURVE ( 'NONE', #41810, #178378, #219194, .T. ) ;
#62798 = CARTESIAN_POINT ( 'NONE',  ( 20.21567752745066215, 65.80188589878034122, -162.1404871368697798 ) ) ;
#62799 = CARTESIAN_POINT ( 'NONE',  ( 20.99999999999997868, 1.115600667400684642E-11, -100.5000000000000284 ) ) ;
#62800 = ORIENTED_EDGE ( 'NONE', *, *, #15903, .F. ) ;
#62801 = DIRECTION ( 'NONE',  ( 1.000000000000000000, 0.000000000000000000, 0.000000000000000000 ) ) ;
#62802 = DIRECTION ( 'NONE',  ( 0.000000000000000000, 0.000000000000000000, 1.000000000000000000 ) ) ;
#62803 = CARTESIAN_POINT ( 'NONE',  ( 21.04999999999999716, 67.10527618163435193, -128.0360231613754536 ) ) ;
#62804 = TOROIDAL_SURFACE ( 'NONE', #162771, 12.97499999999999787, 0.1000000000000000056 ) ;
#62805 = ORIENTED_EDGE ( 'NONE', *, *, #185052, .T. ) ;
#62806 = DIRECTION ( 'NONE',  ( 0.000000000000000000, 0.000000000000000000, -1.000000000000000000 ) ) ;
#62807 = CARTESIAN_POINT ( 'NONE',  ( -15.75000000000000355, 9.850000000011133849, -117.2500000000000284 ) ) ;
#62808 = DIRECTION ( 'NONE',  ( -1.000000000000000000, 0.000000000000000000, 0.000000000000000000 ) ) ;
#62809 = FACE_OUTER_BOUND ( 'NONE', #106199, .T. ) ;
#62810 = ORIENTED_EDGE ( 'NONE', *, *, #217766, .F. ) ;
#62811 = ORIENTED_EDGE ( 'NONE', *, *, #63496, .F. ) ;
#62812 = CARTESIAN_POINT ( 'NONE',  ( 22.50000000000000000, 75.95437663941535789, -81.17361182307570289 ) ) ;
#62813 = CARTESIAN_POINT ( 'NONE',  ( -21.64999999999999858, 68.65000000001199965, -115.3731074845243540 ) ) ;
#62814 = FACE_BOUND ( 'NONE', #9704, .T. ) ;
#62815 = CIRCLE ( 'NONE', #17051, 0.1000000000000028644 ) ;
#62816 = CARTESIAN_POINT ( 'NONE',  ( 20.95262331984771009, 10.50415726280093409, -141.5608883295933822 ) ) ;
#62818 = CARTESIAN_POINT ( 'NONE',  ( 17.23472005113826810, 65.69211804551103739, -80.97653062445571948 ) ) ;
#62817 = AXIS2_PLACEMENT_3D ( 'NONE', #215109, #73075, #53472 ) ;
#62821 = CARTESIAN_POINT ( 'NONE',  ( -22.59080734064477625, 31.82702841783757108, -238.8405965839959322 ) ) ;
#62820 = AXIS2_PLACEMENT_3D ( 'NONE', #18537, #118934, #243 ) ;
#62819 = DIRECTION ( 'NONE',  ( 0.000000000000000000, 0.1298341882519953583, 0.9915357197604862671 ) ) ;
#62822 = CYLINDRICAL_SURFACE ( 'NONE', #206606, 0.1000000000000142025 ) ;
#62823 = CARTESIAN_POINT ( 'NONE',  ( -22.50000000000000000, 64.35000000001167564, -69.52310748452438816 ) ) ;
#62824 = CARTESIAN_POINT ( 'NONE',  ( 22.40000000000010516, 76.00000000001317346, -148.1726782920694063 ) ) ;
#62825 = ORIENTED_EDGE ( 'NONE', *, *, #228405, .T. ) ;
#62826 = DIRECTION ( 'NONE',  ( 0.000000000000000000, -0.9910465087640866200, 0.1335171055202867274 ) ) ;
#62827 = EDGE_CURVE ( 'NONE', #57112, #188655, #226094, .T. ) ;
#62829 = ORIENTED_EDGE ( 'NONE', *, *, #210993, .T. ) ;
#62828 = CARTESIAN_POINT ( 'NONE',  ( 15.74999999999999645, 62.59162599727320497, -217.2417264603073477 ) ) ;
#62830 = AXIS2_PLACEMENT_3D ( 'NONE', #226027, #47408, #147823 ) ;
#62831 = DIRECTION ( 'NONE',  ( 1.000000000000000000, 0.000000000000000000, 0.000000000000000000 ) ) ;
#62832 = LINE ( 'NONE', #8009, #149176 ) ;
#62834 = CYLINDRICAL_SURFACE ( 'NONE', #257475, 0.09999999999999641120 ) ;
#62833 = CARTESIAN_POINT ( 'NONE',  ( 18.59999999999999787, -1.835859311432481045, -78.50443916879852679 ) ) ;
#62835 = VERTEX_POINT ( 'NONE', #60036 ) ;
#62836 = CARTESIAN_POINT ( 'NONE',  ( -18.50000000000000000, 85.40000000001160174, -62.22584772486096938 ) ) ;
#62837 = DIRECTION ( 'NONE',  ( -0.000000000000000000, -0.000000000000000000, 1.000000000000000000 ) ) ;
#62838 = CARTESIAN_POINT ( 'NONE',  ( 21.05000000000005400, 82.64476912853859858, -26.37791261425322986 ) ) ;
#62839 = DIRECTION ( 'NONE',  ( -1.000000000000000000, 0.000000000000000000, 0.000000000000000000 ) ) ;
#62841 = ADVANCED_FACE ( 'NONE', ( #23531 ), #139565, .T. ) ;
#62840 = CARTESIAN_POINT ( 'NONE',  ( 23.24999999999999645, 7.128833340093095217, -233.7327013124392749 ) ) ;
#62842 = EDGE_LOOP ( 'NONE', ( #19199, #89262, #19745, #130028 ) ) ;
#62844 = ORIENTED_EDGE ( 'NONE', *, *, #132850, .T. ) ;
#62843 = AXIS2_PLACEMENT_3D ( 'NONE', #160349, #99027, #123766 ) ;
#62845 = EDGE_CURVE ( 'NONE', #116722, #224475, #5901, .T. ) ;
#62846 = EDGE_CURVE ( 'NONE', #36945, #37194, #197450, .T. ) ;
#62847 = CARTESIAN_POINT ( 'NONE',  ( 20.27550659511088682, 9.216043722520002035, -76.25000000000004263 ) ) ;
#62848 = ORIENTED_EDGE ( 'NONE', *, *, #111161, .F. ) ;
#62849 = LINE ( 'NONE', #40760, #221873 ) ;
#62850 = ORIENTED_EDGE ( 'NONE', *, *, #92779, .F. ) ;
#62851 = DIRECTION ( 'NONE',  ( -0.000000000000000000, -0.000000000000000000, -1.000000000000000000 ) ) ;
#62852 = CARTESIAN_POINT ( 'NONE',  ( 20.85000000000000142, 1.115600667400684642E-11, -108.4000000000000483 ) ) ;
#62853 = ORIENTED_EDGE ( 'NONE', *, *, #80809, .F. ) ;
#62854 = EDGE_CURVE ( 'NONE', #236709, #223475, #17818, .T. ) ;
#62855 = EDGE_CURVE ( 'NONE', #243446, #81993, #163589, .T. ) ;
#62856 = CARTESIAN_POINT ( 'NONE',  ( -20.00857864376270001, 9.150000000011157653, -179.8499999999999943 ) ) ;
#62857 = CARTESIAN_POINT ( 'NONE',  ( -20.90000000000000213, 6.644425182197215562, 9.641788261573355001 ) ) ;
#62858 = AXIS2_PLACEMENT_3D ( 'NONE', #204226, #243352, #144238 ) ;
#62859 = DIRECTION ( 'NONE',  ( -0.000000000000000000, 0.000000000000000000, -1.000000000000000000 ) ) ;
#62860 = CARTESIAN_POINT ( 'NONE',  ( 16.87683809663750267, 9.950000000011138823, -113.1500000000000341 ) ) ;
#62861 = PRODUCT_DEFINITION ( 'UNKNOWN', '', #232138, #254010 ) ;
#62862 = PLANE ( 'NONE',  #187256 ) ;
#62863 = B_SPLINE_CURVE_WITH_KNOTS ( 'NONE', 3,
 ( #100745, #59062, #255961, #392 ),
 .UNSPECIFIED., .F., .F.,
 ( 4, 4 ),
 ( 0.000000000000000000, 0.001767853679387123601 ),
 .UNSPECIFIED. ) ;
#62865 = CARTESIAN_POINT ( 'NONE',  ( 14.56326696814971555, 62.06361769656462712, -218.8193597571736007 ) ) ;
#62864 = AXIS2_PLACEMENT_3D ( 'NONE', #96260, #62280, #58401 ) ;
#62866 = ORIENTED_EDGE ( 'NONE', *, *, #126828, .F. ) ;
#62868 = CARTESIAN_POINT ( 'NONE',  ( 21.05000000000000071, 6.650000000011155876, -76.84382208968317229 ) ) ;
#62867 = FACE_OUTER_BOUND ( 'NONE', #162841, .T. ) ;
#62869 = ORIENTED_EDGE ( 'NONE', *, *, #1998, .T. ) ;
#62871 = ORIENTED_EDGE ( 'NONE', *, *, #112716, .T. ) ;
#62870 = LINE ( 'NONE', #142402, #135720 ) ;
#62872 = EDGE_LOOP ( 'NONE', ( #49535, #204942, #219667, #185823 ) ) ;
#62873 = FACE_BOUND ( 'NONE', #121883, .T. ) ;
#62874 = DIRECTION ( 'NONE',  ( 0.000000000000000000, 0.000000000000000000, -1.000000000000000000 ) ) ;
#62875 = PLANE ( 'NONE',  #180613 ) ;
#62876 = EDGE_CURVE ( 'NONE', #137320, #66524, #243237, .T. ) ;
#62877 = DIRECTION ( 'NONE',  ( 0.000000000000000000, -0.008583690987135041833, 0.9999631594459055250 ) ) ;
#62878 = TOROIDAL_SURFACE ( 'NONE', #141975, 0.4000000000000003553, 0.1000000000000000056 ) ;
#62879 = ORIENTED_EDGE ( 'NONE', *, *, #224617, .F. ) ;
#62880 = ADVANCED_FACE ( 'NONE', ( #187722 ), #130828, .T. ) ;
#62881 = ADVANCED_FACE ( 'NONE', ( #67754 ), #169466, .T. ) ;
#62882 = DIRECTION ( 'NONE',  ( -3.469446951953635015E-14, 0.000000000000000000, -1.000000000000000000 ) ) ;
#62883 = DIRECTION ( 'NONE',  ( 0.5932847527679309119, 0.7769265190100945739, -0.2107092456252266377 ) ) ;
#62884 = ORIENTED_EDGE ( 'NONE', *, *, #198327, .F. ) ;
#62885 = DIRECTION ( 'NONE',  ( 0.000000000000000000, 0.000000000000000000, 1.000000000000000000 ) ) ;
#62886 = AXIS2_PLACEMENT_3D ( 'NONE', #155903, #37229, #178026 ) ;
#62887 = ORIENTED_EDGE ( 'NONE', *, *, #121236, .T. ) ;
#62888 = DIRECTION ( 'NONE',  ( -1.000000000000000000, -0.000000000000000000, -0.000000000000000000 ) ) ;
#62889 = AXIS2_PLACEMENT_3D ( 'NONE', #239295, #144029, #41116 ) ;
#62890 = TOROIDAL_SURFACE ( 'NONE', #237683, 0.4000000000000017431, 0.1000000000000000056 ) ;
#62891 = DIRECTION ( 'NONE',  ( -7.304098846218132695E-16, -0.9770955615653315052, -0.2128009952263603954 ) ) ;
#62892 = ORIENTED_EDGE ( 'NONE', *, *, #10347, .F. ) ;
#62893 = CARTESIAN_POINT ( 'NONE',  ( -18.59999999999999787, 76.00000000001142553, -36.02310748452432421 ) ) ;
#62894 = STYLED_ITEM ( 'NONE', ( #63772 ), #194237 ) ;
#62895 = CARTESIAN_POINT ( 'NONE',  ( 21.05000000000000071, 6.540656951712400691, -134.1000000000000227 ) ) ;
#62896 = CARTESIAN_POINT ( 'NONE',  ( -21.05000000000000071, 87.48912529308822172, -139.4231074845242802 ) ) ;
#62897 = CIRCLE ( 'NONE', #204540, 0.5000000000000004441 ) ;
#62898 = AXIS2_PLACEMENT_3D ( 'NONE', #94331, #168798, #149204 ) ;
#62899 = DIRECTION ( 'NONE',  ( -3.265361837132813093E-16, -1.000000000000000000, 7.445645354460596589E-46 ) ) ;
#62900 = ADVANCED_FACE ( 'NONE', ( #243817 ), #10364, .T. ) ;
#62901 = CARTESIAN_POINT ( 'NONE',  ( -23.15000000000000213, 30.38404434817536526, -239.4399867032565794 ) ) ;
#62902 = CARTESIAN_POINT ( 'NONE',  ( 20.85000000000000142, 11.75000000001115907, -134.0000000000000284 ) ) ;
#62903 = AXIS2_PLACEMENT_3D ( 'NONE', #23062, #202947, #183402 ) ;
#62905 = DIRECTION ( 'NONE',  ( 0.000000000000000000, 0.8814952561688438326, -0.4721928772777331251 ) ) ;
#62904 = VECTOR ( 'NONE', #232282, 1000.000000000000000 ) ;
#62906 = AXIS2_PLACEMENT_3D ( 'NONE', #86188, #119257, #243996 ) ;
#62907 = ORIENTED_EDGE ( 'NONE', *, *, #155374, .F. ) ;
#62910 = DIRECTION ( 'NONE',  ( 0.000000000000000000, 0.8814952561688359500, -0.4721928772777482242 ) ) ;
#62909 = DIRECTION ( 'NONE',  ( 0.000000000000000000, -7.429790795770644761E-15, 1.000000000000000000 ) ) ;
#62908 = AXIS2_PLACEMENT_3D ( 'NONE', #72421, #68557, #52819 ) ;
#62911 = AXIS2_PLACEMENT_3D ( 'NONE', #12838, #67650, #147186 ) ;
#62912 = VERTEX_POINT ( 'NONE', #84705 ) ;
#62913 = DIRECTION ( 'NONE',  ( 0.000000000000000000, 0.9654727137038715545, 0.2605042016806676242 ) ) ;
#62914 = EDGE_CURVE ( 'NONE', #46944, #37340, #66471, .T. ) ;
#62915 = DIRECTION ( 'NONE',  ( 0.000000000000000000, 0.2128009952263603677, -0.9770955615653313941 ) ) ;
#62917 = ORIENTED_EDGE ( 'NONE', *, *, #147508, .F. ) ;
#62916 = CARTESIAN_POINT ( 'NONE',  ( -12.25000000000000178, 66.65000000001155911, -52.77310748452439526 ) ) ;
#62919 = VERTEX_POINT ( 'NONE', #208570 ) ;
#62918 = DIRECTION ( 'NONE',  ( 0.000000000000000000, 0.9770955615653317272, 0.2128009952263595073 ) ) ;
#62920 = FACE_OUTER_BOUND ( 'NONE', #249907, .T. ) ;
#62921 = CARTESIAN_POINT ( 'NONE',  ( 23.14999999999999858, 5.000000000011153745, -54.59473398108690390 ) ) ;
#62922 = CYLINDRICAL_SURFACE ( 'NONE', #235355, 0.09999999999999641120 ) ;
#62923 = ADVANCED_FACE ( 'NONE', ( #247674 ), #167515, .T. ) ;
#62924 = CARTESIAN_POINT ( 'NONE',  ( -23.15000000000000213, 85.60000000001245724, -181.7731074845243029 ) ) ;
#62925 = TOROIDAL_SURFACE ( 'NONE', #241973, 0.2000000000000000111, 0.1000000000000000056 ) ;
#62927 = ORIENTED_EDGE ( 'NONE', *, *, #185527, .F. ) ;
#62926 = DIRECTION ( 'NONE',  ( 0.000000000000000000, 0.000000000000000000, -1.000000000000000000 ) ) ;
#62928 = EDGE_CURVE ( 'NONE', #194903, #150427, #126350, .T. ) ;
#62930 = EDGE_CURVE ( 'NONE', #210814, #100043, #101344, .T. ) ;
#62929 = CARTESIAN_POINT ( 'NONE',  ( 20.94999999999999929, 5.500000000011153745, -112.9052660189131245 ) ) ;
#62932 = EDGE_CURVE ( 'NONE', #58399, #32909, #84611, .T. ) ;
#62931 = ORIENTED_EDGE ( 'NONE', *, *, #65544, .F. ) ;
#62933 = EDGE_LOOP ( 'NONE', ( #154132, #183041, #155430, #89523 ) ) ;
#62934 = DIRECTION ( 'NONE',  ( 1.000000000000000000, -0.000000000000000000, -0.000000000000000000 ) ) ;
#62935 = DIRECTION ( 'NONE',  ( -1.000000000000000000, 0.000000000000000000, 0.000000000000000000 ) ) ;
#62936 = ORIENTED_EDGE ( 'NONE', *, *, #156937, .F. ) ;
#62937 = CARTESIAN_POINT ( 'NONE',  ( -20.54999999999999716, 1.115600667400684642E-11, -154.6250000000000284 ) ) ;
#62938 = AXIS2_PLACEMENT_3D ( 'NONE', #257901, #79297, #158883 ) ;
#62939 = CARTESIAN_POINT ( 'NONE',  ( -23.15000000000000213, 11.75000000001115907, -60.15839931010294350 ) ) ;
#62940 = ORIENTED_EDGE ( 'NONE', *, *, #209202, .F. ) ;
#62942 = EDGE_CURVE ( 'NONE', #134658, #187156, #225511, .T. ) ;
#62941 = CARTESIAN_POINT ( 'NONE',  ( 23.14999999999999858, 1.115600667400684642E-11, -134.0000000000000284 ) ) ;
#62943 = ADVANCED_FACE ( 'NONE', ( #5179 ), #123887, .T. ) ;
#62944 = CARTESIAN_POINT ( 'NONE',  ( 18.59999999999999076, 6.550000000011156231, -54.75000000000000000 ) ) ;
#62946 = ORIENTED_EDGE ( 'NONE', *, *, #41725, .F. ) ;
#62945 = AXIS2_PLACEMENT_3D ( 'NONE', #99923, #118237, #2120 ) ;
#62947 = EDGE_LOOP ( 'NONE', ( #24506, #239906, #253658, #26143 ) ) ;
#62948 = DIRECTION ( 'NONE',  ( 0.000000000000000000, 1.000000000000000000, 0.000000000000000000 ) ) ;
#62949 = ORIENTED_EDGE ( 'NONE', *, *, #20351, .T. ) ;
#62950 = ADVANCED_FACE ( 'NONE', ( #205979 ), #176258, .T. ) ;
#62951 = LINE ( 'NONE', #202468, #179535 ) ;
#62952 = ORIENTED_EDGE ( 'NONE', *, *, #80897, .T. ) ;
#62954 = EDGE_LOOP ( 'NONE', ( #179418, #124777, #133492, #233026 ) ) ;
#62953 = CARTESIAN_POINT ( 'NONE',  ( 18.59999999999999076, 67.23127455305835554, -235.8551265064784559 ) ) ;
#62955 = CARTESIAN_POINT ( 'NONE',  ( 20.94999999999999929, 30.00470580581253799, -236.0305482155950472 ) ) ;
#62956 = VERTEX_POINT ( 'NONE', #203420 ) ;
#62957 = CARTESIAN_POINT ( 'NONE',  ( -21.93340585899455419, 1.115541036281197940E-11, -93.17585297787972820 ) ) ;
#62959 = ORIENTED_EDGE ( 'NONE', *, *, #126166, .F. ) ;
#62958 = EDGE_CURVE ( 'NONE', #248782, #127836, #65178, .T. ) ;
#62961 = EDGE_LOOP ( 'NONE', ( #10028, #163116, #185389, #14499 ) ) ;
#62960 = ORIENTED_EDGE ( 'NONE', *, *, #118590, .T. ) ;
#62962 = DIRECTION ( 'NONE',  ( -6.938893903907222856E-15, -0.4088369013363280513, 0.9126074666063769270 ) ) ;
#62963 = ADVANCED_FACE ( 'NONE', ( #183848 ), #34797, .F. ) ;
#62964 = CARTESIAN_POINT ( 'NONE',  ( -23.15000000000000213, 11.75000000001115552, -88.35000000000003695 ) ) ;
#62965 = AXIS2_PLACEMENT_3D ( 'NONE', #212238, #93547, #113118 ) ;
#62966 = EDGE_LOOP ( 'NONE', ( #175074, #33248, #75268, #148567 ) ) ;
#62967 = CIRCLE ( 'NONE', #17201, 7.899999999999990585 ) ;
#62968 = VECTOR ( 'NONE', #31198, 1000.000000000000000 ) ;
#62969 = EDGE_CURVE ( 'NONE', #225825, #72318, #205439, .T. ) ;
#62970 = ORIENTED_EDGE ( 'NONE', *, *, #102395, .F. ) ;
#62971 = CARTESIAN_POINT ( 'NONE',  ( 21.05000000000000071, 76.00000000001243450, -168.0231074845243597 ) ) ;
#62972 = DIRECTION ( 'NONE',  ( -1.000000000000000000, 0.000000000000000000, 0.000000000000000000 ) ) ;
#62974 = EDGE_LOOP ( 'NONE', ( #210789, #30158, #234038, #64578 ) ) ;
#62973 = CARTESIAN_POINT ( 'NONE',  ( -18.59999999999999787, 69.06610602788505560, -32.23746165015079868 ) ) ;
#62975 = ORIENTED_EDGE ( 'NONE', *, *, #225571, .T. ) ;
#62976 = DIRECTION ( 'NONE',  ( 1.000000000000000000, 0.000000000000000000, 0.000000000000000000 ) ) ;
#62977 = CARTESIAN_POINT ( 'NONE',  ( -20.64999999999999858, 71.65000000001155911, -57.17310748452435121 ) ) ;
#62978 = EDGE_CURVE ( 'NONE', #217227, #207656, #142884, .T. ) ;
#62979 = ORIENTED_EDGE ( 'NONE', *, *, #7199, .F. ) ;
#62980 = DIRECTION ( 'NONE',  ( 0.000000000000000000, 0.8814952561688429444, -0.4721928772777345684 ) ) ;
#62981 = CARTESIAN_POINT ( 'NONE',  ( 20.94999999999999929, -8.999999999988844479, -110.3939691226524786 ) ) ;
#62982 = CIRCLE ( 'NONE', #192353, 0.3999999999999952482 ) ;
#62983 = ORIENTED_EDGE ( 'NONE', *, *, #507, .T. ) ;
#62984 = CYLINDRICAL_SURFACE ( 'NONE', #38972, 0.1000000000000028644 ) ;
#62985 = ORIENTED_EDGE ( 'NONE', *, *, #97611, .T. ) ;
#62987 = ORIENTED_EDGE ( 'NONE', *, *, #227971, .F. ) ;
#62986 = ORIENTED_EDGE ( 'NONE', *, *, #220763, .T. ) ;
#62988 = EDGE_LOOP ( 'NONE', ( #7314, #197518, #35617, #115735 ) ) ;
#62989 = CARTESIAN_POINT ( 'NONE',  ( -21.55000000000000071, 68.65000000001150227, -48.37310748452437537 ) ) ;
#62990 = ORIENTED_EDGE ( 'NONE', *, *, #89203, .F. ) ;
#62991 = LINE ( 'NONE', #142516, #79943 ) ;
#62992 = VERTEX_POINT ( 'NONE', #238038 ) ;
#62993 = CARTESIAN_POINT ( 'NONE',  ( 20.94999999999999574, 10.47338541492405994, -108.0786544642485865 ) ) ;
#62994 = CARTESIAN_POINT ( 'NONE',  ( 20.94999999999999929, 85.50000000001179501, -79.41707660717668205 ) ) ;
#62995 = ORIENTED_EDGE ( 'NONE', *, *, #161238, .T. ) ;
#62996 = AXIS2_PLACEMENT_3D ( 'NONE', #14051, #31068, #110561 ) ;
#62997 = AXIS2_PLACEMENT_3D ( 'NONE', #128627, #205567, #49072 ) ;
#62998 = ORIENTED_EDGE ( 'NONE', *, *, #24520, .T. ) ;
#62999 = EDGE_LOOP ( 'NONE', ( #252465, #40956, #35457, #245153 ) ) ;
#63000 = EDGE_CURVE ( 'NONE', #9118, #207310, #38880, .T. ) ;
#63001 = CARTESIAN_POINT ( 'NONE',  ( 23.14999999999999503, 64.25000000001227818, -157.8731074845244393 ) ) ;
#63002 = ORIENTED_EDGE ( 'NONE', *, *, #148686, .F. ) ;
#63003 = CARTESIAN_POINT ( 'NONE',  ( 20.95512820512820440, 12.96604748760834092, -210.6109454999921411 ) ) ;
#63004 = CARTESIAN_POINT ( 'NONE',  ( 18.49999999999999289, 65.75000000001179501, -81.67310748452439384 ) ) ;
#63005 = CARTESIAN_POINT ( 'NONE',  ( -18.59999999999999787, 66.65000000001229807, -157.6731074845244223 ) ) ;
#63006 = FACE_OUTER_BOUND ( 'NONE', #72950, .T. ) ;
#63007 = AXIS2_PLACEMENT_3D ( 'NONE', #92325, #156185, #192726 ) ;
#63008 = LINE ( 'NONE', #222055, #19403 ) ;
#63009 = DIRECTION ( 'NONE',  ( -1.000000000000000000, 2.775557561562908012E-13, 0.000000000000000000 ) ) ;
#63011 = CARTESIAN_POINT ( 'NONE',  ( 21.07933241753356768, 6.328645948390904330, -100.4066204095807393 ) ) ;
#63010 = CARTESIAN_POINT ( 'NONE',  ( -22.39999999999999858, 76.00000000001213607, -136.6231074845242972 ) ) ;
#63012 = DIRECTION ( 'NONE',  ( 0.000000000000000000, 0.2818822000685679008, -0.9594490217226259166 ) ) ;
#63013 = CARTESIAN_POINT ( 'NONE',  ( -18.50000000000000000, 11.65000000001115232, -45.65000000000000568 ) ) ;
#63014 = DIRECTION ( 'NONE',  ( -0.000000000000000000, -1.000000000000000000, 6.308085367188393199E-16 ) ) ;
#63015 = EDGE_CURVE ( 'NONE', #201244, #31259, #68083, .T. ) ;
#63016 = FACE_OUTER_BOUND ( 'NONE', #101185, .T. ) ;
#63017 = ORIENTED_EDGE ( 'NONE', *, *, #157408, .T. ) ;
#63019 = ORIENTED_EDGE ( 'NONE', *, *, #108051, .F. ) ;
#63018 = CARTESIAN_POINT ( 'NONE',  ( 23.24999999999999645, 1.115600667400684642E-11, -100.5000000000000284 ) ) ;
#63020 = ORIENTED_EDGE ( 'NONE', *, *, #249922, .T. ) ;
#63021 = CARTESIAN_POINT ( 'NONE',  ( -20.54999999999999716, 2.000000000011154189, -147.2246219227621111 ) ) ;
#63022 = VECTOR ( 'NONE', #232193, 1000.000000000000000 ) ;
#63023 = CARTESIAN_POINT ( 'NONE',  ( 20.50589344625199217, 10.48318793148705197, -141.5729949786710336 ) ) ;
#63024 = DIRECTION ( 'NONE',  ( 1.000000000000000000, 0.000000000000000000, 0.000000000000000000 ) ) ;
#63025 = ORIENTED_EDGE ( 'NONE', *, *, #197713, .F. ) ;
#63026 = TOROIDAL_SURFACE ( 'NONE', #208798, 6.258578643762712446, 0.1000000000000000056 ) ;
#63027 = PRESENTATION_STYLE_ASSIGNMENT (( #241677 ) ) ;
#63028 = CARTESIAN_POINT ( 'NONE',  ( 15.48841904831874849, 67.43841904833132617, -182.6731074845244223 ) ) ;
#63029 = AXIS2_PLACEMENT_3D ( 'NONE', #72570, #93388, #172977 ) ;
#63030 = CYLINDRICAL_SURFACE ( 'NONE', #24936, 0.1000000000000028644 ) ;
#63031 = ORIENTED_EDGE ( 'NONE', *, *, #73539, .F. ) ;
#63032 = DIRECTION ( 'NONE',  ( 1.000000000000000000, 0.000000000000000000, 0.000000000000000000 ) ) ;
#63033 = CARTESIAN_POINT ( 'NONE',  ( -21.45000000000000284, 68.29142135624915966, -90.67310748452436542 ) ) ;
#63034 = CIRCLE ( 'NONE', #125428, 0.09999999999999939493 ) ;
#63035 = CARTESIAN_POINT ( 'NONE',  ( 18.39999999999997371, 54.09900352584866567, -229.1663746252470446 ) ) ;
#63036 = AXIS2_PLACEMENT_3D ( 'NONE', #134292, #15682, #235968 ) ;
#63037 = DIRECTION ( 'NONE',  ( 1.000000000000000000, 0.000000000000000000, 0.000000000000000000 ) ) ;
#63039 = ORIENTED_EDGE ( 'NONE', *, *, #82390, .F. ) ;
#63038 = CARTESIAN_POINT ( 'NONE',  ( -16.97683809663753252, 66.05000000001230376, -156.7515827158544823 ) ) ;
#63040 = CARTESIAN_POINT ( 'NONE',  ( 22.50000000000000000, 64.08545097430041437, -247.0723585184913986 ) ) ;
#63042 = ORIENTED_EDGE ( 'NONE', *, *, #211467, .T. ) ;
#63041 = DIRECTION ( 'NONE',  ( -1.000000000000000000, 3.265361837132813093E-16, 2.280189983783949500E-30 ) ) ;
#63043 = DIRECTION ( 'NONE',  ( 1.000000000000000000, 0.000000000000000000, 0.000000000000000000 ) ) ;
#63045 = VECTOR ( 'NONE', #136130, 999.9999999999998863 ) ;
#63044 = LINE ( 'NONE', #65617, #16683 ) ;
#63046 = CARTESIAN_POINT ( 'NONE',  ( -16.93906926870270624, 65.98785312906574063, -157.4696551772975965 ) ) ;
#63047 = CARTESIAN_POINT ( 'NONE',  ( -20.85000000000000142, 68.97833521811131163, -32.18954208262707795 ) ) ;
#63049 = DIRECTION ( 'NONE',  ( 0.000000000000000000, -1.000000000000000000, 0.000000000000000000 ) ) ;
#63048 = LINE ( 'NONE', #100853, #182430 ) ;
#63050 = CARTESIAN_POINT ( 'NONE',  ( 21.05000000000000071, -0.09770955614504285569, -201.0212800995241764 ) ) ;
#63052 = EDGE_CURVE ( 'NONE', #19574, #118769, #63818, .T. ) ;
#63051 = LINE ( 'NONE', #86444, #170048 ) ;
#63054 = CARTESIAN_POINT ( 'NONE',  ( -20.94999999999999929, 64.25000000001233502, -163.1815067946273246 ) ) ;
#63053 = CIRCLE ( 'NONE', #87979, 0.09999999999999986677 ) ;
#63055 = DIRECTION ( 'NONE',  ( 1.000000000000000000, 7.136802563874199107E-16, 1.554319503706929991E-16 ) ) ;
#63056 = DIRECTION ( 'NONE',  ( -1.000000000000000000, 0.000000000000000000, 0.000000000000000000 ) ) ;
#63057 = AXIS2_PLACEMENT_3D ( 'NONE', #77987, #16765, #55836 ) ;
#63058 = ORIENTED_EDGE ( 'NONE', *, *, #140901, .T. ) ;
#63059 = CARTESIAN_POINT ( 'NONE',  ( 21.05000000000000071, 9.374458193048763377, -220.5475659691911119 ) ) ;
#63060 = ORIENTED_EDGE ( 'NONE', *, *, #117485, .T. ) ;
#63061 = AXIS2_PLACEMENT_3D ( 'NONE', #37184, #218344, #56688 ) ;
#63062 = ORIENTED_EDGE ( 'NONE', *, *, #28576, .T. ) ;
#63063 = EDGE_CURVE ( 'NONE', #163271, #19038, #209838, .T. ) ;
#63064 = DIRECTION ( 'NONE',  ( 0.000000000000000000, 0.9126074666062508056, 0.4088369013366094928 ) ) ;
#63065 = CARTESIAN_POINT ( 'NONE',  ( -21.14999999999999858, 87.65000000001165859, -69.52310748452424605 ) ) ;
#63066 = VERTEX_POINT ( 'NONE', #217180 ) ;
#63067 = VECTOR ( 'NONE', #90166, 1000.000000000000000 ) ;
#63068 = EDGE_CURVE ( 'NONE', #81897, #66231, #209552, .T. ) ;
#63069 = VERTEX_POINT ( 'NONE', #176810 ) ;
#63070 = EDGE_CURVE ( 'NONE', #162124, #94393, #98487, .T. ) ;
#63072 = ORIENTED_EDGE ( 'NONE', *, *, #246878, .T. ) ;
#63071 = CIRCLE ( 'NONE', #196352, 0.09999999999999939493 ) ;
#63073 = DIRECTION ( 'NONE',  ( -1.000000000000000000, 0.000000000000000000, 0.000000000000000000 ) ) ;
#63074 = AXIS2_PLACEMENT_3D ( 'NONE', #135399, #196660, #114574 ) ;
#63075 = AXIS2_PLACEMENT_3D ( 'NONE', #244981, #199464, #20827 ) ;
#63076 = ORIENTED_EDGE ( 'NONE', *, *, #127605, .F. ) ;
#63077 = AXIS2_PLACEMENT_3D ( 'NONE', #201714, #163886, #62213 ) ;
#63078 = CARTESIAN_POINT ( 'NONE',  ( 23.14999999999999503, 69.55000000001150795, -48.37310748452436826 ) ) ;
#63079 = PLANE ( 'NONE',  #70248 ) ;
#63080 = DIRECTION ( 'NONE',  ( 1.000000000000000000, -1.772924042024179204E-16, 4.808324575169891715E-17 ) ) ;
#63081 = FACE_OUTER_BOUND ( 'NONE', #39530, .T. ) ;
#63082 = CARTESIAN_POINT ( 'NONE',  ( -18.59999999999999787, 66.46020053479900014, -223.7494053730254961 ) ) ;
#63083 = DIRECTION ( 'NONE',  ( 0.000000000000000000, 0.000000000000000000, -1.000000000000000000 ) ) ;
#63084 = DIRECTION ( 'NONE',  ( -1.000000000000000000, 0.000000000000000000, -0.000000000000000000 ) ) ;
#63086 = ORIENTED_EDGE ( 'NONE', *, *, #139837, .T. ) ;
#63085 = LINE ( 'NONE', #219587, #146608 ) ;
#63088 = CARTESIAN_POINT ( 'NONE',  ( 20.94999999999999574, 6.550000000011159784, -143.8438220896831581 ) ) ;
#63087 = CYLINDRICAL_SURFACE ( 'NONE', #212902, 0.09999999999999609201 ) ;
#63089 = EDGE_CURVE ( 'NONE', #61093, #228115, #36014, .T. ) ;
#63090 = CARTESIAN_POINT ( 'NONE',  ( -23.25000000000000000, -11.48087284838115885, -203.5004116939112464 ) ) ;
#63091 =( BOUNDED_CURVE ( )  B_SPLINE_CURVE ( 3, ( #40424, #119957, #255524, #20848 ),
 .UNSPECIFIED., .F., .T. ) 
 B_SPLINE_CURVE_WITH_KNOTS ( ( 4, 4 ),
 ( 3.141592653589917017, 4.712388980384686121 ),
 .UNSPECIFIED. ) 
 CURVE ( )  GEOMETRIC_REPRESENTATION_ITEM ( )  RATIONAL_B_SPLINE_CURVE ( ( 1.000000000000000000, 0.8047378541243951355, 0.8047378541243951355, 1.000000000000000000 ) ) 
 REPRESENTATION_ITEM ( '' )  );
#63092 = ORIENTED_EDGE ( 'NONE', *, *, #57231, .F. ) ;
#63093 = CARTESIAN_POINT ( 'NONE',  ( 20.94999999999999929, 67.12338541492449906, -61.13802700567970305 ) ) ;
#63094 = ORIENTED_EDGE ( 'NONE', *, *, #243411, .T. ) ;
#63095 = CARTESIAN_POINT ( 'NONE',  ( -21.14999999999994174, 69.83923505573476120, -35.48358590217651454 ) ) ;
#63096 = DIRECTION ( 'NONE',  ( 1.000000000000000000, 0.000000000000000000, 0.000000000000000000 ) ) ;
#63097 = ORIENTED_EDGE ( 'NONE', *, *, #92283, .F. ) ;
#63098 = DIRECTION ( 'NONE',  ( 0.000000000000000000, -1.000000000000000000, 0.000000000000000000 ) ) ;
#63099 = FACE_OUTER_BOUND ( 'NONE', #213776, .T. ) ;
#63100 = CARTESIAN_POINT ( 'NONE',  ( -22.39999999999999858, -0.1008583690875575894, -21.75043287651061164 ) ) ;
#63101 = CARTESIAN_POINT ( 'NONE',  ( -23.25000000000000000, 7.021664781911246322, -171.3335654018973173 ) ) ;
#63102 = EDGE_LOOP ( 'NONE', ( #123985, #128777, #119138, #242085 ) ) ;
#63103 = B_SPLINE_CURVE_WITH_KNOTS ( 'NONE', 3,
 ( #111688, #12616, #153431, #172991, #15170, #94683 ),
 .UNSPECIFIED., .F., .F.,
 ( 4, 2, 4 ),
 ( 0.000000000000000000, 0.0001891491689349583357, 0.0003782983378699166714 ),
 .UNSPECIFIED. ) ;
#63104 = AXIS2_PLACEMENT_3D ( 'NONE', #15202, #94713, #174312 ) ;
#63105 = ADVANCED_FACE ( 'NONE', ( #218462 ), #38567, .T. ) ;
#63106 = CARTESIAN_POINT ( 'NONE',  ( -20.54999999999999716, 76.00000000001189449, -101.1231074845242972 ) ) ;
#63107 = FACE_OUTER_BOUND ( 'NONE', #197094, .T. ) ;
#63108 = CARTESIAN_POINT ( 'NONE',  ( 16.87683809663749557, 66.05000000001203375, -115.6731074845243654 ) ) ;
#63109 = DIRECTION ( 'NONE',  ( -1.000000000000000000, 0.000000000000000000, 0.000000000000000000 ) ) ;
#63110 = CARTESIAN_POINT ( 'NONE',  ( -20.64999999999999858, 4.250000000000000000, -21.14999999999999858 ) ) ;
#63111 =( BOUNDED_CURVE ( )  B_SPLINE_CURVE ( 3, ( #78896, #178045, #56753, #176758 ),
 .UNSPECIFIED., .F., .F. ) 
 B_SPLINE_CURVE_WITH_KNOTS ( ( 4, 4 ),
 ( 0.3000847527772375622, 0.5517402753107888413 ),
 .UNSPECIFIED. ) 
 CURVE ( )  GEOMETRIC_REPRESENTATION_ITEM ( )  RATIONAL_B_SPLINE_CURVE ( ( 1.000000000000000000, 0.9947294176030464508, 0.9947294176030464508, 1.000000000000000000 ) ) 
 REPRESENTATION_ITEM ( '' )  );
#63112 = ADVANCED_FACE ( 'NONE', ( #91166 ), #151156, .F. ) ;
#63113 = CIRCLE ( 'NONE', #146321, 0.1000000000000013933 ) ;
#63115 = VERTEX_POINT ( 'NONE', #138903 ) ;
#63114 = DIRECTION ( 'NONE',  ( 0.000000000000000000, 6.982962677686266711E-15, -1.000000000000000000 ) ) ;
#63116 = DIRECTION ( 'NONE',  ( 2.952720810173289605E-16, -0.9770955615653357240, -0.2128009952263412996 ) ) ;
#63117 = FACE_OUTER_BOUND ( 'NONE', #120188, .T. ) ;
#63118 = CARTESIAN_POINT ( 'NONE',  ( -21.14250536705909411, 76.00000000001169553, -76.04127966140507056 ) ) ;
#63119 = DIRECTION ( 'NONE',  ( -0.4999999999999799050, 0.2266847461454426782, 0.8358313381687697552 ) ) ;
#63120 = CARTESIAN_POINT ( 'NONE',  ( 23.14999999999999503, 8.882751598337874199, -187.0399955572217721 ) ) ;
#63122 = ORIENTED_EDGE ( 'NONE', *, *, #74646, .F. ) ;
#63121 = CARTESIAN_POINT ( 'NONE',  ( 21.11747605621531321, 67.22129199451867976, -57.27854431473461005 ) ) ;
#63123 = DIRECTION ( 'NONE',  ( -1.000000000000000000, 0.000000000000000000, 0.000000000000000000 ) ) ;
#63124 = DIRECTION ( 'NONE',  ( 1.000000000000000000, -0.000000000000000000, 0.000000000000000000 ) ) ;
#63125 = FACE_OUTER_BOUND ( 'NONE', #67152, .T. ) ;
#63126 = ADVANCED_FACE ( 'NONE', ( #110727 ), #251224, .F. ) ;
#63127 = ORIENTED_EDGE ( 'NONE', *, *, #120685, .T. ) ;
#63128 = CARTESIAN_POINT ( 'NONE',  ( -12.92414019175887141, 66.58236703690597835, -151.8741590187921133 ) ) ;
#63129 = SPHERICAL_SURFACE ( 'NONE', #60857, 0.1000000000000000056 ) ;
#63130 = FACE_OUTER_BOUND ( 'NONE', #143613, .T. ) ;
#63131 = EDGE_CURVE ( 'NONE', #78889, #33727, #76033, .T. ) ;
#63133 = CIRCLE ( 'NONE', #208893, 0.1000000000000028644 ) ;
#63132 = LINE ( 'NONE', #142664, #80073 ) ;
#63134 = ORIENTED_EDGE ( 'NONE', *, *, #158554, .F. ) ;
#63136 = AXIS2_PLACEMENT_3D ( 'NONE', #89016, #113417, #248098 ) ;
#63135 = DIRECTION ( 'NONE',  ( -1.000000000000000000, 0.000000000000000000, 0.000000000000000000 ) ) ;
#63137 = ORIENTED_EDGE ( 'NONE', *, *, #12986, .T. ) ;
#63138 = TOROIDAL_SURFACE ( 'NONE', #150636, 0.6000000000000013101, 0.1000000000000000056 ) ;
#63139 = CARTESIAN_POINT ( 'NONE',  ( -18.50000000000000000, 67.23127455305841238, -235.8551265064783991 ) ) ;
#63140 = DIRECTION ( 'NONE',  ( 1.000000000000000000, 0.000000000000000000, 0.000000000000000000 ) ) ;
#63141 = EDGE_CURVE ( 'NONE', #238715, #181403, #42973, .T. ) ;
#63142 = CARTESIAN_POINT ( 'NONE',  ( 20.94999999999999929, 85.00000000001251976, -179.9170766071767389 ) ) ;
#63143 = LINE ( 'NONE', #145251, #18541 ) ;
#63144 = ORIENTED_EDGE ( 'NONE', *, *, #64454, .F. ) ;
#63145 = CARTESIAN_POINT ( 'NONE',  ( 20.95561247346651967, 10.59500736521470721, -175.0937827669816329 ) ) ;
#63146 = EDGE_CURVE ( 'NONE', #233644, #161463, #172200, .T. ) ;
#63148 = EDGE_CURVE ( 'NONE', #126038, #250243, #181930, .T. ) ;
#63147 = DIRECTION ( 'NONE',  ( 1.000000000000000000, 0.000000000000000000, 0.000000000000000000 ) ) ;
#63149 = B_SPLINE_CURVE_WITH_KNOTS ( 'NONE', 3,
 ( #134723, #214286, #240277, #39531 ),
 .UNSPECIFIED., .F., .F.,
 ( 4, 4 ),
 ( 0.000000000000000000, 7.713889350930586977E-05 ),
 .UNSPECIFIED. ) ;
#63150 = VECTOR ( 'NONE', #38793, 1000.000000000000000 ) ;
#63151 = DIRECTION ( 'NONE',  ( 0.000000000000000000, -0.000000000000000000, 1.000000000000000000 ) ) ;
#63152 = CYLINDRICAL_SURFACE ( 'NONE', #161955, 0.1000000000000075273 ) ;
#63153 = CYLINDRICAL_SURFACE ( 'NONE', #211077, 0.09999999999999939493 ) ;
#63154 = DIRECTION ( 'NONE',  ( 0.000000000000000000, 1.000000000000000000, 6.982962677686266711E-15 ) ) ;
#63155 = VERTEX_POINT ( 'NONE', #104912 ) ;
#63157 = ORIENTED_EDGE ( 'NONE', *, *, #37997, .F. ) ;
#63156 = CARTESIAN_POINT ( 'NONE',  ( 21.00000000000000000, 9.749999999999998224, -21.25000000000000000 ) ) ;
#63158 = EDGE_CURVE ( 'NONE', #245138, #166165, #124530, .T. ) ;
#63159 = ORIENTED_EDGE ( 'NONE', *, *, #233134, .T. ) ;
#63160 = CARTESIAN_POINT ( 'NONE',  ( -16.81931177881022776, 9.936996059503902856, -20.77321787861722413 ) ) ;
#63161 = ORIENTED_EDGE ( 'NONE', *, *, #127709, .T. ) ;
#63162 = CARTESIAN_POINT ( 'NONE',  ( 21.05000000000000071, 60.91865828504416669, -234.1430899377568267 ) ) ;
#63163 = FACE_OUTER_BOUND ( 'NONE', #33477, .T. ) ;
#63164 = DIRECTION ( 'NONE',  ( 0.000000000000000000, 0.8814952561688430555, -0.4721928772777346239 ) ) ;
#63165 = ORIENTED_EDGE ( 'NONE', *, *, #90964, .F. ) ;
#63166 = EDGE_CURVE ( 'NONE', #2789, #228417, #47213, .T. ) ;
#63167 = EDGE_CURVE ( 'NONE', #170209, #230954, #197064, .T. ) ;
#63168 = FACE_OUTER_BOUND ( 'NONE', #11723, .T. ) ;
#63169 = CARTESIAN_POINT ( 'NONE',  ( -21.05000000000000071, 0.000000000000000000, -33.50000000000000000 ) ) ;
#63170 = ORIENTED_EDGE ( 'NONE', *, *, #57269, .T. ) ;
#63171 = CARTESIAN_POINT ( 'NONE',  ( -15.51798037960204191, 9.376659938544687378, -151.6281925482172710 ) ) ;
#63173 = ORIENTED_EDGE ( 'NONE', *, *, #97292, .T. ) ;
#63172 = CARTESIAN_POINT ( 'NONE',  ( -21.44999999999999929, 68.75000000001179501, -81.87310748452436826 ) ) ;
#63174 = TOROIDAL_SURFACE ( 'NONE', #129813, 0.2000000000000000111, 0.1000000000000000056 ) ;
#63175 = AXIS2_PLACEMENT_3D ( 'NONE', #107325, #167335, #106019 ) ;
#63176 = DIRECTION ( 'NONE',  ( 0.000000000000000000, 0.000000000000000000, 1.000000000000000000 ) ) ;
#63177 = FACE_OUTER_BOUND ( 'NONE', #202711, .T. ) ;
#63178 = AXIS2_PLACEMENT_3D ( 'NONE', #120570, #85235, #143951 ) ;
#63179 = ORIENTED_EDGE ( 'NONE', *, *, #179880, .F. ) ;
#63180 = CARTESIAN_POINT ( 'NONE',  ( 23.14999999999999858, 5.900000000011162093, -157.2809002353436654 ) ) ;
#63181 = CARTESIAN_POINT ( 'NONE',  ( -18.34374000495059676, 11.47316190336247388, -24.25000000000001066 ) ) ;
#63182 = CARTESIAN_POINT ( 'NONE',  ( -18.59999999999999787, 77.68707439010402993, -182.8376804510660065 ) ) ;
#63183 = ORIENTED_EDGE ( 'NONE', *, *, #162245, .T. ) ;
#63184 = CARTESIAN_POINT ( 'NONE',  ( 23.15000000000000213, 28.42524210734032408, -258.3567845160494585 ) ) ;
#63185 = ADVANCED_FACE ( 'NONE', ( #145356 ), #221989, .T. ) ;
#63186 = ADVANCED_FACE ( 'NONE', ( #243172 ), #26726, .T. ) ;
#63187 = CARTESIAN_POINT ( 'NONE',  ( -21.05000000000000071, 0.000000000000000000, 0.000000000000000000 ) ) ;
#63188 = ORIENTED_EDGE ( 'NONE', *, *, #198687, .T. ) ;
#63189 = EDGE_CURVE ( 'NONE', #48943, #98837, #42413, .T. ) ;
#63190 = EDGE_LOOP ( 'NONE', ( #211976, #190068, #76481, #91727 ) ) ;
#63191 = ORIENTED_EDGE ( 'NONE', *, *, #210771, .F. ) ;
#63192 = CARTESIAN_POINT ( 'NONE',  ( -18.79999999999999716, -1.885425182446133885, -11.49641995933507843 ) ) ;
#63193 = CARTESIAN_POINT ( 'NONE',  ( -16.87401514999228169, 66.05000000001255955, -182.7430894919923219 ) ) ;
#63194 = CIRCLE ( 'NONE', #58908, 0.09999999999999939493 ) ;
#63196 = ORIENTED_EDGE ( 'NONE', *, *, #12581, .F. ) ;
#63195 = CARTESIAN_POINT ( 'NONE',  ( -18.40000000000000213, 70.35000000001187459, -90.37310748452433984 ) ) ;
#63197 = DIRECTION ( 'NONE',  ( -0.000000000000000000, -0.8490545835447238510, -0.5283051335749973099 ) ) ;
#63198 = CARTESIAN_POINT ( 'NONE',  ( 20.95512820512820795, 10.62384868372303615, -112.7001620194244680 ) ) ;
#63199 = CARTESIAN_POINT ( 'NONE',  ( -20.94999999999999929, 87.65000000001172964, -72.42310748452422331 ) ) ;
#63200 = CARTESIAN_POINT ( 'NONE',  ( 23.04999999999999716, 8.822561741677553471, -42.75000000000000000 ) ) ;
#63201 = CARTESIAN_POINT ( 'NONE',  ( 21.05000000000000071, -8.999999999988842703, -91.00603087734759811 ) ) ;
#63202 = TOROIDAL_SURFACE ( 'NONE', #96518, 0.6000000000000004219, 0.1000000000000000056 ) ;
#63203 = EDGE_CURVE ( 'NONE', #86026, #22041, #69034, .T. ) ;
#63204 = CARTESIAN_POINT ( 'NONE',  ( 20.94999999999999574, 14.00000000000000178, -5.427092530382545021 ) ) ;
#63206 = ORIENTED_EDGE ( 'NONE', *, *, #206129, .F. ) ;
#63205 = DIRECTION ( 'NONE',  ( 0.000000000000000000, -0.1350103645451807555, -0.9908441862701610203 ) ) ;
#63208 = VERTEX_POINT ( 'NONE', #162380 ) ;
#63207 = DIRECTION ( 'NONE',  ( 0.7071067811865474617, -0.7071067811865474617, -4.937700262164531476E-15 ) ) ;
#63209 = DIRECTION ( 'NONE',  ( 0.000000000000000000, -0.9126074666063844765, -0.4088369013363114535 ) ) ;
#63210 = ORIENTED_EDGE ( 'NONE', *, *, #233881, .F. ) ;
#63211 = VECTOR ( 'NONE', #163210, 1000.000000000000000 ) ;
#63212 = ADVANCED_FACE ( 'NONE', ( #121956 ), #109593, .T. ) ;
#63213 = CARTESIAN_POINT ( 'NONE',  ( -21.05000000000000071, 74.14897176987101091, -91.36919421510182815 ) ) ;
#63214 = VECTOR ( 'NONE', #194329, 1000.000000000000000 ) ;
#63215 = DIRECTION ( 'NONE',  ( 0.000000000000000000, -0.2868887416115947775, 0.9579639084728169829 ) ) ;
#63216 = CIRCLE ( 'NONE', #208979, 0.09999999999999939493 ) ;
#63217 = DIRECTION ( 'NONE',  ( -0.000000000000000000, 7.272083257015735086E-15, -1.000000000000000000 ) ) ;
#63218 = ADVANCED_FACE ( 'NONE', ( #200211 ), #241889, .T. ) ;
#63219 = DIRECTION ( 'NONE',  ( -1.836970198721029934E-16, -0.4088369013363280513, 0.9126074666063769270 ) ) ;
#63220 = CARTESIAN_POINT ( 'NONE',  ( -18.59999999999999787, -1.835859311432481045, -145.5044391687985694 ) ) ;
#63221 = EDGE_CURVE ( 'NONE', #64056, #29923, #180647, .T. ) ;
#63222 = VECTOR ( 'NONE', #101511, 1000.000000000000000 ) ;
#63223 = ORIENTED_EDGE ( 'NONE', *, *, #43737, .T. ) ;
#63224 = CARTESIAN_POINT ( 'NONE',  ( 20.95263205890695701, 10.49856401425325281, -207.4020386360608086 ) ) ;
#63225 = AXIS2_PLACEMENT_3D ( 'NONE', #174106, #55351, #191080 ) ;
#63226 = EDGE_LOOP ( 'NONE', ( #55728, #39495, #150778, #44623 ) ) ;
#63227 = ORIENTED_EDGE ( 'NONE', *, *, #250264, .F. ) ;
#63228 = EDGE_CURVE ( 'NONE', #255132, #46490, #211771, .T. ) ;
#63229 = DIRECTION ( 'NONE',  ( 0.000000000000000000, -0.3738317757008748909, -0.9274965247785733613 ) ) ;
#63230 = CIRCLE ( 'NONE', #862, 0.09999999999999939493 ) ;
#63231 = B_SPLINE_CURVE_WITH_KNOTS ( 'NONE', 3,
 ( #221098, #42466, #85410, #122013, #5895, #45041, #146680, #241952, #124591, #185832, #201539, #22939, #24215, #107573, #82842, #145415 ),
 .UNSPECIFIED., .F., .F.,
 ( 4, 3, 3, 3, 3, 4 ),
 ( 0.000000000000000000, 2.209075297431620268E-05, 5.594258369009780208E-05, 8.979524372341998934E-05, 0.0001236472815274569225, 0.0001574990747609545522 ),
 .UNSPECIFIED. ) ;
#63232 = ORIENTED_EDGE ( 'NONE', *, *, #207451, .F. ) ;
#63233 = VECTOR ( 'NONE', #116820, 1000.000000000000000 ) ;
#63235 = EDGE_CURVE ( 'NONE', #43046, #86026, #87932, .T. ) ;
#63234 = CYLINDRICAL_SURFACE ( 'NONE', #193508, 0.5000000000000004441 ) ;
#63237 = EDGE_CURVE ( 'NONE', #169179, #155655, #47526, .T. ) ;
#63236 = EDGE_CURVE ( 'NONE', #123166, #255232, #255285, .T. ) ;
#63238 = AXIS2_PLACEMENT_3D ( 'NONE', #250102, #113153, #111885 ) ;
#63239 = LINE ( 'NONE', #142764, #134686 ) ;
#63240 = ORIENTED_EDGE ( 'NONE', *, *, #53240, .T. ) ;
#63241 = DIRECTION ( 'NONE',  ( 0.000000000000000000, -0.9634813093406718876, -0.2677755899091333047 ) ) ;
#63242 = VERTEX_POINT ( 'NONE', #149241 ) ;
#63243 = EDGE_CURVE ( 'NONE', #240326, #69452, #170114, .T. ) ;
#63245 = CIRCLE ( 'NONE', #209181, 2.000000000000001776 ) ;
#63244 = CARTESIAN_POINT ( 'NONE',  ( -14.11697426661281618, 9.457410944778565920, -48.50008397379003355 ) ) ;
#63246 = ORIENTED_EDGE ( 'NONE', *, *, #59806, .F. ) ;
#63247 = DIRECTION ( 'NONE',  ( 1.000000000000000000, 3.265361837132813093E-16, -0.000000000000000000 ) ) ;
#63248 = DIRECTION ( 'NONE',  ( 0.000000000000000000, 0.000000000000000000, 1.000000000000000000 ) ) ;
#63249 = VERTEX_POINT ( 'NONE', #48828 ) ;
#63250 = DIRECTION ( 'NONE',  ( 0.000000000000000000, 0.000000000000000000, -1.000000000000000000 ) ) ;
#63252 = ORIENTED_EDGE ( 'NONE', *, *, #21743, .F. ) ;
#63251 = DIRECTION ( 'NONE',  ( 0.000000000000000000, -5.204170427930272346E-14, -1.000000000000000000 ) ) ;
#63253 = AXIS2_PLACEMENT_3D ( 'NONE', #146568, #48768, #224830 ) ;
#63254 = EDGE_CURVE ( 'NONE', #224632, #155597, #151812, .T. ) ;
#63255 = CARTESIAN_POINT ( 'NONE',  ( 21.14999999999999858, 43.07541598710462694, -233.9110336739111347 ) ) ;
#63256 = EDGE_CURVE ( 'NONE', #102889, #181190, #129656, .T. ) ;
#63258 = VERTEX_POINT ( 'NONE', #247019 ) ;
#63257 = AXIS2_PLACEMENT_3D ( 'NONE', #251400, #136571, #98703 ) ;
#63259 = VECTOR ( 'NONE', #218387, 1000.000000000000000 ) ;
#63260 = CIRCLE ( 'NONE', #184081, 0.5000000000000013323 ) ;
#63261 = EDGE_CURVE ( 'NONE', #86414, #93478, #147379, .T. ) ;
#63262 = DIRECTION ( 'NONE',  ( 0.000000000000000000, -0.3738317757009345654, 0.9274965247785492695 ) ) ;
#63263 = ORIENTED_EDGE ( 'NONE', *, *, #109410, .F. ) ;
#63264 = DIRECTION ( 'NONE',  ( 1.000000000000000000, -7.304098846218133681E-16, -4.639676173203992654E-30 ) ) ;
#63265 = CARTESIAN_POINT ( 'NONE',  ( 22.39999999999999503, 75.90000000001199965, -110.8138870828976934 ) ) ;
#63267 = EDGE_CURVE ( 'NONE', #185216, #125547, #86641, .T. ) ;
#63266 = CARTESIAN_POINT ( 'NONE',  ( 18.49999999999999289, 6.650000000011155876, -88.15000000000004832 ) ) ;
#63268 = CARTESIAN_POINT ( 'NONE',  ( 18.59999999999999076, 69.55000000001207638, -126.5060803140843291 ) ) ;
#63269 = CARTESIAN_POINT ( 'NONE',  ( -14.87779219673431008, 66.56936653093978862, -188.2913416897003174 ) ) ;
#63270 = EDGE_CURVE ( 'NONE', #85751, #176002, #150514, .T. ) ;
#63271 = CARTESIAN_POINT ( 'NONE',  ( -20.64999999999999858, 7.150000000011155876, -179.8499999999999943 ) ) ;
#63272 = VERTEX_POINT ( 'NONE', #132224 ) ;
#63273 = DIRECTION ( 'NONE',  ( -0.7071067811865475727, 0.2890913453342130457, -0.6453109281988448354 ) ) ;
#63274 = CARTESIAN_POINT ( 'NONE',  ( -20.94999999999994245, 67.85000000001119247, -3.023107484524792277 ) ) ;
#63275 = FACE_OUTER_BOUND ( 'NONE', #230283, .T. ) ;
#63276 = CYLINDRICAL_SURFACE ( 'NONE', #38675, 0.1000000000000000472 ) ;
#63277 = ORIENTED_EDGE ( 'NONE', *, *, #24791, .F. ) ;
#63279 = DIRECTION ( 'NONE',  ( 1.000000000000000000, 0.000000000000000000, 0.000000000000000000 ) ) ;
#63278 = CIRCLE ( 'NONE', #21607, 4.150000000000001243 ) ;
#63280 = VERTEX_POINT ( 'NONE', #227458 ) ;
#63281 = CARTESIAN_POINT ( 'NONE',  ( 13.54556439290363379, 9.450592112144860835, -115.5561883188084664 ) ) ;
#63282 = ORIENTED_EDGE ( 'NONE', *, *, #176034, .T. ) ;
#63283 = DIRECTION ( 'NONE',  ( 0.000000000000000000, -0.7397360091702744889, 0.6728971962616842051 ) ) ;
#63284 = CARTESIAN_POINT ( 'NONE',  ( 20.94999999999999574, 1.835341550224411922, -11.55515129256298046 ) ) ;
#63285 = ORIENTED_EDGE ( 'NONE', *, *, #8141, .T. ) ;
#63287 = VERTEX_POINT ( 'NONE', #110085 ) ;
#63286 = CARTESIAN_POINT ( 'NONE',  ( -23.25000000000000355, 70.35000000001159037, -56.87310748452436115 ) ) ;
#63288 = EDGE_CURVE ( 'NONE', #101606, #256898, #39075, .T. ) ;
#63289 = LINE ( 'NONE', #124569, #254635 ) ;
#63290 = ORIENTED_EDGE ( 'NONE', *, *, #108623, .T. ) ;
#63291 = DIRECTION ( 'NONE',  ( 0.000000000000000000, -0.4721928772777346239, -0.8814952561688430555 ) ) ;
#63292 = LINE ( 'NONE', #124574, #98044 ) ;
#63293 = ORIENTED_EDGE ( 'NONE', *, *, #134350, .T. ) ;
#63295 = ORIENTED_EDGE ( 'NONE', *, *, #2228, .F. ) ;
#63294 = EDGE_CURVE ( 'NONE', #6026, #74560, #88910, .T. ) ;
#63296 = CARTESIAN_POINT ( 'NONE',  ( -21.06715728752538652, 11.75000000001115197, -174.5148057706539646 ) ) ;
#63297 = CARTESIAN_POINT ( 'NONE',  ( -16.92570016628984320, 14.17383480627949410, -219.2818793572221523 ) ) ;
#63298 = DIRECTION ( 'NONE',  ( 0.7071067811865473507, 0.3338907855510733769, 0.6233112732207618523 ) ) ;
#63299 = ORIENTED_EDGE ( 'NONE', *, *, #41213, .F. ) ;
#63300 = EDGE_LOOP ( 'NONE', ( #234871, #80354, #144881, #111521, #65987, #106389 ) ) ;
#63301 = AXIS2_PLACEMENT_3D ( 'NONE', #124354, #203875, #25265 ) ;
#63302 = CARTESIAN_POINT ( 'NONE',  ( 23.14999999999999147, 80.15000000001194280, -103.0231074845242887 ) ) ;
#63303 = EDGE_CURVE ( 'NONE', #52663, #238500, #29313, .T. ) ;
#63305 = EDGE_LOOP ( 'NONE', ( #221275, #144874, #176299, #155264 ) ) ;
#63304 = DIRECTION ( 'NONE',  ( 0.000000000000000000, -0.000000000000000000, 1.000000000000000000 ) ) ;
#63306 = DIRECTION ( 'NONE',  ( -1.000000000000000000, 0.000000000000000000, 0.000000000000000000 ) ) ;
#63307 = CARTESIAN_POINT ( 'NONE',  ( -18.50000000000000000, 44.10700160683882132, -235.9691471569721841 ) ) ;
#63308 = CARTESIAN_POINT ( 'NONE',  ( -18.59999999999999787, 11.64999999999999680, -21.25000000000000000 ) ) ;
#63310 = CYLINDRICAL_SURFACE ( 'NONE', #165898, 11.74999999999999645 ) ;
#63309 = CARTESIAN_POINT ( 'NONE',  ( -17.80356949363974195, 65.12326860300986198, -126.2361805087511328 ) ) ;
#63311 = CARTESIAN_POINT ( 'NONE',  ( 21.05000000000072191, 39.26334644455242540, -236.8761453142877542 ) ) ;
#63312 = DIRECTION ( 'NONE',  ( 0.000000000000000000, -0.8660254037844412611, -0.4999999999999956701 ) ) ;
#63313 = CIRCLE ( 'NONE', #104806, 4.049999999999998934 ) ;
#63314 = CARTESIAN_POINT ( 'NONE',  ( -16.89268316805466341, 60.93619025550653134, -221.0468289635910537 ) ) ;
#63315 = EDGE_CURVE ( 'NONE', #81651, #40310, #126535, .T. ) ;
#63316 = FACE_OUTER_BOUND ( 'NONE', #67630, .T. ) ;
#63317 = AXIS2_PLACEMENT_3D ( 'NONE', #163569, #85277, #3182 ) ;
#63318 = ORIENTED_EDGE ( 'NONE', *, *, #120941, .T. ) ;
#63319 = ORIENTED_EDGE ( 'NONE', *, *, #216551, .T. ) ;
#63320 = DIRECTION ( 'NONE',  ( 0.000000000000000000, 0.000000000000000000, -1.000000000000000000 ) ) ;
#63321 = ORIENTED_EDGE ( 'NONE', *, *, #44905, .F. ) ;
#63322 = CARTESIAN_POINT ( 'NONE',  ( -16.87487986503753845, 9.950007555096753720, -146.6499747396867406 ) ) ;
#63323 = VERTEX_POINT ( 'NONE', #228770 ) ;
#63324 = AXIS2_PLACEMENT_3D ( 'NONE', #55587, #133876, #32238 ) ;
#63325 =( NAMED_UNIT ( * ) SI_UNIT ( $, .STERADIAN. ) SOLID_ANGLE_UNIT ( ) );
#63326 = CARTESIAN_POINT ( 'NONE',  ( 20.93975676684922504, 65.68895814178263493, -131.0026557862138645 ) ) ;
#63328 = ORIENTED_EDGE ( 'NONE', *, *, #162397, .F. ) ;
#63327 = VERTEX_POINT ( 'NONE', #146626 ) ;
#63329 = FACE_BOUND ( 'NONE', #95412, .T. ) ;
#63330 = ORIENTED_EDGE ( 'NONE', *, *, #59752, .T. ) ;
#63331 = ORIENTED_EDGE ( 'NONE', *, *, #69986, .F. ) ;
#63332 = DIRECTION ( 'NONE',  ( 0.000000000000000000, 0.000000000000000000, 1.000000000000000000 ) ) ;
#63333 = FACE_OUTER_BOUND ( 'NONE', #216307, .T. ) ;
#63335 = EDGE_LOOP ( 'NONE', ( #54737, #78935, #119106, #20390 ) ) ;
#63334 = CARTESIAN_POINT ( 'NONE',  ( 23.24999999999999645, 67.23127455305835554, -235.8551265064784559 ) ) ;
#63336 = CARTESIAN_POINT ( 'NONE',  ( 19.99999999738043144, 11.75000000001116263, -158.6871719496316473 ) ) ;
#63338 = ORIENTED_EDGE ( 'NONE', *, *, #124177, .F. ) ;
#63337 = CARTESIAN_POINT ( 'NONE',  ( -23.25000000000000000, 64.25000000001215028, -136.5231074845243597 ) ) ;
#63339 = CARTESIAN_POINT ( 'NONE',  ( -22.47071067811865319, 0.09909245471376171288, -59.27992525550198621 ) ) ;
#63340 = VERTEX_POINT ( 'NONE', #51362 ) ;
#63341 = CARTESIAN_POINT ( 'NONE',  ( -18.79999999999999716, 1.212568896937007645, -7.800000000000000711 ) ) ;
#63343 = EDGE_LOOP ( 'NONE', ( #205507, #209423, #128078, #100046 ) ) ;
#63342 = CARTESIAN_POINT ( 'NONE',  ( 18.60000000000000142, 85.40000000001154490, -62.22584772486096227 ) ) ;
#63344 = CARTESIAN_POINT ( 'NONE',  ( -20.94999999999999929, 5.204170427930421283E-15, -2.899999999999982592 ) ) ;
#63345 = CARTESIAN_POINT ( 'NONE',  ( -18.58222699835055280, 10.33200063080771969, -72.59316749566430360 ) ) ;
#63346 = VECTOR ( 'NONE', #205944, 1000.000000000000114 ) ;
#63348 = EDGE_CURVE ( 'NONE', #31642, #221637, #226145, .T. ) ;
#63347 = CIRCLE ( 'NONE', #209116, 0.4000000000000114575 ) ;
#63349 = DIRECTION ( 'NONE',  ( 0.000000000000000000, -6.982962677686266711E-15, 1.000000000000000000 ) ) ;
#63350 = TOROIDAL_SURFACE ( 'NONE', #150850, 4.149999999999999467, 0.1000000000000000056 ) ;
#63351 = ORIENTED_EDGE ( 'NONE', *, *, #44572, .F. ) ;
#63353 = CARTESIAN_POINT ( 'NONE',  ( 20.53930447208004040, 8.977148687536415039, -108.9425071415766553 ) ) ;
#63352 = DIRECTION ( 'NONE',  ( 0.000000000000000000, 0.000000000000000000, 1.000000000000000000 ) ) ;
#63354 = DIRECTION ( 'NONE',  ( -4.336808689941752679E-15, 0.8660254037844482555, 0.4999999999999837907 ) ) ;
#63355 = CARTESIAN_POINT ( 'NONE',  ( 21.00000000000000000, 9.750000000011153745, -45.75000000000000711 ) ) ;
#63356 = CARTESIAN_POINT ( 'NONE',  ( 21.14999999999999858, 6.540656951712400691, -134.0000000000000000 ) ) ;
#63357 = FACE_OUTER_BOUND ( 'NONE', #257888, .T. ) ;
#63358 = ORIENTED_EDGE ( 'NONE', *, *, #123819, .F. ) ;
#63359 = ORIENTED_EDGE ( 'NONE', *, *, #101839, .T. ) ;
#63360 = ORIENTED_EDGE ( 'NONE', *, *, #17088, .T. ) ;
#63361 = CARTESIAN_POINT ( 'NONE',  ( -20.54999999999999716, 85.00000000001251976, -179.9170766071767389 ) ) ;
#63362 = ORIENTED_EDGE ( 'NONE', *, *, #227193, .F. ) ;
#63363 = CYLINDRICAL_SURFACE ( 'NONE', #1756, 0.1000000000000028644 ) ;
#63364 = VERTEX_POINT ( 'NONE', #28018 ) ;
#63365 = EDGE_CURVE ( 'NONE', #103469, #172629, #163949, .T. ) ;
#63366 = DIRECTION ( 'NONE',  ( -1.000000000000000000, 0.000000000000000000, -0.000000000000000000 ) ) ;
#63367 = CARTESIAN_POINT ( 'NONE',  ( -17.78241384939014580, 15.55476280961775792, -221.4083347684370153 ) ) ;
#63368 = EDGE_CURVE ( 'NONE', #15628, #207337, #14130, .T. ) ;
#63369 = ORIENTED_EDGE ( 'NONE', *, *, #152737, .F. ) ;
#63370 = CARTESIAN_POINT ( 'NONE',  ( 21.14999999999999858, 8.786607556611267356, -179.8499999999999943 ) ) ;
#63371 =( LENGTH_UNIT ( ) NAMED_UNIT ( * ) SI_UNIT ( .MILLI., .METRE. ) );
#63372 = EDGE_CURVE ( 'NONE', #163468, #192701, #188897, .T. ) ;
#63373 = AXIS2_PLACEMENT_3D ( 'NONE', #198362, #216638, #180101 ) ;
#63374 = VERTEX_POINT ( 'NONE', #254690 ) ;
#63375 = ORIENTED_EDGE ( 'NONE', *, *, #208230, .F. ) ;
#63376 = ORIENTED_EDGE ( 'NONE', *, *, #37713, .F. ) ;
#63377 = ADVANCED_FACE ( 'NONE', ( #17412 ), #118153, .T. ) ;
#63378 = CARTESIAN_POINT ( 'NONE',  ( -23.25000000000000000, 23.38726701055792745, -229.1122755113798632 ) ) ;
#63379 = LINE ( 'NONE', #47661, #99232 ) ;
#63380 = CARTESIAN_POINT ( 'NONE',  ( 18.59999999999999076, 11.04098673250373785, -220.4458636211660689 ) ) ;
#63382 = EDGE_CURVE ( 'NONE', #62705, #213961, #234689, .T. ) ;
#63381 = CARTESIAN_POINT ( 'NONE',  ( -18.35663730107557257, 20.70056182099758857, -227.9862904610682222 ) ) ;
#63383 = DIRECTION ( 'NONE',  ( -1.000000000000000000, -0.000000000000000000, -0.000000000000000000 ) ) ;
#63384 = FACE_OUTER_BOUND ( 'NONE', #12416, .T. ) ;
#63385 = AXIS2_PLACEMENT_3D ( 'NONE', #78370, #96626, #176220 ) ;
#63387 = DIRECTION ( 'NONE',  ( 0.000000000000000000, 0.9968797965484670343, 0.07893460099023179299 ) ) ;
#63386 = PLANE ( 'NONE',  #58237 ) ;
#63388 = DIRECTION ( 'NONE',  ( 1.000000000000000000, 0.000000000000000000, 0.000000000000000000 ) ) ;
#63390 = ORIENTED_EDGE ( 'NONE', *, *, #213642, .T. ) ;
#63389 = CARTESIAN_POINT ( 'NONE',  ( 18.59999999999999076, 2.272311100394801109, -217.9150152700588592 ) ) ;
#63391 = DIRECTION ( 'NONE',  ( -1.000000000000000000, -0.000000000000000000, 0.000000000000000000 ) ) ;
#63392 = ADVANCED_FACE ( 'NONE', ( #213038 ), #22506, .F. ) ;
#63393 = DIRECTION ( 'NONE',  ( 0.000000000000000000, -1.000000000000000000, 0.000000000000000000 ) ) ;
#63394 = ORIENTED_EDGE ( 'NONE', *, *, #166153, .T. ) ;
#63395 = DIRECTION ( 'NONE',  ( 1.000000000000000000, -0.000000000000000000, -0.000000000000000000 ) ) ;
#63396 = AXIS2_PLACEMENT_3D ( 'NONE', #11483, #195267, #16620 ) ;
#63397 = CARTESIAN_POINT ( 'NONE',  ( 18.49999999999999289, 64.25000000001263345, -195.4231074845244223 ) ) ;
#63398 = CARTESIAN_POINT ( 'NONE',  ( 18.54999999999999716, 67.25000000001205080, -127.2731074845243597 ) ) ;
#63399 = ORIENTED_EDGE ( 'NONE', *, *, #78594, .F. ) ;
#63401 = ADVANCED_FACE ( 'NONE', ( #34442 ), #76095, .F. ) ;
#63400 = AXIS2_PLACEMENT_3D ( 'NONE', #245109, #62628, #221670 ) ;
#63402 = VECTOR ( 'NONE', #114939, 1000.000000000000000 ) ;
#63403 = VECTOR ( 'NONE', #23902, 1000.000000000000227 ) ;
#63404 = CARTESIAN_POINT ( 'NONE',  ( -21.05000000000000071, 76.00000000001165290, -69.52310748452431710 ) ) ;
#63405 = FACE_BOUND ( 'NONE', #98570, .T. ) ;
#63406 = AXIS2_PLACEMENT_3D ( 'NONE', #144577, #244975, #145864 ) ;
#63407 = ORIENTED_EDGE ( 'NONE', *, *, #68793, .T. ) ;
#63408 = VERTEX_POINT ( 'NONE', #56510 ) ;
#63409 = CARTESIAN_POINT ( 'NONE',  ( -16.90202395485773224, 9.965944544550314532, -12.59698627874055354 ) ) ;
#63410 = ORIENTED_EDGE ( 'NONE', *, *, #65028, .T. ) ;
#63411 = DIRECTION ( 'NONE',  ( 1.000000000000000000, 0.000000000000000000, 0.000000000000000000 ) ) ;
#63412 = DIRECTION ( 'NONE',  ( -0.000000000000000000, -6.982962677686266711E-15, 1.000000000000000000 ) ) ;
#63413 = LINE ( 'NONE', #205493, #67684 ) ;
#63414 = VERTEX_POINT ( 'NONE', #175249 ) ;
#63415 = VECTOR ( 'NONE', #23019, 1000.000000000000000 ) ;
#63416 = ADVANCED_FACE ( 'NONE', ( #16157 ), #13572, .T. ) ;
#63418 = VECTOR ( 'NONE', #147465, 1000.000000000000000 ) ;
#63417 = CARTESIAN_POINT ( 'NONE',  ( -21.05000000000000071, 1.115600667400684642E-11, -33.50000000000000000 ) ) ;
#63419 = CARTESIAN_POINT ( 'NONE',  ( 23.24999999999999645, 64.25000000001230660, -157.3731074845244393 ) ) ;
#63421 = LINE ( 'NONE', #243349, #45212 ) ;
#63420 = TOROIDAL_SURFACE ( 'NONE', #230020, 0.4000000000000003553, 0.1000000000000000056 ) ;
#63422 = AXIS2_PLACEMENT_3D ( 'NONE', #173424, #170858, #35183 ) ;
#63423 = CARTESIAN_POINT ( 'NONE',  ( 21.05000000000000071, 76.00000000001142553, -36.02310748452432421 ) ) ;
#63424 = AXIS2_PLACEMENT_3D ( 'NONE', #196809, #255461, #76865 ) ;
#63425 = ORIENTED_EDGE ( 'NONE', *, *, #96709, .F. ) ;
#63426 = VECTOR ( 'NONE', #228948, 1000.000000000000000 ) ;
#63427 = EDGE_CURVE ( 'NONE', #141175, #181190, #215599, .T. ) ;
#63429 = VERTEX_POINT ( 'NONE', #172686 ) ;
#63428 = LINE ( 'NONE', #201662, #25282 ) ;
#63430 = CARTESIAN_POINT ( 'NONE',  ( -21.65000000000000213, 66.05000000001261640, -190.8731074845244393 ) ) ;
#63431 = FACE_OUTER_BOUND ( 'NONE', #229371, .T. ) ;
#63432 = VECTOR ( 'NONE', #153522, 1000.000000000000114 ) ;
#63433 = DIRECTION ( 'NONE',  ( 0.000000000000000000, 0.000000000000000000, 1.000000000000000000 ) ) ;
#63434 = CARTESIAN_POINT ( 'NONE',  ( 22.57320508075688537, 11.38316329224760359, -198.5208684056144079 ) ) ;
#63435 = FACE_OUTER_BOUND ( 'NONE', #128343, .T. ) ;
#63436 = DIRECTION ( 'NONE',  ( 0.000000000000000000, 1.000000000000000000, -0.000000000000000000 ) ) ;
#63437 = ORIENTED_EDGE ( 'NONE', *, *, #28411, .T. ) ;
#63438 = DIRECTION ( 'NONE',  ( -0.000000000000000000, 0.2128009952263603677, -0.9770955615653313941 ) ) ;
#63439 = CARTESIAN_POINT ( 'NONE',  ( -20.65000000000000568, 68.75000000001233502, -160.7731074845244166 ) ) ;
#63440 = CARTESIAN_POINT ( 'NONE',  ( 15.39170923737819230, 9.389529397477891948, -51.31710791289368245 ) ) ;
#63441 = CARTESIAN_POINT ( 'NONE',  ( 21.93340585971691326, 7.324147022868161550, -134.0000000000000000 ) ) ;
#63442 = DIRECTION ( 'NONE',  ( 1.000000000000000000, 0.000000000000000000, 0.000000000000000000 ) ) ;
#63443 = CARTESIAN_POINT ( 'NONE',  ( -18.40000000000000213, 11.47316190337364183, -191.6740539331919990 ) ) ;
#63444 =( BOUNDED_SURFACE ( )  B_SPLINE_SURFACE ( 3, 2, ( 
 ( #244304, #102201, #104770 ),
 ( #159655, #24010, #240466 ),
 ( #125650, #140058, #220888 ),
 ( #21446, #145203, #3117 ),
 ( #219604, #143924, #106062 ),
 ( #205170, #184330, #5677 ) ),
 .UNSPECIFIED., .F., .F., .T. ) 
 B_SPLINE_SURFACE_WITH_KNOTS ( ( 4, 2, 4 ),
 ( 3, 3 ),
 ( 0.0001792624049599543154, 0.0003686986002124625081, 0.0005581347954649706466 ),
 ( 0.000000000000000000, 1.000000000000000000 ),
 .UNSPECIFIED. ) 
 GEOMETRIC_REPRESENTATION_ITEM ( )  RATIONAL_B_SPLINE_SURFACE ( (
 ( 1.000000000000000000, 0.9238795325112830747, 1.000000000000000000),
 ( 1.000000000000000000, 0.9229318695234240977, 1.000000000000000000),
 ( 1.000000000000000000, 0.8926288119236353014, 1.000000000000000000),
 ( 1.000000000000000000, 0.8123777807265625261, 1.000000000000000000),
 ( 1.000000000000000000, 0.7629087100935785237, 1.000000000000000000),
 ( 1.000000000000000000, 0.7071067811865475727, 1.000000000000000000) ) ) 
 REPRESENTATION_ITEM ( '' )  SURFACE ( )  );
#63445 = VECTOR ( 'NONE', #212974, 999.9999999999998863 ) ;
#63446 = ADVANCED_FACE ( 'NONE', ( #95654 ), #98190, .F. ) ;
#63447 = TOROIDAL_SURFACE ( 'NONE', #92678, 11.65000000000000036, 0.1000000000000000056 ) ;
#63448 = ORIENTED_EDGE ( 'NONE', *, *, #178765, .T. ) ;
#63449 = ORIENTED_EDGE ( 'NONE', *, *, #213971, .F. ) ;
#63450 = CYLINDRICAL_SURFACE ( 'NONE', #29367, 0.09999999999999939493 ) ;
#63451 = CARTESIAN_POINT ( 'NONE',  ( 21.05000000000000071, 5.900000000000005684, -23.28090023534362629 ) ) ;
#63452 = FACE_OUTER_BOUND ( 'NONE', #15242, .T. ) ;
#63453 = LINE ( 'NONE', #160023, #199624 ) ;
#63454 = EDGE_CURVE ( 'NONE', #195444, #192399, #193184, .T. ) ;
#63455 = ORIENTED_EDGE ( 'NONE', *, *, #84316, .T. ) ;
#63456 = DIRECTION ( 'NONE',  ( 0.000000000000000000, 0.5868805631290353597, 0.8096735173027127530 ) ) ;
#63457 = CARTESIAN_POINT ( 'NONE',  ( 18.59999999999999432, 74.83729825007431202, -161.9231074845243654 ) ) ;
#63458 = ADVANCED_FACE ( 'NONE', ( #214331 ), #116522, .T. ) ;
#63460 = EDGE_CURVE ( 'NONE', #80050, #82729, #243043, .T. ) ;
#63459 = CARTESIAN_POINT ( 'NONE',  ( 18.59999999999999076, 53.24180694658302571, -234.8354225850497130 ) ) ;
#63461 = DIRECTION ( 'NONE',  ( 0.000000000000000000, 1.734723475976807292E-15, -1.000000000000000000 ) ) ;
#63462 = AXIS2_PLACEMENT_3D ( 'NONE', #126572, #27515, #108296 ) ;
#63463 = ORIENTED_EDGE ( 'NONE', *, *, #67912, .F. ) ;
#63464 = CARTESIAN_POINT ( 'NONE',  ( 20.27550659511088682, 66.78395627750377628, -194.2731074845244166 ) ) ;
#63465 = EDGE_CURVE ( 'NONE', #89290, #41111, #68275, .T. ) ;
#63466 = ORIENTED_EDGE ( 'NONE', *, *, #59418, .T. ) ;
#63467 = CARTESIAN_POINT ( 'NONE',  ( 18.59999999999999076, 6.650000000011155876, -121.7500000000000426 ) ) ;
#63468 = DIRECTION ( 'NONE',  ( 0.000000000000000000, 0.000000000000000000, -1.000000000000000000 ) ) ;
#63469 = CARTESIAN_POINT ( 'NONE',  ( -21.05000000000000071, 10.05599437547273389, -228.2004445046334240 ) ) ;
#63470 = DIRECTION ( 'NONE',  ( 0.000000000000000000, -1.565658005757035267E-14, 1.000000000000000000 ) ) ;
#63471 = DIRECTION ( 'NONE',  ( -0.000000000000000000, -0.000000000000000000, 1.000000000000000000 ) ) ;
#63472 = CARTESIAN_POINT ( 'NONE',  ( -21.52071067811865746, 7.779289321881349473, -21.25000000000000000 ) ) ;
#63473 = CARTESIAN_POINT ( 'NONE',  ( -20.94999999999999929, -11.39257802169451672, -103.5739495798319751 ) ) ;
#63474 = CARTESIAN_POINT ( 'NONE',  ( -18.59999999999999787, 77.86671491006937629, -124.7704322382422788 ) ) ;
#63475 = CARTESIAN_POINT ( 'NONE',  ( 21.07016717457010202, 1.116511100764040927E-11, -94.17905916189916127 ) ) ;
#63476 = CYLINDRICAL_SURFACE ( 'NONE', #63077, 0.09999999999999939493 ) ;
#63477 = DIRECTION ( 'NONE',  ( -1.000000000000000000, 0.000000000000000000, 0.000000000000000000 ) ) ;
#63478 = CARTESIAN_POINT ( 'NONE',  ( -21.44999999999999929, 7.249999999999999112, -12.34999999999999964 ) ) ;
#63479 = DIRECTION ( 'NONE',  ( 0.000000000000000000, 0.000000000000000000, 1.000000000000000000 ) ) ;
#63480 = DIRECTION ( 'NONE',  ( -0.000000000000000000, -6.982962677686266711E-15, 1.000000000000000000 ) ) ;
#63481 = CIRCLE ( 'NONE', #184294, 0.09999999999999939493 ) ;
#63482 = ORIENTED_EDGE ( 'NONE', *, *, #46765, .F. ) ;
#63483 = DIRECTION ( 'NONE',  ( 0.000000000000000000, -1.000000000000000000, -0.000000000000000000 ) ) ;
#63484 = FACE_OUTER_BOUND ( 'NONE', #39342, .T. ) ;
#63485 = EDGE_CURVE ( 'NONE', #121769, #21107, #154397, .T. ) ;
#63486 = EDGE_CURVE ( 'NONE', #136972, #14256, #255481, .T. ) ;
#63487 = SHAPE_REPRESENTATION ( 'Snap Open Cable Crossbars 5', ( #2425 ), #227291 ) ;
#63488 = VERTEX_POINT ( 'NONE', #138607 ) ;
#63489 = DIRECTION ( 'NONE',  ( 0.000000000000000000, 0.000000000000000000, -1.000000000000000000 ) ) ;
#63490 = CARTESIAN_POINT ( 'NONE',  ( 21.12802099929860944, 67.21944740979007804, -157.7749174995927888 ) ) ;
#63491 = B_SPLINE_CURVE_WITH_KNOTS ( 'NONE', 3,
 ( #39130, #159082, #118667, #82045, #196888, #221567, #198175, #18261, #1241, #61237 ),
 .UNSPECIFIED., .F., .F.,
 ( 4, 3, 3, 4 ),
 ( 0.000000000000000000, 4.874959354401679605E-05, 9.785140065121436244E-05, 0.0001360444631935818385 ),
 .UNSPECIFIED. ) ;
#63492 = DIRECTION ( 'NONE',  ( 1.000000000000000000, 0.000000000000000000, 0.000000000000000000 ) ) ;
#63493 = VERTEX_POINT ( 'NONE', #93086 ) ;
#63494 = DIRECTION ( 'NONE',  ( 0.000000000000000000, 1.000000000000000000, 0.000000000000000000 ) ) ;
#63495 = CYLINDRICAL_SURFACE ( 'NONE', #159929, 0.1000000000000122874 ) ;
#63496 = EDGE_CURVE ( 'NONE', #96104, #153822, #218094, .T. ) ;
#63497 = AXIS2_PLACEMENT_3D ( 'NONE', #144247, #146821, #189824 ) ;
#63498 = ORIENTED_EDGE ( 'NONE', *, *, #63548, .T. ) ;
#63499 = AXIS2_PLACEMENT_3D ( 'NONE', #161693, #145943, #182538 ) ;
#63500 = EDGE_LOOP ( 'NONE', ( #137331, #61162, #36732, #192034 ) ) ;
#63501 = DIRECTION ( 'NONE',  ( 0.000000000000000000, 0.000000000000000000, -1.000000000000000000 ) ) ;
#63502 = CIRCLE ( 'NONE', #163480, 7.791421356237338003 ) ;
#63503 = ORIENTED_EDGE ( 'NONE', *, *, #135606, .T. ) ;
#63504 = LINE ( 'NONE', #157867, #66909 ) ;
#63505 = FACE_OUTER_BOUND ( 'NONE', #126185, .T. ) ;
#63506 = DIRECTION ( 'NONE',  ( 0.000000000000000000, 0.8814952561688430555, -0.4721928772777346239 ) ) ;
#63508 = DIRECTION ( 'NONE',  ( 0.000000000000000000, -1.000000000000000000, 0.000000000000000000 ) ) ;
#63507 = PRODUCT_DEFINITION_CONTEXT ( 'detailed design', #65706, 'design' ) ;
#63509 = CARTESIAN_POINT ( 'NONE',  ( -23.25000000000000000, 76.00000000001170974, -69.52310748452431710 ) ) ;
#63510 = FACE_OUTER_BOUND ( 'NONE', #20732, .T. ) ;
#63511 = CARTESIAN_POINT ( 'NONE',  ( 23.24999999999999645, -3.899999999999999467, -33.50000000000000000 ) ) ;
#63512 = AXIS2_PLACEMENT_3D ( 'NONE', #129723, #71058, #150580 ) ;
#63513 = LINE ( 'NONE', #103908, #246971 ) ;
#63515 = FACE_OUTER_BOUND ( 'NONE', #175852, .T. ) ;
#63514 = CIRCLE ( 'NONE', #167602, 0.2000000000000057288 ) ;
#63517 = ORIENTED_EDGE ( 'NONE', *, *, #143026, .F. ) ;
#63516 = CARTESIAN_POINT ( 'NONE',  ( 18.40000000000000213, 86.98067499225015808, -199.3289525933215032 ) ) ;
#63518 = ORIENTED_EDGE ( 'NONE', *, *, #80296, .T. ) ;
#63520 = SPHERICAL_SURFACE ( 'NONE', #210440, 0.1000000000000000056 ) ;
#63519 = DIRECTION ( 'NONE',  ( 1.000000000000000000, 0.000000000000000000, 0.000000000000000000 ) ) ;
#63522 = EDGE_LOOP ( 'NONE', ( #58267, #89096, #111862, #147486 ) ) ;
#63521 = CARTESIAN_POINT ( 'NONE',  ( -16.88783316861822925, 60.96612568567729085, -220.9430291400472868 ) ) ;
#63523 = EDGE_CURVE ( 'NONE', #103673, #167893, #222173, .T. ) ;
#63524 = EDGE_LOOP ( 'NONE', ( #24184, #227782, #35652, #20011, #25029 ) ) ;
#63525 = CARTESIAN_POINT ( 'NONE',  ( -20.05000000000000426, 9.250000000000001776, -21.25000000000000000 ) ) ;
#63526 = DIRECTION ( 'NONE',  ( -0.000000000000000000, 0.2617529984165031243, 0.9651348961777157509 ) ) ;
#63527 = LINE ( 'NONE', #83061, #100626 ) ;
#63528 = TOROIDAL_SURFACE ( 'NONE', #180083, 3.899999999999999467, 0.1000000000000000056 ) ;
#63529 = DIRECTION ( 'NONE',  ( 1.000000000000000000, -0.000000000000000000, -0.000000000000000000 ) ) ;
#63530 = ADVANCED_FACE ( 'NONE', ( #85052 ), #157629, .F. ) ;
#63531 = LINE ( 'NONE', #43980, #224811 ) ;
#63532 = DIRECTION ( 'NONE',  ( 0.000000000000000000, -0.9968797965484669232, -0.07893460099023200116 ) ) ;
#63533 = B_SPLINE_CURVE_WITH_KNOTS ( 'NONE', 3,
 ( #44074, #123612, #203140, #85719, #183585, #165299, #4910, #89598, #71354, #206997, #249974, #68772, #150867, #208293, #107888, #8797 ),
 .UNSPECIFIED., .F., .F.,
 ( 4, 3, 3, 3, 3, 4 ),
 ( 0.000000000000000000, 2.209833635978075103E-05, 5.595056164119271205E-05, 8.979992002655367851E-05, 0.0001236482757198911655, 0.0001574984039362983660 ),
 .UNSPECIFIED. ) ;
#63534 = CIRCLE ( 'NONE', #76025, 0.5999999999999894307 ) ;
#63535 = EDGE_CURVE ( 'NONE', #203841, #119361, #168273, .T. ) ;
#63536 = AXIS2_PLACEMENT_3D ( 'NONE', #148225, #32160, #92099 ) ;
#63537 = CIRCLE ( 'NONE', #188441, 11.75000000000000000 ) ;
#63538 = DIRECTION ( 'NONE',  ( 0.7071359030027593029, 0.7070776581709197206, 0.000000000000000000 ) ) ;
#63539 = ORIENTED_EDGE ( 'NONE', *, *, #37597, .F. ) ;
#63540 = ORIENTED_EDGE ( 'NONE', *, *, #241944, .T. ) ;
#63541 = EDGE_CURVE ( 'NONE', #109914, #47140, #251434, .T. ) ;
#63542 = DIRECTION ( 'NONE',  ( -1.000000000000000000, 2.849773892568378313E-16, -7.728835255496647986E-17 ) ) ;
#63543 = ORIENTED_EDGE ( 'NONE', *, *, #233639, .F. ) ;
#63544 = CARTESIAN_POINT ( 'NONE',  ( 21.05000000000000071, -0.02138556592644368787, -27.19503888731533792 ) ) ;
#63545 = VERTEX_POINT ( 'NONE', #399 ) ;
#63546 = CARTESIAN_POINT ( 'NONE',  ( 21.05000000000000071, 18.47808476326694915, -239.8121846073901224 ) ) ;
#63547 = EDGE_CURVE ( 'NONE', #125678, #43729, #30697, .T. ) ;
#63548 = EDGE_CURVE ( 'NONE', #248822, #45881, #176445, .T. ) ;
#63549 = CARTESIAN_POINT ( 'NONE',  ( 21.14999999999999503, -11.74999999998883560, -36.39999999999999858 ) ) ;
#63550 = CARTESIAN_POINT ( 'NONE',  ( 5.900000000000061640, 64.65000000001120384, -22.12310748452479103 ) ) ;
#63551 = CARTESIAN_POINT ( 'NONE',  ( -21.14250536705909411, 76.00000000001271871, -210.0412796614051274 ) ) ;
#63552 = VERTEX_POINT ( 'NONE', #22562 ) ;
#63553 = CARTESIAN_POINT ( 'NONE',  ( -20.95000000000000284, 11.74999999999999822, -6.841600689897113341 ) ) ;
#63554 = EDGE_LOOP ( 'NONE', ( #135585, #87053, #13600, #166156 ) ) ;
#63555 = CARTESIAN_POINT ( 'NONE',  ( 22.41477678272288188, 0.0008238657741001855503, -122.3504147154846180 ) ) ;
#63556 = CARTESIAN_POINT ( 'NONE',  ( 18.39999999999997371, 64.52683809664929981, -78.77310748452438816 ) ) ;
#63557 = LINE ( 'NONE', #144356, #233938 ) ;
#63558 = CARTESIAN_POINT ( 'NONE',  ( 23.14999999999999858, 7.128833340094563376, -233.7327013124401276 ) ) ;
#63559 = ORIENTED_EDGE ( 'NONE', *, *, #222355, .T. ) ;
#63560 = VECTOR ( 'NONE', #37377, 1000.000000000000000 ) ;
#63561 = DIRECTION ( 'NONE',  ( 0.000000000000000000, 0.000000000000000000, 1.000000000000000000 ) ) ;
#63562 = EDGE_LOOP ( 'NONE', ( #129321, #160226, #214364, #116988 ) ) ;
#63565 = ORIENTED_EDGE ( 'NONE', *, *, #34677, .F. ) ;
#63564 = DIRECTION ( 'NONE',  ( 1.000000000000000000, 0.000000000000000000, 0.000000000000000000 ) ) ;
#63563 = CARTESIAN_POINT ( 'NONE',  ( 18.51997666896889427, 47.01798221041575232, -255.2021870826413021 ) ) ;
#63566 = VECTOR ( 'NONE', #183938, 1000.000000000000227 ) ;
#63567 = EDGE_CURVE ( 'NONE', #75404, #30076, #181638, .T. ) ;
#63568 = CARTESIAN_POINT ( 'NONE',  ( -19.89999999999999858, 1.350000000000000089, 21.90000000000000213 ) ) ;
#63569 = EDGE_CURVE ( 'NONE', #17165, #174644, #26594, .T. ) ;
#63570 = ORIENTED_EDGE ( 'NONE', *, *, #13267, .F. ) ;
#63571 = DIRECTION ( 'NONE',  ( -0.000000000000000000, 1.000000000000000000, -1.224646799147352961E-16 ) ) ;
#63572 = ORIENTED_EDGE ( 'NONE', *, *, #133215, .T. ) ;
#63573 = CARTESIAN_POINT ( 'NONE',  ( 21.53699400384966367, 76.00000000001219291, -143.3108192777618797 ) ) ;
#63574 = ADVANCED_FACE ( 'NONE', ( #2971 ), #15976, .T. ) ;
#63575 = CIRCLE ( 'NONE', #138562, 0.1000000000000028644 ) ;
#63576 = DIRECTION ( 'NONE',  ( -3.469446951953635015E-14, 1.000000000000000000, 0.000000000000000000 ) ) ;
#63577 = LINE ( 'NONE', #66153, #63582 ) ;
#63578 = CARTESIAN_POINT ( 'NONE',  ( -18.52139480978223318, -9.481358845055737561, -74.02455656711912013 ) ) ;
#63579 = AXIS2_PLACEMENT_3D ( 'NONE', #149407, #71150, #234043 ) ;
#63580 = CARTESIAN_POINT ( 'NONE',  ( -16.88560720703333473, 9.950564843749692301, -12.64811192086371783 ) ) ;
#63581 = ADVANCED_FACE ( 'NONE', ( #104615 ), #5528, .T. ) ;
#63582 = VECTOR ( 'NONE', #179701, 1000.000000000000000 ) ;
#63583 = ORIENTED_EDGE ( 'NONE', *, *, #177329, .T. ) ;
#63584 = CIRCLE ( 'NONE', #71983, 0.09999999999999810429 ) ;
#63585 = AXIS2_PLACEMENT_3D ( 'NONE', #148661, #10429, #245186 ) ;
#63587 = EDGE_CURVE ( 'NONE', #149671, #62010, #45961, .T. ) ;
#63586 = CARTESIAN_POINT ( 'NONE',  ( -21.05000000000000071, -11.48912529307605901, -3.000000000000002665 ) ) ;
#63588 = DIRECTION ( 'NONE',  ( -0.000000000000000000, -0.8700118002898356018, 0.4930308989875170078 ) ) ;
#63589 = CARTESIAN_POINT ( 'NONE',  ( -18.54260524012593692, -9.624219390062691559, -140.7407730457707373 ) ) ;
#63590 = EDGE_LOOP ( 'NONE', ( #99637, #108586, #53246, #186507 ) ) ;
#63591 = CARTESIAN_POINT ( 'NONE',  ( -18.59999999999999787, 66.75000000001158185, -57.27310748452438816 ) ) ;
#63593 = ORIENTED_EDGE ( 'NONE', *, *, #220077, .T. ) ;
#63592 = CIRCLE ( 'NONE', #80121, 0.09999999999999810429 ) ;
#63594 = CARTESIAN_POINT ( 'NONE',  ( 20.95512820512820440, 65.37615131630001031, -95.35819391543677170 ) ) ;
#63595 = CIRCLE ( 'NONE', #38478, 0.1000000000000004496 ) ;
#63596 = DIRECTION ( 'NONE',  ( 1.000000000000000000, 0.000000000000000000, 0.000000000000000000 ) ) ;
#63597 = CARTESIAN_POINT ( 'NONE',  ( 20.94560253601876809, 36.04561250502854364, -235.8930046631029711 ) ) ;
#63599 = ORIENTED_EDGE ( 'NONE', *, *, #21343, .F. ) ;
#63598 = LINE ( 'NONE', #37973, #177807 ) ;
#63600 = EDGE_CURVE ( 'NONE', #181442, #10156, #99486, .T. ) ;
#63601 = CARTESIAN_POINT ( 'NONE',  ( -21.00857864376268935, 11.60000000001115161, -174.4282032302755283 ) ) ;
#63602 = AXIS2_PLACEMENT_3D ( 'NONE', #217012, #97032, #114063 ) ;
#63603 = DIRECTION ( 'NONE',  ( 0.000000000000000000, 0.000000000000000000, -1.000000000000000000 ) ) ;
#63604 = AXIS2_PLACEMENT_3D ( 'NONE', #258072, #139435, #118633 ) ;
#63605 = LINE ( 'NONE', #8775, #89506 ) ;
#63606 = ORIENTED_EDGE ( 'NONE', *, *, #15980, .T. ) ;
#63607 = ADVANCED_FACE ( 'NONE', ( #246720 ), #48526, .T. ) ;
#63608 = CIRCLE ( 'NONE', #155236, 0.1000000000000004496 ) ;
#63609 = CARTESIAN_POINT ( 'NONE',  ( 20.94999999999999929, 7.128833340093095217, -233.7327013124392749 ) ) ;
#63610 = CARTESIAN_POINT ( 'NONE',  ( 20.94999999999999929, 43.18640298906419162, -245.2812653309023574 ) ) ;
#63611 = ORIENTED_EDGE ( 'NONE', *, *, #133531, .T. ) ;
#63612 = CARTESIAN_POINT ( 'NONE',  ( 22.94999999999999929, 0.000000000000000000, 0.000000000000000000 ) ) ;
#63613 = CONICAL_SURFACE ( 'NONE', #34600, 4.000000000000000000, 0.7853981633974489451 ) ;
#63614 = ORIENTED_EDGE ( 'NONE', *, *, #118898, .T. ) ;
#63615 = AXIS2_PLACEMENT_3D ( 'NONE', #89126, #186974, #210373 ) ;
#63616 = CIRCLE ( 'NONE', #230212, 0.1000000000000013933 ) ;
#63617 = CARTESIAN_POINT ( 'NONE',  ( -23.25000000000000000, 0.000000000000000000, -41.40000000000000568 ) ) ;
#63618 = VECTOR ( 'NONE', #187352, 1000.000000000000000 ) ;
#63620 = ORIENTED_EDGE ( 'NONE', *, *, #100048, .T. ) ;
#63619 = DIRECTION ( 'NONE',  ( 0.000000000000000000, 0.000000000000000000, 1.000000000000000000 ) ) ;
#63621 = ADVANCED_FACE ( 'NONE', ( #188052 ), #147630, .F. ) ;
#63624 = ORIENTED_EDGE ( 'NONE', *, *, #240200, .F. ) ;
#63623 = ORIENTED_EDGE ( 'NONE', *, *, #163282, .T. ) ;
#63622 = CARTESIAN_POINT ( 'NONE',  ( 20.04999999999999716, 8.750000000000014211, -9.250000000000001776 ) ) ;
#63625 = CARTESIAN_POINT ( 'NONE',  ( 20.94999999999999929, 65.52661458509899717, -95.44445302027584432 ) ) ;
#63626 = DIRECTION ( 'NONE',  ( 0.000000000000000000, 0.000000000000000000, -1.000000000000000000 ) ) ;
#63627 = CARTESIAN_POINT ( 'NONE',  ( 18.59999999999999076, 74.75000000001158185, -61.52310748452433131 ) ) ;
#63629 = CARTESIAN_POINT ( 'NONE',  ( -16.86445178670652467, 9.962211629115985900, -20.89077743811727572 ) ) ;
#63628 = CARTESIAN_POINT ( 'NONE',  ( -16.87683809663752399, 54.76195096157923103, -157.3731074845245246 ) ) ;
#63630 = FACE_OUTER_BOUND ( 'NONE', #56102, .T. ) ;
#63631 = CIRCLE ( 'NONE', #155450, 14.30833333333333890 ) ;
#63632 = DIRECTION ( 'NONE',  ( 0.000000000000000000, 0.9623856809447771665, 0.2716869542551821892 ) ) ;
#63633 = AXIS2_PLACEMENT_3D ( 'NONE', #102622, #3542, #83048 ) ;
#63634 = CARTESIAN_POINT ( 'NONE',  ( -18.59999999999999787, -1.851028230129704522, -145.6539132694225032 ) ) ;
#63635 = FACE_OUTER_BOUND ( 'NONE', #11336, .T. ) ;
#63636 = ORIENTED_EDGE ( 'NONE', *, *, #207459, .F. ) ;
#63637 = ORIENTED_EDGE ( 'NONE', *, *, #247258, .T. ) ;
#63638 = CARTESIAN_POINT ( 'NONE',  ( 21.05000000000000071, 1.115600667400684642E-11, -180.3749999999999716 ) ) ;
#63640 = ORIENTED_EDGE ( 'NONE', *, *, #50789, .T. ) ;
#63639 = FACE_OUTER_BOUND ( 'NONE', #180546, .T. ) ;
#63641 = ORIENTED_EDGE ( 'NONE', *, *, #247156, .F. ) ;
#63642 = CARTESIAN_POINT ( 'NONE',  ( -17.11825945287481332, 65.95000000001201101, -115.7731074845243597 ) ) ;
#63643 = VERTEX_POINT ( 'NONE', #111071 ) ;
#63644 = CARTESIAN_POINT ( 'NONE',  ( -21.04999999999999716, 69.70076908991985931, -136.6215449845246610 ) ) ;
#63645 = ORIENTED_EDGE ( 'NONE', *, *, #19678, .T. ) ;
#63646 = CARTESIAN_POINT ( 'NONE',  ( -23.15000000000000213, 61.47936603916258491, -212.1738987416902376 ) ) ;
#63647 = VECTOR ( 'NONE', #24269, 1000.000000000000000 ) ;
#63649 = ORIENTED_EDGE ( 'NONE', *, *, #30452, .F. ) ;
#63648 = ORIENTED_EDGE ( 'NONE', *, *, #197823, .F. ) ;
#63650 = ORIENTED_EDGE ( 'NONE', *, *, #69337, .F. ) ;
#63651 = DIRECTION ( 'NONE',  ( 0.000000000000000000, 1.000000000000000000, 0.000000000000000000 ) ) ;
#63652 = ORIENTED_EDGE ( 'NONE', *, *, #113924, .T. ) ;
#63653 = ORIENTED_EDGE ( 'NONE', *, *, #15197, .F. ) ;
#63654 = PLANE ( 'NONE',  #126114 ) ;
#63655 = DIRECTION ( 'NONE',  ( 0.000000000000000000, 0.8068669527896844551, 0.5907332058517525963 ) ) ;
#63656 = CIRCLE ( 'NONE', #55253, 11.74999999999999645 ) ;
#63658 = EDGE_LOOP ( 'NONE', ( #107027, #44684, #47112 ) ) ;
#63657 = PLANE ( 'NONE',  #51862 ) ;
#63660 = CARTESIAN_POINT ( 'NONE',  ( -16.87851181299898684, 60.93927877302353124, -221.0418550117870780 ) ) ;
#63659 = DIRECTION ( 'NONE',  ( 1.000000000000000000, 0.000000000000000000, 0.000000000000000000 ) ) ;
#63661 = CARTESIAN_POINT ( 'NONE',  ( 21.07946286933444924, 0.07668384326756234881, -60.67096268099236056 ) ) ;
#63662 = DIRECTION ( 'NONE',  ( 1.000000000000000000, 0.000000000000000000, 0.000000000000000000 ) ) ;
#63663 = CARTESIAN_POINT ( 'NONE',  ( -22.24259225415828567, 7.491937870576586889, -66.90093411654720512 ) ) ;
#63664 = ORIENTED_EDGE ( 'NONE', *, *, #252410, .F. ) ;
#63665 = DIRECTION ( 'NONE',  ( 0.000000000000000000, 0.000000000000000000, -1.000000000000000000 ) ) ;
#63666 = VERTEX_POINT ( 'NONE', #30270 ) ;
#63667 = DIRECTION ( 'NONE',  ( 0.000000000000000000, 0.000000000000000000, -1.000000000000000000 ) ) ;
#63668 = DIRECTION ( 'NONE',  ( -1.000000000000000000, 0.000000000000000000, 0.000000000000000000 ) ) ;
#63669 = EDGE_CURVE ( 'NONE', #154183, #11174, #159869, .T. ) ;
#63670 = ORIENTED_EDGE ( 'NONE', *, *, #134213, .T. ) ;
#63671 = CARTESIAN_POINT ( 'NONE',  ( 21.09551895715218350, 10.62143732718005573, -45.73712466589949344 ) ) ;
#63672 = AXIS2_PLACEMENT_3D ( 'NONE', #8335, #89134, #171299 ) ;
#63673 = CARTESIAN_POINT ( 'NONE',  ( -20.94999999999999929, 76.00000000001195133, -103.0231074845243171 ) ) ;
#63674 = CARTESIAN_POINT ( 'NONE',  ( -12.29659703204451660, 12.60783650272741241, -214.9246183040210667 ) ) ;
#63675 = ORIENTED_EDGE ( 'NONE', *, *, #20272, .F. ) ;
#63676 = ORIENTED_EDGE ( 'NONE', *, *, #52376, .T. ) ;
#63677 = DIRECTION ( 'NONE',  ( 1.000000000000000000, -0.000000000000000000, -0.000000000000000000 ) ) ;
#63678 = FACE_OUTER_BOUND ( 'NONE', #15909, .T. ) ;
#63679 = VERTEX_POINT ( 'NONE', #47227 ) ;
#63680 = DIRECTION ( 'NONE',  ( -1.000000000000000000, 0.000000000000000000, 0.000000000000000000 ) ) ;
#63681 = ORIENTED_EDGE ( 'NONE', *, *, #246397, .T. ) ;
#63682 = CARTESIAN_POINT ( 'NONE',  ( 20.85000000000000142, 64.65966496992308521, -200.4475097531309586 ) ) ;
#63683 = DIRECTION ( 'NONE',  ( -0.7071067811865475727, -0.7071067811865475727, 0.000000000000000000 ) ) ;
#63685 = FACE_OUTER_BOUND ( 'NONE', #235443, .T. ) ;
#63684 = CARTESIAN_POINT ( 'NONE',  ( 20.85000000000000142, 76.00000000001213607, -136.5231074845243313 ) ) ;
#63686 = ADVANCED_FACE ( 'NONE', ( #186776 ), #225848, .T. ) ;
#63687 = CARTESIAN_POINT ( 'NONE',  ( -33.72168855820452649, 16.37079970714665933, -222.2530670965321349 ) ) ;
#63688 = CARTESIAN_POINT ( 'NONE',  ( -20.00857864376270001, 9.150000000000002132, -12.34999999999999964 ) ) ;
#63689 = ORIENTED_EDGE ( 'NONE', *, *, #4608, .F. ) ;
#63690 = AXIS2_PLACEMENT_3D ( 'NONE', #78831, #59243, #123130 ) ;
#63691 = CARTESIAN_POINT ( 'NONE',  ( 18.31572054635732982, -9.548475435767892705, -207.8505701647481487 ) ) ;
#63692 = VECTOR ( 'NONE', #101327, 1000.000000000000000 ) ;
#63694 = ORIENTED_EDGE ( 'NONE', *, *, #71554, .F. ) ;
#63693 = VERTEX_POINT ( 'NONE', #210188 ) ;
#63695 = VERTEX_POINT ( 'NONE', #31573 ) ;
#63696 = ORIENTED_EDGE ( 'NONE', *, *, #29942, .F. ) ;
#63697 = CIRCLE ( 'NONE', #42863, 0.09999999999999395484 ) ;
#63698 = EDGE_CURVE ( 'NONE', #219655, #204834, #64182, .T. ) ;
#63699 = DIRECTION ( 'NONE',  ( 0.7071067811865487940, 0.000000000000000000, -0.7071067811865463515 ) ) ;
#63700 = DIRECTION ( 'NONE',  ( 0.000000000000000000, 0.2534589355813222089, 0.9673461469267261581 ) ) ;
#63701 = CARTESIAN_POINT ( 'NONE',  ( 20.94999999999999929, 7.128833340094563376, -233.7327013124401276 ) ) ;
#63703 = EDGE_CURVE ( 'NONE', #159037, #178237, #255659, .T. ) ;
#63702 = CARTESIAN_POINT ( 'NONE',  ( 18.59999999999999787, 47.95459712139159336, -246.5019368548292675 ) ) ;
#63704 = FACE_OUTER_BOUND ( 'NONE', #106636, .T. ) ;
#63706 = DIRECTION ( 'NONE',  ( 0.000000000000000000, 0.000000000000000000, 1.000000000000000000 ) ) ;
#63705 = DIRECTION ( 'NONE',  ( 0.000000000000000000, 0.000000000000000000, -1.000000000000000000 ) ) ;
#63708 = ORIENTED_EDGE ( 'NONE', *, *, #42807, .T. ) ;
#63707 = PLANE ( 'NONE',  #173068 ) ;
#63709 = CARTESIAN_POINT ( 'NONE',  ( -22.50000000000000000, 11.64976291804307884, -100.4111900236131021 ) ) ;
#63710 = VERTEX_POINT ( 'NONE', #86340 ) ;
#63711 = ADVANCED_FACE ( 'NONE', ( #128074 ), #248007, .T. ) ;
#63712 = CARTESIAN_POINT ( 'NONE',  ( 22.32929514600007792, 33.47007643119025033, -242.6753381395425322 ) ) ;
#63713 = ORIENTED_EDGE ( 'NONE', *, *, #237164, .F. ) ;
#63714 = ORIENTED_EDGE ( 'NONE', *, *, #246706, .T. ) ;
#63715 = DIRECTION ( 'NONE',  ( 1.000000000000000000, 0.000000000000000000, 0.000000000000000000 ) ) ;
#63716 = VECTOR ( 'NONE', #65593, 1000.000000000000000 ) ;
#63717 = CARTESIAN_POINT ( 'NONE',  ( -18.59999999999999787, 66.65000000001259650, -191.1731074845244223 ) ) ;
#63718 = VECTOR ( 'NONE', #179403, 1000.000000000000114 ) ;
#63719 = DIRECTION ( 'NONE',  ( 0.000000000000000000, -0.1298341882520079038, -0.9915357197604846018 ) ) ;
#63720 = EDGE_CURVE ( 'NONE', #142525, #201784, #105844, .T. ) ;
#63721 = ADVANCED_BREP_SHAPE_REPRESENTATION ( '', ( #18376, #2425 ), #89914 ) ;
#63722 = CARTESIAN_POINT ( 'NONE',  ( 23.14999999999999858, 1.115600667400684642E-11, -167.5000000000000284 ) ) ;
#63723 = ORIENTED_EDGE ( 'NONE', *, *, #50008, .F. ) ;
#63725 = VERTEX_POINT ( 'NONE', #11997 ) ;
#63724 = EDGE_CURVE ( 'NONE', #89014, #231809, #109954, .T. ) ;
#63726 = AXIS2_PLACEMENT_3D ( 'NONE', #201919, #63677, #243607 ) ;
#63727 = DIRECTION ( 'NONE',  ( 1.000000000000000000, 0.000000000000000000, 0.000000000000000000 ) ) ;
#63728 = VERTEX_POINT ( 'NONE', #108502 ) ;
#63729 = DIRECTION ( 'NONE',  ( 1.000000000000000000, 0.000000000000000000, 0.000000000000000000 ) ) ;
#63730 = DIRECTION ( 'NONE',  ( 0.000000000000000000, -6.982962677686266711E-15, 1.000000000000000000 ) ) ;
#63731 = DIRECTION ( 'NONE',  ( 0.000000000000000000, -0.9992764785629962843, -0.03803313543132441632 ) ) ;
#63732 = CARTESIAN_POINT ( 'NONE',  ( -23.15000000000000213, 87.65000000001144542, -39.12310748452424747 ) ) ;
#63733 = FACE_OUTER_BOUND ( 'NONE', #221030, .T. ) ;
#63734 = DIRECTION ( 'NONE',  ( 0.000000000000000000, -1.000000000000000000, -6.982962677686266711E-15 ) ) ;
#63735 = FACE_OUTER_BOUND ( 'NONE', #149067, .T. ) ;
#63736 = CIRCLE ( 'NONE', #180439, 0.09999999999999939493 ) ;
#63738 = CARTESIAN_POINT ( 'NONE',  ( 22.10000000000000497, 6.223900101154157483, 12.00000000000000000 ) ) ;
#63737 = CIRCLE ( 'NONE', #118077, 0.09999999999999939493 ) ;
#63740 = DIRECTION ( 'NONE',  ( 0.000000000000000000, 1.000000000000000000, 0.000000000000000000 ) ) ;
#63739 = AXIS2_PLACEMENT_3D ( 'NONE', #247591, #89787, #66393 ) ;
#63741 = EDGE_CURVE ( 'NONE', #60637, #65006, #9395, .T. ) ;
#63742 = AXIS2_PLACEMENT_3D ( 'NONE', #164812, #21464, #124406 ) ;
#63743 = CARTESIAN_POINT ( 'NONE',  ( -21.05000000000000071, 6.284975638137225040, -199.7187985938684847 ) ) ;
#63744 = DIRECTION ( 'NONE',  ( 1.000000000000000000, 1.646408749285562691E-14, 1.073024830501117725E-15 ) ) ;
#63745 = DIRECTION ( 'NONE',  ( 0.000000000000000000, -6.982962677686266711E-15, 1.000000000000000000 ) ) ;
#63746 = B_SPLINE_CURVE_WITH_KNOTS ( 'NONE', 3,
 ( #181949, #142788, #65840, #82801, #204062, #62008, #162396, #63269, #25450, #146643, #145375, #104931, #41178, #224901, #184494, #125811, #222318, #120713, #221056, #42430, #202786, #71012, #33188, #190960, #167544, #129672 ),
 .UNSPECIFIED., .F., .F.,
 ( 4, 2, 2, 2, 2, 2, 2, 2, 2, 2, 2, 2, 4 ),
 ( 0.005476422646581329164, 0.006160811967703526230, 0.006845201288825725032, 0.007187395949386824433, 0.007529590609947924701, 0.007871785270509024102, 0.008213979931070123502, 0.008556174591631222903, 0.008898369252192322304, 0.009240563912753421705, 0.009582758573314522840, 0.01026714789443678236, 0.01095153721555904361 ),
 .UNSPECIFIED. ) ;
#63747 = ORIENTED_EDGE ( 'NONE', *, *, #178575, .T. ) ;
#63748 = DIRECTION ( 'NONE',  ( 0.000000000000000000, 1.000000000000000000, -0.000000000000000000 ) ) ;
#63749 = ORIENTED_EDGE ( 'NONE', *, *, #166281, .T. ) ;
#63750 = DIRECTION ( 'NONE',  ( -0.000000000000000000, -1.000000000000000000, -6.982962677686266711E-15 ) ) ;
#63751 = DIRECTION ( 'NONE',  ( 0.000000000000000000, -1.000000000000000000, -8.717686153663073805E-15 ) ) ;
#63752 = CARTESIAN_POINT ( 'NONE',  ( 23.14999999999999858, 1.115600667400684642E-11, -200.9999999999999432 ) ) ;
#63753 = EDGE_LOOP ( 'NONE', ( #210058, #245614, #43344, #192509, #40982 ) ) ;
#63754 = FACE_OUTER_BOUND ( 'NONE', #234909, .T. ) ;
#63755 = AXIS2_PLACEMENT_3D ( 'NONE', #38460, #157149, #236651 ) ;
#63756 = LINE ( 'NONE', #224107, #56387 ) ;
#63757 = CARTESIAN_POINT ( 'NONE',  ( -21.05000000000000071, 7.980037321000002848, -237.6410835587014390 ) ) ;
#63759 = CIRCLE ( 'NONE', #146940, 0.09999999999998657185 ) ;
#63758 = DIRECTION ( 'NONE',  ( 0.000000000000000000, 0.8814952561688476074, -0.4721928772777262417 ) ) ;
#63760 = FACE_OUTER_BOUND ( 'NONE', #192422, .T. ) ;
#63761 = DIRECTION ( 'NONE',  ( 1.186688945009010077E-16, -1.000000000000000000, -0.000000000000000000 ) ) ;
#63762 = EDGE_CURVE ( 'NONE', #20329, #73365, #5886, .T. ) ;
#63763 = EDGE_CURVE ( 'NONE', #17245, #74531, #84990, .T. ) ;
#63764 = EDGE_LOOP ( 'NONE', ( #122974, #13901, #199862 ) ) ;
#63765 = CARTESIAN_POINT ( 'NONE',  ( -23.25000000000000000, -8.999999999988846255, -43.39396912265245021 ) ) ;
#63767 = EDGE_LOOP ( 'NONE', ( #167910, #174269, #80428, #74046 ) ) ;
#63766 = DIRECTION ( 'NONE',  ( 1.000000000000000000, 0.000000000000000000, 0.000000000000000000 ) ) ;
#63768 = VECTOR ( 'NONE', #215203, 999.9999999999998863 ) ;
#63769 = CARTESIAN_POINT ( 'NONE',  ( 23.24999999999999645, 45.93587830916155212, -239.9163948487882863 ) ) ;
#63770 = CIRCLE ( 'NONE', #155385, 0.1000000000000004774 ) ;
#63771 = CARTESIAN_POINT ( 'NONE',  ( -18.59999999999999787, 45.93315328338058379, -256.6017782078560003 ) ) ;
#63773 = ADVANCED_FACE ( 'NONE', ( #169806 ), #150219, .F. ) ;
#63772 = PRESENTATION_STYLE_ASSIGNMENT (( #242402 ) ) ;
#63774 = EDGE_CURVE ( 'NONE', #73568, #177428, #51668, .T. ) ;
#63775 = VERTEX_POINT ( 'NONE', #51058 ) ;
#63776 = CARTESIAN_POINT ( 'NONE',  ( -21.65000000000000213, 9.950000000011140600, -154.7500000000000284 ) ) ;
#63777 = VECTOR ( 'NONE', #157795, 1000.000000000000000 ) ;
#63779 = AXIS2_PLACEMENT_3D ( 'NONE', #16171, #132239, #192229 ) ;
#63778 = DIRECTION ( 'NONE',  ( -1.000000000000000000, -2.952720810173289112E-16, 0.000000000000000000 ) ) ;
#63780 = EDGE_CURVE ( 'NONE', #171719, #88042, #60064, .T. ) ;
#63781 = ORIENTED_EDGE ( 'NONE', *, *, #149145, .F. ) ;
#63782 = LINE ( 'NONE', #179899, #75346 ) ;
#63783 = CARTESIAN_POINT ( 'NONE',  ( 18.39999999999998082, 20.70020979027691510, -227.9869476361872103 ) ) ;
#63784 = AXIS2_PLACEMENT_3D ( 'NONE', #80634, #203167, #239742 ) ;
#63785 = EDGE_CURVE ( 'NONE', #175396, #86058, #143279, .T. ) ;
#63786 = EDGE_CURVE ( 'NONE', #230954, #2619, #97460, .T. ) ;
#63787 = CIRCLE ( 'NONE', #76245, 0.2000000000000005107 ) ;
#63788 = CARTESIAN_POINT ( 'NONE',  ( 20.94999999999999574, 77.73625713160926409, -91.45445515550680682 ) ) ;
#63789 = ORIENTED_EDGE ( 'NONE', *, *, #118912, .T. ) ;
#63790 = ADVANCED_FACE ( 'NONE', ( #95363 ), #18378, .F. ) ;
#63791 = ORIENTED_EDGE ( 'NONE', *, *, #83314, .T. ) ;
#63792 = DIRECTION ( 'NONE',  ( -1.000000000000000000, -0.000000000000000000, -0.000000000000000000 ) ) ;
#63793 = CARTESIAN_POINT ( 'NONE',  ( 23.15000000000000213, 69.16514130714681130, -247.7543978865853660 ) ) ;
#63795 = AXIS2_PLACEMENT_3D ( 'NONE', #2791, #44517, #221828 ) ;
#63794 = CARTESIAN_POINT ( 'NONE',  ( -16.27683809663750480, 9.350000000011133849, -87.95000000000004547 ) ) ;
#63796 = AXIS2_PLACEMENT_3D ( 'NONE', #121937, #43680, #197601 ) ;
#63797 = CARTESIAN_POINT ( 'NONE',  ( -20.94999999999999929, 0.6713328740235187109, -212.7808875799876205 ) ) ;
#63798 = ADVANCED_FACE ( 'NONE', ( #176203 ), #56213, .F. ) ;
#63799 = CARTESIAN_POINT ( 'NONE',  ( -23.15000000000000213, 64.35000000001176090, -76.53791325517833855 ) ) ;
#63800 = DIRECTION ( 'NONE',  ( 1.000000000000000000, 0.000000000000000000, 0.000000000000000000 ) ) ;
#63802 = DIRECTION ( 'NONE',  ( 1.000000000000000000, 0.000000000000000000, 0.000000000000000000 ) ) ;
#63801 = CARTESIAN_POINT ( 'NONE',  ( 21.09107601085545269, -1.315832710461172006, -194.7735184721627775 ) ) ;
#63803 = AXIS2_PLACEMENT_3D ( 'NONE', #127780, #106912, #185178 ) ;
#63804 = CARTESIAN_POINT ( 'NONE',  ( 20.94999999999999574, 65.57661458509917907, -129.0310555606542664 ) ) ;
#63806 = EDGE_CURVE ( 'NONE', #24262, #67636, #93382, .T. ) ;
#63805 = CYLINDRICAL_SURFACE ( 'NONE', #43902, 0.09999999999999939493 ) ;
#63807 = DIRECTION ( 'NONE',  ( 0.000000000000000000, 1.000000000000000000, 0.000000000000000000 ) ) ;
#63809 = EDGE_CURVE ( 'NONE', #203688, #225819, #139153, .T. ) ;
#63808 = DIRECTION ( 'NONE',  ( 0.000000000000000000, 0.000000000000000000, -1.000000000000000000 ) ) ;
#63810 = ORIENTED_EDGE ( 'NONE', *, *, #123947, .T. ) ;
#63811 = ORIENTED_EDGE ( 'NONE', *, *, #32862, .T. ) ;
#63812 = CARTESIAN_POINT ( 'NONE',  ( 20.94999999999999929, 69.25640205380743453, -247.7135141964517402 ) ) ;
#63813 = CIRCLE ( 'NONE', #205435, 0.09999999999999989453 ) ;
#63814 = DIRECTION ( 'NONE',  ( 0.000000000000000000, 0.8814952561688438326, -0.4721928772777331806 ) ) ;
#63816 = CARTESIAN_POINT ( 'NONE',  ( 20.94999999999999929, 28.34113089492129589, -239.5930034413672161 ) ) ;
#63815 = DIRECTION ( 'NONE',  ( 0.000000000000000000, 0.1686199900910312910, -0.9856811345164826488 ) ) ;
#63817 = CIRCLE ( 'NONE', #130447, 0.1000000000000028644 ) ;
#63818 = CIRCLE ( 'NONE', #188698, 0.09999999999999996392 ) ;
#63819 = ADVANCED_FACE ( 'NONE', ( #173676 ), #57497, .T. ) ;
#63820 = VECTOR ( 'NONE', #115081, 1000.000000000000000 ) ;
#63821 = DIRECTION ( 'NONE',  ( 1.000000000000000000, 0.000000000000000000, 0.000000000000000000 ) ) ;
#63822 = CYLINDRICAL_SURFACE ( 'NONE', #258104, 0.1000000000000028644 ) ;
#63823 = CARTESIAN_POINT ( 'NONE',  ( -17.29158576265543346, 10.36474766602906783, -89.08275824479223104 ) ) ;
#63824 = EDGE_CURVE ( 'NONE', #44180, #122792, #234883, .T. ) ;
#63825 = ADVANCED_FACE ( 'NONE', ( #191928 ), #253140, .F. ) ;
#63826 = DIRECTION ( 'NONE',  ( -1.000000000000000000, -0.000000000000000000, 0.000000000000000000 ) ) ;
#63827 = ORIENTED_EDGE ( 'NONE', *, *, #85094, .F. ) ;
#63828 = DIRECTION ( 'NONE',  ( 1.000000000000000000, 0.000000000000000000, 0.000000000000000000 ) ) ;
#63829 = ORIENTED_EDGE ( 'NONE', *, *, #191542, .F. ) ;
#63830 = DIRECTION ( 'NONE',  ( 0.000000000000000000, 0.000000000000000000, -1.000000000000000000 ) ) ;
#63831 = AXIS2_PLACEMENT_3D ( 'NONE', #62301, #157599, #182259 ) ;
#63832 = TOROIDAL_SURFACE ( 'NONE', #138792, 0.9750000000000019762, 0.1000000000000000056 ) ;
#63833 = VECTOR ( 'NONE', #226520, 1000.000000000000114 ) ;
#63834 = CARTESIAN_POINT ( 'NONE',  ( 18.47135592147649774, 85.47108861327711793, -29.33951254468060554 ) ) ;
#63835 = ORIENTED_EDGE ( 'NONE', *, *, #142696, .F. ) ;
#63836 =( BOUNDED_CURVE ( )  B_SPLINE_CURVE ( 3, ( #92729, #52309, #114875, #194437 ),
 .UNSPECIFIED., .F., .F. ) 
 B_SPLINE_CURVE_WITH_KNOTS ( ( 4, 4 ),
 ( 3.141592653589793116, 4.712388980384689674 ),
 .UNSPECIFIED. ) 
 CURVE ( )  GEOMETRIC_REPRESENTATION_ITEM ( )  RATIONAL_B_SPLINE_CURVE ( ( 1.000000000000000000, 0.8047378541243649375, 0.8047378541243649375, 1.000000000000000000 ) ) 
 REPRESENTATION_ITEM ( '' )  );
#63837 = ORIENTED_EDGE ( 'NONE', *, *, #161923, .T. ) ;
#63838 = CARTESIAN_POINT ( 'NONE',  ( -20.85000000000000142, 68.97833521811179480, -99.28954208262706516 ) ) ;
#63839 = CARTESIAN_POINT ( 'NONE',  ( -23.25000000000000000, 69.06610602788553877, -99.23746165015076315 ) ) ;
#63840 = CARTESIAN_POINT ( 'NONE',  ( -23.15000000000000213, 64.25000000001176659, -76.53791325517833855 ) ) ;
#63841 = LINE ( 'NONE', #20891, #100096 ) ;
#63842 = DIRECTION ( 'NONE',  ( 0.000000000000000000, -0.9770955615653316162, -0.2128009952263604232 ) ) ;
#63843 = CARTESIAN_POINT ( 'NONE',  ( -16.97683809663752186, 66.05000000001257376, -183.4254715027207681 ) ) ;
#63844 = DIRECTION ( 'NONE',  ( 0.000000000000000000, 0.000000000000000000, -1.000000000000000000 ) ) ;
#63846 = ORIENTED_EDGE ( 'NONE', *, *, #16732, .F. ) ;
#63845 = CARTESIAN_POINT ( 'NONE',  ( 21.07888907270776002, 65.27493078649737868, -191.3019138976912359 ) ) ;
#63848 = CARTESIAN_POINT ( 'NONE',  ( -20.85000000000000142, 76.32388570108247450, -136.5655178952103768 ) ) ;
#63847 = LINE ( 'NONE', #123828, #16163 ) ;
#63849 = VERTEX_POINT ( 'NONE', #73267 ) ;
#63851 = ORIENTED_EDGE ( 'NONE', *, *, #6625, .T. ) ;
#63850 = CARTESIAN_POINT ( 'NONE',  ( 20.94999999999999929, -1.835341550213257733, -145.5551512925629822 ) ) ;
#63852 = ORIENTED_EDGE ( 'NONE', *, *, #176846, .T. ) ;
#63853 = DIRECTION ( 'NONE',  ( -1.000000000000000000, 0.000000000000000000, 0.000000000000000000 ) ) ;
#63854 = CARTESIAN_POINT ( 'NONE',  ( 20.94999999999999929, 9.765296417674898422, -220.4624455711005737 ) ) ;
#63855 = AXIS2_PLACEMENT_3D ( 'NONE', #119019, #96837, #198536 ) ;
#63856 = ORIENTED_EDGE ( 'NONE', *, *, #41038, .T. ) ;
#63857 = CARTESIAN_POINT ( 'NONE',  ( 20.85000000000000142, 69.15387683765879956, -32.28538121767450519 ) ) ;
#63858 = CARTESIAN_POINT ( 'NONE',  ( 20.95512820512820440, 8.876151316299269567, -112.6500000000000341 ) ) ;
#63859 = CARTESIAN_POINT ( 'NONE',  ( 18.39999999999999503, 62.50563584222673796, -209.4474707446456421 ) ) ;
#63860 = DIRECTION ( 'NONE',  ( 0.000000000000000000, 1.000000000000000000, 0.000000000000000000 ) ) ;
#63861 = CARTESIAN_POINT ( 'NONE',  ( -18.57399277249657032, 46.46487552657983144, -243.0839400145317484 ) ) ;
#63862 = EDGE_CURVE ( 'NONE', #93783, #242248, #39257, .T. ) ;
#63863 = CARTESIAN_POINT ( 'NONE',  ( 21.08134388332231879, 69.66531941949419604, -136.5989264020313669 ) ) ;
#63864 = ORIENTED_EDGE ( 'NONE', *, *, #68917, .T. ) ;
#63865 = ORIENTED_EDGE ( 'NONE', *, *, #96656, .F. ) ;
#63866 = EDGE_CURVE ( 'NONE', #68194, #56261, #96611, .T. ) ;
#63867 = CARTESIAN_POINT ( 'NONE',  ( 19.90000000000000924, 4.513204987021263825, 22.00000000000000355 ) ) ;
#63868 = TOROIDAL_SURFACE ( 'NONE', #168534, 0.4000000000000015210, 0.1000000000000000056 ) ;
#63869 = AXIS2_PLACEMENT_3D ( 'NONE', #223192, #81110, #141115 ) ;
#63870 = ORIENTED_EDGE ( 'NONE', *, *, #193486, .T. ) ;
#63871 = FACE_OUTER_BOUND ( 'NONE', #187474, .T. ) ;
#63872 = VERTEX_POINT ( 'NONE', #194486 ) ;
#63873 = CARTESIAN_POINT ( 'NONE',  ( -21.05000000000000071, 70.15000000001221281, -146.6556047088023149 ) ) ;
#63874 = ADVANCED_FACE ( 'NONE', ( #137056 ), #30886, .F. ) ;
#63875 = EDGE_CURVE ( 'NONE', #109914, #256719, #180885, .T. ) ;
#63876 = DIRECTION ( 'NONE',  ( 0.000000000000000000, -1.000000000000000000, 0.000000000000000000 ) ) ;
#63877 = DIRECTION ( 'NONE',  ( 1.000000000000000000, 0.000000000000000000, 0.000000000000000000 ) ) ;
#63878 = DIRECTION ( 'NONE',  ( 0.000000000000000000, 0.2617529984164915779, 0.9651348961777187485 ) ) ;
#63879 = CARTESIAN_POINT ( 'NONE',  ( 22.39999999999999503, 0.09999999999999939493, 7.790779598373383408 ) ) ;
#63880 = ORIENTED_EDGE ( 'NONE', *, *, #168658, .T. ) ;
#63881 = CARTESIAN_POINT ( 'NONE',  ( -21.00000000000000000, 0.000000000000000000, 0.000000000000000000 ) ) ;
#63883 = AXIS2_PLACEMENT_3D ( 'NONE', #135004, #38513, #196287 ) ;
#63882 = DIRECTION ( 'NONE',  ( 0.000000000000000000, 0.9876197685951241256, 0.1568667991644932258 ) ) ;
#63884 = CARTESIAN_POINT ( 'NONE',  ( 18.49713797159854778, 85.44648232759047346, -62.45164936291396884 ) ) ;
#63885 = CYLINDRICAL_SURFACE ( 'NONE', #18349, 11.74999999999999645 ) ;
#63886 = ORIENTED_EDGE ( 'NONE', *, *, #155788, .F. ) ;
#63888 = LINE ( 'NONE', #163008, #127214 ) ;
#63887 = CARTESIAN_POINT ( 'NONE',  ( -22.37643362114956602, 75.90091862633104824, -177.6488974784827519 ) ) ;
#63890 = ORIENTED_EDGE ( 'NONE', *, *, #65234, .T. ) ;
#63889 = AXIS2_PLACEMENT_3D ( 'NONE', #125465, #41129, #161061 ) ;
#63893 = ORIENTED_EDGE ( 'NONE', *, *, #128126, .F. ) ;
#63892 = DIRECTION ( 'NONE',  ( 0.000000000000000000, -0.2128009952263403282, 0.9770955615653358350 ) ) ;
#63891 = CARTESIAN_POINT ( 'NONE',  ( -20.85000000000000142, 79.19526988099229925, -196.1889237952725296 ) ) ;
#63894 = ORIENTED_EDGE ( 'NONE', *, *, #14740, .T. ) ;
#63895 = CARTESIAN_POINT ( 'NONE',  ( -17.01764560440453522, 9.950000000011138823, -113.2499999992132302 ) ) ;
#63896 = EDGE_CURVE ( 'NONE', #254455, #189298, #214208, .T. ) ;
#63898 = DIRECTION ( 'NONE',  ( 0.000000000000000000, -1.000000000000000000, -6.982962677686266711E-15 ) ) ;
#63897 = AXIS2_PLACEMENT_3D ( 'NONE', #78473, #19819, #216711 ) ;
#63899 = DIRECTION ( 'NONE',  ( 1.000000000000000000, 3.190570557967288949E-16, 6.948722487160392945E-17 ) ) ;
#63900 = ORIENTED_EDGE ( 'NONE', *, *, #120504, .F. ) ;
#63901 = CARTESIAN_POINT ( 'NONE',  ( 20.73486653747088937, 7.750000000011182166, -113.1500000000000483 ) ) ;
#63902 = CARTESIAN_POINT ( 'NONE',  ( 18.49999999999999289, 64.25000000001246292, -181.7731074845244450 ) ) ;
#63904 = SPHERICAL_SURFACE ( 'NONE', #63400, 0.1000000000000000056 ) ;
#63903 = CARTESIAN_POINT ( 'NONE',  ( 21.14999999999999503, 44.06843597547144498, -258.9974126733343951 ) ) ;
#63906 = ORIENTED_EDGE ( 'NONE', *, *, #216847, .F. ) ;
#63905 = CARTESIAN_POINT ( 'NONE',  ( -21.05000000000000071, 62.82351852614503684, -207.2177435922979214 ) ) ;
#63907 = AXIS2_PLACEMENT_3D ( 'NONE', #64956, #124950, #204464 ) ;
#63908 = ADVANCED_FACE ( 'NONE', ( #135467 ), #138030, .F. ) ;
#63909 = AXIS2_PLACEMENT_3D ( 'NONE', #8356, #150444, #194714 ) ;
#63910 = EDGE_LOOP ( 'NONE', ( #23352, #118870, #159912, #192665 ) ) ;
#63912 = ADVANCED_FACE ( 'NONE', ( #175923 ), #209937, .T. ) ;
#63911 = CARTESIAN_POINT ( 'NONE',  ( -16.87851181299898684, 9.950042924018893231, -79.64985648463313339 ) ) ;
#63913 = DIRECTION ( 'NONE',  ( 1.000000000000000000, 3.469446951953704435E-14, -2.003086131649669752E-14 ) ) ;
#63914 = CARTESIAN_POINT ( 'NONE',  ( 21.05000000000000071, 0.000000000000000000, 0.000000000000000000 ) ) ;
#63915 = EDGE_LOOP ( 'NONE', ( #66149, #74598, #249389, #203759 ) ) ;
#63916 = CARTESIAN_POINT ( 'NONE',  ( -21.05000000000000071, 4.288595810029049993, -211.9930862808554934 ) ) ;
#63917 = ORIENTED_EDGE ( 'NONE', *, *, #63741, .T. ) ;
#63919 = VECTOR ( 'NONE', #167636, 1000.000000000000000 ) ;
#63918 = CARTESIAN_POINT ( 'NONE',  ( -18.50000000000000000, 76.00000000001126921, -203.5231074845248997 ) ) ;
#63920 = CARTESIAN_POINT ( 'NONE',  ( 21.14999999999999503, 11.65000000000000746, -3.469446951953614189E-15 ) ) ;
#63921 = DIRECTION ( 'NONE',  ( 0.000000000000000000, 1.000000000000000000, 0.000000000000000000 ) ) ;
#63922 = ORIENTED_EDGE ( 'NONE', *, *, #44029, .T. ) ;
#63923 = EDGE_CURVE ( 'NONE', #149131, #61324, #26783, .T. ) ;
#63924 = LINE ( 'NONE', #204696, #245926 ) ;
#63925 = CIRCLE ( 'NONE', #176367, 11.74999999999999645 ) ;
#63926 = CIRCLE ( 'NONE', #197181, 0.1000000000000008937 ) ;
#63927 = ADVANCED_FACE ( 'NONE', ( #174668 ), #238436, .T. ) ;
#63928 = VECTOR ( 'NONE', #37837, 1000.000000000000000 ) ;
#63929 = EDGE_CURVE ( 'NONE', #33086, #43374, #172560, .T. ) ;
#63930 = DIRECTION ( 'NONE',  ( -1.000000000000000000, 7.304098846218135653E-16, -4.607487905232624742E-31 ) ) ;
#63931 = ORIENTED_EDGE ( 'NONE', *, *, #64667, .T. ) ;
#63932 = EDGE_LOOP ( 'NONE', ( #231003, #21213, #37116, #46028 ) ) ;
#63933 =( BOUNDED_CURVE ( )  B_SPLINE_CURVE ( 3, ( #51240, #193368, #195939, #74730 ),
 .UNSPECIFIED., .F., .T. ) 
 B_SPLINE_CURVE_WITH_KNOTS ( ( 4, 4 ),
 ( 5.733388419619901200, 5.983100554402347449 ),
 .UNSPECIFIED. ) 
 CURVE ( )  GEOMETRIC_REPRESENTATION_ITEM ( )  RATIONAL_B_SPLINE_CURVE ( ( 1.000000000000000000, 0.9948104011409417691, 0.9948104011409417691, 1.000000000000000000 ) ) 
 REPRESENTATION_ITEM ( '' )  );
#63934 = ORIENTED_EDGE ( 'NONE', *, *, #196733, .F. ) ;
#63935 = DIRECTION ( 'NONE',  ( 0.000000000000000000, -0.4999999999999088507, 0.8660254037844913322 ) ) ;
#63936 = ORIENTED_EDGE ( 'NONE', *, *, #179991, .F. ) ;
#63938 = ORIENTED_EDGE ( 'NONE', *, *, #154801, .F. ) ;
#63937 = CARTESIAN_POINT ( 'NONE',  ( 15.31784899511109010, 66.60336962369487424, -185.6160500917061995 ) ) ;
#63939 = B_SPLINE_CURVE_WITH_KNOTS ( 'NONE', 3,
 ( #111266, #228661, #210371, #95542, #192101, #33059, #154290, #209076, #232516, #52555 ),
 .UNSPECIFIED., .F., .F.,
 ( 4, 2, 2, 2, 4 ),
 ( 5.285415200657074080E-16, 9.930191194499933679E-05, 0.0001986038238894701521, 0.0003972076477784117557, 0.0007944152955563480887 ),
 .UNSPECIFIED. ) ;
#63940 = EDGE_CURVE ( 'NONE', #19038, #127095, #196734, .T. ) ;
#63941 = ORIENTED_EDGE ( 'NONE', *, *, #99081, .T. ) ;
#63944 = ORIENTED_EDGE ( 'NONE', *, *, #11529, .T. ) ;
#63943 = ORIENTED_EDGE ( 'NONE', *, *, #16437, .F. ) ;
#63942 = CARTESIAN_POINT ( 'NONE',  ( -16.79814274880124358, 9.949272542688458287, -113.1524330370480271 ) ) ;
#63945 = ADVANCED_FACE ( 'NONE', ( #254131 ), #243220, .T. ) ;
#63946 = AXIS2_PLACEMENT_3D ( 'NONE', #137888, #196589, #76644 ) ;
#63947 = AXIS2_PLACEMENT_3D ( 'NONE', #197110, #22362, #178885 ) ;
#63948 = VERTEX_POINT ( 'NONE', #178490 ) ;
#63949 = DIRECTION ( 'NONE',  ( 1.000000000000000000, 0.000000000000000000, 0.000000000000000000 ) ) ;
#63950 = CARTESIAN_POINT ( 'NONE',  ( -21.14999999999999858, 11.65000000001115588, -134.1000000000000227 ) ) ;
#63951 = DIRECTION ( 'NONE',  ( 1.000000000000000000, 0.000000000000000000, 0.000000000000000000 ) ) ;
#63952 = VERTEX_POINT ( 'NONE', #55917 ) ;
#63953 = VECTOR ( 'NONE', #92681, 1000.000000000000000 ) ;
#63954 = DIRECTION ( 'NONE',  ( 1.000000000000000000, 0.000000000000000000, 0.000000000000000000 ) ) ;
#63955 = CIRCLE ( 'NONE', #30654, 0.1000000000000028644 ) ;
#63957 = ORIENTED_EDGE ( 'NONE', *, *, #194020, .T. ) ;
#63956 = DIRECTION ( 'NONE',  ( -0.5932847527679309119, 0.7865547670005533787, 0.1713032417725946777 ) ) ;
#63958 = CARTESIAN_POINT ( 'NONE',  ( 13.40000000000000036, -9.650000000000002132, 12.40000000000000391 ) ) ;
#63960 = ORIENTED_EDGE ( 'NONE', *, *, #191204, .T. ) ;
#63959 = PLANE ( 'NONE',  #172966 ) ;
#63961 = ORIENTED_EDGE ( 'NONE', *, *, #10479, .T. ) ;
#63962 = CIRCLE ( 'NONE', #118118, 0.1000000000000054040 ) ;
#63963 = CIRCLE ( 'NONE', #17588, 0.1000000000000002554 ) ;
#63965 = ORIENTED_EDGE ( 'NONE', *, *, #247835, .F. ) ;
#63964 = VECTOR ( 'NONE', #140768, 999.9999999999998863 ) ;
#63966 = EDGE_LOOP ( 'NONE', ( #8696, #71935, #52375, #16477 ) ) ;
#63967 = CIRCLE ( 'NONE', #130598, 0.09999999999999857614 ) ;
#63968 = CARTESIAN_POINT ( 'NONE',  ( -16.97683809663752186, 9.950000000011137047, -180.9023640181964652 ) ) ;
#63969 = CARTESIAN_POINT ( 'NONE',  ( -21.05000000000000071, -0.09999999998884474828, -160.9593430482987344 ) ) ;
#63970 = AXIS2_PLACEMENT_3D ( 'NONE', #153776, #211129, #155035 ) ;
#63972 = ORIENTED_EDGE ( 'NONE', *, *, #120988, .F. ) ;
#63971 = ORIENTED_EDGE ( 'NONE', *, *, #94419, .F. ) ;
#63973 = ORIENTED_EDGE ( 'NONE', *, *, #211617, .F. ) ;
#63974 = CARTESIAN_POINT ( 'NONE',  ( -20.54999999999999716, 68.75000000001253397, -182.3731074845244109 ) ) ;
#63975 = ORIENTED_EDGE ( 'NONE', *, *, #237801, .T. ) ;
#63976 = ORIENTED_EDGE ( 'NONE', *, *, #244823, .F. ) ;
#63977 = CARTESIAN_POINT ( 'NONE',  ( 20.73486653747088582, 68.75000000001156764, -60.27310748452437394 ) ) ;
#63979 = ORIENTED_EDGE ( 'NONE', *, *, #252204, .F. ) ;
#63978 = CARTESIAN_POINT ( 'NONE',  ( -21.05000000000000071, 43.57568952063339651, -245.1784935019914826 ) ) ;
#63980 = CARTESIAN_POINT ( 'NONE',  ( -22.94999999999999929, -1.885425182446134107, -11.49641995933507843 ) ) ;
#63981 = AXIS2_PLACEMENT_3D ( 'NONE', #203274, #139427, #100297 ) ;
#63982 = CARTESIAN_POINT ( 'NONE',  ( 18.59999999999999787, -9.321008403350148797, -107.7359382490778899 ) ) ;
#63983 = VERTEX_POINT ( 'NONE', #160211 ) ;
#63985 = ORIENTED_EDGE ( 'NONE', *, *, #70424, .F. ) ;
#63984 = ORIENTED_EDGE ( 'NONE', *, *, #134902, .F. ) ;
#63986 = AXIS2_PLACEMENT_3D ( 'NONE', #126159, #67481, #87023 ) ;
#63987 = CARTESIAN_POINT ( 'NONE',  ( -21.05000000000000071, 0.000000000000000000, 0.000000000000000000 ) ) ;
#63988 = FILL_AREA_STYLE ('',( #181393 ) ) ;
#63989 = ORIENTED_EDGE ( 'NONE', *, *, #176614, .T. ) ;
#63990 = VECTOR ( 'NONE', #123295, 1000.000000000000000 ) ;
#63991 = DIRECTION ( 'NONE',  ( -1.000000000000000000, -0.000000000000000000, -0.000000000000000000 ) ) ;
#63992 = ORIENTED_EDGE ( 'NONE', *, *, #125434, .T. ) ;
#63993 = ORIENTED_EDGE ( 'NONE', *, *, #215601, .T. ) ;
#63994 = DIRECTION ( 'NONE',  ( 0.000000000000000000, 1.000000000000000000, 0.000000000000000000 ) ) ;
#63995 = EDGE_CURVE ( 'NONE', #175127, #63414, #135060, .T. ) ;
#63996 = ORIENTED_EDGE ( 'NONE', *, *, #140077, .T. ) ;
#63997 = CARTESIAN_POINT ( 'NONE',  ( 18.59999999999999787, -1.835341550213255957, -78.55515129256302487 ) ) ;
#63998 = CARTESIAN_POINT ( 'NONE',  ( 26.01805557925458956, 8.624264858734573380, -347.0000000000001137 ) ) ;
#63999 = ORIENTED_EDGE ( 'NONE', *, *, #63866, .F. ) ;
#64000 = CARTESIAN_POINT ( 'NONE',  ( 19.75857864376268935, 64.25000000001220712, -145.2731074845243882 ) ) ;
#64001 = CARTESIAN_POINT ( 'NONE',  ( -20.64999999999999858, 4.350000000011156054, -112.8500000000000369 ) ) ;
#64003 = DIRECTION ( 'NONE',  ( 0.000000000000000000, 0.000000000000000000, -1.000000000000000000 ) ) ;
#64002 = DIRECTION ( 'NONE',  ( -3.265361837132814079E-16, 0.4721928772777338468, 0.8814952561688436106 ) ) ;
#64004 = FACE_OUTER_BOUND ( 'NONE', #143171, .T. ) ;
#64005 = EDGE_CURVE ( 'NONE', #49226, #91113, #201533, .T. ) ;
#64007 = ADVANCED_FACE ( 'NONE', ( #38968 ), #36411, .T. ) ;
#64006 = DIRECTION ( 'NONE',  ( -1.000000000000000000, -0.000000000000000000, 0.000000000000000000 ) ) ;
#64008 = CARTESIAN_POINT ( 'NONE',  ( 21.14999999999999858, 69.35000000001156195, -57.37310748452436826 ) ) ;
#64009 = CARTESIAN_POINT ( 'NONE',  ( -23.15000000000000213, 76.00000000001190870, -103.0231074845243029 ) ) ;
#64010 = DIRECTION ( 'NONE',  ( 0.000000000000000000, -0.8741572761215355980, 0.4856429311786357172 ) ) ;
#64011 = CIRCLE ( 'NONE', #138428, 0.1000000000000028644 ) ;
#64013 = VERTEX_POINT ( 'NONE', #40267 ) ;
#64012 = AXIS2_PLACEMENT_3D ( 'NONE', #242840, #159463, #100723 ) ;
#64014 = CIRCLE ( 'NONE', #209761, 0.1000000000000059591 ) ;
#64015 = VECTOR ( 'NONE', #13933, 1000.000000000000000 ) ;
#64017 = ORIENTED_EDGE ( 'NONE', *, *, #167730, .T. ) ;
#64016 = VERTEX_POINT ( 'NONE', #114636 ) ;
#64018 = ORIENTED_EDGE ( 'NONE', *, *, #78214, .T. ) ;
#64019 = EDGE_CURVE ( 'NONE', #219844, #64653, #119796, .T. ) ;
#64020 = DIRECTION ( 'NONE',  ( 1.000000000000000000, -0.000000000000000000, 0.000000000000000000 ) ) ;
#64021 = CARTESIAN_POINT ( 'NONE',  ( 18.50000000000000000, 85.50000000001166711, -62.92291809330219365 ) ) ;
#64023 = CARTESIAN_POINT ( 'NONE',  ( -13.88555196119803625, 9.457431528848909252, -14.99991693789966085 ) ) ;
#64022 = DIRECTION ( 'NONE',  ( 0.000000000000000000, 0.000000000000000000, 1.000000000000000000 ) ) ;
#64024 = DIRECTION ( 'NONE',  ( 0.000000000000000000, -0.7397360091702802620, 0.6728971962616779878 ) ) ;
#64025 = VERTEX_POINT ( 'NONE', #58488 ) ;
#64026 = CARTESIAN_POINT ( 'NONE',  ( -18.50000000000000000, 76.00000000001190870, -103.0231074845243029 ) ) ;
#64027 = CARTESIAN_POINT ( 'NONE',  ( -15.75000000000000355, 12.70026017068886937, -215.3766613508543628 ) ) ;
#64028 = CARTESIAN_POINT ( 'NONE',  ( 21.14999999999999503, 31.98723526783714277, -238.8784020251475511 ) ) ;
#64029 = DIRECTION ( 'NONE',  ( 0.000000000000000000, 0.1022405907414166426, 0.9947597004326453884 ) ) ;
#64030 = ORIENTED_EDGE ( 'NONE', *, *, #196, .T. ) ;
#64031 = FACE_OUTER_BOUND ( 'NONE', #53043, .T. ) ;
#64032 = AXIS2_PLACEMENT_3D ( 'NONE', #253374, #77300, #39506 ) ;
#64033 = CARTESIAN_POINT ( 'NONE',  ( -18.59999999999999787, 77.83585931145546510, -91.51866831572576189 ) ) ;
#64034 = ORIENTED_EDGE ( 'NONE', *, *, #170118, .T. ) ;
#64035 = EDGE_CURVE ( 'NONE', #148820, #135828, #118508, .T. ) ;
#64036 = DIRECTION ( 'NONE',  ( 0.000000000000000000, -1.000000000000000000, -6.352154140967427193E-15 ) ) ;
#64037 = CARTESIAN_POINT ( 'NONE',  ( 18.49999999999999645, 68.68284540823283635, -224.2482512540334767 ) ) ;
#64038 = ADVANCED_FACE ( 'NONE', ( #195488 ), #184235, .F. ) ;
#64039 = DIRECTION ( 'NONE',  ( 1.000000000000000000, 0.000000000000000000, 0.000000000000000000 ) ) ;
#64040 = DIRECTION ( 'NONE',  ( -1.000000000000000000, -0.000000000000000000, -0.000000000000000000 ) ) ;
#64041 = CARTESIAN_POINT ( 'NONE',  ( 20.27550659511089037, 9.216043722520002035, -87.85000000000003695 ) ) ;
#64042 = CARTESIAN_POINT ( 'NONE',  ( -20.64999999999999858, 0.000000000000000000, -33.50000000000000000 ) ) ;
#64043 = VERTEX_POINT ( 'NONE', #181047 ) ;
#64044 = DIRECTION ( 'NONE',  ( 1.000000000000000000, 0.000000000000000000, -0.000000000000000000 ) ) ;
#64045 = CARTESIAN_POINT ( 'NONE',  ( 20.94999999999999929, 85.40000000001231228, -160.1291383618718385 ) ) ;
#64046 = DIRECTION ( 'NONE',  ( -1.000000000000000000, 0.000000000000000000, 0.000000000000000000 ) ) ;
#64048 = DIRECTION ( 'NONE',  ( 1.000000000000000000, 0.000000000000000000, 0.000000000000000000 ) ) ;
#64047 = CARTESIAN_POINT ( 'NONE',  ( 20.12500000000000000, 14.04870287383362992, -219.6884709798077893 ) ) ;
#64049 = CARTESIAN_POINT ( 'NONE',  ( -21.05000000000000071, 77.83534155023598089, -57.86795619196132634 ) ) ;
#64050 = EDGE_CURVE ( 'NONE', #66671, #162149, #255843, .T. ) ;
#64051 = DIRECTION ( 'NONE',  ( -1.000000000000000000, -0.000000000000000000, -0.000000000000000000 ) ) ;
#64052 = DIRECTION ( 'NONE',  ( 0.000000000000000000, -0.8814952561688398358, 0.4721928772777406746 ) ) ;
#64053 = DIRECTION ( 'NONE',  ( -1.000000000000000000, 0.000000000000000000, 0.000000000000000000 ) ) ;
#64054 = AXIS2_PLACEMENT_3D ( 'NONE', #149219, #173949, #108780 ) ;
#64056 = VERTEX_POINT ( 'NONE', #23269 ) ;
#64055 = DIRECTION ( 'NONE',  ( 0.000000000000000000, 1.000000000000000000, -6.308085367188393199E-16 ) ) ;
#64057 = TOROIDAL_SURFACE ( 'NONE', #84862, 7.791421356237316687, 0.1000000000000000056 ) ;
#64058 = AXIS2_PLACEMENT_3D ( 'NONE', #24259, #82885, #7224 ) ;
#64059 = CARTESIAN_POINT ( 'NONE',  ( 23.14999999999999503, 9.104497675943859392, -211.5542940109215522 ) ) ;
#64061 = CARTESIAN_POINT ( 'NONE',  ( -18.54148534481894472, 65.67467670974366456, -30.45317318268843110 ) ) ;
#64060 = CIRCLE ( 'NONE', #5774, 11.70000000000000462 ) ;
#64062 = CARTESIAN_POINT ( 'NONE',  ( 20.94999999999999574, 1.115600667400684642E-11, -167.4999999999999716 ) ) ;
#64063 = EDGE_LOOP ( 'NONE', ( #132994, #29485, #171768, #6828 ) ) ;
#64064 = CIRCLE ( 'NONE', #151585, 0.09999999999999834022 ) ;
#64065 = DIRECTION ( 'NONE',  ( -0.000000000000000000, -6.982962677686266711E-15, 1.000000000000000000 ) ) ;
#64066 = TOROIDAL_SURFACE ( 'NONE', #139038, 0.4000000000000012990, 0.1000000000000000056 ) ;
#64067 = DIRECTION ( 'NONE',  ( 0.000000000000000000, 1.000000000000000000, 6.982962677686266711E-15 ) ) ;
#64068 = CARTESIAN_POINT ( 'NONE',  ( -18.55807992284872299, 65.67101464000501210, -97.44043916224792667 ) ) ;
#64069 = AXIS2_PLACEMENT_3D ( 'NONE', #63609, #84404, #240972 ) ;
#64070 = ADVANCED_FACE ( 'NONE', ( #201874 ), #2370, .F. ) ;
#64071 = ADVANCED_FACE ( 'NONE', ( #186168 ), #194169, .F. ) ;
#64072 = ORIENTED_EDGE ( 'NONE', *, *, #198891, .T. ) ;
#64073 = CARTESIAN_POINT ( 'NONE',  ( -23.15000000000000213, 74.00000000001254818, -183.2477294072864709 ) ) ;
#64075 = EDGE_LOOP ( 'NONE', ( #88136, #145168, #190413, #209112 ) ) ;
#64074 = CARTESIAN_POINT ( 'NONE',  ( 21.05000000000000071, 70.10000000001220144, -146.7422072491807796 ) ) ;
#64077 = CARTESIAN_POINT ( 'NONE',  ( 21.08479644141223019, 0.05855444256413740861, 6.345038657731894460 ) ) ;
#64076 = FACE_OUTER_BOUND ( 'NONE', #67548, .T. ) ;
#64078 = EDGE_CURVE ( 'NONE', #252758, #163705, #31081, .T. ) ;
#64079 = EDGE_CURVE ( 'NONE', #195497, #143163, #56145, .T. ) ;
#64080 = EDGE_LOOP ( 'NONE', ( #99267, #63957 ) ) ;
#64081 = AXIS2_PLACEMENT_3D ( 'NONE', #99896, #180763, #176932 ) ;
#64082 = DIRECTION ( 'NONE',  ( 1.000000000000000000, 0.000000000000000000, 0.000000000000000000 ) ) ;
#64084 = CARTESIAN_POINT ( 'NONE',  ( -20.54999999999999716, 87.75000000001256240, -186.7731074845242745 ) ) ;
#64083 = VECTOR ( 'NONE', #123619, 1000.000000000000000 ) ;
#64086 = CIRCLE ( 'NONE', #209846, 0.1999999999999987899 ) ;
#64085 = DIRECTION ( 'NONE',  ( -1.000000000000000000, -0.000000000000000000, -0.000000000000000000 ) ) ;
#64087 = ORIENTED_EDGE ( 'NONE', *, *, #168610, .T. ) ;
#64088 = DIRECTION ( 'NONE',  ( 0.000000000000000000, -0.9126074666063748175, -0.4088369013363328808 ) ) ;
#64089 = AXIS2_PLACEMENT_3D ( 'NONE', #227435, #48801, #128356 ) ;
#64090 = EDGE_CURVE ( 'NONE', #76307, #19374, #126903, .T. ) ;
#64091 = CARTESIAN_POINT ( 'NONE',  ( 18.58143601961952029, 54.97944794300098437, -229.9087248094723464 ) ) ;
#64093 = EDGE_CURVE ( 'NONE', #88576, #134285, #145738, .T. ) ;
#64092 = EDGE_CURVE ( 'NONE', #166820, #8831, #51863, .T. ) ;
#64094 = TOROIDAL_SURFACE ( 'NONE', #176542, 0.4000000000000015210, 0.1000000000000000056 ) ;
#64095 = DIRECTION ( 'NONE',  ( -1.000000000000000000, -0.000000000000000000, -0.000000000000000000 ) ) ;
#64096 = DIRECTION ( 'NONE',  ( 1.000000000000000000, 0.000000000000000000, 0.000000000000000000 ) ) ;
#64097 = VERTEX_POINT ( 'NONE', #183600 ) ;
#64098 = ADVANCED_FACE ( 'NONE', ( #64919 ), #189268, .T. ) ;
#64099 = ORIENTED_EDGE ( 'NONE', *, *, #226155, .T. ) ;
#64100 = AXIS2_PLACEMENT_3D ( 'NONE', #171065, #250541, #71926 ) ;
#64101 = CARTESIAN_POINT ( 'NONE',  ( 20.04142135623730070, 64.35000000001180354, -81.77310748452438816 ) ) ;
#64102 = CIRCLE ( 'NONE', #109874, 0.09999999999999892308 ) ;
#64103 = TOROIDAL_SURFACE ( 'NONE', #126462, 0.2000000000000000111, 0.1000000000000000056 ) ;
#64104 = DIRECTION ( 'NONE',  ( 1.000000000000000000, -0.000000000000000000, -0.000000000000000000 ) ) ;
#64105 = FACE_OUTER_BOUND ( 'NONE', #207927, .T. ) ;
#64106 = EDGE_CURVE ( 'NONE', #172217, #97864, #25804, .T. ) ;
#64107 = CARTESIAN_POINT ( 'NONE',  ( 21.05000000000000071, 10.68429367439815891, -141.5266739386365771 ) ) ;
#64108 = CYLINDRICAL_SURFACE ( 'NONE', #70208, 0.09999999999999939493 ) ;
#64110 = FILL_AREA_STYLE_COLOUR ( '', #32818 ) ;
#64109 = DIRECTION ( 'NONE',  ( 1.000000000000000000, -0.000000000000000000, -0.000000000000000000 ) ) ;
#64111 = DIRECTION ( 'NONE',  ( 0.000000000000000000, 0.8814952561688428334, -0.4721928772777350125 ) ) ;
#64113 = ADVANCED_FACE ( 'NONE', ( #121091 ), #165317, .T. ) ;
#64112 = CARTESIAN_POINT ( 'NONE',  ( -22.59080734064477980, 12.64999392629038155, -223.3606122593135979 ) ) ;
#64115 = EDGE_CURVE ( 'NONE', #103572, #58136, #146096, .T. ) ;
#64114 = DIRECTION ( 'NONE',  ( 0.000000000000000000, -7.086529944415894657E-15, 1.000000000000000000 ) ) ;
#64116 = CARTESIAN_POINT ( 'NONE',  ( -22.48660254037843487, 64.35000000001238618, -170.0731074845244279 ) ) ;
#64118 = ORIENTED_EDGE ( 'NONE', *, *, #47518, .F. ) ;
#64117 = CARTESIAN_POINT ( 'NONE',  ( 23.14999999999999858, 0.000000000000000000, -33.50000000000000000 ) ) ;
#64119 = DIRECTION ( 'NONE',  ( 1.000000000000000000, 0.000000000000000000, 0.000000000000000000 ) ) ;
#64121 = DIRECTION ( 'NONE',  ( 0.000000000000000000, 0.000000000000000000, -1.000000000000000000 ) ) ;
#64120 = CARTESIAN_POINT ( 'NONE',  ( 22.57320508075687115, 64.25000000001195133, -103.0231074845244024 ) ) ;
#64122 = EDGE_CURVE ( 'NONE', #223652, #82861, #33557, .T. ) ;
#64123 = VERTEX_POINT ( 'NONE', #113046 ) ;
#64125 = DIRECTION ( 'NONE',  ( 0.000000000000000000, 0.8814952561688430555, -0.4721928772777344019 ) ) ;
#64124 = DIRECTION ( 'NONE',  ( -1.000000000000000000, -0.000000000000000000, -0.000000000000000000 ) ) ;
#64126 = FACE_OUTER_BOUND ( 'NONE', #103441, .T. ) ;
#64127 = CARTESIAN_POINT ( 'NONE',  ( 21.05000000000000071, 85.50000000001179501, -79.41707660717668205 ) ) ;
#64128 = CARTESIAN_POINT ( 'NONE',  ( 23.14999999999999503, 64.35000000001218723, -143.5379132551783812 ) ) ;
#64129 = CARTESIAN_POINT ( 'NONE',  ( -13.54036565897074773, 66.54845833862705717, -185.0692319856938468 ) ) ;
#64130 = ORIENTED_EDGE ( 'NONE', *, *, #60193, .T. ) ;
#64131 = ADVANCED_FACE ( 'NONE', ( #12687 ), #51757, .T. ) ;
#64132 = ORIENTED_EDGE ( 'NONE', *, *, #165993, .F. ) ;
#64133 = CIRCLE ( 'NONE', #89052, 0.1000000000000072220 ) ;
#64134 = EDGE_CURVE ( 'NONE', #211462, #255132, #193543, .T. ) ;
#64135 = AXIS2_PLACEMENT_3D ( 'NONE', #42386, #106190, #185752 ) ;
#64136 = DIRECTION ( 'NONE',  ( -0.7071067811865562325, -0.7071067811865388020, 0.000000000000000000 ) ) ;
#64137 = ORIENTED_EDGE ( 'NONE', *, *, #196605, .T. ) ;
#64138 = CARTESIAN_POINT ( 'NONE',  ( -20.64999999999999858, 7.250000000011155521, -155.1500000000000057 ) ) ;
#64139 = AXIS2_PLACEMENT_3D ( 'NONE', #35021, #53266, #256530 ) ;
#64140 = ORIENTED_EDGE ( 'NONE', *, *, #228199, .F. ) ;
#64141 = LINE ( 'NONE', #1580, #55958 ) ;
#64142 = DIRECTION ( 'NONE',  ( 1.000000000000000000, 0.000000000000000000, 0.000000000000000000 ) ) ;
#64143 = CIRCLE ( 'NONE', #176752, 0.1999999999999981515 ) ;
#64144 = CIRCLE ( 'NONE', #80682, 0.1999999999999865219 ) ;
#64145 = CARTESIAN_POINT ( 'NONE',  ( -20.85000000106584750, 62.86809779110723184, -207.0533710558943881 ) ) ;
#64146 = EDGE_LOOP ( 'NONE', ( #173372, #243648, #166532, #5946 ) ) ;
#64147 = ADVANCED_FACE ( 'NONE', ( #88310 ), #111764, .T. ) ;
#64148 = CARTESIAN_POINT ( 'NONE',  ( -23.25000000000000000, 64.35000000001268461, -203.5231074845244166 ) ) ;
#64149 = CARTESIAN_POINT ( 'NONE',  ( 21.07928932188134397, 69.67148334361883144, -136.6220026301787414 ) ) ;
#64151 = AXIS2_PLACEMENT_3D ( 'NONE', #226573, #47943, #207036 ) ;
#64150 = DIRECTION ( 'NONE',  ( -0.000000000000000000, 0.9969158384938638928, -0.07847809223010317192 ) ) ;
#64152 = DIRECTION ( 'NONE',  ( 1.000000000000000000, -1.809991526360996944E-16, 4.908854824437060108E-17 ) ) ;
#64154 = TOROIDAL_SURFACE ( 'NONE', #218235, 12.97499999999999787, 0.1000000000000000056 ) ;
#64153 = CYLINDRICAL_SURFACE ( 'NONE', #34746, 0.09999999999999939493 ) ;
#64155 = CARTESIAN_POINT ( 'NONE',  ( 23.15000000000000213, 85.00000000001179501, -78.91707660717668205 ) ) ;
#64156 = CARTESIAN_POINT ( 'NONE',  ( 21.08832698747859169, 11.17665284714344764, -211.0812192837269379 ) ) ;
#64157 = ORIENTED_EDGE ( 'NONE', *, *, #129472, .F. ) ;
#64159 = DIRECTION ( 'NONE',  ( -0.7071067811865474617, 0.7071067811865474617, 4.937700262164531476E-15 ) ) ;
#64158 = CARTESIAN_POINT ( 'NONE',  ( 18.50000000000000000, 85.40000000001137437, -29.14106563635157698 ) ) ;
#64160 = ORIENTED_EDGE ( 'NONE', *, *, #188927, .F. ) ;
#64162 = ORIENTED_EDGE ( 'NONE', *, *, #205184, .T. ) ;
#64161 = DIRECTION ( 'NONE',  ( 0.000000000000000000, -1.000000000000000000, 0.000000000000000000 ) ) ;
#64163 = AXIS2_PLACEMENT_3D ( 'NONE', #213690, #95024, #91182 ) ;
#64164 = ORIENTED_EDGE ( 'NONE', *, *, #212986, .T. ) ;
#64165 = DIRECTION ( 'NONE',  ( -1.000000000000000000, 0.000000000000000000, 0.000000000000000000 ) ) ;
#64166 = LINE ( 'NONE', #23786, #221709 ) ;
#64167 = CARTESIAN_POINT ( 'NONE',  ( -23.25000000000000355, 65.95000000001255103, -182.7731074845244450 ) ) ;
#64168 = DIRECTION ( 'NONE',  ( 0.000000000000000000, -0.1975078988072421216, 0.9803012954743803853 ) ) ;
#64169 = ORIENTED_EDGE ( 'NONE', *, *, #174407, .T. ) ;
#64170 = CARTESIAN_POINT ( 'NONE',  ( -0.8999999999999993561, -8.250000000000005329, 26.00000000000000355 ) ) ;
#64172 = FACE_OUTER_BOUND ( 'NONE', #99683, .T. ) ;
#64171 = TOROIDAL_SURFACE ( 'NONE', #255653, 0.6000000000000009770, 0.1000000000000000056 ) ;
#64173 = ORIENTED_EDGE ( 'NONE', *, *, #195629, .T. ) ;
#64174 = CARTESIAN_POINT ( 'NONE',  ( -18.59999999999999787, 76.00000000001244871, -170.0231074845243597 ) ) ;
#64175 = CIRCLE ( 'NONE', #22677, 0.1000000000000124678 ) ;
#64176 = EDGE_CURVE ( 'NONE', #80057, #49235, #222549, .T. ) ;
#64177 = DIRECTION ( 'NONE',  ( 0.000000000000000000, -6.608470384673558123E-15, 1.000000000000000000 ) ) ;
#64178 = ORIENTED_EDGE ( 'NONE', *, *, #56379, .T. ) ;
#64179 = EDGE_CURVE ( 'NONE', #53002, #729, #1973, .T. ) ;
#64180 = DIRECTION ( 'NONE',  ( 0.000000000000000000, 0.1335171055202867274, 0.9910465087640866200 ) ) ;
#64181 = CIRCLE ( 'NONE', #205825, 0.2000000000000048683 ) ;
#64182 = CIRCLE ( 'NONE', #114239, 0.1000000000000124678 ) ;
#64183 = VERTEX_POINT ( 'NONE', #109173 ) ;
#64184 = DIRECTION ( 'NONE',  ( 0.000000000000000000, 0.05689261644170980764, -0.9983803033886519129 ) ) ;
#64185 = VERTEX_POINT ( 'NONE', #89614 ) ;
#64186 = CARTESIAN_POINT ( 'NONE',  ( 21.05000000000000071, -1.736257131586239844, -112.0686523290175245 ) ) ;
#64187 = EDGE_CURVE ( 'NONE', #206030, #41545, #53063, .T. ) ;
#64188 = EDGE_CURVE ( 'NONE', #179315, #173321, #181082, .T. ) ;
#64189 = LINE ( 'NONE', #237689, #43778 ) ;
#64191 = CARTESIAN_POINT ( 'NONE',  ( 18.39999999999999503, 64.52683809664981140, -157.3731074845244393 ) ) ;
#64190 =( REPRESENTATION_RELATIONSHIP ('NONE','NONE', #36900, #178537 ) REPRESENTATION_RELATIONSHIP_WITH_TRANSFORMATION ( #88446 )SHAPE_REPRESENTATION_RELATIONSHIP( ) );
#64192 = CYLINDRICAL_SURFACE ( 'NONE', #136856, 0.09999999999999867328 ) ;
#64193 = CIRCLE ( 'NONE', #126556, 0.09999999999998898659 ) ;
#64194 = CARTESIAN_POINT ( 'NONE',  ( 18.59999999999999432, -1.736257131586239844, -45.06865232901750318 ) ) ;
#64195 = DIRECTION ( 'NONE',  ( 0.000000000000000000, 0.9875055080513743810, -0.1575844902526802316 ) ) ;
#64196 = TOROIDAL_SURFACE ( 'NONE', #234893, 0.4000000000000010214, 0.1000000000000000056 ) ;
#64197 = AXIS2_PLACEMENT_3D ( 'NONE', #9757, #190996, #250923 ) ;
#64198 = CARTESIAN_POINT ( 'NONE',  ( 20.94999027547553894, 10.29326151435327219, -72.45928225104148623 ) ) ;
#64199 = ORIENTED_EDGE ( 'NONE', *, *, #94114, .T. ) ;
#64201 = LINE ( 'NONE', #143723, #104393 ) ;
#64200 = CARTESIAN_POINT ( 'NONE',  ( -21.05000000000000071, 69.45934304831114048, -169.9231074845244223 ) ) ;
#64202 = VERTEX_POINT ( 'NONE', #11382 ) ;
#64203 = CARTESIAN_POINT ( 'NONE',  ( -18.46907102845854709, 85.47372736477650790, -163.3470727457878411 ) ) ;
#64204 = CARTESIAN_POINT ( 'NONE',  ( 18.59999999999999432, 1.162701749949165642, -41.60000000000000142 ) ) ;
#64205 = EDGE_LOOP ( 'NONE', ( #218593, #89313, #17021, #251589 ) ) ;
#64207 = ORIENTED_EDGE ( 'NONE', *, *, #228048, .F. ) ;
#64206 = CARTESIAN_POINT ( 'NONE',  ( 20.97462148592276776, 67.12526242356098294, -57.26846315279335897 ) ) ;
#64208 = DIRECTION ( 'NONE',  ( 4.377807931758639578E-15, -0.2605042016806606298, -0.9654727137038736640 ) ) ;
#64209 = CARTESIAN_POINT ( 'NONE',  ( 21.05000000000000071, 71.14953271029291670, -182.0573748935260880 ) ) ;
#64210 = CARTESIAN_POINT ( 'NONE',  ( -18.59999999999999787, 68.97833521811203639, -132.7895420826271220 ) ) ;
#64211 = LINE ( 'NONE', #223267, #209760 ) ;
#64213 = ORIENTED_EDGE ( 'NONE', *, *, #194811, .T. ) ;
#64212 = CARTESIAN_POINT ( 'NONE',  ( -23.15000000000000213, 76.00000000001213607, -136.5231074845242745 ) ) ;
#64214 = EDGE_CURVE ( 'NONE', #31422, #31772, #90906, .T. ) ;
#64215 = DIRECTION ( 'NONE',  ( 1.000000000000000000, -0.000000000000000000, -0.000000000000000000 ) ) ;
#64216 = AXIS2_PLACEMENT_3D ( 'NONE', #87248, #230643, #148536 ) ;
#64217 = ORIENTED_EDGE ( 'NONE', *, *, #215398, .T. ) ;
#64218 = VERTEX_POINT ( 'NONE', #50471 ) ;
#64219 = CARTESIAN_POINT ( 'NONE',  ( -20.54999999999999716, 1.115600667400684642E-11, -200.9999999999999432 ) ) ;
#64220 = DIRECTION ( 'NONE',  ( -1.000000000000000000, -0.000000000000000000, -0.000000000000000000 ) ) ;
#64221 = ORIENTED_EDGE ( 'NONE', *, *, #60463, .F. ) ;
#64222 = EDGE_CURVE ( 'NONE', #2636, #239290, #43518, .T. ) ;
#64223 = DIRECTION ( 'NONE',  ( 0.000000000000000000, -1.734723475983068283E-15, 1.000000000000000000 ) ) ;
#64224 = ADVANCED_FACE ( 'NONE', ( #249991 ), #166637, .T. ) ;
#64225 = DIRECTION ( 'NONE',  ( -1.000000000000000000, 0.000000000000000000, -0.000000000000000000 ) ) ;
#64226 = ORIENTED_EDGE ( 'NONE', *, *, #120907, .F. ) ;
#64227 = CARTESIAN_POINT ( 'NONE',  ( 21.08198257630413508, 6.176001972649067362, -199.5805864394077105 ) ) ;
#64228 = CIRCLE ( 'NONE', #97510, 0.5000000000000004441 ) ;
#64229 = AXIS2_PLACEMENT_3D ( 'NONE', #14357, #93860, #155159 ) ;
#64230 = DIRECTION ( 'NONE',  ( 1.000000000000000000, 0.000000000000000000, -0.000000000000000000 ) ) ;
#64231 = AXIS2_PLACEMENT_3D ( 'NONE', #235582, #56920, #136467 ) ;
#64232 = ADVANCED_FACE ( 'NONE', ( #246142 ), #188724, .F. ) ;
#64233 = ORIENTED_EDGE ( 'NONE', *, *, #236960, .T. ) ;
#64234 = ORIENTED_EDGE ( 'NONE', *, *, #178070, .F. ) ;
#64235 = CARTESIAN_POINT ( 'NONE',  ( 23.14999999999999858, -3.999999999988843147, -167.5000000000000284 ) ) ;
#64236 = ORIENTED_EDGE ( 'NONE', *, *, #148852, .F. ) ;
#64237 = DIRECTION ( 'NONE',  ( 0.000000000000000000, 0.9770955615653315052, 0.2128009952263607008 ) ) ;
#64238 = ORIENTED_EDGE ( 'NONE', *, *, #247247, .T. ) ;
#64240 = ORIENTED_EDGE ( 'NONE', *, *, #110067, .F. ) ;
#64239 = SPHERICAL_SURFACE ( 'NONE', #243065, 0.1000000000000000056 ) ;
#64241 = EDGE_CURVE ( 'NONE', #65719, #206526, #85159, .T. ) ;
#64242 = EDGE_CURVE ( 'NONE', #193922, #157057, #68789, .T. ) ;
#64243 = CARTESIAN_POINT ( 'NONE',  ( 21.14999999999999858, 87.65000000001214175, -136.5231074845242176 ) ) ;
#64244 = ORIENTED_EDGE ( 'NONE', *, *, #99341, .T. ) ;
#64245 = CARTESIAN_POINT ( 'NONE',  ( 22.49999999999999645, 0.04562336060752910510, -88.84949566144861421 ) ) ;
#64246 = ORIENTED_EDGE ( 'NONE', *, *, #252959, .T. ) ;
#64248 = ORIENTED_EDGE ( 'NONE', *, *, #180419, .T. ) ;
#64247 = VERTEX_POINT ( 'NONE', #70095 ) ;
#64250 = DIRECTION ( 'NONE',  ( -0.7071067811865456854, 0.6909108974501254608, 0.1504730267678059674 ) ) ;
#64249 = AXIS2_PLACEMENT_3D ( 'NONE', #74497, #57438, #134400 ) ;
#64251 = EDGE_CURVE ( 'NONE', #104788, #75549, #18640, .T. ) ;
#64252 = CARTESIAN_POINT ( 'NONE',  ( -21.05000000000000071, 56.18374508921704802, -227.9290876000916057 ) ) ;
#64253 = ORIENTED_EDGE ( 'NONE', *, *, #256570, .T. ) ;
#64254 = CIRCLE ( 'NONE', #193258, 0.1000000000000028644 ) ;
#64255 = CIRCLE ( 'NONE', #214284, 0.09999999999998898659 ) ;
#64256 = AXIS2_PLACEMENT_3D ( 'NONE', #53026, #34790, #12648 ) ;
#64257 = AXIS2_PLACEMENT_3D ( 'NONE', #167109, #169688, #69274 ) ;
#64258 = ORIENTED_EDGE ( 'NONE', *, *, #15983, .F. ) ;
#64259 = CARTESIAN_POINT ( 'NONE',  ( -18.59999999999999787, 102.4393534156131977, -151.8815988770167280 ) ) ;
#64260 = EDGE_CURVE ( 'NONE', #19031, #135854, #6076, .T. ) ;
#64261 = DIRECTION ( 'NONE',  ( 4.336808689942128965E-15, 0.1022405907414274118, 0.9947597004326442782 ) ) ;
#64263 = ORIENTED_EDGE ( 'NONE', *, *, #112633, .T. ) ;
#64262 = CYLINDRICAL_SURFACE ( 'NONE', #232482, 0.09999999999999939493 ) ;
#64264 = FACE_OUTER_BOUND ( 'NONE', #29591, .T. ) ;
#64265 = VERTEX_POINT ( 'NONE', #37375 ) ;
#64266 = CARTESIAN_POINT ( 'NONE',  ( 20.85000000000000142, 79.15532900748003442, -196.2806010913881778 ) ) ;
#64267 = DIRECTION ( 'NONE',  ( 0.000000000000000000, 0.000000000000000000, -1.000000000000000000 ) ) ;
#64268 = AXIS2_PLACEMENT_3D ( 'NONE', #65631, #6943, #126901 ) ;
#64269 = ORIENTED_EDGE ( 'NONE', *, *, #162904, .F. ) ;
#64270 = AXIS2_PLACEMENT_3D ( 'NONE', #166190, #164876, #107461 ) ;
#64271 = DIRECTION ( 'NONE',  ( 1.000000000000000000, -4.851622311275599710E-17, 1.082981191754467113E-16 ) ) ;
#64272 = AXIS2_PLACEMENT_3D ( 'NONE', #41108, #236695, #99742 ) ;
#64273 = ORIENTED_EDGE ( 'NONE', *, *, #126816, .T. ) ;
#64274 = DIRECTION ( 'NONE',  ( 1.000000000000000000, 0.000000000000000000, 0.000000000000000000 ) ) ;
#64275 = ORIENTED_EDGE ( 'NONE', *, *, #136753, .T. ) ;
#64276 = CIRCLE ( 'NONE', #93301, 0.09999999999998712696 ) ;
#64279 = ORIENTED_EDGE ( 'NONE', *, *, #19117, .T. ) ;
#64278 = VERTEX_POINT ( 'NONE', #196422 ) ;
#64277 = CIRCLE ( 'NONE', #222467, 4.000000000000003553 ) ;
#64280 = ORIENTED_EDGE ( 'NONE', *, *, #27656, .F. ) ;
#64281 = CARTESIAN_POINT ( 'NONE',  ( -16.94225986326250322, 9.950000000011135270, -79.94671937560791264 ) ) ;
#64282 = VERTEX_POINT ( 'NONE', #96032 ) ;
#64283 = CARTESIAN_POINT ( 'NONE',  ( -16.91049119928362998, 66.05000000001153637, -48.64138709133355576 ) ) ;
#64284 = ORIENTED_EDGE ( 'NONE', *, *, #117240, .F. ) ;
#64285 = DIRECTION ( 'NONE',  ( -0.000000000000000000, 6.982962677686266711E-15, -1.000000000000000000 ) ) ;
#64286 = AXIS2_PLACEMENT_3D ( 'NONE', #90842, #133826, #114267 ) ;
#64287 = CIRCLE ( 'NONE', #6007, 0.1000000000000028644 ) ;
#64288 = CARTESIAN_POINT ( 'NONE',  ( 20.94999999999999574, 70.56573376625485139, -228.3808404818380779 ) ) ;
#64289 = VECTOR ( 'NONE', #180870, 1000.000000000000000 ) ;
#64290 = VERTEX_POINT ( 'NONE', #215973 ) ;
#64291 = EDGE_LOOP ( 'NONE', ( #157413, #25041, #167650, #173861 ) ) ;
#64292 = ORIENTED_EDGE ( 'NONE', *, *, #166988, .F. ) ;
#64293 = EDGE_CURVE ( 'NONE', #109178, #205457, #235056, .T. ) ;
#64294 = CARTESIAN_POINT ( 'NONE',  ( -16.90202395485847475, 66.03405545546029032, -82.12009376326403753 ) ) ;
#64295 = EDGE_LOOP ( 'NONE', ( #65272, #193046, #69437, #229636 ) ) ;
#64296 = CARTESIAN_POINT ( 'NONE',  ( -18.59999999999999787, 66.65000000001180069, -81.87310748452438247 ) ) ;
#64297 = ADVANCED_FACE ( 'NONE', ( #238109 ), #118180, .F. ) ;
#64298 = DIRECTION ( 'NONE',  ( 0.000000000000000000, -0.8700118002898321601, 0.4930308989875230030 ) ) ;
#64299 = DIRECTION ( 'NONE',  ( 1.000000000000000000, 2.952720810173289112E-16, -0.000000000000000000 ) ) ;
#64300 = DIRECTION ( 'NONE',  ( 4.377807931758638789E-15, 0.2605042016806672911, 0.9654727137038716656 ) ) ;
#64301 = CARTESIAN_POINT ( 'NONE',  ( 21.05000000000000071, 65.37127968600796635, -162.3581939154368285 ) ) ;
#64302 = DIRECTION ( 'NONE',  ( 0.000000000000000000, -0.9910465087640860649, -0.1335171055202901413 ) ) ;
#64303 = CARTESIAN_POINT ( 'NONE',  ( -18.39999999999999858, 85.50000000001263345, -196.4910380878246201 ) ) ;
#64304 = CIRCLE ( 'NONE', #147517, 11.75000000000000000 ) ;
#64305 = EDGE_CURVE ( 'NONE', #228417, #45673, #213412, .T. ) ;
#64307 = CARTESIAN_POINT ( 'NONE',  ( 21.05000000000000071, 34.11495408474048929, -243.6626398385084826 ) ) ;
#64306 = CARTESIAN_POINT ( 'NONE',  ( 13.99999999999999822, 9.850000000011137402, -50.24999999999999289 ) ) ;
#64309 = EDGE_CURVE ( 'NONE', #123636, #111449, #106022, .T. ) ;
#64308 = LINE ( 'NONE', #48587, #103335 ) ;
#64310 = AXIS2_PLACEMENT_3D ( 'NONE', #215266, #36661, #195730 ) ;
#64311 = CARTESIAN_POINT ( 'NONE',  ( 20.04142135623730070, 34.40595771266846725, -235.0146864773515176 ) ) ;
#64313 = CARTESIAN_POINT ( 'NONE',  ( -18.59999999999999787, -26.43935341558978891, -85.14150860750750383 ) ) ;
#64312 = AXIS2_PLACEMENT_3D ( 'NONE', #192462, #214577, #132487 ) ;
#64314 = VERTEX_POINT ( 'NONE', #34821 ) ;
#64315 = AXIS2_PLACEMENT_3D ( 'NONE', #71608, #208549, #151136 ) ;
#64316 = CIRCLE ( 'NONE', #210081, 0.09999999999999971412 ) ;
#64318 = ORIENTED_EDGE ( 'NONE', *, *, #85173, .T. ) ;
#64317 = CARTESIAN_POINT ( 'NONE',  ( 18.39999999999999503, 64.25000000001159606, -56.87310748452440379 ) ) ;
#64319 = VERTEX_POINT ( 'NONE', #176892 ) ;
#64320 = EDGE_CURVE ( 'NONE', #81651, #89898, #253821, .T. ) ;
#64321 = FACE_OUTER_BOUND ( 'NONE', #80357, .T. ) ;
#64322 = DIRECTION ( 'NONE',  ( 0.000000000000000000, -0.9126074666063770380, -0.4088369013363281068 ) ) ;
#64323 = VECTOR ( 'NONE', #124431, 1000.000000000000000 ) ;
#64324 = ADVANCED_FACE ( 'NONE', ( #136423 ), #60249, .T. ) ;
#64325 = LINE ( 'NONE', #5601, #186311 ) ;
#64326 = ORIENTED_EDGE ( 'NONE', *, *, #233668, .T. ) ;
#64327 = AXIS2_PLACEMENT_3D ( 'NONE', #39975, #119490, #199019 ) ;
#64328 = CIRCLE ( 'NONE', #114209, 14.30833333333333890 ) ;
#64329 = B_SPLINE_CURVE_WITH_KNOTS ( 'NONE', 3,
 ( #168283, #127835, #7897, #108271, #69158, #114356, #207377, #153531, #133905, #246483, #213444, #28776, #106963, #126544, #105665, #148689 ),
 .UNSPECIFIED., .F., .F.,
 ( 4, 3, 3, 3, 3, 4 ),
 ( 0.000000000000000000, 2.372700795693552043E-05, 5.739057815866868386E-05, 9.073899019179277486E-05, 0.0001243544287365655867, 0.0001585386695601107032 ),
 .UNSPECIFIED. ) ;
#64330 = FACE_OUTER_BOUND ( 'NONE', #7532, .T. ) ;
#64331 = CIRCLE ( 'NONE', #76793, 4.000000000000003553 ) ;
#64332 = PRODUCT_DEFINITION_SHAPE ( 'NONE', 'NONE',  #258131 ) ;
#64333 = DIRECTION ( 'NONE',  ( 0.000000000000000000, 0.2128009952264685312, -0.9770955615653078574 ) ) ;
#64334 = ORIENTED_EDGE ( 'NONE', *, *, #81753, .F. ) ;
#64335 = FACE_OUTER_BOUND ( 'NONE', #111350, .T. ) ;
#64336 = DIRECTION ( 'NONE',  ( 0.000000000000000000, -1.000000000000000000, 0.000000000000000000 ) ) ;
#64337 = DIRECTION ( 'NONE',  ( 0.000000000000000000, 0.9856811345164803173, 0.1686199900910455851 ) ) ;
#64338 = ADVANCED_FACE ( 'NONE', ( #137719 ), #77745, .T. ) ;
#64339 = EDGE_CURVE ( 'NONE', #142179, #22186, #175600, .T. ) ;
#64340 = CYLINDRICAL_SURFACE ( 'NONE', #41105, 0.1000000000000064587 ) ;
#64342 = ORIENTED_EDGE ( 'NONE', *, *, #149604, .T. ) ;
#64341 = CARTESIAN_POINT ( 'NONE',  ( -20.88420186297724257, 67.49234744263520724, -195.4268335588911611 ) ) ;
#64343 = EDGE_CURVE ( 'NONE', #120362, #197089, #55597, .T. ) ;
#64344 = AXIS2_PLACEMENT_3D ( 'NONE', #8318, #87807, #96788 ) ;
#64345 = CARTESIAN_POINT ( 'NONE',  ( 23.14999999999999858, 1.115600667400684642E-11, -100.5000000000000426 ) ) ;
#64347 = VERTEX_POINT ( 'NONE', #15243 ) ;
#64346 = LINE ( 'NONE', #201273, #118923 ) ;
#64348 = CARTESIAN_POINT ( 'NONE',  ( -22.48970261584618058, 11.65000000001115588, -167.4446305117825773 ) ) ;
#64349 = LINE ( 'NONE', #202569, #229056 ) ;
#64350 = ORIENTED_EDGE ( 'NONE', *, *, #53567, .T. ) ;
#64351 = DIRECTION ( 'NONE',  ( -1.000000000000000000, -0.000000000000000000, 0.000000000000000000 ) ) ;
#64352 = FACE_OUTER_BOUND ( 'NONE', #30165, .T. ) ;
#64353 = AXIS2_PLACEMENT_3D ( 'NONE', #227530, #167591, #28087 ) ;
#64355 = DIRECTION ( 'NONE',  ( 0.000000000000000000, -0.2617529984165028467, -0.9651348961777157509 ) ) ;
#64354 = CARTESIAN_POINT ( 'NONE',  ( -16.93234230245721861, 63.05702038518566610, -213.0496990854739749 ) ) ;
#64356 = CARTESIAN_POINT ( 'NONE',  ( -20.64999999999999858, 1.115600667400684642E-11, -100.5000000000000284 ) ) ;
#64357 = CARTESIAN_POINT ( 'NONE',  ( 18.59999999999998721, 6.933893972137497030, -137.7856458343736108 ) ) ;
#64358 = ADVANCED_FACE ( 'NONE', ( #218533 ), #135152, .T. ) ;
#64359 = CARTESIAN_POINT ( 'NONE',  ( -18.55807992284872299, 10.32898536000685574, -39.08266832227644016 ) ) ;
#64360 = DIRECTION ( 'NONE',  ( 1.000000000000000000, -0.000000000000000000, -0.000000000000000000 ) ) ;
#64361 = CARTESIAN_POINT ( 'NONE',  ( 21.14999999999999858, 12.76524917372336887, -223.4223513401831269 ) ) ;
#64362 = CIRCLE ( 'NONE', #76821, 0.4000000000000114575 ) ;
#64364 = ORIENTED_EDGE ( 'NONE', *, *, #80885, .F. ) ;
#64363 = VECTOR ( 'NONE', #6226, 1000.000000000000000 ) ;
#64365 = CARTESIAN_POINT ( 'NONE',  ( -20.64999999999999858, 85.00000000001232081, -160.1291383618718385 ) ) ;
#64366 = AXIS2_PLACEMENT_3D ( 'NONE', #70895, #128278, #112571 ) ;
#64367 = ORIENTED_EDGE ( 'NONE', *, *, #77044, .F. ) ;
#64368 = ORIENTED_EDGE ( 'NONE', *, *, #158656, .T. ) ;
#64369 = CARTESIAN_POINT ( 'NONE',  ( -20.85000000000000142, 11.74999999999999645, -26.71613433702190576 ) ) ;
#64370 = FACE_OUTER_BOUND ( 'NONE', #46262, .T. ) ;
#64371 = VERTEX_POINT ( 'NONE', #94755 ) ;
#64373 = EDGE_CURVE ( 'NONE', #4242, #34877, #10211, .T. ) ;
#64372 = ORIENTED_EDGE ( 'NONE', *, *, #85825, .F. ) ;
#64374 = ORIENTED_EDGE ( 'NONE', *, *, #12428, .T. ) ;
#64375 = DIRECTION ( 'NONE',  ( 1.000000000000000000, 0.000000000000000000, 0.000000000000000000 ) ) ;
#64376 = CIRCLE ( 'NONE', #147580, 4.049999999999998046 ) ;
#64377 = VERTEX_POINT ( 'NONE', #153508 ) ;
#64378 = CARTESIAN_POINT ( 'NONE',  ( -21.05000000000000071, 76.00000000001267608, -203.5231074845243597 ) ) ;
#64379 = CARTESIAN_POINT ( 'NONE',  ( -0.8999999999999437339, 67.75000000001118394, -5.981686128287480919 ) ) ;
#64380 = CARTESIAN_POINT ( 'NONE',  ( 20.94999999999999574, 1.148907358139439339E-11, -201.0000000000015064 ) ) ;
#64381 = DIRECTION ( 'NONE',  ( 0.000000000000000000, 0.2128009952263605897, -0.9770955615653315052 ) ) ;
#64382 = CARTESIAN_POINT ( 'NONE',  ( 22.39999999999999503, 11.75000000001115552, -134.0000000000000284 ) ) ;
#64383 = EDGE_CURVE ( 'NONE', #228818, #97848, #75229, .T. ) ;
#64384 = AXIS2_PLACEMENT_3D ( 'NONE', #76939, #95225, #114791 ) ;
#64385 = SPHERICAL_SURFACE ( 'NONE', #25149, 0.1000000000000000056 ) ;
#64386 = CARTESIAN_POINT ( 'NONE',  ( -21.44999999999999929, 29.24307565605548120, -237.2405905340223455 ) ) ;
#64388 = EDGE_LOOP ( 'NONE', ( #52944, #187766, #88600, #63196 ) ) ;
#64387 = DIRECTION ( 'NONE',  ( 0.000000000000000000, 0.8660254037844281605, -0.5000000000000185407 ) ) ;
#64390 = CARTESIAN_POINT ( 'NONE',  ( 18.59999999999999076, -1.164121893241208960, -41.41484808557160591 ) ) ;
#64389 = CARTESIAN_POINT ( 'NONE',  ( 20.95545211741311320, 65.41358668846766022, -61.93696062493610555 ) ) ;
#64391 = DIRECTION ( 'NONE',  ( -1.000000000000000000, 0.000000000000000000, -0.000000000000000000 ) ) ;
#64392 = ORIENTED_EDGE ( 'NONE', *, *, #143004, .T. ) ;
#64393 = CARTESIAN_POINT ( 'NONE',  ( -15.75000000000000355, 9.350000000011140955, -117.2500000000000284 ) ) ;
#64395 = EDGE_CURVE ( 'NONE', #116921, #7289, #156049, .T. ) ;
#64394 = CARTESIAN_POINT ( 'NONE',  ( 20.05000000000002913, 9.052352027203996343, -208.4953267290897259 ) ) ;
#64396 = ORIENTED_EDGE ( 'NONE', *, *, #14937, .T. ) ;
#64398 = DIRECTION ( 'NONE',  ( 1.000000000000000000, 0.000000000000000000, 0.000000000000000000 ) ) ;
#64397 = CARTESIAN_POINT ( 'NONE',  ( -26.01805557925458956, 8.624264858734566275, -347.0000000000001137 ) ) ;
#64399 = DIRECTION ( 'NONE',  ( 1.000000000000000000, 0.000000000000000000, 0.000000000000000000 ) ) ;
#64400 = ORIENTED_EDGE ( 'NONE', *, *, #133954, .F. ) ;
#64401 = EDGE_CURVE ( 'NONE', #239112, #180347, #177001, .T. ) ;
#64402 =( GEOMETRIC_REPRESENTATION_CONTEXT ( 3 ) GLOBAL_UNCERTAINTY_ASSIGNED_CONTEXT ( ( #156309 ) ) GLOBAL_UNIT_ASSIGNED_CONTEXT ( ( #60655, #163637, #241876 ) ) REPRESENTATION_CONTEXT ( 'NONE', 'WORKASPACE' ) );
#64403 = FILL_AREA_STYLE_COLOUR ( '', #143296 ) ;
#64405 = ADVANCED_FACE ( 'NONE', ( #180727 ), #142841, .F. ) ;
#64404 = DIRECTION ( 'NONE',  ( 0.000000000000000000, 1.000000000000000000, 1.445602896647339410E-16 ) ) ;
#64406 = CARTESIAN_POINT ( 'NONE',  ( -23.15000000000000213, 51.33926024308902925, -230.0993571250899379 ) ) ;
#64407 = DIRECTION ( 'NONE',  ( -0.000000000000000000, -0.000000000000000000, 1.000000000000000000 ) ) ;
#64408 = VERTEX_POINT ( 'NONE', #42478 ) ;
#64409 = VERTEX_POINT ( 'NONE', #5908 ) ;
#64410 = DIRECTION ( 'NONE',  ( 0.000000000000000000, -1.000000000000000000, -6.982962677686266711E-15 ) ) ;
#64411 = CARTESIAN_POINT ( 'NONE',  ( -20.00857864376270001, 52.13794731297493712, -232.3713824252124880 ) ) ;
#64412 = EDGE_CURVE ( 'NONE', #46326, #141829, #247880, .T. ) ;
#64413 = DIRECTION ( 'NONE',  ( 5.421010862427554711E-16, 1.000000000000000000, 1.023556919514279895E-14 ) ) ;
#64414 = CARTESIAN_POINT ( 'NONE',  ( -23.15000000000000213, 36.65892442174472876, -249.5511627012454596 ) ) ;
#64415 = CIRCLE ( 'NONE', #80960, 0.09999999999998898659 ) ;
#64416 = DIRECTION ( 'NONE',  ( 0.000000000000000000, -0.9910827722268042983, 0.1332476588733650935 ) ) ;
#64417 = TOROIDAL_SURFACE ( 'NONE', #22742, 7.800000000000000711, 0.1000000000000000056 ) ;
#64419 = ADVANCED_FACE ( 'NONE', ( #140281 ), #243243, .T. ) ;
#64418 = LINE ( 'NONE', #143940, #51227 ) ;
#64420 = VECTOR ( 'NONE', #81965, 1000.000000000000000 ) ;
#64421 = VECTOR ( 'NONE', #217106, 1000.000000000000000 ) ;
#64423 = VERTEX_POINT ( 'NONE', #81577 ) ;
#64422 = CARTESIAN_POINT ( 'NONE',  ( 21.14999999999999858, 8.786607556611267356, -179.7499999999999716 ) ) ;
#64424 = FACE_OUTER_BOUND ( 'NONE', #210626, .T. ) ;
#64425 = DIRECTION ( 'NONE',  ( 0.000000000000000000, 0.000000000000000000, 1.000000000000000000 ) ) ;
#64426 = CARTESIAN_POINT ( 'NONE',  ( -21.13498764882296044, 75.99834360528038246, -76.01872562799826483 ) ) ;
#64428 = CARTESIAN_POINT ( 'NONE',  ( 21.05000000000000071, 6.477067021135912483, -167.5999999999999375 ) ) ;
#64427 = COLOUR_RGB ( '', 0.31764706, 0.68627451, 0.89019608) ;
#64429 = ADVANCED_FACE ( 'NONE', ( #84123 ), #210301, .T. ) ;
#64430 = CARTESIAN_POINT ( 'NONE',  ( -23.15000000000000213, -11.48912529307605546, -30.39999999999999858 ) ) ;
#64432 = VERTEX_POINT ( 'NONE', #85424 ) ;
#64431 = DIRECTION ( 'NONE',  ( 0.7071067811865475727, 0.7071067811865475727, 0.000000000000000000 ) ) ;
#64433 = DIRECTION ( 'NONE',  ( 0.000000000000000000, 0.000000000000000000, -1.000000000000000000 ) ) ;
#64434 = CARTESIAN_POINT ( 'NONE',  ( 21.05563370358598263, 10.72423035585766549, -179.6830908159630269 ) ) ;
#64435 = DIRECTION ( 'NONE',  ( -1.000000000000000000, -0.000000000000000000, -0.000000000000000000 ) ) ;
#64436 = ORIENTED_EDGE ( 'NONE', *, *, #193512, .F. ) ;
#64437 = DIRECTION ( 'NONE',  ( 0.000000000000000000, 1.000000000000000000, 0.000000000000000000 ) ) ;
#64438 = CARTESIAN_POINT ( 'NONE',  ( -16.87333278164152972, 66.11739021543316142, -116.1562752906778542 ) ) ;
#64439 = EDGE_CURVE ( 'NONE', #109631, #79720, #243600, .T. ) ;
#64440 = CARTESIAN_POINT ( 'NONE',  ( -23.25000000000000000, -11.48912529306489994, -130.9000000000000341 ) ) ;
#64441 = EDGE_CURVE ( 'NONE', #208598, #245837, #18742, .T. ) ;
#64442 = DIRECTION ( 'NONE',  ( 1.186688945009010077E-16, 1.000000000000000000, 6.982962677686266711E-15 ) ) ;
#64443 = VECTOR ( 'NONE', #159919, 1000.000000000000000 ) ;
#64444 = ORIENTED_EDGE ( 'NONE', *, *, #1769, .T. ) ;
#64445 = DIRECTION ( 'NONE',  ( 1.000000000000000000, 0.000000000000000000, 0.000000000000000000 ) ) ;
#64446 = CIRCLE ( 'NONE', #160328, 4.049999999999998046 ) ;
#64447 = ORIENTED_EDGE ( 'NONE', *, *, #246771, .F. ) ;
#64448 = AXIS2_PLACEMENT_3D ( 'NONE', #22293, #44414, #41858 ) ;
#64449 = CARTESIAN_POINT ( 'NONE',  ( -20.64999999999999858, 68.85000000001151932, -48.37310748452436826 ) ) ;
#64450 = CARTESIAN_POINT ( 'NONE',  ( -21.14999999999999858, 33.98486250090727623, -243.5821103306120108 ) ) ;
#64451 = DIRECTION ( 'NONE',  ( 1.000000000000000000, 0.000000000000000000, 0.000000000000000000 ) ) ;
#64452 = DIRECTION ( 'NONE',  ( 1.000000000000000000, 3.403959061552269104E-14, 2.112458025737858499E-14 ) ) ;
#64453 = ORIENTED_EDGE ( 'NONE', *, *, #182785, .T. ) ;
#64454 = EDGE_CURVE ( 'NONE', #217484, #60627, #214550, .T. ) ;
#64455 = ADVANCED_FACE ( 'NONE', ( #239414 ), #82855, .F. ) ;
#64456 = AXIS2_PLACEMENT_3D ( 'NONE', #203972, #97464, #104836 ) ;
#64457 = TOROIDAL_SURFACE ( 'NONE', #10300, 0.2000000000000000111, 0.1000000000000000056 ) ;
#64458 = CARTESIAN_POINT ( 'NONE',  ( 20.94999999999999929, 1.835341550235569663, -45.05515129256298223 ) ) ;
#64459 = AXIS2_PLACEMENT_3D ( 'NONE', #147587, #73220, #31530 ) ;
#64460 = CARTESIAN_POINT ( 'NONE',  ( -23.15000000000000213, 4.150000000011156764, -112.8500000000000369 ) ) ;
#64461 = LINE ( 'NONE', #206533, #66257 ) ;
#64462 = AXIS2_PLACEMENT_3D ( 'NONE', #250547, #249285, #48495 ) ;
#64463 = CARTESIAN_POINT ( 'NONE',  ( 18.49999999999998934, 10.29288807859941457, -206.4580020160121308 ) ) ;
#64464 = VERTEX_POINT ( 'NONE', #124604 ) ;
#64466 = ORIENTED_EDGE ( 'NONE', *, *, #221477, .T. ) ;
#64465 = DIRECTION ( 'NONE',  ( -1.000000000000000000, -2.952720810173289112E-16, 0.000000000000000000 ) ) ;
#64467 = CIRCLE ( 'NONE', #81186, 0.09999999999999939493 ) ;
#64468 = ORIENTED_EDGE ( 'NONE', *, *, #200097, .T. ) ;
#64469 = DIRECTION ( 'NONE',  ( 0.000000000000000000, 0.9915357197604892647, -0.1298341882519715440 ) ) ;
#64470 = EDGE_LOOP ( 'NONE', ( #124920, #152055, #130, #50428 ) ) ;
#64471 = LINE ( 'NONE', #82702, #154945 ) ;
#64472 = AXIS2_PLACEMENT_3D ( 'NONE', #16678, #157490, #115759 ) ;
#64473 = DIRECTION ( 'NONE',  ( 0.000000000000000000, 0.000000000000000000, 1.000000000000000000 ) ) ;
#64474 = CARTESIAN_POINT ( 'NONE',  ( -20.64999999999999858, 7.150000000011155876, -45.85000000000000142 ) ) ;
#64475 = ORIENTED_EDGE ( 'NONE', *, *, #12419, .F. ) ;
#64477 = AXIS2_PLACEMENT_3D ( 'NONE', #255670, #238724, #234886 ) ;
#64476 = CARTESIAN_POINT ( 'NONE',  ( -16.85718274719441823, 66.02385768538987065, -56.95976115234177684 ) ) ;
#64478 = CARTESIAN_POINT ( 'NONE',  ( 20.85000000000000142, 6.982009704867603972, -204.6961521182562649 ) ) ;
#64479 = AXIS2_PLACEMENT_3D ( 'NONE', #4827, #60972, #84338 ) ;
#64480 = ORIENTED_EDGE ( 'NONE', *, *, #43396, .F. ) ;
#64481 = CARTESIAN_POINT ( 'NONE',  ( -14.87770893841224940, 9.430637101707896264, -152.2682606180609639 ) ) ;
#64483 = VERTEX_POINT ( 'NONE', #60749 ) ;
#64482 = PLANE ( 'NONE',  #209021 ) ;
#64484 = FACE_OUTER_BOUND ( 'NONE', #220277, .T. ) ;
#64485 = DIRECTION ( 'NONE',  ( -1.000000000000000000, -7.304098846218135653E-16, -5.100424963727256530E-30 ) ) ;
#64486 = EDGE_CURVE ( 'NONE', #239010, #105589, #152043, .T. ) ;
#64487 = VERTEX_POINT ( 'NONE', #219835 ) ;
#64488 = DIRECTION ( 'NONE',  ( -1.836970198721030181E-16, -0.9651348961777157509, 0.2617529984165031243 ) ) ;
#64489 = CARTESIAN_POINT ( 'NONE',  ( -23.15000000000000213, 71.85000000001259934, -191.1731074845243654 ) ) ;
#64490 = DIRECTION ( 'NONE',  ( 0.000000000000000000, 0.000000000000000000, 1.000000000000000000 ) ) ;
#64491 = ORIENTED_EDGE ( 'NONE', *, *, #19494, .T. ) ;
#64492 = DIRECTION ( 'NONE',  ( 0.000000000000000000, 0.000000000000000000, -1.000000000000000000 ) ) ;
#64493 = CARTESIAN_POINT ( 'NONE',  ( -23.15000000000000213, 71.65000000001151648, -48.37310748452435405 ) ) ;
#64494 = AXIS2_PLACEMENT_3D ( 'NONE', #108113, #231924, #187668 ) ;
#64495 = ORIENTED_EDGE ( 'NONE', *, *, #176486, .F. ) ;
#64496 = CIRCLE ( 'NONE', #222682, 0.5000000000000004441 ) ;
#64497 = EDGE_CURVE ( 'NONE', #163061, #183157, #131165, .T. ) ;
#64498 = ORIENTED_EDGE ( 'NONE', *, *, #120936, .F. ) ;
#64499 = CARTESIAN_POINT ( 'NONE',  ( 20.97468175916167255, 65.37473483564157561, -191.2683460491116421 ) ) ;
#64500 = CIRCLE ( 'NONE', #210260, 7.900000000000003908 ) ;
#64501 = AXIS2_PLACEMENT_3D ( 'NONE', #185276, #187863, #90013 ) ;
#64502 = ORIENTED_EDGE ( 'NONE', *, *, #138757, .F. ) ;
#64503 = DIRECTION ( 'NONE',  ( 1.000000000000000000, 0.000000000000000000, 0.000000000000000000 ) ) ;
#64504 = CARTESIAN_POINT ( 'NONE',  ( -21.44999999999999929, 7.350000000011155166, -155.1500000000000057 ) ) ;
#64506 = ORIENTED_EDGE ( 'NONE', *, *, #13262, .F. ) ;
#64505 = DIRECTION ( 'NONE',  ( 0.000000000000000000, 0.1350103645451876666, 0.9908441862701600211 ) ) ;
#64507 = CARTESIAN_POINT ( 'NONE',  ( 20.96077737575349786, 11.62390063401585394, -127.1407919571063729 ) ) ;
#64508 = CARTESIAN_POINT ( 'NONE',  ( 21.14999999999999858, 11.65000000001115943, -67.10000000000005116 ) ) ;
#64509 = CYLINDRICAL_SURFACE ( 'NONE', #56095, 0.09999999999999939493 ) ;
#64510 = CIRCLE ( 'NONE', #160397, 11.80000000000000426 ) ;
#64511 = DIRECTION ( 'NONE',  ( 0.000000000000000000, -0.8660254037844411501, -0.4999999999999956146 ) ) ;
#64512 = PLANE ( 'NONE',  #23986 ) ;
#64514 = EDGE_LOOP ( 'NONE', ( #251873, #18551, #78434, #187711, #62949 ) ) ;
#64513 = DIRECTION ( 'NONE',  ( 0.000000000000000000, -0.9209589331071360574, 0.3896596508880098009 ) ) ;
#64515 = DIRECTION ( 'NONE',  ( -2.602085213965226419E-14, -0.000000000000000000, 1.000000000000000000 ) ) ;
#64516 = AXIS2_PLACEMENT_3D ( 'NONE', #86004, #63913, #6492 ) ;
#64517 = VERTEX_POINT ( 'NONE', #102423 ) ;
#64518 = DIRECTION ( 'NONE',  ( -2.602085213965226419E-14, -6.982962677686266711E-15, 1.000000000000000000 ) ) ;
#64519 = DIRECTION ( 'NONE',  ( 0.000000000000000000, -1.000000000000000000, 0.000000000000000000 ) ) ;
#64520 = CARTESIAN_POINT ( 'NONE',  ( 21.05000000000000071, 40.68212387350988735, -238.0221676322813096 ) ) ;
#64521 = AXIS2_PLACEMENT_3D ( 'NONE', #48848, #128395, #188365 ) ;
#64522 = DIRECTION ( 'NONE',  ( 1.000000000000000000, 0.000000000000000000, 0.000000000000000000 ) ) ;
#64523 = ORIENTED_EDGE ( 'NONE', *, *, #67913, .F. ) ;
#64524 = DIRECTION ( 'NONE',  ( 0.000000000000000000, 0.8814952561688476074, -0.4721928772777262417 ) ) ;
#64525 = CARTESIAN_POINT ( 'NONE',  ( 23.24999999999999645, 13.05738666989944363, -219.4949925395660557 ) ) ;
#64526 = EDGE_CURVE ( 'NONE', #82762, #80585, #182008, .T. ) ;
#64527 = ORIENTED_EDGE ( 'NONE', *, *, #812, .T. ) ;
#64528 = AXIS2_PLACEMENT_3D ( 'NONE', #106288, #172435, #154157 ) ;
#64529 = DIRECTION ( 'NONE',  ( 0.000000000000000000, -1.000000000000000000, 0.000000000000000000 ) ) ;
#64530 = VECTOR ( 'NONE', #86239, 1000.000000000000114 ) ;
#64531 = CYLINDRICAL_SURFACE ( 'NONE', #209528, 0.1000000000000118433 ) ;
#64532 = ADVANCED_FACE ( 'NONE', ( #202840 ), #24232, .T. ) ;
#64533 = VERTEX_POINT ( 'NONE', #125861 ) ;
#64534 = CARTESIAN_POINT ( 'NONE',  ( -33.72168855820452649, 58.57934086597919077, -223.9244941873113817 ) ) ;
#64535 = ORIENTED_EDGE ( 'NONE', *, *, #110074, .F. ) ;
#64536 = CARTESIAN_POINT ( 'NONE',  ( -13.12432614554023402, 9.430764995433477793, -48.73053739475046342 ) ) ;
#64537 = VERTEX_POINT ( 'NONE', #20382 ) ;
#64538 = EDGE_CURVE ( 'NONE', #233908, #141418, #118727, .T. ) ;
#64539 = CARTESIAN_POINT ( 'NONE',  ( -23.25000000000000000, 1.115600667400684642E-11, -100.5000000000000426 ) ) ;
#64540 = CARTESIAN_POINT ( 'NONE',  ( 12.29592348164039883, 9.355806591641288250, -183.7911025315461302 ) ) ;
#64541 = VERTEX_POINT ( 'NONE', #41238 ) ;
#64542 = DIRECTION ( 'NONE',  ( -0.000000000000000000, -0.000000000000000000, -1.000000000000000000 ) ) ;
#64543 = ADVANCED_FACE ( 'NONE', ( #226221 ), #52042, .T. ) ;
#64545 = ORIENTED_EDGE ( 'NONE', *, *, #227514, .F. ) ;
#64544 = LINE ( 'NONE', #144064, #230614 ) ;
#64546 = CARTESIAN_POINT ( 'NONE',  ( 21.04105312098497649, 67.12466737696898633, -191.1946007373123564 ) ) ;
#64547 = CIRCLE ( 'NONE', #210315, 0.1000000000000000472 ) ;
#64548 = EDGE_LOOP ( 'NONE', ( #119819, #204770, #8249, #69307 ) ) ;
#64549 =( BOUNDED_SURFACE ( )  B_SPLINE_SURFACE ( 3, 2, ( 
 ( #9644, #149180, #130871 ),
 ( #10945, #89172, #248260 ),
 ( #168776, #69636, #228714 ),
 ( #205259, #106153, #170054 ) ),
 .UNSPECIFIED., .F., .F., .T. ) 
 B_SPLINE_SURFACE_WITH_KNOTS ( ( 4, 4 ),
 ( 3, 3 ),
 ( 5.727910411845712702, 5.983100554402348337 ),
 ( 0.000000000000000000, 1.000000000000000000 ),
 .UNSPECIFIED. ) 
 GEOMETRIC_REPRESENTATION_ITEM ( )  RATIONAL_B_SPLINE_SURFACE ( (
 ( 1.000000000000000000, 0.8946697475932871013, 1.000000000000000000),
 ( 1.000000000000000000, 0.9035312726220107171, 1.000000000000000000),
 ( 1.000000000000000000, 0.9104333467450814732, 1.000000000000000000),
 ( 1.000000000000000000, 0.9152888060719538421, 1.000000000000000000) ) ) 
 REPRESENTATION_ITEM ( '' )  SURFACE ( )  );
#64550 = ORIENTED_EDGE ( 'NONE', *, *, #256516, .F. ) ;
#64551 = CARTESIAN_POINT ( 'NONE',  ( -23.25000000000000000, 74.08971962617972906, -48.65447533972326966 ) ) ;
#64552 = EDGE_CURVE ( 'NONE', #114106, #226270, #114607, .T. ) ;
#64553 = CARTESIAN_POINT ( 'NONE',  ( 18.59999999999999076, 69.45000000001230944, -160.0060803140843859 ) ) ;
#64554 = CARTESIAN_POINT ( 'NONE',  ( 20.94999999999999574, 14.00000000000000178, -5.427092530382545021 ) ) ;
#64555 = DIRECTION ( 'NONE',  ( 0.000000000000000000, 7.056502275159890832E-15, -1.000000000000000000 ) ) ;
#64556 = DIRECTION ( 'NONE',  ( 0.000000000000000000, -1.000000000000000000, 0.000000000000000000 ) ) ;
#64557 = ORIENTED_EDGE ( 'NONE', *, *, #67634, .F. ) ;
#64558 = PLANE ( 'NONE',  #183394 ) ;
#64559 = CARTESIAN_POINT ( 'NONE',  ( 22.57320508075687115, 64.25000000001269029, -203.5231074845244166 ) ) ;
#64560 = DIRECTION ( 'NONE',  ( -4.408576920032448588E-17, 0.1350103645451876944, -0.9908441862701601321 ) ) ;
#64561 = DIRECTION ( 'NONE',  ( 1.000000000000000000, 0.000000000000000000, 0.000000000000000000 ) ) ;
#64562 = ORIENTED_EDGE ( 'NONE', *, *, #18937, .F. ) ;
#64563 = DIRECTION ( 'NONE',  ( 0.000000000000000000, 0.000000000000000000, -1.000000000000000000 ) ) ;
#64564 = ORIENTED_EDGE ( 'NONE', *, *, #47354, .F. ) ;
#64565 = DIRECTION ( 'NONE',  ( 0.000000000000000000, -7.304098846218139203E-15, 1.000000000000000000 ) ) ;
#64566 = VERTEX_POINT ( 'NONE', #94130 ) ;
#64567 = TOROIDAL_SURFACE ( 'NONE', #77045, 0.2000000000000000111, 0.1000000000000000056 ) ;
#64568 = VECTOR ( 'NONE', #37802, 1000.000000000000000 ) ;
#64569 = DIRECTION ( 'NONE',  ( 0.000000000000000000, 1.000000000000000000, -0.000000000000000000 ) ) ;
#64570 = DIRECTION ( 'NONE',  ( 0.000000000000000000, 0.9126074666063769270, 0.4088369013363282733 ) ) ;
#64571 = ORIENTED_EDGE ( 'NONE', *, *, #88772, .T. ) ;
#64573 = ORIENTED_EDGE ( 'NONE', *, *, #28805, .T. ) ;
#64572 = DIRECTION ( 'NONE',  ( 0.000000000000000000, 0.000000000000000000, -1.000000000000000000 ) ) ;
#64574 = DIRECTION ( 'NONE',  ( 0.000000000000000000, 7.086529944415894657E-15, -1.000000000000000000 ) ) ;
#64575 = EDGE_LOOP ( 'NONE', ( #147673, #236354, #243270, #20232 ) ) ;
#64576 = DIRECTION ( 'NONE',  ( 0.000000000000000000, 0.000000000000000000, -1.000000000000000000 ) ) ;
#64577 = DIRECTION ( 'NONE',  ( 0.000000000000000000, 0.9908441862701782288, 0.1350103645450542456 ) ) ;
#64578 = ORIENTED_EDGE ( 'NONE', *, *, #191502, .F. ) ;
#64579 = CARTESIAN_POINT ( 'NONE',  ( -33.72168855820452649, 11.47316190337362585, -42.74999999999999289 ) ) ;
#64581 = CARTESIAN_POINT ( 'NONE',  ( -20.54999999999999716, 11.46684968301824448, -245.9610388612851750 ) ) ;
#64580 = VECTOR ( 'NONE', #62024, 1000.000000000000000 ) ;
#64582 = CIRCLE ( 'NONE', #218697, 0.09999999999999693856 ) ;
#64583 = ORIENTED_EDGE ( 'NONE', *, *, #52665, .T. ) ;
#64584 = ORIENTED_EDGE ( 'NONE', *, *, #223809, .T. ) ;
#64585 = CIRCLE ( 'NONE', #210358, 0.1000000000000028644 ) ;
#64586 = VECTOR ( 'NONE', #168324, 1000.000000000000000 ) ;
#64587 = EDGE_CURVE ( 'NONE', #52328, #251948, #211522, .T. ) ;
#64588 = CARTESIAN_POINT ( 'NONE',  ( 0.000000000000000000, 1.350000000000000089, 21.90000000000000213 ) ) ;
#64589 = EDGE_CURVE ( 'NONE', #975, #98150, #210249, .T. ) ;
#64591 = ORIENTED_EDGE ( 'NONE', *, *, #25441, .T. ) ;
#64590 = DIRECTION ( 'NONE',  ( -4.391705002472929091E-16, 1.000000000000000000, 0.000000000000000000 ) ) ;
#64592 = DIRECTION ( 'NONE',  ( -1.186688945009010077E-16, -1.000000000000000000, -6.789366196018717631E-15 ) ) ;
#64593 = DIRECTION ( 'NONE',  ( 1.000000000000000000, 0.000000000000000000, 0.000000000000000000 ) ) ;
#64594 = CARTESIAN_POINT ( 'NONE',  ( -16.87036670365548474, 9.989418819312801290, -121.4795601173020856 ) ) ;
#64595 = ADVANCED_FACE ( 'NONE', ( #131976 ), #233661, .T. ) ;
#64597 = CARTESIAN_POINT ( 'NONE',  ( -23.15000000000000213, 2.000000000011154189, -154.2753780772379173 ) ) ;
#64596 = DIRECTION ( 'NONE',  ( 0.000000000000000000, -1.000000000000000000, -7.272083257015735086E-15 ) ) ;
#64599 = ADVANCED_FACE ( 'NONE', ( #127165 ), #91571, .T. ) ;
#64598 = CARTESIAN_POINT ( 'NONE',  ( -20.93975676684922504, 65.68895814178293335, -164.5026557862138645 ) ) ;
#64600 = CARTESIAN_POINT ( 'NONE',  ( 21.05000000000000071, 8.776282895303632259, -108.9880007215843989 ) ) ;
#64601 = FACE_OUTER_BOUND ( 'NONE', #75770, .T. ) ;
#64602 = CARTESIAN_POINT ( 'NONE',  ( -21.05000000000000071, -11.64999999998884483, -36.50000000000000711 ) ) ;
#64603 = VECTOR ( 'NONE', #178446, 1000.000000000000000 ) ;
#64604 = ORIENTED_EDGE ( 'NONE', *, *, #247855, .T. ) ;
#64605 = AXIS2_PLACEMENT_3D ( 'NONE', #43127, #125227, #66540 ) ;
#64606 = VECTOR ( 'NONE', #52913, 1000.000000000000000 ) ;
#64607 = ORIENTED_EDGE ( 'NONE', *, *, #23175, .F. ) ;
#64608 = DIRECTION ( 'NONE',  ( -1.000000000000000000, 0.000000000000000000, 0.000000000000000000 ) ) ;
#64609 = EDGE_CURVE ( 'NONE', #213669, #18414, #65282, .T. ) ;
#64610 = EDGE_LOOP ( 'NONE', ( #24775, #37292, #91026 ) ) ;
#64611 = EDGE_CURVE ( 'NONE', #72948, #5563, #60426, .T. ) ;
#64612 =( BOUNDED_SURFACE ( )  B_SPLINE_SURFACE ( 3, 2, ( 
 ( #199685, #62722, #21049 ),
 ( #138374, #159269, #2724 ),
 ( #238793, #180112, #257014 ),
 ( #219210, #60131, #163121 ) ),
 .UNSPECIFIED., .F., .F., .F. ) 
 B_SPLINE_SURFACE_WITH_KNOTS ( ( 4, 4 ),
 ( 3, 3 ),
 ( 5.727910411845712702, 5.983100554402349225 ),
 ( 0.000000000000000000, 1.000000000000000000 ),
 .UNSPECIFIED. ) 
 GEOMETRIC_REPRESENTATION_ITEM ( )  RATIONAL_B_SPLINE_SURFACE ( (
 ( 1.000000000000000000, 0.8946697475932142707, 1.000000000000000000),
 ( 1.000000000000000000, 0.9035312726220516844, 1.000000000000000000),
 ( 1.000000000000000000, 0.9104333467450316242, 1.000000000000000000),
 ( 1.000000000000000000, 0.9152888060719367447, 1.000000000000000000) ) ) 
 REPRESENTATION_ITEM ( '' )  SURFACE ( )  );
#64613 = CARTESIAN_POINT ( 'NONE',  ( -20.85000000000000142, 64.25000000001220712, -143.3069731475025321 ) ) ;
#64614 = CIRCLE ( 'NONE', #10478, 0.09999999999999939493 ) ;
#64615 = ADVANCED_FACE ( 'NONE', ( #14624 ), #227030, .F. ) ;
#64616 = TOROIDAL_SURFACE ( 'NONE', #10481, 11.65000000000000036, 0.1000000000000000056 ) ;
#64617 = CIRCLE ( 'NONE', #256679, 0.1000000000000028644 ) ;
#64618 = ORIENTED_EDGE ( 'NONE', *, *, #130199, .T. ) ;
#64619 = CARTESIAN_POINT ( 'NONE',  ( 20.93302460841142931, 65.68434038414380893, -130.9866880726065972 ) ) ;
#64620 = ORIENTED_EDGE ( 'NONE', *, *, #117147, .F. ) ;
#64621 = PLANE ( 'NONE',  #67312 ) ;
#64622 = ORIENTED_EDGE ( 'NONE', *, *, #169215, .F. ) ;
#64623 = ORIENTED_EDGE ( 'NONE', *, *, #10872, .F. ) ;
#64624 = EDGE_CURVE ( 'NONE', #633, #115886, #168817, .T. ) ;
#64626 = DIRECTION ( 'NONE',  ( -0.000000000000000000, 0.8814952561688430555, -0.4721928772777346239 ) ) ;
#64625 = AXIS2_PLACEMENT_3D ( 'NONE', #82511, #103367, #180368 ) ;
#64627 = DIRECTION ( 'NONE',  ( 0.000000000000000000, 0.000000000000000000, -1.000000000000000000 ) ) ;
#64629 = ORIENTED_EDGE ( 'NONE', *, *, #29689, .F. ) ;
#64628 = DIRECTION ( 'NONE',  ( 0.000000000000000000, -0.9915357197604971473, 0.1298341882519111479 ) ) ;
#64630 = AXIS2_PLACEMENT_3D ( 'NONE', #417, #255983, #21314 ) ;
#64631 = ADVANCED_FACE ( 'NONE', ( #26809 ), #95421, .F. ) ;
#64632 = EDGE_CURVE ( 'NONE', #233320, #58778, #146694, .T. ) ;
#64633 = CARTESIAN_POINT ( 'NONE',  ( 19.87657994471988232, 11.75000000001116263, -158.7657881246250611 ) ) ;
#64635 = ORIENTED_EDGE ( 'NONE', *, *, #43834, .F. ) ;
#64634 = CARTESIAN_POINT ( 'NONE',  ( -18.59999999999999787, 9.150000000011157653, -122.2500000000000284 ) ) ;
#64636 = DIRECTION ( 'NONE',  ( 1.000000000000000000, 0.000000000000000000, 0.000000000000000000 ) ) ;
#64638 = EDGE_CURVE ( 'NONE', #28434, #8217, #122996, .T. ) ;
#64637 = EDGE_LOOP ( 'NONE', ( #124445, #170817, #13273, #25373 ) ) ;
#64639 = TOROIDAL_SURFACE ( 'NONE', #27271, 0.2000000000000000111, 0.1000000000000000056 ) ;
#64640 = CIRCLE ( 'NONE', #35656, 0.1000000000000028644 ) ;
#64641 = VERTEX_POINT ( 'NONE', #60130 ) ;
#64642 = FACE_OUTER_BOUND ( 'NONE', #186737, .T. ) ;
#64643 = CARTESIAN_POINT ( 'NONE',  ( 20.05000000000002913, 7.250000000011171508, -109.7500000000000426 ) ) ;
#64644 = DIRECTION ( 'NONE',  ( -1.000000000000000000, -2.952720810173289112E-16, 0.000000000000000000 ) ) ;
#64645 = ORIENTED_EDGE ( 'NONE', *, *, #231666, .T. ) ;
#64647 = CARTESIAN_POINT ( 'NONE',  ( -16.87383368123029825, 44.13548170601895038, -235.2989316066074821 ) ) ;
#64646 = CARTESIAN_POINT ( 'NONE',  ( -21.05000000000000071, 43.48442877397276618, -245.2193771921251084 ) ) ;
#64648 = CARTESIAN_POINT ( 'NONE',  ( 23.24999999999999645, 5.000000000011153745, -54.59473398108690390 ) ) ;
#64649 = DIRECTION ( 'NONE',  ( -1.000000000000000000, 0.000000000000000000, 0.000000000000000000 ) ) ;
#64650 = DIRECTION ( 'NONE',  ( -0.7071067811865388020, 0.7071067811865561215, 0.000000000000000000 ) ) ;
#64651 = CARTESIAN_POINT ( 'NONE',  ( 23.14999999999999858, -11.74999999998883560, -55.25000000000004974 ) ) ;
#64652 = ORIENTED_EDGE ( 'NONE', *, *, #92454, .T. ) ;
#64653 = VERTEX_POINT ( 'NONE', #241368 ) ;
#64654 =( BOUNDED_CURVE ( )  B_SPLINE_CURVE ( 3, ( #117129, #36323, #196647, #140517 ),
 .UNSPECIFIED., .F., .F. ) 
 B_SPLINE_CURVE_WITH_KNOTS ( ( 4, 4 ),
 ( 4.790818349670541706E-14, 1.570796326794909881 ),
 .UNSPECIFIED. ) 
 CURVE ( )  GEOMETRIC_REPRESENTATION_ITEM ( )  RATIONAL_B_SPLINE_CURVE ( ( 1.000000000000000000, 0.8047378541243732641, 0.8047378541243732641, 1.000000000000000000 ) ) 
 REPRESENTATION_ITEM ( '' )  );
#64655 = ORIENTED_EDGE ( 'NONE', *, *, #147470, .T. ) ;
#64656 = DIRECTION ( 'NONE',  ( -3.265361837132813093E-16, -1.000000000000000000, -7.026728003956683390E-15 ) ) ;
#64658 = ORIENTED_EDGE ( 'NONE', *, *, #104113, .T. ) ;
#64657 = EDGE_CURVE ( 'NONE', #163705, #185332, #97824, .T. ) ;
#64659 = DIRECTION ( 'NONE',  ( -1.000000000000000000, 0.000000000000000000, 0.000000000000000000 ) ) ;
#64660 = VERTEX_POINT ( 'NONE', #41895 ) ;
#64661 = EDGE_CURVE ( 'NONE', #69624, #193905, #85344, .T. ) ;
#64662 = CARTESIAN_POINT ( 'NONE',  ( -22.00411653962179770, 7.253442868381131170, -100.4009618941994404 ) ) ;
#64663 = SURFACE_STYLE_USAGE ( .BOTH. , #84169 ) ;
#64664 = AXIS2_PLACEMENT_3D ( 'NONE', #80491, #160092, #239614 ) ;
#64665 = AXIS2_PLACEMENT_3D ( 'NONE', #133811, #170435, #210790 ) ;
#64667 = EDGE_CURVE ( 'NONE', #41516, #57247, #22334, .T. ) ;
#64666 = ORIENTED_EDGE ( 'NONE', *, *, #111611, .F. ) ;
#64668 = LINE ( 'NONE', #4674, #69568 ) ;
#64669 = ORIENTED_EDGE ( 'NONE', *, *, #231641, .T. ) ;
#64670 = ORIENTED_EDGE ( 'NONE', *, *, #212169, .F. ) ;
#64671 = ORIENTED_EDGE ( 'NONE', *, *, #179163, .T. ) ;
#64672 = AXIS2_PLACEMENT_3D ( 'NONE', #113627, #233585, #173660 ) ;
#64673 = DIRECTION ( 'NONE',  ( 0.000000000000000000, 0.000000000000000000, -1.000000000000000000 ) ) ;
#64674 = AXIS2_PLACEMENT_3D ( 'NONE', #190432, #170902, #33953 ) ;
#64675 = PLANE ( 'NONE',  #13548 ) ;
#64676 = CARTESIAN_POINT ( 'NONE',  ( -16.87683809663752399, 60.93935776605891164, -221.0417277355860790 ) ) ;
#64677 = FACE_OUTER_BOUND ( 'NONE', #125934, .T. ) ;
#64678 = FACE_OUTER_BOUND ( 'NONE', #206074, .T. ) ;
#64680 = LINE ( 'NONE', #123383, #166023 ) ;
#64679 = CARTESIAN_POINT ( 'NONE',  ( 21.00000000000000000, 66.25000000001253397, -182.3731074845244393 ) ) ;
#64681 = CARTESIAN_POINT ( 'NONE',  ( -21.05000000000000071, 11.75000000001115552, -160.4851942293460638 ) ) ;
#64683 = VERTEX_POINT ( 'NONE', #101808 ) ;
#64682 = DIRECTION ( 'NONE',  ( 0.000000000000000000, 1.000000000000000000, 6.982962677686266711E-15 ) ) ;
#64685 = CARTESIAN_POINT ( 'NONE',  ( -16.94275863009466576, 12.44375159665070463, -211.1937418259165611 ) ) ;
#64684 = DIRECTION ( 'NONE',  ( -1.000000000000000000, -0.000000000000000000, -0.000000000000000000 ) ) ;
#64686 = CARTESIAN_POINT ( 'NONE',  ( -16.27683809663750480, 66.65000000001225544, -149.0731074845244279 ) ) ;
#64687 = VECTOR ( 'NONE', #115284, 1000.000000000000000 ) ;
#64688 = ORIENTED_EDGE ( 'NONE', *, *, #229748, .T. ) ;
#64689 = CYLINDRICAL_SURFACE ( 'NONE', #96446, 0.09999999999999939493 ) ;
#64690 = AXIS2_PLACEMENT_3D ( 'NONE', #7591, #87113, #89677 ) ;
#64691 = FACE_OUTER_BOUND ( 'NONE', #53501, .T. ) ;
#64693 = EDGE_CURVE ( 'NONE', #94408, #230665, #39630, .T. ) ;
#64692 = DIRECTION ( 'NONE',  ( -1.000000000000000000, 0.000000000000000000, 0.000000000000000000 ) ) ;
#64694 = ORIENTED_EDGE ( 'NONE', *, *, #253975, .F. ) ;
#64695 = AXIS2_PLACEMENT_3D ( 'NONE', #207130, #225378, #182437 ) ;
#64696 = CARTESIAN_POINT ( 'NONE',  ( -21.05000000000000071, 46.59314322379660922, -243.1831726892433210 ) ) ;
#64697 = EDGE_CURVE ( 'NONE', #217763, #222344, #185344, .T. ) ;
#64698 = CARTESIAN_POINT ( 'NONE',  ( -21.29999999999995808, 1.115600667400684642E-11, -37.54999999999999716 ) ) ;
#64699 = CARTESIAN_POINT ( 'NONE',  ( -20.94999999999999929, 2.953700692300310848, -208.6327728934509764 ) ) ;
#64700 = ORIENTED_EDGE ( 'NONE', *, *, #84104, .T. ) ;
#64701 = ORIENTED_EDGE ( 'NONE', *, *, #180233, .F. ) ;
#64702 = EDGE_CURVE ( 'NONE', #173853, #186763, #2723, .T. ) ;
#64704 = EDGE_CURVE ( 'NONE', #206150, #85588, #72947, .T. ) ;
#64703 = CARTESIAN_POINT ( 'NONE',  ( -16.94107738177415712, 10.01423928513661821, -12.55000000000000249 ) ) ;
#64705 = ORIENTED_EDGE ( 'NONE', *, *, #192497, .F. ) ;
#64706 = CARTESIAN_POINT ( 'NONE',  ( 23.15000000000000213, -4.756823075239756449, -233.1486023682345490 ) ) ;
#64707 = AXIS2_PLACEMENT_3D ( 'NONE', #132913, #230731, #212453 ) ;
#64708 = CARTESIAN_POINT ( 'NONE',  ( 20.94999999999999929, 76.00000000001244871, -170.0231074845243597 ) ) ;
#64709 = CARTESIAN_POINT ( 'NONE',  ( -22.39999999999999858, 1.115600667400684642E-11, -134.0000000000000000 ) ) ;
#64710 = VERTEX_POINT ( 'NONE', #236210 ) ;
#64711 = ADVANCED_FACE ( 'NONE', ( #180111 ), #1445, .F. ) ;
#64712 = CARTESIAN_POINT ( 'NONE',  ( -12.30589683808040213, 9.356746017089404788, -117.7033597213642082 ) ) ;
#64713 = DIRECTION ( 'NONE',  ( 0.000000000000000000, 6.982962677686266711E-15, -1.000000000000000000 ) ) ;
#64714 = CARTESIAN_POINT ( 'NONE',  ( 18.50000000000000711, 10.28015861706802880, -192.2245720712021182 ) ) ;
#64715 = CARTESIAN_POINT ( 'NONE',  ( -20.94999999999999929, 10.29270135740183179, -38.95736188715193293 ) ) ;
#64716 = ADVANCED_FACE ( 'NONE', ( #237510 ), #2159, .F. ) ;
#64717 = EDGE_LOOP ( 'NONE', ( #31854, #183373, #44037, #230576 ) ) ;
#64718 = AXIS2_PLACEMENT_3D ( 'NONE', #205253, #46188, #203979 ) ;
#64719 = ADVANCED_FACE ( 'NONE', ( #18453 ), #256013, .T. ) ;
#64721 = EDGE_LOOP ( 'NONE', ( #23034, #234999, #175961 ) ) ;
#64720 = CARTESIAN_POINT ( 'NONE',  ( -1.739115166359751801E-14, 61.57587952878036930, -212.2000740415318774 ) ) ;
#64722 = CARTESIAN_POINT ( 'NONE',  ( -18.59999999999999787, 7.021664781911246322, -70.83356540189728889 ) ) ;
#64723 = DIRECTION ( 'NONE',  ( 0.000000000000000000, 0.000000000000000000, 1.000000000000000000 ) ) ;
#64724 = ADVANCED_FACE ( 'NONE', ( #82241 ), #158010, .T. ) ;
#64725 = CARTESIAN_POINT ( 'NONE',  ( -16.86445178670638256, 9.962211629127160961, -87.89077743811738230 ) ) ;
#64726 = PLANE ( 'NONE',  #246356 ) ;
#64727 = LINE ( 'NONE', #182118, #225898 ) ;
#64728 = DIRECTION ( 'NONE',  ( 1.000000000000000000, -1.836970198721029934E-16, -1.282749433769087582E-30 ) ) ;
#64729 = EDGE_LOOP ( 'NONE', ( #222271, #253177, #221076, #122235 ) ) ;
#64730 = DIRECTION ( 'NONE',  ( 0.000000000000000000, 0.000000000000000000, 1.000000000000000000 ) ) ;
#64731 = DIRECTION ( 'NONE',  ( -1.000000000000000000, -0.000000000000000000, -0.000000000000000000 ) ) ;
#64732 = DIRECTION ( 'NONE',  ( -1.000000000000000000, -0.000000000000000000, -0.000000000000000000 ) ) ;
#64733 = ADVANCED_FACE ( 'NONE', ( #118855 ), #140985, .F. ) ;
#64734 = AXIS2_PLACEMENT_3D ( 'NONE', #24256, #8526, #161186 ) ;
#64735 = DIRECTION ( 'NONE',  ( 1.000000000000000000, 0.000000000000000000, 0.000000000000000000 ) ) ;
#64736 = CARTESIAN_POINT ( 'NONE',  ( 18.59999999999999076, 65.50857864377418593, -44.67310748452439384 ) ) ;
#64737 = ORIENTED_EDGE ( 'NONE', *, *, #132833, .T. ) ;
#64738 = ORIENTED_EDGE ( 'NONE', *, *, #137773, .F. ) ;
#64739 = CARTESIAN_POINT ( 'NONE',  ( 18.59999999999999076, 69.35000000001180354, -81.67310748452436542 ) ) ;
#64740 = CARTESIAN_POINT ( 'NONE',  ( -23.25000000000000000, 5.950000000000007283, -23.19429769496518645 ) ) ;
#64741 = EDGE_CURVE ( 'NONE', #87344, #157707, #160620, .T. ) ;
#64743 = CARTESIAN_POINT ( 'NONE',  ( 20.27550659511089037, 66.78395627750374786, -190.8731074845244393 ) ) ;
#64742 = VECTOR ( 'NONE', #201715, 1000.000000000000000 ) ;
#64744 = CARTESIAN_POINT ( 'NONE',  ( -16.97683809663753252, 23.52593859471641125, -231.2285429799402721 ) ) ;
#64746 = EDGE_CURVE ( 'NONE', #201487, #23181, #220517, .T. ) ;
#64745 = LINE ( 'NONE', #103854, #205790 ) ;
#64747 = ADVANCED_FACE ( 'NONE', ( #116286 ), #14444, .T. ) ;
#64748 = CARTESIAN_POINT ( 'NONE',  ( -20.94999999999999929, 62.99095723518624368, -207.1734234082435080 ) ) ;
#64749 = DIRECTION ( 'NONE',  ( 1.000000000000000000, 2.952720810173289112E-16, -0.000000000000000000 ) ) ;
#64750 = CARTESIAN_POINT ( 'NONE',  ( -20.94999999999999929, 17.06838326776700399, -224.6250846885016870 ) ) ;
#64751 = AXIS2_PLACEMENT_3D ( 'NONE', #132264, #211817, #13612 ) ;
#64752 = AXIS2_PLACEMENT_3D ( 'NONE', #82003, #3793, #142006 ) ;
#64753 = ORIENTED_EDGE ( 'NONE', *, *, #230354, .T. ) ;
#64754 = CARTESIAN_POINT ( 'NONE',  ( 18.59999999999999076, 8.531609279343539853, -209.3937462695851366 ) ) ;
#64755 = VERTEX_POINT ( 'NONE', #243910 ) ;
#64756 = ADVANCED_FACE ( 'NONE', ( #88670 ), #225610, .T. ) ;
#64757 = CARTESIAN_POINT ( 'NONE',  ( -21.05000000000000071, 76.08579911628613957, -75.93708636601274975 ) ) ;
#64758 = DIRECTION ( 'NONE',  ( 0.000000000000000000, -0.8660254037844384856, 0.5000000000000003331 ) ) ;
#64759 = DIRECTION ( 'NONE',  ( 1.000000000000000000, 0.000000000000000000, 0.000000000000000000 ) ) ;
#64760 = DIRECTION ( 'NONE',  ( -1.000000000000000000, 0.000000000000000000, 0.000000000000000000 ) ) ;
#64761 = FACE_OUTER_BOUND ( 'NONE', #93650, .T. ) ;
#64762 = DIRECTION ( 'NONE',  ( 1.186688945009010077E-16, 1.000000000000000000, 6.982962677686266711E-15 ) ) ;
#64763 = DIRECTION ( 'NONE',  ( 0.000000000000000000, 0.008583690987124399305, -0.9999631594459055250 ) ) ;
#64764 = FACE_OUTER_BOUND ( 'NONE', #47827, .T. ) ;
#64765 = CYLINDRICAL_SURFACE ( 'NONE', #220582, 0.09999999999999939493 ) ;
#64766 = LINE ( 'NONE', #21810, #146454 ) ;
#64767 = CARTESIAN_POINT ( 'NONE',  ( 20.94999999999999929, 87.65000000001214175, -136.5231074845242745 ) ) ;
#64768 = CARTESIAN_POINT ( 'NONE',  ( 20.04999999999999716, 41.52322060116084401, -237.7841060310786077 ) ) ;
#64769 = CIRCLE ( 'NONE', #181324, 0.09999999999999939493 ) ;
#64770 = VECTOR ( 'NONE', #47815, 1000.000000000000000 ) ;
#64771 = DIRECTION ( 'NONE',  ( 0.000000000000000000, 0.000000000000000000, -1.000000000000000000 ) ) ;
#64773 = CARTESIAN_POINT ( 'NONE',  ( 21.05000000000000071, 63.58084468663284383, -237.4904741118237723 ) ) ;
#64772 = CIRCLE ( 'NONE', #106440, 0.5000000000000004441 ) ;
#64774 = AXIS2_PLACEMENT_3D ( 'NONE', #207325, #169508, #112071 ) ;
#64775 = ORIENTED_EDGE ( 'NONE', *, *, #19986, .T. ) ;
#64776 = DIRECTION ( 'NONE',  ( 0.000000000000000000, 0.000000000000000000, -1.000000000000000000 ) ) ;
#64777 = SPHERICAL_SURFACE ( 'NONE', #116864, 0.1000000000000000056 ) ;
#64778 = ADVANCED_FACE ( 'NONE', ( #186527 ), #105667, .F. ) ;
#64779 = ORIENTED_EDGE ( 'NONE', *, *, #146392, .T. ) ;
#64780 = DIRECTION ( 'NONE',  ( 1.000000000000000000, 0.000000000000000000, 0.000000000000000000 ) ) ;
#64781 = CARTESIAN_POINT ( 'NONE',  ( 20.94999999999999929, 1.115650877919449413E-11, -62.90000000000001279 ) ) ;
#64782 = CARTESIAN_POINT ( 'NONE',  ( 18.59999999999999432, -1.162701749926855266, -41.60000000000000142 ) ) ;
#64783 = EDGE_LOOP ( 'NONE', ( #199579, #150837, #47948, #205653 ) ) ;
#64784 = CARTESIAN_POINT ( 'NONE',  ( 18.39999999999999858, -9.499999999988844479, -174.1001893912220737 ) ) ;
#64785 = CARTESIAN_POINT ( 'NONE',  ( 22.48660254037844552, 31.85034414784619727, -238.9397275603479898 ) ) ;
#64786 = ADVANCED_FACE ( 'NONE', ( #182682 ), #177182, .F. ) ;
#64787 = ORIENTED_EDGE ( 'NONE', *, *, #201848, .T. ) ;
#64788 = AXIS2_PLACEMENT_3D ( 'NONE', #15193, #12635, #33505 ) ;
#64789 = CIRCLE ( 'NONE', #139804, 0.1000000000000028644 ) ;
#64790 = AXIS2_PLACEMENT_3D ( 'NONE', #170734, #9037, #188961 ) ;
#64791 = DIRECTION ( 'NONE',  ( 1.000000000000000000, 0.000000000000000000, 0.000000000000000000 ) ) ;
#64792 = VERTEX_POINT ( 'NONE', #123988 ) ;
#64793 = VECTOR ( 'NONE', #94285, 1000.000000000000000 ) ;
#64794 = CYLINDRICAL_SURFACE ( 'NONE', #229251, 0.09999999999998898659 ) ;
#64795 = CYLINDRICAL_SURFACE ( 'NONE', #70906, 0.09999999999999939493 ) ;
#64796 = CARTESIAN_POINT ( 'NONE',  ( 21.05000000000000071, 11.60000000001116227, -60.07179676972450011 ) ) ;
#64798 = VECTOR ( 'NONE', #199544, 1000.000000000000000 ) ;
#64797 = CARTESIAN_POINT ( 'NONE',  ( 21.07928932188134397, 33.98134083355422774, -243.8161431329846778 ) ) ;
#64800 = DIRECTION ( 'NONE',  ( 1.000000000000000000, -0.000000000000000000, -0.000000000000000000 ) ) ;
#64799 = CIRCLE ( 'NONE', #114893, 0.1999999999999945155 ) ;
#64801 = AXIS2_PLACEMENT_3D ( 'NONE', #83799, #82526, #42166 ) ;
#64802 = CARTESIAN_POINT ( 'NONE',  ( -16.87683809663752399, 66.15000000001232650, -156.6207434663279230 ) ) ;
#64803 = CYLINDRICAL_SURFACE ( 'NONE', #29421, 0.09999999999999609201 ) ;
#64804 = LINE ( 'NONE', #144317, #151146 ) ;
#64805 = CARTESIAN_POINT ( 'NONE',  ( 18.49999999999999645, -1.135018845899022466, -74.71697688343232358 ) ) ;
#64807 = VERTEX_POINT ( 'NONE', #48286 ) ;
#64806 = CARTESIAN_POINT ( 'NONE',  ( -20.94999999999999929, -1.835341550213255957, -179.0551512925629538 ) ) ;
#64808 = ORIENTED_EDGE ( 'NONE', *, *, #9901, .F. ) ;
#64810 = DIRECTION ( 'NONE',  ( -1.000000000000000000, 0.000000000000000000, -0.000000000000000000 ) ) ;
#64809 = CARTESIAN_POINT ( 'NONE',  ( -21.14999999999999858, 30.99601144558850763, -252.1976540812581504 ) ) ;
#64812 = ORIENTED_EDGE ( 'NONE', *, *, #72680, .T. ) ;
#64811 = DIRECTION ( 'NONE',  ( 1.000000000000000000, -1.207181226542539700E-16, 2.694675058168174199E-16 ) ) ;
#64813 = ORIENTED_EDGE ( 'NONE', *, *, #220569, .F. ) ;
#64814 = DIRECTION ( 'NONE',  ( 7.589415207398576792E-15, -1.000000000000000000, -0.000000000000000000 ) ) ;
#64815 = CYLINDRICAL_SURFACE ( 'NONE', #121964, 0.09999999999999939493 ) ;
#64816 = CIRCLE ( 'NONE', #10668, 4.000000000000003553 ) ;
#64817 = DIRECTION ( 'NONE',  ( -1.000000000000000000, -0.000000000000000000, -0.000000000000000000 ) ) ;
#64818 = CARTESIAN_POINT ( 'NONE',  ( -21.05000000000000071, 77.83534155023646406, -124.9679561919613064 ) ) ;
#64819 = VECTOR ( 'NONE', #191806, 1000.000000000000000 ) ;
#64820 = CARTESIAN_POINT ( 'NONE',  ( -20.85000000000000142, 11.75000000001115197, -194.2161343370218560 ) ) ;
#64821 = TOROIDAL_SURFACE ( 'NONE', #173217, 4.099999999999999645, 0.1000000000000000056 ) ;
#64822 = DIRECTION ( 'NONE',  ( -1.000000000000000000, -0.000000000000000000, -0.000000000000000000 ) ) ;
#64823 = ADVANCED_FACE ( 'NONE', ( #87401 ), #203515, .T. ) ;
#64824 = CARTESIAN_POINT ( 'NONE',  ( 21.05000000000005400, 74.83745509109094485, -43.82310748452479743 ) ) ;
#64825 = ORIENTED_EDGE ( 'NONE', *, *, #85710, .F. ) ;
#64826 = VERTEX_POINT ( 'NONE', #28778 ) ;
#64827 = LINE ( 'NONE', #122250, #2217 ) ;
#64828 = VERTEX_POINT ( 'NONE', #86095 ) ;
#64829 = ORIENTED_EDGE ( 'NONE', *, *, #21145, .T. ) ;
#64830 = DIRECTION ( 'NONE',  ( 1.000000000000000000, 0.000000000000000000, 0.000000000000000000 ) ) ;
#64831 = LINE ( 'NONE', #186079, #171983 ) ;
#64832 = EDGE_CURVE ( 'NONE', #224952, #186279, #108274, .T. ) ;
#64833 = DIRECTION ( 'NONE',  ( 0.000000000000000000, 0.000000000000000000, -1.000000000000000000 ) ) ;
#64834 = CARTESIAN_POINT ( 'NONE',  ( -21.08621493067320429, 75.94380516053668373, -209.8724017756962894 ) ) ;
#64835 = EDGE_LOOP ( 'NONE', ( #198029, #32603, #181917, #101093 ) ) ;
#64836 = DIRECTION ( 'NONE',  ( 0.000000000000000000, -1.000000000000000000, 0.000000000000000000 ) ) ;
#64837 = ORIENTED_EDGE ( 'NONE', *, *, #173074, .T. ) ;
#64838 = ADVANCED_FACE ( 'NONE', ( #221758 ), #187822, .T. ) ;
#64839 = AXIS2_PLACEMENT_3D ( 'NONE', #256900, #80861, #78297 ) ;
#64840 = CARTESIAN_POINT ( 'NONE',  ( -16.81744102076748959, 66.05000000001153637, -48.67310748452439384 ) ) ;
#64841 = CARTESIAN_POINT ( 'NONE',  ( -20.64999999999999858, 26.13474583767463244, -241.1910018098189141 ) ) ;
#64842 = CIRCLE ( 'NONE', #210600, 0.1000000000000054040 ) ;
#64843 = DIRECTION ( 'NONE',  ( -1.000000000000000000, -0.000000000000000000, -0.000000000000000000 ) ) ;
#64844 = DIRECTION ( 'NONE',  ( 0.000000000000000000, 0.000000000000000000, 1.000000000000000000 ) ) ;
#64845 = AXIS2_PLACEMENT_3D ( 'NONE', #242197, #2288, #180956 ) ;
#64846 = ORIENTED_EDGE ( 'NONE', *, *, #233901, .F. ) ;
#64847 = EDGE_CURVE ( 'NONE', #205114, #211183, #45718, .T. ) ;
#64848 = ORIENTED_EDGE ( 'NONE', *, *, #139422, .F. ) ;
#64851 = ORIENTED_EDGE ( 'NONE', *, *, #68702, .F. ) ;
#64850 = CARTESIAN_POINT ( 'NONE',  ( 21.05000000000000426, 6.258817194692632313, -66.96636726466641676 ) ) ;
#64849 = CARTESIAN_POINT ( 'NONE',  ( -18.59999999999999787, 18.37021030142088662, -237.6367305148568221 ) ) ;
#64852 = FACE_OUTER_BOUND ( 'NONE', #168583, .T. ) ;
#64853 = ORIENTED_EDGE ( 'NONE', *, *, #13518, .T. ) ;
#64854 = AXIS2_PLACEMENT_3D ( 'NONE', #31261, #149903, #173348 ) ;
#64855 = EDGE_CURVE ( 'NONE', #13565, #232528, #23236, .T. ) ;
#64856 = DIRECTION ( 'NONE',  ( 0.000000000000000000, -0.4721928772777346239, -0.8814952561688430555 ) ) ;
#64857 = EDGE_LOOP ( 'NONE', ( #68025, #235432, #247002, #82719, #8559, #7552, #144755, #15048, #245534, #222717, #202398 ) ) ;
#64858 = CARTESIAN_POINT ( 'NONE',  ( 20.94999999999999929, 67.23127455305835554, -235.8551265064784559 ) ) ;
#64859 = CARTESIAN_POINT ( 'NONE',  ( -20.85000000000000142, -1.835859311443637010, -45.00443916879852679 ) ) ;
#64860 = EDGE_CURVE ( 'NONE', #69117, #177551, #185525, .T. ) ;
#64861 = CARTESIAN_POINT ( 'NONE',  ( 21.05000000000000071, -4.871452838297987142, -233.3782557782877518 ) ) ;
#64862 = AXIS2_PLACEMENT_3D ( 'NONE', #230805, #229509, #50833 ) ;
#64863 = DIRECTION ( 'NONE',  ( 1.000000000000000000, -1.836970198721029934E-16, -1.601412966608202925E-30 ) ) ;
#64864 = VECTOR ( 'NONE', #234330, 1000.000000000000000 ) ;
#64865 = CARTESIAN_POINT ( 'NONE',  ( -23.15000000000000213, 4.768403829798271154, -213.4961173936592331 ) ) ;
#64866 = EDGE_CURVE ( 'NONE', #159714, #161165, #202289, .T. ) ;
#64867 = CIRCLE ( 'NONE', #139877, 7.800000000000002487 ) ;
#64868 = ORIENTED_EDGE ( 'NONE', *, *, #179542, .F. ) ;
#64869 = FACE_OUTER_BOUND ( 'NONE', #226495, .T. ) ;
#64870 = CARTESIAN_POINT ( 'NONE',  ( 21.05000000000000071, 70.60000000001222986, -148.9283735034374843 ) ) ;
#64871 = CARTESIAN_POINT ( 'NONE',  ( -18.50000000000000000, -9.480686695267820596, -140.9411151687578752 ) ) ;
#64872 = ORIENTED_EDGE ( 'NONE', *, *, #8795, .T. ) ;
#64873 = DIRECTION ( 'NONE',  ( 2.952720810173289112E-16, -1.000000000000000000, 0.000000000000000000 ) ) ;
#64874 = ORIENTED_EDGE ( 'NONE', *, *, #126659, .F. ) ;
#64875 = CARTESIAN_POINT ( 'NONE',  ( -16.97683809663752186, 9.850000000011140955, -146.6500000000000341 ) ) ;
#64876 = CYLINDRICAL_SURFACE ( 'NONE', #72357, 0.09999999999998898659 ) ;
#64877 = DIRECTION ( 'NONE',  ( 0.000000000000000000, 0.2128009952263601456, -0.9770955615653315052 ) ) ;
#64878 = AXIS2_PLACEMENT_3D ( 'NONE', #56528, #203459, #137366 ) ;
#64880 = ORIENTED_EDGE ( 'NONE', *, *, #93268, .T. ) ;
#64879 = CARTESIAN_POINT ( 'NONE',  ( 0.9000000000000547562, 64.35000000001120668, -7.423107484524793520 ) ) ;
#64881 = DIRECTION ( 'NONE',  ( 0.000000000000000000, -0.2128009952263506810, 0.9770955615653337256 ) ) ;
#64882 = EDGE_CURVE ( 'NONE', #145935, #143032, #43877, .T. ) ;
#64883 = DIRECTION ( 'NONE',  ( -0.000000000000000000, -1.000000000000000000, -0.000000000000000000 ) ) ;
#64884 = CARTESIAN_POINT ( 'NONE',  ( -18.50000000000000000, 66.46020053479900014, -223.7494053730254961 ) ) ;
#64885 = ORIENTED_EDGE ( 'NONE', *, *, #64552, .F. ) ;
#64886 = CARTESIAN_POINT ( 'NONE',  ( -23.15000000000000213, 73.40000000001157332, -56.29848556176223440 ) ) ;
#64887 = EDGE_LOOP ( 'NONE', ( #122990, #189531, #152278, #1353 ) ) ;
#64888 = CARTESIAN_POINT ( 'NONE',  ( -16.93909480342659890, 9.993078364812696179, -146.6003470166723446 ) ) ;
#64889 = VECTOR ( 'NONE', #179519, 999.9999999999998863 ) ;
#64890 = AXIS2_PLACEMENT_3D ( 'NONE', #7571, #224036, #246186 ) ;
#64891 = AXIS2_PLACEMENT_3D ( 'NONE', #253382, #74791, #175184 ) ;
#64892 = CIRCLE ( 'NONE', #144172, 4.149999999999987033 ) ;
#64893 = VERTEX_POINT ( 'NONE', #192944 ) ;
#64894 = EDGE_CURVE ( 'NONE', #215740, #44321, #53424, .T. ) ;
#64895 = CARTESIAN_POINT ( 'NONE',  ( -20.54999999999999716, 7.150000000011155876, -112.7500000000000284 ) ) ;
#64897 = VERTEX_POINT ( 'NONE', #190390 ) ;
#64896 = DIRECTION ( 'NONE',  ( 0.000000000000000000, -1.000000000000000000, -6.982962677686266711E-15 ) ) ;
#64900 = EDGE_LOOP ( 'NONE', ( #161729, #4916, #220987, #70113, #206968 ) ) ;
#64899 = VERTEX_POINT ( 'NONE', #173429 ) ;
#64898 = DIRECTION ( 'NONE',  ( 0.000000000000000000, -1.000000000000000000, 0.000000000000000000 ) ) ;
#64901 = CARTESIAN_POINT ( 'NONE',  ( -18.59999999999999787, 30.18746141061095045, -235.4776000216846796 ) ) ;
#64902 = CYLINDRICAL_SURFACE ( 'NONE', #160782, 0.1000000000000124678 ) ;
#64904 = CARTESIAN_POINT ( 'NONE',  ( -20.54999999999999716, 71.65000000001187175, -90.67310748452433700 ) ) ;
#64903 = DIRECTION ( 'NONE',  ( 0.000000000000000000, 0.000000000000000000, 1.000000000000000000 ) ) ;
#64906 = EDGE_CURVE ( 'NONE', #90674, #61206, #131352, .T. ) ;
#64905 = LINE ( 'NONE', #188710, #52912 ) ;
#64907 = VECTOR ( 'NONE', #203840, 1000.000000000000000 ) ;
#64908 = CARTESIAN_POINT ( 'NONE',  ( -17.29838795458362100, 65.62845014206548910, -58.12784876713939752 ) ) ;
#64909 = EDGE_CURVE ( 'NONE', #201244, #246634, #189529, .T. ) ;
#64910 = FACE_OUTER_BOUND ( 'NONE', #58140, .T. ) ;
#64911 = CARTESIAN_POINT ( 'NONE',  ( 21.05000000000000071, 69.09936979046463534, -247.6075824278584889 ) ) ;
#64912 = EDGE_LOOP ( 'NONE', ( #245071, #192436, #243158, #56576, #76477, #245666, #22000, #181574, #142477, #57367, #189746, #139523, #132902, #28407, #66140, #155966 ) ) ;
#64913 = EDGE_LOOP ( 'NONE', ( #240799, #229649, #129967, #117821 ) ) ;
#64914 = CARTESIAN_POINT ( 'NONE',  ( -18.40000000000000213, 64.66825945288714195, -157.3731074845244393 ) ) ;
#64915 = AXIS2_PLACEMENT_3D ( 'NONE', #50323, #7363, #163887 ) ;
#64917 = ORIENTED_EDGE ( 'NONE', *, *, #144488, .F. ) ;
#64916 = DIRECTION ( 'NONE',  ( 0.000000000000000000, -1.265107689135680095E-16, 1.000000000000000000 ) ) ;
#64918 = ORIENTED_EDGE ( 'NONE', *, *, #199548, .T. ) ;
#64919 = FACE_OUTER_BOUND ( 'NONE', #228745, .T. ) ;
#64920 = EDGE_CURVE ( 'NONE', #43421, #129336, #106388, .T. ) ;
#64921 = VERTEX_POINT ( 'NONE', #208669 ) ;
#64922 = CARTESIAN_POINT ( 'NONE',  ( -21.05000000000000071, 69.50298221358116280, -136.5085617939581653 ) ) ;
#64923 = ADVANCED_FACE ( 'NONE', ( #109530 ), #22812, .T. ) ;
#64924 = EDGE_CURVE ( 'NONE', #45345, #87352, #252902, .T. ) ;
#64925 = ORIENTED_EDGE ( 'NONE', *, *, #203835, .T. ) ;
#64926 = CARTESIAN_POINT ( 'NONE',  ( -23.49999999999994316, 76.00000000001119815, -36.02310748452479316 ) ) ;
#64927 = CARTESIAN_POINT ( 'NONE',  ( 21.05000000000000071, 1.162701749949165642, -175.3999999999999773 ) ) ;
#64930 = ORIENTED_EDGE ( 'NONE', *, *, #18038, .T. ) ;
#64929 = ORIENTED_EDGE ( 'NONE', *, *, #8340, .T. ) ;
#64928 = AXIS2_PLACEMENT_3D ( 'NONE', #37048, #35761, #177840 ) ;
#64931 = ORIENTED_EDGE ( 'NONE', *, *, #186226, .T. ) ;
#64932 = LINE ( 'NONE', #67504, #28133 ) ;
#64933 = ORIENTED_EDGE ( 'NONE', *, *, #39908, .F. ) ;
#64934 = ORIENTED_EDGE ( 'NONE', *, *, #166153, .F. ) ;
#64935 = EDGE_CURVE ( 'NONE', #171037, #241225, #135627, .T. ) ;
#64936 = CARTESIAN_POINT ( 'NONE',  ( -20.54999999999999716, 1.115600667400684642E-11, -200.9999999999999432 ) ) ;
#64937 = CARTESIAN_POINT ( 'NONE',  ( 18.59999999999999787, 85.40000000001165859, -62.64106563635156277 ) ) ;
#64939 = ORIENTED_EDGE ( 'NONE', *, *, #86325, .T. ) ;
#64938 = CARTESIAN_POINT ( 'NONE',  ( 18.79999999999999716, -1.885425182446134107, -11.49641995933507843 ) ) ;
#64940 = DIRECTION ( 'NONE',  ( -1.000000000000000000, -0.000000000000000000, -0.000000000000000000 ) ) ;
#64941 = DIRECTION ( 'NONE',  ( -1.000000000000000000, -0.000000000000000000, -0.000000000000000000 ) ) ;
#64943 = ORIENTED_EDGE ( 'NONE', *, *, #192464, .T. ) ;
#64942 = CARTESIAN_POINT ( 'NONE',  ( -20.94999999999999929, 36.18002604163306302, -236.0784499204090991 ) ) ;
#64944 = CARTESIAN_POINT ( 'NONE',  ( -23.15000000000000213, -11.41227409413852811, -97.50000000000004263 ) ) ;
#64945 = VERTEX_POINT ( 'NONE', #233376 ) ;
#64946 = CARTESIAN_POINT ( 'NONE',  ( 20.94999999999999929, 1.835341550235569663, -179.0551512925629538 ) ) ;
#64947 = ORIENTED_EDGE ( 'NONE', *, *, #67308, .F. ) ;
#64948 = CARTESIAN_POINT ( 'NONE',  ( -20.94684162748235678, 18.70797638544537733, -226.6057076234665999 ) ) ;
#64949 = DIRECTION ( 'NONE',  ( 0.000000000000000000, 0.9915357197604982575, -0.1298341882519033486 ) ) ;
#64950 = CIRCLE ( 'NONE', #214800, 12.87499999999999822 ) ;
#64951 = VERTEX_POINT ( 'NONE', #54704 ) ;
#64953 = CARTESIAN_POINT ( 'NONE',  ( -18.50000000000000000, 43.17747518314619271, -245.0773422074893233 ) ) ;
#64952 = CARTESIAN_POINT ( 'NONE',  ( 23.14999999999998437, 76.00000000001165290, -69.52310748452431710 ) ) ;
#64954 = CIRCLE ( 'NONE', #256431, 0.6000000000000033085 ) ;
#64955 = CIRCLE ( 'NONE', #210710, 0.1000000000000013933 ) ;
#64956 = CARTESIAN_POINT ( 'NONE',  ( 21.05000000000000071, 1.115600667400684642E-11, -134.0000000000000284 ) ) ;
#64957 = CARTESIAN_POINT ( 'NONE',  ( -17.22361732159832926, 22.03703477488457807, -229.9826991372272573 ) ) ;
#64958 = ORIENTED_EDGE ( 'NONE', *, *, #198164, .T. ) ;
#64959 = ORIENTED_EDGE ( 'NONE', *, *, #124439, .F. ) ;
#64960 = PRESENTATION_LAYER_ASSIGNMENT (  '', '', ( #52482 ) ) ;
#64961 = CARTESIAN_POINT ( 'NONE',  ( 22.39999999999999503, 68.20922040163900135, -170.1231074845244109 ) ) ;
#64962 = DIRECTION ( 'NONE',  ( -0.000000000000000000, -1.000000000000000000, -0.000000000000000000 ) ) ;
#64964 = ORIENTED_EDGE ( 'NONE', *, *, #206863, .F. ) ;
#64963 = ADVANCED_FACE ( 'NONE', ( #35189 ), #18146, .T. ) ;
#64965 = DIRECTION ( 'NONE',  ( 0.000000000000000000, 0.000000000000000000, 1.000000000000000000 ) ) ;
#64966 = VERTEX_POINT ( 'NONE', #36461 ) ;
#64967 = EDGE_CURVE ( 'NONE', #195862, #83522, #164680, .T. ) ;
#64968 = DIRECTION ( 'NONE',  ( 3.616040088954497272E-32, -1.224646799147352961E-16, 1.000000000000000000 ) ) ;
#64969 = DIRECTION ( 'NONE',  ( 0.000000000000000000, -6.547589603894034005E-15, 1.000000000000000000 ) ) ;
#64970 = CARTESIAN_POINT ( 'NONE',  ( -20.54999999999999716, 54.34471204062663219, -239.4366250215122420 ) ) ;
#64971 = DIRECTION ( 'NONE',  ( 1.000000000000000000, 0.000000000000000000, -0.000000000000000000 ) ) ;
#64973 = EDGE_CURVE ( 'NONE', #141186, #143156, #48147, .T. ) ;
#64972 = ORIENTED_EDGE ( 'NONE', *, *, #150324, .F. ) ;
#64974 = CARTESIAN_POINT ( 'NONE',  ( 18.33996824403518389, -9.569639859420076888, -207.8190656375170704 ) ) ;
#64975 = B_SPLINE_CURVE_WITH_KNOTS ( 'NONE', 3,
 ( #243774, #142098, #185084, #27339, #121301, #220372, #143384, #61288, #5125, #83382 ),
 .UNSPECIFIED., .F., .F.,
 ( 4, 3, 3, 4 ),
 ( 4.906538933386797396E-18, 0.0002000000000002911992, 0.001000000000045103915, 0.001967863649472127805 ),
 .UNSPECIFIED. ) ;
#64976 = AXIS2_PLACEMENT_3D ( 'NONE', #245351, #242758, #48415 ) ;
#64977 =( BOUNDED_SURFACE ( )  B_SPLINE_SURFACE ( 3, 2, ( 
 ( #249206, #150119, #210082 ),
 ( #96203, #250468, #31466 ),
 ( #110967, #175777, #255233 ),
 ( #190533, #97467, #256505 ) ),
 .UNSPECIFIED., .F., .F., .T. ) 
 B_SPLINE_SURFACE_WITH_KNOTS ( ( 4, 4 ),
 ( 3, 3 ),
 ( 1.570796326794896558, 3.141592653589793116 ),
 ( 0.000000000000000000, 1.000000000000000000 ),
 .UNSPECIFIED. ) 
 GEOMETRIC_REPRESENTATION_ITEM ( )  RATIONAL_B_SPLINE_SURFACE ( (
 ( 1.000000000000000000, 0.7071067811865505703, 1.000000000000000000),
 ( 1.000000000000000000, 0.6753870962079620011, 1.000000000000000000),
 ( 1.000000000000000000, 0.6438648806865411300, 1.000000000000000000),
 ( 1.000000000000000000, 0.6447402616205117898, 1.000000000000000000) ) ) 
 REPRESENTATION_ITEM ( '' )  SURFACE ( )  );
#64979 = EDGE_LOOP ( 'NONE', ( #29888, #106297, #18206, #126290 ) ) ;
#64978 = ORIENTED_EDGE ( 'NONE', *, *, #246478, .F. ) ;
#64980 = ORIENTED_EDGE ( 'NONE', *, *, #17937, .F. ) ;
#64981 = TOROIDAL_SURFACE ( 'NONE', #69289, 4.041421356237310469, 0.1000000000000000056 ) ;
#64982 = ORIENTED_EDGE ( 'NONE', *, *, #69333, .F. ) ;
#64983 = CARTESIAN_POINT ( 'NONE',  ( 18.59999999999999787, -9.849999999999994316, 30.00000000000000000 ) ) ;
#64984 = CARTESIAN_POINT ( 'NONE',  ( 19.99999999999998934, 64.25000000001179501, -81.67310748452439384 ) ) ;
#64985 = FACE_OUTER_BOUND ( 'NONE', #200829, .T. ) ;
#64986 = DIRECTION ( 'NONE',  ( 0.000000000000000000, 0.000000000000000000, -1.000000000000000000 ) ) ;
#64987 = AXIS2_PLACEMENT_3D ( 'NONE', #74465, #40475, #62571 ) ;
#64988 = CARTESIAN_POINT ( 'NONE',  ( -18.59999999999999787, 1.162701749949165642, -142.1000000000000227 ) ) ;
#64989 = DIRECTION ( 'NONE',  ( 0.000000000000000000, 0.000000000000000000, 1.000000000000000000 ) ) ;
#64991 = ORIENTED_EDGE ( 'NONE', *, *, #41216, .F. ) ;
#64990 = CARTESIAN_POINT ( 'NONE',  ( 18.50000000000000355, 77.35494420175976416, -241.6200040285045532 ) ) ;
#64992 = DIRECTION ( 'NONE',  ( 0.000000000000000000, 0.000000000000000000, -1.000000000000000000 ) ) ;
#64993 = ORIENTED_EDGE ( 'NONE', *, *, #200081, .F. ) ;
#64994 = CARTESIAN_POINT ( 'NONE',  ( 21.08489247129321242, 8.877675190881227252, -79.35000000000005116 ) ) ;
#64995 = CIRCLE ( 'NONE', #52514, 3.970710678118657189 ) ;
#64996 = ORIENTED_EDGE ( 'NONE', *, *, #39788, .T. ) ;
#64997 = VERTEX_POINT ( 'NONE', #59812 ) ;
#64998 = CARTESIAN_POINT ( 'NONE',  ( 21.05000000000000426, 69.58617371119916584, -136.4373665474909956 ) ) ;
#64999 = DIRECTION ( 'NONE',  ( 0.000000000000000000, 0.000000000000000000, 1.000000000000000000 ) ) ;
#65000 = CARTESIAN_POINT ( 'NONE',  ( -16.84981964351508665, 66.08268176591256804, -48.89270909854381131 ) ) ;
#65001 = LINE ( 'NONE', #45446, #95799 ) ;
#65002 = EDGE_CURVE ( 'NONE', #152770, #54116, #93941, .T. ) ;
#65003 = TOROIDAL_SURFACE ( 'NONE', #231614, 0.2000000000000000111, 0.1000000000000000056 ) ;
#65004 = DIRECTION ( 'NONE',  ( -1.000000000000000000, 0.000000000000000000, 0.000000000000000000 ) ) ;
#65005 = EDGE_LOOP ( 'NONE', ( #185890, #41960, #220709, #138819 ) ) ;
#65006 = VERTEX_POINT ( 'NONE', #239770 ) ;
#65007 = CIRCLE ( 'NONE', #239813, 11.70000000000000284 ) ;
#65009 = EDGE_CURVE ( 'NONE', #99760, #39027, #178536, .T. ) ;
#65008 = FACE_OUTER_BOUND ( 'NONE', #190731, .T. ) ;
#65010 = ORIENTED_EDGE ( 'NONE', *, *, #10148, .F. ) ;
#65011 = DIRECTION ( 'NONE',  ( 1.000000000000000000, 0.000000000000000000, -0.000000000000000000 ) ) ;
#65012 = DIRECTION ( 'NONE',  ( -0.7071067811865389130, 8.659560562355038861E-17, -0.7071067811865561215 ) ) ;
#65013 = LINE ( 'NONE', #5016, #73857 ) ;
#65014 = DIRECTION ( 'NONE',  ( 1.000000000000000000, 0.000000000000000000, 0.000000000000000000 ) ) ;
#65015 = CARTESIAN_POINT ( 'NONE',  ( 21.97500000000000497, 66.25000000001206502, -124.1731074845243654 ) ) ;
#65016 = DIRECTION ( 'NONE',  ( -1.000000000000000000, -0.000000000000000000, -0.000000000000000000 ) ) ;
#65017 = EDGE_LOOP ( 'NONE', ( #183775, #201367, #129924, #108224 ) ) ;
#65018 = CARTESIAN_POINT ( 'NONE',  ( -20.54999999999999716, 62.08148826970418099, -247.6553521922769221 ) ) ;
#65019 = ADVANCED_FACE ( 'NONE', ( #177257 ), #27354, .F. ) ;
#65020 = DIRECTION ( 'NONE',  ( 0.000000000000000000, -0.8814952561688430555, 0.4721928772777346239 ) ) ;
#65021 = FACE_OUTER_BOUND ( 'NONE', #42664, .T. ) ;
#65023 = ADVANCED_FACE ( 'NONE', ( #40317 ), #196771, .F. ) ;
#65022 = DIRECTION ( 'NONE',  ( -1.000000000000000000, 0.000000000000000000, 0.000000000000000000 ) ) ;
#65024 = AXIS2_PLACEMENT_3D ( 'NONE', #47909, #40586, #147004 ) ;
#65025 = CARTESIAN_POINT ( 'NONE',  ( 21.05000000000000071, 28.42524210734032408, -258.3567845160494585 ) ) ;
#65026 = ADVANCED_FACE ( 'NONE', ( #175967 ), #156415, .T. ) ;
#65027 = EDGE_LOOP ( 'NONE', ( #187442, #234807, #101400, #123163 ) ) ;
#65029 = EDGE_CURVE ( 'NONE', #206404, #22410, #78108, .T. ) ;
#65028 = EDGE_CURVE ( 'NONE', #246982, #246161, #197982, .T. ) ;
#65030 = CARTESIAN_POINT ( 'NONE',  ( -16.87242674293850087, 66.05000000001231797, -157.3741977308967819 ) ) ;
#65031 = EDGE_LOOP ( 'NONE', ( #176890, #95516, #171533, #243031 ) ) ;
#65032 =( BOUNDED_SURFACE ( )  B_SPLINE_SURFACE ( 3, 2, ( 
 ( #122988, #182964, #224631 ),
 ( #126826, #105950, #164675 ),
 ( #8173, #86378, #163393 ),
 ( #124271, #223340, #65561 ) ),
 .UNSPECIFIED., .F., .F., .F. ) 
 B_SPLINE_SURFACE_WITH_KNOTS ( ( 4, 4 ),
 ( 3, 3 ),
 ( 0.0008258556059633768206, 0.0009616864997632841496 ),
 ( 0.000000000000000000, 1.000000000000000000 ),
 .UNSPECIFIED. ) 
 GEOMETRIC_REPRESENTATION_ITEM ( )  RATIONAL_B_SPLINE_SURFACE ( (
 ( 1.000000000000000000, 0.9152888060719408525, 1.000000000000000000),
 ( 1.000000000000000000, 0.9327727094138220654, 1.000000000000000000),
 ( 1.000000000000000000, 0.9369023509258298521, 1.000000000000000000),
 ( 1.000000000000000000, 0.9246339933864542449, 1.000000000000000000) ) ) 
 REPRESENTATION_ITEM ( '' )  SURFACE ( )  );
#65033 = CARTESIAN_POINT ( 'NONE',  ( 23.14999999999999858, 5.500000000011153745, -121.5947339810869465 ) ) ;
#65035 = VECTOR ( 'NONE', #86958, 1000.000000000000000 ) ;
#65034 = CYLINDRICAL_SURFACE ( 'NONE', #252131, 0.1000000000000028644 ) ;
#65036 = CARTESIAN_POINT ( 'NONE',  ( 21.05000005001233276, 61.85690724456019041, -221.7796802661272295 ) ) ;
#65038 = ORIENTED_EDGE ( 'NONE', *, *, #56675, .T. ) ;
#65037 = AXIS2_PLACEMENT_3D ( 'NONE', #81831, #240953, #62313 ) ;
#65039 = DIRECTION ( 'NONE',  ( 1.000000000000000000, 0.000000000000000000, -0.000000000000000000 ) ) ;
#65040 = DIRECTION ( 'NONE',  ( 0.000000000000000000, -0.8700118002898322711, 0.4930308989875231140 ) ) ;
#65041 = AXIS2_PLACEMENT_3D ( 'NONE', #70139, #45407, #207056 ) ;
#65042 = VECTOR ( 'NONE', #239335, 1000.000000000000000 ) ;
#65043 = SURFACE_STYLE_FILL_AREA ( #147143 ) ;
#65044 = FACE_OUTER_BOUND ( 'NONE', #236591, .T. ) ;
#65045 = EDGE_CURVE ( 'NONE', #176002, #7516, #14855, .T. ) ;
#65046 = DIRECTION ( 'NONE',  ( -1.000000000000000000, 1.836970198721029934E-16, 1.282749433769087757E-30 ) ) ;
#65047 = EDGE_CURVE ( 'NONE', #18361, #31867, #123173, .T. ) ;
#65048 = LINE ( 'NONE', #125038, #165426 ) ;
#65049 = CIRCLE ( 'NONE', #210792, 0.1000000000000000472 ) ;
#65050 = ORIENTED_EDGE ( 'NONE', *, *, #192038, .F. ) ;
#65051 = CARTESIAN_POINT ( 'NONE',  ( -20.54999999999999716, 84.66355140188177586, -193.9990063664569959 ) ) ;
#65053 = ORIENTED_EDGE ( 'NONE', *, *, #199289, .T. ) ;
#65052 = DIRECTION ( 'NONE',  ( -0.000000000000000000, 1.000000000000000000, -0.000000000000000000 ) ) ;
#65054 = CARTESIAN_POINT ( 'NONE',  ( -23.25000000000000000, 71.65000000001259650, -191.2731074845243882 ) ) ;
#65055 = EDGE_CURVE ( 'NONE', #85165, #9680, #22014, .T. ) ;
#65056 = FACE_OUTER_BOUND ( 'NONE', #27833, .T. ) ;
#65057 = AXIS2_PLACEMENT_3D ( 'NONE', #206726, #67215, #248425 ) ;
#65058 = EDGE_LOOP ( 'NONE', ( #11430, #40977, #134461, #183037 ) ) ;
#65059 = DIRECTION ( 'NONE',  ( 2.952720810173289112E-16, -1.000000000000000000, -0.000000000000000000 ) ) ;
#65060 = CIRCLE ( 'NONE', #210802, 0.09999999999999939493 ) ;
#65061 = EDGE_CURVE ( 'NONE', #204227, #234655, #20735, .T. ) ;
#65062 = CARTESIAN_POINT ( 'NONE',  ( -20.85000000000000142, 75.83895117929343144, -136.8072973288845731 ) ) ;
#65063 = TOROIDAL_SURFACE ( 'NONE', #210804, 4.149999999999999467, 0.1000000000000000056 ) ;
#65064 = ORIENTED_EDGE ( 'NONE', *, *, #102347, .T. ) ;
#65065 = DIRECTION ( 'NONE',  ( 0.000000000000000000, 0.000000000000000000, 1.000000000000000000 ) ) ;
#65066 = CARTESIAN_POINT ( 'NONE',  ( 13.77030915526559340, 9.456007326080465347, -185.9886334941467396 ) ) ;
#65067 = ADVANCED_FACE ( 'NONE', ( #174709 ), #189627, .F. ) ;
#65068 = ORIENTED_EDGE ( 'NONE', *, *, #160864, .T. ) ;
#65069 = EDGE_LOOP ( 'NONE', ( #44889, #169340, #213692, #181458, #11216, #115881 ) ) ;
#65070 = EDGE_CURVE ( 'NONE', #133285, #47404, #110502, .T. ) ;
#65071 = DIRECTION ( 'NONE',  ( 0.000000000000000000, 0.000000000000000000, -1.000000000000000000 ) ) ;
#65072 = CARTESIAN_POINT ( 'NONE',  ( 21.87500000000000355, 14.04870287383362992, -219.6884709798077893 ) ) ;
#65073 = DIRECTION ( 'NONE',  ( 1.284434275755705789E-16, -0.7071067811865472397, 0.7071067811865479058 ) ) ;
#65074 = CARTESIAN_POINT ( 'NONE',  ( 20.94999999999999929, 1.115600667400684642E-11, -100.5000000000000426 ) ) ;
#65075 = DIRECTION ( 'NONE',  ( -0.000000000000000000, 0.000000000000000000, 1.000000000000000000 ) ) ;
#65076 = CYLINDRICAL_SURFACE ( 'NONE', #216092, 0.09999999999998898659 ) ;
#65077 = DIRECTION ( 'NONE',  ( -3.265361837132812600E-16, 0.4721928772777346239, 0.8814952561688430555 ) ) ;
#65079 = CARTESIAN_POINT ( 'NONE',  ( -18.47653818581419927, -9.465280387751805691, -74.12596081613986598 ) ) ;
#65078 = CARTESIAN_POINT ( 'NONE',  ( 21.53752568617668572, 6.786807874503922200, 0.09897446126639813935 ) ) ;
#65080 = ADVANCED_FACE ( 'NONE', ( #234628 ), #195532, .F. ) ;
#65081 = DIRECTION ( 'NONE',  ( -1.000000000000000000, 0.000000000000000000, 0.000000000000000000 ) ) ;
#65082 = CARTESIAN_POINT ( 'NONE',  ( -21.64999999999999858, 7.250000000011148416, -54.65000000000000568 ) ) ;
#65083 = DIRECTION ( 'NONE',  ( 0.000000000000000000, -1.000000000000000000, 0.000000000000000000 ) ) ;
#65084 = FACE_OUTER_BOUND ( 'NONE', #104321, .T. ) ;
#65085 = VECTOR ( 'NONE', #237877, 1000.000000000000000 ) ;
#65086 = EDGE_LOOP ( 'NONE', ( #247745, #158545, #27902, #131335, #62070 ) ) ;
#65087 = CIRCLE ( 'NONE', #19294, 0.4000000000000114575 ) ;
#65088 = EDGE_LOOP ( 'NONE', ( #154515, #48221, #82483, #217906 ) ) ;
#65089 = AXIS2_PLACEMENT_3D ( 'NONE', #123846, #78272, #241231 ) ;
#65090 = DIRECTION ( 'NONE',  ( 0.000000000000000000, -6.608470384673536824E-15, 1.000000000000000000 ) ) ;
#65091 = TOROIDAL_SURFACE ( 'NONE', #215293, 11.65000000000000036, 0.1000000000000000056 ) ;
#65092 = CARTESIAN_POINT ( 'NONE',  ( 23.14999999999999503, 64.35000000001195986, -110.0379132551783243 ) ) ;
#65094 = CARTESIAN_POINT ( 'NONE',  ( -23.15000000000000213, 36.65892442174935439, -249.5511627012433848 ) ) ;
#65093 = DIRECTION ( 'NONE',  ( 0.000000000000000000, 0.7071067811865472397, -0.7071067811865479058 ) ) ;
#65095 = CARTESIAN_POINT ( 'NONE',  ( 21.05000000000000071, 1.115600667400684642E-11, -33.50000000000000000 ) ) ;
#65096 = DIRECTION ( 'NONE',  ( 0.000000000000000000, 0.000000000000000000, 1.000000000000000000 ) ) ;
#65097 = EDGE_CURVE ( 'NONE', #14219, #87677, #145780, .T. ) ;
#65098 = CYLINDRICAL_SURFACE ( 'NONE', #193463, 0.1000000000000028644 ) ;
#65099 = PLANE ( 'NONE',  #109925 ) ;
#65100 = ORIENTED_EDGE ( 'NONE', *, *, #142629, .T. ) ;
#65101 = DIRECTION ( 'NONE',  ( -1.000000000000000000, -0.000000000000000000, -0.000000000000000000 ) ) ;
#65102 = AXIS2_PLACEMENT_3D ( 'NONE', #105715, #165747, #122768 ) ;
#65103 = EDGE_LOOP ( 'NONE', ( #50390, #189706, #72720, #214630 ) ) ;
#65104 = CARTESIAN_POINT ( 'NONE',  ( -18.47140463609786920, -9.671474685209730637, -73.67276045827406961 ) ) ;
#65105 = VECTOR ( 'NONE', #28820, 1000.000000000000000 ) ;
#65106 = CARTESIAN_POINT ( 'NONE',  ( 18.39999999999999503, 50.88295650978584206, -230.3037755757580953 ) ) ;
#65107 = AXIS2_PLACEMENT_3D ( 'NONE', #191166, #152040, #112894 ) ;
#65108 = ORIENTED_EDGE ( 'NONE', *, *, #172978, .F. ) ;
#65109 = CARTESIAN_POINT ( 'NONE',  ( -18.56579813702275672, 18.41141989892753017, -236.9935361838138022 ) ) ;
#65110 = ORIENTED_EDGE ( 'NONE', *, *, #178844, .F. ) ;
#65111 = CARTESIAN_POINT ( 'NONE',  ( -21.44999999999999929, 68.85000000001222986, -148.7731074845244166 ) ) ;
#65112 = CARTESIAN_POINT ( 'NONE',  ( -22.00356870143097154, 68.74575763753914259, -69.52310748452435973 ) ) ;
#65113 = CARTESIAN_POINT ( 'NONE',  ( 23.14999999999999858, 6.650000000011155876, -146.3500000000000227 ) ) ;
#65114 = CARTESIAN_POINT ( 'NONE',  ( 18.46947024752513045, -9.509297157144889212, -140.9866894486979731 ) ) ;
#65115 = CARTESIAN_POINT ( 'NONE',  ( -18.50000000000000000, -1.687074390080403941, -87.68542703345838163 ) ) ;
#65116 = DIRECTION ( 'NONE',  ( 0.8049926720990051576, -0.5932847527679298016, -4.142885285818778274E-15 ) ) ;
#65117 = FACE_OUTER_BOUND ( 'NONE', #156663, .T. ) ;
#65118 = DIRECTION ( 'NONE',  ( 0.000000000000000000, 0.000000000000000000, -1.000000000000000000 ) ) ;
#65120 = VERTEX_POINT ( 'NONE', #47970 ) ;
#65119 = LINE ( 'NONE', #123826, #152633 ) ;
#65122 = CARTESIAN_POINT ( 'NONE',  ( 22.39999999999999503, 76.00000000001243450, -177.8138870828977360 ) ) ;
#65121 = CARTESIAN_POINT ( 'NONE',  ( -18.43569575749026512, 85.51932773110507924, -196.5501311079650293 ) ) ;
#65123 = VERTEX_POINT ( 'NONE', #122389 ) ;
#65124 = VERTEX_POINT ( 'NONE', #204473 ) ;
#65125 = AXIS2_PLACEMENT_3D ( 'NONE', #75841, #219188, #197053 ) ;
#65126 = ORIENTED_EDGE ( 'NONE', *, *, #26437, .F. ) ;
#65127 = DIRECTION ( 'NONE',  ( 0.000000000000000000, 0.8814952561688444987, -0.4721928772777320149 ) ) ;
#65128 = CARTESIAN_POINT ( 'NONE',  ( -20.65000000000000568, 7.250000000011138646, -76.25000000000004263 ) ) ;
#65129 = DIRECTION ( 'NONE',  ( 0.000000000000000000, 0.000000000000000000, -1.000000000000000000 ) ) ;
#65130 = CARTESIAN_POINT ( 'NONE',  ( 21.04999999999999716, 8.871279686006799281, -112.6500000000000199 ) ) ;
#65131 = CARTESIAN_POINT ( 'NONE',  ( 18.49999999999998934, 69.45000000001252261, -182.2731074845244166 ) ) ;
#65133 = CARTESIAN_POINT ( 'NONE',  ( -16.92778301347364689, 10.00094491684727771, -154.9285181079674487 ) ) ;
#65132 = AXIS2_PLACEMENT_3D ( 'NONE', #27862, #68240, #44823 ) ;
#65134 = DIRECTION ( 'NONE',  ( -1.000000000000000000, -3.265361837132813093E-16, 0.000000000000000000 ) ) ;
#65135 = ADVANCED_FACE ( 'NONE', ( #44139 ), #110694, .T. ) ;
#65137 = CIRCLE ( 'NONE', #15084, 0.1000000000000028644 ) ;
#65136 = CARTESIAN_POINT ( 'NONE',  ( 23.24999999999999289, 64.25000000001202238, -114.7731074845243882 ) ) ;
#65138 = ORIENTED_EDGE ( 'NONE', *, *, #41193, .T. ) ;
#65139 = ORIENTED_EDGE ( 'NONE', *, *, #94095, .F. ) ;
#65140 = CIRCLE ( 'NONE', #98416, 0.09999999999999939493 ) ;
#65141 = AXIS2_PLACEMENT_3D ( 'NONE', #142829, #201542, #43761 ) ;
#65142 = EDGE_LOOP ( 'NONE', ( #68054, #108101, #21846, #238429 ) ) ;
#65143 = FACE_OUTER_BOUND ( 'NONE', #232765, .T. ) ;
#65144 = ORIENTED_EDGE ( 'NONE', *, *, #143356, .T. ) ;
#65145 = CARTESIAN_POINT ( 'NONE',  ( 21.14999999999999858, 69.35000000001156195, -57.27310748452436684 ) ) ;
#65146 = CARTESIAN_POINT ( 'NONE',  ( -16.92209698673726237, 9.950000000011138823, -180.2106355670536573 ) ) ;
#65147 = CARTESIAN_POINT ( 'NONE',  ( -21.53699400379683127, 69.21228820681116645, -103.0231074845243455 ) ) ;
#65148 = EDGE_CURVE ( 'NONE', #251500, #53868, #10940, .T. ) ;
#65149 = CARTESIAN_POINT ( 'NONE',  ( -21.11101077989000174, 30.79037258772926577, -252.1634526128120797 ) ) ;
#65150 = DIRECTION ( 'NONE',  ( 0.000000000000000000, -0.000000000000000000, -1.000000000000000000 ) ) ;
#65151 = ORIENTED_EDGE ( 'NONE', *, *, #97641, .F. ) ;
#65152 = EDGE_CURVE ( 'NONE', #19542, #55997, #202279, .T. ) ;
#65153 = CARTESIAN_POINT ( 'NONE',  ( -13.39999999999994351, 64.35000000001120668, -23.72310748452479245 ) ) ;
#65154 = LINE ( 'NONE', #166872, #221264 ) ;
#65155 = CARTESIAN_POINT ( 'NONE',  ( -20.54999999999999716, 9.350000000011156942, -112.7500000000000284 ) ) ;
#65156 = CARTESIAN_POINT ( 'NONE',  ( -23.25000000000000000, 1.115651490242849210E-11, -29.35000000000000142 ) ) ;
#65157 = ORIENTED_EDGE ( 'NONE', *, *, #237792, .T. ) ;
#65159 = CARTESIAN_POINT ( 'NONE',  ( 23.50000000000005684, 83.80000000001119531, -34.86056257560453986 ) ) ;
#65158 = CARTESIAN_POINT ( 'NONE',  ( -23.15000000000000213, 64.35000000001156195, -57.37310748452439668 ) ) ;
#65160 = VECTOR ( 'NONE', #130791, 1000.000000000000000 ) ;
#65161 = ORIENTED_EDGE ( 'NONE', *, *, #131737, .F. ) ;
#65164 = EDGE_LOOP ( 'NONE', ( #250210, #92508, #146573, #2663 ) ) ;
#65163 = DIRECTION ( 'NONE',  ( -1.000000000000000000, 2.952720810173289112E-16, 2.061873921506763405E-30 ) ) ;
#65162 = DIRECTION ( 'NONE',  ( 0.000000000000000000, 0.000000000000000000, -1.000000000000000000 ) ) ;
#65165 = ORIENTED_EDGE ( 'NONE', *, *, #191849, .F. ) ;
#65166 = DIRECTION ( 'NONE',  ( 0.000000000000000000, 0.000000000000000000, -1.000000000000000000 ) ) ;
#65167 = AXIS2_PLACEMENT_3D ( 'NONE', #134757, #171386, #31860 ) ;
#65168 = DIRECTION ( 'NONE',  ( 0.000000000000000000, 0.9770955615653313941, 0.2128009952263603677 ) ) ;
#65169 = EDGE_CURVE ( 'NONE', #192209, #241724, #123675, .T. ) ;
#65170 = DIRECTION ( 'NONE',  ( 0.000000000000000000, -0.2128009952263603677, 0.9770955615653313941 ) ) ;
#65171 = ORIENTED_EDGE ( 'NONE', *, *, #224337, .F. ) ;
#65172 = FACE_OUTER_BOUND ( 'NONE', #90194, .T. ) ;
#65173 = EDGE_CURVE ( 'NONE', #36355, #196464, #248255, .T. ) ;
#65174 = CIRCLE ( 'NONE', #136058, 11.64999999999999325 ) ;
#65175 = CARTESIAN_POINT ( 'NONE',  ( 20.94999999999999929, -8.999999999988842703, -90.60603087734760663 ) ) ;
#65176 = CIRCLE ( 'NONE', #69479, 0.1000000000000072220 ) ;
#65177 = EDGE_CURVE ( 'NONE', #68414, #151483, #85783, .T. ) ;
#65179 = DIRECTION ( 'NONE',  ( 0.000000000000000000, 0.9651348961777157509, -0.2617529984165031243 ) ) ;
#65178 = LINE ( 'NONE', #226822, #238781 ) ;
#65180 = CIRCLE ( 'NONE', #110974, 0.2000000000000057288 ) ;
#65182 = EDGE_LOOP ( 'NONE', ( #252302, #233847, #133543, #42280 ) ) ;
#65181 = CARTESIAN_POINT ( 'NONE',  ( 21.40925344232283223, 0.09895018861964713364, 6.658518859390456512 ) ) ;
#65183 = EDGE_CURVE ( 'NONE', #233091, #137562, #135801, .T. ) ;
#65184 = ORIENTED_EDGE ( 'NONE', *, *, #193337, .F. ) ;
#65185 = DIRECTION ( 'NONE',  ( 0.000000000000000000, 0.9126074666063769270, 0.4088369013363280513 ) ) ;
#65186 = DIRECTION ( 'NONE',  ( 1.000000000000000000, 0.000000000000000000, 0.000000000000000000 ) ) ;
#65187 = VECTOR ( 'NONE', #64302, 1000.000000000000114 ) ;
#65188 = CARTESIAN_POINT ( 'NONE',  ( 21.14999999999999858, 6.550000000011156231, -79.35000000000005116 ) ) ;
#65189 = ORIENTED_EDGE ( 'NONE', *, *, #101064, .F. ) ;
#65191 = MECHANICAL_DESIGN_GEOMETRIC_PRESENTATION_REPRESENTATION (  '', ( #11027 ), #210944 ) ;
#65190 = CARTESIAN_POINT ( 'NONE',  ( -21.14999999999999858, 76.10000000001174669, -81.17267829206912211 ) ) ;
#65192 = EDGE_CURVE ( 'NONE', #31598, #165206, #225307, .T. ) ;
#65193 = ORIENTED_EDGE ( 'NONE', *, *, #196069, .T. ) ;
#65194 = AXIS2_PLACEMENT_3D ( 'NONE', #45192, #165151, #124744 ) ;
#65195 = CARTESIAN_POINT ( 'NONE',  ( 21.05000000000000071, 18.81166555858609257, -229.8642012822692777 ) ) ;
#65196 = LINE ( 'NONE', #104303, #7813 ) ;
#65197 = DIRECTION ( 'NONE',  ( 1.000000000000000000, -1.646408749285562060E-14, -1.073024830501232702E-15 ) ) ;
#65198 = ORIENTED_EDGE ( 'NONE', *, *, #13996, .T. ) ;
#65199 = CARTESIAN_POINT ( 'NONE',  ( 20.85000000000000142, 87.24382154048164750, -206.5725299160771726 ) ) ;
#65200 = ADVANCED_FACE ( 'NONE', ( #141938 ), #24591, .T. ) ;
#65201 = TOROIDAL_SURFACE ( 'NONE', #202578, 0.2000000000000000111, 0.1000000000000000056 ) ;
#65202 = CARTESIAN_POINT ( 'NONE',  ( 18.49999999999998934, 69.45000000001199680, -115.2731074845243455 ) ) ;
#65203 = ORIENTED_EDGE ( 'NONE', *, *, #159609, .F. ) ;
#65204 = ORIENTED_EDGE ( 'NONE', *, *, #19334, .T. ) ;
#65205 = ORIENTED_EDGE ( 'NONE', *, *, #210701, .T. ) ;
#65206 = DIRECTION ( 'NONE',  ( 0.000000000000000000, -0.9656312546561486299, -0.2599159095384356855 ) ) ;
#65207 = VERTEX_POINT ( 'NONE', #201925 ) ;
#65209 = ORIENTED_EDGE ( 'NONE', *, *, #128994, .T. ) ;
#65208 = CARTESIAN_POINT ( 'NONE',  ( 18.49999999999999645, 77.16412189325360771, -162.1082593989527254 ) ) ;
#65210 = ORIENTED_EDGE ( 'NONE', *, *, #250072, .T. ) ;
#65211 = AXIS2_PLACEMENT_3D ( 'NONE', #38570, #17702, #157260 ) ;
#65212 = VECTOR ( 'NONE', #224905, 1000.000000000000000 ) ;
#65215 = ORIENTED_EDGE ( 'NONE', *, *, #123909, .T. ) ;
#65214 = ORIENTED_EDGE ( 'NONE', *, *, #198580, .T. ) ;
#65213 = DIRECTION ( 'NONE',  ( -1.000000000000000000, -1.541976423090492636E-14, 0.000000000000000000 ) ) ;
#65216 = CIRCLE ( 'NONE', #40327, 0.09999999999998898659 ) ;
#65217 = AXIS2_PLACEMENT_3D ( 'NONE', #22034, #256724, #200660 ) ;
#65218 = LINE ( 'NONE', #235839, #89820 ) ;
#65219 = ORIENTED_EDGE ( 'NONE', *, *, #122194, .F. ) ;
#65220 = CARTESIAN_POINT ( 'NONE',  ( -20.00857864376270001, 9.150000000011157653, -121.7500000000000426 ) ) ;
#65221 = CARTESIAN_POINT ( 'NONE',  ( 18.49999999999999289, 69.35000000001254250, -182.1731074845243938 ) ) ;
#65222 = AXIS2_PLACEMENT_3D ( 'NONE', #77713, #195144, #138954 ) ;
#65223 = EDGE_CURVE ( 'NONE', #180985, #17556, #3710, .T. ) ;
#65224 = CARTESIAN_POINT ( 'NONE',  ( -18.52309608778520555, 87.06385610752170123, -199.5665633308501299 ) ) ;
#65225 = ORIENTED_EDGE ( 'NONE', *, *, #172471, .F. ) ;
#65226 = CARTESIAN_POINT ( 'NONE',  ( 18.49999999999999289, 53.42432843990430058, -234.7536552047824330 ) ) ;
#65228 = ORIENTED_EDGE ( 'NONE', *, *, #216873, .F. ) ;
#65227 = DIRECTION ( 'NONE',  ( 0.000000000000000000, -0.9999176327611369874, 0.01283462868041984617 ) ) ;
#65229 = CARTESIAN_POINT ( 'NONE',  ( -16.86379686415369150, 14.20138720008526789, -219.3311860823795030 ) ) ;
#65231 = ORIENTED_EDGE ( 'NONE', *, *, #178298, .F. ) ;
#65230 = CYLINDRICAL_SURFACE ( 'NONE', #227083, 0.09999999999999939493 ) ;
#65232 = ADVANCED_FACE ( 'NONE', ( #23313 ), #27541, .F. ) ;
#65234 = EDGE_CURVE ( 'NONE', #146785, #104724, #73313, .T. ) ;
#65233 = CIRCLE ( 'NONE', #252668, 0.09999999999999685529 ) ;
#65235 = EDGE_LOOP ( 'NONE', ( #231858, #48498 ) ) ;
#65236 = DIRECTION ( 'NONE',  ( -1.000000000000000000, -1.836970198721029934E-16, 0.000000000000000000 ) ) ;
#65237 = AXIS2_PLACEMENT_3D ( 'NONE', #202028, #222860, #28574 ) ;
#65238 = EDGE_CURVE ( 'NONE', #215983, #142842, #143214, .T. ) ;
#65239 = ADVANCED_FACE ( 'NONE', ( #186215 ), #101488, .T. ) ;
#65240 = VERTEX_POINT ( 'NONE', #105345 ) ;
#65241 = EDGE_LOOP ( 'NONE', ( #93495, #193339, #193947, #224083, #162843 ) ) ;
#65242 = PLANE ( 'NONE',  #64605 ) ;
#65244 = ADVANCED_FACE ( 'NONE', ( #147063 ), #67725, .T. ) ;
#65243 = CARTESIAN_POINT ( 'NONE',  ( -21.52071067811865746, 7.779289321892505882, -179.8499999999999943 ) ) ;
#65245 = EDGE_CURVE ( 'NONE', #161343, #57517, #210646, .T. ) ;
#65247 = VERTEX_POINT ( 'NONE', #131364 ) ;
#65246 = ORIENTED_EDGE ( 'NONE', *, *, #138333, .T. ) ;
#65248 = ORIENTED_EDGE ( 'NONE', *, *, #89683, .T. ) ;
#65249 = CARTESIAN_POINT ( 'NONE',  ( 23.04999999999999716, 8.822561741677553471, -154.8500000000000227 ) ) ;
#65250 = ORIENTED_EDGE ( 'NONE', *, *, #215464, .F. ) ;
#65251 = ORIENTED_EDGE ( 'NONE', *, *, #185820, .F. ) ;
#65252 = EDGE_CURVE ( 'NONE', #143490, #183369, #247460, .T. ) ;
#65253 = CARTESIAN_POINT ( 'NONE',  ( 21.14999999999999858, 67.23127455305841238, -235.8551265064783991 ) ) ;
#65254 = AXIS2_PLACEMENT_3D ( 'NONE', #184539, #28079, #85411 ) ;
#65256 = EDGE_LOOP ( 'NONE', ( #207937, #160906, #51981, #151032, #99885, #37082, #188035 ) ) ;
#65255 = DIRECTION ( 'NONE',  ( 1.000000000000000000, 0.000000000000000000, 0.000000000000000000 ) ) ;
#65257 = FACE_OUTER_BOUND ( 'NONE', #38871, .T. ) ;
#65259 = CARTESIAN_POINT ( 'NONE',  ( 18.51565452909384746, -9.352859338825702196, -107.6949093212341353 ) ) ;
#65258 = DIRECTION ( 'NONE',  ( -0.000000000000000000, -0.8814952561688430555, 0.4721928772777346239 ) ) ;
#65260 = CARTESIAN_POINT ( 'NONE',  ( 16.87683809663750267, 9.949999999999983302, -12.65000000000000036 ) ) ;
#65261 = ORIENTED_EDGE ( 'NONE', *, *, #178252, .T. ) ;
#65262 = ORIENTED_EDGE ( 'NONE', *, *, #726, .T. ) ;
#65263 = FACE_OUTER_BOUND ( 'NONE', #192137, .T. ) ;
#65264 =( NAMED_UNIT ( * ) PLANE_ANGLE_UNIT ( ) SI_UNIT ( $, .RADIAN. ) );
#65265 = VERTEX_POINT ( 'NONE', #250033 ) ;
#65266 = AXIS2_PLACEMENT_3D ( 'NONE', #82318, #238860, #41964 ) ;
#65267 = AXIS2_PLACEMENT_3D ( 'NONE', #222791, #44188, #243655 ) ;
#65268 = CIRCLE ( 'NONE', #131908, 0.1000000000000000472 ) ;
#65269 = AXIS2_PLACEMENT_3D ( 'NONE', #245274, #146150, #48340 ) ;
#65270 = EDGE_CURVE ( 'NONE', #250175, #168296, #219017, .T. ) ;
#65271 = DIRECTION ( 'NONE',  ( 0.000000000000000000, -6.982962677686266711E-15, 1.000000000000000000 ) ) ;
#65272 = ORIENTED_EDGE ( 'NONE', *, *, #131224, .F. ) ;
#65273 = ORIENTED_EDGE ( 'NONE', *, *, #26756, .F. ) ;
#65274 = CARTESIAN_POINT ( 'NONE',  ( -18.59999999999999787, -1.164121893241208960, -41.21484808557161017 ) ) ;
#65276 = EDGE_CURVE ( 'NONE', #191700, #248135, #71418, .T. ) ;
#65275 = ORIENTED_EDGE ( 'NONE', *, *, #27971, .T. ) ;
#65277 = CARTESIAN_POINT ( 'NONE',  ( -21.00448002041558482, 11.75000000001147704, -107.3483408623108488 ) ) ;
#65278 = LINE ( 'NONE', #99251, #106036 ) ;
#65279 = ORIENTED_EDGE ( 'NONE', *, *, #250258, .F. ) ;
#65280 = EDGE_CURVE ( 'NONE', #248032, #68619, #191376, .T. ) ;
#65282 = B_SPLINE_CURVE_WITH_KNOTS ( 'NONE', 3,
 ( #191982, #52425, #35483, #73326, #251923, #72020, #31629, #173730, #32926, #112431, #54983, #111133, #133267, #190702, #13325, #92842, #185846, #152867, #53722, #212813, #34198, #75858 ),
 .UNSPECIFIED., .F., .F.,
 ( 4, 3, 3, 3, 3, 3, 3, 4 ),
 ( 0.000000000000000000, 7.307836821087015899E-06, 4.161455748548358328E-05, 7.576591810648404394E-05, 0.0001098090429817646371, 0.0001438003617351047325, 0.0001777914035423768749, 0.0002117966137402968007 ),
 .UNSPECIFIED. ) ;
#65281 = CARTESIAN_POINT ( 'NONE',  ( -18.59999999999999787, 68.75000000001179501, -81.67310748452436542 ) ) ;
#65283 = DIRECTION ( 'NONE',  ( 0.000000000000000000, 1.000000000000000000, 6.982962677686266711E-15 ) ) ;
#65285 = DIRECTION ( 'NONE',  ( 0.000000000000000000, -6.982962677686266711E-15, 1.000000000000000000 ) ) ;
#65284 = CARTESIAN_POINT ( 'NONE',  ( -22.39999999999999858, 1.115600667400684642E-11, -66.90000000000004832 ) ) ;
#65286 = DIRECTION ( 'NONE',  ( -1.000000000000000000, 0.000000000000000000, 0.000000000000000000 ) ) ;
#65287 = DIRECTION ( 'NONE',  ( 0.000000000000000000, 1.000000000000000000, 0.000000000000000000 ) ) ;
#65288 = DIRECTION ( 'NONE',  ( 1.000000000000000000, 0.000000000000000000, 0.000000000000000000 ) ) ;
#65289 = LINE ( 'NONE', #43168, #74326 ) ;
#65290 = AXIS2_PLACEMENT_3D ( 'NONE', #84201, #196830, #56011 ) ;
#65291 = AXIS2_PLACEMENT_3D ( 'NONE', #178581, #63730, #81978 ) ;
#65292 = VECTOR ( 'NONE', #239977, 1000.000000000000000 ) ;
#65293 = ORIENTED_EDGE ( 'NONE', *, *, #243383, .T. ) ;
#65294 = B_SPLINE_CURVE_WITH_KNOTS ( 'NONE', 3,
 ( #213606, #94941, #153706, #257820, #174549, #134066, #135347, #195364, #16716, #96226, #117091, #98759, #175794, #255252, #194077, #76663, #156242, #178368, #216169, #37564, #196611, #256531, #139186, #79216, #157539, #17970 ),
 .UNSPECIFIED., .F., .F.,
 ( 4, 2, 2, 2, 2, 2, 2, 2, 2, 2, 2, 2, 4 ),
 ( 0.005476422646581359521, 0.006160811967703560058, 0.006845201288825762329, 0.007187395949386863464, 0.007529590609947964600, 0.007871785270509065735, 0.008213979931070168605, 0.008556174591631268006, 0.008898369252192370876, 0.009240563912753472012, 0.009582758573314573147, 0.01026714789443681011, 0.01095153721555904534 ),
 .UNSPECIFIED. ) ;
#65296 = EDGE_LOOP ( 'NONE', ( #62595, #212929, #209921, #102850 ) ) ;
#65295 = ORIENTED_EDGE ( 'NONE', *, *, #219145, .T. ) ;
#65297 = VECTOR ( 'NONE', #98763, 1000.000000000000000 ) ;
#65298 = VERTEX_POINT ( 'NONE', #12736 ) ;
#65299 = CYLINDRICAL_SURFACE ( 'NONE', #249314, 0.8750000000000007772 ) ;
#65300 = CARTESIAN_POINT ( 'NONE',  ( -20.00857864376270001, 52.31097543990284038, -232.5130202284001371 ) ) ;
#65302 = CARTESIAN_POINT ( 'NONE',  ( 21.00000000000000000, 9.750000000011153745, -79.25000000000004263 ) ) ;
#65301 = DIRECTION ( 'NONE',  ( 1.000000000000000000, -0.000000000000000000, -0.000000000000000000 ) ) ;
#65303 = CARTESIAN_POINT ( 'NONE',  ( 21.05000000000000071, 67.18479819544532461, -161.6025699878404396 ) ) ;
#65304 = ORIENTED_EDGE ( 'NONE', *, *, #81759, .T. ) ;
#65305 = CARTESIAN_POINT ( 'NONE',  ( -22.50014994444013894, 11.74971973190330843, -100.4169198432810788 ) ) ;
#65306 = DIRECTION ( 'NONE',  ( 1.000000000000000000, 0.000000000000000000, -1.020425574104004196E-15 ) ) ;
#65307 = CARTESIAN_POINT ( 'NONE',  ( 20.94999999999999574, 59.13236860818124541, -225.8959333647716505 ) ) ;
#65308 = CARTESIAN_POINT ( 'NONE',  ( 21.14999999999999858, 76.10000000001218723, -143.0637644362255401 ) ) ;
#65309 = ORIENTED_EDGE ( 'NONE', *, *, #249459, .T. ) ;
#65310 = AXIS2_PLACEMENT_3D ( 'NONE', #71065, #112741, #154470 ) ;
#65311 = FACE_OUTER_BOUND ( 'NONE', #236544, .T. ) ;
#65312 = VERTEX_POINT ( 'NONE', #210906 ) ;
#65313 = ORIENTED_EDGE ( 'NONE', *, *, #109769, .F. ) ;
#65314 = CARTESIAN_POINT ( 'NONE',  ( 22.59999999999999432, 75.90000000001245439, -181.6726782920691505 ) ) ;
#65315 = CARTESIAN_POINT ( 'NONE',  ( 20.04142135623730070, 31.44980407958351165, -233.5445995079518866 ) ) ;
#65316 = FACE_OUTER_BOUND ( 'NONE', #2070, .T. ) ;
#65317 = CARTESIAN_POINT ( 'NONE',  ( 20.95483826173900255, 67.12383379524162308, -60.97683193162487925 ) ) ;
#65318 = CARTESIAN_POINT ( 'NONE',  ( -21.00000000000000000, 5.021051876504148371E-16, -4.100000000000000533 ) ) ;
#65319 = AXIS2_PLACEMENT_3D ( 'NONE', #21131, #96752, #176346 ) ;
#65320 = DIRECTION ( 'NONE',  ( 1.000000000000000000, 0.000000000000000000, 0.000000000000000000 ) ) ;
#65321 = ORIENTED_EDGE ( 'NONE', *, *, #7854, .T. ) ;
#65322 = LINE ( 'NONE', #241410, #223548 ) ;
#65323 = CARTESIAN_POINT ( 'NONE',  ( -21.07928932188134041, 1.115600667400684642E-11, -134.0000000000000000 ) ) ;
#65324 = CARTESIAN_POINT ( 'NONE',  ( -21.04999999999999716, -0.01465611850199566996, -60.50331341423223108 ) ) ;
#65325 = ADVANCED_FACE ( 'NONE', ( #110514 ), #92231, .F. ) ;
#65327 = DIRECTION ( 'NONE',  ( 0.000000000000000000, 0.9908441862701596881, 0.1350103645451904977 ) ) ;
#65326 = CARTESIAN_POINT ( 'NONE',  ( -23.15000000000000213, -11.74999999998884448, -197.8999999999999773 ) ) ;
#65328 = FACE_OUTER_BOUND ( 'NONE', #154730, .T. ) ;
#65329 = PRESENTATION_STYLE_ASSIGNMENT (( #144859 ) ) ;
#65331 = ADVANCED_FACE ( 'NONE', ( #10142 ), #128814, .T. ) ;
#65330 = CARTESIAN_POINT ( 'NONE',  ( 20.94999999999999929, 76.00000000001244871, -170.0231074845243597 ) ) ;
#65332 = CARTESIAN_POINT ( 'NONE',  ( -21.05000000000000071, 70.10000000001267040, -193.3040077198679967 ) ) ;
#65333 = TOROIDAL_SURFACE ( 'NONE', #11167, 11.65000000000000036, 0.1000000000000000056 ) ;
#65335 = VERTEX_POINT ( 'NONE', #170555 ) ;
#65334 = CARTESIAN_POINT ( 'NONE',  ( 22.00356870067775361, 30.03864867784147918, -252.5169646700140902 ) ) ;
#65336 = VECTOR ( 'NONE', #78096, 1000.000000000000000 ) ;
#65337 = MECHANICAL_DESIGN_GEOMETRIC_PRESENTATION_REPRESENTATION (  '', ( #7067 ), #256818 ) ;
#65338 = EDGE_CURVE ( 'NONE', #57631, #162828, #93519, .T. ) ;
#65339 = EDGE_CURVE ( 'NONE', #108629, #92943, #230474, .T. ) ;
#65340 = TOROIDAL_SURFACE ( 'NONE', #219438, 0.2000000000000000111, 0.1000000000000000056 ) ;
#65341 = DIRECTION ( 'NONE',  ( -1.000000000000000000, -2.952720810173289112E-16, 0.000000000000000000 ) ) ;
#65342 = DIRECTION ( 'NONE',  ( 1.000000000000000000, 2.885090398161910739E-16, 6.283419270304611573E-17 ) ) ;
#65343 = FACE_OUTER_BOUND ( 'NONE', #211892, .T. ) ;
#65344 = ORIENTED_EDGE ( 'NONE', *, *, #146564, .F. ) ;
#65345 = EDGE_CURVE ( 'NONE', #48405, #47449, #56667, .T. ) ;
#65346 = DIRECTION ( 'NONE',  ( -1.000000000000000000, -0.000000000000000000, 0.000000000000000000 ) ) ;
#65348 = ADVANCED_FACE ( 'NONE', ( #149673 ), #33605, .F. ) ;
#65347 = VECTOR ( 'NONE', #100743, 1000.000000000000000 ) ;
#65349 = CARTESIAN_POINT ( 'NONE',  ( 13.40000000000005898, 64.35000000001120668, -18.32310748452479743 ) ) ;
#65350 = AXIS2_PLACEMENT_3D ( 'NONE', #38081, #195872, #115030 ) ;
#65351 = VERTEX_POINT ( 'NONE', #50522 ) ;
#65352 = DIRECTION ( 'NONE',  ( 0.000000000000000000, 0.8814952561688438326, -0.4721928772777330696 ) ) ;
#65355 = ORIENTED_EDGE ( 'NONE', *, *, #175234, .F. ) ;
#65354 = FACE_OUTER_BOUND ( 'NONE', #19290, .T. ) ;
#65353 = AXIS2_PLACEMENT_3D ( 'NONE', #237701, #34388, #76047 ) ;
#65357 = DIRECTION ( 'NONE',  ( 0.000000000000000000, -1.000000000000000000, 0.000000000000000000 ) ) ;
#65356 = CARTESIAN_POINT ( 'NONE',  ( -20.54999999999999716, -8.730841121484170131, -90.90192528101572123 ) ) ;
#65358 =( BOUNDED_CURVE ( )  B_SPLINE_CURVE ( 3, ( #38118, #134607, #133358, #257095 ),
 .UNSPECIFIED., .F., .F. ) 
 B_SPLINE_CURVE_WITH_KNOTS ( ( 4, 4 ),
 ( 1.570796326794895448, 3.141592653589791784 ),
 .UNSPECIFIED. ) 
 CURVE ( )  GEOMETRIC_REPRESENTATION_ITEM ( )  RATIONAL_B_SPLINE_CURVE ( ( 1.000000000000000000, 0.8047378541243650485, 0.8047378541243650485, 1.000000000000000000 ) ) 
 REPRESENTATION_ITEM ( '' )  );
#65359 = TOROIDAL_SURFACE ( 'NONE', #40460, 0.2000000000000000111, 0.1000000000000000056 ) ;
#65360 = CARTESIAN_POINT ( 'NONE',  ( -23.15000000000000213, 1.910280373842936141, -113.1313678551989739 ) ) ;
#65362 = ORIENTED_EDGE ( 'NONE', *, *, #31816, .T. ) ;
#65361 = AXIS2_PLACEMENT_3D ( 'NONE', #60151, #160583, #180129 ) ;
#65363 = CARTESIAN_POINT ( 'NONE',  ( 18.59999999999999076, 6.450000000011156587, -77.01702717044007329 ) ) ;
#65364 = DIRECTION ( 'NONE',  ( 1.000000000000000000, 0.000000000000000000, 0.000000000000000000 ) ) ;
#65365 = CARTESIAN_POINT ( 'NONE',  ( 20.85000000000000142, 7.783179459866048866, -245.3643104511423019 ) ) ;
#65366 = EDGE_CURVE ( 'NONE', #84702, #147965, #139889, .T. ) ;
#65367 = CARTESIAN_POINT ( 'NONE',  ( 20.95512820512820440, 67.12384868372396340, -127.9644784893834100 ) ) ;
#65368 = CARTESIAN_POINT ( 'NONE',  ( 20.97239005616515684, 8.874843841361279573, -179.7501528021531954 ) ) ;
#65369 = ORIENTED_EDGE ( 'NONE', *, *, #1134, .F. ) ;
#65370 = DIRECTION ( 'NONE',  ( -0.000000000000000000, -6.982962677686266711E-15, 1.000000000000000000 ) ) ;
#65371 = ADVANCED_FACE ( 'NONE', ( #133928 ), #107955, .F. ) ;
#65372 = AXIS2_PLACEMENT_3D ( 'NONE', #221760, #139659, #104384 ) ;
#65373 = LINE ( 'NONE', #62807, #143077 ) ;
#65374 = AXIS2_PLACEMENT_3D ( 'NONE', #31693, #192040, #186903 ) ;
#65375 = FACE_BOUND ( 'NONE', #178636, .T. ) ;
#65376 = ORIENTED_EDGE ( 'NONE', *, *, #44090, .F. ) ;
#65377 = EDGE_LOOP ( 'NONE', ( #45448, #247030, #122675, #211819 ) ) ;
#65378 = EDGE_CURVE ( 'NONE', #23758, #192851, #17825, .T. ) ;
#65379 = CARTESIAN_POINT ( 'NONE',  ( 21.14999999999999858, 65.28660755661216797, -124.2731074845243739 ) ) ;
#65380 = EDGE_CURVE ( 'NONE', #103462, #89253, #60789, .T. ) ;
#65381 = DIRECTION ( 'NONE',  ( 1.000000000000000000, -0.000000000000000000, -0.000000000000000000 ) ) ;
#65382 = DIRECTION ( 'NONE',  ( 0.000000000000000000, -1.000000000000000000, -6.982962677686265922E-15 ) ) ;
#65383 = CARTESIAN_POINT ( 'NONE',  ( 21.05000000000000071, 13.06362847850371622, -210.5896934006125889 ) ) ;
#65384 = CARTESIAN_POINT ( 'NONE',  ( 23.14999999999999858, 20.42498087366621817, -235.1829032864613396 ) ) ;
#65385 = VECTOR ( 'NONE', #176570, 999.9999999999998863 ) ;
#65387 = LINE ( 'NONE', #2828, #253513 ) ;
#65386 = CARTESIAN_POINT ( 'NONE',  ( 21.05000000000000071, 9.374458193048763377, -220.5475659691911119 ) ) ;
#65388 = ADVANCED_FACE ( 'NONE', ( #76519 ), #175645, .T. ) ;
#65389 = LINE ( 'NONE', #8000, #119319 ) ;
#65390 = CARTESIAN_POINT ( 'NONE',  ( -16.85312841634287295, 66.08639382269134899, -56.62593435123186936 ) ) ;
#65391 = CARTESIAN_POINT ( 'NONE',  ( -18.59999999999999787, 77.16270174995010223, -128.5231074845242745 ) ) ;
#65392 = FACE_OUTER_BOUND ( 'NONE', #77992, .T. ) ;
#65394 = VERTEX_POINT ( 'NONE', #235591 ) ;
#65393 = CARTESIAN_POINT ( 'NONE',  ( 14.45963434102923273, 62.93961911720151647, -215.5706779233118766 ) ) ;
#65395 = CARTESIAN_POINT ( 'NONE',  ( 20.95520789717937404, 65.42306940062766785, -195.9428745106495739 ) ) ;
#65396 = DIRECTION ( 'NONE',  ( -3.265361837132813093E-16, -1.000000000000000000, -6.982962677686266711E-15 ) ) ;
#65398 = CARTESIAN_POINT ( 'NONE',  ( 20.94999999999999929, 5.000000000011153745, -146.4052660189131245 ) ) ;
#65397 = DIRECTION ( 'NONE',  ( -1.000000000000000000, 0.000000000000000000, -0.000000000000000000 ) ) ;
#65399 = ORIENTED_EDGE ( 'NONE', *, *, #229667, .T. ) ;
#65400 = DIRECTION ( 'NONE',  ( 0.000000000000000000, 0.000000000000000000, -1.000000000000000000 ) ) ;
#65401 = FACE_OUTER_BOUND ( 'NONE', #74777, .T. ) ;
#65402 = ADVANCED_FACE ( 'NONE', ( #197755 ), #135198, .F. ) ;
#65403 = CARTESIAN_POINT ( 'NONE',  ( -21.64999999999999858, 65.95000000001188312, -90.37310748452438247 ) ) ;
#65404 = CARTESIAN_POINT ( 'NONE',  ( -15.69373346032658034, 66.64320997496669463, -186.3182809759104543 ) ) ;
#65405 = ORIENTED_EDGE ( 'NONE', *, *, #236265, .T. ) ;
#65406 = AXIS2_PLACEMENT_3D ( 'NONE', #5834, #26731, #65826 ) ;
#65407 = ORIENTED_EDGE ( 'NONE', *, *, #8759, .T. ) ;
#65408 = EDGE_CURVE ( 'NONE', #249539, #15261, #178225, .T. ) ;
#65409 = VECTOR ( 'NONE', #28818, 1000.000000000000000 ) ;
#65410 = AXIS2_PLACEMENT_3D ( 'NONE', #230492, #192653, #152261 ) ;
#65411 = CYLINDRICAL_SURFACE ( 'NONE', #46967, 0.09999999999999939493 ) ;
#65412 = EDGE_LOOP ( 'NONE', ( #253570, #120239, #225844, #227613 ) ) ;
#65413 = FACE_OUTER_BOUND ( 'NONE', #75835, .T. ) ;
#65414 = EDGE_LOOP ( 'NONE', ( #178449, #76021, #163684, #235784 ) ) ;
#65415 = CIRCLE ( 'NONE', #111208, 0.09999999999999939493 ) ;
#65416 = CARTESIAN_POINT ( 'NONE',  ( -20.94999999999999929, 62.46832465249013921, -225.2232495205141731 ) ) ;
#65417 = SPHERICAL_SURFACE ( 'NONE', #169261, 0.1000000000000000056 ) ;
#65418 = CARTESIAN_POINT ( 'NONE',  ( -23.15000000000000213, 71.75000000001151079, -48.37310748452435405 ) ) ;
#65419 = ORIENTED_EDGE ( 'NONE', *, *, #23237, .F. ) ;
#65420 = DIRECTION ( 'NONE',  ( 1.000000000000000000, 0.000000000000000000, 0.000000000000000000 ) ) ;
#65422 = CIRCLE ( 'NONE', #44212, 0.09999999999999939493 ) ;
#65421 = CARTESIAN_POINT ( 'NONE',  ( -21.04999999999999716, 65.56240296622316066, -242.0762802233569744 ) ) ;
#65423 = FACE_OUTER_BOUND ( 'NONE', #218544, .T. ) ;
#65424 = CIRCLE ( 'NONE', #140426, 0.8750000000000007772 ) ;
#65425 = CARTESIAN_POINT ( 'NONE',  ( -16.77683809663752257, 30.19206623356022234, -234.8041291499450551 ) ) ;
#65426 = DIRECTION ( 'NONE',  ( 1.000000000000000000, 0.000000000000000000, 0.000000000000000000 ) ) ;
#65427 = CYLINDRICAL_SURFACE ( 'NONE', #66440, 0.09999999999999939493 ) ;
#65428 = CARTESIAN_POINT ( 'NONE',  ( 21.07964655665547227, 11.17474170846107029, -211.0746752039685248 ) ) ;
#65429 = ORIENTED_EDGE ( 'NONE', *, *, #99608, .T. ) ;
#65431 = DIRECTION ( 'NONE',  ( 1.000000000000000000, 0.000000000000000000, 0.000000000000000000 ) ) ;
#65430 = CARTESIAN_POINT ( 'NONE',  ( -16.86132326855785735, 66.05000000001209060, -123.8244716998560619 ) ) ;
#65432 = ORIENTED_EDGE ( 'NONE', *, *, #128157, .F. ) ;
#65434 = ORIENTED_EDGE ( 'NONE', *, *, #160897, .F. ) ;
#65433 = CARTESIAN_POINT ( 'NONE',  ( -22.39999999999999858, -1.560176095955062348, -193.3663837337744837 ) ) ;
#65435 = VECTOR ( 'NONE', #147864, 1000.000000000000000 ) ;
#65436 = ORIENTED_EDGE ( 'NONE', *, *, #67944, .T. ) ;
#65437 = DIRECTION ( 'NONE',  ( -1.000000000000000000, -0.000000000000000000, 0.000000000000000000 ) ) ;
#65438 = CARTESIAN_POINT ( 'NONE',  ( -20.64999999999999858, 7.249999999999999112, -12.34999999999999964 ) ) ;
#65439 = FACE_OUTER_BOUND ( 'NONE', #252595, .T. ) ;
#65440 = FACE_OUTER_BOUND ( 'NONE', #213876, .T. ) ;
#65441 = ORIENTED_EDGE ( 'NONE', *, *, #238598, .F. ) ;
#65442 = CARTESIAN_POINT ( 'NONE',  ( 23.14999999999999503, 11.65000000001116298, -193.9851942293460070 ) ) ;
#65443 = CARTESIAN_POINT ( 'NONE',  ( 23.24999999999999289, 11.75000000001116263, -79.15000000000004832 ) ) ;
#65444 = ORIENTED_EDGE ( 'NONE', *, *, #80409, .T. ) ;
#65445 = DIRECTION ( 'NONE',  ( 0.000000000000000000, 0.3738317757009942399, -0.9274965247785252886 ) ) ;
#65446 = ADVANCED_FACE ( 'NONE', ( #15295 ), #123354, .F. ) ;
#65447 = DIRECTION ( 'NONE',  ( 0.000000000000000000, -7.086529944415886769E-15, 1.000000000000000000 ) ) ;
#65448 = CIRCLE ( 'NONE', #44794, 0.1000000000000028644 ) ;
#65449 = ORIENTED_EDGE ( 'NONE', *, *, #210907, .F. ) ;
#65450 = VECTOR ( 'NONE', #179547, 1000.000000000000000 ) ;
#65451 = CARTESIAN_POINT ( 'NONE',  ( -16.83233564386404169, 9.930221796595757766, -146.7754793365243984 ) ) ;
#65452 = CIRCLE ( 'NONE', #69567, 0.1000000000000017680 ) ;
#65453 = ORIENTED_EDGE ( 'NONE', *, *, #59030, .F. ) ;
#65454 = DIRECTION ( 'NONE',  ( 1.000000000000000000, 0.000000000000000000, 0.000000000000000000 ) ) ;
#65455 = ORIENTED_EDGE ( 'NONE', *, *, #222160, .F. ) ;
#65456 =( BOUNDED_SURFACE ( )  B_SPLINE_SURFACE ( 3, 2, ( 
 ( #139195, #42687, #3549 ),
 ( #118388, #141774, #182209 ),
 ( #199203, #23151, #162647 ),
 ( #19276, #123513, #43970 ),
 ( #40156, #20580, #242165 ),
 ( #63521, #222582, #41428 ),
 ( #179651, #955, #200484 ),
 ( #143054, #203035, #24437 ),
 ( #80493, #160093, #120970 ),
 ( #103916, #183489, #178376 ) ),
 .UNSPECIFIED., .F., .F., .T. ) 
 B_SPLINE_SURFACE_WITH_KNOTS ( ( 4, 2, 2, 2, 4 ),
 ( 3, 3 ),
 ( 0.002161241639767781664, 0.002579950749617448968, 0.002789305304542282621, 0.002893982582004699447, 0.002998659859467116707 ),
 ( 0.000000000000000000, 1.000000000000000000 ),
 .UNSPECIFIED. ) 
 GEOMETRIC_REPRESENTATION_ITEM ( )  RATIONAL_B_SPLINE_SURFACE ( (
 ( 1.000000000000000000, 0.7071067811864784058, 1.000000000000000000),
 ( 1.000000000000000000, 0.7632447400667680126, 1.000000000000000000),
 ( 1.000000000000000000, 0.8158073005103720909, 1.000000000000000000),
 ( 1.000000000000000000, 0.8906973462398690700, 1.000000000000000000),
 ( 1.000000000000000000, 0.9149408947801378478, 1.000000000000000000),
 ( 1.000000000000000000, 0.9493368785274739485, 1.000000000000000000),
 ( 1.000000000000000000, 0.9605194247157018417, 1.000000000000000000),
 ( 1.000000000000000000, 0.9803630264780553993, 1.000000000000000000),
 ( 1.000000000000000000, 0.9900844824271457512, 1.000000000000000000),
 ( 1.000000000000000000, 0.9894588281429201881, 1.000000000000000000) ) ) 
 REPRESENTATION_ITEM ( '' )  SURFACE ( )  );
#65457 = EDGE_CURVE ( 'NONE', #129320, #187942, #236882, .T. ) ;
#65458 = DIRECTION ( 'NONE',  ( 3.469446951953515108E-14, 1.000000000000000000, 0.000000000000000000 ) ) ;
#65459 = DIRECTION ( 'NONE',  ( 0.000000000000000000, 0.9126074666063772600, 0.4088369013363274962 ) ) ;
#65460 = LINE ( 'NONE', #126727, #199426 ) ;
#65461 = EDGE_CURVE ( 'NONE', #255780, #95676, #15032, .T. ) ;
#65462 = ADVANCED_FACE ( 'NONE', ( #257667 ), #214751, .F. ) ;
#65463 = CIRCLE ( 'NONE', #73877, 0.1000000000000011990 ) ;
#65464 = VECTOR ( 'NONE', #208403, 1000.000000000000000 ) ;
#65465 = AXIS2_PLACEMENT_3D ( 'NONE', #87796, #186954, #229904 ) ;
#65466 = CARTESIAN_POINT ( 'NONE',  ( -20.85000000000000142, 77.85161776048073534, -91.41991776492061206 ) ) ;
#65467 = CARTESIAN_POINT ( 'NONE',  ( -19.99999999999999645, 4.547418889303921574, 21.90000000000000213 ) ) ;
#65468 = FACE_OUTER_BOUND ( 'NONE', #19907, .T. ) ;
#65469 = ORIENTED_EDGE ( 'NONE', *, *, #55043, .F. ) ;
#65471 = LINE ( 'NONE', #109723, #221108 ) ;
#65470 = CARTESIAN_POINT ( 'NONE',  ( -21.05000000000041993, 69.65527659592207499, -170.0378253410491709 ) ) ;
#65472 = VECTOR ( 'NONE', #142743, 1000.000000000000000 ) ;
#65473 = CARTESIAN_POINT ( 'NONE',  ( -18.50000000000000355, 85.41908450282569731, -163.1931996774988818 ) ) ;
#65474 = ADVANCED_FACE ( 'NONE', ( #75276 ), #189807, .T. ) ;
#65475 = CARTESIAN_POINT ( 'NONE',  ( 21.14999999999999503, -2.598867842139046314, -189.5410128746472083 ) ) ;
#65477 = ORIENTED_EDGE ( 'NONE', *, *, #249965, .T. ) ;
#65476 = DIRECTION ( 'NONE',  ( -1.000000000000000000, 0.000000000000000000, 0.000000000000000000 ) ) ;
#65479 = ORIENTED_EDGE ( 'NONE', *, *, #68190, .T. ) ;
#65478 = DIRECTION ( 'NONE',  ( -3.469446951953352918E-14, -0.4721928772776973204, -0.8814952561688629284 ) ) ;
#65480 = CARTESIAN_POINT ( 'NONE',  ( -20.85000000000000142, 65.66751761918692409, -130.9282609406112670 ) ) ;
#65481 = DIRECTION ( 'NONE',  ( 0.000000000000000000, -1.734723475976810250E-14, 1.000000000000000000 ) ) ;
#65482 = FACE_OUTER_BOUND ( 'NONE', #199288, .T. ) ;
#65483 = CARTESIAN_POINT ( 'NONE',  ( -23.25000000000000000, -1.736705739467587772, -45.01742258762372728 ) ) ;
#65485 = ORIENTED_EDGE ( 'NONE', *, *, #45309, .F. ) ;
#65484 = CARTESIAN_POINT ( 'NONE',  ( -21.55000000000000071, 7.350000000011155166, -188.6499999999999488 ) ) ;
#65486 = AXIS2_PLACEMENT_3D ( 'NONE', #207703, #29096, #181708 ) ;
#65487 = DIRECTION ( 'NONE',  ( 0.000000000000000000, 0.4999999999999543698, 0.8660254037844650199 ) ) ;
#65488 = DIRECTION ( 'NONE',  ( 0.000000000000000000, 0.2617529984164955192, 0.9651348961777178603 ) ) ;
#65489 = VERTEX_POINT ( 'NONE', #37422 ) ;
#65490 = ADVANCED_FACE ( 'NONE', ( #234311 ), #20425, .F. ) ;
#65491 = ORIENTED_EDGE ( 'NONE', *, *, #196890, .F. ) ;
#65492 = CARTESIAN_POINT ( 'NONE',  ( 18.39999999999999503, 11.47316190336248454, -24.25000000000001066 ) ) ;
#65493 = ORIENTED_EDGE ( 'NONE', *, *, #225939, .F. ) ;
#65494 = DIRECTION ( 'NONE',  ( 0.000000000000000000, 0.000000000000000000, -1.000000000000000000 ) ) ;
#65496 = EDGE_CURVE ( 'NONE', #137417, #206232, #48341, .T. ) ;
#65495 = CARTESIAN_POINT ( 'NONE',  ( -20.05000000000000426, 9.250000000011157297, -146.3500000000000227 ) ) ;
#65498 = CIRCLE ( 'NONE', #211269, 0.09999999999999939493 ) ;
#65497 = B_SPLINE_CURVE_WITH_KNOTS ( 'NONE', 3,
 ( #20134, #219589, #239170, #60509, #81341, #180485, #202610, #124368, #541, #203884 ),
 .UNSPECIFIED., .F., .F.,
 ( 4, 2, 2, 2, 4 ),
 ( 5.134898698599272065E-16, 9.930191194498475427E-05, 0.0001986038238894560033, 0.0003972076477783985284, 0.0007944152955562835787 ),
 .UNSPECIFIED. ) ;
#65499 = VERTEX_POINT ( 'NONE', #97339 ) ;
#65500 = AXIS2_PLACEMENT_3D ( 'NONE', #242177, #102640, #63532 ) ;
#65501 = AXIS2_PLACEMENT_3D ( 'NONE', #257978, #117243, #196760 ) ;
#65502 = CARTESIAN_POINT ( 'NONE',  ( 18.59999999999999432, 1.261786168576181755, -41.58649896354548048 ) ) ;
#65503 = PRODUCT_DEFINITION_FORMATION_WITH_SPECIFIED_SOURCE ( 'ANY', '', #49357, .NOT_KNOWN. ) ;
#65504 = EDGE_LOOP ( 'NONE', ( #96502, #161885, #248017, #159014, #157693, #26975, #246026, #54215, #132257, #39009, #121406, #105321 ) ) ;
#65505 = ORIENTED_EDGE ( 'NONE', *, *, #132711, .F. ) ;
#65507 = CARTESIAN_POINT ( 'NONE',  ( -18.41817142474039315, -9.498703066590936217, -73.60396548763712588 ) ) ;
#65506 = AXIS2_PLACEMENT_3D ( 'NONE', #182340, #3675, #117221 ) ;
#65508 = ORIENTED_EDGE ( 'NONE', *, *, #238660, .T. ) ;
#65509 = FACE_OUTER_BOUND ( 'NONE', #179092, .T. ) ;
#65510 = CIRCLE ( 'NONE', #211281, 0.09999999999999520384 ) ;
#65511 = ORIENTED_EDGE ( 'NONE', *, *, #52727, .F. ) ;
#65513 = VERTEX_POINT ( 'NONE', #195225 ) ;
#65512 = DIRECTION ( 'NONE',  ( 0.000000000000000000, 1.000000000000000000, 0.000000000000000000 ) ) ;
#65514 = ORIENTED_EDGE ( 'NONE', *, *, #246424, .T. ) ;
#65515 = EDGE_CURVE ( 'NONE', #172262, #222515, #144000, .T. ) ;
#65516 = DIRECTION ( 'NONE',  ( -3.265361837132813093E-16, -1.000000000000000000, -6.982962677686266711E-15 ) ) ;
#65517 = ORIENTED_EDGE ( 'NONE', *, *, #79196, .F. ) ;
#65519 = ORIENTED_EDGE ( 'NONE', *, *, #159720, .T. ) ;
#65518 = ORIENTED_EDGE ( 'NONE', *, *, #53008, .T. ) ;
#65520 = LINE ( 'NONE', #218158, #23919 ) ;
#65521 = CARTESIAN_POINT ( 'NONE',  ( 18.49999999999999645, 1.637172712981537659, -78.58215336547205254 ) ) ;
#65523 = ORIENTED_EDGE ( 'NONE', *, *, #15540, .F. ) ;
#65522 = AXIS2_PLACEMENT_3D ( 'NONE', #55744, #37518, #32405 ) ;
#65524 = AXIS2_PLACEMENT_3D ( 'NONE', #4591, #24188, #243205 ) ;
#65525 = EDGE_CURVE ( 'NONE', #114775, #225348, #65087, .T. ) ;
#65526 = AXIS2_PLACEMENT_3D ( 'NONE', #6567, #86073, #224332 ) ;
#65527 = EDGE_CURVE ( 'NONE', #44687, #229705, #240065, .T. ) ;
#65528 = VERTEX_POINT ( 'NONE', #213468 ) ;
#65529 = AXIS2_PLACEMENT_3D ( 'NONE', #62614, #182574, #80863 ) ;
#65530 = CARTESIAN_POINT ( 'NONE',  ( -21.05000000000000071, 76.00000000001253397, -181.7231074845243484 ) ) ;
#65531 = CARTESIAN_POINT ( 'NONE',  ( -23.25000000000000000, 1.115600667400684642E-11, -200.9999999999999432 ) ) ;
#65533 = EDGE_LOOP ( 'NONE', ( #40456, #222465, #40784 ) ) ;
#65532 = DIRECTION ( 'NONE',  ( -1.000000000000000000, -0.000000000000000000, -0.000000000000000000 ) ) ;
#65534 = DIRECTION ( 'NONE',  ( 0.000000000000000000, -1.000000000000000000, 0.000000000000000000 ) ) ;
#65535 = ORIENTED_EDGE ( 'NONE', *, *, #146696, .F. ) ;
#65536 = AXIS2_PLACEMENT_3D ( 'NONE', #145995, #67753, #228122 ) ;
#65537 = EDGE_CURVE ( 'NONE', #7336, #3248, #11107, .T. ) ;
#65539 = EDGE_CURVE ( 'NONE', #123398, #132009, #2107, .T. ) ;
#65538 = DIRECTION ( 'NONE',  ( 1.000000000000000000, 0.000000000000000000, 0.000000000000000000 ) ) ;
#65540 = CARTESIAN_POINT ( 'NONE',  ( 18.52928932304161336, 65.72071067697032731, -111.8468540517208112 ) ) ;
#65541 = VERTEX_POINT ( 'NONE', #182056 ) ;
#65542 = CARTESIAN_POINT ( 'NONE',  ( 20.94999999999999574, 8.299331953467152800, -209.2670685529822663 ) ) ;
#65543 = CARTESIAN_POINT ( 'NONE',  ( -20.64999999999999858, 2.000000000011154189, -121.1753780772379230 ) ) ;
#65544 = EDGE_CURVE ( 'NONE', #237980, #246766, #42591, .T. ) ;
#65545 = VERTEX_POINT ( 'NONE', #25555 ) ;
#65546 = CYLINDRICAL_SURFACE ( 'NONE', #155519, 0.9000000000000014655 ) ;
#65547 = EDGE_LOOP ( 'NONE', ( #24883, #179477, #172032 ) ) ;
#65548 = ADVANCED_FACE ( 'NONE', ( #125910 ), #165039, .T. ) ;
#65549 = AXIS2_PLACEMENT_3D ( 'NONE', #196775, #174711, #3712 ) ;
#65552 = ADVANCED_FACE ( 'NONE', ( #224995 ), #162505, .F. ) ;
#65551 = EDGE_CURVE ( 'NONE', #225338, #56627, #252507, .T. ) ;
#65550 = AXIS2_PLACEMENT_3D ( 'NONE', #164057, #148335, #227871 ) ;
#65553 = AXIS2_PLACEMENT_3D ( 'NONE', #88408, #243656, #207111 ) ;
#65555 = ORIENTED_EDGE ( 'NONE', *, *, #176326, .T. ) ;
#65554 = VERTEX_POINT ( 'NONE', #81623 ) ;
#65556 = ORIENTED_EDGE ( 'NONE', *, *, #245805, .T. ) ;
#65557 = CARTESIAN_POINT ( 'NONE',  ( -23.15000000000000213, 1.999999999999998224, -13.22462192276210224 ) ) ;
#65558 = EDGE_LOOP ( 'NONE', ( #198056, #90754, #196003, #138392 ) ) ;
#65559 = FACE_OUTER_BOUND ( 'NONE', #244813, .T. ) ;
#65560 = EDGE_LOOP ( 'NONE', ( #106860, #20857, #113733, #32327 ) ) ;
#65561 = CARTESIAN_POINT ( 'NONE',  ( -16.94878442675511110, 66.00827089702052319, -48.63488790888651891 ) ) ;
#65562 = FACE_OUTER_BOUND ( 'NONE', #150190, .T. ) ;
#65563 = ORIENTED_EDGE ( 'NONE', *, *, #22622, .F. ) ;
#65564 = AXIS2_PLACEMENT_3D ( 'NONE', #255754, #32943, #137140 ) ;
#65565 = EDGE_CURVE ( 'NONE', #117247, #90674, #69382, .T. ) ;
#65566 = CIRCLE ( 'NONE', #98848, 1.500000000000001332 ) ;
#65567 = EDGE_LOOP ( 'NONE', ( #153863, #256972, #76863, #67519 ) ) ;
#65568 = EDGE_CURVE ( 'NONE', #154626, #156652, #210832, .T. ) ;
#65569 = EDGE_CURVE ( 'NONE', #237787, #224923, #142892, .T. ) ;
#65570 = EDGE_LOOP ( 'NONE', ( #135508, #47602, #214715, #238689 ) ) ;
#65571 = EDGE_CURVE ( 'NONE', #258000, #189298, #85471, .T. ) ;
#65572 = CARTESIAN_POINT ( 'NONE',  ( 20.94999999999999574, 1.835341550235569663, -112.0551512925630249 ) ) ;
#65573 = ORIENTED_EDGE ( 'NONE', *, *, #15520, .F. ) ;
#65574 = DIRECTION ( 'NONE',  ( -3.265361837132813093E-16, -0.9651348961777155289, 0.2617529984165037904 ) ) ;
#65576 = ORIENTED_EDGE ( 'NONE', *, *, #158900, .F. ) ;
#65575 = DIRECTION ( 'NONE',  ( 0.000000000000000000, 0.4930308989875230585, 0.8700118002898322711 ) ) ;
#65577 = CARTESIAN_POINT ( 'NONE',  ( 20.85000000000000142, 69.38854649060171198, -247.7638912529787376 ) ) ;
#65578 = DIRECTION ( 'NONE',  ( 0.000000000000000000, 0.000000000000000000, -1.000000000000000000 ) ) ;
#65579 = EDGE_CURVE ( 'NONE', #17245, #154129, #240746, .T. ) ;
#65580 = AXIS2_PLACEMENT_3D ( 'NONE', #206336, #126790, #68101 ) ;
#65581 = FACE_OUTER_BOUND ( 'NONE', #193061, .T. ) ;
#65582 = LINE ( 'NONE', #163412, #65187 ) ;
#65583 = AXIS2_PLACEMENT_3D ( 'NONE', #194508, #94087, #36729 ) ;
#65584 = CARTESIAN_POINT ( 'NONE',  ( -20.64999999999999858, 76.00000000001237765, -170.0231074845243597 ) ) ;
#65586 = CARTESIAN_POINT ( 'NONE',  ( 21.08035267497491105, 6.331706839794169817, -100.4173113752239033 ) ) ;
#65585 = CARTESIAN_POINT ( 'NONE',  ( -21.04999999999999716, -0.08574093702224443170, -60.58617371118707240 ) ) ;
#65588 = AXIS2_PLACEMENT_3D ( 'NONE', #22055, #224074, #2458 ) ;
#65587 = CARTESIAN_POINT ( 'NONE',  ( -20.94999999999999929, 77.83534155023599510, -57.96795619196132776 ) ) ;
#65589 = VECTOR ( 'NONE', #20442, 1000.000000000000000 ) ;
#65590 = DIRECTION ( 'NONE',  ( 2.915501640297154283E-16, 0.9651348961777159730, -0.2617529984165023471 ) ) ;
#65592 = DIRECTION ( 'NONE',  ( -1.000000000000000000, 1.207181226542539700E-16, -2.694675058168174199E-16 ) ) ;
#65591 = VECTOR ( 'NONE', #241850, 1000.000000000000000 ) ;
#65593 = DIRECTION ( 'NONE',  ( 0.000000000000000000, -0.8814952561688430555, 0.4721928772777346239 ) ) ;
#65595 = ORIENTED_EDGE ( 'NONE', *, *, #40051, .F. ) ;
#65594 = CIRCLE ( 'NONE', #207071, 0.09999999999999939493 ) ;
#65597 = ORIENTED_EDGE ( 'NONE', *, *, #214438, .T. ) ;
#65596 = LINE ( 'NONE', #64317, #53237 ) ;
#65598 = EDGE_LOOP ( 'NONE', ( #95938, #45329, #34374, #68327, #219403 ) ) ;
#65599 = DIRECTION ( 'NONE',  ( -0.000000000000000000, 0.4721928772777346239, 0.8814952561688430555 ) ) ;
#65600 = DIRECTION ( 'NONE',  ( 1.000000000000000000, 0.000000000000000000, 0.000000000000000000 ) ) ;
#65601 = ORIENTED_EDGE ( 'NONE', *, *, #99646, .T. ) ;
#65602 = AXIS2_PLACEMENT_3D ( 'NONE', #193712, #254895, #257466 ) ;
#65603 = PRESENTATION_STYLE_ASSIGNMENT (( #225930 ) ) ;
#65604 = FACE_OUTER_BOUND ( 'NONE', #114351, .T. ) ;
#65605 = DIRECTION ( 'NONE',  ( 0.000000000000000000, -1.000000000000000000, -0.000000000000000000 ) ) ;
#65606 = ORIENTED_EDGE ( 'NONE', *, *, #34309, .T. ) ;
#65607 = VECTOR ( 'NONE', #40779, 1000.000000000000000 ) ;
#65608 = DIRECTION ( 'NONE',  ( 0.000000000000000000, 0.2617529984165152257, 0.9651348961777124202 ) ) ;
#65609 = CARTESIAN_POINT ( 'NONE',  ( -18.59999999999999787, -1.162701749938009677, -8.099999999999999645 ) ) ;
#65610 = PLANE ( 'NONE',  #130392 ) ;
#65611 = DIRECTION ( 'NONE',  ( -0.000000000000000000, 0.8660254037844411501, 0.4999999999999956701 ) ) ;
#65613 = ORIENTED_EDGE ( 'NONE', *, *, #81032, .F. ) ;
#65612 = CARTESIAN_POINT ( 'NONE',  ( -16.86132326855785735, 66.05000000001230376, -157.3244716998561046 ) ) ;
#65614 = DIRECTION ( 'NONE',  ( 0.000000000000000000, 0.000000000000000000, -1.000000000000000000 ) ) ;
#65615 = DIRECTION ( 'NONE',  ( 0.000000000000000000, -0.2128009952263603677, 0.9770955615653313941 ) ) ;
#65616 = DIRECTION ( 'NONE',  ( 0.000000000000000000, 0.000000000000000000, 1.000000000000000000 ) ) ;
#65617 = CARTESIAN_POINT ( 'NONE',  ( 21.05000000000000071, 9.863005973831429074, -220.4411654715779321 ) ) ;
#65618 = VERTEX_POINT ( 'NONE', #43826 ) ;
#65619 = CYLINDRICAL_SURFACE ( 'NONE', #127794, 0.1000000000000028644 ) ;
#65620 = EDGE_CURVE ( 'NONE', #164805, #197574, #223285, .T. ) ;
#65622 = CARTESIAN_POINT ( 'NONE',  ( -20.94999999999999929, 68.48451787451661232, -224.2224406095231757 ) ) ;
#65621 = CARTESIAN_POINT ( 'NONE',  ( -23.25000000000000000, 64.25000000001215028, -136.5231074845244166 ) ) ;
#65623 = CARTESIAN_POINT ( 'NONE',  ( -20.94999999999999929, 76.00000000001213607, -136.5231074845243313 ) ) ;
#65624 = CARTESIAN_POINT ( 'NONE',  ( 20.95392731769792150, 40.80464997849164632, -237.9602131893646231 ) ) ;
#65625 = CARTESIAN_POINT ( 'NONE',  ( -23.25000000000000000, 73.40000000001222702, -149.7477294072864709 ) ) ;
#65626 = DIRECTION ( 'NONE',  ( 1.000000000000000000, 0.000000000000000000, 0.000000000000000000 ) ) ;
#65627 = CIRCLE ( 'NONE', #198899, 3.999999999999999112 ) ;
#65628 = AXIS2_PLACEMENT_3D ( 'NONE', #201341, #124386, #202623 ) ;
#65630 = ADVANCED_FACE ( 'NONE', ( #24278 ), #229191, .F. ) ;
#65629 = DIRECTION ( 'NONE',  ( 0.000000000000000000, 0.2617529984165031243, 0.9651348961777157509 ) ) ;
#65631 = CARTESIAN_POINT ( 'NONE',  ( -23.25000000000000000, 71.65000000001222702, -148.8731074845244109 ) ) ;
#65632 = AXIS2_PLACEMENT_3D ( 'NONE', #215119, #116038, #195582 ) ;
#65633 = ORIENTED_EDGE ( 'NONE', *, *, #110515, .F. ) ;
#65634 = PLANE ( 'NONE',  #205729 ) ;
#65635 = ORIENTED_EDGE ( 'NONE', *, *, #153782, .T. ) ;
#65636 = ORIENTED_EDGE ( 'NONE', *, *, #188301, .F. ) ;
#65637 = EDGE_CURVE ( 'NONE', #27458, #167415, #142823, .T. ) ;
#65638 = ADVANCED_FACE ( 'NONE', ( #187204 ), #6820, .T. ) ;
#65639 = SPHERICAL_SURFACE ( 'NONE', #169478, 0.1000000000000000056 ) ;
#65640 = ORIENTED_EDGE ( 'NONE', *, *, #206833, .T. ) ;
#65641 = VERTEX_POINT ( 'NONE', #167640 ) ;
#65642 = CIRCLE ( 'NONE', #211402, 12.97499999999999964 ) ;
#65643 = VECTOR ( 'NONE', #84602, 1000.000000000000000 ) ;
#65644 = ORIENTED_EDGE ( 'NONE', *, *, #39328, .T. ) ;
#65645 = CARTESIAN_POINT ( 'NONE',  ( -17.01825945287482966, 44.09459801588531036, -235.2076708599468020 ) ) ;
#65646 = ORIENTED_EDGE ( 'NONE', *, *, #241465, .T. ) ;
#65647 = EDGE_CURVE ( 'NONE', #79677, #235545, #13675, .T. ) ;
#65648 = CARTESIAN_POINT ( 'NONE',  ( 18.49999999999999645, -1.637172712959225507, -179.0821533654719815 ) ) ;
#65649 = DIRECTION ( 'NONE',  ( 0.000000000000000000, -1.000000000000000000, -0.000000000000000000 ) ) ;
#65650 = AXIS2_PLACEMENT_3D ( 'NONE', #4521, #163618, #243143 ) ;
#65651 = DIRECTION ( 'NONE',  ( 1.000000000000000000, 0.000000000000000000, 0.000000000000000000 ) ) ;
#65652 = EDGE_CURVE ( 'NONE', #111358, #114655, #152614, .T. ) ;
#65653 = DIRECTION ( 'NONE',  ( 0.000000000000000000, 0.4088369013363280513, -0.9126074666063769270 ) ) ;
#65654 = CARTESIAN_POINT ( 'NONE',  ( -21.08078803292166725, 1.583703513802046547, -230.6724956268899689 ) ) ;
#65655 = FACE_OUTER_BOUND ( 'NONE', #25382, .T. ) ;
#65656 = LINE ( 'NONE', #162223, #74430 ) ;
#65658 = ORIENTED_EDGE ( 'NONE', *, *, #31753, .T. ) ;
#65657 = CARTESIAN_POINT ( 'NONE',  ( 21.13461538461538680, 44.29694026544699881, -236.3931290369748126 ) ) ;
#65660 = CARTESIAN_POINT ( 'NONE',  ( -20.94999999999999929, 88.41227409416143246, -72.52310748452423184 ) ) ;
#65659 = CARTESIAN_POINT ( 'NONE',  ( 21.13461538461538325, 67.11458296203758778, -124.1731074845243512 ) ) ;
#65661 = CARTESIAN_POINT ( 'NONE',  ( 23.24999999999999645, 64.25000000001188027, -90.37310748452438247 ) ) ;
#65662 = ORIENTED_EDGE ( 'NONE', *, *, #114300, .T. ) ;
#65663 = PLANE ( 'NONE',  #252713 ) ;
#65664 = CARTESIAN_POINT ( 'NONE',  ( 16.87683809663749557, 14.15900158805613174, -219.2550725561364118 ) ) ;
#65665 = CARTESIAN_POINT ( 'NONE',  ( 20.94999999999999929, 88.41227409416143246, -72.52310748452423184 ) ) ;
#65666 = ORIENTED_EDGE ( 'NONE', *, *, #208756, .F. ) ;
#65668 = CARTESIAN_POINT ( 'NONE',  ( -17.11825945287482753, 9.950000000011138823, -113.2500000000000284 ) ) ;
#65667 = FACE_OUTER_BOUND ( 'NONE', #185529, .T. ) ;
#65669 = EDGE_CURVE ( 'NONE', #28671, #165453, #210594, .T. ) ;
#65670 = CIRCLE ( 'NONE', #198936, 0.9750000000000036415 ) ;
#65671 = DIRECTION ( 'NONE',  ( 0.000000000000000000, -0.000000000000000000, -1.000000000000000000 ) ) ;
#65672 = EDGE_CURVE ( 'NONE', #147965, #186298, #129770, .T. ) ;
#65673 = ORIENTED_EDGE ( 'NONE', *, *, #247804, .F. ) ;
#65674 = VECTOR ( 'NONE', #53984, 1000.000000000000000 ) ;
#65675 = CARTESIAN_POINT ( 'NONE',  ( -18.59999999999999787, 77.83585931145600512, -158.5186683157258187 ) ) ;
#65676 = FACE_OUTER_BOUND ( 'NONE', #236871, .T. ) ;
#65677 = FACE_OUTER_BOUND ( 'NONE', #22405, .T. ) ;
#65678 = ORIENTED_EDGE ( 'NONE', *, *, #177768, .T. ) ;
#65679 = VECTOR ( 'NONE', #17581, 1000.000000000000000 ) ;
#65680 = EDGE_LOOP ( 'NONE', ( #180902, #163328, #103958, #204984 ) ) ;
#65681 = EDGE_CURVE ( 'NONE', #58960, #4697, #209303, .T. ) ;
#65682 = ADVANCED_FACE ( 'NONE', ( #110198 ), #168948, .F. ) ;
#65683 = AXIS2_PLACEMENT_3D ( 'NONE', #22169, #19593, #121291 ) ;
#65684 = CARTESIAN_POINT ( 'NONE',  ( 21.12400222705965547, 67.22148809293476290, -90.77310748452437394 ) ) ;
#65685 = DIRECTION ( 'NONE',  ( 1.000000000000000000, -0.000000000000000000, -0.000000000000000000 ) ) ;
#65686 = DIRECTION ( 'NONE',  ( 0.000000000000000000, 0.4721928772776973204, 0.8814952561688629284 ) ) ;
#65687 = DIRECTION ( 'NONE',  ( 1.000000000000000000, 0.000000000000000000, 0.000000000000000000 ) ) ;
#65689 = CARTESIAN_POINT ( 'NONE',  ( 21.13498764882293557, 6.495618143485025975, -167.4983436052686443 ) ) ;
#65688 = VECTOR ( 'NONE', #181730, 1000.000000000000000 ) ;
#65690 = DIRECTION ( 'NONE',  ( -1.000000000000000000, 0.000000000000000000, 0.000000000000000000 ) ) ;
#65691 = CIRCLE ( 'NONE', #165863, 0.09999999999999063804 ) ;
#65692 = ORIENTED_EDGE ( 'NONE', *, *, #11750, .F. ) ;
#65693 = FACE_OUTER_BOUND ( 'NONE', #37374, .T. ) ;
#65694 = EDGE_CURVE ( 'NONE', #143687, #51386, #90187, .T. ) ;
#65696 = ORIENTED_EDGE ( 'NONE', *, *, #28071, .F. ) ;
#65695 = FACE_OUTER_BOUND ( 'NONE', #161176, .T. ) ;
#65697 = CARTESIAN_POINT ( 'NONE',  ( 21.13461538461538325, 65.38541703798603066, -57.17310748452439384 ) ) ;
#65698 = AXIS2_PLACEMENT_3D ( 'NONE', #42194, #198688, #60447 ) ;
#65699 = DIRECTION ( 'NONE',  ( 0.000000000000000000, 0.000000000000000000, 1.000000000000000000 ) ) ;
#65700 = CARTESIAN_POINT ( 'NONE',  ( -21.14999999999999858, 87.75000000001163869, -66.62310748452424036 ) ) ;
#65701 = DIRECTION ( 'NONE',  ( -0.7071067811865475727, -0.7071067811865475727, 0.000000000000000000 ) ) ;
#65702 = CIRCLE ( 'NONE', #219813, 1.500000000000001332 ) ;
#65703 = CARTESIAN_POINT ( 'NONE',  ( -21.04999999999994387, 67.75000000001118394, -25.49719488170504533 ) ) ;
#65705 = ORIENTED_EDGE ( 'NONE', *, *, #27861, .F. ) ;
#65704 = CARTESIAN_POINT ( 'NONE',  ( -23.25000000000000000, 76.00000000001216449, -140.4231074845243370 ) ) ;
#65707 = DIRECTION ( 'NONE',  ( 0.000000000000000000, 0.2868887416115947775, -0.9579639084728169829 ) ) ;
#65706 = APPLICATION_CONTEXT ( 'automotive_design' ) ;
#65708 = CARTESIAN_POINT ( 'NONE',  ( 21.08750232978087524, 10.72486338602132250, -179.7288581729995371 ) ) ;
#65709 = EDGE_CURVE ( 'NONE', #143962, #20178, #91923, .T. ) ;
#65710 = CARTESIAN_POINT ( 'NONE',  ( -21.14999999999994174, 82.72707916847673459, -26.51159310135756897 ) ) ;
#65711 = DIRECTION ( 'NONE',  ( 0.000000000000000000, 0.2617529984165152257, 0.9651348961777124202 ) ) ;
#65712 = ORIENTED_EDGE ( 'NONE', *, *, #5662, .F. ) ;
#65713 = CARTESIAN_POINT ( 'NONE',  ( -23.49999999999994316, 83.90000000001120384, -34.77310748452479316 ) ) ;
#65714 = CARTESIAN_POINT ( 'NONE',  ( -16.82055514392360607, 66.05000000001200533, -115.6999055590665932 ) ) ;
#65715 = CARTESIAN_POINT ( 'NONE',  ( -18.60000000000000497, 86.99328926435038056, -199.3739562671294721 ) ) ;
#65716 = EDGE_CURVE ( 'NONE', #227485, #84132, #48510, .T. ) ;
#65717 = CARTESIAN_POINT ( 'NONE',  ( -20.94999999999999929, 11.75000000001115552, -174.5148057706539930 ) ) ;
#65718 = AXIS2_PLACEMENT_3D ( 'NONE', #231879, #233164, #16676 ) ;
#65719 = VERTEX_POINT ( 'NONE', #69825 ) ;
#65720 = CARTESIAN_POINT ( 'NONE',  ( -16.84981964351497297, 9.917318234109998798, -87.63039838598058395 ) ) ;
#65721 = CIRCLE ( 'NONE', #107413, 0.1999999999999996503 ) ;
#65722 = ORIENTED_EDGE ( 'NONE', *, *, #101380, .F. ) ;
#65723 = CIRCLE ( 'NONE', #240683, 0.1999999999999987899 ) ;
#65724 = CARTESIAN_POINT ( 'NONE',  ( 22.42357213249528769, 59.79992344103889934, -233.9423457344157953 ) ) ;
#65726 = DIRECTION ( 'NONE',  ( -1.000000000000000000, 0.000000000000000000, 0.000000000000000000 ) ) ;
#65725 = VECTOR ( 'NONE', #128099, 1000.000000000000000 ) ;
#65727 = AXIS2_PLACEMENT_3D ( 'NONE', #59700, #117141, #180965 ) ;
#65728 = EDGE_CURVE ( 'NONE', #60411, #111234, #194304, .T. ) ;
#65729 = CARTESIAN_POINT ( 'NONE',  ( -18.50000000000000000, 47.16152503674118890, -255.1462838189583806 ) ) ;
#65730 = CARTESIAN_POINT ( 'NONE',  ( 18.43565242384934066, -9.519327731081283162, -174.4729763765593020 ) ) ;
#65731 = ORIENTED_EDGE ( 'NONE', *, *, #181461, .T. ) ;
#65732 = AXIS2_PLACEMENT_3D ( 'NONE', #167850, #126107, #229087 ) ;
#65733 = DIRECTION ( 'NONE',  ( -1.000000000000000000, 0.000000000000000000, -0.000000000000000000 ) ) ;
#65734 = CARTESIAN_POINT ( 'NONE',  ( -5.899999999999938183, 64.75000000001119815, -25.92310748452479174 ) ) ;
#65735 = DIRECTION ( 'NONE',  ( 0.000000000000000000, -0.01562499999999307672, 0.9998779222360100194 ) ) ;
#65736 = CARTESIAN_POINT ( 'NONE',  ( -16.80891096016321384, 9.949999999999983302, -20.86766280726859080 ) ) ;
#65737 = AXIS2_PLACEMENT_3D ( 'NONE', #76188, #38366, #137438 ) ;
#65738 = CARTESIAN_POINT ( 'NONE',  ( -23.15000000000000213, 64.25000000001173817, -81.27310748452440237 ) ) ;
#65739 = AXIS2_PLACEMENT_3D ( 'NONE', #137496, #37155, #219607 ) ;
#65740 = EDGE_LOOP ( 'NONE', ( #116859, #10699, #7736, #95573 ) ) ;
#65742 = ORIENTED_EDGE ( 'NONE', *, *, #39666, .F. ) ;
#65741 = CARTESIAN_POINT ( 'NONE',  ( -22.00356870140456422, 7.254242362510445297, -167.4999999999999432 ) ) ;
#65743 = VERTEX_POINT ( 'NONE', #29431 ) ;
#65744 = CARTESIAN_POINT ( 'NONE',  ( -20.54999999999999716, 66.33592547490526670, -222.9197737850312251 ) ) ;
#65745 = ORIENTED_EDGE ( 'NONE', *, *, #142683, .T. ) ;
#65746 = CARTESIAN_POINT ( 'NONE',  ( 21.07954763557365396, 61.10541173128874703, -234.2619947598618069 ) ) ;
#65747 = CARTESIAN_POINT ( 'NONE',  ( -2.995603634470829482E-16, 23.39757462225858475, -255.7770442850471113 ) ) ;
#65748 = DIRECTION ( 'NONE',  ( -0.000000000000000000, -0.8660254037844377084, -0.5000000000000016653 ) ) ;
#65749 = VERTEX_POINT ( 'NONE', #71105 ) ;
#65750 = CYLINDRICAL_SURFACE ( 'NONE', #190724, 0.1000000000000028644 ) ;
#65751 = CARTESIAN_POINT ( 'NONE',  ( -20.64999999999999858, 2.000000000011154189, -113.2246219227621395 ) ) ;
#65752 = CARTESIAN_POINT ( 'NONE',  ( 20.53930447207976684, 8.977148687535432714, -41.94250714157757187 ) ) ;
#65753 = ORIENTED_EDGE ( 'NONE', *, *, #11224, .T. ) ;
#65754 = DIRECTION ( 'NONE',  ( -0.000000000000000000, -0.08413937888704771384, 0.9964539953858891908 ) ) ;
#65755 = CIRCLE ( 'NONE', #211505, 0.1000000000000022815 ) ;
#65757 = ORIENTED_EDGE ( 'NONE', *, *, #47016, .F. ) ;
#65756 = DIRECTION ( 'NONE',  ( -0.000000000000000000, 6.982962677686266711E-15, -1.000000000000000000 ) ) ;
#65758 = CARTESIAN_POINT ( 'NONE',  ( 18.59999999999999076, 7.070967871809997973, -70.74656422186831151 ) ) ;
#65759 = DIRECTION ( 'NONE',  ( 1.000000000000000000, 2.952720810173289112E-16, -0.000000000000000000 ) ) ;
#65760 = AXIS2_PLACEMENT_3D ( 'NONE', #192093, #113815, #94247 ) ;
#65761 = ORIENTED_EDGE ( 'NONE', *, *, #203258, .F. ) ;
#65762 = AXIS2_PLACEMENT_3D ( 'NONE', #68158, #241658, #146388 ) ;
#65763 = CARTESIAN_POINT ( 'NONE',  ( -18.59999999999999787, 64.35000000001205933, -124.3731074845243825 ) ) ;
#65764 = CARTESIAN_POINT ( 'NONE',  ( -21.05000000000000071, 77.85102823015292017, -124.8691942151017855 ) ) ;
#65765 = CARTESIAN_POINT ( 'NONE',  ( -21.64999999999999858, 7.350000000011155166, -188.6499999999999488 ) ) ;
#65766 = ORIENTED_EDGE ( 'NONE', *, *, #144477, .T. ) ;
#65767 = CARTESIAN_POINT ( 'NONE',  ( 21.15000000000005542, 64.35000000001120668, -3.123107484524795474 ) ) ;
#65768 = ADVANCED_FACE ( 'NONE', ( #111499 ), #50219, .F. ) ;
#65769 = LINE ( 'NONE', #224832, #47287 ) ;
#65770 = B_SPLINE_CURVE_WITH_KNOTS ( 'NONE', 3,
 ( #15442, #250189, #94947, #234459, #55793, #135354, #115810, #110673 ),
 .UNSPECIFIED., .F., .F.,
 ( 4, 2, 2, 4 ),
 ( 0.000000000000000000, 9.550056980124818076E-05, 0.0001910011396024963615, 0.0003820022792049927230 ),
 .UNSPECIFIED. ) ;
#65771 = ADVANCED_FACE ( 'NONE', ( #247141 ), #228881, .T. ) ;
#65772 = VERTEX_POINT ( 'NONE', #211898 ) ;
#65773 = EDGE_CURVE ( 'NONE', #186173, #38706, #89346, .T. ) ;
#65774 = CIRCLE ( 'NONE', #211530, 11.80000000000000249 ) ;
#65775 = CIRCLE ( 'NONE', #215784, 0.09999999999998898659 ) ;
#65776 = AXIS2_PLACEMENT_3D ( 'NONE', #31949, #168910, #29392 ) ;
#65777 = ORIENTED_EDGE ( 'NONE', *, *, #207468, .F. ) ;
#65778 = CARTESIAN_POINT ( 'NONE',  ( 21.08804281139604342, 65.37816569817142920, -191.1731075171456098 ) ) ;
#65779 = EDGE_LOOP ( 'NONE', ( #34469, #45060, #38272, #219170, #138057 ) ) ;
#65780 = DIRECTION ( 'NONE',  ( -4.336808689942017736E-16, 0.000000000000000000, -1.000000000000000000 ) ) ;
#65781 = ADVANCED_FACE ( 'NONE', ( #93206 ), #149365, .F. ) ;
#65782 = CARTESIAN_POINT ( 'NONE',  ( -16.96982749440682525, 66.05000000001255955, -183.1478858933352001 ) ) ;
#65784 = ORIENTED_EDGE ( 'NONE', *, *, #180532, .F. ) ;
#65783 = DIRECTION ( 'NONE',  ( 0.000000000000000000, -1.000000000000000000, 0.000000000000000000 ) ) ;
#65785 = LINE ( 'NONE', #107479, #107561 ) ;
#65786 = DIRECTION ( 'NONE',  ( 0.000000000000000000, -1.000000000000000000, -6.982962677686266711E-15 ) ) ;
#65787 = CARTESIAN_POINT ( 'NONE',  ( -18.59999999999999787, 11.75000000001115197, -112.6500000000000341 ) ) ;
#65788 = DIRECTION ( 'NONE',  ( 0.000000000000000000, 0.000000000000000000, -1.000000000000000000 ) ) ;
#65789 = CARTESIAN_POINT ( 'NONE',  ( -18.59999999999999787, 64.35000000001180354, -81.67310748452439384 ) ) ;
#65790 = CARTESIAN_POINT ( 'NONE',  ( -20.94999999999999929, 87.75000000001216449, -139.6231074845242688 ) ) ;
#65791 = AXIS2_PLACEMENT_3D ( 'NONE', #2561, #179944, #101639 ) ;
#65792 = CARTESIAN_POINT ( 'NONE',  ( -18.59999999999999787, 7.021664781911246322, -204.6335654018972434 ) ) ;
#65793 = CARTESIAN_POINT ( 'NONE',  ( -18.49346865148320518, -9.443073798513779593, -107.6851962553148496 ) ) ;
#65795 = EDGE_LOOP ( 'NONE', ( #72544, #225921, #130422, #130242 ) ) ;
#65794 = PLANE ( 'NONE',  #31976 ) ;
#65796 = CARTESIAN_POINT ( 'NONE',  ( 18.79999999999999716, 7.986648289447971116, -1.311673547813416718 ) ) ;
#65797 = ORIENTED_EDGE ( 'NONE', *, *, #256856, .T. ) ;
#65798 = CARTESIAN_POINT ( 'NONE',  ( 21.14999999999999503, 87.65000000001212754, -133.6231074845242119 ) ) ;
#65799 = AXIS2_PLACEMENT_3D ( 'NONE', #185081, #45574, #28632 ) ;
#65800 = DIRECTION ( 'NONE',  ( 0.000000000000000000, -1.000000000000000000, 0.000000000000000000 ) ) ;
#65801 = EDGE_CURVE ( 'NONE', #192844, #21650, #185880, .T. ) ;
#65802 = ADVANCED_FACE ( 'NONE', ( #116630 ), #175349, .T. ) ;
#65803 = CARTESIAN_POINT ( 'NONE',  ( 20.72390388899090041, 65.41003688158858154, -196.0117591887780861 ) ) ;
#65804 = CARTESIAN_POINT ( 'NONE',  ( 18.39999999999999858, 77.42559394857967447, -241.6979299484999615 ) ) ;
#65805 = VERTEX_POINT ( 'NONE', #137460 ) ;
#65806 = LINE ( 'NONE', #206604, #106494 ) ;
#65807 = DIRECTION ( 'NONE',  ( 1.000000000000000000, 0.000000000000000000, 0.000000000000000000 ) ) ;
#65808 = B_SPLINE_CURVE_WITH_KNOTS ( 'NONE', 3,
 ( #243726, #85898, #140776, #205872, #41691, #62524, #121255, #200750, #181204, #2528, #247574, #248865, #168086, #68963, #131479, #31137 ),
 .UNSPECIFIED., .F., .F.,
 ( 4, 3, 3, 3, 3, 4 ),
 ( 0.000000000000000000, 2.209833635978080524E-05, 5.595056164119276626E-05, 8.979992002655378693E-05, 0.0001236482757198913282, 0.0001574984039362987726 ),
 .UNSPECIFIED. ) ;
#65809 = EDGE_CURVE ( 'NONE', #18598, #147011, #254799, .T. ) ;
#65810 = AXIS2_PLACEMENT_3D ( 'NONE', #254587, #14753, #212925 ) ;
#65811 = AXIS2_PLACEMENT_3D ( 'NONE', #231498, #11155, #151977 ) ;
#65812 = EDGE_LOOP ( 'NONE', ( #25576, #49092, #25864, #15155, #162161, #106729 ) ) ;
#65813 = AXIS2_PLACEMENT_3D ( 'NONE', #185950, #227631, #247193 ) ;
#65814 = LINE ( 'NONE', #245746, #130603 ) ;
#65815 = ORIENTED_EDGE ( 'NONE', *, *, #145774, .F. ) ;
#65816 = DIRECTION ( 'NONE',  ( 0.000000000000000000, -1.000000000000000000, 0.000000000000000000 ) ) ;
#65817 = ORIENTED_EDGE ( 'NONE', *, *, #146470, .T. ) ;
#65818 = DIRECTION ( 'NONE',  ( 0.000000000000000000, 6.982962677686266711E-15, -1.000000000000000000 ) ) ;
#65819 = ORIENTED_EDGE ( 'NONE', *, *, #223331, .F. ) ;
#65820 = DIRECTION ( 'NONE',  ( -0.000000000000000000, -1.000000000000000000, -6.982962677686266711E-15 ) ) ;
#65821 = EDGE_CURVE ( 'NONE', #131894, #10114, #97021, .T. ) ;
#65822 = CARTESIAN_POINT ( 'NONE',  ( 15.74999999999999645, 9.350000000011139178, -184.0185689574026071 ) ) ;
#65823 = CIRCLE ( 'NONE', #90957, 0.09999999999998898659 ) ;
#65824 = VERTEX_POINT ( 'NONE', #253558 ) ;
#65826 = DIRECTION ( 'NONE',  ( 0.000000000000000000, 0.000000000000000000, 1.000000000000000000 ) ) ;
#65825 = CIRCLE ( 'NONE', #257490, 12.87499999999999822 ) ;
#65828 = ORIENTED_EDGE ( 'NONE', *, *, #1267, .T. ) ;
#65827 = CARTESIAN_POINT ( 'NONE',  ( 12.84233041328156766, 9.410538608540024441, -48.93268799714088146 ) ) ;
#65829 = DIRECTION ( 'NONE',  ( 0.000000000000000000, -0.2128009952263403282, 0.9770955615653358350 ) ) ;
#65830 = ORIENTED_EDGE ( 'NONE', *, *, #185252, .T. ) ;
#65831 = VECTOR ( 'NONE', #79362, 1000.000000000000000 ) ;
#65832 = EDGE_CURVE ( 'NONE', #59020, #40483, #127637, .T. ) ;
#65833 = ORIENTED_EDGE ( 'NONE', *, *, #21124, .F. ) ;
#65834 = DIRECTION ( 'NONE',  ( 2.710505431213777355E-16, 1.000000000000000000, 6.982962677686266711E-15 ) ) ;
#65835 = FACE_OUTER_BOUND ( 'NONE', #239020, .T. ) ;
#65836 = CARTESIAN_POINT ( 'NONE',  ( -20.94999999999999929, 18.81339837015603322, -226.7756228984618190 ) ) ;
#65837 = ADVANCED_FACE ( 'NONE', ( #77471 ), #37119, .T. ) ;
#65839 = EDGE_CURVE ( 'NONE', #198025, #127762, #56853, .T. ) ;
#65838 = DIRECTION ( 'NONE',  ( -7.304098846218134667E-16, -1.000000000000000000, 0.000000000000000000 ) ) ;
#65840 = CARTESIAN_POINT ( 'NONE',  ( -15.70407651835961005, 66.64419340838244921, -187.2320049529782011 ) ) ;
#65841 = CARTESIAN_POINT ( 'NONE',  ( 20.99999999999999645, 51.70063031245850027, -232.1289905089708441 ) ) ;
#65842 = ORIENTED_EDGE ( 'NONE', *, *, #36759, .F. ) ;
#65843 = CARTESIAN_POINT ( 'NONE',  ( 18.59999999999996945, 68.11287320386161070, -224.1382462126928488 ) ) ;
#65844 = CARTESIAN_POINT ( 'NONE',  ( 22.59080734064468388, 64.25000000001269029, -203.5538571926215070 ) ) ;
#65845 = DIRECTION ( 'NONE',  ( 0.000000000000000000, 0.000000000000000000, -1.000000000000000000 ) ) ;
#65846 = CARTESIAN_POINT ( 'NONE',  ( 21.05000000000000071, 70.10000000001197407, -113.2422072491807086 ) ) ;
#65847 = CIRCLE ( 'NONE', #11712, 0.1000000000000001443 ) ;
#65848 = ORIENTED_EDGE ( 'NONE', *, *, #90270, .F. ) ;
#65849 = CARTESIAN_POINT ( 'NONE',  ( 20.94788355080264353, 68.02921119886117651, -224.2090419302654141 ) ) ;
#65850 = VERTEX_POINT ( 'NONE', #174084 ) ;
#65851 = CARTESIAN_POINT ( 'NONE',  ( 14.56326696814971022, 9.446648990640015953, -115.5891632959232140 ) ) ;
#65852 = TOROIDAL_SURFACE ( 'NONE', #128229, 0.6000000000000013101, 0.1000000000000000056 ) ;
#65853 = ORIENTED_EDGE ( 'NONE', *, *, #187721, .F. ) ;
#65854 = VECTOR ( 'NONE', #248855, 1000.000000000000000 ) ;
#65855 = ADVANCED_FACE ( 'NONE', ( #95760 ), #234002, .F. ) ;
#65856 = ADVANCED_FACE ( 'NONE', ( #76204 ), #214435, .T. ) ;
#65857 = DIRECTION ( 'NONE',  ( 0.000000000000000000, 0.000000000000000000, -1.000000000000000000 ) ) ;
#65858 = DIRECTION ( 'NONE',  ( 0.000000000000000000, 0.000000000000000000, -1.000000000000000000 ) ) ;
#65859 = EDGE_LOOP ( 'NONE', ( #251179, #209050, #102223, #252899 ) ) ;
#65860 = EDGE_LOOP ( 'NONE', ( #214864, #134469, #24484, #152821 ) ) ;
#65862 = ORIENTED_EDGE ( 'NONE', *, *, #187979, .T. ) ;
#65861 = CARTESIAN_POINT ( 'NONE',  ( 20.85000000000000142, 7.668827189579289438, -241.6142244293585009 ) ) ;
#65863 = FACE_OUTER_BOUND ( 'NONE', #22778, .T. ) ;
#65864 = ORIENTED_EDGE ( 'NONE', *, *, #122398, .T. ) ;
#65865 = CIRCLE ( 'NONE', #111655, 0.09999999999999609201 ) ;
#65866 = EDGE_CURVE ( 'NONE', #110678, #242581, #110886, .T. ) ;
#65867 = CARTESIAN_POINT ( 'NONE',  ( -22.41119224318417125, 1.115600667400684642E-11, -21.85042919245520210 ) ) ;
#65868 = CARTESIAN_POINT ( 'NONE',  ( -20.94999999999999929, 0.2561057921033771945, -167.4651035583276553 ) ) ;
#65869 = ORIENTED_EDGE ( 'NONE', *, *, #43213, .T. ) ;
#65870 = ADVANCED_FACE ( 'NONE', ( #38381 ), #56612, .F. ) ;
#65871 = CARTESIAN_POINT ( 'NONE',  ( -18.59999999999999787, 7.128833340094563376, -233.7327013124401276 ) ) ;
#65872 = DIRECTION ( 'NONE',  ( 1.000000000000000000, 1.394253735153569469E-16, 2.602809386958778209E-16 ) ) ;
#65873 = B_SPLINE_CURVE_WITH_KNOTS ( 'NONE', 3,
 ( #172443, #234949, #215368, #175019 ),
 .UNSPECIFIED., .F., .F.,
 ( 4, 4 ),
 ( 0.000000000000000000, 7.713889350927083648E-05 ),
 .UNSPECIFIED. ) ;
#65874 = AXIS2_PLACEMENT_3D ( 'NONE', #22540, #257229, #40836 ) ;
#65875 = VECTOR ( 'NONE', #44499, 1000.000000000000000 ) ;
#65876 = ADVANCED_FACE ( 'NONE', ( #153226 ), #256564, .T. ) ;
#65877 = EDGE_CURVE ( 'NONE', #209971, #240643, #215711, .T. ) ;
#65879 = ORIENTED_EDGE ( 'NONE', *, *, #37060, .T. ) ;
#65878 = CIRCLE ( 'NONE', #186708, 0.09999999999999939493 ) ;
#65881 = SPHERICAL_SURFACE ( 'NONE', #68272, 0.1000000000000000056 ) ;
#65880 = AXIS2_PLACEMENT_3D ( 'NONE', #110932, #170964, #70558 ) ;
#65882 = EDGE_CURVE ( 'NONE', #128006, #85343, #173659, .T. ) ;
#65883 = DIRECTION ( 'NONE',  ( -1.000000000000000000, -0.000000000000000000, -0.000000000000000000 ) ) ;
#65885 = ORIENTED_EDGE ( 'NONE', *, *, #222001, .F. ) ;
#65884 = CARTESIAN_POINT ( 'NONE',  ( 18.44364597020196328, 85.49048731717419969, -95.96512959484043392 ) ) ;
#65886 = EDGE_CURVE ( 'NONE', #193899, #82204, #213157, .T. ) ;
#65887 = CARTESIAN_POINT ( 'NONE',  ( 23.14999999999999858, 76.00000000001244871, -170.0231074845243597 ) ) ;
#65888 = CARTESIAN_POINT ( 'NONE',  ( 23.15000000000000213, 86.43238724539048690, -209.5644480942280836 ) ) ;
#65889 = EDGE_CURVE ( 'NONE', #222470, #230504, #73684, .T. ) ;
#65890 = DIRECTION ( 'NONE',  ( 0.000000000000000000, 0.000000000000000000, 1.000000000000000000 ) ) ;
#65892 = DIRECTION ( 'NONE',  ( 0.000000000000000000, 0.9126074666063770380, 0.4088369013363280513 ) ) ;
#65891 = CARTESIAN_POINT ( 'NONE',  ( -16.93583594267724379, 65.99137656495966553, -90.46371664520363254 ) ) ;
#65893 = CARTESIAN_POINT ( 'NONE',  ( 21.05000000000000071, 39.29335463311362275, -236.8946393634875278 ) ) ;
#65895 = ADVANCED_FACE ( 'NONE', ( #34548 ), #36259, .F. ) ;
#65894 = LINE ( 'NONE', #245823, #35997 ) ;
#65896 = CIRCLE ( 'NONE', #19945, 11.75000000000001066 ) ;
#65897 = DIRECTION ( 'NONE',  ( 0.000000000000000000, 1.000000000000000000, 2.891205793294679805E-16 ) ) ;
#65898 = DIRECTION ( 'NONE',  ( 1.000000000000000000, 0.000000000000000000, 0.000000000000000000 ) ) ;
#65899 = AXIS2_PLACEMENT_3D ( 'NONE', #57532, #134499, #96641 ) ;
#65900 = EDGE_LOOP ( 'NONE', ( #90990, #115809, #18892, #21333 ) ) ;
#65901 = CIRCLE ( 'NONE', #107586, 0.09999999999999939493 ) ;
#65902 = CIRCLE ( 'NONE', #3530, 0.1000000000000028644 ) ;
#65903 = AXIS2_PLACEMENT_3D ( 'NONE', #51681, #172987, #253748 ) ;
#65904 = ORIENTED_EDGE ( 'NONE', *, *, #210925, .T. ) ;
#65905 = CARTESIAN_POINT ( 'NONE',  ( 20.73486653747088937, 68.25000000001149658, -48.67310748452437963 ) ) ;
#65906 = VERTEX_POINT ( 'NONE', #143888 ) ;
#65907 = ADVANCED_FACE ( 'NONE', ( #81318 ), #181982, .T. ) ;
#65908 = AXIS2_PLACEMENT_3D ( 'NONE', #43762, #180716, #104974 ) ;
#65909 = EDGE_CURVE ( 'NONE', #33536, #53603, #152788, .T. ) ;
#65910 = CARTESIAN_POINT ( 'NONE',  ( -20.94999999999999929, 64.25000000001219291, -143.3069731475025321 ) ) ;
#65911 = ORIENTED_EDGE ( 'NONE', *, *, #146857, .T. ) ;
#65912 = SURFACE_SIDE_STYLE ('',( #244534 ) ) ;
#65913 = DIRECTION ( 'NONE',  ( 0.000000000000000000, 6.982962677686266711E-15, -1.000000000000000000 ) ) ;
#65914 = PRODUCT_DEFINITION_SHAPE ( 'NONE', 'NONE',  #97863 ) ;
#65915 = ORIENTED_EDGE ( 'NONE', *, *, #8706, .T. ) ;
#65916 = CARTESIAN_POINT ( 'NONE',  ( -20.54999999999999716, 6.294532028225942710, -220.7845521659012888 ) ) ;
#65917 = ORIENTED_EDGE ( 'NONE', *, *, #136797, .T. ) ;
#65918 = AXIS2_PLACEMENT_3D ( 'NONE', #7465, #86977, #184816 ) ;
#65919 = CIRCLE ( 'NONE', #32655, 0.09999999999998898659 ) ;
#65920 = VERTEX_POINT ( 'NONE', #125613 ) ;
#65921 = LINE ( 'NONE', #46337, #121278 ) ;
#65923 = AXIS2_PLACEMENT_3D ( 'NONE', #162981, #143393, #80834 ) ;
#65922 = DIRECTION ( 'NONE',  ( 0.000000000000000000, 0.2617529984164915779, 0.9651348961777187485 ) ) ;
#65925 = VERTEX_POINT ( 'NONE', #46072 ) ;
#65924 = DIRECTION ( 'NONE',  ( -1.000000000000000000, -0.000000000000000000, -0.000000000000000000 ) ) ;
#65926 = CARTESIAN_POINT ( 'NONE',  ( 19.97071067695831559, 11.72071067696947644, -158.6762534328032075 ) ) ;
#65928 = ORIENTED_EDGE ( 'NONE', *, *, #128534, .F. ) ;
#65927 = CARTESIAN_POINT ( 'NONE',  ( 23.14999999999999858, 67.23127455305835554, -235.8551265064784559 ) ) ;
#65929 = LINE ( 'NONE', #145448, #57967 ) ;
#65930 = DIRECTION ( 'NONE',  ( 0.000000000000000000, -6.982962677686266711E-15, 1.000000000000000000 ) ) ;
#65932 = ORIENTED_EDGE ( 'NONE', *, *, #85034, .F. ) ;
#65931 = DIRECTION ( 'NONE',  ( 1.000000000000000000, 0.000000000000000000, 0.000000000000000000 ) ) ;
#65933 = TOROIDAL_SURFACE ( 'NONE', #157560, 11.90000000000000213, 0.1000000000000000056 ) ;
#65934 = CARTESIAN_POINT ( 'NONE',  ( 18.55807992284871233, 10.32898536001801659, -173.0826683222764757 ) ) ;
#65935 = DIRECTION ( 'NONE',  ( 0.000000000000000000, 0.2617529984165035128, 0.9651348961777155289 ) ) ;
#65936 = CYLINDRICAL_SURFACE ( 'NONE', #140045, 0.1000000000000013933 ) ;
#65937 = ADVANCED_FACE ( 'NONE', ( #242986 ), #255792, .T. ) ;
#65939 = CARTESIAN_POINT ( 'NONE',  ( 21.05000000000000071, 10.30543449102040654, -228.0143625250146329 ) ) ;
#65938 = CARTESIAN_POINT ( 'NONE',  ( -23.25000000000000000, 67.23127455305835554, -235.8551265064784559 ) ) ;
#65940 = CARTESIAN_POINT ( 'NONE',  ( -21.05000000000000071, 69.45934304831114048, -169.9231074845244223 ) ) ;
#65941 = AXIS2_PLACEMENT_3D ( 'NONE', #197202, #38152, #180228 ) ;
#65942 = CARTESIAN_POINT ( 'NONE',  ( 21.03670563405601968, 65.37517631068404000, -157.6975605983152775 ) ) ;
#65943 = ADVANCED_FACE ( 'NONE', ( #42237 ), #186072, .F. ) ;
#65944 = CARTESIAN_POINT ( 'NONE',  ( -18.59999999999999787, -1.835341550213255957, -145.5551512925629822 ) ) ;
#65945 = DIRECTION ( 'NONE',  ( 0.000000000000000000, -0.9999631594459057471, 0.008583690987121077309 ) ) ;
#65946 = ORIENTED_EDGE ( 'NONE', *, *, #135594, .T. ) ;
#65947 = ORIENTED_EDGE ( 'NONE', *, *, #118488, .T. ) ;
#65949 = VERTEX_POINT ( 'NONE', #205132 ) ;
#65948 = AXIS2_PLACEMENT_3D ( 'NONE', #114988, #56283, #164 ) ;
#65950 = ORIENTED_EDGE ( 'NONE', *, *, #18185, .F. ) ;
#65951 = PLANE ( 'NONE',  #101703 ) ;
#65952 = ORIENTED_EDGE ( 'NONE', *, *, #192654, .T. ) ;
#65953 = CARTESIAN_POINT ( 'NONE',  ( 18.59999999999999076, 10.49142135624846439, -91.75000000000005684 ) ) ;
#65954 = LINE ( 'NONE', #43827, #239994 ) ;
#65955 = VECTOR ( 'NONE', #247067, 1000.000000000000000 ) ;
#65956 = AXIS2_PLACEMENT_3D ( 'NONE', #247843, #187886, #190466 ) ;
#65957 = ORIENTED_EDGE ( 'NONE', *, *, #56287, .F. ) ;
#65958 = CARTESIAN_POINT ( 'NONE',  ( 15.74999999999999645, 9.350000000011139178, -150.7500000000000284 ) ) ;
#65959 = EDGE_CURVE ( 'NONE', #118151, #36208, #69564, .T. ) ;
#65960 = AXIS2_PLACEMENT_3D ( 'NONE', #66517, #186467, #245155 ) ;
#65961 = ORIENTED_EDGE ( 'NONE', *, *, #231552, .T. ) ;
#65962 = ORIENTED_EDGE ( 'NONE', *, *, #89946, .F. ) ;
#65963 = VERTEX_POINT ( 'NONE', #123061 ) ;
#65964 = CYLINDRICAL_SURFACE ( 'NONE', #12915, 0.09999999999999999167 ) ;
#65965 = SURFACE_SIDE_STYLE ('',( #247154 ) ) ;
#65966 = CARTESIAN_POINT ( 'NONE',  ( 23.24999999999999289, 11.75000000001116263, -155.7499999999999716 ) ) ;
#65967 = CARTESIAN_POINT ( 'NONE',  ( -21.05000000000000071, 76.00000000001267608, -203.5231074845243597 ) ) ;
#65968 = DIRECTION ( 'NONE',  ( 0.000000000000000000, 0.2128009952263485993, -0.9770955615653341697 ) ) ;
#65969 = CYLINDRICAL_SURFACE ( 'NONE', #246853, 11.74999999999999645 ) ;
#65971 = FACE_OUTER_BOUND ( 'NONE', #210500, .T. ) ;
#65970 = FACE_OUTER_BOUND ( 'NONE', #73545, .T. ) ;
#65972 = CARTESIAN_POINT ( 'NONE',  ( -23.15000000000000213, 74.00000000001259082, -190.2984855617622770 ) ) ;
#65974 = ORIENTED_EDGE ( 'NONE', *, *, #77540, .F. ) ;
#65973 = DIRECTION ( 'NONE',  ( 0.000000000000000000, 2.775557561562812086E-13, -1.000000000000000000 ) ) ;
#65976 = LINE ( 'NONE', #119549, #170850 ) ;
#65975 = CARTESIAN_POINT ( 'NONE',  ( -40.23850191057533010, 87.75000000001119815, -6.023107484524794941 ) ) ;
#65977 = DIRECTION ( 'NONE',  ( 1.000000000000000000, 1.394253735153569469E-16, 2.602809386958778209E-16 ) ) ;
#65978 = ORIENTED_EDGE ( 'NONE', *, *, #101668, .F. ) ;
#65979 = VECTOR ( 'NONE', #89801, 1000.000000000000000 ) ;
#65980 = CARTESIAN_POINT ( 'NONE',  ( -1.739115166359751170E-14, 51.38014393322266216, -230.1906178717505611 ) ) ;
#65981 = FACE_OUTER_BOUND ( 'NONE', #93082, .T. ) ;
#65982 = ORIENTED_EDGE ( 'NONE', *, *, #44984, .F. ) ;
#65983 = CARTESIAN_POINT ( 'NONE',  ( -21.05000000000000071, -11.39257802169451139, -130.9260504201681101 ) ) ;
#65984 = CARTESIAN_POINT ( 'NONE',  ( 20.94999999999999574, -11.64999999998883595, -170.3999999999999773 ) ) ;
#65985 = FACE_OUTER_BOUND ( 'NONE', #226113, .T. ) ;
#65986 = ORIENTED_EDGE ( 'NONE', *, *, #48349, .F. ) ;
#65987 = ORIENTED_EDGE ( 'NONE', *, *, #92267, .F. ) ;
#65988 = CARTESIAN_POINT ( 'NONE',  ( -20.94999999999999929, 68.13014604066189861, -227.7202878558733516 ) ) ;
#65989 = ORIENTED_EDGE ( 'NONE', *, *, #69778, .T. ) ;
#65990 = CARTESIAN_POINT ( 'NONE',  ( -20.85000000000000142, 77.83585931145570669, -125.0186683157258329 ) ) ;
#65991 = CARTESIAN_POINT ( 'NONE',  ( -18.40904629823843663, -9.499999999988851584, -174.1001895624823135 ) ) ;
#65992 = CARTESIAN_POINT ( 'NONE',  ( 18.59999999999999076, 11.65000000001115943, -58.35000000000000142 ) ) ;
#65993 = ORIENTED_EDGE ( 'NONE', *, *, #52388, .F. ) ;
#65994 = EDGE_CURVE ( 'NONE', #132474, #148485, #119445, .T. ) ;
#65995 = CARTESIAN_POINT ( 'NONE',  ( -18.50000000000000000, 9.350000000011156942, -121.6500000000000341 ) ) ;
#65996 = CARTESIAN_POINT ( 'NONE',  ( -20.94999999999999929, 76.00000000001213607, -136.5231074845243313 ) ) ;
#65997 = ADVANCED_FACE ( 'NONE', ( #244264 ), #179203, .T. ) ;
#65998 = CARTESIAN_POINT ( 'NONE',  ( 18.59999999999999787, -1.835341550224411922, -11.55515129256297868 ) ) ;
#65999 = TOROIDAL_SURFACE ( 'NONE', #211755, 2.100000000000002309, 0.1000000000000000056 ) ;
#66000 = CARTESIAN_POINT ( 'NONE',  ( -23.15000000000000213, -9.500000000000001776, -23.60603087734756045 ) ) ;
#66001 = VECTOR ( 'NONE', #60432, 1000.000000000000000 ) ;
#66002 = CIRCLE ( 'NONE', #178460, 0.1000000000000124678 ) ;
#66003 = ORIENTED_EDGE ( 'NONE', *, *, #186700, .T. ) ;
#66004 = CARTESIAN_POINT ( 'NONE',  ( -20.64999999999999858, 4.350000000011156054, -54.65000000000000568 ) ) ;
#66005 = EDGE_CURVE ( 'NONE', #11718, #97145, #140256, .T. ) ;
#66007 = ORIENTED_EDGE ( 'NONE', *, *, #254488, .T. ) ;
#66006 = DIRECTION ( 'NONE',  ( -0.000000000000000000, -0.9126074666063769270, -0.4088369013363282733 ) ) ;
#66008 = CIRCLE ( 'NONE', #86832, 4.049999999999998934 ) ;
#66009 = DIRECTION ( 'NONE',  ( -0.000000000000000000, 0.000000000000000000, 1.000000000000000000 ) ) ;
#66010 = CARTESIAN_POINT ( 'NONE',  ( 20.94999999999999929, 11.65000000000000391, -33.50000000000000000 ) ) ;
#66011 = CARTESIAN_POINT ( 'NONE',  ( 22.50000000000000000, 33.39917768972755141, -242.5193385251796769 ) ) ;
#66012 = ADVANCED_FACE ( 'NONE', ( #224703 ), #112654, .T. ) ;
#66013 = DIRECTION ( 'NONE',  ( 1.000000000000000000, 0.000000000000000000, 0.000000000000000000 ) ) ;
#66014 = DIRECTION ( 'NONE',  ( -0.000000000000000000, 0.000000000000000000, 1.000000000000000000 ) ) ;
#66015 = DIRECTION ( 'NONE',  ( 0.000000000000000000, -1.000000000000000000, 0.000000000000000000 ) ) ;
#66016 = ORIENTED_EDGE ( 'NONE', *, *, #79162, .T. ) ;
#66017 = FACE_OUTER_BOUND ( 'NONE', #47229, .T. ) ;
#66018 = DIRECTION ( 'NONE',  ( 0.000000000000000000, -1.000000000000000000, -6.982962677686266711E-15 ) ) ;
#66019 = CIRCLE ( 'NONE', #203573, 0.09999999999999939493 ) ;
#66020 = DIRECTION ( 'NONE',  ( 2.465190328815662439E-32, -0.2617529984165030132, -0.9651348961777158619 ) ) ;
#66021 = CIRCLE ( 'NONE', #228349, 11.75000000000000000 ) ;
#66022 = EDGE_CURVE ( 'NONE', #79682, #106008, #102846, .T. ) ;
#66023 = DIRECTION ( 'NONE',  ( 0.000000000000000000, 0.1350103645451904977, -0.9908441862701596881 ) ) ;
#66024 = CIRCLE ( 'NONE', #224240, 4.149999999999987033 ) ;
#66025 = ORIENTED_EDGE ( 'NONE', *, *, #103594, .F. ) ;
#66026 = ORIENTED_EDGE ( 'NONE', *, *, #240596, .T. ) ;
#66027 = SPHERICAL_SURFACE ( 'NONE', #113487, 0.1000000000000000056 ) ;
#66028 = CARTESIAN_POINT ( 'NONE',  ( 21.00023020733501866, 1.115539681028482333E-11, -127.6091307547316518 ) ) ;
#66029 = EDGE_CURVE ( 'NONE', #100678, #149751, #231890, .T. ) ;
#66030 = DIRECTION ( 'NONE',  ( -0.000000000000000000, 0.8814952561688430555, -0.4721928772777346239 ) ) ;
#66031 = CARTESIAN_POINT ( 'NONE',  ( -20.85000000000000142, 87.75000000001142553, -36.02310748452423894 ) ) ;
#66032 = LINE ( 'NONE', #225085, #125738 ) ;
#66033 = CARTESIAN_POINT ( 'NONE',  ( -20.99749315643146730, 17.11694853957537887, -224.3781540366317131 ) ) ;
#66034 = AXIS2_PLACEMENT_3D ( 'NONE', #71127, #88068, #150645 ) ;
#66035 = TOROIDAL_SURFACE ( 'NONE', #11908, 3.899999999999999467, 0.1000000000000000056 ) ;
#66036 = VECTOR ( 'NONE', #49048, 1000.000000000000000 ) ;
#66037 = ORIENTED_EDGE ( 'NONE', *, *, #114851, .T. ) ;
#66038 = DIRECTION ( 'NONE',  ( 1.000000000000000000, -0.000000000000000000, 0.000000000000000000 ) ) ;
#66039 = ORIENTED_EDGE ( 'NONE', *, *, #58530, .T. ) ;
#66040 = DIRECTION ( 'NONE',  ( 0.000000000000000000, 0.2128009952263403282, -0.9770955615653358350 ) ) ;
#66041 = AXIS2_PLACEMENT_3D ( 'NONE', #54370, #234284, #50500 ) ;
#66042 = FACE_OUTER_BOUND ( 'NONE', #200834, .T. ) ;
#66043 = DIRECTION ( 'NONE',  ( 0.000000000000000000, 0.008583690987127922528, 0.9999631594459055250 ) ) ;
#66044 = CARTESIAN_POINT ( 'NONE',  ( 21.05000000000000071, 28.08470566095357057, -239.2860081655328770 ) ) ;
#66045 = DIRECTION ( 'NONE',  ( 0.000000000000000000, 0.000000000000000000, -1.000000000000000000 ) ) ;
#66046 = DIRECTION ( 'NONE',  ( -6.938893903907224433E-15, 1.000000000000000000, 0.000000000000000000 ) ) ;
#66047 = DIRECTION ( 'NONE',  ( 0.000000000000000000, 0.9908441862701596881, -0.1350103645451904977 ) ) ;
#66048 = CARTESIAN_POINT ( 'NONE',  ( -22.00356870142746146, 7.254242362487302032, -67.00000000000005684 ) ) ;
#66049 = LINE ( 'NONE', #148156, #192284 ) ;
#66050 = CARTESIAN_POINT ( 'NONE',  ( -20.85000000000000142, 70.17424292862648372, -198.1782849070719124 ) ) ;
#66051 = CARTESIAN_POINT ( 'NONE',  ( 20.94999999999999929, 86.19075908668452257, -209.4719249499869136 ) ) ;
#66052 = AXIS2_PLACEMENT_3D ( 'NONE', #123904, #164314, #132554 ) ;
#66053 = CIRCLE ( 'NONE', #111871, 11.75000000000000178 ) ;
#66054 = AXIS2_PLACEMENT_3D ( 'NONE', #88556, #112008, #109408 ) ;
#66055 = FACE_OUTER_BOUND ( 'NONE', #130165, .T. ) ;
#66056 = CARTESIAN_POINT ( 'NONE',  ( 21.05000000000000071, 8.926614585098256782, -175.9716830192231214 ) ) ;
#66057 = ADVANCED_FACE ( 'NONE', ( #10815 ), #109891, .T. ) ;
#66058 = AXIS2_PLACEMENT_3D ( 'NONE', #190177, #87190, #251421 ) ;
#66059 = ORIENTED_EDGE ( 'NONE', *, *, #98520, .F. ) ;
#66060 = CARTESIAN_POINT ( 'NONE',  ( -23.25000000000000355, 11.75000000001113953, -113.1500000000000341 ) ) ;
#66061 = CARTESIAN_POINT ( 'NONE',  ( -20.85000000000000142, -11.74999999998884448, -100.5000000000000426 ) ) ;
#66062 = EDGE_CURVE ( 'NONE', #16906, #53843, #165220, .T. ) ;
#66063 = EDGE_LOOP ( 'NONE', ( #104711, #207296, #202304, #31699 ) ) ;
#66064 = CARTESIAN_POINT ( 'NONE',  ( -16.94052228080550648, 51.64087742373390455, -231.8968528649357950 ) ) ;
#66065 = CARTESIAN_POINT ( 'NONE',  ( 21.12400222705969099, 11.18425721308768850, -211.1013445587443869 ) ) ;
#66066 = CIRCLE ( 'NONE', #232683, 0.09999999999998898659 ) ;
#66067 = AXIS2_PLACEMENT_3D ( 'NONE', #83623, #241463, #218017 ) ;
#66068 = CARTESIAN_POINT ( 'NONE',  ( -17.01825945287481545, 66.05000000001182059, -82.27310748452437394 ) ) ;
#66069 = EDGE_CURVE ( 'NONE', #110700, #204714, #244317, .T. ) ;
#66070 = VERTEX_POINT ( 'NONE', #147761 ) ;
#66071 = EDGE_CURVE ( 'NONE', #99579, #80509, #149170, .T. ) ;
#66072 = CARTESIAN_POINT ( 'NONE',  ( -21.05000000000000071, 87.65000000001212754, -133.6231074845242119 ) ) ;
#66073 = CIRCLE ( 'NONE', #45229, 0.09999999999999939493 ) ;
#66074 = EDGE_LOOP ( 'NONE', ( #5491, #156169, #90225, #170499 ) ) ;
#66075 = AXIS2_PLACEMENT_3D ( 'NONE', #167013, #127859, #207403 ) ;
#66076 = CIRCLE ( 'NONE', #115995, 0.3999999999999975797 ) ;
#66077 = CIRCLE ( 'NONE', #16229, 0.5000000000000004441 ) ;
#66078 = AXIS2_PLACEMENT_3D ( 'NONE', #255405, #175953, #215050 ) ;
#66079 = CARTESIAN_POINT ( 'NONE',  ( 21.05000000000000071, 76.00000000001143974, -38.02310748452432421 ) ) ;
#66080 =( BOUNDED_CURVE ( )  B_SPLINE_CURVE ( 3, ( #37417, #19116, #2103, #238152 ),
 .UNSPECIFIED., .F., .F. ) 
 B_SPLINE_CURVE_WITH_KNOTS ( ( 4, 4 ),
 ( 4.712388980384689674, 5.672655318024514060 ),
 .UNSPECIFIED. ) 
 CURVE ( )  GEOMETRIC_REPRESENTATION_ITEM ( )  RATIONAL_B_SPLINE_CURVE ( ( 1.000000000000000000, 0.9246222802177627154, 0.9246222802177627154, 1.000000000000000000 ) ) 
 REPRESENTATION_ITEM ( '' )  );
#66081 = EDGE_LOOP ( 'NONE', ( #162132, #634, #176121, #200103, #219346, #74776, #255012, #229960, #138290, #36724, #54669, #48598 ) ) ;
#66082 = ADVANCED_FACE ( 'NONE', ( #250693 ), #9513, .F. ) ;
#66083 = CARTESIAN_POINT ( 'NONE',  ( -18.50000000000000000, 23.42819724844703444, -229.2476443247244902 ) ) ;
#66084 = CARTESIAN_POINT ( 'NONE',  ( 22.40000000000020819, -0.1008583690885111045, -21.75043287651029900 ) ) ;
#66085 = CARTESIAN_POINT ( 'NONE',  ( 18.79999999999999716, -1.212568896937008089, -7.800000000000000711 ) ) ;
#66087 = CARTESIAN_POINT ( 'NONE',  ( 11.60000000000006004, 67.72071067812984779, -24.99381816264344991 ) ) ;
#66086 = UNCERTAINTY_MEASURE_WITH_UNIT (LENGTH_MEASURE( 1.000000000000000082E-05 ), #179460, 'distance_accuracy_value', 'NONE');
#66088 = EDGE_CURVE ( 'NONE', #128297, #102889, #151634, .T. ) ;
#66089 = CARTESIAN_POINT ( 'NONE',  ( -22.47071067811865319, 68.27992525551461256, -203.6221999392270448 ) ) ;
#66090 = LINE ( 'NONE', #187341, #72516 ) ;
#66091 = CARTESIAN_POINT ( 'NONE',  ( -20.99142135623731065, 11.60000000001115161, -194.0717967697245001 ) ) ;
#66092 = DIRECTION ( 'NONE',  ( 0.000000000000000000, 0.000000000000000000, -1.000000000000000000 ) ) ;
#66093 = CARTESIAN_POINT ( 'NONE',  ( -18.50000000000000000, 68.87972903831409610, -65.86354444268502561 ) ) ;
#66095 = VERTEX_POINT ( 'NONE', #211585 ) ;
#66094 = DIRECTION ( 'NONE',  ( -1.000000000000000000, -0.000000000000000000, -0.000000000000000000 ) ) ;
#66096 = ORIENTED_EDGE ( 'NONE', *, *, #244084, .T. ) ;
#66098 = CARTESIAN_POINT ( 'NONE',  ( -21.14999999999999858, 64.35000000001214460, -136.4231074845243938 ) ) ;
#66097 = DIRECTION ( 'NONE',  ( 0.000000000000000000, 0.000000000000000000, -1.000000000000000000 ) ) ;
#66100 = ORIENTED_EDGE ( 'NONE', *, *, #173563, .F. ) ;
#66099 = LINE ( 'NONE', #29578, #63618 ) ;
#66101 = ORIENTED_EDGE ( 'NONE', *, *, #229858, .T. ) ;
#66102 = CARTESIAN_POINT ( 'NONE',  ( -20.65000000000000568, 53.37686160793744961, -235.8706811220569932 ) ) ;
#66103 = AXIS2_PLACEMENT_3D ( 'NONE', #108821, #206650, #163677 ) ;
#66104 = CIRCLE ( 'NONE', #136837, 0.09999999999999971412 ) ;
#66105 = CARTESIAN_POINT ( 'NONE',  ( 20.96937028524355640, 10.62446937163783289, -174.9914261011695373 ) ) ;
#66106 = CIRCLE ( 'NONE', #211869, 0.9750000000000036415 ) ;
#66108 = EDGE_CURVE ( 'NONE', #16613, #154602, #15405, .T. ) ;
#66107 = LINE ( 'NONE', #45263, #188158 ) ;
#66109 = DIRECTION ( 'NONE',  ( 1.000000000000000000, 0.000000000000000000, -0.000000000000000000 ) ) ;
#66110 = ADVANCED_FACE ( 'NONE', ( #6948 ), #235001, .F. ) ;
#66111 = ADVANCED_FACE ( 'NONE', ( #56334 ), #15978, .F. ) ;
#66112 = CARTESIAN_POINT ( 'NONE',  ( -18.54148534481894472, 67.49261718274587452, -195.4446851895584416 ) ) ;
#66113 = DIRECTION ( 'NONE',  ( -0.000000000000000000, 1.000000000000000000, -0.000000000000000000 ) ) ;
#66114 = AXIS2_PLACEMENT_3D ( 'NONE', #250396, #224714, #146457 ) ;
#66115 = AXIS2_PLACEMENT_3D ( 'NONE', #49754, #249251, #230985 ) ;
#66116 = CARTESIAN_POINT ( 'NONE',  ( -23.15000000000000213, -4.756823075239756449, -233.1486023682345490 ) ) ;
#66117 = ORIENTED_EDGE ( 'NONE', *, *, #36017, .F. ) ;
#66118 = EDGE_LOOP ( 'NONE', ( #56921, #27658, #180810, #133286 ) ) ;
#66119 = DIRECTION ( 'NONE',  ( 1.000000000000000000, 0.000000000000000000, 0.000000000000000000 ) ) ;
#66120 = TOROIDAL_SURFACE ( 'NONE', #207608, 11.65000000000000036, 0.1000000000000000056 ) ;
#66121 = ORIENTED_EDGE ( 'NONE', *, *, #223024, .F. ) ;
#66122 = CARTESIAN_POINT ( 'NONE',  ( 21.05000000000000071, -0.01454569055822367736, -27.00298221356814565 ) ) ;
#66123 = VERTEX_POINT ( 'NONE', #95474 ) ;
#66124 = CARTESIAN_POINT ( 'NONE',  ( -16.79140778683508728, 9.944941598865716159, -154.8297372337707998 ) ) ;
#66125 = CIRCLE ( 'NONE', #78595, 0.09999999999999693856 ) ;
#66126 = CARTESIAN_POINT ( 'NONE',  ( 23.14999999999999858, 76.00000000001213607, -136.5231074845243313 ) ) ;
#66127 = DIRECTION ( 'NONE',  ( -1.000000000000000000, 0.000000000000000000, 0.000000000000000000 ) ) ;
#66128 = CARTESIAN_POINT ( 'NONE',  ( -16.85718274719361176, 22.91402687719062570, -230.8711018400638864 ) ) ;
#66129 = VERTEX_POINT ( 'NONE', #133330 ) ;
#66130 = CARTESIAN_POINT ( 'NONE',  ( 19.97071067811865674, 11.72071067812981759, -125.2085786437627206 ) ) ;
#66131 = ORIENTED_EDGE ( 'NONE', *, *, #138148, .T. ) ;
#66132 = CARTESIAN_POINT ( 'NONE',  ( -16.90138253750127362, 66.05000000001155058, -48.81154477661981161 ) ) ;
#66133 = AXIS2_PLACEMENT_3D ( 'NONE', #121222, #181172, #42933 ) ;
#66135 = LINE ( 'NONE', #225185, #185672 ) ;
#66134 = CIRCLE ( 'NONE', #136873, 0.09999999999998898659 ) ;
#66136 = EDGE_CURVE ( 'NONE', #154949, #40168, #197137, .T. ) ;
#66137 = CARTESIAN_POINT ( 'NONE',  ( 18.39999999999999503, 70.35000000001207354, -123.8731074845243398 ) ) ;
#66138 = CIRCLE ( 'NONE', #37125, 4.049999999999998046 ) ;
#66139 = FACE_OUTER_BOUND ( 'NONE', #63524, .T. ) ;
#66140 = ORIENTED_EDGE ( 'NONE', *, *, #108909, .T. ) ;
#66141 = CARTESIAN_POINT ( 'NONE',  ( -18.50000000000000000, 64.35000000001157616, -57.27310748452440237 ) ) ;
#66142 = EDGE_LOOP ( 'NONE', ( #92439, #223344, #163623, #134094, #228664 ) ) ;
#66145 = ORIENTED_EDGE ( 'NONE', *, *, #43515, .F. ) ;
#66144 = CARTESIAN_POINT ( 'NONE',  ( 18.57399277249656322, 46.46487552657982434, -243.0839400145317200 ) ) ;
#66143 = CARTESIAN_POINT ( 'NONE',  ( 18.41789779300711771, 46.96039426765801039, -255.3459640616293598 ) ) ;
#66146 = DIRECTION ( 'NONE',  ( 0.000000000000000000, 0.000000000000000000, -1.000000000000000000 ) ) ;
#66147 = ORIENTED_EDGE ( 'NONE', *, *, #202714, .T. ) ;
#66148 = CARTESIAN_POINT ( 'NONE',  ( -21.05000000000000071, 32.73471231533735448, -251.3091613769916535 ) ) ;
#66149 = ORIENTED_EDGE ( 'NONE', *, *, #37379, .T. ) ;
#66150 = CARTESIAN_POINT ( 'NONE',  ( 18.59999999999999432, -1.261786168565025568, -8.086498963545480478 ) ) ;
#66151 = EDGE_CURVE ( 'NONE', #119315, #188675, #48686, .T. ) ;
#66152 = FACE_BOUND ( 'NONE', #138497, .T. ) ;
#66153 = CARTESIAN_POINT ( 'NONE',  ( -16.77683809663752257, 9.950000000011138823, -121.3500000000000369 ) ) ;
#66154 =( BOUNDED_CURVE ( )  B_SPLINE_CURVE ( 3, ( #198336, #22294, #157978, #19719 ),
 .UNSPECIFIED., .F., .F. ) 
 B_SPLINE_CURVE_WITH_KNOTS ( ( 4, 4 ),
 ( 4.712388980384690562, 6.283185307179586232 ),
 .UNSPECIFIED. ) 
 CURVE ( )  GEOMETRIC_REPRESENTATION_ITEM ( )  RATIONAL_B_SPLINE_CURVE ( ( 1.000000000000000000, 0.8047378541243652705, 0.8047378541243652705, 1.000000000000000000 ) ) 
 REPRESENTATION_ITEM ( '' )  );
#66155 = LINE ( 'NONE', #124853, #60176 ) ;
#66156 = CIRCLE ( 'NONE', #219701, 0.1000000000000002554 ) ;
#66157 = EDGE_CURVE ( 'NONE', #15171, #252227, #194474, .T. ) ;
#66158 = CARTESIAN_POINT ( 'NONE',  ( -23.15000000000000213, 54.34471204062663219, -239.4366250215122420 ) ) ;
#66159 = ORIENTED_EDGE ( 'NONE', *, *, #66866, .F. ) ;
#66160 = ADVANCED_FACE ( 'NONE', ( #92899 ), #127825, .F. ) ;
#66161 = CARTESIAN_POINT ( 'NONE',  ( -17.71734398241074970, 15.53635165935942375, -221.3859150949375589 ) ) ;
#66162 = SURFACE_SIDE_STYLE ('',( #223933 ) ) ;
#66163 = CARTESIAN_POINT ( 'NONE',  ( -18.39999999999999503, -9.499999999988851584, -140.6001893912220737 ) ) ;
#66164 = EDGE_LOOP ( 'NONE', ( #148657, #157346, #162899, #132254 ) ) ;
#66165 = CARTESIAN_POINT ( 'NONE',  ( -18.59999999999999787, 64.35000000001157616, -57.37310748452440379 ) ) ;
#66166 = ORIENTED_EDGE ( 'NONE', *, *, #66804, .T. ) ;
#66167 = DIRECTION ( 'NONE',  ( -1.000000000000000000, 0.000000000000000000, 0.000000000000000000 ) ) ;
#66168 = EDGE_CURVE ( 'NONE', #176862, #238954, #57045, .T. ) ;
#66169 = EDGE_CURVE ( 'NONE', #172794, #79018, #115329, .T. ) ;
#66170 = DIRECTION ( 'NONE',  ( -1.000000000000000000, 0.000000000000000000, -0.000000000000000000 ) ) ;
#66171 = CARTESIAN_POINT ( 'NONE',  ( 21.05315837413339253, 36.17631400070159486, -235.9630178772347051 ) ) ;
#66173 = ORIENTED_EDGE ( 'NONE', *, *, #176052, .F. ) ;
#66172 = CARTESIAN_POINT ( 'NONE',  ( 20.46382478191415188, 10.59862044130854031, -141.6778144693454919 ) ) ;
#66174 = DIRECTION ( 'NONE',  ( 1.000000000000000000, 0.000000000000000000, 0.000000000000000000 ) ) ;
#66175 = CARTESIAN_POINT ( 'NONE',  ( -15.66061380678751824, 62.72888572355476811, -216.6946536606585028 ) ) ;
#66176 = CARTESIAN_POINT ( 'NONE',  ( 22.60000000000000142, 0.1008583691098682150, -55.25043287651065782 ) ) ;
#66177 = VERTEX_POINT ( 'NONE', #254523 ) ;
#66178 = TOROIDAL_SURFACE ( 'NONE', #99298, 7.800000000000000711, 0.1000000000000000056 ) ;
#66180 = CIRCLE ( 'NONE', #99470, 0.1000000000000001305 ) ;
#66179 = CARTESIAN_POINT ( 'NONE',  ( 20.09999999999999787, 9.750000000011137757, -76.25000000000004263 ) ) ;
#66181 = FACE_OUTER_BOUND ( 'NONE', #107917, .T. ) ;
#66182 = ORIENTED_EDGE ( 'NONE', *, *, #257148, .F. ) ;
#66183 = AXIS2_PLACEMENT_3D ( 'NONE', #86202, #163215, #161940 ) ;
#66185 = CARTESIAN_POINT ( 'NONE',  ( 22.49533356619862801, 64.34999999370828050, -170.0882300648472096 ) ) ;
#66184 = CIRCLE ( 'NONE', #166752, 0.09999999999999939493 ) ;
#66186 = EDGE_CURVE ( 'NONE', #197986, #70815, #223646, .T. ) ;
#66187 = EDGE_CURVE ( 'NONE', #40059, #145384, #112492, .T. ) ;
#66188 = ORIENTED_EDGE ( 'NONE', *, *, #76872, .F. ) ;
#66189 =( BOUNDED_SURFACE ( )  B_SPLINE_SURFACE ( 3, 2, ( 
 ( #37027, #216908, #34468 ),
 ( #117816, #232655, #116545 ),
 ( #136071, #115252, #113960 ),
 ( #175268, #197348, #253465 ),
 ( #194819, #215624, #196081 ),
 ( #173995, #119116, #38293 ),
 ( #14891, #98214, #158276 ),
 ( #53992, #16179, #17433 ),
 ( #198638, #76121, #177825 ),
 ( #154422, #254714, #59090 ) ),
 .UNSPECIFIED., .F., .F., .F. ) 
 B_SPLINE_SURFACE_WITH_KNOTS ( ( 4, 2, 2, 2, 4 ),
 ( 3, 3 ),
 ( 0.0001836757140119120197, 0.0004000170051583426273, 0.0005081876507315579447, 0.0005622729735181655492, 0.0006163582963047732621 ),
 ( 0.000000000000000000, 1.000000000000000000 ),
 .UNSPECIFIED. ) 
 GEOMETRIC_REPRESENTATION_ITEM ( )  RATIONAL_B_SPLINE_SURFACE ( (
 ( 1.000000000000000000, 0.7071067811865543451, 1.000000000000000000),
 ( 1.000000000000000000, 0.6461995200018084695, 1.000000000000000000),
 ( 1.000000000000000000, 0.5776453529564903322, 1.000000000000000000),
 ( 1.000000000000000000, 0.4585233068343699259, 1.000000000000000000),
 ( 1.000000000000000000, 0.4154092989948574566, 1.000000000000000000),
 ( 1.000000000000000000, 0.3550093145831485497, 1.000000000000000000),
 ( 1.000000000000000000, 0.3354498651685384747, 1.000000000000000000),
 ( 1.000000000000000000, 0.3060347992258684036, 1.000000000000000000),
 ( 1.000000000000000000, 0.2963555829624233140, 1.000000000000000000),
 ( 1.000000000000000000, 0.2966190024561738969, 1.000000000000000000) ) ) 
 REPRESENTATION_ITEM ( '' )  SURFACE ( )  );
#66190 = CARTESIAN_POINT ( 'NONE',  ( -18.50000000000000000, 11.74999999999999645, 11.75000000000000000 ) ) ;
#66191 = AXIS2_PLACEMENT_3D ( 'NONE', #116360, #15991, #36844 ) ;
#66193 = ORIENTED_EDGE ( 'NONE', *, *, #207196, .F. ) ;
#66192 = CYLINDRICAL_SURFACE ( 'NONE', #201166, 0.09999999999999939493 ) ;
#66194 = ADVANCED_FACE ( 'NONE', ( #117615 ), #155496, .T. ) ;
#66197 = ORIENTED_EDGE ( 'NONE', *, *, #233134, .F. ) ;
#66196 = VERTEX_POINT ( 'NONE', #18517 ) ;
#66195 = LINE ( 'NONE', #162744, #63833 ) ;
#66199 = CIRCLE ( 'NONE', #174593, 4.049999999999998934 ) ;
#66198 = FACE_OUTER_BOUND ( 'NONE', #180819, .T. ) ;
#66200 = TOROIDAL_SURFACE ( 'NONE', #120227, 0.2000000000000000111, 0.1000000000000000056 ) ;
#66201 = DIRECTION ( 'NONE',  ( 0.000000000000000000, 0.000000000000000000, -1.000000000000000000 ) ) ;
#66202 = EDGE_CURVE ( 'NONE', #214314, #83582, #156770, .T. ) ;
#66203 = CARTESIAN_POINT ( 'NONE',  ( 21.72449340488910607, 65.71604372252089377, -115.6731074845243796 ) ) ;
#66204 = AXIS2_PLACEMENT_3D ( 'NONE', #27330, #204623, #28627 ) ;
#66206 = DIRECTION ( 'NONE',  ( 0.000000000000000000, -0.1350103645451904977, 0.9908441862701596881 ) ) ;
#66205 = CARTESIAN_POINT ( 'NONE',  ( -21.29999999999995808, 76.00000000001237765, -170.0231074845243597 ) ) ;
#66207 = DIRECTION ( 'NONE',  ( -1.000000000000000000, -0.000000000000000000, 0.000000000000000000 ) ) ;
#66209 = EDGE_CURVE ( 'NONE', #101793, #252329, #177622, .T. ) ;
#66208 = CARTESIAN_POINT ( 'NONE',  ( -16.27683809663751191, 9.350000000011132073, -146.5500000000000114 ) ) ;
#66210 = CARTESIAN_POINT ( 'NONE',  ( 23.40000000000005542, 77.16254490893143725, -43.82310748452479743 ) ) ;
#66211 = DIRECTION ( 'NONE',  ( -0.7071067811865486830, 0.3338907855510734324, 0.6233112732207604090 ) ) ;
#66212 = CARTESIAN_POINT ( 'NONE',  ( -20.94999999999999929, -11.65000000000000036, -30.50000000000000000 ) ) ;
#66213 = ORIENTED_EDGE ( 'NONE', *, *, #175695, .F. ) ;
#66214 = ORIENTED_EDGE ( 'NONE', *, *, #83648, .T. ) ;
#66215 = ADVANCED_FACE ( 'NONE', ( #233723 ), #236141, .T. ) ;
#66216 = CARTESIAN_POINT ( 'NONE',  ( -21.65000000000000213, 68.75000000001263345, -194.2731074845244166 ) ) ;
#66218 = EDGE_LOOP ( 'NONE', ( #158675, #56375, #232320, #172470 ) ) ;
#66217 = CARTESIAN_POINT ( 'NONE',  ( -20.54999999999999716, 68.85000000001259934, -191.1731074845243938 ) ) ;
#66219 = ORIENTED_EDGE ( 'NONE', *, *, #130200, .T. ) ;
#66220 = DIRECTION ( 'NONE',  ( 0.000000000000000000, -0.9770955615653315052, -0.2128009952263603954 ) ) ;
#66221 = ORIENTED_EDGE ( 'NONE', *, *, #50790, .F. ) ;
#66222 = CARTESIAN_POINT ( 'NONE',  ( -21.07954640115405454, 69.67071230398723003, -136.5891151916643480 ) ) ;
#66223 = EDGE_CURVE ( 'NONE', #133612, #164331, #190376, .T. ) ;
#66224 = ORIENTED_EDGE ( 'NONE', *, *, #213966, .T. ) ;
#66225 = LINE ( 'NONE', #149631, #102001 ) ;
#66226 = DIRECTION ( 'NONE',  ( 0.000000000000000000, 0.2617529984164506107, 0.9651348961777299618 ) ) ;
#66227 = CIRCLE ( 'NONE', #99516, 0.2000000000000005107 ) ;
#66228 = AXIS2_PLACEMENT_3D ( 'NONE', #62557, #78248, #1273 ) ;
#66230 = EDGE_LOOP ( 'NONE', ( #59459, #177770, #74131, #97533 ) ) ;
#66229 = VERTEX_POINT ( 'NONE', #138431 ) ;
#66231 = VERTEX_POINT ( 'NONE', #232449 ) ;
#66232 = DIRECTION ( 'NONE',  ( 1.000000000000000000, 2.885090398161910739E-16, 6.283419270304611573E-17 ) ) ;
#66233 = ORIENTED_EDGE ( 'NONE', *, *, #191498, .T. ) ;
#66234 = EDGE_LOOP ( 'NONE', ( #121017, #77709, #43672, #170820 ) ) ;
#66235 = CARTESIAN_POINT ( 'NONE',  ( 22.47071067811865319, 68.27992525551390202, -103.1221999392269737 ) ) ;
#66236 = CARTESIAN_POINT ( 'NONE',  ( -20.94999999999999929, -1.835341550213257733, -179.0551512925629538 ) ) ;
#66238 = EDGE_LOOP ( 'NONE', ( #166191, #80348, #224888, #32992, #180896 ) ) ;
#66237 = CARTESIAN_POINT ( 'NONE',  ( 18.59999999999999787, -1.851028230129704522, -145.6539132694225032 ) ) ;
#66239 = AXIS2_PLACEMENT_3D ( 'NONE', #54049, #128459, #170205 ) ;
#66240 = CARTESIAN_POINT ( 'NONE',  ( 20.94999999999999929, -8.663551401869158397, -9.524101118067305194 ) ) ;
#66241 = CARTESIAN_POINT ( 'NONE',  ( 18.59999999999999076, -1.851617760457748618, -212.6031897196036198 ) ) ;
#66243 = VERTEX_POINT ( 'NONE', #192039 ) ;
#66242 = DIRECTION ( 'NONE',  ( 0.000000000000000000, 0.000000000000000000, -1.000000000000000000 ) ) ;
#66244 = CARTESIAN_POINT ( 'NONE',  ( 18.60000000000000142, -9.399999999988782662, -174.7972597596632625 ) ) ;
#66245 = ORIENTED_EDGE ( 'NONE', *, *, #159794, .T. ) ;
#66246 = CARTESIAN_POINT ( 'NONE',  ( -23.15000000000000213, -8.596261682242992919, -9.450127517150276546 ) ) ;
#66247 = VERTEX_POINT ( 'NONE', #251982 ) ;
#66248 = PLANE ( 'NONE',  #242920 ) ;
#66249 = DIRECTION ( 'NONE',  ( 0.000000000000000000, 0.000000000000000000, 1.000000000000000000 ) ) ;
#66250 = ORIENTED_EDGE ( 'NONE', *, *, #151798, .F. ) ;
#66253 = DIRECTION ( 'NONE',  ( 0.000000000000000000, -0.8814952561688476074, 0.4721928772777262417 ) ) ;
#66252 = DIRECTION ( 'NONE',  ( -1.000000000000000000, -7.304098846218134667E-16, 0.000000000000000000 ) ) ;
#66251 = VECTOR ( 'NONE', #174116, 1000.000000000000000 ) ;
#66254 = VECTOR ( 'NONE', #106092, 1000.000000000000000 ) ;
#66255 = DIRECTION ( 'NONE',  ( 0.000000000000000000, -0.9550021345545530727, 0.2965989261549131228 ) ) ;
#66256 = LINE ( 'NONE', #167952, #93438 ) ;
#66257 = VECTOR ( 'NONE', #186994, 1000.000000000000000 ) ;
#66258 = ORIENTED_EDGE ( 'NONE', *, *, #42695, .F. ) ;
#66259 = ORIENTED_EDGE ( 'NONE', *, *, #29012, .F. ) ;
#66260 = DIRECTION ( 'NONE',  ( 0.000000000000000000, 1.000000000000000000, 0.000000000000000000 ) ) ;
#66261 = EDGE_CURVE ( 'NONE', #121101, #247064, #256935, .T. ) ;
#66262 = CARTESIAN_POINT ( 'NONE',  ( -20.54999999999999716, 7.150000000011155876, -117.2500000000000284 ) ) ;
#66263 = VERTEX_POINT ( 'NONE', #143267 ) ;
#66264 = DIRECTION ( 'NONE',  ( 1.000000000000000000, 0.000000000000000000, 0.000000000000000000 ) ) ;
#66265 = ORIENTED_EDGE ( 'NONE', *, *, #19168, .F. ) ;
#66266 = CARTESIAN_POINT ( 'NONE',  ( -22.59080734064477625, 11.75000000001115907, -66.96925029190302325 ) ) ;
#66267 = ORIENTED_EDGE ( 'NONE', *, *, #98909, .T. ) ;
#66268 = CARTESIAN_POINT ( 'NONE',  ( 20.99999999999999645, 66.25000000001226397, -149.1731074845244223 ) ) ;
#66269 = VECTOR ( 'NONE', #155486, 1000.000000000000000 ) ;
#66270 = AXIS2_PLACEMENT_3D ( 'NONE', #108065, #205867, #145887 ) ;
#66271 = CARTESIAN_POINT ( 'NONE',  ( 23.14999999999998437, 1.115600667400684642E-11, -33.50000000000000000 ) ) ;
#66272 = CARTESIAN_POINT ( 'NONE',  ( -16.87383368123029825, 66.05000000001187743, -90.37310748452438247 ) ) ;
#66273 = VERTEX_POINT ( 'NONE', #123719 ) ;
#66274 = CARTESIAN_POINT ( 'NONE',  ( 18.39999999999999858, -9.682403433465237796, -207.6568433774127698 ) ) ;
#66275 = EDGE_CURVE ( 'NONE', #49841, #67817, #177738, .T. ) ;
#66277 = ORIENTED_EDGE ( 'NONE', *, *, #37348, .T. ) ;
#66276 = AXIS2_PLACEMENT_3D ( 'NONE', #203221, #107978, #64989 ) ;
#66278 = ORIENTED_EDGE ( 'NONE', *, *, #80885, .T. ) ;
#66279 = AXIS2_PLACEMENT_3D ( 'NONE', #147183, #230589, #228012 ) ;
#66280 = CIRCLE ( 'NONE', #158086, 0.6000000000000015321 ) ;
#66281 = ORIENTED_EDGE ( 'NONE', *, *, #99980, .F. ) ;
#66282 = CIRCLE ( 'NONE', #91226, 0.1000000000000033779 ) ;
#66283 = CARTESIAN_POINT ( 'NONE',  ( -21.05000000000000071, 28.56975825374500388, -258.1421690862028413 ) ) ;
#66284 = CARTESIAN_POINT ( 'NONE',  ( 23.24999999999999289, 8.882751598337874199, -187.0399955572217721 ) ) ;
#66285 = LINE ( 'NONE', #106660, #21751 ) ;
#66286 = DIRECTION ( 'NONE',  ( 0.000000000000000000, 0.2617529984165152257, 0.9651348961777124202 ) ) ;
#66287 = VECTOR ( 'NONE', #120168, 1000.000000000000000 ) ;
#66289 = CARTESIAN_POINT ( 'NONE',  ( 21.05000000000000071, 58.88961935843800433, -225.7942249309140834 ) ) ;
#66288 = CARTESIAN_POINT ( 'NONE',  ( 18.59999999999999076, 63.53162788017662166, -224.4728618886983043 ) ) ;
#66291 = EDGE_LOOP ( 'NONE', ( #220439, #102435, #99722, #63961, #172145, #245806 ) ) ;
#66290 = LINE ( 'NONE', #166701, #10541 ) ;
#66292 = CARTESIAN_POINT ( 'NONE',  ( -18.59999999999999787, 11.75000000001115197, -88.75000000000004263 ) ) ;
#66293 = ORIENTED_EDGE ( 'NONE', *, *, #198602, .T. ) ;
#66294 = LINE ( 'NONE', #226628, #113364 ) ;
#66295 = ORIENTED_EDGE ( 'NONE', *, *, #148533, .F. ) ;
#66296 = EDGE_LOOP ( 'NONE', ( #192303, #5912 ) ) ;
#66297 = CARTESIAN_POINT ( 'NONE',  ( 20.94999999999999929, -11.48912529307605546, -30.39999999999999503 ) ) ;
#66298 = LINE ( 'NONE', #105374, #72627 ) ;
#66299 = CARTESIAN_POINT ( 'NONE',  ( 18.49999999999999289, 7.021664781911246322, -70.83356540189728889 ) ) ;
#66300 = DIRECTION ( 'NONE',  ( 0.000000000000000000, 0.000000000000000000, -1.000000000000000000 ) ) ;
#66301 = CIRCLE ( 'NONE', #16243, 0.2000000000000000944 ) ;
#66302 = CARTESIAN_POINT ( 'NONE',  ( -18.59999999999999787, 1.835341550235567887, -45.05515129256298223 ) ) ;
#66303 = EDGE_LOOP ( 'NONE', ( #171856, #225836, #252669, #28105 ) ) ;
#66304 = EDGE_LOOP ( 'NONE', ( #34278, #109259, #257227, #37661 ) ) ;
#66305 = CYLINDRICAL_SURFACE ( 'NONE', #169878, 0.09999999999999939493 ) ;
#66306 = ORIENTED_EDGE ( 'NONE', *, *, #78548, .F. ) ;
#66307 = DIRECTION ( 'NONE',  ( 1.000000000000000000, 0.000000000000000000, 0.000000000000000000 ) ) ;
#66308 = DIRECTION ( 'NONE',  ( 1.000000000000000000, 0.000000000000000000, 0.000000000000000000 ) ) ;
#66309 = DIRECTION ( 'NONE',  ( 0.000000000000000000, -0.4856429311786307212, -0.8741572761215384846 ) ) ;
#66310 = CARTESIAN_POINT ( 'NONE',  ( -17.22361732159831860, 52.62473031027478498, -231.0628565205512928 ) ) ;
#66311 = FACE_OUTER_BOUND ( 'NONE', #126387, .T. ) ;
#66312 = CARTESIAN_POINT ( 'NONE',  ( -21.55000000000000426, 68.29142135624915966, -90.67310748452436542 ) ) ;
#66313 = ORIENTED_EDGE ( 'NONE', *, *, #257376, .T. ) ;
#66314 = DIRECTION ( 'NONE',  ( 0.000000000000000000, -0.9999631594459057471, 0.008583690987121077309 ) ) ;
#66315 = AXIS2_PLACEMENT_3D ( 'NONE', #214805, #193987, #253924 ) ;
#66316 = CARTESIAN_POINT ( 'NONE',  ( 21.05000000000000071, 70.50000000001260503, -191.1178414656113205 ) ) ;
#66318 = EDGE_CURVE ( 'NONE', #142934, #215339, #31974, .T. ) ;
#66317 = CARTESIAN_POINT ( 'NONE',  ( -21.05000000000000071, 6.400000000011158541, -143.9304246300615944 ) ) ;
#66319 = AXIS2_PLACEMENT_3D ( 'NONE', #87270, #105531, #185108 ) ;
#66320 = DIRECTION ( 'NONE',  ( 0.000000000000000000, 0.8814952561688438326, -0.4721928772777331806 ) ) ;
#66321 = DIRECTION ( 'NONE',  ( -1.000000000000000000, 0.000000000000000000, 0.000000000000000000 ) ) ;
#66322 = AXIS2_PLACEMENT_3D ( 'NONE', #34994, #255225, #237008 ) ;
#66323 = ADVANCED_FACE ( 'NONE', ( #7617 ), #87134, .F. ) ;
#66324 = DIRECTION ( 'NONE',  ( 1.000000000000000000, -0.000000000000000000, -0.000000000000000000 ) ) ;
#66325 = ORIENTED_EDGE ( 'NONE', *, *, #920, .F. ) ;
#66326 = EDGE_CURVE ( 'NONE', #177620, #212700, #23966, .T. ) ;
#66327 = CARTESIAN_POINT ( 'NONE',  ( -22.00411653962151348, 68.74655713164203519, -136.6221455902930018 ) ) ;
#66328 = VERTEX_POINT ( 'NONE', #24644 ) ;
#66329 = DIRECTION ( 'NONE',  ( -1.000000000000000000, 0.000000000000000000, 0.000000000000000000 ) ) ;
#66330 = EDGE_CURVE ( 'NONE', #253481, #240913, #65013, .T. ) ;
#66331 = CARTESIAN_POINT ( 'NONE',  ( -21.05000000000000071, 79.03126467873600802, -235.8703919547671717 ) ) ;
#66332 = FACE_OUTER_BOUND ( 'NONE', #180077, .T. ) ;
#66333 = VECTOR ( 'NONE', #54473, 1000.000000000000000 ) ;
#66334 = EDGE_LOOP ( 'NONE', ( #36658, #101386, #3583, #170008 ) ) ;
#66335 = DIRECTION ( 'NONE',  ( 0.7071067811865474617, 0.7071067811865474617, 0.000000000000000000 ) ) ;
#66336 = CIRCLE ( 'NONE', #53866, 11.89999999999999325 ) ;
#66337 = DIRECTION ( 'NONE',  ( -0.000000000000000000, -0.000000000000000000, -1.000000000000000000 ) ) ;
#66338 = DIRECTION ( 'NONE',  ( 0.000000000000000000, 1.000000000000000000, 6.982962677686267499E-15 ) ) ;
#66339 = CARTESIAN_POINT ( 'NONE',  ( -23.25000000000000000, 45.93315328338058379, -256.6017782078560003 ) ) ;
#66340 = ADVANCED_FACE ( 'NONE', ( #84531 ), #144541, .F. ) ;
#66341 = CARTESIAN_POINT ( 'NONE',  ( -21.09610168723073187, 69.62104428478760099, -170.0566969914158904 ) ) ;
#66342 = AXIS2_PLACEMENT_3D ( 'NONE', #226246, #183303, #64628 ) ;
#66343 = DIRECTION ( 'NONE',  ( -1.000000000000000000, 0.000000000000000000, -0.000000000000000000 ) ) ;
#66344 = ORIENTED_EDGE ( 'NONE', *, *, #239466, .T. ) ;
#66345 = EDGE_LOOP ( 'NONE', ( #119964, #50841, #71297, #235242 ) ) ;
#66347 = ORIENTED_EDGE ( 'NONE', *, *, #35781, .T. ) ;
#66346 = CARTESIAN_POINT ( 'NONE',  ( 23.14999999999999503, 64.35000000001156195, -57.37310748452439668 ) ) ;
#66348 = CARTESIAN_POINT ( 'NONE',  ( 22.40000000000010516, 1.020945751984553285E-11, -122.3504291924549108 ) ) ;
#66349 = CARTESIAN_POINT ( 'NONE',  ( -23.25000000000000000, 76.00000000001213607, -136.5231074845243313 ) ) ;
#66350 = EDGE_CURVE ( 'NONE', #28556, #85045, #136329, .T. ) ;
#66351 = ORIENTED_EDGE ( 'NONE', *, *, #41822, .F. ) ;
#66352 = CARTESIAN_POINT ( 'NONE',  ( 22.48660254037844552, 11.65000000001115588, -33.45000000000000995 ) ) ;
#66353 = CARTESIAN_POINT ( 'NONE',  ( 23.14999999999999858, 6.650000000011155876, -112.8500000000000369 ) ) ;
#66354 = ORIENTED_EDGE ( 'NONE', *, *, #53787, .T. ) ;
#66355 = DIRECTION ( 'NONE',  ( 0.000000000000000000, 0.000000000000000000, -1.000000000000000000 ) ) ;
#66356 = TOROIDAL_SURFACE ( 'NONE', #216374, 0.2000000000000000111, 0.1000000000000000056 ) ;
#66357 = DIRECTION ( 'NONE',  ( -0.000000000000000000, -0.000000000000000000, -1.000000000000000000 ) ) ;
#66358 = ORIENTED_EDGE ( 'NONE', *, *, #177723, .F. ) ;
#66359 = ORIENTED_EDGE ( 'NONE', *, *, #27036, .F. ) ;
#66360 = DIRECTION ( 'NONE',  ( -1.000000000000000000, 0.000000000000000000, 0.000000000000000000 ) ) ;
#66361 = DIRECTION ( 'NONE',  ( 0.000000000000000000, 1.224646799142185182E-16, 1.000000000000000000 ) ) ;
#66362 = B_SPLINE_CURVE_WITH_KNOTS ( 'NONE', 3,
 ( #36340, #130272, #115861, #16775, #70349, #217500 ),
 .UNSPECIFIED., .F., .F.,
 ( 4, 2, 4 ),
 ( 0.000000000000000000, 0.0001569047307838632198, 0.0003138094615677264397 ),
 .UNSPECIFIED. ) ;
#66363 = DIRECTION ( 'NONE',  ( 0.000000000000000000, 0.000000000000000000, 1.000000000000000000 ) ) ;
#66364 = EDGE_CURVE ( 'NONE', #66550, #14558, #224079, .T. ) ;
#66365 = CARTESIAN_POINT ( 'NONE',  ( -21.08479644141223019, 69.65496134228006042, -103.0816619270884473 ) ) ;
#66366 = DIRECTION ( 'NONE',  ( 0.000000000000000000, -0.9770955615653316162, -0.2128009952263604232 ) ) ;
#66367 = DIRECTION ( 'NONE',  ( 0.000000000000000000, 0.2128009952263603677, -0.9770955615653313941 ) ) ;
#66368 = CARTESIAN_POINT ( 'NONE',  ( -16.93909480342659890, 9.993078364801540658, -12.60034701667233037 ) ) ;
#66370 = CARTESIAN_POINT ( 'NONE',  ( 20.94999999999999574, 11.84624361595475506, -206.1763227999733203 ) ) ;
#66369 = CARTESIAN_POINT ( 'NONE',  ( -21.14999999999999858, 65.51923798433686841, -242.1677427744926092 ) ) ;
#66371 = AXIS2_PLACEMENT_3D ( 'NONE', #67329, #145573, #6060 ) ;
#66372 = AXIS2_PLACEMENT_3D ( 'NONE', #80665, #22015, #257989 ) ;
#66373 = CARTESIAN_POINT ( 'NONE',  ( -23.25000000000000000, -1.851617760457748618, -212.6031897196036198 ) ) ;
#66374 = CARTESIAN_POINT ( 'NONE',  ( -20.94999999999999929, 76.00000000001267608, -203.5231074845243597 ) ) ;
#66375 = CIRCLE ( 'NONE', #212127, 2.000000000000001776 ) ;
#66377 = LINE ( 'NONE', #207181, #11512 ) ;
#66376 = AXIS2_PLACEMENT_3D ( 'NONE', #240101, #154488, #100545 ) ;
#66378 = ORIENTED_EDGE ( 'NONE', *, *, #191032, .F. ) ;
#66379 = ORIENTED_EDGE ( 'NONE', *, *, #59413, .T. ) ;
#66380 = DIRECTION ( 'NONE',  ( 0.000000000000000000, 0.8700118002898321601, -0.4930308989875230030 ) ) ;
#66381 = CARTESIAN_POINT ( 'NONE',  ( 22.19999999999999929, -1.467286812112899463, 32.89999999999999858 ) ) ;
#66383 = CARTESIAN_POINT ( 'NONE',  ( -12.68215100488890457, 12.99204546914880432, -216.4972940033653401 ) ) ;
#66382 = CARTESIAN_POINT ( 'NONE',  ( -21.56666275994540172, 76.00000000001271871, -210.4804758914176830 ) ) ;
#66384 = ADVANCED_FACE ( 'NONE', ( #204518 ), #25906, .F. ) ;
#66385 = AXIS2_PLACEMENT_3D ( 'NONE', #250409, #167064, #30108 ) ;
#66386 = CARTESIAN_POINT ( 'NONE',  ( 23.14999999999999503, 11.65000000001116298, -121.8500000000000369 ) ) ;
#66387 = CARTESIAN_POINT ( 'NONE',  ( 18.59999999999999787, 16.44800918141279311, -240.8068063186265135 ) ) ;
#66388 = DIRECTION ( 'NONE',  ( -0.000000000000000000, -0.000000000000000000, -1.000000000000000000 ) ) ;
#66389 = VERTEX_POINT ( 'NONE', #85830 ) ;
#66390 = ADVANCED_FACE ( 'NONE', ( #165414 ), #244935, .F. ) ;
#66391 = EDGE_LOOP ( 'NONE', ( #10539, #16585, #113755, #48285 ) ) ;
#66392 = CIRCLE ( 'NONE', #162080, 0.4999999999999968359 ) ;
#66394 = AXIS2_PLACEMENT_3D ( 'NONE', #184754, #3547, #86919 ) ;
#66393 = DIRECTION ( 'NONE',  ( 0.000000000000000000, 0.000000000000000000, 1.000000000000000000 ) ) ;
#66395 = VERTEX_POINT ( 'NONE', #27212 ) ;
#66396 = EDGE_CURVE ( 'NONE', #32589, #180521, #82169, .T. ) ;
#66397 = DIRECTION ( 'NONE',  ( -0.000000000000000000, -0.000000000000000000, -1.000000000000000000 ) ) ;
#66398 = TOROIDAL_SURFACE ( 'NONE', #24734, 12.77499999999999858, 0.1000000000000000056 ) ;
#66399 = CARTESIAN_POINT ( 'NONE',  ( 21.05000000000000071, 2.585532092011767702, -212.8717110730202933 ) ) ;
#66400 = VERTEX_POINT ( 'NONE', #68891 ) ;
#66401 = CARTESIAN_POINT ( 'NONE',  ( -23.15000000000000213, 76.00000000001126921, -203.5231074845248997 ) ) ;
#66402 = ADVANCED_FACE ( 'NONE', ( #147110 ), #165428, .F. ) ;
#66403 = ORIENTED_EDGE ( 'NONE', *, *, #177076, .F. ) ;
#66404 = DIRECTION ( 'NONE',  ( 0.000000000000000000, -1.000000000000000000, 0.000000000000000000 ) ) ;
#66405 = DIRECTION ( 'NONE',  ( -1.000000000000000000, -0.000000000000000000, -0.000000000000000000 ) ) ;
#66406 = ADVANCED_FACE ( 'NONE', ( #207109 ), #8901, .T. ) ;
#66407 = CARTESIAN_POINT ( 'NONE',  ( 18.40000000000000213, -9.519327731081279609, -140.9729763765593304 ) ) ;
#66408 = EDGE_CURVE ( 'NONE', #231005, #246455, #123911, .T. ) ;
#66409 = DIRECTION ( 'NONE',  ( 2.952720810173289112E-16, -1.000000000000000000, 0.000000000000000000 ) ) ;
#66410 = CARTESIAN_POINT ( 'NONE',  ( -20.94999999999999929, -1.736257131586239844, -145.5686523290175387 ) ) ;
#66411 = SPHERICAL_SURFACE ( 'NONE', #13584, 0.1000000000000000056 ) ;
#66412 = CARTESIAN_POINT ( 'NONE',  ( 20.94999999999999929, 18.18127959618848877, -237.5711165786817389 ) ) ;
#66414 = ORIENTED_EDGE ( 'NONE', *, *, #185293, .F. ) ;
#66413 = FACE_OUTER_BOUND ( 'NONE', #7534, .T. ) ;
#66416 = DIRECTION ( 'NONE',  ( 0.7071067811865474617, 0.7071067811865474617, 0.000000000000000000 ) ) ;
#66415 = CARTESIAN_POINT ( 'NONE',  ( -20.54999999999999716, 4.250000000011156409, -45.85000000000000142 ) ) ;
#66417 = EDGE_LOOP ( 'NONE', ( #174372, #245170, #125785, #205046 ) ) ;
#66419 = ORIENTED_EDGE ( 'NONE', *, *, #49810, .F. ) ;
#66418 = DIRECTION ( 'NONE',  ( 0.000000000000000000, -1.000000000000000000, -6.982962677686266711E-15 ) ) ;
#66420 = VECTOR ( 'NONE', #187656, 1000.000000000000000 ) ;
#66421 = ORIENTED_EDGE ( 'NONE', *, *, #177558, .F. ) ;
#66422 = DIRECTION ( 'NONE',  ( 6.484947573744954877E-15, -0.7973076739542579450, 0.6035730884107166627 ) ) ;
#66423 = CARTESIAN_POINT ( 'NONE',  ( 21.87500000000000355, 9.749999999999998224, -21.15000000000000213 ) ) ;
#66424 = EDGE_CURVE ( 'NONE', #56194, #4734, #83267, .T. ) ;
#66425 = CARTESIAN_POINT ( 'NONE',  ( 21.05000000000000071, 0.05148288189266662929, -127.6998201820867820 ) ) ;
#66426 = DIRECTION ( 'NONE',  ( -1.000000000000000000, -0.000000000000000000, -0.000000000000000000 ) ) ;
#66427 = AXIS2_PLACEMENT_3D ( 'NONE', #75889, #234971, #173761 ) ;
#66428 = DIRECTION ( 'NONE',  ( -3.265361837132813093E-16, 1.000000000000000000, 0.000000000000000000 ) ) ;
#66429 = EDGE_CURVE ( 'NONE', #243885, #62106, #90562, .T. ) ;
#66430 = EDGE_CURVE ( 'NONE', #224607, #179279, #53157, .T. ) ;
#66431 = LINE ( 'NONE', #149832, #20336 ) ;
#66432 = DIRECTION ( 'NONE',  ( 0.000000000000000000, 1.000000000000000000, 0.000000000000000000 ) ) ;
#66433 = CARTESIAN_POINT ( 'NONE',  ( 21.08884785362045378, 69.64280663258689685, -136.5728905795911885 ) ) ;
#66434 = ORIENTED_EDGE ( 'NONE', *, *, #176685, .F. ) ;
#66435 = ORIENTED_EDGE ( 'NONE', *, *, #39818, .T. ) ;
#66436 = FACE_OUTER_BOUND ( 'NONE', #252341, .T. ) ;
#66437 = AXIS2_PLACEMENT_3D ( 'NONE', #118976, #220635, #135938 ) ;
#66438 = ORIENTED_EDGE ( 'NONE', *, *, #194445, .T. ) ;
#66439 = SPHERICAL_SURFACE ( 'NONE', #59221, 0.1000000000000000056 ) ;
#66441 = ORIENTED_EDGE ( 'NONE', *, *, #56798, .T. ) ;
#66440 = AXIS2_PLACEMENT_3D ( 'NONE', #142395, #225767, #165838 ) ;
#66442 = DIRECTION ( 'NONE',  ( 0.000000000000000000, -0.4088369013363494231, 0.9126074666063672680 ) ) ;
#66443 = EDGE_CURVE ( 'NONE', #248870, #236989, #12773, .T. ) ;
#66444 = CARTESIAN_POINT ( 'NONE',  ( -23.25000000000000000, 5.950000000011163692, -90.19429769496522908 ) ) ;
#66445 = CARTESIAN_POINT ( 'NONE',  ( -22.50000000000000000, -2.388551469052506260, -189.5974192130969698 ) ) ;
#66446 = EDGE_CURVE ( 'NONE', #231169, #101967, #52964, .T. ) ;
#66447 = DIRECTION ( 'NONE',  ( 1.000000000000000000, -0.000000000000000000, -0.000000000000000000 ) ) ;
#66448 = ORIENTED_EDGE ( 'NONE', *, *, #168746, .F. ) ;
#66449 = AXIS2_PLACEMENT_3D ( 'NONE', #214856, #192744, #14116 ) ;
#66450 = DIRECTION ( 'NONE',  ( 2.557131231893036985E-16, 0.7049548389605067023, -0.7092521942342977503 ) ) ;
#66451 = CARTESIAN_POINT ( 'NONE',  ( 18.48536876927968109, 85.46352724987909255, -62.47448921944115341 ) ) ;
#66452 = CARTESIAN_POINT ( 'NONE',  ( -21.14999999999999858, 76.00000000001173817, -81.17267829206912211 ) ) ;
#66453 = ORIENTED_EDGE ( 'NONE', *, *, #184155, .T. ) ;
#66455 = CARTESIAN_POINT ( 'NONE',  ( -23.25000000000000000, 1.115600667400684642E-11, -100.5000000000000426 ) ) ;
#66454 = CARTESIAN_POINT ( 'NONE',  ( 21.12757541349815682, 60.98223810379111853, -234.1656810015468579 ) ) ;
#66456 = ORIENTED_EDGE ( 'NONE', *, *, #79480, .T. ) ;
#66458 = EDGE_LOOP ( 'NONE', ( #106137, #50715, #26739, #166809, #214607 ) ) ;
#66457 = CARTESIAN_POINT ( 'NONE',  ( -22.59999999999999787, 1.115600667400684642E-11, -134.0000000000000000 ) ) ;
#66459 = AXIS2_PLACEMENT_3D ( 'NONE', #76223, #39709, #34564 ) ;
#66460 = ORIENTED_EDGE ( 'NONE', *, *, #6697, .F. ) ;
#66461 = DIRECTION ( 'NONE',  ( 0.000000000000000000, 0.000000000000000000, 1.000000000000000000 ) ) ;
#66462 = AXIS2_PLACEMENT_3D ( 'NONE', #97128, #93318, #215814 ) ;
#66463 = AXIS2_PLACEMENT_3D ( 'NONE', #59170, #55324, #138709 ) ;
#66464 = AXIS2_PLACEMENT_3D ( 'NONE', #102772, #243597, #145764 ) ;
#66465 = DIRECTION ( 'NONE',  ( 0.000000000000000000, 6.982962677686267499E-15, -1.000000000000000000 ) ) ;
#66466 = DIRECTION ( 'NONE',  ( -3.265361837132813586E-16, 0.9770955615653313941, 0.2128009952263610061 ) ) ;
#66467 = ORIENTED_EDGE ( 'NONE', *, *, #128615, .F. ) ;
#66468 = LINE ( 'NONE', #247671, #234503 ) ;
#66469 = VECTOR ( 'NONE', #98599, 1000.000000000000114 ) ;
#66470 = PLANE ( 'NONE',  #115610 ) ;
#66472 = LINE ( 'NONE', #185134, #221602 ) ;
#66471 = LINE ( 'NONE', #9060, #138771 ) ;
#66474 = ORIENTED_EDGE ( 'NONE', *, *, #34723, .F. ) ;
#66473 = DIRECTION ( 'NONE',  ( 0.000000000000000000, -0.2617529984164856383, -0.9651348961777204138 ) ) ;
#66475 = EDGE_CURVE ( 'NONE', #119497, #218147, #149720, .T. ) ;
#66476 = ORIENTED_EDGE ( 'NONE', *, *, #90529, .T. ) ;
#66477 = EDGE_CURVE ( 'NONE', #104053, #224583, #132709, .T. ) ;
#66478 = DIRECTION ( 'NONE',  ( -1.000000000000000000, 0.000000000000000000, 0.000000000000000000 ) ) ;
#66479 = VECTOR ( 'NONE', #38459, 1000.000000000000000 ) ;
#66480 = CARTESIAN_POINT ( 'NONE',  ( 20.95512820512820440, 10.62384868371188062, -12.15000000000000036 ) ) ;
#66481 = DIRECTION ( 'NONE',  ( -0.000000000000000000, 1.000000000000000000, 6.982962677686266711E-15 ) ) ;
#66482 = VERTEX_POINT ( 'NONE', #113134 ) ;
#66483 = DIRECTION ( 'NONE',  ( -1.000000000000000000, 0.000000000000000000, 0.000000000000000000 ) ) ;
#66484 = VERTEX_POINT ( 'NONE', #251347 ) ;
#66485 = DIRECTION ( 'NONE',  ( -0.000000000000000000, -0.000000000000000000, 1.000000000000000000 ) ) ;
#66486 = ADVANCED_FACE ( 'NONE', ( #93565 ), #169298, .T. ) ;
#66487 = DIRECTION ( 'NONE',  ( 1.000000000000000000, 0.000000000000000000, -0.000000000000000000 ) ) ;
#66488 = CARTESIAN_POINT ( 'NONE',  ( 22.39999999999999858, 7.790779598384538041, -33.50000000000000711 ) ) ;
#66489 = ORIENTED_EDGE ( 'NONE', *, *, #138253, .F. ) ;
#66490 = LINE ( 'NONE', #146015, #58636 ) ;
#66491 = ADVANCED_FACE ( 'NONE', ( #72758 ), #92275, .T. ) ;
#66492 = AXIS2_PLACEMENT_3D ( 'NONE', #158840, #16757, #238344 ) ;
#66493 = ADVANCED_FACE ( 'NONE', ( #213507 ), #227947, .F. ) ;
#66494 = CIRCLE ( 'NONE', #249662, 0.5000000000000051070 ) ;
#66495 = ORIENTED_EDGE ( 'NONE', *, *, #159188, .T. ) ;
#66496 = CARTESIAN_POINT ( 'NONE',  ( 18.39999999999999503, 64.25000000001199396, -112.2731074845243739 ) ) ;
#66497 = CARTESIAN_POINT ( 'NONE',  ( -23.25000000000000000, -8.596261682242992919, -9.450127517150276546 ) ) ;
#66498 = AXIS2_PLACEMENT_3D ( 'NONE', #238837, #57611, #100571 ) ;
#66499 = B_SPLINE_CURVE_WITH_KNOTS ( 'NONE', 3,
 ( #131333, #110484, #70111, #53078, #250003, #50489, #132628, #10112, #190032, #111784, #107921, #187482, #93486, #11405, #29704, #191345, #90920, #51778, #12703, #109191, #92200, #173083, #13972, #227872, #171786, #71387, #150902, #230440, #212175, #167932 ),
 .UNSPECIFIED., .F., .F.,
 ( 4, 2, 2, 2, 2, 2, 2, 2, 2, 2, 2, 2, 2, 2, 4 ),
 ( 0.000000000000000000, 0.0003422764154113550820, 0.0006845528308227101641, 0.001026829246234065192, 0.001369105661645420328, 0.002053658492468071403, 0.002738211323290723129, 0.003080487738702051594, 0.003422764154113379625, 0.003765040569524708090, 0.004107316984936036121, 0.004449593400347364586, 0.004791869815758693051, 0.005134146231170021515, 0.005476422646581349113 ),
 .UNSPECIFIED. ) ;
#66500 = EDGE_CURVE ( 'NONE', #176792, #108503, #252888, .T. ) ;
#66501 = EDGE_LOOP ( 'NONE', ( #161874, #55976, #226584, #44268 ) ) ;
#66502 = ORIENTED_EDGE ( 'NONE', *, *, #17045, .T. ) ;
#66504 = EDGE_CURVE ( 'NONE', #79556, #134587, #49304, .T. ) ;
#66503 = EDGE_CURVE ( 'NONE', #208882, #243771, #15601, .T. ) ;
#66505 = CARTESIAN_POINT ( 'NONE',  ( 20.90000000000000213, 7.886648289447972360, 1.399104650876408451 ) ) ;
#66506 = EDGE_LOOP ( 'NONE', ( #245260, #158703, #86546, #66756 ) ) ;
#66508 = EDGE_LOOP ( 'NONE', ( #243594, #145788, #29809, #175748 ) ) ;
#66507 = CARTESIAN_POINT ( 'NONE',  ( -22.39999999999999858, -0.1008583690875575894, -155.7504328765105868 ) ) ;
#66509 = ORIENTED_EDGE ( 'NONE', *, *, #114406, .T. ) ;
#66510 = TOROIDAL_SURFACE ( 'NONE', #8257, 12.97499999999999609, 0.1000000000000000056 ) ;
#66512 = EDGE_LOOP ( 'NONE', ( #213045, #39497, #143182, #183205 ) ) ;
#66511 = ORIENTED_EDGE ( 'NONE', *, *, #122673, .T. ) ;
#66513 = AXIS2_PLACEMENT_3D ( 'NONE', #143480, #203471, #164347 ) ;
#66514 = CARTESIAN_POINT ( 'NONE',  ( 21.14999999999998082, -11.74999999998884448, -134.0000000000000000 ) ) ;
#66515 = EDGE_LOOP ( 'NONE', ( #250505, #62099, #22688, #6876, #153716 ) ) ;
#66516 = CARTESIAN_POINT ( 'NONE',  ( 21.30000000000002558, 1.148907358139439339E-11, -201.0000000000015064 ) ) ;
#66517 = CARTESIAN_POINT ( 'NONE',  ( -23.39999999999994529, 74.94272479589878344, -3.123107484524795474 ) ) ;
#66518 = EDGE_CURVE ( 'NONE', #219486, #99212, #44795, .T. ) ;
#66520 = EDGE_CURVE ( 'NONE', #38227, #50660, #240424, .T. ) ;
#66519 = AXIS2_PLACEMENT_3D ( 'NONE', #100834, #4333, #205096 ) ;
#66521 = LINE ( 'NONE', #186468, #163762 ) ;
#66522 =( BOUNDED_CURVE ( )  B_SPLINE_CURVE ( 3, ( #50194, #8522, #148034, #28107 ),
 .UNSPECIFIED., .F., .T. ) 
 B_SPLINE_CURVE_WITH_KNOTS ( ( 4, 4 ),
 ( 3.752122642744585068, 4.712388980384675463 ),
 .UNSPECIFIED. ) 
 CURVE ( )  GEOMETRIC_REPRESENTATION_ITEM ( )  RATIONAL_B_SPLINE_CURVE ( ( 1.000000000000000000, 0.9246222802177217481, 0.9246222802177217481, 1.000000000000000000 ) ) 
 REPRESENTATION_ITEM ( '' )  );
#66523 = CARTESIAN_POINT ( 'NONE',  ( -18.40000000000000213, 11.41458325961093756, -146.6500000000000057 ) ) ;
#66524 = VERTEX_POINT ( 'NONE', #209667 ) ;
#66525 = ORIENTED_EDGE ( 'NONE', *, *, #28942, .T. ) ;
#66526 = ADVANCED_FACE ( 'NONE', ( #150982 ), #190562, .T. ) ;
#66527 = DIRECTION ( 'NONE',  ( 0.000000000000000000, 0.000000000000000000, -1.000000000000000000 ) ) ;
#66529 = ORIENTED_EDGE ( 'NONE', *, *, #117503, .F. ) ;
#66528 = CARTESIAN_POINT ( 'NONE',  ( 18.49999999999999289, 63.84457430183214655, -209.3417490372068528 ) ) ;
#66530 = CARTESIAN_POINT ( 'NONE',  ( -20.54999999999999716, 76.00000000001141132, -34.12310748452431852 ) ) ;
#66532 = ORIENTED_EDGE ( 'NONE', *, *, #122360, .T. ) ;
#66531 = DIRECTION ( 'NONE',  ( 2.952720810173289112E-16, -1.000000000000000000, -0.000000000000000000 ) ) ;
#66533 = ORIENTED_EDGE ( 'NONE', *, *, #165099, .T. ) ;
#66534 = EDGE_CURVE ( 'NONE', #130825, #150252, #50565, .T. ) ;
#66535 = DIRECTION ( 'NONE',  ( -1.000000000000000000, 0.000000000000000000, 0.000000000000000000 ) ) ;
#66536 = EDGE_CURVE ( 'NONE', #238500, #251464, #115506, .T. ) ;
#66537 = EDGE_LOOP ( 'NONE', ( #216400, #14257, #137720, #112062 ) ) ;
#66538 = EDGE_LOOP ( 'NONE', ( #109455, #173684, #230897, #255729 ) ) ;
#66539 = CIRCLE ( 'NONE', #8285, 0.09999999999999080458 ) ;
#66540 = DIRECTION ( 'NONE',  ( 0.7071067811865474617, 0.6909108974501236844, 0.1504730267678055788 ) ) ;
#66541 = CARTESIAN_POINT ( 'NONE',  ( 21.05000000000000071, 61.95000000001218154, -142.0368025552853624 ) ) ;
#66543 = ORIENTED_EDGE ( 'NONE', *, *, #128489, .T. ) ;
#66542 = ORIENTED_EDGE ( 'NONE', *, *, #191902, .T. ) ;
#66544 = ORIENTED_EDGE ( 'NONE', *, *, #109448, .T. ) ;
#66545 = CARTESIAN_POINT ( 'NONE',  ( -22.50000000000088463, 64.13793881490383342, -247.0875655909796649 ) ) ;
#66546 = ORIENTED_EDGE ( 'NONE', *, *, #112336, .F. ) ;
#66547 = ORIENTED_EDGE ( 'NONE', *, *, #99862, .T. ) ;
#66548 = CARTESIAN_POINT ( 'NONE',  ( 21.05000000000000071, 87.75000000001264766, -200.6231074845242688 ) ) ;
#66550 = VERTEX_POINT ( 'NONE', #32345 ) ;
#66549 = DIRECTION ( 'NONE',  ( -1.000000000000000000, 0.000000000000000000, 0.000000000000000000 ) ) ;
#66551 = ADVANCED_FACE ( 'NONE', ( #116985 ), #118273, .T. ) ;
#66552 = EDGE_CURVE ( 'NONE', #125866, #3738, #148862, .T. ) ;
#66554 = CARTESIAN_POINT ( 'NONE',  ( 18.51997666896864914, -9.392332131508057458, -107.6434061874831656 ) ) ;
#66553 = CARTESIAN_POINT ( 'NONE',  ( -16.90257928357875628, 22.96791734292147069, -230.9249673455850598 ) ) ;
#66555 = CARTESIAN_POINT ( 'NONE',  ( 18.51997666896902928, 85.39233213153144675, -196.3797012970422031 ) ) ;
#66556 = CARTESIAN_POINT ( 'NONE',  ( -12.47155713865592475, 62.33593033127510097, -218.0864590324957248 ) ) ;
#66557 = EDGE_LOOP ( 'NONE', ( #193240, #150625, #132469, #128527 ) ) ;
#66558 = ORIENTED_EDGE ( 'NONE', *, *, #185727, .F. ) ;
#66559 = EDGE_CURVE ( 'NONE', #205047, #123180, #80385, .T. ) ;
#66561 = CIRCLE ( 'NONE', #212317, 0.1000000000000028644 ) ;
#66560 = FACE_OUTER_BOUND ( 'NONE', #116197, .T. ) ;
#66562 = DIRECTION ( 'NONE',  ( 1.000000000000000000, 0.000000000000000000, 0.000000000000000000 ) ) ;
#66563 = VECTOR ( 'NONE', #170223, 1000.000000000000000 ) ;
#66564 = VECTOR ( 'NONE', #171313, 1000.000000000000000 ) ;
#66565 = AXIS2_PLACEMENT_3D ( 'NONE', #165392, #243634, #220240 ) ;
#66566 = ORIENTED_EDGE ( 'NONE', *, *, #187938, .F. ) ;
#66567 = AXIS2_PLACEMENT_3D ( 'NONE', #224117, #200719, #199452 ) ;
#66568 = CARTESIAN_POINT ( 'NONE',  ( -23.25000000000000000, 76.00000000001142553, -36.02310748452432421 ) ) ;
#66569 = ORIENTED_EDGE ( 'NONE', *, *, #233721, .F. ) ;
#66570 = ORIENTED_EDGE ( 'NONE', *, *, #147901, .F. ) ;
#66571 = DIRECTION ( 'NONE',  ( 0.000000000000000000, -0.2617529984165026247, -0.9651348961777158619 ) ) ;
#66572 = EDGE_CURVE ( 'NONE', #170827, #103624, #182168, .T. ) ;
#66573 = LINE ( 'NONE', #31329, #207090 ) ;
#66574 = ORIENTED_EDGE ( 'NONE', *, *, #230518, .T. ) ;
#66575 = CARTESIAN_POINT ( 'NONE',  ( 18.59999999999999432, -1.835859311432481045, -112.0044391687985694 ) ) ;
#66576 = CARTESIAN_POINT ( 'NONE',  ( -21.10257677756356642, 6.398381742543883810, -167.4750492504319936 ) ) ;
#66577 = ORIENTED_EDGE ( 'NONE', *, *, #115343, .F. ) ;
#66578 = DIRECTION ( 'NONE',  ( 1.000000000000000000, -0.000000000000000000, -0.000000000000000000 ) ) ;
#66580 = DIRECTION ( 'NONE',  ( 0.000000000000000000, 1.000000000000000000, 0.000000000000000000 ) ) ;
#66579 =( BOUNDED_CURVE ( )  B_SPLINE_CURVE ( 3, ( #148459, #210992, #29821, #10232 ),
 .UNSPECIFIED., .F., .F. ) 
 B_SPLINE_CURVE_WITH_KNOTS ( ( 4, 4 ),
 ( 1.570796326794896558, 3.141592653589793116 ),
 .UNSPECIFIED. ) 
 CURVE ( )  GEOMETRIC_REPRESENTATION_ITEM ( )  RATIONAL_B_SPLINE_CURVE ( ( 1.000000000000000000, 0.8047378541243649375, 0.8047378541243649375, 1.000000000000000000 ) ) 
 REPRESENTATION_ITEM ( '' )  );
#66582 = PLANE ( 'NONE',  #191411 ) ;
#66581 = LINE ( 'NONE', #110824, #94762 ) ;
#66583 = DIRECTION ( 'NONE',  ( 0.000000000000000000, 6.982962677686266711E-15, -1.000000000000000000 ) ) ;
#66585 = DIRECTION ( 'NONE',  ( 2.827886303505248766E-16, -0.7397890806274223241, -0.6728388485993012091 ) ) ;
#66584 = AXIS2_PLACEMENT_3D ( 'NONE', #50576, #15346, #70193 ) ;
#66586 = CARTESIAN_POINT ( 'NONE',  ( 18.59999999999999076, 64.35000000001190301, -103.0231074845243882 ) ) ;
#66587 = TOROIDAL_SURFACE ( 'NONE', #62489, 11.70000000000000639, 0.1000000000000000056 ) ;
#66588 = CARTESIAN_POINT ( 'NONE',  ( -21.05000000000000071, 76.00000000001170974, -69.52310748452431710 ) ) ;
#66589 = VERTEX_POINT ( 'NONE', #158709 ) ;
#66590 = EDGE_CURVE ( 'NONE', #191338, #170720, #219931, .T. ) ;
#66591 = TOROIDAL_SURFACE ( 'NONE', #228891, 3.899999999999999467, 0.1000000000000000056 ) ;
#66593 = ORIENTED_EDGE ( 'NONE', *, *, #207887, .F. ) ;
#66592 = EDGE_LOOP ( 'NONE', ( #214714, #133351, #166464 ) ) ;
#66594 = ORIENTED_EDGE ( 'NONE', *, *, #257406, .F. ) ;
#66595 = CARTESIAN_POINT ( 'NONE',  ( -23.25000000000000000, 1.115600667400684642E-11, -100.5000000000000426 ) ) ;
#66596 = FACE_OUTER_BOUND ( 'NONE', #203725, .T. ) ;
#66598 = CARTESIAN_POINT ( 'NONE',  ( -16.92209698673723395, 9.950000000011138823, -146.7106355670536573 ) ) ;
#66597 = CARTESIAN_POINT ( 'NONE',  ( -21.05000000000000071, 1.115600667400684642E-11, -167.5000000000000284 ) ) ;
#66599 = CARTESIAN_POINT ( 'NONE',  ( 23.14999999999998437, 1.115600667400684642E-11, -134.0000000000000000 ) ) ;
#66600 = ORIENTED_EDGE ( 'NONE', *, *, #7961, .T. ) ;
#66601 = DIRECTION ( 'NONE',  ( 1.000000000000000000, 0.000000000000000000, -0.000000000000000000 ) ) ;
#66602 = DIRECTION ( 'NONE',  ( 1.000000000000000000, 0.000000000000000000, 0.000000000000000000 ) ) ;
#66603 = CARTESIAN_POINT ( 'NONE',  ( -16.89020380669786192, 66.05000000001187743, -90.26569633641385337 ) ) ;
#66604 = CARTESIAN_POINT ( 'NONE',  ( -18.39999999999999858, 78.23214007969471595, -231.5865251354359771 ) ) ;
#66605 = ORIENTED_EDGE ( 'NONE', *, *, #218740, .F. ) ;
#66606 = CIRCLE ( 'NONE', #174978, 0.09999999999999609201 ) ;
#66607 = CARTESIAN_POINT ( 'NONE',  ( 18.39999999999999858, -9.499999999999998224, -7.032069396699667685 ) ) ;
#66608 = CARTESIAN_POINT ( 'NONE',  ( 23.24999999999999645, 67.23127455305841238, -235.8551265064783991 ) ) ;
#66609 = ORIENTED_EDGE ( 'NONE', *, *, #81531, .T. ) ;
#66610 = ORIENTED_EDGE ( 'NONE', *, *, #208627, .T. ) ;
#66611 = CARTESIAN_POINT ( 'NONE',  ( -16.89208623190940273, 9.951577948986638944, -54.35527220321827002 ) ) ;
#66612 = DIRECTION ( 'NONE',  ( -0.000000000000000000, 0.1298341882520022694, 0.9915357197604853789 ) ) ;
#66613 = CIRCLE ( 'NONE', #20838, 0.1000000000000028644 ) ;
#66614 = FACE_OUTER_BOUND ( 'NONE', #205830, .T. ) ;
#66615 = CARTESIAN_POINT ( 'NONE',  ( 20.95289811251229750, 67.10683199555300860, -61.02129799060586635 ) ) ;
#66616 = CARTESIAN_POINT ( 'NONE',  ( -23.25000000000000000, 47.91013932883114990, -242.3192343197862044 ) ) ;
#66617 = DIRECTION ( 'NONE',  ( 1.000000000000000000, 0.000000000000000000, 0.000000000000000000 ) ) ;
#66618 = EDGE_LOOP ( 'NONE', ( #203748, #150394, #227773, #217796 ) ) ;
#66619 = CARTESIAN_POINT ( 'NONE',  ( -23.25000000000000000, 87.75000000001237765, -170.0231074845242745 ) ) ;
#66620 = CARTESIAN_POINT ( 'NONE',  ( -21.05000000000000071, 1.736257131608553550, -45.06865232901750318 ) ) ;
#66622 = LINE ( 'NONE', #27534, #108145 ) ;
#66621 = CARTESIAN_POINT ( 'NONE',  ( -16.93294127766158752, 10.00328010296601988, -87.92990726582927152 ) ) ;
#66624 = ADVANCED_FACE ( 'NONE', ( #197793 ), #255150, .F. ) ;
#66623 = DIRECTION ( 'NONE',  ( 1.000000000000000000, 0.000000000000000000, 0.000000000000000000 ) ) ;
#66625 = LINE ( 'NONE', #230853, #120831 ) ;
#66626 = CARTESIAN_POINT ( 'NONE',  ( -23.15000000000000213, 1.115600667400684642E-11, -67.00000000000000000 ) ) ;
#66627 = CIRCLE ( 'NONE', #199904, 0.1000000000000075273 ) ;
#66629 = ORIENTED_EDGE ( 'NONE', *, *, #38462, .T. ) ;
#66628 = CARTESIAN_POINT ( 'NONE',  ( -18.59999999999999787, 5.341242990002807112, -124.1933497935119988 ) ) ;
#66630 = CIRCLE ( 'NONE', #70933, 0.4999999999999944489 ) ;
#66631 = VECTOR ( 'NONE', #68245, 1000.000000000000000 ) ;
#66632 = EDGE_CURVE ( 'NONE', #176065, #133309, #38741, .T. ) ;
#66633 = AXIS2_PLACEMENT_3D ( 'NONE', #82633, #240462, #43556 ) ;
#66634 = CARTESIAN_POINT ( 'NONE',  ( 22.14074124539698829, 7.390077851054901892, -100.4009471041559607 ) ) ;
#66635 = ADVANCED_FACE ( 'NONE', ( #235635 ), #111428, .T. ) ;
#66636 = DIRECTION ( 'NONE',  ( -0.000000000000000000, -0.000000000000000000, -1.000000000000000000 ) ) ;
#66637 = CARTESIAN_POINT ( 'NONE',  ( 12.84233041328156588, 9.410538608540022665, -149.4326879971409596 ) ) ;
#66638 = EDGE_CURVE ( 'NONE', #218497, #74755, #32358, .T. ) ;
#66639 = ORIENTED_EDGE ( 'NONE', *, *, #90004, .F. ) ;
#66640 = VECTOR ( 'NONE', #138135, 1000.000000000000000 ) ;
#66641 = DIRECTION ( 'NONE',  ( 1.000000000000000000, 0.000000000000000000, 0.000000000000000000 ) ) ;
#66642 = AXIS2_PLACEMENT_3D ( 'NONE', #253047, #125722, #227393 ) ;
#66643 = VECTOR ( 'NONE', #39387, 1000.000000000000227 ) ;
#66644 = LINE ( 'NONE', #243982, #220080 ) ;
#66645 = CARTESIAN_POINT ( 'NONE',  ( -20.65000000000000568, 68.75000000001202238, -115.6731074845243512 ) ) ;
#66646 = VECTOR ( 'NONE', #204141, 1000.000000000000000 ) ;
#66647 = AXIS2_PLACEMENT_3D ( 'NONE', #132502, #110360, #89504 ) ;
#66648 = EDGE_CURVE ( 'NONE', #136679, #103596, #99956, .T. ) ;
#66650 = VERTEX_POINT ( 'NONE', #855 ) ;
#66649 = EDGE_CURVE ( 'NONE', #159384, #217170, #77843, .T. ) ;
#66651 = CARTESIAN_POINT ( 'NONE',  ( 18.49999999999999289, 11.75000000001115907, -108.6000000000000227 ) ) ;
#66653 = ORIENTED_EDGE ( 'NONE', *, *, #102023, .F. ) ;
#66652 = CARTESIAN_POINT ( 'NONE',  ( -20.54999999999999716, 76.00000000001165290, -69.52310748452431710 ) ) ;
#66655 = DIRECTION ( 'NONE',  ( -0.000000000000000000, 1.000000000000000000, 0.000000000000000000 ) ) ;
#66654 = DIRECTION ( 'NONE',  ( 0.000000000000000000, -7.086529944415894657E-15, 1.000000000000000000 ) ) ;
#66656 = VECTOR ( 'NONE', #98294, 1000.000000000000000 ) ;
#66657 = EDGE_CURVE ( 'NONE', #162009, #110145, #211201, .T. ) ;
#66658 = ORIENTED_EDGE ( 'NONE', *, *, #138933, .T. ) ;
#66659 = CARTESIAN_POINT ( 'NONE',  ( 5.899999999999995914, -11.75000000000000000, 10.10000000000000142 ) ) ;
#66660 = DIRECTION ( 'NONE',  ( 1.000000000000000000, 0.000000000000000000, 0.000000000000000000 ) ) ;
#66661 = DIRECTION ( 'NONE',  ( 1.000000000000000000, 0.000000000000000000, 0.000000000000000000 ) ) ;
#66662 = DIRECTION ( 'NONE',  ( 0.000000000000000000, 0.000000000000000000, 1.000000000000000000 ) ) ;
#66664 = ADVANCED_FACE ( 'NONE', ( #234353 ), #55682, .F. ) ;
#66663 = CARTESIAN_POINT ( 'NONE',  ( -16.94445028196807002, 66.00793639031481064, -182.6304376629428816 ) ) ;
#66665 = VERTEX_POINT ( 'NONE', #217344 ) ;
#66666 = CARTESIAN_POINT ( 'NONE',  ( -23.15000000000000213, 71.75000000001205080, -124.1731074845243228 ) ) ;
#66667 = FACE_OUTER_BOUND ( 'NONE', #212441, .T. ) ;
#66668 = DIRECTION ( 'NONE',  ( 0.000000000000000000, 0.8814952561688429444, -0.4721928772777348460 ) ) ;
#66669 = DIRECTION ( 'NONE',  ( -4.801466763864313332E-15, -0.2605042016806672911, -0.9654727137038716656 ) ) ;
#66670 = ORIENTED_EDGE ( 'NONE', *, *, #186160, .T. ) ;
#66671 = VERTEX_POINT ( 'NONE', #238201 ) ;
#66672 = CARTESIAN_POINT ( 'NONE',  ( 23.25000000000000000, 64.25000000001222134, -148.6731074845244507 ) ) ;
#66673 = AXIS2_PLACEMENT_3D ( 'NONE', #163332, #65494, #105886 ) ;
#66674 = EDGE_CURVE ( 'NONE', #65489, #159084, #94852, .T. ) ;
#66675 = CARTESIAN_POINT ( 'NONE',  ( 18.50000000000000711, 85.41907808086139653, -96.19318213431596121 ) ) ;
#66676 = CARTESIAN_POINT ( 'NONE',  ( -18.59999999999999787, 1.115600667400684642E-11, -134.0000000000000284 ) ) ;
#66677 = CARTESIAN_POINT ( 'NONE',  ( 21.06490991615909536, 13.07620565549636993, -210.6419246457020620 ) ) ;
#66678 = CARTESIAN_POINT ( 'NONE',  ( 21.05000000000000071, 7.533155231024649012, -235.5891828794142384 ) ) ;
#66679 = AXIS2_PLACEMENT_3D ( 'NONE', #217843, #104316, #202162 ) ;
#66681 =( LENGTH_UNIT ( ) NAMED_UNIT ( * ) SI_UNIT ( .MILLI., .METRE. ) );
#66680 = CARTESIAN_POINT ( 'NONE',  ( -20.94999999999999929, 1.115600667400684642E-11, -134.0000000000000000 ) ) ;
#66682 = CARTESIAN_POINT ( 'NONE',  ( -23.15000000000000213, 2.000000000011154189, -87.27537807723794572 ) ) ;
#66683 = DIRECTION ( 'NONE',  ( 1.000000000000000000, 0.000000000000000000, 0.000000000000000000 ) ) ;
#66684 = FACE_OUTER_BOUND ( 'NONE', #226359, .T. ) ;
#66685 = CARTESIAN_POINT ( 'NONE',  ( -20.85000000000000142, 76.00000000001190870, -103.0231074845243029 ) ) ;
#66686 = TOROIDAL_SURFACE ( 'NONE', #170783, 3.899999999999999467, 0.1000000000000000056 ) ;
#66688 = ORIENTED_EDGE ( 'NONE', *, *, #113241, .F. ) ;
#66687 = LINE ( 'NONE', #185345, #236244 ) ;
#66689 = DIRECTION ( 'NONE',  ( 1.000000000000000000, 0.000000000000000000, 0.000000000000000000 ) ) ;
#66690 = DIRECTION ( 'NONE',  ( 1.000000000000000000, 0.000000000000000000, 0.000000000000000000 ) ) ;
#66692 = LINE ( 'NONE', #148802, #207487 ) ;
#66691 = CARTESIAN_POINT ( 'NONE',  ( -22.50000000000000000, 36.56766367508408422, -249.5920463913791139 ) ) ;
#66693 = ADVANCED_FACE ( 'NONE', ( #60845 ), #140381, .T. ) ;
#66694 = EDGE_LOOP ( 'NONE', ( #135717, #215756, #160862, #8342, #176848 ) ) ;
#66695 = CARTESIAN_POINT ( 'NONE',  ( -16.89146115310546037, 66.04855675435554474, -115.6682850655701600 ) ) ;
#66696 = DIRECTION ( 'NONE',  ( 0.000000000000000000, 0.000000000000000000, 1.000000000000000000 ) ) ;
#66697 = CARTESIAN_POINT ( 'NONE',  ( -21.14999999999999858, -11.64999999998884483, -100.5000000000000284 ) ) ;
#66698 = DIRECTION ( 'NONE',  ( 0.000000000000000000, -0.1568667991644863147, 0.9876197685951252359 ) ) ;
#66699 = DIRECTION ( 'NONE',  ( 0.000000000000000000, -6.982962677686266711E-15, 1.000000000000000000 ) ) ;
#66700 = ORIENTED_EDGE ( 'NONE', *, *, #91509, .F. ) ;
#66702 = ORIENTED_EDGE ( 'NONE', *, *, #26694, .T. ) ;
#66701 = AXIS2_PLACEMENT_3D ( 'NONE', #130835, #245652, #207842 ) ;
#66703 = AXIS2_PLACEMENT_3D ( 'NONE', #213408, #135147, #34817 ) ;
#66704 = DIRECTION ( 'NONE',  ( -1.000000000000000000, 0.000000000000000000, 0.000000000000000000 ) ) ;
#66705 = ORIENTED_EDGE ( 'NONE', *, *, #73190, .F. ) ;
#66706 = CARTESIAN_POINT ( 'NONE',  ( -20.94999999999999929, 7.070967871809997973, -137.7465642218683399 ) ) ;
#66707 = AXIS2_PLACEMENT_3D ( 'NONE', #91598, #190727, #151600 ) ;
#66708 = EDGE_LOOP ( 'NONE', ( #139568, #220243, #165130, #203225 ) ) ;
#66709 = EDGE_CURVE ( 'NONE', #216113, #216303, #115704, .T. ) ;
#66710 = CIRCLE ( 'NONE', #12550, 0.09999999999999939493 ) ;
#66711 = CARTESIAN_POINT ( 'NONE',  ( -20.94999999999999929, 1.115600667400684642E-11, -67.00000000000000000 ) ) ;
#66712 = CARTESIAN_POINT ( 'NONE',  ( 18.59999999999999076, -1.249999999988843369, -75.00000000000004263 ) ) ;
#66713 = DIRECTION ( 'NONE',  ( -4.336808689942052446E-15, -0.7397890806274316500, -0.6728388485992908841 ) ) ;
#66714 = ORIENTED_EDGE ( 'NONE', *, *, #150204, .F. ) ;
#66715 = EDGE_CURVE ( 'NONE', #22303, #18611, #174014, .T. ) ;
#66716 = CARTESIAN_POINT ( 'NONE',  ( -18.39999999999999858, 11.75000000001113953, -109.7500000000000426 ) ) ;
#66717 = CARTESIAN_POINT ( 'NONE',  ( -21.05000000000000071, 65.49889199258218753, -241.8691648588935266 ) ) ;
#66718 = CARTESIAN_POINT ( 'NONE',  ( 21.05000000000000071, 11.75000000001115907, -160.4851942293460638 ) ) ;
#66719 = EDGE_CURVE ( 'NONE', #128108, #113878, #141670, .T. ) ;
#66720 = DIRECTION ( 'NONE',  ( -1.000000000000000000, -0.000000000000000000, -0.000000000000000000 ) ) ;
#66721 = EDGE_CURVE ( 'NONE', #62775, #99917, #207306, .T. ) ;
#66722 = CARTESIAN_POINT ( 'NONE',  ( -16.89020380669786903, 44.23350592178142904, -235.2550179656449814 ) ) ;
#66724 = VECTOR ( 'NONE', #135171, 1000.000000000000114 ) ;
#66723 = DIRECTION ( 'NONE',  ( 0.000000000000000000, -0.2617529984164856383, -0.9651348961777204138 ) ) ;
#66725 = AXIS2_PLACEMENT_3D ( 'NONE', #248966, #109424, #212411 ) ;
#66726 = CARTESIAN_POINT ( 'NONE',  ( 15.15590539855246277, 62.18784473894375964, -218.4987171750605057 ) ) ;
#66727 = ORIENTED_EDGE ( 'NONE', *, *, #219564, .F. ) ;
#66730 = EDGE_CURVE ( 'NONE', #70460, #180003, #240786, .T. ) ;
#66729 = SPHERICAL_SURFACE ( 'NONE', #194971, 0.1000000000000000056 ) ;
#66728 = DIRECTION ( 'NONE',  ( 0.000000000000000000, -0.4088369013363280513, 0.9126074666063769270 ) ) ;
#66731 = VERTEX_POINT ( 'NONE', #24322 ) ;
#66733 = ORIENTED_EDGE ( 'NONE', *, *, #47955, .F. ) ;
#66732 = CARTESIAN_POINT ( 'NONE',  ( 21.05000000000000071, 64.35000000001176090, -76.53791325517833855 ) ) ;
#66734 = ORIENTED_EDGE ( 'NONE', *, *, #103433, .T. ) ;
#66735 = CARTESIAN_POINT ( 'NONE',  ( -21.59142135623730852, 44.72025695884330787, -237.3380583568817315 ) ) ;
#66736 = CARTESIAN_POINT ( 'NONE',  ( 18.50000972452444969, 10.29326151435342851, -72.45928225104145781 ) ) ;
#66737 = DIRECTION ( 'NONE',  ( 0.000000000000000000, 0.000000000000000000, 1.000000000000000000 ) ) ;
#66738 = ADVANCED_FACE ( 'NONE', ( #223766 ), #103810, .T. ) ;
#66739 = CARTESIAN_POINT ( 'NONE',  ( -23.25000000000000000, 76.00000000001170974, -69.52310748452431710 ) ) ;
#66740 = EDGE_LOOP ( 'NONE', ( #192195, #30714, #248773, #96802 ) ) ;
#66741 = DIRECTION ( 'NONE',  ( -1.000000000000000000, -0.000000000000000000, -0.000000000000000000 ) ) ;
#66742 = DIRECTION ( 'NONE',  ( 1.000000000000000000, 0.000000000000000000, 0.000000000000000000 ) ) ;
#66743 = B_SPLINE_CURVE_WITH_KNOTS ( 'NONE', 3,
 ( #159673, #140078, #219623, #41024, #21460, #180520, #1846, #201354, #160964, #22747, #102214, #108681, #224757, #25311, #243044, #64422 ),
 .UNSPECIFIED., .F., .F.,
 ( 4, 3, 3, 3, 3, 4 ),
 ( 0.000000000000000000, 2.372700795694929657E-05, 5.739057815869540267E-05, 9.073899019181866019E-05, 0.0001243544287365906317, 0.0001585386695601349893 ),
 .UNSPECIFIED. ) ;
#66744 = ORIENTED_EDGE ( 'NONE', *, *, #96704, .F. ) ;
#66745 = LINE ( 'NONE', #148857, #89834 ) ;
#66746 = AXIS2_PLACEMENT_3D ( 'NONE', #216807, #215526, #38201 ) ;
#66747 = AXIS2_PLACEMENT_3D ( 'NONE', #62761, #143579, #4063 ) ;
#66748 = AXIS2_PLACEMENT_3D ( 'NONE', #96820, #117697, #36922 ) ;
#66749 = AXIS2_PLACEMENT_3D ( 'NONE', #58256, #137790, #218607 ) ;
#66750 = VERTEX_POINT ( 'NONE', #7296 ) ;
#66751 = CARTESIAN_POINT ( 'NONE',  ( -21.65000000000000213, 68.75000000001233502, -160.7731074845244166 ) ) ;
#66752 = ADVANCED_FACE ( 'NONE', ( #144225 ), #94354, .T. ) ;
#66753 = ORIENTED_EDGE ( 'NONE', *, *, #248140, .T. ) ;
#66754 = AXIS2_PLACEMENT_3D ( 'NONE', #117019, #231851, #77875 ) ;
#66755 = FACE_OUTER_BOUND ( 'NONE', #169831, .T. ) ;
#66756 = ORIENTED_EDGE ( 'NONE', *, *, #80729, .F. ) ;
#66757 = DIRECTION ( 'NONE',  ( -0.000000000000000000, -0.000000000000000000, -1.000000000000000000 ) ) ;
#66758 = EDGE_CURVE ( 'NONE', #256392, #208088, #26898, .T. ) ;
#66759 = CARTESIAN_POINT ( 'NONE',  ( 20.94560253601876809, 64.25000000001175238, -76.51302397200892358 ) ) ;
#66760 = DIRECTION ( 'NONE',  ( -1.000000000000000000, -0.000000000000000000, -0.000000000000000000 ) ) ;
#66761 = ADVANCED_FACE ( 'NONE', ( #106379 ), #245922, .F. ) ;
#66762 = CARTESIAN_POINT ( 'NONE',  ( -0.8999999999999993561, -11.65000000000000036, 26.00000000000000355 ) ) ;
#66763 = CIRCLE ( 'NONE', #4200, 0.09999999999998898659 ) ;
#66764 = AXIS2_PLACEMENT_3D ( 'NONE', #167615, #11094, #165026 ) ;
#66765 = DIRECTION ( 'NONE',  ( 0.000000000000000000, 0.000000000000000000, 1.000000000000000000 ) ) ;
#66766 = CARTESIAN_POINT ( 'NONE',  ( 22.59999999999999432, 0.1000000000111554016, -21.85042919245520210 ) ) ;
#66767 = DIRECTION ( 'NONE',  ( -0.000000000000000000, 0.1335171055202901413, -0.9910465087640860649 ) ) ;
#66768 = ORIENTED_EDGE ( 'NONE', *, *, #198379, .F. ) ;
#66770 = PLANE ( 'NONE',  #4452 ) ;
#66769 = CARTESIAN_POINT ( 'NONE',  ( -18.59999999999999787, 48.14768554360777841, -246.4498133360871179 ) ) ;
#66771 = VERTEX_POINT ( 'NONE', #127252 ) ;
#66772 = CARTESIAN_POINT ( 'NONE',  ( 21.05000000000000071, 8.776282895303632259, -176.0586289951409071 ) ) ;
#66773 = CARTESIAN_POINT ( 'NONE',  ( -18.42637059832564717, 85.49694546190212918, -163.4140301747244450 ) ) ;
#66774 = DIRECTION ( 'NONE',  ( 0.000000000000000000, 0.000000000000000000, 1.000000000000000000 ) ) ;
#66775 = VERTEX_POINT ( 'NONE', #28184 ) ;
#66777 = EDGE_LOOP ( 'NONE', ( #214251, #43337, #84941, #67857 ) ) ;
#66776 = DIRECTION ( 'NONE',  ( 1.000000000000000000, 0.000000000000000000, 0.000000000000000000 ) ) ;
#66778 = DIRECTION ( 'NONE',  ( -1.000000000000000000, 0.000000000000000000, 0.000000000000000000 ) ) ;
#66779 = CARTESIAN_POINT ( 'NONE',  ( 21.05000000000000071, 35.97645343225767789, -235.9694016464868014 ) ) ;
#66782 = EDGE_CURVE ( 'NONE', #162036, #239074, #32538, .T. ) ;
#66781 = ORIENTED_EDGE ( 'NONE', *, *, #129287, .T. ) ;
#66780 = CARTESIAN_POINT ( 'NONE',  ( -23.25000000000000000, 1.115600667400684642E-11, -167.5000000000000284 ) ) ;
#66783 = TOROIDAL_SURFACE ( 'NONE', #216795, 0.4000000000000005773, 0.1000000000000000056 ) ;
#66784 = CARTESIAN_POINT ( 'NONE',  ( 22.50014994444007499, 11.74971973190327468, -167.4169198432807093 ) ) ;
#66785 = DIRECTION ( 'NONE',  ( 1.000000000000000000, -1.335000415235278971E-16, 2.979993593738921214E-16 ) ) ;
#66786 = VERTEX_POINT ( 'NONE', #122125 ) ;
#66787 = DIRECTION ( 'NONE',  ( 1.000000000000000000, 0.000000000000000000, 0.000000000000000000 ) ) ;
#66788 = ORIENTED_EDGE ( 'NONE', *, *, #103968, .T. ) ;
#66789 = CIRCLE ( 'NONE', #229292, 0.1000000000000000472 ) ;
#66790 = DIRECTION ( 'NONE',  ( 1.000000000000000000, -0.000000000000000000, -0.000000000000000000 ) ) ;
#66791 = CARTESIAN_POINT ( 'NONE',  ( 19.83283456528359423, 34.58225676339163357, -235.1091250525335568 ) ) ;
#66792 = ORIENTED_EDGE ( 'NONE', *, *, #178030, .T. ) ;
#66793 = CARTESIAN_POINT ( 'NONE',  ( -20.94999999999999929, 1.116121084443477685E-11, -69.90000000000003411 ) ) ;
#66794 = EDGE_CURVE ( 'NONE', #231369, #100115, #210900, .T. ) ;
#66795 = DIRECTION ( 'NONE',  ( -1.000000000000000000, 0.000000000000000000, 0.000000000000000000 ) ) ;
#66796 = EDGE_CURVE ( 'NONE', #134353, #60484, #11672, .T. ) ;
#66797 = ORIENTED_EDGE ( 'NONE', *, *, #172201, .F. ) ;
#66798 = DIRECTION ( 'NONE',  ( -1.000000000000000000, 0.000000000000000000, -0.000000000000000000 ) ) ;
#66799 = AXIS2_PLACEMENT_3D ( 'NONE', #6102, #101311, #60949 ) ;
#66800 = EDGE_CURVE ( 'NONE', #84696, #27038, #136534, .T. ) ;
#66801 = EDGE_LOOP ( 'NONE', ( #33858, #221364, #209206, #144957 ) ) ;
#66802 = ORIENTED_EDGE ( 'NONE', *, *, #125657, .F. ) ;
#66804 = EDGE_CURVE ( 'NONE', #86414, #148410, #161517, .T. ) ;
#66803 = CARTESIAN_POINT ( 'NONE',  ( -18.44232395689875759, -9.552282557039388777, -73.84225198480679353 ) ) ;
#66805 = AXIS2_PLACEMENT_3D ( 'NONE', #30113, #207458, #146175 ) ;
#66806 = VERTEX_POINT ( 'NONE', #30745 ) ;
#66807 = CARTESIAN_POINT ( 'NONE',  ( 18.43709777086139923, -0.9152171842606990904, -242.2974985173726736 ) ) ;
#66808 = EDGE_LOOP ( 'NONE', ( #233323, #174179, #91849, #178028 ) ) ;
#66810 = EDGE_LOOP ( 'NONE', ( #124262, #181246, #3848, #114468 ) ) ;
#66809 = DIRECTION ( 'NONE',  ( 1.000000000000000000, 0.000000000000000000, 0.000000000000000000 ) ) ;
#66811 = TOROIDAL_SURFACE ( 'NONE', #29433, 12.77499999999999858, 0.1000000000000000056 ) ;
#66812 = AXIS2_PLACEMENT_3D ( 'NONE', #239921, #23462, #119994 ) ;
#66813 = CARTESIAN_POINT ( 'NONE',  ( -20.95613430942427513, 11.75000000001115552, -73.85716264821988375 ) ) ;
#66814 = EDGE_LOOP ( 'NONE', ( #104509, #146003, #176972, #27164 ) ) ;
#66815 = DIRECTION ( 'NONE',  ( -3.265361837132813093E-16, -1.000000000000000000, -6.982962677686266711E-15 ) ) ;
#66816 = ORIENTED_EDGE ( 'NONE', *, *, #179929, .T. ) ;
#66818 = ORIENTED_EDGE ( 'NONE', *, *, #154673, .T. ) ;
#66817 = ORIENTED_EDGE ( 'NONE', *, *, #175582, .F. ) ;
#66819 = DIRECTION ( 'NONE',  ( 0.000000000000000000, -7.272083257015735086E-15, 1.000000000000000000 ) ) ;
#66820 = DIRECTION ( 'NONE',  ( -0.000000000000000000, -0.000000000000000000, -1.000000000000000000 ) ) ;
#66821 = ORIENTED_EDGE ( 'NONE', *, *, #43945, .T. ) ;
#66822 = AXIS2_PLACEMENT_3D ( 'NONE', #182436, #85850, #187580 ) ;
#66823 = EDGE_CURVE ( 'NONE', #92094, #121951, #46116, .T. ) ;
#66825 = ADVANCED_FACE ( 'NONE', ( #93248 ), #103209, .T. ) ;
#66824 = CIRCLE ( 'NONE', #112615, 12.87499999999999289 ) ;
#66826 = AXIS2_PLACEMENT_3D ( 'NONE', #239828, #45464, #24653 ) ;
#66827 = TOROIDAL_SURFACE ( 'NONE', #21066, 11.65000000000000036, 0.1000000000000000056 ) ;
#66828 = ORIENTED_EDGE ( 'NONE', *, *, #7308, .F. ) ;
#66829 = CARTESIAN_POINT ( 'NONE',  ( 21.30000000000002558, 1.115600667400684642E-11, -67.00000000000004263 ) ) ;
#66830 = CARTESIAN_POINT ( 'NONE',  ( 12.25000000000000000, 66.65000000001155911, -52.77310748452440237 ) ) ;
#66832 = ORIENTED_EDGE ( 'NONE', *, *, #44470, .F. ) ;
#66831 = FACE_OUTER_BOUND ( 'NONE', #248803, .T. ) ;
#66833 = CARTESIAN_POINT ( 'NONE',  ( 21.00000000000000000, 22.61918030723622408, -230.9697045991730988 ) ) ;
#66834 = EDGE_LOOP ( 'NONE', ( #124155, #241344, #121680, #158151, #105958 ) ) ;
#66835 = CYLINDRICAL_SURFACE ( 'NONE', #257670, 4.049999999999998046 ) ;
#66836 = CYLINDRICAL_SURFACE ( 'NONE', #218938, 0.09999999999999939493 ) ;
#66837 = ORIENTED_EDGE ( 'NONE', *, *, #158264, .T. ) ;
#66839 = EDGE_CURVE ( 'NONE', #222677, #52138, #240599, .T. ) ;
#66838 = LINE ( 'NONE', #6859, #173414 ) ;
#66840 = AXIS2_PLACEMENT_3D ( 'NONE', #176546, #78686, #138645 ) ;
#66841 = FACE_OUTER_BOUND ( 'NONE', #7979, .T. ) ;
#66842 = ORIENTED_EDGE ( 'NONE', *, *, #225224, .T. ) ;
#66843 = EDGE_CURVE ( 'NONE', #79119, #160483, #150668, .T. ) ;
#66844 = CARTESIAN_POINT ( 'NONE',  ( 19.75857864376269291, 54.48300931968434213, -228.8005724072070564 ) ) ;
#66846 = EDGE_LOOP ( 'NONE', ( #188009, #139477, #27232, #12909, #213620 ) ) ;
#66845 = ORIENTED_EDGE ( 'NONE', *, *, #252306, .F. ) ;
#66847 = VERTEX_POINT ( 'NONE', #210636 ) ;
#66848 = DIRECTION ( 'NONE',  ( 0.000000000000000000, 0.2128009952263485993, -0.9770955615653341697 ) ) ;
#66849 = VERTEX_POINT ( 'NONE', #48990 ) ;
#66850 = CARTESIAN_POINT ( 'NONE',  ( 21.00000000000000000, 66.25000000001186606, -90.77310748452438816 ) ) ;
#66851 = ORIENTED_EDGE ( 'NONE', *, *, #94401, .T. ) ;
#66852 = EDGE_CURVE ( 'NONE', #75869, #164855, #115712, .T. ) ;
#66853 = CARTESIAN_POINT ( 'NONE',  ( 21.05000000000000071, 11.65000000001116298, -134.0000000000000000 ) ) ;
#66854 = CARTESIAN_POINT ( 'NONE',  ( 22.39999999999999503, 64.25000000001269029, -203.4231074845244507 ) ) ;
#66855 = CIRCLE ( 'NONE', #104427, 0.1000000000000028644 ) ;
#66856 = ORIENTED_EDGE ( 'NONE', *, *, #1149, .T. ) ;
#66857 = VECTOR ( 'NONE', #98857, 1000.000000000000000 ) ;
#66858 = ORIENTED_EDGE ( 'NONE', *, *, #245669, .T. ) ;
#66859 = ADVANCED_FACE ( 'NONE', ( #91966 ), #121061, .T. ) ;
#66860 = VERTEX_POINT ( 'NONE', #94524 ) ;
#66861 = CIRCLE ( 'NONE', #216705, 0.1000000000000028644 ) ;
#66862 = AXIS2_PLACEMENT_3D ( 'NONE', #195238, #96087, #191390 ) ;
#66863 = CARTESIAN_POINT ( 'NONE',  ( -18.43569575749026512, 85.51932773110456765, -129.5501311079648872 ) ) ;
#66864 = VERTEX_POINT ( 'NONE', #176664 ) ;
#66865 = DIRECTION ( 'NONE',  ( -1.836970198721029934E-16, 1.000000000000000000, 0.000000000000000000 ) ) ;
#66866 = EDGE_CURVE ( 'NONE', #20400, #77369, #111237, .T. ) ;
#66868 = ORIENTED_EDGE ( 'NONE', *, *, #143262, .F. ) ;
#66867 = DIRECTION ( 'NONE',  ( -1.000000000000000000, 0.000000000000000000, 0.000000000000000000 ) ) ;
#66869 = FACE_OUTER_BOUND ( 'NONE', #122940, .T. ) ;
#66870 = FACE_OUTER_BOUND ( 'NONE', #30586, .T. ) ;
#66871 = CARTESIAN_POINT ( 'NONE',  ( -16.95709691156562471, 12.41617368651195541, -211.2527161509892153 ) ) ;
#66872 = CARTESIAN_POINT ( 'NONE',  ( 21.05000000000000071, -0.09999999998884512298, -127.5229536182101384 ) ) ;
#66873 = CARTESIAN_POINT ( 'NONE',  ( -18.50000000000000000, 102.4393534156129562, -118.3815988770166427 ) ) ;
#66875 = CARTESIAN_POINT ( 'NONE',  ( 23.14999999999999503, 11.65000000000000746, -12.15000000000000036 ) ) ;
#66874 = CARTESIAN_POINT ( 'NONE',  ( -21.05000000000000071, 0.09779029131994770863, -60.74218538952393232 ) ) ;
#66876 = CYLINDRICAL_SURFACE ( 'NONE', #190691, 0.1000000000000000472 ) ;
#66877 = CARTESIAN_POINT ( 'NONE',  ( 20.94999999999999929, 6.550000000000000711, -10.01702717044001822 ) ) ;
#66878 = DIRECTION ( 'NONE',  ( 0.000000000000000000, -1.000000000000000000, 0.000000000000000000 ) ) ;
#66879 = AXIS2_PLACEMENT_3D ( 'NONE', #1157, #241099, #2449 ) ;
#66880 = ORIENTED_EDGE ( 'NONE', *, *, #187479, .T. ) ;
#66881 = CIRCLE ( 'NONE', #245958, 12.87499999999999467 ) ;
#66882 = AXIS2_PLACEMENT_3D ( 'NONE', #217250, #238106, #85102 ) ;
#66884 = VERTEX_POINT ( 'NONE', #253596 ) ;
#66883 = LINE ( 'NONE', #166017, #19937 ) ;
#66885 = ORIENTED_EDGE ( 'NONE', *, *, #140393, .F. ) ;
#66886 = DIRECTION ( 'NONE',  ( 1.296989514748957922E-15, 0.9887567792719351711, -0.1495327102803594987 ) ) ;
#66887 =( BOUNDED_CURVE ( )  B_SPLINE_CURVE ( 3, ( #140328, #98604, #96064, #178216 ),
 .UNSPECIFIED., .F., .F. ) 
 B_SPLINE_CURVE_WITH_KNOTS ( ( 4, 4 ),
 ( 3.432212674861197854, 3.693332928900583401 ),
 .UNSPECIFIED. ) 
 CURVE ( )  GEOMETRIC_REPRESENTATION_ITEM ( )  RATIONAL_B_SPLINE_CURVE ( ( 1.000000000000000000, 0.9943260843901261525, 0.9943260843901261525, 1.000000000000000000 ) ) 
 REPRESENTATION_ITEM ( '' )  );
#66888 = CARTESIAN_POINT ( 'NONE',  ( 20.74625933824108870, 8.882913521095431975, -142.5551710241120986 ) ) ;
#66890 = DIRECTION ( 'NONE',  ( 1.000000000000000000, 0.000000000000000000, 0.000000000000000000 ) ) ;
#66889 = CARTESIAN_POINT ( 'NONE',  ( 20.12481660106788439, 40.27144177145531501, -237.4941997744894024 ) ) ;
#66891 = ORIENTED_EDGE ( 'NONE', *, *, #226178, .T. ) ;
#66892 = FILL_AREA_STYLE_COLOUR ( '', #122884 ) ;
#66893 = CARTESIAN_POINT ( 'NONE',  ( 18.49999999999998579, -9.321008403350155902, -40.73593824907785432 ) ) ;
#66894 = CIRCLE ( 'NONE', #121095, 0.1000000000000028644 ) ;
#66895 = DIRECTION ( 'NONE',  ( 1.000000000000000000, 0.000000000000000000, 0.000000000000000000 ) ) ;
#66896 = VERTEX_POINT ( 'NONE', #115377 ) ;
#66897 = CARTESIAN_POINT ( 'NONE',  ( -20.54999999999999716, 66.65000000001253966, -182.3731074845244393 ) ) ;
#66898 = DIRECTION ( 'NONE',  ( -1.000000000000000000, 0.000000000000000000, 0.000000000000000000 ) ) ;
#66899 = CARTESIAN_POINT ( 'NONE',  ( 20.95595012432475457, 65.39582078693585743, -61.92733815430646871 ) ) ;
#66901 = ORIENTED_EDGE ( 'NONE', *, *, #61188, .T. ) ;
#66900 = CARTESIAN_POINT ( 'NONE',  ( -16.90137573187933739, 66.05000000001230376, -157.2346900604275390 ) ) ;
#66902 = LINE ( 'NONE', #186876, #81938 ) ;
#66903 = DIRECTION ( 'NONE',  ( 1.000000000000000000, 0.000000000000000000, 0.000000000000000000 ) ) ;
#66904 = DIRECTION ( 'NONE',  ( 0.000000000000000000, 0.000000000000000000, -1.000000000000000000 ) ) ;
#66905 = DIRECTION ( 'NONE',  ( 1.000000000000000000, 0.000000000000000000, 0.000000000000000000 ) ) ;
#66906 = ORIENTED_EDGE ( 'NONE', *, *, #66318, .F. ) ;
#66907 = DIRECTION ( 'NONE',  ( -2.952720810173289605E-16, -1.000000000000000000, -7.086529944415894657E-15 ) ) ;
#66908 = CARTESIAN_POINT ( 'NONE',  ( -18.50000000000000000, 64.35000000001214460, -136.4231074845243938 ) ) ;
#66909 = VECTOR ( 'NONE', #36625, 1000.000000000000000 ) ;
#66912 = DIRECTION ( 'NONE',  ( 1.000000000000000000, 0.000000000000000000, 0.000000000000000000 ) ) ;
#66911 = VECTOR ( 'NONE', #242365, 1000.000000000000000 ) ;
#66910 = CARTESIAN_POINT ( 'NONE',  ( -23.25000000000000000, 71.85000000001157616, -57.17310748452435121 ) ) ;
#66914 = EDGE_CURVE ( 'NONE', #213545, #70203, #197478, .T. ) ;
#66913 = DIRECTION ( 'NONE',  ( 0.000000000000000000, 1.000000000000000000, 0.000000000000000000 ) ) ;
#66915 = CARTESIAN_POINT ( 'NONE',  ( 18.59999999999999076, 6.550000000011156231, -77.01702717044007329 ) ) ;
#66916 = CIRCLE ( 'NONE', #120933, 0.8750000000000007772 ) ;
#66917 = CARTESIAN_POINT ( 'NONE',  ( -18.39999999999999858, 11.47867410001042998, -143.2746932163406655 ) ) ;
#66918 = CARTESIAN_POINT ( 'NONE',  ( -21.14999999999999858, 11.75000000001115552, -134.1000000000000227 ) ) ;
#66919 = DIRECTION ( 'NONE',  ( -0.000000000000000000, -1.000000000000000000, -0.000000000000000000 ) ) ;
#66920 = CARTESIAN_POINT ( 'NONE',  ( 20.84999999999998721, 87.75000000001142553, -36.02310748452423894 ) ) ;
#66921 = ORIENTED_EDGE ( 'NONE', *, *, #149382, .T. ) ;
#66922 = DIRECTION ( 'NONE',  ( -1.000000000000000000, 0.000000000000000000, -0.000000000000000000 ) ) ;
#66923 = AXIS2_PLACEMENT_3D ( 'NONE', #1850, #39752, #237914 ) ;
#66924 = EDGE_LOOP ( 'NONE', ( #192941, #131822, #28050, #90085 ) ) ;
#66925 = VERTEX_POINT ( 'NONE', #256112 ) ;
#66926 = DIRECTION ( 'NONE',  ( 1.000000000000000000, 0.000000000000000000, 0.000000000000000000 ) ) ;
#66927 = SPHERICAL_SURFACE ( 'NONE', #177831, 0.1000000000000000056 ) ;
#66928 = ORIENTED_EDGE ( 'NONE', *, *, #79968, .T. ) ;
#66930 = EDGE_CURVE ( 'NONE', #136769, #58719, #254835, .T. ) ;
#66929 = CIRCLE ( 'NONE', #220860, 0.1000000000000024342 ) ;
#66931 = ORIENTED_EDGE ( 'NONE', *, *, #49493, .T. ) ;
#66932 = PRESENTATION_STYLE_ASSIGNMENT (( #189460 ) ) ;
#66933 = ORIENTED_EDGE ( 'NONE', *, *, #71758, .T. ) ;
#66934 = CARTESIAN_POINT ( 'NONE',  ( -21.05000000000000071, 4.273531877263400780, -211.9976340888692050 ) ) ;
#66935 = ORIENTED_EDGE ( 'NONE', *, *, #175460, .F. ) ;
#66936 = DIRECTION ( 'NONE',  ( 0.000000000000000000, -0.000000000000000000, 1.000000000000000000 ) ) ;
#66937 = CYLINDRICAL_SURFACE ( 'NONE', #66114, 0.1000000000000024342 ) ;
#66938 = CARTESIAN_POINT ( 'NONE',  ( -16.93433913041102912, 30.30801039134145825, -234.7980092385606383 ) ) ;
#66939 = DIRECTION ( 'NONE',  ( 1.186688945009009831E-16, -0.9770955615653316162, -0.2128009952263604232 ) ) ;
#66940 = DIRECTION ( 'NONE',  ( 0.7070776581708965169, 4.937903618720407826E-15, -0.7071359030027827286 ) ) ;
#66941 = EDGE_CURVE ( 'NONE', #114879, #24454, #55371, .T. ) ;
#66942 = DIRECTION ( 'NONE',  ( -0.000000000000000000, 0.1350103645451945777, -0.9908441862701590219 ) ) ;
#66943 = EDGE_CURVE ( 'NONE', #170209, #2619, #124097, .T. ) ;
#66944 = FACE_OUTER_BOUND ( 'NONE', #16231, .T. ) ;
#66946 = ORIENTED_EDGE ( 'NONE', *, *, #245462, .T. ) ;
#66945 = CARTESIAN_POINT ( 'NONE',  ( -21.05000000000000071, 1.115600667400684642E-11, -67.00000000000004263 ) ) ;
#66948 = CARTESIAN_POINT ( 'NONE',  ( 21.09546886439553504, 8.878553113026075749, -79.23709385055506971 ) ) ;
#66947 = CARTESIAN_POINT ( 'NONE',  ( 20.96077737575330957, 11.62390063400469487, -26.64079195710655412 ) ) ;
#66949 = DIRECTION ( 'NONE',  ( 2.952720810173288126E-16, -0.9770955615653313941, -0.2128009952263603677 ) ) ;
#66950 = ORIENTED_EDGE ( 'NONE', *, *, #167658, .F. ) ;
#66951 = LINE ( 'NONE', #179545, #248063 ) ;
#66953 = EDGE_CURVE ( 'NONE', #133285, #247461, #19862, .T. ) ;
#66952 = DIRECTION ( 'NONE',  ( 0.000000000000000000, 1.000000000000000000, 0.000000000000000000 ) ) ;
#66954 = DIRECTION ( 'NONE',  ( -0.000000000000000000, 0.4721928772777345684, 0.8814952561688429444 ) ) ;
#66955 = ORIENTED_EDGE ( 'NONE', *, *, #16946, .F. ) ;
#66956 = CIRCLE ( 'NONE', #4570, 0.2000000000000048683 ) ;
#66957 = CARTESIAN_POINT ( 'NONE',  ( -16.93860193097148326, 66.00689223268274475, -115.6229691172175222 ) ) ;
#66958 = ADVANCED_FACE ( 'NONE', ( #196205 ), #136197, .F. ) ;
#66959 = CIRCLE ( 'NONE', #314, 0.9000000000000014655 ) ;
#66960 = CARTESIAN_POINT ( 'NONE',  ( -21.65000000000000213, 7.250000000011138646, -188.3499999999999659 ) ) ;
#66961 = VERTEX_POINT ( 'NONE', #98341 ) ;
#66962 = DIRECTION ( 'NONE',  ( 1.000000000000000000, 0.000000000000000000, 0.000000000000000000 ) ) ;
#66963 = DIRECTION ( 'NONE',  ( 0.000000000000000000, 0.9893560106964510714, -0.1455152366551481502 ) ) ;
#66964 = ADVANCED_FACE ( 'NONE', ( #177941 ), #257401, .F. ) ;
#66966 = CARTESIAN_POINT ( 'NONE',  ( -22.59999970745345976, -0.009356377315828669564, -21.74948679233078863 ) ) ;
#66965 = CIRCLE ( 'NONE', #237835, 0.1000000000000028644 ) ;
#66967 = DIRECTION ( 'NONE',  ( 0.000000000000000000, -6.982962677686266711E-15, 1.000000000000000000 ) ) ;
#66968 = VERTEX_POINT ( 'NONE', #137495 ) ;
#66969 = ORIENTED_EDGE ( 'NONE', *, *, #16266, .T. ) ;
#66970 = ADVANCED_FACE ( 'NONE', ( #214477 ), #147685, .T. ) ;
#66971 = CARTESIAN_POINT ( 'NONE',  ( 18.54999999999999716, 67.25000000001183764, -90.37310748452436826 ) ) ;
#66972 = DIRECTION ( 'NONE',  ( 0.000000000000000000, -0.2128009952263603677, 0.9770955615653313941 ) ) ;
#66973 = CARTESIAN_POINT ( 'NONE',  ( 18.59999999999999432, 43.57568952063339651, -245.1784935019914826 ) ) ;
#66974 = DIRECTION ( 'NONE',  ( 0.000000000000000000, 0.000000000000000000, -1.000000000000000000 ) ) ;
#66975 = AXIS2_PLACEMENT_3D ( 'NONE', #92042, #170354, #28263 ) ;
#66976 = SPHERICAL_SURFACE ( 'NONE', #7576, 0.1000000000000000056 ) ;
#66978 = CYLINDRICAL_SURFACE ( 'NONE', #172112, 0.09999999999999892308 ) ;
#66977 = VECTOR ( 'NONE', #25402, 1000.000000000000000 ) ;
#66979 = EDGE_LOOP ( 'NONE', ( #172360, #205390, #176161, #74464 ) ) ;
#66980 = DIRECTION ( 'NONE',  ( 1.000000000000000000, 7.304098846218134667E-16, 4.639676173203993355E-30 ) ) ;
#66981 = CIRCLE ( 'NONE', #87804, 0.09999999999999939493 ) ;
#66983 = ORIENTED_EDGE ( 'NONE', *, *, #124086, .T. ) ;
#66982 = DIRECTION ( 'NONE',  ( 0.000000000000000000, 0.000000000000000000, -1.000000000000000000 ) ) ;
#66984 = DIRECTION ( 'NONE',  ( 1.040834085586049673E-13, 0.7899159663865300551, 0.6132151058540831201 ) ) ;
#66985 = DIRECTION ( 'NONE',  ( 1.000000000000000000, 1.541880601228652350E-16, 2.878400969107352921E-16 ) ) ;
#66986 = CARTESIAN_POINT ( 'NONE',  ( -23.39999999999994529, 82.84256550613280012, -26.34830530078816935 ) ) ;
#66987 = CIRCLE ( 'NONE', #221091, 11.74999999999999645 ) ;
#66988 = CARTESIAN_POINT ( 'NONE',  ( -16.89935556175729658, 66.05000000001207638, -123.3834311216395463 ) ) ;
#66990 = VERTEX_POINT ( 'NONE', #64406 ) ;
#66989 = CARTESIAN_POINT ( 'NONE',  ( 21.05000000000000071, 43.36285386911620776, -234.7972500504784534 ) ) ;
#66991 = CARTESIAN_POINT ( 'NONE',  ( -23.24999999999999645, -9.599999999988845900, -73.60018939122203108 ) ) ;
#66992 = DIRECTION ( 'NONE',  ( -0.000000000000000000, 7.272083257015735086E-15, -1.000000000000000000 ) ) ;
#66993 = VECTOR ( 'NONE', #101424, 1000.000000000000000 ) ;
#66994 = DIRECTION ( 'NONE',  ( 0.000000000000000000, 0.8660254037844383745, -0.5000000000000003331 ) ) ;
#66995 = LINE ( 'NONE', #226034, #61599 ) ;
#66996 = AXIS2_PLACEMENT_3D ( 'NONE', #8688, #186042, #227721 ) ;
#66997 = ORIENTED_EDGE ( 'NONE', *, *, #89019, .F. ) ;
#66998 = CARTESIAN_POINT ( 'NONE',  ( -15.57281606413132025, 66.62934494888880010, -152.4972842285435206 ) ) ;
#66999 = CARTESIAN_POINT ( 'NONE',  ( -16.83558968593868954, 66.05000000001201954, -115.6854126721413110 ) ) ;
#67000 = CARTESIAN_POINT ( 'NONE',  ( 5.900000000000059863, 64.35000000001120668, -25.92310748452479174 ) ) ;
#67001 = ORIENTED_EDGE ( 'NONE', *, *, #188089, .T. ) ;
#67003 = CYLINDRICAL_SURFACE ( 'NONE', #180224, 0.09999999999999939493 ) ;
#67002 = AXIS2_PLACEMENT_3D ( 'NONE', #205511, #3458, #63433 ) ;
#67004 = AXIS2_PLACEMENT_3D ( 'NONE', #157906, #156612, #36657 ) ;
#67005 = AXIS2_PLACEMENT_3D ( 'NONE', #85839, #225367, #126276 ) ;
#67006 = EDGE_LOOP ( 'NONE', ( #109774, #69796 ) ) ;
#67007 = AXIS2_PLACEMENT_3D ( 'NONE', #96103, #174430, #234339 ) ;
#67008 = CIRCLE ( 'NONE', #212765, 0.1000000000000028644 ) ;
#67009 = EDGE_CURVE ( 'NONE', #195092, #105820, #53168, .T. ) ;
#67010 = CARTESIAN_POINT ( 'NONE',  ( 22.37643362114956247, 59.84542367231799176, -233.9546800015663166 ) ) ;
#67012 = ADVANCED_FACE ( 'NONE', ( #65676 ), #86448, .F. ) ;
#67011 = CARTESIAN_POINT ( 'NONE',  ( -18.59999999999999787, 80.80934863333322937, -192.8037999715871535 ) ) ;
#67013 = DIRECTION ( 'NONE',  ( 1.000000000000000000, 0.000000000000000000, 0.000000000000000000 ) ) ;
#67014 = CARTESIAN_POINT ( 'NONE',  ( 18.39999999999999858, -9.519327731081283162, -174.4729763765593020 ) ) ;
#67015 = ORIENTED_EDGE ( 'NONE', *, *, #196871, .F. ) ;
#67016 = ADVANCED_FACE ( 'NONE', ( #143927 ), #145206, .T. ) ;
#67017 = ADVANCED_FACE ( 'NONE', ( #163502 ), #49444, .T. ) ;
#67018 = DIRECTION ( 'NONE',  ( 1.000000000000000000, 0.000000000000000000, 0.000000000000000000 ) ) ;
#67019 = AXIS2_PLACEMENT_3D ( 'NONE', #148323, #68791, #227853 ) ;
#67020 = EDGE_CURVE ( 'NONE', #186223, #74336, #219740, .T. ) ;
#67021 = CARTESIAN_POINT ( 'NONE',  ( -21.07928932188134041, 6.162520550847337297, -199.5566553493351307 ) ) ;
#67022 = CARTESIAN_POINT ( 'NONE',  ( 15.74999999999999645, 9.349999999999983658, -16.75000000000000000 ) ) ;
#67023 = DIRECTION ( 'NONE',  ( -1.000000000000000000, 0.000000000000000000, 0.000000000000000000 ) ) ;
#67024 = EDGE_CURVE ( 'NONE', #231870, #34933, #253067, .T. ) ;
#67027 = EDGE_CURVE ( 'NONE', #16177, #51868, #28254, .T. ) ;
#67026 = EDGE_CURVE ( 'NONE', #213186, #190383, #140641, .T. ) ;
#67025 = CARTESIAN_POINT ( 'NONE',  ( 23.14999999999999858, 64.35000000001195986, -110.0379132551783243 ) ) ;
#67028 = ORIENTED_EDGE ( 'NONE', *, *, #230815, .T. ) ;
#67030 = ORIENTED_EDGE ( 'NONE', *, *, #128318, .T. ) ;
#67029 = CARTESIAN_POINT ( 'NONE',  ( 20.88420186297724257, 10.33025634372637391, -106.0870929282639281 ) ) ;
#67031 = VERTEX_POINT ( 'NONE', #125652 ) ;
#67032 = DIRECTION ( 'NONE',  ( 0.000000000000000000, -0.2617529984165031243, -0.9651348961777157509 ) ) ;
#67033 = ORIENTED_EDGE ( 'NONE', *, *, #218113, .F. ) ;
#67034 = CARTESIAN_POINT ( 'NONE',  ( 21.09696443733127325, 65.27599011609358115, -124.2883299574761509 ) ) ;
#67035 = CARTESIAN_POINT ( 'NONE',  ( -6.000000000000002665, -11.34999999999999964, 13.90000000000000213 ) ) ;
#67036 = ADVANCED_FACE ( 'NONE', ( #82641 ), #205173, .T. ) ;
#67037 = CARTESIAN_POINT ( 'NONE',  ( -20.94999999999999929, 87.48912529308798014, -100.0231074845242318 ) ) ;
#67038 = EDGE_LOOP ( 'NONE', ( #180659, #8478, #75739, #79597 ) ) ;
#67039 = CARTESIAN_POINT ( 'NONE',  ( -16.90202395485742670, 66.03405545546095823, -56.92612120578434087 ) ) ;
#67040 = CARTESIAN_POINT ( 'NONE',  ( 19.88284271247461987, 11.69142135624847256, -91.75000000000005684 ) ) ;
#67041 = CARTESIAN_POINT ( 'NONE',  ( 20.74897398619109268, 10.59569302167756888, -41.17931145625621525 ) ) ;
#67043 = VERTEX_POINT ( 'NONE', #220890 ) ;
#67042 = VECTOR ( 'NONE', #171726, 999.9999999999998863 ) ;
#67044 = DIRECTION ( 'NONE',  ( 0.000000000000000000, -0.9999176327611369874, 0.01283462868041987913 ) ) ;
#67045 = EDGE_CURVE ( 'NONE', #59875, #41194, #215645, .T. ) ;
#67047 = ORIENTED_EDGE ( 'NONE', *, *, #247502, .F. ) ;
#67046 = LINE ( 'NONE', #48754, #213280 ) ;
#67048 = FACE_OUTER_BOUND ( 'NONE', #115121, .T. ) ;
#67049 = LINE ( 'NONE', #206556, #189629 ) ;
#67050 = EDGE_CURVE ( 'NONE', #83828, #155749, #183076, .T. ) ;
#67051 = EDGE_CURVE ( 'NONE', #72236, #54023, #203185, .T. ) ;
#67052 = VECTOR ( 'NONE', #139930, 1000.000000000000000 ) ;
#67053 = ORIENTED_EDGE ( 'NONE', *, *, #158079, .T. ) ;
#67054 = DIRECTION ( 'NONE',  ( 1.000000000000000000, 0.000000000000000000, 0.000000000000000000 ) ) ;
#67056 = ADVANCED_FACE ( 'NONE', ( #5679 ), #200065, .T. ) ;
#67055 = DIRECTION ( 'NONE',  ( 0.000000000000000000, 0.000000000000000000, -1.000000000000000000 ) ) ;
#67057 = VECTOR ( 'NONE', #227596, 999.9999999999998863 ) ;
#67058 = DIRECTION ( 'NONE',  ( 0.000000000000000000, -1.000000000000000000, -0.000000000000000000 ) ) ;
#67059 = VERTEX_POINT ( 'NONE', #186944 ) ;
#67060 = DIRECTION ( 'NONE',  ( 0.000000000000000000, 0.8660254037844377084, 0.5000000000000016653 ) ) ;
#67061 = EDGE_CURVE ( 'NONE', #221635, #174969, #29171, .T. ) ;
#67062 = CARTESIAN_POINT ( 'NONE',  ( 20.94999999999999929, 78.04167338765999773, -195.9950552943387265 ) ) ;
#67063 = EDGE_CURVE ( 'NONE', #12413, #153891, #24332, .T. ) ;
#67064 = ORIENTED_EDGE ( 'NONE', *, *, #241972, .F. ) ;
#67065 = CIRCLE ( 'NONE', #46201, 0.1000000000000028644 ) ;
#67066 = AXIS2_PLACEMENT_3D ( 'NONE', #157353, #80309, #239429 ) ;
#67068 = EDGE_LOOP ( 'NONE', ( #217723, #225146, #139549, #152415 ) ) ;
#67067 = AXIS2_PLACEMENT_3D ( 'NONE', #247631, #148540, #199267 ) ;
#67069 = DIRECTION ( 'NONE',  ( 0.000000000000000000, -6.982962677686266711E-15, 1.000000000000000000 ) ) ;
#67070 = VERTEX_POINT ( 'NONE', #8293 ) ;
#67071 = CYLINDRICAL_SURFACE ( 'NONE', #210035, 0.1000000000000002554 ) ;
#67072 = CARTESIAN_POINT ( 'NONE',  ( -16.82055514392354567, 66.05000000001255955, -182.6999055590671048 ) ) ;
#67074 = ORIENTED_EDGE ( 'NONE', *, *, #12872, .T. ) ;
#67073 = CARTESIAN_POINT ( 'NONE',  ( 20.94999999999999574, -1.360870587180885716, -142.0729979270909951 ) ) ;
#67075 = CARTESIAN_POINT ( 'NONE',  ( -23.49999999999994316, 74.94272479589878344, -8.023107484524793165 ) ) ;
#67076 = DIRECTION ( 'NONE',  ( 0.000000000000000000, 0.1332476588733589318, -0.9910827722268049644 ) ) ;
#67077 = CYLINDRICAL_SURFACE ( 'NONE', #10244, 4.049999999999994493 ) ;
#67078 = CARTESIAN_POINT ( 'NONE',  ( -20.94999999999999929, 43.35377423437995503, -245.1717807829448930 ) ) ;
#67079 = PLANE ( 'NONE',  #197762 ) ;
#67080 = CARTESIAN_POINT ( 'NONE',  ( -20.64999999999999858, 1.115600667400684642E-11, -200.9999999999999432 ) ) ;
#67081 = DIRECTION ( 'NONE',  ( -1.000000000000000000, -2.885090398161910739E-16, -6.283419270304611573E-17 ) ) ;
#67082 = CARTESIAN_POINT ( 'NONE',  ( -18.40000000000000568, -9.499999999988851584, -107.4993620971801391 ) ) ;
#67084 = ORIENTED_EDGE ( 'NONE', *, *, #224780, .F. ) ;
#67083 = FACE_OUTER_BOUND ( 'NONE', #153121, .T. ) ;
#67085 = DIRECTION ( 'NONE',  ( 0.000000000000000000, -0.2128009952263602012, 0.9770955615653315052 ) ) ;
#67086 = CIRCLE ( 'NONE', #204618, 6.329289321881370611 ) ;
#67087 = VERTEX_POINT ( 'NONE', #51222 ) ;
#67088 = FACE_OUTER_BOUND ( 'NONE', #208585, .T. ) ;
#67089 = DIRECTION ( 'NONE',  ( -1.186688945009009831E-16, 0.9770955615653313941, 0.2128009952263603677 ) ) ;
#67090 = DIRECTION ( 'NONE',  ( 1.000000000000000000, 0.000000000000000000, 0.000000000000000000 ) ) ;
#67091 = DIRECTION ( 'NONE',  ( 0.000000000000000000, 1.000000000000000000, 0.000000000000000000 ) ) ;
#67092 = ORIENTED_EDGE ( 'NONE', *, *, #218882, .T. ) ;
#67093 = FACE_OUTER_BOUND ( 'NONE', #223992, .T. ) ;
#67094 = AXIS2_PLACEMENT_3D ( 'NONE', #75105, #111631, #71241 ) ;
#67095 = EDGE_CURVE ( 'NONE', #171580, #66786, #253251, .T. ) ;
#67096 = AXIS2_PLACEMENT_3D ( 'NONE', #192159, #13511, #50052 ) ;
#67097 = CIRCLE ( 'NONE', #212860, 11.80000000000000426 ) ;
#67098 = DIRECTION ( 'NONE',  ( -1.000000000000000000, 0.000000000000000000, 0.000000000000000000 ) ) ;
#67099 = AXIS2_PLACEMENT_3D ( 'NONE', #153614, #131426, #113151 ) ;
#67100 = EDGE_CURVE ( 'NONE', #15908, #15171, #107500, .T. ) ;
#67101 = VERTEX_POINT ( 'NONE', #167382 ) ;
#67102 = CARTESIAN_POINT ( 'NONE',  ( 21.04999999999999716, 75.98528214348870335, -209.8678308886149750 ) ) ;
#67103 = DIRECTION ( 'NONE',  ( 0.000000000000000000, 0.000000000000000000, -1.000000000000000000 ) ) ;
#67104 = EDGE_CURVE ( 'NONE', #149131, #59064, #174195, .T. ) ;
#67105 = ORIENTED_EDGE ( 'NONE', *, *, #129606, .F. ) ;
#67107 = ADVANCED_FACE ( 'NONE', ( #12156 ), #189493, .T. ) ;
#67106 = DIRECTION ( 'NONE',  ( 1.000000000000000000, 0.000000000000000000, 1.073024830501117725E-15 ) ) ;
#67108 = ORIENTED_EDGE ( 'NONE', *, *, #211240, .T. ) ;
#67109 = CARTESIAN_POINT ( 'NONE',  ( -12.84409460144754433, 9.410682294279110849, -48.93114344194827936 ) ) ;
#67110 = VERTEX_POINT ( 'NONE', #210342 ) ;
#67111 = CIRCLE ( 'NONE', #121138, 0.09999999999999939493 ) ;
#67112 = CARTESIAN_POINT ( 'NONE',  ( -22.94999999999999929, 0.000000000000000000, 3.900000000000000355 ) ) ;
#67113 = DIRECTION ( 'NONE',  ( 0.000000000000000000, -0.9126074666063545004, -0.4088369013363783999 ) ) ;
#67114 = ORIENTED_EDGE ( 'NONE', *, *, #85000, .F. ) ;
#67115 = ORIENTED_EDGE ( 'NONE', *, *, #177442, .F. ) ;
#67116 = LINE ( 'NONE', #146629, #61123 ) ;
#67118 = ORIENTED_EDGE ( 'NONE', *, *, #246282, .F. ) ;
#67117 = CARTESIAN_POINT ( 'NONE',  ( 18.59999999999999432, -1.866714910046153308, -45.25267524628200988 ) ) ;
#67119 = CARTESIAN_POINT ( 'NONE',  ( 21.05000000000000071, 67.22371710472012296, -191.3731074845244109 ) ) ;
#67120 = EDGE_LOOP ( 'NONE', ( #225179, #173745, #199436, #218808 ) ) ;
#67121 = EDGE_CURVE ( 'NONE', #135643, #68978, #40908, .T. ) ;
#67122 = EDGE_CURVE ( 'NONE', #149997, #20295, #215279, .T. ) ;
#67123 = VERTEX_POINT ( 'NONE', #246880 ) ;
#67124 = FACE_OUTER_BOUND ( 'NONE', #219567, .T. ) ;
#67126 = FACE_OUTER_BOUND ( 'NONE', #239553, .T. ) ;
#67125 = AXIS2_PLACEMENT_3D ( 'NONE', #185031, #6392, #246298 ) ;
#67127 = DIRECTION ( 'NONE',  ( 0.000000000000000000, 0.8814952561688476074, -0.4721928772777262417 ) ) ;
#67128 = CARTESIAN_POINT ( 'NONE',  ( -16.78270389226382875, 9.947372616617009555, -20.84120703691148080 ) ) ;
#67129 = DIRECTION ( 'NONE',  ( 1.000000000000000000, 0.000000000000000000, 0.000000000000000000 ) ) ;
#67130 = CARTESIAN_POINT ( 'NONE',  ( 20.94999999999999929, -1.835341550224413698, -11.55515129256298046 ) ) ;
#67131 = TOROIDAL_SURFACE ( 'NONE', #137853, 2.100000000000002309, 0.1000000000000000056 ) ;
#67132 = ORIENTED_EDGE ( 'NONE', *, *, #229230, .F. ) ;
#67133 = LINE ( 'NONE', #226167, #8602 ) ;
#67135 = EDGE_CURVE ( 'NONE', #47002, #248655, #52102, .T. ) ;
#67134 = DIRECTION ( 'NONE',  ( 1.000000000000000000, -0.000000000000000000, -0.000000000000000000 ) ) ;
#67136 = CARTESIAN_POINT ( 'NONE',  ( 23.25000000000000000, 69.45000000001205365, -124.1731074845243370 ) ) ;
#67137 = DIRECTION ( 'NONE',  ( 0.000000000000000000, 0.1350103645451974088, -0.9908441862701587999 ) ) ;
#67138 = AXIS2_PLACEMENT_3D ( 'NONE', #55513, #65818, #125786 ) ;
#67139 = ORIENTED_EDGE ( 'NONE', *, *, #195714, .F. ) ;
#67140 = EDGE_CURVE ( 'NONE', #230477, #52139, #232441, .T. ) ;
#67141 = CARTESIAN_POINT ( 'NONE',  ( 18.51024323315077069, 10.31104185824064245, -106.0204516983106373 ) ) ;
#67142 = VERTEX_POINT ( 'NONE', #48677 ) ;
#67143 = CARTESIAN_POINT ( 'NONE',  ( 15.75000000000000000, 9.350000000011137402, -117.0185689574026924 ) ) ;
#67144 = EDGE_LOOP ( 'NONE', ( #196834, #248573, #118900, #163346 ) ) ;
#67145 = AXIS2_PLACEMENT_3D ( 'NONE', #56351, #233741, #216725 ) ;
#67146 = CARTESIAN_POINT ( 'NONE',  ( -15.70407651835961360, 25.90710817316711001, -233.1781447626815122 ) ) ;
#67147 = DIRECTION ( 'NONE',  ( 1.000000000000000000, 0.000000000000000000, 0.000000000000000000 ) ) ;
#67148 = ORIENTED_EDGE ( 'NONE', *, *, #82177, .F. ) ;
#67149 = AXIS2_PLACEMENT_3D ( 'NONE', #118624, #244960, #3795 ) ;
#67150 = ORIENTED_EDGE ( 'NONE', *, *, #223855, .F. ) ;
#67152 = EDGE_LOOP ( 'NONE', ( #13459, #61345, #210632, #158074 ) ) ;
#67151 = DIRECTION ( 'NONE',  ( 0.000000000000000000, 0.000000000000000000, -1.000000000000000000 ) ) ;
#67153 = CARTESIAN_POINT ( 'NONE',  ( 23.14999999999999503, 61.45319073932094511, -212.2704122313080006 ) ) ;
#67154 = VERTEX_POINT ( 'NONE', #70851 ) ;
#67155 = ADVANCED_FACE ( 'NONE', ( #150372 ), #147800, .F. ) ;
#67156 = CARTESIAN_POINT ( 'NONE',  ( -22.49917693094574389, 0.08522996423282767908, -21.85020421546933989 ) ) ;
#67157 = VECTOR ( 'NONE', #69791, 1000.000000000000000 ) ;
#67158 = DIRECTION ( 'NONE',  ( 0.000000000000000000, 0.8660254037844385966, -0.5000000000000003331 ) ) ;
#67159 = ADVANCED_FACE ( 'NONE', ( #171257 ), #73420, .T. ) ;
#67160 = ORIENTED_EDGE ( 'NONE', *, *, #70675, .T. ) ;
#67161 = CARTESIAN_POINT ( 'NONE',  ( 18.59999999999999076, 69.55000000001159322, -59.50608031408435039 ) ) ;
#67162 = DIRECTION ( 'NONE',  ( 0.000000000000000000, 1.000000000000000000, 2.891205793294679805E-16 ) ) ;
#67164 = EDGE_CURVE ( 'NONE', #161458, #193922, #124277, .T. ) ;
#67163 = CIRCLE ( 'NONE', #146433, 0.1000000000000028644 ) ;
#67165 = VECTOR ( 'NONE', #209818, 1000.000000000000227 ) ;
#67166 = VERTEX_POINT ( 'NONE', #13425 ) ;
#67167 = DIRECTION ( 'NONE',  ( 4.239556034732056127E-17, 0.8127272543710951647, -0.5826443254700257590 ) ) ;
#67168 = AXIS2_PLACEMENT_3D ( 'NONE', #73749, #132420, #93277 ) ;
#67169 = DIRECTION ( 'NONE',  ( 0.000000000000000000, 0.000000000000000000, -1.000000000000000000 ) ) ;
#67170 = EDGE_CURVE ( 'NONE', #133244, #2313, #194462, .T. ) ;
#67171 = VECTOR ( 'NONE', #103603, 1000.000000000000000 ) ;
#67172 = CARTESIAN_POINT ( 'NONE',  ( -18.59999999999999787, 0.5876173420563349792, -209.1618981382189588 ) ) ;
#67174 = VERTEX_POINT ( 'NONE', #126944 ) ;
#67173 = DIRECTION ( 'NONE',  ( 0.000000000000000000, 0.000000000000000000, -1.000000000000000000 ) ) ;
#67175 = CARTESIAN_POINT ( 'NONE',  ( -21.05000000000000071, 1.115600667400684642E-11, -155.8000000000000398 ) ) ;
#67176 = DIRECTION ( 'NONE',  ( 0.000000000000000000, 0.2617529984165024026, 0.9651348961777158619 ) ) ;
#67177 = LINE ( 'NONE', #108867, #98518 ) ;
#67178 = EDGE_CURVE ( 'NONE', #116285, #128410, #206480, .T. ) ;
#67180 = DIRECTION ( 'NONE',  ( 0.000000000000000000, -0.2128009952263603677, 0.9770955615653313941 ) ) ;
#67179 = DIRECTION ( 'NONE',  ( 0.000000000000000000, -7.172728831056617961E-15, 1.000000000000000000 ) ) ;
#67181 = CARTESIAN_POINT ( 'NONE',  ( -20.94999027547553894, 65.70673848567030007, -164.5638252334829588 ) ) ;
#67182 = DIRECTION ( 'NONE',  ( -1.000000000000000000, 3.151514657663852580E-16, -8.547182517843351137E-17 ) ) ;
#67183 = FACE_OUTER_BOUND ( 'NONE', #62546, .T. ) ;
#67184 = AXIS2_PLACEMENT_3D ( 'NONE', #148507, #54197, #197563 ) ;
#67185 = CARTESIAN_POINT ( 'NONE',  ( 18.59999999999999076, 78.48087866980282001, -232.8271061603568910 ) ) ;
#67186 = AXIS2_PLACEMENT_3D ( 'NONE', #66457, #2618, #41787 ) ;
#67187 = AXIS2_PLACEMENT_3D ( 'NONE', #200379, #21752, #204215 ) ;
#67189 = ORIENTED_EDGE ( 'NONE', *, *, #120101, .F. ) ;
#67188 = CIRCLE ( 'NONE', #17145, 0.1000000000000054040 ) ;
#67190 = ORIENTED_EDGE ( 'NONE', *, *, #90833, .T. ) ;
#67191 = CARTESIAN_POINT ( 'NONE',  ( -21.05000000000000071, 61.95000000001265050, -198.0094124137634708 ) ) ;
#67192 = ORIENTED_EDGE ( 'NONE', *, *, #160251, .F. ) ;
#67193 = DIRECTION ( 'NONE',  ( -1.000000000000000000, -0.000000000000000000, -0.000000000000000000 ) ) ;
#67194 = EDGE_LOOP ( 'NONE', ( #22214, #228303, #170885, #151438 ) ) ;
#67195 = PLANE ( 'NONE',  #32697 ) ;
#67196 = CYLINDRICAL_SURFACE ( 'NONE', #162386, 0.09999999999999895084 ) ;
#67197 = ORIENTED_EDGE ( 'NONE', *, *, #22329, .T. ) ;
#67198 = FACE_OUTER_BOUND ( 'NONE', #178613, .T. ) ;
#67199 = ORIENTED_EDGE ( 'NONE', *, *, #66443, .T. ) ;
#67200 = ORIENTED_EDGE ( 'NONE', *, *, #18480, .T. ) ;
#67201 = CARTESIAN_POINT ( 'NONE',  ( -23.25000000000000000, 76.00000000001244871, -170.0231074845243597 ) ) ;
#67202 = CARTESIAN_POINT ( 'NONE',  ( -23.15000000000000213, 56.06656052939784729, -228.0911609752645290 ) ) ;
#67204 = ORIENTED_EDGE ( 'NONE', *, *, #133147, .T. ) ;
#67203 = DIRECTION ( 'NONE',  ( 0.000000000000000000, 0.000000000000000000, 1.000000000000000000 ) ) ;
#67205 = CARTESIAN_POINT ( 'NONE',  ( -22.94999999999999929, 8.000000000000000000, -1.212568896937008089 ) ) ;
#67207 = VERTEX_POINT ( 'NONE', #253296 ) ;
#67206 = CARTESIAN_POINT ( 'NONE',  ( -18.59999999999999787, -1.835859311432481045, -112.0044391687985694 ) ) ;
#67208 = DIRECTION ( 'NONE',  ( 0.000000000000000000, 0.9126074666063773710, 0.4088369013363274962 ) ) ;
#67209 = FACE_OUTER_BOUND ( 'NONE', #228482, .T. ) ;
#67210 = AXIS2_PLACEMENT_3D ( 'NONE', #8772, #129976, #113006 ) ;
#67212 = VERTEX_POINT ( 'NONE', #19851 ) ;
#67211 = DIRECTION ( 'NONE',  ( 1.000000000000000000, 0.000000000000000000, 0.000000000000000000 ) ) ;
#67213 = LINE ( 'NONE', #132006, #222240 ) ;
#67214 = FACE_OUTER_BOUND ( 'NONE', #167492, .T. ) ;
#67215 = DIRECTION ( 'NONE',  ( 0.000000000000000000, -0.2128009952263603954, 0.9770955615653315052 ) ) ;
#67217 = FACE_OUTER_BOUND ( 'NONE', #150777, .T. ) ;
#67216 = CARTESIAN_POINT ( 'NONE',  ( -20.94999999999999929, 66.97496366775517629, -235.8217698210967512 ) ) ;
#67218 = CARTESIAN_POINT ( 'NONE',  ( 18.49999999999978328, 10.28015861706823841, -91.72457207120132239 ) ) ;
#67219 = DIRECTION ( 'NONE',  ( 0.000000000000000000, 0.000000000000000000, -1.000000000000000000 ) ) ;
#67220 = DIRECTION ( 'NONE',  ( -1.000000000000000000, 0.000000000000000000, 0.000000000000000000 ) ) ;
#67221 = FACE_OUTER_BOUND ( 'NONE', #55045, .T. ) ;
#67222 = ORIENTED_EDGE ( 'NONE', *, *, #81045, .F. ) ;
#67223 = ORIENTED_EDGE ( 'NONE', *, *, #220982, .T. ) ;
#67224 = VERTEX_POINT ( 'NONE', #158107 ) ;
#67226 = VECTOR ( 'NONE', #136167, 999.9999999999998863 ) ;
#67225 = LINE ( 'NONE', #222417, #30614 ) ;
#67227 = EDGE_LOOP ( 'NONE', ( #225168, #38059, #88864, #112582 ) ) ;
#67228 = CARTESIAN_POINT ( 'NONE',  ( -23.15000000000000213, 1.999999999999998224, -20.27537807723789953 ) ) ;
#67229 = ORIENTED_EDGE ( 'NONE', *, *, #116568, .F. ) ;
#67230 = DIRECTION ( 'NONE',  ( 0.000000000000000000, -0.9126074666063769270, -0.4088369013363280513 ) ) ;
#67231 = ADVANCED_FACE ( 'NONE', ( #177658 ), #133369, .F. ) ;
#67232 = CARTESIAN_POINT ( 'NONE',  ( -16.77683809663752257, 52.34166666667894674, -153.2731074845245303 ) ) ;
#67233 = ADVANCED_FACE ( 'NONE', ( #38130 ), #194652, .F. ) ;
#67234 = EDGE_CURVE ( 'NONE', #92906, #257555, #203381, .T. ) ;
#67235 = EDGE_LOOP ( 'NONE', ( #244541, #72219, #6862, #8807 ) ) ;
#67236 = DIRECTION ( 'NONE',  ( 0.000000000000000000, -0.1350103645451876666, -0.9908441862701600211 ) ) ;
#67237 = CIRCLE ( 'NONE', #117321, 11.75000000000001066 ) ;
#67239 = VERTEX_POINT ( 'NONE', #137207 ) ;
#67238 = CIRCLE ( 'NONE', #250582, 0.1000000000000055844 ) ;
#67240 = EDGE_LOOP ( 'NONE', ( #4239, #2660, #95860, #191995 ) ) ;
#67241 = ORIENTED_EDGE ( 'NONE', *, *, #164623, .T. ) ;
#67242 = CIRCLE ( 'NONE', #58849, 0.09999999999998898659 ) ;
#67243 = DIRECTION ( 'NONE',  ( -1.000000000000000000, 2.952720810173289112E-16, 2.061873921506763405E-30 ) ) ;
#67244 = DIRECTION ( 'NONE',  ( 1.000000000000000000, 3.265361837132813093E-16, -0.000000000000000000 ) ) ;
#67245 = CARTESIAN_POINT ( 'NONE',  ( 21.05000000000000071, 76.00000000001165290, -69.42310748452432279 ) ) ;
#67246 = DIRECTION ( 'NONE',  ( 0.000000000000000000, 0.000000000000000000, 1.000000000000000000 ) ) ;
#67247 = DIRECTION ( 'NONE',  ( 1.000000000000000000, 0.000000000000000000, 0.000000000000000000 ) ) ;
#67248 = CARTESIAN_POINT ( 'NONE',  ( 20.85000000000000142, 78.48087866980282001, -232.8271061603568910 ) ) ;
#67249 = EDGE_CURVE ( 'NONE', #215584, #17744, #227742, .T. ) ;
#67251 = CARTESIAN_POINT ( 'NONE',  ( -20.94999999999999929, 11.59999999999999964, -26.57179676972449656 ) ) ;
#67250 = CARTESIAN_POINT ( 'NONE',  ( 20.84999999999999787, 11.75000000001116085, -194.0808527540412172 ) ) ;
#67252 = CARTESIAN_POINT ( 'NONE',  ( -16.87683809663752399, 9.850000000011144508, -80.40236401819635148 ) ) ;
#67254 = EDGE_LOOP ( 'NONE', ( #58065, #210217, #30303, #139190 ) ) ;
#67253 = CARTESIAN_POINT ( 'NONE',  ( -18.40000000000000213, 64.58541674041249792, -157.3731074845244677 ) ) ;
#67256 = DIRECTION ( 'NONE',  ( 0.000000000000000000, 0.8814952561688430555, -0.4721928772777346239 ) ) ;
#67255 = CARTESIAN_POINT ( 'NONE',  ( -20.64999999999999858, 71.65000000001180069, -81.87310748452433984 ) ) ;
#67257 = FACE_OUTER_BOUND ( 'NONE', #183977, .T. ) ;
#67258 = ORIENTED_EDGE ( 'NONE', *, *, #27712, .F. ) ;
#67259 = CARTESIAN_POINT ( 'NONE',  ( 20.95496329884391784, 10.56743320610419445, -74.57430993228486216 ) ) ;
#67260 = CARTESIAN_POINT ( 'NONE',  ( 20.90000000000000213, 1.212568896937007645, -7.800000000000000711 ) ) ;
#67261 = CARTESIAN_POINT ( 'NONE',  ( 20.85000000000000142, -1.835859311432481045, -145.5044391687985694 ) ) ;
#67262 = ORIENTED_EDGE ( 'NONE', *, *, #217683, .T. ) ;
#67263 = VECTOR ( 'NONE', #203308, 1000.000000000000000 ) ;
#67264 = CARTESIAN_POINT ( 'NONE',  ( -16.94052228080552069, 30.25905040575426952, -234.7941296169553311 ) ) ;
#67265 = CARTESIAN_POINT ( 'NONE',  ( -20.85000000000000142, 1.115600667400684642E-11, -200.9999999999999432 ) ) ;
#67266 = DIRECTION ( 'NONE',  ( 1.000000000000000000, 0.000000000000000000, 0.000000000000000000 ) ) ;
#67267 = ORIENTED_EDGE ( 'NONE', *, *, #227709, .T. ) ;
#67268 = EDGE_LOOP ( 'NONE', ( #248085, #56773, #137537, #117115, #214952, #89605 ) ) ;
#67269 = CARTESIAN_POINT ( 'NONE',  ( -18.40000000000000213, 64.52683809664939929, -90.41452884076171870 ) ) ;
#67271 = ORIENTED_EDGE ( 'NONE', *, *, #99450, .T. ) ;
#67270 = EDGE_CURVE ( 'NONE', #185478, #158940, #102828, .T. ) ;
#67272 = DIRECTION ( 'NONE',  ( 2.259780016855445309E-14, -0.9875055080513764905, 0.1575844902526679359 ) ) ;
#67273 = ADVANCED_FACE ( 'NONE', ( #134619 ), #82532, .T. ) ;
#67274 = CARTESIAN_POINT ( 'NONE',  ( 13.99999999999999822, 66.15000000001228386, -153.2731074845244450 ) ) ;
#67275 = CARTESIAN_POINT ( 'NONE',  ( 18.42636655943171320, 85.49694431578232923, -62.91402691336873687 ) ) ;
#67276 = DIRECTION ( 'NONE',  ( 2.952720810173289605E-16, 1.000000000000000000, 7.086529944415894657E-15 ) ) ;
#67277 = EDGE_LOOP ( 'NONE', ( #167742, #114457, #107914, #109669 ) ) ;
#67278 = CARTESIAN_POINT ( 'NONE',  ( -14.87770893841226894, 9.430637101707898040, -118.7682606180610065 ) ) ;
#67279 = VECTOR ( 'NONE', #173604, 1000.000000000000000 ) ;
#67281 = DIRECTION ( 'NONE',  ( 0.000000000000000000, 6.769652589177795712E-15, -1.000000000000000000 ) ) ;
#67280 = AXIS2_PLACEMENT_3D ( 'NONE', #149437, #111576, #34623 ) ;
#67282 = EDGE_CURVE ( 'NONE', #102805, #46904, #219942, .T. ) ;
#67283 = AXIS2_PLACEMENT_3D ( 'NONE', #146816, #71170, #192383 ) ;
#67284 = CARTESIAN_POINT ( 'NONE',  ( -16.92507428761698662, 63.06913787792631609, -213.1888086875385966 ) ) ;
#67285 = CARTESIAN_POINT ( 'NONE',  ( -23.25000000000000000, 71.85000000001151932, -48.27310748452434552 ) ) ;
#67286 = ORIENTED_EDGE ( 'NONE', *, *, #90882, .F. ) ;
#67287 = CARTESIAN_POINT ( 'NONE',  ( 20.92356734117541706, 10.31973158070286622, -39.05053347133544150 ) ) ;
#67289 = ORIENTED_EDGE ( 'NONE', *, *, #202759, .T. ) ;
#67288 = CYLINDRICAL_SURFACE ( 'NONE', #33691, 0.1000000000000028644 ) ;
#67290 = DIRECTION ( 'NONE',  ( 1.000000000000000000, -0.000000000000000000, 0.000000000000000000 ) ) ;
#67291 = CARTESIAN_POINT ( 'NONE',  ( 23.14999999999999858, 71.00000000001253397, -182.4283735034374843 ) ) ;
#67292 = DIRECTION ( 'NONE',  ( 1.000000000000000000, 0.000000000000000000, 0.000000000000000000 ) ) ;
#67293 = DIRECTION ( 'NONE',  ( 0.000000000000000000, -0.9908441862701596881, 0.1350103645451904977 ) ) ;
#67294 = CARTESIAN_POINT ( 'NONE',  ( 21.06086055315977390, 8.774707514956258336, -12.20232215515397023 ) ) ;
#67295 = LINE ( 'NONE', #226346, #21761 ) ;
#67296 = DIRECTION ( 'NONE',  ( 1.000000000000000000, 0.000000000000000000, 0.000000000000000000 ) ) ;
#67297 = CIRCLE ( 'NONE', #29740, 4.150000000000001243 ) ;
#67298 = EDGE_LOOP ( 'NONE', ( #107831, #98259, #150703, #49637 ) ) ;
#67299 = ADVANCED_FACE ( 'NONE', ( #254558 ), #255826, .T. ) ;
#67300 = CARTESIAN_POINT ( 'NONE',  ( -20.85000000000000142, 11.74999999999999645, -26.71613433702190576 ) ) ;
#67301 = DIRECTION ( 'NONE',  ( -1.000000000000000000, 0.000000000000000000, 0.000000000000000000 ) ) ;
#67302 = CARTESIAN_POINT ( 'NONE',  ( -18.59999999999999787, 52.21971469324220294, -232.5539039185337913 ) ) ;
#67303 = LINE ( 'NONE', #226353, #150674 ) ;
#67304 = DIRECTION ( 'NONE',  ( -1.000000000000000000, 0.000000000000000000, 0.000000000000000000 ) ) ;
#67305 = VERTEX_POINT ( 'NONE', #56370 ) ;
#67306 = ORIENTED_EDGE ( 'NONE', *, *, #62339, .F. ) ;
#67307 = FACE_OUTER_BOUND ( 'NONE', #87037, .T. ) ;
#67308 = EDGE_CURVE ( 'NONE', #92740, #88402, #235947, .T. ) ;
#67309 = DIRECTION ( 'NONE',  ( 1.000000000000000000, 0.000000000000000000, 0.000000000000000000 ) ) ;
#67311 = EDGE_CURVE ( 'NONE', #98899, #164655, #90936, .T. ) ;
#67310 = CARTESIAN_POINT ( 'NONE',  ( 23.14999999999999858, 56.06656052939784729, -228.0911609752645290 ) ) ;
#67312 = AXIS2_PLACEMENT_3D ( 'NONE', #224963, #148024, #163739 ) ;
#67313 = CARTESIAN_POINT ( 'NONE',  ( 18.39999999999999858, -0.6821283177418837607, -242.5105927437468836 ) ) ;
#67314 = ADVANCED_FACE ( 'NONE', ( #118949 ), #77224, .T. ) ;
#67315 = EDGE_CURVE ( 'NONE', #162858, #105040, #240795, .T. ) ;
#67316 = DIRECTION ( 'NONE',  ( 0.000000000000000000, -0.2617529984165031243, -0.9651348961777157509 ) ) ;
#67317 = AXIS2_PLACEMENT_3D ( 'NONE', #229551, #31381, #110877 ) ;
#67318 = LINE ( 'NONE', #85556, #159093 ) ;
#67319 = DIRECTION ( 'NONE',  ( -0.000000000000000000, -1.000000000000000000, 6.308085367188393199E-16 ) ) ;
#67320 = AXIS2_PLACEMENT_3D ( 'NONE', #146621, #127083, #25428 ) ;
#67321 = EDGE_CURVE ( 'NONE', #84452, #248210, #198466, .T. ) ;
#67323 = EDGE_CURVE ( 'NONE', #218845, #243814, #81068, .T. ) ;
#67322 = AXIS2_PLACEMENT_3D ( 'NONE', #167067, #69237, #227000 ) ;
#67324 = ORIENTED_EDGE ( 'NONE', *, *, #184264, .F. ) ;
#67325 = CARTESIAN_POINT ( 'NONE',  ( -20.94999999999999929, 74.83729825007462466, -195.5231074845243597 ) ) ;
#67326 = AXIS2_PLACEMENT_3D ( 'NONE', #55708, #173187, #117014 ) ;
#67327 = ORIENTED_EDGE ( 'NONE', *, *, #49349, .F. ) ;
#67328 = DIRECTION ( 'NONE',  ( 0.000000000000000000, -0.9770955615653316162, -0.2128009952263604232 ) ) ;
#67329 = CARTESIAN_POINT ( 'NONE',  ( 21.15000000000005542, 74.16448838626247664, -47.52760213295649550 ) ) ;
#67331 = ADVANCED_FACE ( 'NONE', ( #242717 ), #43251, .F. ) ;
#67330 = CARTESIAN_POINT ( 'NONE',  ( 21.05095171578076574, 8.776179878782192745, -79.16587327663792450 ) ) ;
#67332 = CYLINDRICAL_SURFACE ( 'NONE', #119614, 0.09999999999998002154 ) ;
#67333 = DIRECTION ( 'NONE',  ( -0.000000000000000000, -6.982962677686266711E-15, 1.000000000000000000 ) ) ;
#67334 = B_SPLINE_CURVE_WITH_KNOTS ( 'NONE', 3,
 ( #19914, #21214, #182851, #103260, #238957, #121600, #179012, #237665 ),
 .UNSPECIFIED., .F., .F.,
 ( 4, 2, 2, 4 ),
 ( 0.000000000000000000, 0.0002114466876442075882, 0.0003171700314663105421, 0.0004228933752884134960 ),
 .UNSPECIFIED. ) ;
#67335 = CARTESIAN_POINT ( 'NONE',  ( 18.55857864376268296, 65.63284271248713253, -178.7731074845244450 ) ) ;
#67336 = CARTESIAN_POINT ( 'NONE',  ( -17.04295772865454239, 65.97510057475034273, -82.17310748452439384 ) ) ;
#67337 = ORIENTED_EDGE ( 'NONE', *, *, #20835, .T. ) ;
#67338 = CARTESIAN_POINT ( 'NONE',  ( -16.93658211146646408, 22.95103440912690118, -230.8705440892085505 ) ) ;
#67339 = AXIS2_PLACEMENT_3D ( 'NONE', #17532, #97039, #155806 ) ;
#67340 = EDGE_CURVE ( 'NONE', #190222, #100804, #181964, .T. ) ;
#67341 = CARTESIAN_POINT ( 'NONE',  ( -33.72168855820452649, 64.52683809664983983, -160.7731074845244450 ) ) ;
#67342 = FACE_OUTER_BOUND ( 'NONE', #78276, .T. ) ;
#67343 = DIRECTION ( 'NONE',  ( 1.000000000000000000, 0.000000000000000000, 0.000000000000000000 ) ) ;
#67344 = CIRCLE ( 'NONE', #158959, 0.1000000000000089567 ) ;
#67345 = ADVANCED_FACE ( 'NONE', ( #40720 ), #21146, .F. ) ;
#67347 = ADVANCED_FACE ( 'NONE', ( #2819 ), #184035, .F. ) ;
#67346 = AXIS2_PLACEMENT_3D ( 'NONE', #166553, #123546, #165236 ) ;
#67348 = CARTESIAN_POINT ( 'NONE',  ( 12.25000000000000000, 9.850000000011137402, -50.24999999999999289 ) ) ;
#67349 = CARTESIAN_POINT ( 'NONE',  ( 21.05000000000000071, 8.776282895303630482, -176.0586289951409071 ) ) ;
#67350 = EDGE_LOOP ( 'NONE', ( #41695, #108699, #17114, #228481, #238696, #172425, #73908, #240533, #58109, #225674, #81774, #41824, #49396, #239966, #118504, #129645, #174359, #19523, #119017, #37039, #139352, #69878, #246895, #51022, #154642 ) ) ;
#67351 = AXIS2_PLACEMENT_3D ( 'NONE', #86838, #242073, #26919 ) ;
#67352 = LINE ( 'NONE', #148166, #60501 ) ;
#67354 = ADVANCED_FACE ( 'NONE', ( #100613 ), #219309, .T. ) ;
#67353 = CARTESIAN_POINT ( 'NONE',  ( -18.40000000000000213, 11.41458325961095177, -154.8500000000000512 ) ) ;
#67355 = VECTOR ( 'NONE', #255295, 1000.000000000000000 ) ;
#67356 = VERTEX_POINT ( 'NONE', #122802 ) ;
#67357 = DIRECTION ( 'NONE',  ( 1.000000000000000000, -0.000000000000000000, 0.000000000000000000 ) ) ;
#67358 = CARTESIAN_POINT ( 'NONE',  ( -21.55000000000000426, 7.750000000011159074, -88.25000000000005684 ) ) ;
#67359 = EDGE_CURVE ( 'NONE', #222817, #64290, #201037, .T. ) ;
#67360 = EDGE_CURVE ( 'NONE', #230693, #117118, #84900, .T. ) ;
#67361 = DIRECTION ( 'NONE',  ( -1.000000000000000000, -0.000000000000000000, -0.000000000000000000 ) ) ;
#67362 = ORIENTED_EDGE ( 'NONE', *, *, #144235, .T. ) ;
#67363 = FACE_OUTER_BOUND ( 'NONE', #40049, .T. ) ;
#67364 = FACE_OUTER_BOUND ( 'NONE', #61863, .T. ) ;
#67365 = EDGE_CURVE ( 'NONE', #22691, #11008, #244874, .T. ) ;
#67366 = AXIS2_PLACEMENT_3D ( 'NONE', #3206, #243116, #237971 ) ;
#67367 = ORIENTED_EDGE ( 'NONE', *, *, #74544, .T. ) ;
#67368 = AXIS2_PLACEMENT_3D ( 'NONE', #133062, #107052, #109623 ) ;
#67369 = AXIS2_PLACEMENT_3D ( 'NONE', #28249, #149469, #227688 ) ;
#67370 = AXIS2_PLACEMENT_3D ( 'NONE', #129151, #245250, #226960 ) ;
#67371 = VERTEX_POINT ( 'NONE', #163206 ) ;
#67372 = ADVANCED_FACE ( 'NONE', ( #103198 ), #164493, .T. ) ;
#67373 = LINE ( 'NONE', #29560, #120927 ) ;
#67374 = CARTESIAN_POINT ( 'NONE',  ( 21.05000000000000426, 0.09843750000031840919, 6.299230910092287417 ) ) ;
#67375 = DIRECTION ( 'NONE',  ( 0.000000000000000000, 0.000000000000000000, -1.000000000000000000 ) ) ;
#67376 = DIRECTION ( 'NONE',  ( 1.000000000000000000, 0.000000000000000000, 0.000000000000000000 ) ) ;
#67377 = CARTESIAN_POINT ( 'NONE',  ( 22.88900146558018989, 8.703904791123973084, -188.3499999999999659 ) ) ;
#67378 = DIRECTION ( 'NONE',  ( 0.000000000000000000, 0.000000000000000000, -1.000000000000000000 ) ) ;
#67379 = CARTESIAN_POINT ( 'NONE',  ( 21.14999999999999503, 64.27847795353595473, -247.1247091181747066 ) ) ;
#67380 = DIRECTION ( 'NONE',  ( 0.000000000000000000, -0.8454177738465953329, -0.5341055959866617409 ) ) ;
#67381 = DIRECTION ( 'NONE',  ( 0.000000000000000000, 0.000000000000000000, 1.000000000000000000 ) ) ;
#67383 = VERTEX_POINT ( 'NONE', #181492 ) ;
#67382 = CARTESIAN_POINT ( 'NONE',  ( -21.55000000000000071, 68.65000000001180069, -81.87310748452436826 ) ) ;
#67384 = ORIENTED_EDGE ( 'NONE', *, *, #132859, .T. ) ;
#67386 = CARTESIAN_POINT ( 'NONE',  ( -15.51798037960204368, 9.376659938544690931, -84.62819254821734205 ) ) ;
#67385 = LINE ( 'NONE', #162645, #191317 ) ;
#67388 = ORIENTED_EDGE ( 'NONE', *, *, #194739, .F. ) ;
#67387 = CARTESIAN_POINT ( 'NONE',  ( -23.15000000000000213, 1.115600667400684642E-11, -70.90000000000000568 ) ) ;
#67389 = ORIENTED_EDGE ( 'NONE', *, *, #153643, .T. ) ;
#67390 = CARTESIAN_POINT ( 'NONE',  ( 22.50000000000000000, 76.00000000001213607, -136.5231074845242745 ) ) ;
#67391 = TOROIDAL_SURFACE ( 'NONE', #13244, 0.4000000000000012990, 0.1000000000000000056 ) ;
#67392 = DIRECTION ( 'NONE',  ( 0.000000000000000000, 0.000000000000000000, -1.000000000000000000 ) ) ;
#67393 = CYLINDRICAL_SURFACE ( 'NONE', #175704, 4.000000000000003553 ) ;
#67394 = CARTESIAN_POINT ( 'NONE',  ( -20.92356734117541706, 10.31973158071402175, -173.0505334713354841 ) ) ;
#67395 = CARTESIAN_POINT ( 'NONE',  ( -18.50000000000000000, 64.35000000001187459, -90.87310748452438247 ) ) ;
#67396 = DIRECTION ( 'NONE',  ( 0.000000000000000000, 6.982962677686267499E-15, -1.000000000000000000 ) ) ;
#67397 = CARTESIAN_POINT ( 'NONE',  ( 18.59999999999999432, 14.81796439977981272, -236.5325475414793743 ) ) ;
#67399 = ORIENTED_EDGE ( 'NONE', *, *, #51077, .T. ) ;
#67398 = EDGE_CURVE ( 'NONE', #108495, #18666, #165800, .T. ) ;
#67400 = VERTEX_POINT ( 'NONE', #4113 ) ;
#67401 = FACE_BOUND ( 'NONE', #218272, .T. ) ;
#67402 = EDGE_CURVE ( 'NONE', #140123, #73589, #232046, .T. ) ;
#67403 = ORIENTED_EDGE ( 'NONE', *, *, #30668, .T. ) ;
#67404 = DIRECTION ( 'NONE',  ( 1.000000000000000000, 0.000000000000000000, 0.000000000000000000 ) ) ;
#67405 = ORIENTED_EDGE ( 'NONE', *, *, #134694, .F. ) ;
#67406 = VECTOR ( 'NONE', #155219, 1000.000000000000114 ) ;
#67407 = FACE_OUTER_BOUND ( 'NONE', #214360, .T. ) ;
#67408 = EDGE_CURVE ( 'NONE', #80343, #88161, #124083, .T. ) ;
#67410 = ADVANCED_FACE ( 'NONE', ( #10266 ), #11555, .F. ) ;
#67409 = DIRECTION ( 'NONE',  ( -0.000000000000000000, 1.000000000000000000, 6.352154140967427193E-15 ) ) ;
#67411 = CARTESIAN_POINT ( 'NONE',  ( -21.07933241753356413, 75.90662040959345802, -209.8517534329041041 ) ) ;
#67412 = ORIENTED_EDGE ( 'NONE', *, *, #90569, .F. ) ;
#67413 = CARTESIAN_POINT ( 'NONE',  ( -18.50000000000000000, 66.85000000001254250, -182.3731074845244393 ) ) ;
#67414 = EDGE_LOOP ( 'NONE', ( #54956, #14991, #2841, #106305 ) ) ;
#67415 = DIRECTION ( 'NONE',  ( -1.000000000000000000, -0.000000000000000000, -0.000000000000000000 ) ) ;
#67416 = CARTESIAN_POINT ( 'NONE',  ( -22.39999999999999858, 33.47376623175146904, -242.4412390690852703 ) ) ;
#67417 = CARTESIAN_POINT ( 'NONE',  ( -20.85000000000000142, 77.16412189325286874, -61.80825939895269272 ) ) ;
#67418 = LINE ( 'NONE', #86955, #24155 ) ;
#67419 = ORIENTED_EDGE ( 'NONE', *, *, #20306, .F. ) ;
#67421 = DIRECTION ( 'NONE',  ( 1.000000000000000000, 0.000000000000000000, 0.000000000000000000 ) ) ;
#67420 = CIRCLE ( 'NONE', #146519, 0.09999999999999958922 ) ;
#67422 = ORIENTED_EDGE ( 'NONE', *, *, #210836, .T. ) ;
#67425 = ORIENTED_EDGE ( 'NONE', *, *, #230864, .F. ) ;
#67424 = CARTESIAN_POINT ( 'NONE',  ( 18.79999999999999716, -11.65000000000000036, 0.000000000000000000 ) ) ;
#67423 = CARTESIAN_POINT ( 'NONE',  ( 18.52165635395213883, 46.94608792946566211, -255.3317188026131248 ) ) ;
#67426 = AXIS2_PLACEMENT_3D ( 'NONE', #51819, #165383, #244906 ) ;
#67427 = FACE_OUTER_BOUND ( 'NONE', #126772, .T. ) ;
#67428 = VERTEX_POINT ( 'NONE', #248871 ) ;
#67429 = AXIS2_PLACEMENT_3D ( 'NONE', #248240, #134689, #188261 ) ;
#67430 = DIRECTION ( 'NONE',  ( 1.000000000000000000, -0.000000000000000000, -0.000000000000000000 ) ) ;
#67431 = ORIENTED_EDGE ( 'NONE', *, *, #130394, .T. ) ;
#67432 = CYLINDRICAL_SURFACE ( 'NONE', #65732, 0.09999999999998898659 ) ;
#67433 = CARTESIAN_POINT ( 'NONE',  ( -37.88850191057539973, -14.35849056603774976, -0.4952830188679671064 ) ) ;
#67434 = DIRECTION ( 'NONE',  ( 0.000000000000000000, 0.000000000000000000, -1.000000000000000000 ) ) ;
#67435 = CIRCLE ( 'NONE', #246511, 0.09999999999999939493 ) ;
#67436 = ORIENTED_EDGE ( 'NONE', *, *, #77598, .F. ) ;
#67437 = DIRECTION ( 'NONE',  ( 0.000000000000000000, -0.8814952561688388366, 0.4721928772777422845 ) ) ;
#67438 = CARTESIAN_POINT ( 'NONE',  ( -16.81931177881022776, 14.12995618366871753, -219.1828163376052032 ) ) ;
#67439 = CARTESIAN_POINT ( 'NONE',  ( -22.50000000000000000, 1.619487989037824871, -230.7814958294534335 ) ) ;
#67440 = ORIENTED_EDGE ( 'NONE', *, *, #238713, .F. ) ;
#67441 = ADVANCED_FACE ( 'NONE', ( #211027 ), #159152, .T. ) ;
#67442 = SPHERICAL_SURFACE ( 'NONE', #96985, 0.1000000000000000056 ) ;
#67443 = ORIENTED_EDGE ( 'NONE', *, *, #166425, .T. ) ;
#67444 = CARTESIAN_POINT ( 'NONE',  ( 20.95512820512820440, 12.01161663143393632, -206.2285874551107554 ) ) ;
#67445 = LINE ( 'NONE', #146970, #9595 ) ;
#67446 = CARTESIAN_POINT ( 'NONE',  ( -22.50000000000096989, 75.89914163091383159, -181.7726746080137445 ) ) ;
#67448 = ORIENTED_EDGE ( 'NONE', *, *, #78800, .F. ) ;
#67447 = CARTESIAN_POINT ( 'NONE',  ( -23.25000000000000000, 1.148907358139439339E-11, -201.0000000000015064 ) ) ;
#67449 = CARTESIAN_POINT ( 'NONE',  ( -21.05000000000000071, 1.115600667400684642E-11, -33.50000000000000000 ) ) ;
#67450 = EDGE_CURVE ( 'NONE', #22457, #189336, #82157, .T. ) ;
#67451 = DIRECTION ( 'NONE',  ( 0.000000000000000000, 0.000000000000000000, -1.000000000000000000 ) ) ;
#67452 = AXIS2_PLACEMENT_3D ( 'NONE', #196949, #174888, #159148 ) ;
#67453 = AXIS2_PLACEMENT_3D ( 'NONE', #583, #59249, #219642 ) ;
#67454 = LINE ( 'NONE', #64884, #152089 ) ;
#67455 = ADVANCED_FACE ( 'NONE', ( #209743 ), #50641, .F. ) ;
#67456 = ORIENTED_EDGE ( 'NONE', *, *, #189941, .F. ) ;
#67457 = VECTOR ( 'NONE', #114116, 1000.000000000000227 ) ;
#67458 = CARTESIAN_POINT ( 'NONE',  ( 21.53752568617687402, 69.21319212550885425, -203.6220819458088158 ) ) ;
#67459 = DIRECTION ( 'NONE',  ( 0.000000000000000000, 0.000000000000000000, -1.000000000000000000 ) ) ;
#67460 = ORIENTED_EDGE ( 'NONE', *, *, #252819, .T. ) ;
#67461 = CARTESIAN_POINT ( 'NONE',  ( -23.25000000000000000, 2.571758278209444422E-16, -31.39999999999999858 ) ) ;
#67462 = ORIENTED_EDGE ( 'NONE', *, *, #194246, .F. ) ;
#67463 = ADVANCED_FACE ( 'NONE', ( #130185 ), #76084, .T. ) ;
#67464 = DIRECTION ( 'NONE',  ( 0.7071067811865214825, -0.7071067811865735520, 0.000000000000000000 ) ) ;
#67466 = ORIENTED_EDGE ( 'NONE', *, *, #157343, .F. ) ;
#67465 = CARTESIAN_POINT ( 'NONE',  ( -20.15000000000000568, 66.70857864377425983, -57.27310748452438816 ) ) ;
#67467 = EDGE_CURVE ( 'NONE', #59699, #50249, #39794, .T. ) ;
#67468 = ADVANCED_FACE ( 'NONE', ( #4473 ), #141422, .T. ) ;
#67469 = CIRCLE ( 'NONE', #811, 3.899999999999999467 ) ;
#67472 = ORIENTED_EDGE ( 'NONE', *, *, #87882, .T. ) ;
#67471 = ORIENTED_EDGE ( 'NONE', *, *, #169441, .T. ) ;
#67470 = DIRECTION ( 'NONE',  ( 0.000000000000000000, 0.000000000000000000, -1.000000000000000000 ) ) ;
#67473 = DIRECTION ( 'NONE',  ( 0.000000000000000000, 0.2617529984165035684, 0.9651348961777156399 ) ) ;
#67474 = DIRECTION ( 'NONE',  ( -1.000000000000000000, 0.000000000000000000, -0.000000000000000000 ) ) ;
#67475 = CARTESIAN_POINT ( 'NONE',  ( -23.15000000000000213, -11.64999999998884483, -130.9000000000000341 ) ) ;
#67476 = EDGE_CURVE ( 'NONE', #174560, #109031, #257459, .T. ) ;
#67478 = CARTESIAN_POINT ( 'NONE',  ( -16.90202395485793829, 9.965944544550675133, -20.90301372125983193 ) ) ;
#67477 = DIRECTION ( 'NONE',  ( 1.000000000000000000, 0.000000000000000000, 0.000000000000000000 ) ) ;
#67479 = DIRECTION ( 'NONE',  ( 1.000000000000000000, 0.000000000000000000, 0.000000000000000000 ) ) ;
#67480 = CYLINDRICAL_SURFACE ( 'NONE', #65024, 0.09999999999999939493 ) ;
#67481 = DIRECTION ( 'NONE',  ( 1.000000000000000000, 0.000000000000000000, 0.000000000000000000 ) ) ;
#67482 = CARTESIAN_POINT ( 'NONE',  ( -22.50000000000000000, 11.64976291804307884, -33.41119002361307366 ) ) ;
#67483 = VERTEX_POINT ( 'NONE', #201394 ) ;
#67484 = ORIENTED_EDGE ( 'NONE', *, *, #212828, .F. ) ;
#67485 = CARTESIAN_POINT ( 'NONE',  ( 21.05000000000000071, 76.00000000001195133, -103.0231074845243171 ) ) ;
#67487 = EDGE_LOOP ( 'NONE', ( #168816, #256565, #97287, #248470, #12525, #106314 ) ) ;
#67486 = LINE ( 'NONE', #244836, #241019 ) ;
#67488 = ORIENTED_EDGE ( 'NONE', *, *, #221581, .F. ) ;
#67489 = EDGE_CURVE ( 'NONE', #99499, #147639, #42332, .T. ) ;
#67491 = CARTESIAN_POINT ( 'NONE',  ( 18.39999999999999503, 5.650000000011139001, -180.1499999999999773 ) ) ;
#67490 = TOROIDAL_SURFACE ( 'NONE', #204855, 0.2000000000000000111, 0.1000000000000000056 ) ;
#67492 = ORIENTED_EDGE ( 'NONE', *, *, #150270, .T. ) ;
#67493 = CARTESIAN_POINT ( 'NONE',  ( -21.05000000000000071, 69.74218538953063273, -136.6208977758335550 ) ) ;
#67494 = CIRCLE ( 'NONE', #134129, 0.09999999999998898659 ) ;
#67495 = ORIENTED_EDGE ( 'NONE', *, *, #96991, .T. ) ;
#67496 = AXIS2_PLACEMENT_3D ( 'NONE', #140880, #220423, #53324 ) ;
#67497 = VECTOR ( 'NONE', #78363, 1000.000000000000114 ) ;
#67498 = CARTESIAN_POINT ( 'NONE',  ( 20.94999999999999929, 71.00000000001253397, -181.9283735034374843 ) ) ;
#67499 = AXIS2_PLACEMENT_3D ( 'NONE', #52401, #208926, #229772 ) ;
#67501 = ORIENTED_EDGE ( 'NONE', *, *, #169333, .T. ) ;
#67500 = VERTEX_POINT ( 'NONE', #218373 ) ;
#67502 = ORIENTED_EDGE ( 'NONE', *, *, #175832, .T. ) ;
#67504 = CARTESIAN_POINT ( 'NONE',  ( -23.25000000000000000, 70.05000000001176375, -79.82880978955917328 ) ) ;
#67503 = AXIS2_PLACEMENT_3D ( 'NONE', #115737, #51886, #74077 ) ;
#67505 = ORIENTED_EDGE ( 'NONE', *, *, #156473, .T. ) ;
#67506 = ORIENTED_EDGE ( 'NONE', *, *, #121542, .T. ) ;
#67507 = CYLINDRICAL_SURFACE ( 'NONE', #242845, 0.09999999999999939493 ) ;
#67508 = CARTESIAN_POINT ( 'NONE',  ( -17.11825945287482753, 23.06621698515930063, -230.9822826988504119 ) ) ;
#67510 = ORIENTED_EDGE ( 'NONE', *, *, #124153, .F. ) ;
#67509 = LINE ( 'NONE', #28433, #6073 ) ;
#67511 = DIRECTION ( 'NONE',  ( -1.000000000000000000, -0.000000000000000000, -0.000000000000000000 ) ) ;
#67512 = DIRECTION ( 'NONE',  ( 0.000000000000000000, 0.1335171055202867274, -0.9910465087640865089 ) ) ;
#67514 = EDGE_LOOP ( 'NONE', ( #162475, #121910, #178810, #158543, #257012 ) ) ;
#67513 = CARTESIAN_POINT ( 'NONE',  ( 21.14999999999999858, 14.06640494040442135, -210.3712993791105532 ) ) ;
#67515 = LINE ( 'NONE', #47945, #71943 ) ;
#67516 = VERTEX_POINT ( 'NONE', #119303 ) ;
#67517 = DIRECTION ( 'NONE',  ( 0.000000000000000000, 0.000000000000000000, 1.000000000000000000 ) ) ;
#67518 = VECTOR ( 'NONE', #81949, 1000.000000000000000 ) ;
#67519 = ORIENTED_EDGE ( 'NONE', *, *, #237452, .F. ) ;
#67520 = TOROIDAL_SURFACE ( 'NONE', #13551, 11.65000000000000036, 0.1000000000000000056 ) ;
#67521 = DIRECTION ( 'NONE',  ( 0.000000000000000000, 0.9126074666063767049, 0.4088369013363286619 ) ) ;
#67522 = CARTESIAN_POINT ( 'NONE',  ( 21.05000000000000071, 11.60058429089262333, -246.3380203656811887 ) ) ;
#67524 = EDGE_LOOP ( 'NONE', ( #125805, #250483, #37983, #131130 ) ) ;
#67523 = CIRCLE ( 'NONE', #246416, 0.1000000000000024342 ) ;
#67526 = DIRECTION ( 'NONE',  ( -1.000000000000000000, 1.614276770400120371E-15, 3.515722686956159758E-16 ) ) ;
#67525 = LINE ( 'NONE', #241048, #223711 ) ;
#67527 = AXIS2_PLACEMENT_3D ( 'NONE', #111243, #72132, #151687 ) ;
#67528 = EDGE_CURVE ( 'NONE', #160733, #29906, #177875, .T. ) ;
#67529 = FACE_OUTER_BOUND ( 'NONE', #174362, .T. ) ;
#67530 = CARTESIAN_POINT ( 'NONE',  ( -12.60206096961793065, 12.50981721680830105, -214.3157313002988644 ) ) ;
#67531 = ORIENTED_EDGE ( 'NONE', *, *, #43659, .T. ) ;
#67532 = EDGE_LOOP ( 'NONE', ( #73636, #17084, #21288, #93338 ) ) ;
#67533 = AXIS2_PLACEMENT_3D ( 'NONE', #11183, #248504, #189821 ) ;
#67534 = FACE_OUTER_BOUND ( 'NONE', #187959, .T. ) ;
#67535 = CARTESIAN_POINT ( 'NONE',  ( -18.50000000000000000, 66.85000000001203091, -114.7731074845243739 ) ) ;
#67536 = EDGE_LOOP ( 'NONE', ( #44610, #74553, #192252 ) ) ;
#67537 = DIRECTION ( 'NONE',  ( -1.000000000000000000, 0.000000000000000000, 0.000000000000000000 ) ) ;
#67538 = VERTEX_POINT ( 'NONE', #240532 ) ;
#67539 = CARTESIAN_POINT ( 'NONE',  ( -22.59999999999999787, 11.74956712350054744, -66.89914163090134025 ) ) ;
#67541 = ADVANCED_FACE ( 'NONE', ( #82700 ), #41071, .F. ) ;
#67540 = AXIS2_PLACEMENT_3D ( 'NONE', #246066, #205628, #86949 ) ;
#67542 = ORIENTED_EDGE ( 'NONE', *, *, #188144, .F. ) ;
#67543 = DIRECTION ( 'NONE',  ( 1.073024830501117725E-15, -6.982962677686266711E-15, 1.000000000000000000 ) ) ;
#67544 = LINE ( 'NONE', #29741, #140770 ) ;
#67545 = FACE_OUTER_BOUND ( 'NONE', #59912, .T. ) ;
#67546 = EDGE_CURVE ( 'NONE', #25623, #96530, #143982, .T. ) ;
#67547 = EDGE_CURVE ( 'NONE', #106852, #27978, #247928, .T. ) ;
#67548 = EDGE_LOOP ( 'NONE', ( #217358, #75193, #230978, #78663 ) ) ;
#67549 = DIRECTION ( 'NONE',  ( 1.000000000000000000, 0.000000000000000000, 0.000000000000000000 ) ) ;
#67550 = VECTOR ( 'NONE', #130159, 1000.000000000000000 ) ;
#67551 = ORIENTED_EDGE ( 'NONE', *, *, #63774, .F. ) ;
#67553 = EDGE_LOOP ( 'NONE', ( #160680, #107314, #178096, #253054 ) ) ;
#67552 = AXIS2_PLACEMENT_3D ( 'NONE', #236917, #79106, #139064 ) ;
#67554 = VERTEX_POINT ( 'NONE', #179298 ) ;
#67555 = DIRECTION ( 'NONE',  ( 1.000000000000000000, -0.000000000000000000, -0.000000000000000000 ) ) ;
#67556 = DIRECTION ( 'NONE',  ( -1.000000000000000000, 1.836970198721029934E-16, 1.282749433769087582E-30 ) ) ;
#67557 = DIRECTION ( 'NONE',  ( 1.000000000000000000, 0.000000000000000000, -0.000000000000000000 ) ) ;
#67558 = CARTESIAN_POINT ( 'NONE',  ( 21.14999999999999503, -11.74999999999999112, 11.75000000000000000 ) ) ;
#67559 = CARTESIAN_POINT ( 'NONE',  ( -16.87304349924914604, 9.961745077957175454, -20.88906667504524961 ) ) ;
#67560 = ADVANCED_FACE ( 'NONE', ( #123157 ), #244489, .T. ) ;
#67562 = DIRECTION ( 'NONE',  ( -4.408576920032447355E-17, 0.9371753822965316338, -0.3488585713686134793 ) ) ;
#67561 = DIRECTION ( 'NONE',  ( -1.000000000000000000, -1.394253735153569469E-16, -2.602809386958778209E-16 ) ) ;
#67564 = ORIENTED_EDGE ( 'NONE', *, *, #242321, .F. ) ;
#67563 = CARTESIAN_POINT ( 'NONE',  ( -21.05000000000000071, 60.94483358488582070, -234.0465764481390636 ) ) ;
#67565 = DIRECTION ( 'NONE',  ( -1.000000000000000000, -0.000000000000000000, -0.000000000000000000 ) ) ;
#67566 = EDGE_LOOP ( 'NONE', ( #164958, #246323, #238388, #155127 ) ) ;
#67567 = EDGE_CURVE ( 'NONE', #57578, #108295, #11276, .T. ) ;
#67568 = CARTESIAN_POINT ( 'NONE',  ( 21.05000000000000071, -9.399999999988844834, -191.1060308773475072 ) ) ;
#67569 = ORIENTED_EDGE ( 'NONE', *, *, #48174, .F. ) ;
#67570 = ORIENTED_EDGE ( 'NONE', *, *, #149762, .T. ) ;
#67571 = PLANE ( 'NONE',  #71181 ) ;
#67572 = DIRECTION ( 'NONE',  ( 1.000000000000000000, 0.000000000000000000, 0.000000000000000000 ) ) ;
#67573 = CARTESIAN_POINT ( 'NONE',  ( -16.88783316861814754, 66.05000000001153637, -48.77537152650415919 ) ) ;
#67574 = CARTESIAN_POINT ( 'NONE',  ( 20.94999999999999574, -11.48912529306490349, -170.5999999999999659 ) ) ;
#67575 = PRODUCT_RELATED_PRODUCT_CATEGORY ( 'part', '', ( #32833 ) ) ;
#67576 = CARTESIAN_POINT ( 'NONE',  ( -20.94999999999999929, 4.313202326203128933, -245.5540684919841681 ) ) ;
#67577 = ORIENTED_EDGE ( 'NONE', *, *, #114079, .T. ) ;
#67578 = VERTEX_POINT ( 'NONE', #80127 ) ;
#67579 = EDGE_CURVE ( 'NONE', #206237, #213025, #161311, .T. ) ;
#67580 = DIRECTION ( 'NONE',  ( 2.952720810173289112E-16, 0.9651348961777157509, -0.2617529984165031243 ) ) ;
#67582 = ORIENTED_EDGE ( 'NONE', *, *, #60502, .F. ) ;
#67581 = EDGE_CURVE ( 'NONE', #39176, #200766, #107127, .T. ) ;
#67583 = CARTESIAN_POINT ( 'NONE',  ( -21.07928932188134041, 0.09889514566555068775, -127.6714833436067238 ) ) ;
#67584 = LINE ( 'NONE', #207107, #223493 ) ;
#67585 = ORIENTED_EDGE ( 'NONE', *, *, #130920, .F. ) ;
#67586 = EDGE_CURVE ( 'NONE', #144717, #168277, #243091, .T. ) ;
#67587 = DIRECTION ( 'NONE',  ( 0.000000000000000000, 0.000000000000000000, -1.000000000000000000 ) ) ;
#67588 = CARTESIAN_POINT ( 'NONE',  ( -18.69999999999999929, 10.31653824539118069, -11.82383137372478110 ) ) ;
#67589 = CARTESIAN_POINT ( 'NONE',  ( 18.59999999999999076, 14.05000000001116689, -72.51369507076103105 ) ) ;
#67590 = ORIENTED_EDGE ( 'NONE', *, *, #10721, .T. ) ;
#67591 = CARTESIAN_POINT ( 'NONE',  ( 21.14999999999999503, -11.74999999998883560, -136.9000000000000341 ) ) ;
#67592 = DIRECTION ( 'NONE',  ( 1.000000000000000000, -0.000000000000000000, -0.000000000000000000 ) ) ;
#67593 = DIRECTION ( 'NONE',  ( 0.000000000000000000, 0.000000000000000000, 1.000000000000000000 ) ) ;
#67594 = FACE_OUTER_BOUND ( 'NONE', #51899, .T. ) ;
#67595 = LINE ( 'NONE', #48025, #191503 ) ;
#67596 = EDGE_CURVE ( 'NONE', #251815, #56792, #207856, .T. ) ;
#67597 = VERTEX_POINT ( 'NONE', #166167 ) ;
#67598 = DIRECTION ( 'NONE',  ( 0.000000000000000000, -0.4721928772776973204, -0.8814952561688629284 ) ) ;
#67599 = ORIENTED_EDGE ( 'NONE', *, *, #68904, .T. ) ;
#67600 = DIRECTION ( 'NONE',  ( 0.000000000000000000, 0.000000000000000000, 1.000000000000000000 ) ) ;
#67601 = LINE ( 'NONE', #241133, #231314 ) ;
#67602 = DIRECTION ( 'NONE',  ( 0.000000000000000000, 0.000000000000000000, -1.000000000000000000 ) ) ;
#67603 = CARTESIAN_POINT ( 'NONE',  ( -18.40000000000000213, 8.212522512469059066, -212.1579332307740344 ) ) ;
#67604 = ORIENTED_EDGE ( 'NONE', *, *, #177886, .F. ) ;
#67605 = EDGE_CURVE ( 'NONE', #145382, #137027, #7154, .T. ) ;
#67606 = DIRECTION ( 'NONE',  ( 1.000000000000000000, 2.986185139342070877E-16, -6.665775143889691788E-16 ) ) ;
#67607 = CARTESIAN_POINT ( 'NONE',  ( 21.87500000000000355, 9.750000000011153745, -121.6500000000000341 ) ) ;
#67608 = CARTESIAN_POINT ( 'NONE',  ( -18.59999999999999787, 68.97833521811179480, -99.38954208262707368 ) ) ;
#67609 = DIRECTION ( 'NONE',  ( -6.938893903907222067E-15, 1.000000000000000000, 0.000000000000000000 ) ) ;
#67610 = AXIS2_PLACEMENT_3D ( 'NONE', #70211, #108031, #147140 ) ;
#67611 = PLANE ( 'NONE',  #114226 ) ;
#67613 = DIRECTION ( 'NONE',  ( -1.000000000000000000, -0.000000000000000000, 0.000000000000000000 ) ) ;
#67612 = AXIS2_PLACEMENT_3D ( 'NONE', #80825, #46835, #24759 ) ;
#67614 = VERTEX_POINT ( 'NONE', #249534 ) ;
#67615 = ORIENTED_EDGE ( 'NONE', *, *, #176326, .F. ) ;
#67616 = LINE ( 'NONE', #25939, #120751 ) ;
#67617 = DIRECTION ( 'NONE',  ( 0.000000000000000000, 0.000000000000000000, 1.000000000000000000 ) ) ;
#67619 = FACE_OUTER_BOUND ( 'NONE', #49704, .T. ) ;
#67618 = CIRCLE ( 'NONE', #30222, 0.2000000000000057288 ) ;
#67621 = ADVANCED_FACE ( 'NONE', ( #248238 ), #246938, .F. ) ;
#67620 = LINE ( 'NONE', #71504, #22787 ) ;
#67622 =( BOUNDED_CURVE ( )  B_SPLINE_CURVE ( 3, ( #209215, #147526, #148825, #168427 ),
 .UNSPECIFIED., .F., .F. ) 
 B_SPLINE_CURVE_WITH_KNOTS ( ( 4, 4 ),
 ( 5.731445031868798168, 5.983100554402349225 ),
 .UNSPECIFIED. ) 
 CURVE ( )  GEOMETRIC_REPRESENTATION_ITEM ( )  RATIONAL_B_SPLINE_CURVE ( ( 1.000000000000000000, 0.9947294176030464508, 0.9947294176030464508, 1.000000000000000000 ) ) 
 REPRESENTATION_ITEM ( '' )  );
#67623 = DIRECTION ( 'NONE',  ( 0.000000000000000000, -0.4088369013363296611, 0.9126074666063764829 ) ) ;
#67624 = ORIENTED_EDGE ( 'NONE', *, *, #121800, .F. ) ;
#67625 = DIRECTION ( 'NONE',  ( 2.694716079187272946E-16, -1.000000000000000000, 0.000000000000000000 ) ) ;
#67626 = EDGE_CURVE ( 'NONE', #169137, #211645, #226070, .T. ) ;
#67627 = CONTEXT_DEPENDENT_SHAPE_REPRESENTATION ( #144112, #55733 ) ;
#67628 = CARTESIAN_POINT ( 'NONE',  ( 20.94999999999999929, 79.37986612816742138, -196.2658927859692142 ) ) ;
#67629 = AXIS2_PLACEMENT_3D ( 'NONE', #136412, #80287, #197690 ) ;
#67630 = EDGE_LOOP ( 'NONE', ( #232992, #250640, #34590, #252001 ) ) ;
#67631 = AXIS2_PLACEMENT_3D ( 'NONE', #3613, #204379, #27071 ) ;
#67632 = LINE ( 'NONE', #166771, #117007 ) ;
#67633 = EDGE_CURVE ( 'NONE', #13472, #201172, #223626, .T. ) ;
#67634 = EDGE_CURVE ( 'NONE', #42134, #42010, #15575, .T. ) ;
#67635 = ORIENTED_EDGE ( 'NONE', *, *, #41883, .T. ) ;
#67636 = VERTEX_POINT ( 'NONE', #125712 ) ;
#67637 = CIRCLE ( 'NONE', #55138, 0.1000000000000028644 ) ;
#67638 = ORIENTED_EDGE ( 'NONE', *, *, #150069, .F. ) ;
#67639 = DIRECTION ( 'NONE',  ( -1.000000000000000000, -7.304098846218135653E-16, 4.607487905232624742E-31 ) ) ;
#67640 = DIRECTION ( 'NONE',  ( 0.000000000000000000, -7.026728003956683390E-15, 1.000000000000000000 ) ) ;
#67641 = CARTESIAN_POINT ( 'NONE',  ( -23.15000000000000213, 36.17635217701699446, -235.9630383263116471 ) ) ;
#67642 = FACE_OUTER_BOUND ( 'NONE', #115415, .T. ) ;
#67644 = DIRECTION ( 'NONE',  ( 1.000000000000000000, 0.000000000000000000, 0.000000000000000000 ) ) ;
#67643 = CIRCLE ( 'NONE', #142636, 0.1000000000000028644 ) ;
#67645 = VECTOR ( 'NONE', #78549, 1000.000000000000000 ) ;
#67646 = CARTESIAN_POINT ( 'NONE',  ( 21.14999999999999858, 64.25000000001205080, -124.3731074845243825 ) ) ;
#67649 = DIRECTION ( 'NONE',  ( 0.000000000000000000, 1.000000000000000000, 0.000000000000000000 ) ) ;
#67648 = CIRCLE ( 'NONE', #100913, 0.5000000000000004441 ) ;
#67647 = CARTESIAN_POINT ( 'NONE',  ( 20.95035502843362707, 10.47763832678762164, -108.0762997087363999 ) ) ;
#67650 = DIRECTION ( 'NONE',  ( 0.7071067811865493491, 0.7071067811865456854, 0.000000000000000000 ) ) ;
#67651 = CARTESIAN_POINT ( 'NONE',  ( -23.15000000000000213, 6.878457983866232972, -212.1414458560986986 ) ) ;
#67652 = DIRECTION ( 'NONE',  ( 1.000000000000000000, 0.000000000000000000, 0.000000000000000000 ) ) ;
#67653 = FACE_OUTER_BOUND ( 'NONE', #147190, .T. ) ;
#67654 = ORIENTED_EDGE ( 'NONE', *, *, #111768, .T. ) ;
#67655 = ORIENTED_EDGE ( 'NONE', *, *, #52105, .F. ) ;
#67656 = DIRECTION ( 'NONE',  ( -0.000000000000000000, -0.1350103645451807555, -0.9908441862701610203 ) ) ;
#67657 = EDGE_CURVE ( 'NONE', #41196, #74683, #29233, .T. ) ;
#67658 = CARTESIAN_POINT ( 'NONE',  ( 21.05000000000000071, 67.23127455305841238, -235.8551265064783991 ) ) ;
#67660 = CARTESIAN_POINT ( 'NONE',  ( -15.75000000000001066, 12.72457643131171245, -215.4883117230867526 ) ) ;
#67659 = CARTESIAN_POINT ( 'NONE',  ( -23.25000000000000355, 64.25000000001190870, -93.77310748452438816 ) ) ;
#67661 = CYLINDRICAL_SURFACE ( 'NONE', #206098, 0.09999999999999939493 ) ;
#67663 = EDGE_CURVE ( 'NONE', #139774, #135040, #224803, .T. ) ;
#67662 = DIRECTION ( 'NONE',  ( 1.073024830501117923E-15, -0.9126074666063771490, -0.4088369013363281623 ) ) ;
#67664 = CARTESIAN_POINT ( 'NONE',  ( 18.49999999999999289, 11.75000000001115552, -58.35000000000000142 ) ) ;
#67665 = ORIENTED_EDGE ( 'NONE', *, *, #3424, .T. ) ;
#67666 = ORIENTED_EDGE ( 'NONE', *, *, #168950, .F. ) ;
#67667 = ADVANCED_FACE ( 'NONE', ( #48740 ), #128300, .T. ) ;
#67668 = CARTESIAN_POINT ( 'NONE',  ( -15.31895204843005587, 9.396533993953919861, -17.90593977917330193 ) ) ;
#67669 = EDGE_LOOP ( 'NONE', ( #135664, #223532, #14321 ) ) ;
#67670 = DIRECTION ( 'NONE',  ( 0.000000000000000000, 0.000000000000000000, 1.000000000000000000 ) ) ;
#67671 = ADVANCED_FACE ( 'NONE', ( #108725 ), #256923, .T. ) ;
#67672 = AXIS2_PLACEMENT_3D ( 'NONE', #138987, #17773, #178179 ) ;
#67673 = VECTOR ( 'NONE', #108263, 1000.000000000000000 ) ;
#67674 = DIRECTION ( 'NONE',  ( -1.000000000000000000, -0.000000000000000000, -0.000000000000000000 ) ) ;
#67675 = ORIENTED_EDGE ( 'NONE', *, *, #84155, .F. ) ;
#67676 = CARTESIAN_POINT ( 'NONE',  ( -18.53317502108577131, 18.39833411442327460, -236.9692678682430369 ) ) ;
#67677 = CIRCLE ( 'NONE', #42736, 4.149999999999987033 ) ;
#67678 = ORIENTED_EDGE ( 'NONE', *, *, #49272, .F. ) ;
#67679 = EDGE_CURVE ( 'NONE', #49603, #68445, #3050, .T. ) ;
#67680 = DIRECTION ( 'NONE',  ( 0.2834754621636438876, 0.5133902848552793774, 0.8099827638705180410 ) ) ;
#67681 = EDGE_CURVE ( 'NONE', #9869, #171947, #28049, .T. ) ;
#67682 = CARTESIAN_POINT ( 'NONE',  ( -22.50000000000000000, 1.115600667400684642E-11, -161.2499999999999716 ) ) ;
#67684 = VECTOR ( 'NONE', #162550, 999.9999999999998863 ) ;
#67683 = DIRECTION ( 'NONE',  ( 1.000000000000000000, 0.000000000000000000, 0.000000000000000000 ) ) ;
#67685 = DIRECTION ( 'NONE',  ( 0.7071067811865475727, 0.7071067811865475727, 2.044391222244500083E-16 ) ) ;
#67686 = CARTESIAN_POINT ( 'NONE',  ( -21.05000000000000071, -9.519327731092440459, -6.972976376559336664 ) ) ;
#67687 = CARTESIAN_POINT ( 'NONE',  ( -16.90138253750126651, 66.05000000001254534, -182.8115447766198827 ) ) ;
#67688 = CIRCLE ( 'NONE', #180138, 0.9000000000000014655 ) ;
#67689 = FACE_OUTER_BOUND ( 'NONE', #89785, .T. ) ;
#67691 = CYLINDRICAL_SURFACE ( 'NONE', #191274, 0.09999999999999939493 ) ;
#67690 = VECTOR ( 'NONE', #113346, 1000.000000000000000 ) ;
#67692 = AXIS2_PLACEMENT_3D ( 'NONE', #136771, #33882, #32591 ) ;
#67694 = VERTEX_POINT ( 'NONE', #30492 ) ;
#67693 = CARTESIAN_POINT ( 'NONE',  ( 18.39999999999999858, -0.7490476236415669620, -242.2033265267442061 ) ) ;
#67696 = CARTESIAN_POINT ( 'NONE',  ( -18.50000000000000000, 59.16775194334852728, -221.0793150863668473 ) ) ;
#67695 = DIRECTION ( 'NONE',  ( 1.000000000000000000, -0.000000000000000000, 0.000000000000000000 ) ) ;
#67697 = ORIENTED_EDGE ( 'NONE', *, *, #27844, .T. ) ;
#67699 = ORIENTED_EDGE ( 'NONE', *, *, #71764, .F. ) ;
#67698 = DIRECTION ( 'NONE',  ( -1.000000000000000000, 0.000000000000000000, 0.000000000000000000 ) ) ;
#67700 = ORIENTED_EDGE ( 'NONE', *, *, #84634, .T. ) ;
#67701 = DIRECTION ( 'NONE',  ( 0.000000000000000000, 0.000000000000000000, 1.000000000000000000 ) ) ;
#67702 = CARTESIAN_POINT ( 'NONE',  ( -23.25000000000000355, 64.25000000001261924, -190.8731074845244393 ) ) ;
#67703 = AXIS2_PLACEMENT_3D ( 'NONE', #51989, #114554, #211088 ) ;
#67704 = DIRECTION ( 'NONE',  ( -1.000000000000000000, 0.000000000000000000, 0.000000000000000000 ) ) ;
#67705 = DIRECTION ( 'NONE',  ( 0.000000000000000000, -1.000000000000000000, 0.000000000000000000 ) ) ;
#67706 = CARTESIAN_POINT ( 'NONE',  ( 18.59999999999999076, 1.115600667400684642E-11, -100.5000000000000426 ) ) ;
#67707 = DIRECTION ( 'NONE',  ( -1.073024830501117725E-15, -0.000000000000000000, -1.000000000000000000 ) ) ;
#67708 = AXIS2_PLACEMENT_3D ( 'NONE', #68540, #227598, #148076 ) ;
#67709 = DIRECTION ( 'NONE',  ( 1.000000000000000000, 0.000000000000000000, 0.000000000000000000 ) ) ;
#67710 = DIRECTION ( 'NONE',  ( 0.000000000000000000, 0.2617529984165185009, 0.9651348961777115321 ) ) ;
#67711 = CIRCLE ( 'NONE', #42582, 3.999999999999999112 ) ;
#67712 = DIRECTION ( 'NONE',  ( 0.000000000000000000, -0.5000000000000078826, -0.8660254037844340447 ) ) ;
#67713 = AXIS2_PLACEMENT_3D ( 'NONE', #256225, #157230, #217148 ) ;
#67714 = CIRCLE ( 'NONE', #250855, 0.09999999999998898659 ) ;
#67715 = EDGE_LOOP ( 'NONE', ( #88375, #26971, #219399, #11338 ) ) ;
#67716 = ORIENTED_EDGE ( 'NONE', *, *, #113155, .F. ) ;
#67717 = CARTESIAN_POINT ( 'NONE',  ( -21.05000000000000071, 77.85102823015273543, -91.36919421510179973 ) ) ;
#67718 = ADVANCED_FACE ( 'NONE', ( #127003 ), #90430, .F. ) ;
#67719 = ORIENTED_EDGE ( 'NONE', *, *, #56199, .F. ) ;
#67720 = LINE ( 'NONE', #89836, #113444 ) ;
#67721 = ORIENTED_EDGE ( 'NONE', *, *, #84048, .T. ) ;
#67723 = AXIS2_PLACEMENT_3D ( 'NONE', #203452, #103040, #143465 ) ;
#67722 = DIRECTION ( 'NONE',  ( -1.020425574104004196E-15, 0.000000000000000000, -1.000000000000000000 ) ) ;
#67725 =( BOUNDED_SURFACE ( )  B_SPLINE_SURFACE ( 3, 2, ( 
 ( #241063, #222750, #70144 ),
 ( #227903, #51807, #49260 ),
 ( #28461, #152247, #130073 ),
 ( #231767, #171819, #14002 ) ),
 .UNSPECIFIED., .F., .F., .F. ) 
 B_SPLINE_SURFACE_WITH_KNOTS ( ( 4, 4 ),
 ( 3, 3 ),
 ( -1.355252715606880543E-20, 0.0003124336117481266921 ),
 ( 0.000000000000000000, 1.000000000000000000 ),
 .UNSPECIFIED. ) 
 GEOMETRIC_REPRESENTATION_ITEM ( )  RATIONAL_B_SPLINE_SURFACE ( (
 ( 1.000000000000000000, 0.7040654476015972829, 1.000000000000000000),
 ( 1.000000000000000000, 0.7039193538781918225, 1.000000000000000000),
 ( 1.000000000000000000, 0.7089171279145408677, 1.000000000000000000),
 ( 1.000000000000000000, 0.7071067811865506814, 1.000000000000000000) ) ) 
 REPRESENTATION_ITEM ( '' )  SURFACE ( )  );
#67724 = AXIS2_PLACEMENT_3D ( 'NONE', #125681, #200091, #21470 ) ;
#67726 = CARTESIAN_POINT ( 'NONE',  ( -23.25000000000000000, 76.00000000001213607, -136.5231074845243313 ) ) ;
#67727 = CARTESIAN_POINT ( 'NONE',  ( -22.43310005002225438, -2.473551863546898932, -189.6159672949451362 ) ) ;
#67728 = DIRECTION ( 'NONE',  ( 0.000000000000000000, 0.000000000000000000, 1.000000000000000000 ) ) ;
#67729 = CARTESIAN_POINT ( 'NONE',  ( -18.50000000000000000, 77.63717271298267519, -158.4409541190523214 ) ) ;
#67730 = ORIENTED_EDGE ( 'NONE', *, *, #82554, .F. ) ;
#67731 = DIRECTION ( 'NONE',  ( 1.000000000000000000, 0.000000000000000000, 0.000000000000000000 ) ) ;
#67732 = CARTESIAN_POINT ( 'NONE',  ( -16.86420534634261514, 66.02938455442082955, -182.6047709352870356 ) ) ;
#67733 = DIRECTION ( 'NONE',  ( 0.000000000000000000, -1.000000000000000000, -6.982962677686265922E-15 ) ) ;
#67735 = EDGE_CURVE ( 'NONE', #181648, #110818, #194649, .T. ) ;
#67734 = CARTESIAN_POINT ( 'NONE',  ( 28.12018973533754362, 11.62642356364896123, 33.00000000000000000 ) ) ;
#67737 = ORIENTED_EDGE ( 'NONE', *, *, #84312, .F. ) ;
#67736 = B_SPLINE_CURVE_WITH_KNOTS ( 'NONE', 3,
 ( #92736, #210143, #34102, #154061, #193147, #112327, #111029, #191882 ),
 .UNSPECIFIED., .F., .F.,
 ( 4, 2, 2, 4 ),
 ( 0.000000000000000000, 6.534141206311569483E-05, 0.0001306828241262313897, 0.0002613656482524659235 ),
 .UNSPECIFIED. ) ;
#67739 = DIRECTION ( 'NONE',  ( 0.000000000000000000, 6.982962677686266711E-15, -1.000000000000000000 ) ) ;
#67738 = CARTESIAN_POINT ( 'NONE',  ( 21.13498764882293557, 60.96169324425918035, -234.1564776252124886 ) ) ;
#67740 = VECTOR ( 'NONE', #103855, 1000.000000000000000 ) ;
#67741 = EDGE_LOOP ( 'NONE', ( #204698, #70648, #111780, #50134 ) ) ;
#67744 = VERTEX_POINT ( 'NONE', #124447 ) ;
#67743 = CARTESIAN_POINT ( 'NONE',  ( -16.83794479845803949, 51.48839318213948957, -232.0308244825887414 ) ) ;
#67742 = DIRECTION ( 'NONE',  ( 1.000000000000000000, 0.000000000000000000, 0.000000000000000000 ) ) ;
#67745 = AXIS2_PLACEMENT_3D ( 'NONE', #176437, #255896, #77304 ) ;
#67746 = ORIENTED_EDGE ( 'NONE', *, *, #146159, .T. ) ;
#67747 = CARTESIAN_POINT ( 'NONE',  ( 18.59999999999999076, 6.400000000011158541, -177.4304246300615375 ) ) ;
#67748 = VECTOR ( 'NONE', #217334, 1000.000000000000000 ) ;
#67749 = DIRECTION ( 'NONE',  ( 1.000000000000000000, 3.448943450116723568E-16, 6.438528483529607644E-16 ) ) ;
#67750 = DIRECTION ( 'NONE',  ( 0.000000000000000000, -1.000000000000000000, 0.000000000000000000 ) ) ;
#67751 = VERTEX_POINT ( 'NONE', #5742 ) ;
#67752 = CARTESIAN_POINT ( 'NONE',  ( -23.15000000000000213, 30.69873658968802488, -264.9868732779115703 ) ) ;
#67753 = DIRECTION ( 'NONE',  ( 1.000000000000000000, 0.000000000000000000, 0.000000000000000000 ) ) ;
#67755 = CARTESIAN_POINT ( 'NONE',  ( -18.39999999999999858, 11.47316190336247388, -9.299829248466007670 ) ) ;
#67754 = FACE_OUTER_BOUND ( 'NONE', #37294, .T. ) ;
#67757 = ORIENTED_EDGE ( 'NONE', *, *, #85294, .F. ) ;
#67756 = LINE ( 'NONE', #29938, #43255 ) ;
#67758 = ORIENTED_EDGE ( 'NONE', *, *, #42882, .T. ) ;
#67759 = CARTESIAN_POINT ( 'NONE',  ( -16.89060415895971090, 9.951220762813354881, -79.64592022427049756 ) ) ;
#67760 = AXIS2_PLACEMENT_3D ( 'NONE', #2098, #25545, #26845 ) ;
#67761 = DIRECTION ( 'NONE',  ( 0.000000000000000000, 6.982962677686266711E-15, -1.000000000000000000 ) ) ;
#67762 = DIRECTION ( 'NONE',  ( -2.978066053179069723E-16, -1.000000000000000000, -7.147358527629766941E-15 ) ) ;
#67763 = ORIENTED_EDGE ( 'NONE', *, *, #156696, .T. ) ;
#67764 = DIRECTION ( 'NONE',  ( 1.000000000000000000, 0.000000000000000000, 0.000000000000000000 ) ) ;
#67765 = CIRCLE ( 'NONE', #155289, 0.5000000000000004441 ) ;
#67766 = CARTESIAN_POINT ( 'NONE',  ( 20.94999999999999929, 1.115600667400684642E-11, -33.50000000000000000 ) ) ;
#67767 = DIRECTION ( 'NONE',  ( 0.000000000000000000, 0.4999999999999956701, -0.8660254037844411501 ) ) ;
#67768 = VERTEX_POINT ( 'NONE', #86561 ) ;
#67769 = DIRECTION ( 'NONE',  ( 0.000000000000000000, 1.000000000000000000, 0.000000000000000000 ) ) ;
#67770 = B_SPLINE_CURVE_WITH_KNOTS ( 'NONE', 3,
 ( #207504, #148805, #210066, #30152, #31452, #86222, #125388, #66695, #244031, #229622 ),
 .UNSPECIFIED., .F., .F.,
 ( 4, 3, 3, 4 ),
 ( 0.000000000000000000, 1.004626015991719593E-05, 1.831183478183680716E-05, 2.062343583996558100E-05 ),
 .UNSPECIFIED. ) ;
#67771 = ADVANCED_FACE ( 'NONE', ( #203963 ), #127989, .T. ) ;
#67772 = EDGE_LOOP ( 'NONE', ( #174789, #85750, #132978 ) ) ;
#67773 = DIRECTION ( 'NONE',  ( -1.000000000000000000, 0.000000000000000000, 0.000000000000000000 ) ) ;
#67774 = DIRECTION ( 'NONE',  ( 0.000000000000000000, 6.982962677686266711E-15, -1.000000000000000000 ) ) ;
#67776 = ORIENTED_EDGE ( 'NONE', *, *, #169783, .T. ) ;
#67775 = AXIS2_PLACEMENT_3D ( 'NONE', #112569, #150419, #50012 ) ;
#67777 = EDGE_LOOP ( 'NONE', ( #88601, #161828, #180079, #230320 ) ) ;
#67778 = ADVANCED_FACE ( 'NONE', ( #25359 ), #57025, .F. ) ;
#67779 = LINE ( 'NONE', #84735, #83206 ) ;
#67780 = ORIENTED_EDGE ( 'NONE', *, *, #254255, .F. ) ;
#67782 = VERTEX_POINT ( 'NONE', #192138 ) ;
#67781 = CARTESIAN_POINT ( 'NONE',  ( 12.25000000000000355, 66.65000000001256808, -186.6588398769083028 ) ) ;
#67783 = EDGE_CURVE ( 'NONE', #88021, #54936, #120494, .T. ) ;
#67784 = ORIENTED_EDGE ( 'NONE', *, *, #145227, .F. ) ;
#67786 = ORIENTED_EDGE ( 'NONE', *, *, #242275, .T. ) ;
#67785 = VERTEX_POINT ( 'NONE', #12218 ) ;
#67787 = DIRECTION ( 'NONE',  ( 0.000000000000000000, 0.000000000000000000, -1.000000000000000000 ) ) ;
#67788 = VECTOR ( 'NONE', #192389, 999.9999999999998863 ) ;
#67790 = EDGE_CURVE ( 'NONE', #162955, #248032, #140431, .T. ) ;
#67789 = ORIENTED_EDGE ( 'NONE', *, *, #177754, .T. ) ;
#67791 = DIRECTION ( 'NONE',  ( 0.000000000000000000, 0.000000000000000000, 1.000000000000000000 ) ) ;
#67792 = CARTESIAN_POINT ( 'NONE',  ( -20.54999999999999716, 70.80971041069356886, -215.3055740759912453 ) ) ;
#67793 = CARTESIAN_POINT ( 'NONE',  ( 21.05000000000000071, 67.22371710472015138, -194.9644784893834810 ) ) ;
#67794 = AXIS2_PLACEMENT_3D ( 'NONE', #959, #160097, #80497 ) ;
#67795 = DIRECTION ( 'NONE',  ( 0.000000000000000000, -0.4088369013363783999, 0.9126074666063545004 ) ) ;
#67796 = ORIENTED_EDGE ( 'NONE', *, *, #221550, .F. ) ;
#67797 = ORIENTED_EDGE ( 'NONE', *, *, #13507, .T. ) ;
#67798 = VECTOR ( 'NONE', #219906, 1000.000000000000000 ) ;
#67799 = DIRECTION ( 'NONE',  ( 1.000000000000000000, -0.000000000000000000, -0.000000000000000000 ) ) ;
#67801 = ORIENTED_EDGE ( 'NONE', *, *, #162331, .T. ) ;
#67800 = CARTESIAN_POINT ( 'NONE',  ( 20.95000000000000284, 11.60000000001116227, -60.07179676972450011 ) ) ;
#67802 = DIRECTION ( 'NONE',  ( 1.000000000000000000, 0.000000000000000000, 0.000000000000000000 ) ) ;
#67804 = EDGE_LOOP ( 'NONE', ( #7594, #220224, #130201, #47080, #1257 ) ) ;
#67803 = DIRECTION ( 'NONE',  ( 0.000000000000000000, -0.2965989261549410450, -0.9550021345545443019 ) ) ;
#67805 = ADVANCED_FACE ( 'NONE', ( #116441 ), #215523, .T. ) ;
#67806 = ORIENTED_EDGE ( 'NONE', *, *, #158386, .T. ) ;
#67807 = DIRECTION ( 'NONE',  ( 0.000000000000000000, 0.000000000000000000, -1.000000000000000000 ) ) ;
#67808 = VECTOR ( 'NONE', #39645, 1000.000000000000000 ) ;
#67809 = AXIS2_PLACEMENT_3D ( 'NONE', #247358, #251201, #127425 ) ;
#67810 = ORIENTED_EDGE ( 'NONE', *, *, #80854, .F. ) ;
#67811 = DIRECTION ( 'NONE',  ( 1.000000000000000000, 2.952720810173289112E-16, -0.000000000000000000 ) ) ;
#67812 = LINE ( 'NONE', #144760, #127781 ) ;
#67814 = ORIENTED_EDGE ( 'NONE', *, *, #251391, .T. ) ;
#67813 = ORIENTED_EDGE ( 'NONE', *, *, #44947, .F. ) ;
#67815 = ORIENTED_EDGE ( 'NONE', *, *, #250059, .F. ) ;
#67816 = DIRECTION ( 'NONE',  ( -2.578261006436900068E-14, 0.1350103645451904977, -0.9908441862701597991 ) ) ;
#67817 = VERTEX_POINT ( 'NONE', #14794 ) ;
#67818 = ORIENTED_EDGE ( 'NONE', *, *, #125210, .F. ) ;
#67820 = CARTESIAN_POINT ( 'NONE',  ( -18.59999999999999787, 16.56538529403860238, -240.6448716151659823 ) ) ;
#67819 = VECTOR ( 'NONE', #123669, 1000.000000000000000 ) ;
#67822 = ORIENTED_EDGE ( 'NONE', *, *, #110532, .T. ) ;
#67821 = CARTESIAN_POINT ( 'NONE',  ( 20.94999999999999574, 1.851028230152016674, -45.15391326942249606 ) ) ;
#67823 = DIRECTION ( 'NONE',  ( 0.000000000000000000, 0.000000000000000000, -1.000000000000000000 ) ) ;
#67825 = CARTESIAN_POINT ( 'NONE',  ( 21.08489247129321242, 11.30242931707484821, -211.1779520694198311 ) ) ;
#67824 = DIRECTION ( 'NONE',  ( -0.000000000000000000, -0.000000000000000000, -1.000000000000000000 ) ) ;
#67826 = LINE ( 'NONE', #87375, #149068 ) ;
#67827 = CARTESIAN_POINT ( 'NONE',  ( -18.38204789744325396, 11.47950103717623982, -191.7499999999999716 ) ) ;
#67828 = ORIENTED_EDGE ( 'NONE', *, *, #241356, .F. ) ;
#67829 = VECTOR ( 'NONE', #9877, 1000.000000000000000 ) ;
#67830 = AXIS2_PLACEMENT_3D ( 'NONE', #77970, #55819, #97512 ) ;
#67831 = AXIS2_PLACEMENT_3D ( 'NONE', #125397, #244038, #240218 ) ;
#67832 = EDGE_LOOP ( 'NONE', ( #124918, #108078, #5100, #184397, #98363, #169714, #211339, #121702 ) ) ;
#67833 = AXIS2_PLACEMENT_3D ( 'NONE', #9882, #13741, #206810 ) ;
#67834 = CARTESIAN_POINT ( 'NONE',  ( -21.14999999999994174, 84.00000000001119815, -37.18565239344504647 ) ) ;
#67835 = CARTESIAN_POINT ( 'NONE',  ( -18.40000000000000213, 64.66825945288661615, -82.17310748452439384 ) ) ;
#67836 = VERTEX_POINT ( 'NONE', #130851 ) ;
#67837 = EDGE_CURVE ( 'NONE', #195886, #12754, #69731, .T. ) ;
#67838 = LINE ( 'NONE', #147381, #998 ) ;
#67839 = VERTEX_POINT ( 'NONE', #252083 ) ;
#67840 = EDGE_LOOP ( 'NONE', ( #184258, #245374, #225058, #48624, #181514, #238315, #158904, #48568, #148604, #232326, #27435, #104616 ) ) ;
#67841 = CARTESIAN_POINT ( 'NONE',  ( -21.14999999893415250, 64.25000000001264766, -196.6786121409979273 ) ) ;
#67842 = DIRECTION ( 'NONE',  ( 1.000000000000000000, 0.000000000000000000, 0.000000000000000000 ) ) ;
#67843 = ORIENTED_EDGE ( 'NONE', *, *, #233172, .T. ) ;
#67844 = CARTESIAN_POINT ( 'NONE',  ( 23.14999999999999503, 35.97645343225767789, -235.9694016464868298 ) ) ;
#67845 = ORIENTED_EDGE ( 'NONE', *, *, #123725, .F. ) ;
#67846 = CARTESIAN_POINT ( 'NONE',  ( 19.87657994472041523, 64.25000000001220712, -145.2573193598975081 ) ) ;
#67848 = EDGE_CURVE ( 'NONE', #116279, #111921, #31793, .T. ) ;
#67847 = DIRECTION ( 'NONE',  ( 1.000000000000000000, -2.952720810173289112E-16, -2.061873921506763405E-30 ) ) ;
#67850 = DIRECTION ( 'NONE',  ( 0.000000000000000000, 0.4999999999999943379, 0.8660254037844420383 ) ) ;
#67849 = CARTESIAN_POINT ( 'NONE',  ( 21.00000000000000000, 0.000000000000000000, -7.800000000000000711 ) ) ;
#67851 = DIRECTION ( 'NONE',  ( 0.000000000000000000, 0.2128009952263604232, -0.9770955615653316162 ) ) ;
#67852 = DIRECTION ( 'NONE',  ( 0.000000000000000000, 1.000000000000000000, 0.000000000000000000 ) ) ;
#67853 = CARTESIAN_POINT ( 'NONE',  ( -23.24999999999999645, -9.599999999988845900, -207.6001893912220169 ) ) ;
#67854 = CARTESIAN_POINT ( 'NONE',  ( -20.54999999999999716, 82.09643798151613225, -215.4278993322501208 ) ) ;
#67855 = ADVANCED_FACE ( 'NONE', ( #210411 ), #248795, .T. ) ;
#67856 = CIRCLE ( 'NONE', #209495, 11.80000000000000426 ) ;
#67857 = ORIENTED_EDGE ( 'NONE', *, *, #77356, .T. ) ;
#67859 = VERTEX_POINT ( 'NONE', #52593 ) ;
#67858 = VERTEX_POINT ( 'NONE', #195987 ) ;
#67860 = ORIENTED_EDGE ( 'NONE', *, *, #95951, .T. ) ;
#67861 = CIRCLE ( 'NONE', #60046, 0.1000000000000060146 ) ;
#67862 = FACE_OUTER_BOUND ( 'NONE', #91892, .T. ) ;
#67863 = AXIS2_PLACEMENT_3D ( 'NONE', #231102, #212811, #112428 ) ;
#67864 = EDGE_CURVE ( 'NONE', #210604, #138871, #169531, .T. ) ;
#67865 = DIRECTION ( 'NONE',  ( 1.000000000000000000, 3.265361837132813093E-16, -0.000000000000000000 ) ) ;
#67867 = CARTESIAN_POINT ( 'NONE',  ( 20.94999999999999574, 11.62071067812981795, -194.1315833476589887 ) ) ;
#67866 = DIRECTION ( 'NONE',  ( -1.000000000000000000, 0.000000000000000000, 0.000000000000000000 ) ) ;
#67868 = CARTESIAN_POINT ( 'NONE',  ( 21.05000000000000071, 67.22371710471985295, -161.4644784893834810 ) ) ;
#67869 = ORIENTED_EDGE ( 'NONE', *, *, #136119, .T. ) ;
#67870 = CIRCLE ( 'NONE', #221963, 0.09999999999999939493 ) ;
#67871 = EDGE_CURVE ( 'NONE', #192399, #151179, #90547, .T. ) ;
#67872 = CARTESIAN_POINT ( 'NONE',  ( -22.48660254037843487, 11.65000000001115588, -100.4500000000000597 ) ) ;
#67873 = ADVANCED_FACE ( 'NONE', ( #231264 ), #129402, .F. ) ;
#67874 = CARTESIAN_POINT ( 'NONE',  ( -21.05000000000000071, -0.01465611851314312965, 6.496686585767865729 ) ) ;
#67875 = AXIS2_PLACEMENT_3D ( 'NONE', #137654, #112989, #132553 ) ;
#67876 = DIRECTION ( 'NONE',  ( 0.000000000000000000, 0.9770955615653548199, 0.2128009952262535920 ) ) ;
#67877 = VECTOR ( 'NONE', #181683, 999.9999999999998863 ) ;
#67878 = CIRCLE ( 'NONE', #101130, 7.720710678118692272 ) ;
#67879 = CARTESIAN_POINT ( 'NONE',  ( 20.94999999999999574, 36.65892442174472876, -249.5511627012454596 ) ) ;
#67880 = ORIENTED_EDGE ( 'NONE', *, *, #133221, .F. ) ;
#67881 = DIRECTION ( 'NONE',  ( -0.000000000000000000, -0.000000000000000000, -1.000000000000000000 ) ) ;
#67882 = CIRCLE ( 'NONE', #38657, 0.09999999999999939493 ) ;
#67883 = EDGE_CURVE ( 'NONE', #30427, #60636, #135973, .T. ) ;
#67884 = DIRECTION ( 'NONE',  ( 1.000000000000000000, -2.849773892568378313E-16, 7.728835255496647986E-17 ) ) ;
#67885 = EDGE_LOOP ( 'NONE', ( #106945, #4603, #177563, #82605 ) ) ;
#67886 = ORIENTED_EDGE ( 'NONE', *, *, #128632, .F. ) ;
#67887 = CARTESIAN_POINT ( 'NONE',  ( -20.64999999999999858, 68.75000000001205080, -124.2731074845243455 ) ) ;
#67888 = CARTESIAN_POINT ( 'NONE',  ( -20.94999999999999929, -12.41227409413852811, -131.0000000000000284 ) ) ;
#67889 = LINE ( 'NONE', #70498, #227910 ) ;
#67890 = EDGE_CURVE ( 'NONE', #92187, #2878, #176428, .T. ) ;
#67891 = CARTESIAN_POINT ( 'NONE',  ( -23.39999999999994529, 87.50449464844290048, -34.18759587077607165 ) ) ;
#67892 = CARTESIAN_POINT ( 'NONE',  ( -21.55000000000000426, 68.25000000001253397, -182.3731074845244109 ) ) ;
#67893 = ADVANCED_FACE ( 'NONE', ( #177720 ), #182336, .T. ) ;
#67895 = CIRCLE ( 'NONE', #192800, 0.09999999999999939493 ) ;
#67894 = DIRECTION ( 'NONE',  ( 1.000000000000000000, 0.000000000000000000, 0.000000000000000000 ) ) ;
#67896 = ORIENTED_EDGE ( 'NONE', *, *, #176658, .F. ) ;
#67897 = DIRECTION ( 'NONE',  ( -0.000000000000000000, 1.000000000000000000, -0.000000000000000000 ) ) ;
#67898 = CARTESIAN_POINT ( 'NONE',  ( 21.05000000000012150, 12.00928618750723231, -206.1912950450977746 ) ) ;
#67900 = CYLINDRICAL_SURFACE ( 'NONE', #78885, 0.09999999999999954758 ) ;
#67899 = DIRECTION ( 'NONE',  ( -1.000000000000000000, 0.000000000000000000, 0.000000000000000000 ) ) ;
#67901 = CARTESIAN_POINT ( 'NONE',  ( 18.39999999999999858, 85.60000000001166143, -62.92291809330219365 ) ) ;
#67902 = CIRCLE ( 'NONE', #176076, 11.75000000000001066 ) ;
#67903 = CYLINDRICAL_SURFACE ( 'NONE', #170487, 0.09999999999999939493 ) ;
#67904 = LINE ( 'NONE', #65332, #214943 ) ;
#67906 = ORIENTED_EDGE ( 'NONE', *, *, #173222, .T. ) ;
#67905 = CARTESIAN_POINT ( 'NONE',  ( 18.59999999999999076, 68.48451787451661232, -224.2224406095231757 ) ) ;
#67907 = VECTOR ( 'NONE', #225235, 1000.000000000000227 ) ;
#67908 = AXIS2_PLACEMENT_3D ( 'NONE', #65710, #86527, #46143 ) ;
#67909 = VECTOR ( 'NONE', #2630, 1000.000000000000000 ) ;
#67910 = VECTOR ( 'NONE', #39427, 1000.000000000000000 ) ;
#67911 = EDGE_CURVE ( 'NONE', #85343, #192073, #67334, .T. ) ;
#67912 = EDGE_CURVE ( 'NONE', #41742, #46950, #169720, .T. ) ;
#67913 = EDGE_CURVE ( 'NONE', #30860, #24511, #201100, .T. ) ;
#67914 = CARTESIAN_POINT ( 'NONE',  ( -23.15000000000000213, 36.65892442174472876, -249.5511627012454596 ) ) ;
#67915 = FACE_OUTER_BOUND ( 'NONE', #18909, .T. ) ;
#67916 = VECTOR ( 'NONE', #231004, 1000.000000000000000 ) ;
#67917 = EDGE_LOOP ( 'NONE', ( #247589, #5523, #79649, #4173 ) ) ;
#67918 = VECTOR ( 'NONE', #47792, 1000.000000000000000 ) ;
#67919 = AXIS2_PLACEMENT_3D ( 'NONE', #86961, #246076, #90823 ) ;
#67921 = CARTESIAN_POINT ( 'NONE',  ( -23.25000000000000000, 1.115626384983466744E-11, -64.90000000000000568 ) ) ;
#67920 = AXIS2_PLACEMENT_3D ( 'NONE', #204402, #84420, #222676 ) ;
#67922 = CARTESIAN_POINT ( 'NONE',  ( 23.15000000000000213, 84.59626168225486254, -93.57297996737396772 ) ) ;
#67923 = FACE_OUTER_BOUND ( 'NONE', #61565, .T. ) ;
#67924 = ORIENTED_EDGE ( 'NONE', *, *, #257468, .F. ) ;
#67925 = CARTESIAN_POINT ( 'NONE',  ( -23.15000000000000213, 4.776122516674676300E-16, -29.60000000000000142 ) ) ;
#67927 = VERTEX_POINT ( 'NONE', #120325 ) ;
#67926 = CARTESIAN_POINT ( 'NONE',  ( -20.07928932188135107, 9.220710678129810489, -54.75000000000000000 ) ) ;
#67928 = DIRECTION ( 'NONE',  ( 0.000000000000000000, 0.9274965247785529332, 0.3738317757009255171 ) ) ;
#67929 = CARTESIAN_POINT ( 'NONE',  ( -23.15000000000000213, 67.23127455305841238, -235.8551265064783991 ) ) ;
#67930 = VERTEX_POINT ( 'NONE', #78577 ) ;
#67931 = CARTESIAN_POINT ( 'NONE',  ( -16.92280123533723568, 66.05000000001261640, -190.6724751704383323 ) ) ;
#67932 = EDGE_CURVE ( 'NONE', #182212, #257159, #4175, .T. ) ;
#67933 = DIRECTION ( 'NONE',  ( 1.000000000000000000, 0.000000000000000000, 0.000000000000000000 ) ) ;
#67934 = CARTESIAN_POINT ( 'NONE',  ( -20.85000000000000142, 65.66751761918648356, -63.92826094061123143 ) ) ;
#67935 = CARTESIAN_POINT ( 'NONE',  ( -23.15000000000000213, -8.999999999988844479, -191.1060308773475356 ) ) ;
#67936 = FACE_OUTER_BOUND ( 'NONE', #47462, .T. ) ;
#67937 = ORIENTED_EDGE ( 'NONE', *, *, #76177, .T. ) ;
#67939 = EDGE_CURVE ( 'NONE', #97490, #131374, #99411, .T. ) ;
#67938 = FACE_OUTER_BOUND ( 'NONE', #201904, .T. ) ;
#67940 = FACE_OUTER_BOUND ( 'NONE', #120811, .T. ) ;
#67941 = DIRECTION ( 'NONE',  ( 0.000000000000000000, -0.4088369013363280513, 0.9126074666063769270 ) ) ;
#67942 = EDGE_CURVE ( 'NONE', #223851, #71853, #61531, .T. ) ;
#67943 = AXIS2_PLACEMENT_3D ( 'NONE', #201401, #47451, #85284 ) ;
#67944 = EDGE_CURVE ( 'NONE', #95308, #143032, #194824, .T. ) ;
#67945 = DIRECTION ( 'NONE',  ( -1.000000000000000000, 0.000000000000000000, -0.000000000000000000 ) ) ;
#67946 = ORIENTED_EDGE ( 'NONE', *, *, #207560, .T. ) ;
#67947 = ORIENTED_EDGE ( 'NONE', *, *, #131979, .F. ) ;
#67948 = ADVANCED_FACE ( 'NONE', ( #219369, #221919, #62873 ), #61593, .F. ) ;
#67949 = FACE_OUTER_BOUND ( 'NONE', #129049, .T. ) ;
#67950 = DIRECTION ( 'NONE',  ( 0.000000000000000000, 0.000000000000000000, -1.000000000000000000 ) ) ;
#67951 = PLANE ( 'NONE',  #15185 ) ;
#67952 = DIRECTION ( 'NONE',  ( -1.000000000000000000, -2.952720810173289112E-16, 0.000000000000000000 ) ) ;
#67953 = CARTESIAN_POINT ( 'NONE',  ( 23.24999999999999289, 61.57587952878035509, -212.2000740415318774 ) ) ;
#67954 = CYLINDRICAL_SURFACE ( 'NONE', #7635, 0.1000000000000002554 ) ;
#67955 = DIRECTION ( 'NONE',  ( 0.000000000000000000, -0.2617529984165152257, -0.9651348961777124202 ) ) ;
#67956 = LINE ( 'NONE', #185341, #176819 ) ;
#67958 = CARTESIAN_POINT ( 'NONE',  ( -18.41799967126709703, 46.96039440171526991, -255.3459640015733783 ) ) ;
#67957 = AXIS2_PLACEMENT_3D ( 'NONE', #69029, #148556, #251486 ) ;
#67959 = DIRECTION ( 'NONE',  ( 0.000000000000000000, 0.000000000000000000, -1.000000000000000000 ) ) ;
#67960 = EDGE_CURVE ( 'NONE', #148690, #133237, #100680, .T. ) ;
#67961 = VECTOR ( 'NONE', #30163, 1000.000000000000000 ) ;
#67963 = ORIENTED_EDGE ( 'NONE', *, *, #23116, .T. ) ;
#67962 = DIRECTION ( 'NONE',  ( 2.952720810173289112E-16, -1.000000000000000000, 0.000000000000000000 ) ) ;
#67964 = CARTESIAN_POINT ( 'NONE',  ( 21.08078803292165659, 69.66698703557526073, -170.1022934716822022 ) ) ;
#67965 = EDGE_CURVE ( 'NONE', #25637, #79373, #160728, .T. ) ;
#67966 = CARTESIAN_POINT ( 'NONE',  ( -21.07971444708686093, -1.261174164707013157, -194.7964993367602062 ) ) ;
#67968 = DIRECTION ( 'NONE',  ( -0.000000000000000000, 0.8814952561688430555, -0.4721928772777346239 ) ) ;
#67967 = CARTESIAN_POINT ( 'NONE',  ( -18.59999999999999787, 78.06784868750165174, -195.8985418047209350 ) ) ;
#67969 = VERTEX_POINT ( 'NONE', #220671 ) ;
#67970 = DIRECTION ( 'NONE',  ( 1.000000000000000000, -0.000000000000000000, -0.000000000000000000 ) ) ;
#67972 = ADVANCED_FACE ( 'NONE', ( #42048 ), #22490, .T. ) ;
#67971 = CARTESIAN_POINT ( 'NONE',  ( -33.72168855820451938, 66.05000000001260219, -190.8731074845244962 ) ) ;
#67973 = CARTESIAN_POINT ( 'NONE',  ( 20.94999999999999929, 13.06362847850371978, -210.5896934006125889 ) ) ;
#67974 = DIRECTION ( 'NONE',  ( -0.000000000000000000, -1.000000000000000000, -0.000000000000000000 ) ) ;
#67975 = DIRECTION ( 'NONE',  ( 0.000000000000000000, 0.000000000000000000, -1.000000000000000000 ) ) ;
#67976 = ORIENTED_EDGE ( 'NONE', *, *, #35103, .T. ) ;
#67977 = ORIENTED_EDGE ( 'NONE', *, *, #252174, .T. ) ;
#67979 = CIRCLE ( 'NONE', #242936, 0.09999999999998898659 ) ;
#67978 = DIRECTION ( 'NONE',  ( -1.000000000000000000, 0.000000000000000000, -0.000000000000000000 ) ) ;
#67980 = ORIENTED_EDGE ( 'NONE', *, *, #202167, .F. ) ;
#67981 = DIRECTION ( 'NONE',  ( -1.000000000000000000, -0.000000000000000000, -0.000000000000000000 ) ) ;
#67982 = EDGE_CURVE ( 'NONE', #78107, #228775, #82406, .T. ) ;
#67983 = ORIENTED_EDGE ( 'NONE', *, *, #187033, .T. ) ;
#67984 = DIRECTION ( 'NONE',  ( -1.000000000000000000, 0.000000000000000000, 0.000000000000000000 ) ) ;
#67985 = CARTESIAN_POINT ( 'NONE',  ( -23.25000000000000000, -1.164121893230052995, -141.9148480855716343 ) ) ;
#67986 = CIRCLE ( 'NONE', #63897, 0.09999999999999950595 ) ;
#67987 = EDGE_CURVE ( 'NONE', #118259, #133767, #43322, .T. ) ;
#67988 = CARTESIAN_POINT ( 'NONE',  ( -23.15000000000000213, 76.00000000001199396, -114.8231074845243000 ) ) ;
#67989 = ORIENTED_EDGE ( 'NONE', *, *, #62636, .F. ) ;
#67990 = EDGE_CURVE ( 'NONE', #233373, #244528, #128163, .T. ) ;
#67991 = DIRECTION ( 'NONE',  ( 0.000000000000000000, -0.2128009952263403282, 0.9770955615653358350 ) ) ;
#67992 = EDGE_CURVE ( 'NONE', #173202, #184295, #53145, .T. ) ;
#67993 = CARTESIAN_POINT ( 'NONE',  ( -21.05000000000000071, -0.09999999998884338825, -160.9593430482987344 ) ) ;
#67994 = VECTOR ( 'NONE', #162148, 1000.000000000000000 ) ;
#67996 = DIRECTION ( 'NONE',  ( 1.000000000000000000, -0.000000000000000000, 0.000000000000000000 ) ) ;
#67995 = CIRCLE ( 'NONE', #30601, 11.65000000000000036 ) ;
#67997 = DIRECTION ( 'NONE',  ( 1.000000000000000000, 0.000000000000000000, 0.000000000000000000 ) ) ;
#67999 = AXIS2_PLACEMENT_3D ( 'NONE', #26645, #47447, #229958 ) ;
#67998 = DIRECTION ( 'NONE',  ( -0.000000000000000000, -0.000000000000000000, 1.000000000000000000 ) ) ;
#68000 = CARTESIAN_POINT ( 'NONE',  ( 14.87567385445978196, 62.11595298889567118, -218.6870723643519341 ) ) ;
#68001 = EDGE_LOOP ( 'NONE', ( #28317, #58708, #116244, #112016 ) ) ;
#68003 = CARTESIAN_POINT ( 'NONE',  ( -22.43310005002225438, 75.99436305787187962, -215.1727696116587651 ) ) ;
#68002 = DIRECTION ( 'NONE',  ( 1.000000000000000000, -0.000000000000000000, 0.000000000000000000 ) ) ;
#68004 = EDGE_LOOP ( 'NONE', ( #17784, #194640, #143524, #117166, #244123 ) ) ;
#68006 = ORIENTED_EDGE ( 'NONE', *, *, #169123, .F. ) ;
#68005 = FACE_OUTER_BOUND ( 'NONE', #247383, .T. ) ;
#68007 = ORIENTED_EDGE ( 'NONE', *, *, #97295, .T. ) ;
#68008 = DIRECTION ( 'NONE',  ( 1.000000000000000000, 0.000000000000000000, 0.000000000000000000 ) ) ;
#68009 = LINE ( 'NONE', #6751, #217430 ) ;
#68010 = LINE ( 'NONE', #49731, #188995 ) ;
#68011 = AXIS2_PLACEMENT_3D ( 'NONE', #81923, #100216, #217600 ) ;
#68012 = CARTESIAN_POINT ( 'NONE',  ( -20.64999999999999858, 2.000000000011154189, -46.72462192276210402 ) ) ;
#68013 = EDGE_LOOP ( 'NONE', ( #18384, #218891, #133314, #101013 ) ) ;
#68014 = ADVANCED_FACE ( 'NONE', ( #148846 ), #5438, .T. ) ;
#68015 = CARTESIAN_POINT ( 'NONE',  ( 23.14999999999999858, 67.23127455305841238, -235.8551265064783991 ) ) ;
#68016 = CARTESIAN_POINT ( 'NONE',  ( 18.53691006697058796, 10.30215155716188669, -158.7021987172990976 ) ) ;
#68017 = TOROIDAL_SURFACE ( 'NONE', #238706, 0.9750000000000019762, 0.1000000000000000056 ) ;
#68018 = EDGE_LOOP ( 'NONE', ( #139301, #111534, #54242, #196431 ) ) ;
#68019 = AXIS2_PLACEMENT_3D ( 'NONE', #225822, #138891, #140192 ) ;
#68020 = CIRCLE ( 'NONE', #34718, 0.09999999999999939493 ) ;
#68021 = DIRECTION ( 'NONE',  ( 0.000000000000000000, 1.000000000000000000, 0.000000000000000000 ) ) ;
#68022 = AXIS2_PLACEMENT_3D ( 'NONE', #47714, #91985, #127271 ) ;
#68023 = ADVANCED_FACE ( 'NONE', ( #6749 ), #184100, .T. ) ;
#68024 = DIRECTION ( 'NONE',  ( 0.000000000000000000, 0.000000000000000000, 1.000000000000000000 ) ) ;
#68025 = ORIENTED_EDGE ( 'NONE', *, *, #35593, .T. ) ;
#68026 = FACE_OUTER_BOUND ( 'NONE', #81225, .T. ) ;
#68027 = VERTEX_POINT ( 'NONE', #186692 ) ;
#68028 = DIRECTION ( 'NONE',  ( -0.7071067811865456854, 0.7071067811865493491, 0.000000000000000000 ) ) ;
#68029 = ORIENTED_EDGE ( 'NONE', *, *, #248971, .F. ) ;
#68030 = CYLINDRICAL_SURFACE ( 'NONE', #71285, 0.09999999999999609201 ) ;
#68031 = EDGE_CURVE ( 'NONE', #226768, #77793, #127992, .T. ) ;
#68032 = CARTESIAN_POINT ( 'NONE',  ( 23.14999999999999858, 7.525330762710603416, -212.0571253909869256 ) ) ;
#68033 = CARTESIAN_POINT ( 'NONE',  ( 21.05000000000000071, 76.10000000001170406, -76.06376443622556849 ) ) ;
#68034 = DIRECTION ( 'NONE',  ( 2.952720810173289112E-16, 0.4088369013363388205, -0.9126074666063722640 ) ) ;
#68035 = AXIS2_PLACEMENT_3D ( 'NONE', #195864, #70786, #229827 ) ;
#68036 = DIRECTION ( 'NONE',  ( 0.000000000000000000, 0.000000000000000000, -1.000000000000000000 ) ) ;
#68038 = EDGE_CURVE ( 'NONE', #69280, #50336, #186439, .T. ) ;
#68037 = CARTESIAN_POINT ( 'NONE',  ( -20.00894256274684224, 4.611773101055291590, 22.11686199560476140 ) ) ;
#68039 = AXIS2_PLACEMENT_3D ( 'NONE', #27628, #32763, #150125 ) ;
#68040 = VERTEX_POINT ( 'NONE', #207537 ) ;
#68041 = CARTESIAN_POINT ( 'NONE',  ( -21.56666275994539816, 1.115600667400684642E-11, -26.54263159310667675 ) ) ;
#68042 = ORIENTED_EDGE ( 'NONE', *, *, #137577, .T. ) ;
#68045 =( BOUNDED_SURFACE ( )  B_SPLINE_SURFACE ( 3, 2, ( 
 ( #221383, #122310, #105268 ),
 ( #42771, #184837, #222670 ),
 ( #6198, #46596, #66185 ),
 ( #203123, #145703, #225229 ) ),
 .UNSPECIFIED., .F., .F., .T. ) 
 B_SPLINE_SURFACE_WITH_KNOTS ( ( 4, 4 ),
 ( 3, 3 ),
 ( 0.0006461284895273780972, 0.0007503702773985888950 ),
 ( 0.000000000000000000, 1.000000000000000000 ),
 .UNSPECIFIED. ) 
 GEOMETRIC_REPRESENTATION_ITEM ( )  RATIONAL_B_SPLINE_SURFACE ( (
 ( 1.000000000000000000, 0.7071067811865475727, 1.000000000000000000),
 ( 1.000000000000000000, 0.7076476444649381081, 1.000000000000000000),
 ( 1.000000000000000000, 0.7075727925191463985, 1.000000000000000000),
 ( 1.000000000000000000, 0.7071067811865475727, 1.000000000000000000) ) ) 
 REPRESENTATION_ITEM ( '' )  SURFACE ( )  );
#68044 = DIRECTION ( 'NONE',  ( 1.000000000000000000, 0.000000000000000000, 0.000000000000000000 ) ) ;
#68043 = FACE_OUTER_BOUND ( 'NONE', #172534, .T. ) ;
#68046 = ORIENTED_EDGE ( 'NONE', *, *, #93395, .F. ) ;
#68047 = CARTESIAN_POINT ( 'NONE',  ( 21.05000000000000071, 8.815452279208711772, -175.9203925526142314 ) ) ;
#68048 = AXIS2_PLACEMENT_3D ( 'NONE', #21327, #137378, #116551 ) ;
#68049 = DIRECTION ( 'NONE',  ( -1.000000000000000000, -0.000000000000000000, -0.000000000000000000 ) ) ;
#68050 = CIRCLE ( 'NONE', #143031, 0.09999999999998898659 ) ;
#68052 = ORIENTED_EDGE ( 'NONE', *, *, #187082, .F. ) ;
#68051 = CARTESIAN_POINT ( 'NONE',  ( 20.94999999999999929, 74.16465844978745281, -91.46795619196133487 ) ) ;
#68054 = ORIENTED_EDGE ( 'NONE', *, *, #13530, .T. ) ;
#68053 = LINE ( 'NONE', #165895, #174720 ) ;
#68055 = CARTESIAN_POINT ( 'NONE',  ( 23.14999999999999503, 11.75000000001116263, -79.15000000000004832 ) ) ;
#68056 = AXIS2_PLACEMENT_3D ( 'NONE', #258078, #22103, #217688 ) ;
#68057 = DIRECTION ( 'NONE',  ( 0.000000000000000000, 0.000000000000000000, -1.000000000000000000 ) ) ;
#68059 = ORIENTED_EDGE ( 'NONE', *, *, #102220, .T. ) ;
#68058 = CARTESIAN_POINT ( 'NONE',  ( 18.59999999999999076, 69.55000000001230376, -160.0060803140843859 ) ) ;
#68060 = AXIS2_PLACEMENT_3D ( 'NONE', #101798, #23621, #182673 ) ;
#68061 = AXIS2_PLACEMENT_3D ( 'NONE', #179747, #143153, #240998 ) ;
#68062 = VECTOR ( 'NONE', #208955, 1000.000000000000114 ) ;
#68063 = PRODUCT ( 'Snap Open Cable Crossbars 7', 'Snap Open Cable Crossbars 7', '', ( #215151 ) ) ;
#68064 = ORIENTED_EDGE ( 'NONE', *, *, #233482, .T. ) ;
#68065 = CIRCLE ( 'NONE', #197248, 12.97499999999999787 ) ;
#68066 = CARTESIAN_POINT ( 'NONE',  ( 18.59999999999999076, 69.55000000001187743, -93.00608031408432907 ) ) ;
#68067 = FACE_OUTER_BOUND ( 'NONE', #116134, .T. ) ;
#68068 = ORIENTED_EDGE ( 'NONE', *, *, #25286, .T. ) ;
#68069 = DIRECTION ( 'NONE',  ( -1.000000000000000000, -0.000000000000000000, -0.000000000000000000 ) ) ;
#68070 = ORIENTED_EDGE ( 'NONE', *, *, #196040, .T. ) ;
#68071 = SPHERICAL_SURFACE ( 'NONE', #111663, 0.1000000000000000056 ) ;
#68072 = CARTESIAN_POINT ( 'NONE',  ( 19.99999999737999090, 34.43872460993190288, -235.0322388072028161 ) ) ;
#68073 = VECTOR ( 'NONE', #168666, 1000.000000000000000 ) ;
#68074 = ORIENTED_EDGE ( 'NONE', *, *, #18641, .F. ) ;
#68075 = DIRECTION ( 'NONE',  ( -0.000000000000000000, -1.000000000000000000, -0.000000000000000000 ) ) ;
#68076 = EDGE_CURVE ( 'NONE', #116470, #37214, #15771, .T. ) ;
#68077 = CARTESIAN_POINT ( 'NONE',  ( -18.59999999999999787, 59.19392724319018129, -220.9828015967491126 ) ) ;
#68078 = VECTOR ( 'NONE', #86038, 1000.000000000000000 ) ;
#68079 = EDGE_LOOP ( 'NONE', ( #70848, #204287, #76907, #89130, #246456 ) ) ;
#68080 = CARTESIAN_POINT ( 'NONE',  ( -16.88005004766534967, 66.04989949669047178, -48.67277137257563879 ) ) ;
#68081 = AXIS2_PLACEMENT_3D ( 'NONE', #221387, #218827, #182300 ) ;
#68082 = AXIS2_PLACEMENT_3D ( 'NONE', #124114, #45842, #61562 ) ;
#68083 = CIRCLE ( 'NONE', #134708, 6.258578643762696458 ) ;
#68084 = ORIENTED_EDGE ( 'NONE', *, *, #216869, .T. ) ;
#68085 = CIRCLE ( 'NONE', #38881, 11.79999999999999716 ) ;
#68086 = ORIENTED_EDGE ( 'NONE', *, *, #27868, .F. ) ;
#68087 = ORIENTED_EDGE ( 'NONE', *, *, #114524, .F. ) ;
#68088 = EDGE_CURVE ( 'NONE', #248699, #217909, #84970, .T. ) ;
#68089 = DIRECTION ( 'NONE',  ( -0.000000000000000000, 0.9770955615653313941, 0.2128009952263603954 ) ) ;
#68090 = VERTEX_POINT ( 'NONE', #108426 ) ;
#68092 = ORIENTED_EDGE ( 'NONE', *, *, #161650, .T. ) ;
#68091 = FACE_OUTER_BOUND ( 'NONE', #99599, .T. ) ;
#68094 = ADVANCED_FACE ( 'NONE', ( #25061 ), #187966, .F. ) ;
#68093 = FACE_OUTER_BOUND ( 'NONE', #160250, .T. ) ;
#68095 = ORIENTED_EDGE ( 'NONE', *, *, #146925, .T. ) ;
#68096 = CARTESIAN_POINT ( 'NONE',  ( -18.59999999999999787, -1.835859311432481045, -179.0044391687985410 ) ) ;
#68097 = ORIENTED_EDGE ( 'NONE', *, *, #79443, .F. ) ;
#68100 = ORIENTED_EDGE ( 'NONE', *, *, #135245, .F. ) ;
#68099 = ORIENTED_EDGE ( 'NONE', *, *, #173235, .T. ) ;
#68098 = DIRECTION ( 'NONE',  ( -1.000000000000000000, 2.952720810173289112E-16, 2.061873921506763405E-30 ) ) ;
#68101 = DIRECTION ( 'NONE',  ( -1.000000000000000000, 0.000000000000000000, 0.000000000000000000 ) ) ;
#68102 = CARTESIAN_POINT ( 'NONE',  ( 23.15000000000000213, -11.64999999998883595, -97.40000000000004832 ) ) ;
#68105 = ADVANCED_FACE ( 'NONE', ( #88830 ), #228379, .T. ) ;
#68104 = ORIENTED_EDGE ( 'NONE', *, *, #169442, .F. ) ;
#68103 = VECTOR ( 'NONE', #117790, 1000.000000000000000 ) ;
#68106 = AXIS2_PLACEMENT_3D ( 'NONE', #88193, #7393, #89493 ) ;
#68107 = AXIS2_PLACEMENT_3D ( 'NONE', #181934, #78947, #80219 ) ;
#68108 = CIRCLE ( 'NONE', #188912, 0.5000000000000057732 ) ;
#68109 = EDGE_CURVE ( 'NONE', #29923, #255801, #178067, .T. ) ;
#68110 = ADVANCED_FACE ( 'NONE', ( #147549 ), #44605, .T. ) ;
#68111 = ORIENTED_EDGE ( 'NONE', *, *, #112067, .F. ) ;
#68112 = CARTESIAN_POINT ( 'NONE',  ( -21.55000000000000426, 7.750000000011159074, -121.6500000000000341 ) ) ;
#68113 = CARTESIAN_POINT ( 'NONE',  ( 23.14999999999999858, 1.115600667400684642E-11, -180.3749999999999716 ) ) ;
#68115 = ORIENTED_EDGE ( 'NONE', *, *, #105555, .T. ) ;
#68114 = PLANE ( 'NONE',  #203234 ) ;
#68116 = CARTESIAN_POINT ( 'NONE',  ( 18.54999999999999716, 8.750000000011182166, -146.6500000000000341 ) ) ;
#68117 = VERTEX_POINT ( 'NONE', #203671 ) ;
#68118 = EDGE_CURVE ( 'NONE', #91552, #196832, #190548, .T. ) ;
#68119 = DIRECTION ( 'NONE',  ( -1.000000000000000000, 0.000000000000000000, 0.000000000000000000 ) ) ;
#68120 = CARTESIAN_POINT ( 'NONE',  ( 18.49999999999999289, 65.65621891165885415, -111.6946622066469530 ) ) ;
#68121 = VERTEX_POINT ( 'NONE', #8050 ) ;
#68122 = CARTESIAN_POINT ( 'NONE',  ( 20.73486653747088937, 7.750000000011182166, -42.75000000000000000 ) ) ;
#68123 = CARTESIAN_POINT ( 'NONE',  ( -18.50000000000000000, 9.250000000011157297, -79.35000000000005116 ) ) ;
#68124 = ADVANCED_FACE ( 'NONE', ( #87553 ), #26327, .F. ) ;
#68125 = ORIENTED_EDGE ( 'NONE', *, *, #69466, .F. ) ;
#68127 = ORIENTED_EDGE ( 'NONE', *, *, #253642, .F. ) ;
#68126 = CARTESIAN_POINT ( 'NONE',  ( 19.97071067811865319, 54.36283943849028333, -228.7769250045207912 ) ) ;
#68128 = CARTESIAN_POINT ( 'NONE',  ( -15.55912972643741199, 67.50912972644901799, -56.97310748452438389 ) ) ;
#68130 = VERTEX_POINT ( 'NONE', #244069 ) ;
#68129 = ORIENTED_EDGE ( 'NONE', *, *, #93372, .T. ) ;
#68131 = VECTOR ( 'NONE', #240252, 1000.000000000000000 ) ;
#68132 = ORIENTED_EDGE ( 'NONE', *, *, #87850, .T. ) ;
#68133 = CYLINDRICAL_SURFACE ( 'NONE', #249089, 0.09999999999998304689 ) ;
#68134 = ORIENTED_EDGE ( 'NONE', *, *, #104928, .T. ) ;
#68135 = DIRECTION ( 'NONE',  ( -1.000000000000000000, -0.000000000000000000, -0.000000000000000000 ) ) ;
#68136 = ORIENTED_EDGE ( 'NONE', *, *, #102329, .F. ) ;
#68137 = DIRECTION ( 'NONE',  ( -0.000000000000000000, -6.982962677686266711E-15, 1.000000000000000000 ) ) ;
#68138 = CARTESIAN_POINT ( 'NONE',  ( -20.94999999999999929, 43.47002849391839874, -245.0086825852825143 ) ) ;
#68139 = EDGE_CURVE ( 'NONE', #111770, #7110, #57411, .T. ) ;
#68140 = ORIENTED_EDGE ( 'NONE', *, *, #4037, .T. ) ;
#68141 = ORIENTED_EDGE ( 'NONE', *, *, #130079, .F. ) ;
#68142 = AXIS2_PLACEMENT_3D ( 'NONE', #247001, #179672, #140513 ) ;
#68143 = ORIENTED_EDGE ( 'NONE', *, *, #201300, .T. ) ;
#68144 = VECTOR ( 'NONE', #62547, 1000.000000000000000 ) ;
#68145 = CIRCLE ( 'NONE', #213896, 0.09999999999999609201 ) ;
#68146 = EDGE_CURVE ( 'NONE', #25360, #172629, #49041, .T. ) ;
#68147 = DIRECTION ( 'NONE',  ( 0.000000000000000000, 0.000000000000000000, -1.000000000000000000 ) ) ;
#68148 = ORIENTED_EDGE ( 'NONE', *, *, #143841, .F. ) ;
#68149 = CARTESIAN_POINT ( 'NONE',  ( -20.54999999999999716, 1.115624548013267999E-11, -199.0999999999999375 ) ) ;
#68151 = ORIENTED_EDGE ( 'NONE', *, *, #242015, .T. ) ;
#68150 = LINE ( 'NONE', #171150, #170992 ) ;
#68152 = DIRECTION ( 'NONE',  ( 1.000000000000000000, -3.448943450116721102E-16, -6.438528483529607644E-16 ) ) ;
#68153 = DIRECTION ( 'NONE',  ( 1.000000000000000000, -2.952720810173289112E-16, -2.061873921506763405E-30 ) ) ;
#68154 = CARTESIAN_POINT ( 'NONE',  ( -21.45000000000000284, 7.708578643762696636, -12.34999999999999964 ) ) ;
#68155 = DIRECTION ( 'NONE',  ( -1.000000000000000000, 0.000000000000000000, -0.000000000000000000 ) ) ;
#68157 = DIRECTION ( 'NONE',  ( -1.000000000000000000, 0.000000000000000000, 0.000000000000000000 ) ) ;
#68156 = DIRECTION ( 'NONE',  ( -1.000000000000000000, 0.000000000000000000, 0.000000000000000000 ) ) ;
#68158 = CARTESIAN_POINT ( 'NONE',  ( -21.05000000000000071, -11.74999999998884448, -97.60000000000005116 ) ) ;
#68159 = CARTESIAN_POINT ( 'NONE',  ( 22.50000000000000000, 75.95437663941604001, -181.6736118230765271 ) ) ;
#68160 = AXIS2_PLACEMENT_3D ( 'NONE', #23808, #81160, #223240 ) ;
#68161 = DIRECTION ( 'NONE',  ( 0.000000000000000000, 0.2617529984164915779, 0.9651348961777187485 ) ) ;
#68162 = ADVANCED_FACE ( 'NONE', ( #206241 ), #246636, .F. ) ;
#68163 = CIRCLE ( 'NONE', #213909, 4.000000000000003553 ) ;
#68164 = EDGE_LOOP ( 'NONE', ( #174659, #40865, #237478, #170785 ) ) ;
#68165 = EDGE_CURVE ( 'NONE', #103588, #30076, #82335, .T. ) ;
#68166 = CIRCLE ( 'NONE', #206110, 11.64999999999999325 ) ;
#68167 = AXIS2_PLACEMENT_3D ( 'NONE', #245133, #209866, #108196 ) ;
#68168 = ORIENTED_EDGE ( 'NONE', *, *, #87150, .F. ) ;
#68170 = VERTEX_POINT ( 'NONE', #73180 ) ;
#68169 = DIRECTION ( 'NONE',  ( 1.000000000000000000, 0.000000000000000000, 0.000000000000000000 ) ) ;
#68171 = EDGE_LOOP ( 'NONE', ( #164877, #35807, #104910, #191729 ) ) ;
#68172 = CARTESIAN_POINT ( 'NONE',  ( -21.14999999999999858, 64.25000000001195133, -102.9231074845243938 ) ) ;
#68173 = EDGE_CURVE ( 'NONE', #12012, #191970, #140616, .T. ) ;
#68174 = CARTESIAN_POINT ( 'NONE',  ( 20.19326291201655721, 10.15606098791450229, -141.7618618076040775 ) ) ;
#68176 = DIRECTION ( 'NONE',  ( -0.000000000000000000, -0.000000000000000000, -1.000000000000000000 ) ) ;
#68175 = CARTESIAN_POINT ( 'NONE',  ( 20.21567752745038504, 39.68329723881405613, -237.0215815498126233 ) ) ;
#68177 = ORIENTED_EDGE ( 'NONE', *, *, #223809, .F. ) ;
#68178 = CIRCLE ( 'NONE', #126443, 0.8750000000000007772 ) ;
#68179 = ADVANCED_FACE ( 'NONE', ( #152718 ), #257299, .T. ) ;
#68180 = CIRCLE ( 'NONE', #134790, 0.5000000000000087708 ) ;
#68181 = EDGE_CURVE ( 'NONE', #159998, #32909, #174000, .T. ) ;
#68183 = CIRCLE ( 'NONE', #176355, 0.09999999999999939493 ) ;
#68182 = SPHERICAL_SURFACE ( 'NONE', #141700, 0.1000000000000000056 ) ;
#68184 = CARTESIAN_POINT ( 'NONE',  ( 21.13736287352038445, 67.95335762362751097, -48.67310748452438673 ) ) ;
#68185 = ORIENTED_EDGE ( 'NONE', *, *, #230207, .T. ) ;
#68186 = DIRECTION ( 'NONE',  ( 6.938893903907222067E-15, -1.000000000000000000, -0.000000000000000000 ) ) ;
#68187 = DIRECTION ( 'NONE',  ( 0.000000000000000000, 0.1575844902526769009, 0.9875055080513748251 ) ) ;
#68188 = DIRECTION ( 'NONE',  ( 0.000000000000000000, 1.000000000000000000, 0.000000000000000000 ) ) ;
#68189 = FACE_OUTER_BOUND ( 'NONE', #18730, .T. ) ;
#68190 = EDGE_CURVE ( 'NONE', #167556, #136922, #25858, .T. ) ;
#68191 = AXIS2_PLACEMENT_3D ( 'NONE', #166367, #148056, #8544 ) ;
#68192 = CARTESIAN_POINT ( 'NONE',  ( 23.14999999999999503, 6.650000000011155876, -79.25000000000004263 ) ) ;
#68194 = VERTEX_POINT ( 'NONE', #194402 ) ;
#68193 = CARTESIAN_POINT ( 'NONE',  ( -20.85000000000000142, 65.66751761918668251, -97.42826094061121012 ) ) ;
#68195 = DIRECTION ( 'NONE',  ( 0.000000000000000000, 0.000000000000000000, 1.000000000000000000 ) ) ;
#68196 = DIRECTION ( 'NONE',  ( -1.000000000000000000, -0.000000000000000000, -0.000000000000000000 ) ) ;
#68197 = TOROIDAL_SURFACE ( 'NONE', #18128, 0.2000000000000000111, 0.1000000000000000056 ) ;
#68198 = CARTESIAN_POINT ( 'NONE',  ( -18.59999999999999787, 76.00000000001142553, -36.02310748452432421 ) ) ;
#68199 = DIRECTION ( 'NONE',  ( 0.000000000000000000, -0.1298341882519953860, -0.9915357197604862671 ) ) ;
#68201 = VERTEX_POINT ( 'NONE', #32776 ) ;
#68200 = CIRCLE ( 'NONE', #142999, 0.09999999999999749367 ) ;
#68202 = CARTESIAN_POINT ( 'NONE',  ( -18.40000000000000213, 11.47867410001106236, -124.7253067836594340 ) ) ;
#68203 = CYLINDRICAL_SURFACE ( 'NONE', #165189, 0.1000000000000057648 ) ;
#68204 = AXIS2_PLACEMENT_3D ( 'NONE', #156514, #80763, #178637 ) ;
#68205 = DIRECTION ( 'NONE',  ( -0.000000000000000000, 0.9770955615653313941, 0.2128009952263603954 ) ) ;
#68206 = DIRECTION ( 'NONE',  ( 1.000000000000000000, 0.000000000000000000, 1.073024830501117725E-15 ) ) ;
#68207 = CARTESIAN_POINT ( 'NONE',  ( -16.87998658237740912, 9.950000000011138823, -54.13636043226178884 ) ) ;
#68208 = FACE_OUTER_BOUND ( 'NONE', #87782, .T. ) ;
#68209 = CARTESIAN_POINT ( 'NONE',  ( -16.80939487329394666, 66.05000000001153637, -48.67310748452351277 ) ) ;
#68210 = DIRECTION ( 'NONE',  ( 0.000000000000000000, 0.2617529984165152257, 0.9651348961777124202 ) ) ;
#68211 = DIRECTION ( 'NONE',  ( 0.000000000000000000, -0.2868887416115947775, 0.9579639084728169829 ) ) ;
#68212 = ORIENTED_EDGE ( 'NONE', *, *, #180707, .T. ) ;
#68213 = ORIENTED_EDGE ( 'NONE', *, *, #43838, .F. ) ;
#68214 = ORIENTED_EDGE ( 'NONE', *, *, #58772, .F. ) ;
#68215 = DIRECTION ( 'NONE',  ( -1.000000000000000000, 0.000000000000000000, 0.000000000000000000 ) ) ;
#68216 = FACE_OUTER_BOUND ( 'NONE', #156844, .T. ) ;
#68217 = EDGE_CURVE ( 'NONE', #143709, #190923, #123897, .T. ) ;
#68218 = ORIENTED_EDGE ( 'NONE', *, *, #203182, .F. ) ;
#68219 = EDGE_CURVE ( 'NONE', #194531, #235463, #2209, .T. ) ;
#68220 = ORIENTED_EDGE ( 'NONE', *, *, #30889, .F. ) ;
#68221 = CIRCLE ( 'NONE', #184723, 0.1000000000000002554 ) ;
#68222 = FILL_AREA_STYLE_COLOUR ( '', #19365 ) ;
#68223 = CIRCLE ( 'NONE', #226606, 0.09999999999999939493 ) ;
#68224 = ADVANCED_FACE ( 'NONE', ( #251780 ), #74469, .F. ) ;
#68225 = ORIENTED_EDGE ( 'NONE', *, *, #95201, .T. ) ;
#68226 = AXIS2_PLACEMENT_3D ( 'NONE', #254013, #157537, #54537 ) ;
#68227 = DIRECTION ( 'NONE',  ( 1.000000000000000000, 0.000000000000000000, 0.000000000000000000 ) ) ;
#68228 = VERTEX_POINT ( 'NONE', #31485 ) ;
#68229 = CARTESIAN_POINT ( 'NONE',  ( -16.93234230245722216, 30.28871318002137514, -234.7966014547397720 ) ) ;
#68230 = FACE_OUTER_BOUND ( 'NONE', #211456, .T. ) ;
#68231 = CARTESIAN_POINT ( 'NONE',  ( -21.08884785362073089, 1.548504767058726417, -230.6869963227249229 ) ) ;
#68232 = AXIS2_PLACEMENT_3D ( 'NONE', #242819, #122892, #144989 ) ;
#68233 = CIRCLE ( 'NONE', #234835, 0.09999999999999967248 ) ;
#68234 = CARTESIAN_POINT ( 'NONE',  ( 23.24999999999999289, 64.35000000001173248, -81.27310748452440237 ) ) ;
#68235 = DIRECTION ( 'NONE',  ( 0.000000000000000000, 3.469446951953515108E-14, 1.000000000000000000 ) ) ;
#68237 = ORIENTED_EDGE ( 'NONE', *, *, #37055, .F. ) ;
#68236 = DIRECTION ( 'NONE',  ( 0.000000000000000000, -1.734723475983309083E-15, 1.000000000000000000 ) ) ;
#68239 = DIRECTION ( 'NONE',  ( -0.000000000000000000, 0.9126074666063771490, 0.4088369013363281623 ) ) ;
#68238 = CARTESIAN_POINT ( 'NONE',  ( 23.14999999999999147, -4.149999999988843058, -67.00000000000004263 ) ) ;
#68240 = DIRECTION ( 'NONE',  ( -1.000000000000000000, -0.000000000000000000, -0.000000000000000000 ) ) ;
#68241 = VERTEX_POINT ( 'NONE', #15773 ) ;
#68242 = CARTESIAN_POINT ( 'NONE',  ( 20.85000000000000142, -1.736705739467587772, -45.01742258762372728 ) ) ;
#68243 = CIRCLE ( 'NONE', #213996, 2.000000000000003109 ) ;
#68244 = CARTESIAN_POINT ( 'NONE',  ( -20.54999999999999716, 76.00000000001170974, -69.52310748452431710 ) ) ;
#68245 = DIRECTION ( 'NONE',  ( -0.000000000000000000, -0.000000000000000000, 1.000000000000000000 ) ) ;
#68246 = ORIENTED_EDGE ( 'NONE', *, *, #21124, .T. ) ;
#68247 = VECTOR ( 'NONE', #106619, 1000.000000000000000 ) ;
#68248 = DIRECTION ( 'NONE',  ( -1.000000000000000000, 0.000000000000000000, -0.000000000000000000 ) ) ;
#68249 = AXIS2_PLACEMENT_3D ( 'NONE', #14117, #32408, #213570 ) ;
#68250 = VECTOR ( 'NONE', #75868, 1000.000000000000227 ) ;
#68251 = EDGE_CURVE ( 'NONE', #136580, #51183, #161494, .T. ) ;
#68252 = DIRECTION ( 'NONE',  ( 1.000000000000000000, 0.000000000000000000, 0.000000000000000000 ) ) ;
#68253 = ORIENTED_EDGE ( 'NONE', *, *, #103714, .F. ) ;
#68254 = AXIS2_PLACEMENT_3D ( 'NONE', #177168, #257897, #19347 ) ;
#68255 = DIRECTION ( 'NONE',  ( 0.000000000000000000, 6.982962677686266711E-15, -1.000000000000000000 ) ) ;
#68256 = LINE ( 'NONE', #124384, #145238 ) ;
#68257 = CARTESIAN_POINT ( 'NONE',  ( 22.59080734064467677, 64.25000000001165290, -69.55385719262146438 ) ) ;
#68258 = EDGE_CURVE ( 'NONE', #255984, #89858, #250487, .T. ) ;
#68259 = ORIENTED_EDGE ( 'NONE', *, *, #49658, .F. ) ;
#68260 = CIRCLE ( 'NONE', #130612, 0.1000000000000012546 ) ;
#68261 = ORIENTED_EDGE ( 'NONE', *, *, #133631, .F. ) ;
#68262 = EDGE_CURVE ( 'NONE', #143362, #112749, #154203, .T. ) ;
#68263 = CARTESIAN_POINT ( 'NONE',  ( 21.05000000000000071, 11.65000000001116298, -193.9851942293460070 ) ) ;
#68265 = AXIS2_PLACEMENT_3D ( 'NONE', #140594, #216278, #177199 ) ;
#68264 = DIRECTION ( 'NONE',  ( 1.000000000000000000, 2.885090398161910739E-16, 6.283419270304611573E-17 ) ) ;
#68266 = LINE ( 'NONE', #238897, #82718 ) ;
#68267 = CARTESIAN_POINT ( 'NONE',  ( -20.64999999999999858, -8.999999999988846255, -110.3939691226524786 ) ) ;
#68268 = EDGE_CURVE ( 'NONE', #173665, #19956, #150137, .T. ) ;
#68269 = LINE ( 'NONE', #227331, #190940 ) ;
#68270 = LINE ( 'NONE', #202960, #27395 ) ;
#68271 = CARTESIAN_POINT ( 'NONE',  ( 22.47071067811865319, 68.27992525551464098, -203.6221999392270448 ) ) ;
#68272 = AXIS2_PLACEMENT_3D ( 'NONE', #124585, #9753, #205371 ) ;
#68273 = EDGE_LOOP ( 'NONE', ( #170863, #224994, #194578, #88052 ) ) ;
#68274 = CARTESIAN_POINT ( 'NONE',  ( 15.74999999999999645, 9.850000000011137402, -50.24999999999999289 ) ) ;
#68275 = CIRCLE ( 'NONE', #9818, 0.1000000000000028644 ) ;
#68276 = EDGE_CURVE ( 'NONE', #221781, #246673, #220371, .T. ) ;
#68278 = ORIENTED_EDGE ( 'NONE', *, *, #170387, .F. ) ;
#68277 = DIRECTION ( 'NONE',  ( 1.000000000000000000, 0.000000000000000000, 0.000000000000000000 ) ) ;
#68279 = AXIS2_PLACEMENT_3D ( 'NONE', #200105, #25341, #21484 ) ;
#68280 = LINE ( 'NONE', #69573, #243396 ) ;
#68282 = ADVANCED_FACE ( 'NONE', ( #160415 ), #139524, .T. ) ;
#68281 = ADVANCED_FACE ( 'NONE', ( #97809 ), #2578, .T. ) ;
#68283 = LINE ( 'NONE', #162256, #136464 ) ;
#68284 = CARTESIAN_POINT ( 'NONE',  ( -20.64999999999999858, 71.65000000001253966, -182.2731074845243882 ) ) ;
#68285 = DIRECTION ( 'NONE',  ( 0.000000000000000000, 0.2617529984165152257, 0.9651348961777124202 ) ) ;
#68287 = ORIENTED_EDGE ( 'NONE', *, *, #183782, .F. ) ;
#68286 = DIRECTION ( 'NONE',  ( 0.000000000000000000, -6.608470384673580212E-15, 1.000000000000000000 ) ) ;
#68288 = CARTESIAN_POINT ( 'NONE',  ( 18.59999999999997655, 18.60970618848720903, -231.2322896185303875 ) ) ;
#68289 = CARTESIAN_POINT ( 'NONE',  ( -18.50016250449483479, 65.70233904877069619, -164.5487410911968595 ) ) ;
#68290 = FACE_OUTER_BOUND ( 'NONE', #53377, .T. ) ;
#68291 = CYLINDRICAL_SURFACE ( 'NONE', #36501, 0.5000000000000004441 ) ;
#68292 = ORIENTED_EDGE ( 'NONE', *, *, #26730, .F. ) ;
#68293 = CARTESIAN_POINT ( 'NONE',  ( 18.49713797159835948, -7.725302628690933204, -209.9197111851193256 ) ) ;
#68294 = CARTESIAN_POINT ( 'NONE',  ( -16.77431908686106610, 66.05419424549403118, -115.6872682668741277 ) ) ;
#68295 = VERTEX_POINT ( 'NONE', #22178 ) ;
#68296 = DIRECTION ( 'NONE',  ( 0.000000000000000000, -0.9908441862701600211, -0.1350103645451876666 ) ) ;
#68297 = CARTESIAN_POINT ( 'NONE',  ( -17.04295772865474490, 65.97510057475035694, -90.37310748452436826 ) ) ;
#68299 = EDGE_LOOP ( 'NONE', ( #184632, #65518, #88749 ) ) ;
#68298 = CIRCLE ( 'NONE', #76651, 0.09999999999999939493 ) ;
#68301 = ADVANCED_FACE ( 'NONE', ( #1290 ), #78264, .T. ) ;
#68300 = CIRCLE ( 'NONE', #101571, 0.8750000000000007772 ) ;
#68302 = AXIS2_PLACEMENT_3D ( 'NONE', #253498, #74905, #115279 ) ;
#68303 = EDGE_CURVE ( 'NONE', #115637, #168786, #239935, .T. ) ;
#68304 = ORIENTED_EDGE ( 'NONE', *, *, #24515, .F. ) ;
#68305 = LINE ( 'NONE', #231243, #214211 ) ;
#68306 = DIRECTION ( 'NONE',  ( 0.000000000000000000, -0.2617529984162567103, -0.9651348961777825863 ) ) ;
#68307 = EDGE_CURVE ( 'NONE', #95409, #54081, #178262, .T. ) ;
#68308 = CARTESIAN_POINT ( 'NONE',  ( 18.58685178364168777, -9.406733083793099581, -174.6244204690876813 ) ) ;
#68309 = ORIENTED_EDGE ( 'NONE', *, *, #45037, .T. ) ;
#68310 = DIRECTION ( 'NONE',  ( 0.000000000000000000, 0.9126074666063771490, 0.4088369013363278293 ) ) ;
#68311 = EDGE_CURVE ( 'NONE', #91860, #219191, #40479, .T. ) ;
#68312 = CARTESIAN_POINT ( 'NONE',  ( -23.25000000000000000, 11.75000000001115552, -67.00000000000000000 ) ) ;
#68313 = EDGE_CURVE ( 'NONE', #239914, #125623, #95018, .T. ) ;
#68314 = DIRECTION ( 'NONE',  ( 1.000000000000000000, 0.000000000000000000, 0.000000000000000000 ) ) ;
#68315 = CARTESIAN_POINT ( 'NONE',  ( 21.05000000000000071, 1.148907358139439339E-11, -201.0000000000015064 ) ) ;
#68316 = DIRECTION ( 'NONE',  ( 1.000000000000000000, 0.000000000000000000, 0.000000000000000000 ) ) ;
#68317 = VERTEX_POINT ( 'NONE', #178701 ) ;
#68319 = VERTEX_POINT ( 'NONE', #200798 ) ;
#68318 = DIRECTION ( 'NONE',  ( 0.000000000000000000, 0.000000000000000000, -1.000000000000000000 ) ) ;
#68320 = ORIENTED_EDGE ( 'NONE', *, *, #99999, .T. ) ;
#68321 = CIRCLE ( 'NONE', #209977, 0.09999999999998898659 ) ;
#68322 = DIRECTION ( 'NONE',  ( -1.646408749285562691E-14, 1.000000000000000000, 0.000000000000000000 ) ) ;
#68323 = ORIENTED_EDGE ( 'NONE', *, *, #97341, .T. ) ;
#68324 = CARTESIAN_POINT ( 'NONE',  ( -22.50000000000000000, 68.20922040163897293, -170.1231074845244109 ) ) ;
#68325 = DIRECTION ( 'NONE',  ( 0.000000000000000000, 0.000000000000000000, 1.000000000000000000 ) ) ;
#68326 = DIRECTION ( 'NONE',  ( -1.000000000000000000, -0.000000000000000000, -0.000000000000000000 ) ) ;
#68327 = ORIENTED_EDGE ( 'NONE', *, *, #74520, .F. ) ;
#68328 = EDGE_CURVE ( 'NONE', #118225, #69009, #99098, .T. ) ;
#68329 = CARTESIAN_POINT ( 'NONE',  ( 20.94999999999999929, 76.00000000001170974, -69.52310748452431710 ) ) ;
#68330 = CARTESIAN_POINT ( 'NONE',  ( -16.86379686415369150, 66.02478224075835556, -48.58971759543411650 ) ) ;
#68331 = CARTESIAN_POINT ( 'NONE',  ( 21.14999999999999858, 11.65000000000000746, -12.15000000000000036 ) ) ;
#68332 = ORIENTED_EDGE ( 'NONE', *, *, #94314, .F. ) ;
#68333 = LINE ( 'NONE', #212658, #29268 ) ;
#68335 = VERTEX_POINT ( 'NONE', #199535 ) ;
#68334 = DIRECTION ( 'NONE',  ( -1.000000000000000000, 0.000000000000000000, 0.000000000000000000 ) ) ;
#68336 = PLANE ( 'NONE',  #69233 ) ;
#68337 = B_SPLINE_CURVE_WITH_KNOTS ( 'NONE', 3,
 ( #198088, #76851, #37759, #175987, #218923, #254195, #1151, #156437, #215087, #118576, #19464, #36481, #235924, #138099 ),
 .UNSPECIFIED., .F., .F.,
 ( 4, 2, 2, 2, 2, 2, 4 ),
 ( 1.387778780781445676E-17, 0.0003823333598417824023, 0.0005735000397626774252, 0.0006690833797231165612, 0.0007168750497033334187, 0.0007407708846934392454, 0.0007646667196835449636 ),
 .UNSPECIFIED. ) ;
#68338 = CARTESIAN_POINT ( 'NONE',  ( 18.39999999999999503, 68.12577260125452483, -210.9717008331155341 ) ) ;
#68339 = EDGE_CURVE ( 'NONE', #113549, #223315, #157425, .T. ) ;
#68340 = VECTOR ( 'NONE', #194470, 1000.000000000000000 ) ;
#68341 = CIRCLE ( 'NONE', #193237, 2.000000000000003109 ) ;
#68342 = VERTEX_POINT ( 'NONE', #159129 ) ;
#68343 = AXIS2_PLACEMENT_3D ( 'NONE', #187852, #91304, #109558 ) ;
#68345 = CARTESIAN_POINT ( 'NONE',  ( 21.05000000000000071, 69.45934304831114048, -169.9231074845244223 ) ) ;
#68344 = CIRCLE ( 'NONE', #143342, 0.09999999999999721612 ) ;
#68346 = CARTESIAN_POINT ( 'NONE',  ( -15.15766958671843589, 66.58946139148316945, -121.0904194873834285 ) ) ;
#68347 = LINE ( 'NONE', #106154, #164235 ) ;
#68348 = VERTEX_POINT ( 'NONE', #221614 ) ;
#68349 = DIRECTION ( 'NONE',  ( 1.000000000000000000, 0.000000000000000000, 0.000000000000000000 ) ) ;
#68350 = EDGE_CURVE ( 'NONE', #77791, #34933, #18304, .T. ) ;
#68351 = DIRECTION ( 'NONE',  ( -1.000000000000000000, 0.000000000000000000, -0.000000000000000000 ) ) ;
#68352 = VERTEX_POINT ( 'NONE', #43014 ) ;
#68353 = AXIS2_PLACEMENT_3D ( 'NONE', #211400, #148872, #228407 ) ;
#68354 = AXIS2_PLACEMENT_3D ( 'NONE', #3456, #205508, #103828 ) ;
#68355 = CIRCLE ( 'NONE', #101627, 12.77500000000000924 ) ;
#68356 = ORIENTED_EDGE ( 'NONE', *, *, #154802, .F. ) ;
#68357 = CARTESIAN_POINT ( 'NONE',  ( 23.25000000000000000, 87.75000000001173817, -81.27310748452423184 ) ) ;
#68358 = AXIS2_PLACEMENT_3D ( 'NONE', #102396, #118145, #236794 ) ;
#68359 = AXIS2_PLACEMENT_3D ( 'NONE', #56083, #211340, #71847 ) ;
#68360 = ORIENTED_EDGE ( 'NONE', *, *, #126211, .F. ) ;
#68361 = FACE_OUTER_BOUND ( 'NONE', #33652, .T. ) ;
#68363 = VERTEX_POINT ( 'NONE', #238640 ) ;
#68362 = CARTESIAN_POINT ( 'NONE',  ( 12.93225390519044815, 25.11447974268060079, -232.6833957968051720 ) ) ;
#68364 = CARTESIAN_POINT ( 'NONE',  ( 20.87155475150661132, 11.75000000001115907, -127.0955865291576714 ) ) ;
#68365 = FACE_OUTER_BOUND ( 'NONE', #143521, .T. ) ;
#68366 = CARTESIAN_POINT ( 'NONE',  ( -23.25000000000000000, 2.600000000011156054, -80.22462192276213955 ) ) ;
#68367 = CARTESIAN_POINT ( 'NONE',  ( 18.59999999999999076, 11.65000000001115943, -91.85000000000003695 ) ) ;
#68368 = CARTESIAN_POINT ( 'NONE',  ( 21.04999999999998650, 9.104497675943859392, -211.5542940109215522 ) ) ;
#68369 = AXIS2_PLACEMENT_3D ( 'NONE', #223713, #103752, #26844 ) ;
#68370 = CARTESIAN_POINT ( 'NONE',  ( -17.11825945287482753, 10.05000000001113847, -79.65000000000004832 ) ) ;
#68371 = VECTOR ( 'NONE', #8373, 1000.000000000000114 ) ;
#68372 = DIRECTION ( 'NONE',  ( 1.000000000000000000, 0.000000000000000000, 0.000000000000000000 ) ) ;
#68374 = ORIENTED_EDGE ( 'NONE', *, *, #166826, .F. ) ;
#68373 = DIRECTION ( 'NONE',  ( 0.7071067811865474617, -0.7071067811865474617, -4.937700262164531476E-15 ) ) ;
#68376 = LINE ( 'NONE', #18340, #195594 ) ;
#68375 = AXIS2_PLACEMENT_3D ( 'NONE', #161694, #242481, #182539 ) ;
#68377 = ORIENTED_EDGE ( 'NONE', *, *, #23368, .T. ) ;
#68378 = AXIS2_PLACEMENT_3D ( 'NONE', #153090, #136018, #215575 ) ;
#68379 = CYLINDRICAL_SURFACE ( 'NONE', #80819, 7.900000000000003908 ) ;
#68380 = AXIS2_PLACEMENT_3D ( 'NONE', #11318, #242545, #52997 ) ;
#68381 = DIRECTION ( 'NONE',  ( -2.889348024582214003E-16, -0.1332476588733650935, -0.9910827722268042983 ) ) ;
#68382 = DIRECTION ( 'NONE',  ( 1.000000000000000000, -0.000000000000000000, -0.000000000000000000 ) ) ;
#68383 = DIRECTION ( 'NONE',  ( 0.000000000000000000, -1.000000000000000000, 0.000000000000000000 ) ) ;
#68384 = AXIS2_PLACEMENT_3D ( 'NONE', #154069, #57466, #194456 ) ;
#68386 = VERTEX_POINT ( 'NONE', #20903 ) ;
#68385 = CIRCLE ( 'NONE', #39191, 0.09999999999999080458 ) ;
#68388 = AXIS2_PLACEMENT_3D ( 'NONE', #169353, #208462, #130168 ) ;
#68387 = CARTESIAN_POINT ( 'NONE',  ( 21.05000000000000071, 10.30543449102040654, -228.0143625250146329 ) ) ;
#68389 = EDGE_CURVE ( 'NONE', #175979, #42715, #100381, .T. ) ;
#68390 = CARTESIAN_POINT ( 'NONE',  ( -21.07946286933444924, 6.329037319018851804, -100.4233161567436525 ) ) ;
#68391 = ORIENTED_EDGE ( 'NONE', *, *, #3417, .T. ) ;
#68392 = DIRECTION ( 'NONE',  ( -0.000000000000000000, -1.000000000000000000, 0.000000000000000000 ) ) ;
#68393 = DIRECTION ( 'NONE',  ( 0.000000000000000000, 0.1332476588733589040, -0.9910827722268049644 ) ) ;
#68394 = ORIENTED_EDGE ( 'NONE', *, *, #131031, .T. ) ;
#68395 = DIRECTION ( 'NONE',  ( 1.073024830501117725E-15, -0.2617529984165031243, -0.9651348961777157509 ) ) ;
#68396 = ORIENTED_EDGE ( 'NONE', *, *, #46126, .T. ) ;
#68397 = DIRECTION ( 'NONE',  ( -0.000000000000000000, -0.000000000000000000, 1.000000000000000000 ) ) ;
#68398 = ORIENTED_EDGE ( 'NONE', *, *, #20605, .F. ) ;
#68400 = ADVANCED_FACE ( 'NONE', ( #176122 ), #255578, .T. ) ;
#68399 = CARTESIAN_POINT ( 'NONE',  ( 21.14999999999999858, 69.45000000001157048, -57.37310748452436115 ) ) ;
#68401 = CARTESIAN_POINT ( 'NONE',  ( -18.40000000000000213, 11.47316190337364183, -124.7500000000000426 ) ) ;
#68402 = ORIENTED_EDGE ( 'NONE', *, *, #124887, .T. ) ;
#68403 = CIRCLE ( 'NONE', #243367, 0.2000000000000057288 ) ;
#68404 = ORIENTED_EDGE ( 'NONE', *, *, #182471, .T. ) ;
#68405 = DIRECTION ( 'NONE',  ( 0.000000000000000000, -0.1350103645451945777, 0.9908441862701590219 ) ) ;
#68407 = ORIENTED_EDGE ( 'NONE', *, *, #186631, .F. ) ;
#68406 = FILL_AREA_STYLE_COLOUR ( '', #47426 ) ;
#68408 = AXIS2_PLACEMENT_3D ( 'NONE', #153379, #17657, #234143 ) ;
#68409 = CARTESIAN_POINT ( 'NONE',  ( -18.39999999999999858, 86.99291436658650412, -199.6658631664729739 ) ) ;
#68410 = EDGE_LOOP ( 'NONE', ( #35442, #13271, #186068, #246965, #178831, #167803, #193213 ) ) ;
#68411 = AXIS2_PLACEMENT_3D ( 'NONE', #225495, #245088, #186417 ) ;
#68412 = ADVANCED_FACE ( 'NONE', ( #177412 ), #256859, .T. ) ;
#68413 = ADVANCED_FACE ( 'NONE', ( #58690 ), #138229, .T. ) ;
#68414 = VERTEX_POINT ( 'NONE', #125126 ) ;
#68415 = LINE ( 'NONE', #111396, #41045 ) ;
#68416 = DIRECTION ( 'NONE',  ( 0.000000000000000000, -6.853228547068871147E-15, 1.000000000000000000 ) ) ;
#68417 =( BOUNDED_SURFACE ( )  B_SPLINE_SURFACE ( 3, 2, ( 
 ( #87455, #246536, #105717 ),
 ( #225665, #65334, #5333 ),
 ( #130444, #47037, #165748 ),
 ( #148743, #10514, #88729 ) ),
 .UNSPECIFIED., .F., .F., .F. ) 
 B_SPLINE_SURFACE_WITH_KNOTS ( ( 4, 4 ),
 ( 3, 3 ),
 ( -5.204170427930421283E-18, 0.001979672783031532438 ),
 ( 0.000000000000000000, 1.000000000000000000 ),
 .UNSPECIFIED. ) 
 GEOMETRIC_REPRESENTATION_ITEM ( )  RATIONAL_B_SPLINE_SURFACE ( (
 ( 1.000000000000000000, 0.7103081912007900289, 1.000000000000000000),
 ( 1.000000000000000000, 0.7104998333560322843, 1.000000000000000000),
 ( 1.000000000000000000, 0.7107238315753141578, 1.000000000000000000),
 ( 1.000000000000000000, 0.7110073749539798094, 1.000000000000000000) ) ) 
 REPRESENTATION_ITEM ( '' )  SURFACE ( )  );
#68418 = DIRECTION ( 'NONE',  ( -1.000000000000000000, 0.000000000000000000, 0.000000000000000000 ) ) ;
#68419 = TOROIDAL_SURFACE ( 'NONE', #155924, 11.89999999999999858, 0.1000000000000000056 ) ;
#68420 = EDGE_CURVE ( 'NONE', #181065, #103372, #106814, .T. ) ;
#68421 = DIRECTION ( 'NONE',  ( -1.000000000000000000, -0.000000000000000000, -0.000000000000000000 ) ) ;
#68422 = DIRECTION ( 'NONE',  ( 0.000000000000000000, 0.000000000000000000, 1.000000000000000000 ) ) ;
#68423 = CARTESIAN_POINT ( 'NONE',  ( -20.94999999999999929, 1.115600667400684642E-11, -167.5000000000000284 ) ) ;
#68424 = CIRCLE ( 'NONE', #76791, 0.1000000000000028644 ) ;
#68425 = ORIENTED_EDGE ( 'NONE', *, *, #215547, .F. ) ;
#68426 = DIRECTION ( 'NONE',  ( 0.000000000000000000, 0.000000000000000000, -1.000000000000000000 ) ) ;
#68427 = AXIS2_PLACEMENT_3D ( 'NONE', #148153, #9931, #227684 ) ;
#68428 = DIRECTION ( 'NONE',  ( 0.000000000000000000, -0.9908441862701791170, 0.1350103645450472789 ) ) ;
#68429 = FACE_OUTER_BOUND ( 'NONE', #116846, .T. ) ;
#68430 = EDGE_CURVE ( 'NONE', #241914, #21212, #48131, .T. ) ;
#68431 = CARTESIAN_POINT ( 'NONE',  ( 21.00000000000000000, 22.61918030723622408, -230.9697045991730988 ) ) ;
#68432 = ORIENTED_EDGE ( 'NONE', *, *, #3016, .F. ) ;
#68433 = CARTESIAN_POINT ( 'NONE',  ( 22.49999999999999645, 0.1000000000111554016, -55.35042919245523763 ) ) ;
#68434 = ORIENTED_EDGE ( 'NONE', *, *, #257363, .F. ) ;
#68435 = CARTESIAN_POINT ( 'NONE',  ( 15.52844286134407881, 9.375669526436931633, -116.3677900093859705 ) ) ;
#68437 = VERTEX_POINT ( 'NONE', #102957 ) ;
#68436 = AXIS2_PLACEMENT_3D ( 'NONE', #170457, #154721, #213366 ) ;
#68438 = ADVANCED_FACE ( 'NONE', ( #165534 ), #247622, .F. ) ;
#68439 =( BOUNDED_CURVE ( )  B_SPLINE_CURVE ( 3, ( #43078, #242548, #220437, #41814 ),
 .UNSPECIFIED., .F., .F. ) 
 B_SPLINE_CURVE_WITH_KNOTS ( ( 4, 4 ),
 ( 4.712388980384690562, 6.283185307179586232 ),
 .UNSPECIFIED. ) 
 CURVE ( )  GEOMETRIC_REPRESENTATION_ITEM ( )  RATIONAL_B_SPLINE_CURVE ( ( 1.000000000000000000, 0.8047378541243652705, 0.8047378541243652705, 1.000000000000000000 ) ) 
 REPRESENTATION_ITEM ( '' )  );
#68440 = CARTESIAN_POINT ( 'NONE',  ( -14.87779219673428877, 25.00864058361856479, -232.6119739634630150 ) ) ;
#68441 = CARTESIAN_POINT ( 'NONE',  ( -20.85000000000000142, 31.11065811373596190, -259.9087319612273177 ) ) ;
#68442 = VERTEX_POINT ( 'NONE', #144657 ) ;
#68443 = VERTEX_POINT ( 'NONE', #207229 ) ;
#68445 = VERTEX_POINT ( 'NONE', #49424 ) ;
#68444 = DIRECTION ( 'NONE',  ( -1.000000000000000000, 2.952720810173289112E-16, 2.061873921506763405E-30 ) ) ;
#68446 = LINE ( 'NONE', #33208, #4278 ) ;
#68447 = EDGE_LOOP ( 'NONE', ( #3204, #166063, #33870, #164012 ) ) ;
#68448 = AXIS2_PLACEMENT_3D ( 'NONE', #19519, #80740, #82007 ) ;
#68449 = CARTESIAN_POINT ( 'NONE',  ( -22.47120815636973745, 0.02890382191504723558, -21.85006801124650266 ) ) ;
#68450 = DIRECTION ( 'NONE',  ( 0.000000000000000000, -0.9770955615653551529, -0.2128009952262517601 ) ) ;
#68451 = EDGE_CURVE ( 'NONE', #61365, #121084, #39189, .T. ) ;
#68452 = ORIENTED_EDGE ( 'NONE', *, *, #235951, .T. ) ;
#68453 = AXIS2_PLACEMENT_3D ( 'NONE', #187451, #127462, #148313 ) ;
#68454 = CARTESIAN_POINT ( 'NONE',  ( -23.15000000000000213, 11.75000000001115552, -188.8499999999999659 ) ) ;
#68456 = VERTEX_POINT ( 'NONE', #162972 ) ;
#68455 = CIRCLE ( 'NONE', #93381, 0.1000000000000046685 ) ;
#68457 =( BOUNDED_SURFACE ( )  B_SPLINE_SURFACE ( 3, 2, ( 
 ( #195226, #56929, #238157 ),
 ( #38696, #175646, #216025 ),
 ( #219887, #41289, #37423 ),
 ( #136478, #120820, #21702 ) ),
 .UNSPECIFIED., .F., .F., .F. ) 
 B_SPLINE_SURFACE_WITH_KNOTS ( ( 4, 4 ),
 ( 3, 3 ),
 ( 2.081668171172168513E-17, 0.001979672783031568434 ),
 ( 0.000000000000000000, 1.000000000000000000 ),
 .UNSPECIFIED. ) 
 GEOMETRIC_REPRESENTATION_ITEM ( )  RATIONAL_B_SPLINE_SURFACE ( (
 ( 1.000000000000000000, 0.7103081912007698229, 1.000000000000000000),
 ( 1.000000000000000000, 0.7104998333559727763, 1.000000000000000000),
 ( 1.000000000000000000, 0.7107238315755050051, 1.000000000000000000),
 ( 1.000000000000000000, 0.7110073749539208565, 1.000000000000000000) ) ) 
 REPRESENTATION_ITEM ( '' )  SURFACE ( )  );
#68458 = VECTOR ( 'NONE', #134464, 1000.000000000000000 ) ;
#68459 = B_SPLINE_CURVE_WITH_KNOTS ( 'NONE', 3,
 ( #10252, #246290, #66365, #25962, #87185, #229298, #48077, #28573 ),
 .UNSPECIFIED., .F., .F.,
 ( 4, 2, 2, 4 ),
 ( 0.000000000000000000, 6.534141206310559820E-05, 0.0001306828241262111964, 0.0002613656482524725371 ),
 .UNSPECIFIED. ) ;
#68460 = AXIS2_PLACEMENT_3D ( 'NONE', #105798, #180246, #45856 ) ;
#68461 = DIRECTION ( 'NONE',  ( -0.000000000000000000, -0.8660254037844411501, -0.4999999999999956701 ) ) ;
#68462 = DIRECTION ( 'NONE',  ( 0.000000000000000000, -0.9889818879709272315, -0.1480365673253073999 ) ) ;
#68463 = CARTESIAN_POINT ( 'NONE',  ( -23.25000000000000000, 46.01276039807270024, -256.6622985126337539 ) ) ;
#68465 = ORIENTED_EDGE ( 'NONE', *, *, #42190, .F. ) ;
#68464 = CARTESIAN_POINT ( 'NONE',  ( 22.94999999999999929, 4.837354856632045057E-16, 3.900000000000000355 ) ) ;
#68466 = CARTESIAN_POINT ( 'NONE',  ( 23.24999999999999645, 5.650000000011139001, -146.6500000000000341 ) ) ;
#68467 = CARTESIAN_POINT ( 'NONE',  ( -22.59999999999999787, 11.74956712350054744, -133.8991416309013118 ) ) ;
#68468 = CYLINDRICAL_SURFACE ( 'NONE', #27702, 0.5000000000000022204 ) ;
#68470 = CARTESIAN_POINT ( 'NONE',  ( -5.900000000000003020, -11.65000000000000036, 10.00000000000000178 ) ) ;
#68469 = CARTESIAN_POINT ( 'NONE',  ( -20.85000000000000142, 11.65000000001115232, -134.0000000000000284 ) ) ;
#68471 = CARTESIAN_POINT ( 'NONE',  ( -20.91682497891422798, 65.67736539654997330, -164.4625116876572406 ) ) ;
#68472 = LINE ( 'NONE', #253507, #65385 ) ;
#68473 = PLANE ( 'NONE',  #164143 ) ;
#68474 = DIRECTION ( 'NONE',  ( 0.000000000000000000, 1.000000000000000000, 0.000000000000000000 ) ) ;
#68475 = AXIS2_PLACEMENT_3D ( 'NONE', #1739, #205073, #46011 ) ;
#68476 = ORIENTED_EDGE ( 'NONE', *, *, #166418, .T. ) ;
#68477 = EDGE_CURVE ( 'NONE', #74533, #127058, #194998, .T. ) ;
#68478 = ORIENTED_EDGE ( 'NONE', *, *, #78632, .F. ) ;
#68479 = CIRCLE ( 'NONE', #189295, 0.09999999999998898659 ) ;
#68480 = ORIENTED_EDGE ( 'NONE', *, *, #19887, .T. ) ;
#68481 = ADVANCED_FACE ( 'NONE', ( #88522 ), #108118, .F. ) ;
#68482 = EDGE_CURVE ( 'NONE', #189704, #99810, #24758, .T. ) ;
#68483 = CARTESIAN_POINT ( 'NONE',  ( -20.99749315643149927, 64.25000000001220712, -143.5379132532823974 ) ) ;
#68484 = CARTESIAN_POINT ( 'NONE',  ( -16.87331047859651179, 60.93935776605891164, -221.0417277355860790 ) ) ;
#68485 = ORIENTED_EDGE ( 'NONE', *, *, #115307, .T. ) ;
#68486 = EDGE_CURVE ( 'NONE', #40333, #65719, #199080, .T. ) ;
#68487 = LINE ( 'NONE', #209267, #90712 ) ;
#68488 = CARTESIAN_POINT ( 'NONE',  ( 23.24999999999997513, 64.35000000001249987, -177.0379132551783812 ) ) ;
#68489 = EDGE_CURVE ( 'NONE', #255081, #9432, #7740, .T. ) ;
#68490 = ORIENTED_EDGE ( 'NONE', *, *, #135584, .F. ) ;
#68491 = EDGE_CURVE ( 'NONE', #144504, #257922, #52481, .T. ) ;
#68492 = VERTEX_POINT ( 'NONE', #242476 ) ;
#68493 = CARTESIAN_POINT ( 'NONE',  ( -16.86379686415369861, 9.975217759264314310, -46.06661011090972124 ) ) ;
#68494 = LINE ( 'NONE', #72360, #21943 ) ;
#68495 = ORIENTED_EDGE ( 'NONE', *, *, #106225, .F. ) ;
#68496 = EDGE_CURVE ( 'NONE', #29575, #196694, #144894, .T. ) ;
#68497 = DIRECTION ( 'NONE',  ( 0.000000000000000000, -0.2128009952263650861, 0.9770955615653305060 ) ) ;
#68499 = EDGE_LOOP ( 'NONE', ( #219786, #146212, #4461, #179965 ) ) ;
#68498 = DIRECTION ( 'NONE',  ( -1.000000000000000000, -0.000000000000000000, -0.000000000000000000 ) ) ;
#68500 = CARTESIAN_POINT ( 'NONE',  ( -20.64999999999999858, 68.85000000001228670, -157.7731074845244166 ) ) ;
#68501 = DIRECTION ( 'NONE',  ( 1.000000000000000000, 0.000000000000000000, -0.000000000000000000 ) ) ;
#68503 = ORIENTED_EDGE ( 'NONE', *, *, #238983, .T. ) ;
#68502 = PLANE ( 'NONE',  #56343 ) ;
#68505 = EDGE_CURVE ( 'NONE', #199664, #19568, #124081, .T. ) ;
#68504 = CARTESIAN_POINT ( 'NONE',  ( -18.57399277249657032, 10.33112638556969465, -72.59012289269747953 ) ) ;
#68506 = CARTESIAN_POINT ( 'NONE',  ( -17.11825945287482753, 9.950000000011138823, -46.25000000000000711 ) ) ;
#68507 = DIRECTION ( 'NONE',  ( 0.000000000000000000, -7.086529944415894657E-15, 1.000000000000000000 ) ) ;
#68508 = CARTESIAN_POINT ( 'NONE',  ( -16.81744102076749314, 9.950000000011142376, -113.1500000000000341 ) ) ;
#68510 = CARTESIAN_POINT ( 'NONE',  ( 20.59588692710267921, 10.36872342117990975, -108.1390810945106864 ) ) ;
#68509 = DIRECTION ( 'NONE',  ( 0.000000000000000000, 0.000000000000000000, 1.000000000000000000 ) ) ;
#68511 = CARTESIAN_POINT ( 'NONE',  ( -20.85000000000000142, 87.65000000001172964, -72.42310748452422331 ) ) ;
#68512 = ADVANCED_FACE ( 'NONE', ( #104238 ), #44959, .F. ) ;
#68513 = AXIS2_PLACEMENT_3D ( 'NONE', #160168, #24499, #121044 ) ;
#68514 = DIRECTION ( 'NONE',  ( 0.000000000000000000, 0.000000000000000000, 1.000000000000000000 ) ) ;
#68515 = CIRCLE ( 'NONE', #81150, 0.1000000000000028644 ) ;
#68516 = DIRECTION ( 'NONE',  ( 0.000000000000000000, 6.467318590049456648E-15, -1.000000000000000000 ) ) ;
#68517 = CARTESIAN_POINT ( 'NONE',  ( -20.94999999999999929, 76.25610579210386675, -69.55800392619661920 ) ) ;
#68518 = ORIENTED_EDGE ( 'NONE', *, *, #157408, .F. ) ;
#68519 = AXIS2_PLACEMENT_3D ( 'NONE', #118583, #198097, #2450 ) ;
#68520 = ORIENTED_EDGE ( 'NONE', *, *, #233015, .T. ) ;
#68521 = VECTOR ( 'NONE', #59301, 1000.000000000000000 ) ;
#68522 = EDGE_CURVE ( 'NONE', #241304, #135375, #147234, .T. ) ;
#68523 = FACE_OUTER_BOUND ( 'NONE', #69345, .T. ) ;
#68524 = VERTEX_POINT ( 'NONE', #14174 ) ;
#68525 = PLANE ( 'NONE',  #239477 ) ;
#68526 = ORIENTED_EDGE ( 'NONE', *, *, #70853, .F. ) ;
#68527 = CARTESIAN_POINT ( 'NONE',  ( 21.14999999999999858, -11.74999999998884448, -79.25000000000004263 ) ) ;
#68528 = ADVANCED_FACE ( 'NONE', ( #230639 ), #74154, .F. ) ;
#68529 = EDGE_CURVE ( 'NONE', #31563, #229898, #40891, .T. ) ;
#68530 = ORIENTED_EDGE ( 'NONE', *, *, #254250, .F. ) ;
#68531 = VECTOR ( 'NONE', #151125, 1000.000000000000000 ) ;
#68532 = FACE_BOUND ( 'NONE', #169258, .T. ) ;
#68533 = SURFACE_STYLE_USAGE ( .BOTH. , #8555 ) ;
#68534 = AXIS2_PLACEMENT_3D ( 'NONE', #79368, #88342, #68825 ) ;
#68535 = ORIENTED_EDGE ( 'NONE', *, *, #245769, .T. ) ;
#68536 = ORIENTED_EDGE ( 'NONE', *, *, #123236, .F. ) ;
#68537 = AXIS2_PLACEMENT_3D ( 'NONE', #236734, #78928, #176797 ) ;
#68538 = VERTEX_POINT ( 'NONE', #234463 ) ;
#68539 = VECTOR ( 'NONE', #89278, 1000.000000000000000 ) ;
#68540 = CARTESIAN_POINT ( 'NONE',  ( 18.39999999999999858, 85.60000000001160458, -62.49103808782458458 ) ) ;
#68541 = VECTOR ( 'NONE', #40438, 1000.000000000000000 ) ;
#68542 = CARTESIAN_POINT ( 'NONE',  ( 20.94999999999999929, 36.65892442174935439, -249.5511627012433848 ) ) ;
#68543 = CARTESIAN_POINT ( 'NONE',  ( 23.14999999999999858, 5.000000000011153745, -155.0947339810869323 ) ) ;
#68545 = CARTESIAN_POINT ( 'NONE',  ( 18.60000000000000853, 85.36423601037941467, -196.3428530837996959 ) ) ;
#68544 = DIRECTION ( 'NONE',  ( 0.000000000000000000, -1.000000000000000000, -7.109473446599835262E-15 ) ) ;
#68546 = FACE_OUTER_BOUND ( 'NONE', #93940, .T. ) ;
#68548 = ORIENTED_EDGE ( 'NONE', *, *, #227211, .T. ) ;
#68547 = CARTESIAN_POINT ( 'NONE',  ( 23.24999999999999289, 69.35000000001259934, -191.3731074845244109 ) ) ;
#68550 = CARTESIAN_POINT ( 'NONE',  ( -22.59080734064477625, 11.75000000001115907, -100.4692502919030090 ) ) ;
#68549 = CARTESIAN_POINT ( 'NONE',  ( 20.44999100639894962, 10.43971070322319683, -74.75907572597057538 ) ) ;
#68551 = LINE ( 'NONE', #43852, #73928 ) ;
#68552 = EDGE_LOOP ( 'NONE', ( #93677, #70720, #40227, #120780, #170086, #40062, #86975 ) ) ;
#68553 = FACE_OUTER_BOUND ( 'NONE', #100504, .T. ) ;
#68554 = AXIS2_PLACEMENT_3D ( 'NONE', #134044, #192761, #213585 ) ;
#68556 = AXIS2_PLACEMENT_3D ( 'NONE', #57617, #56328, #180166 ) ;
#68555 = CARTESIAN_POINT ( 'NONE',  ( 22.48660254037843131, 64.25000000001193712, -103.0731074845243853 ) ) ;
#68557 = DIRECTION ( 'NONE',  ( 0.000000000000000000, -0.4088369013363280513, 0.9126074666063769270 ) ) ;
#68558 = VECTOR ( 'NONE', #254004, 1000.000000000000000 ) ;
#68559 = ORIENTED_EDGE ( 'NONE', *, *, #77297, .F. ) ;
#68560 = CARTESIAN_POINT ( 'NONE',  ( 21.97500000000000497, 9.750000000011153745, -121.6500000000000341 ) ) ;
#68561 = CIRCLE ( 'NONE', #243328, 0.1999999999999996503 ) ;
#68562 = FACE_OUTER_BOUND ( 'NONE', #218551, .T. ) ;
#68563 = CYLINDRICAL_SURFACE ( 'NONE', #159340, 0.09999999999999641120 ) ;
#68564 = EDGE_LOOP ( 'NONE', ( #239455, #138357, #207371, #38408 ) ) ;
#68565 = ORIENTED_EDGE ( 'NONE', *, *, #113471, .T. ) ;
#68566 = AXIS2_PLACEMENT_3D ( 'NONE', #95966, #252473, #254987 ) ;
#68567 = DIRECTION ( 'NONE',  ( -0.000000000000000000, 0.4721928772777343464, 0.8814952561688431665 ) ) ;
#68568 = CARTESIAN_POINT ( 'NONE',  ( -16.91256925476571737, 66.01426884188410327, -157.4907499735297449 ) ) ;
#68569 = DIRECTION ( 'NONE',  ( 1.000000000000000000, 0.000000000000000000, 0.000000000000000000 ) ) ;
#68570 = FACE_OUTER_BOUND ( 'NONE', #8714, .T. ) ;
#68571 = VERTEX_POINT ( 'NONE', #131523 ) ;
#68572 = CIRCLE ( 'NONE', #1903, 0.09999999999999939493 ) ;
#68573 = AXIS2_PLACEMENT_3D ( 'NONE', #173600, #135678, #215238 ) ;
#68574 = DIRECTION ( 'NONE',  ( 0.000000000000000000, 0.000000000000000000, -1.000000000000000000 ) ) ;
#68575 = EDGE_CURVE ( 'NONE', #180198, #182048, #165785, .T. ) ;
#68576 = DIRECTION ( 'NONE',  ( 0.000000000000000000, 0.000000000000000000, 1.000000000000000000 ) ) ;
#68577 = CARTESIAN_POINT ( 'NONE',  ( 21.17356465864818205, 0.09891124102502621418, -127.5771968737582966 ) ) ;
#68578 = DIRECTION ( 'NONE',  ( 1.000000000000000000, -2.952720810173289112E-16, -2.061873921506763405E-30 ) ) ;
#68579 = EDGE_CURVE ( 'NONE', #112587, #77509, #153322, .T. ) ;
#68580 = VERTEX_POINT ( 'NONE', #191532 ) ;
#68581 = CARTESIAN_POINT ( 'NONE',  ( 20.94999999999999929, 67.23127455305835554, -235.8551265064784559 ) ) ;
#68582 = EDGE_CURVE ( 'NONE', #112216, #130629, #74220, .T. ) ;
#68584 = ORIENTED_EDGE ( 'NONE', *, *, #43789, .F. ) ;
#68583 = DIRECTION ( 'NONE',  ( 1.000000000000000000, 0.000000000000000000, 0.000000000000000000 ) ) ;
#68585 = EDGE_CURVE ( 'NONE', #203688, #37447, #28423, .T. ) ;
#68586 = LINE ( 'NONE', #245940, #86951 ) ;
#68587 = CARTESIAN_POINT ( 'NONE',  ( -21.14999999999999858, -11.74999999998884448, -103.4000000000000341 ) ) ;
#68588 = CARTESIAN_POINT ( 'NONE',  ( 18.59999999999999787, -1.835859311432481045, -145.5044391687985694 ) ) ;
#68589 = DIRECTION ( 'NONE',  ( 0.000000000000000000, 0.000000000000000000, -1.000000000000000000 ) ) ;
#68590 = CARTESIAN_POINT ( 'NONE',  ( -23.25000000000000000, 1.115600667400684642E-11, -100.5000000000000284 ) ) ;
#68591 = CARTESIAN_POINT ( 'NONE',  ( -18.59999999999999787, 64.35000000001234355, -163.0083017138704236 ) ) ;
#68592 = CARTESIAN_POINT ( 'NONE',  ( 18.59999999999999076, 51.96945017402672562, -231.5060697639786440 ) ) ;
#68593 = EDGE_LOOP ( 'NONE', ( #41165, #251651, #82809, #191334 ) ) ;
#68594 = CARTESIAN_POINT ( 'NONE',  ( 18.79999999999999716, 4.513204987021263825, 22.00000000000000355 ) ) ;
#68595 = VECTOR ( 'NONE', #66416, 1000.000000000000114 ) ;
#68596 = DIRECTION ( 'NONE',  ( -1.000000000000000000, -0.000000000000000000, -0.000000000000000000 ) ) ;
#68597 = B_SPLINE_CURVE_WITH_KNOTS ( 'NONE', 3,
 ( #73445, #31755, #152990, #232512, #133396, #55099, #175134, #212928, #10436, #110804, #26153, #31312, #209928, #7878, #126525, #106944, #127817, #228201, #70440, #165672, #207359, #30019, #66556, #48267, #105646, #187797 ),
 .UNSPECIFIED., .F., .F.,
 ( 4, 2, 2, 2, 2, 2, 2, 2, 2, 2, 2, 2, 4 ),
 ( 0.005476422646581361256, 0.006160811967703612099, 0.006845201288825863810, 0.007187395949386962343, 0.007529590609948060009, 0.007871785270509157675, 0.008213979931070255341, 0.008556174591631353007, 0.008898369252192450674, 0.009240563912753550074, 0.009582758573314646006, 0.01026714789443683787, 0.01095153721555903147 ),
 .UNSPECIFIED. ) ;
#68599 = TOROIDAL_SURFACE ( 'NONE', #130942, 0.2000000000000000111, 0.1000000000000000056 ) ;
#68598 = LINE ( 'NONE', #226351, #79777 ) ;
#68600 = AXIS2_PLACEMENT_3D ( 'NONE', #170079, #35689, #192181 ) ;
#68601 = FACE_OUTER_BOUND ( 'NONE', #72058, .T. ) ;
#68602 = ADVANCED_FACE ( 'NONE', ( #229358 ), #29083, .T. ) ;
#68603 = ORIENTED_EDGE ( 'NONE', *, *, #95194, .T. ) ;
#68604 = EDGE_LOOP ( 'NONE', ( #117406, #61165, #254037, #24476, #37803, #235583, #50914, #146982, #145084, #202953, #11796, #115958, #58084, #171733, #183002, #103668, #88669, #96146 ) ) ;
#68605 = AXIS2_PLACEMENT_3D ( 'NONE', #219745, #18977, #176800 ) ;
#68606 = FACE_OUTER_BOUND ( 'NONE', #191311, .T. ) ;
#68607 = CARTESIAN_POINT ( 'NONE',  ( -18.39999999999999858, -9.499999999988849808, -141.0320693966996828 ) ) ;
#68608 = VECTOR ( 'NONE', #149362, 1000.000000000000000 ) ;
#68609 = DIRECTION ( 'NONE',  ( -1.000000000000000000, 0.000000000000000000, 0.000000000000000000 ) ) ;
#68610 = DIRECTION ( 'NONE',  ( -0.000000000000000000, 0.8660254037844377084, 0.5000000000000016653 ) ) ;
#68612 = AXIS2_PLACEMENT_3D ( 'NONE', #90304, #169909, #249407 ) ;
#68611 = DIRECTION ( 'NONE',  ( 1.000000000000000000, 0.000000000000000000, 0.000000000000000000 ) ) ;
#68613 = DIRECTION ( 'NONE',  ( 0.000000000000000000, 0.000000000000000000, 1.000000000000000000 ) ) ;
#68614 = AXIS2_PLACEMENT_3D ( 'NONE', #47123, #221909, #1592 ) ;
#68615 = EDGE_CURVE ( 'NONE', #5081, #66896, #233221, .T. ) ;
#68616 = CIRCLE ( 'NONE', #197594, 0.1999999999999987899 ) ;
#68617 = DIRECTION ( 'NONE',  ( 0.000000000000000000, 0.000000000000000000, 1.000000000000000000 ) ) ;
#68618 = ADVANCED_FACE ( 'NONE', ( #93681 ), #187283, .T. ) ;
#68619 = VERTEX_POINT ( 'NONE', #71578 ) ;
#68620 = CARTESIAN_POINT ( 'NONE',  ( -20.85000000000000142, 64.25000000001220712, -143.3647081744214802 ) ) ;
#68621 = ORIENTED_EDGE ( 'NONE', *, *, #219395, .F. ) ;
#68622 = DIRECTION ( 'NONE',  ( 1.000000000000000000, 0.000000000000000000, 0.000000000000000000 ) ) ;
#68623 = CARTESIAN_POINT ( 'NONE',  ( 21.05000000000000071, -0.09999999999999939493, 6.540656951701244282 ) ) ;
#68625 = AXIS2_PLACEMENT_3D ( 'NONE', #83636, #62831, #182799 ) ;
#68624 = CARTESIAN_POINT ( 'NONE',  ( -22.19999999999999929, -11.65000000000000036, -15.00000000000000000 ) ) ;
#68626 = EDGE_CURVE ( 'NONE', #197038, #163061, #151098, .T. ) ;
#68627 = CARTESIAN_POINT ( 'NONE',  ( -23.25000000000000000, -11.75000000000000000, -30.39999999999999858 ) ) ;
#68628 = DIRECTION ( 'NONE',  ( 0.000000000000000000, 0.000000000000000000, -1.000000000000000000 ) ) ;
#68629 = CARTESIAN_POINT ( 'NONE',  ( -18.40000000000000213, -9.500000000000007105, -6.999362097180126696 ) ) ;
#68630 = SPHERICAL_SURFACE ( 'NONE', #68427, 0.1000000000000000056 ) ;
#68631 = ADVANCED_FACE ( 'NONE', ( #113243 ), #54551, .F. ) ;
#68632 = EDGE_LOOP ( 'NONE', ( #25179, #247982, #163233, #144088 ) ) ;
#68633 = DIRECTION ( 'NONE',  ( 1.000000000000000000, 0.000000000000000000, 0.000000000000000000 ) ) ;
#68634 = AXIS2_PLACEMENT_3D ( 'NONE', #43464, #60441, #142547 ) ;
#68635 = DIRECTION ( 'NONE',  ( 0.000000000000000000, 0.000000000000000000, 1.000000000000000000 ) ) ;
#68636 = DIRECTION ( 'NONE',  ( -1.000000000000000000, 0.000000000000000000, 0.000000000000000000 ) ) ;
#68637 = LINE ( 'NONE', #251096, #56332 ) ;
#68638 = EDGE_CURVE ( 'NONE', #23353, #74847, #174562, .T. ) ;
#68639 = CIRCLE ( 'NONE', #85158, 0.1999999999999987899 ) ;
#68640 = DIRECTION ( 'NONE',  ( 6.938893903907224433E-15, -1.000000000000000000, -2.891205793294679805E-16 ) ) ;
#68641 = AXIS2_PLACEMENT_3D ( 'NONE', #30974, #110470, #208312 ) ;
#68642 = AXIS2_PLACEMENT_3D ( 'NONE', #174840, #114814, #251756 ) ;
#68643 = ORIENTED_EDGE ( 'NONE', *, *, #54381, .F. ) ;
#68644 = LINE ( 'NONE', #223837, #256087 ) ;
#68645 = CARTESIAN_POINT ( 'NONE',  ( -18.34374000495060386, 58.57934086597919077, -223.9244941873113817 ) ) ;
#68646 = ORIENTED_EDGE ( 'NONE', *, *, #6977, .F. ) ;
#68647 = EDGE_CURVE ( 'NONE', #216962, #184062, #109376, .T. ) ;
#68648 = ORIENTED_EDGE ( 'NONE', *, *, #227229, .T. ) ;
#68649 = CARTESIAN_POINT ( 'NONE',  ( -23.25000000000000000, 8.809961202382810441, -241.4517562488062481 ) ) ;
#68650 = CARTESIAN_POINT ( 'NONE',  ( 21.11747605621531321, 67.22129199451940451, -157.7785443147346598 ) ) ;
#68651 = CARTESIAN_POINT ( 'NONE',  ( 20.97239005616515684, 44.21014168011738832, -236.4435994341349101 ) ) ;
#68652 = ADVANCED_FACE ( 'NONE', ( #53279 ), #132825, .F. ) ;
#68653 = ORIENTED_EDGE ( 'NONE', *, *, #193548, .F. ) ;
#68654 = CARTESIAN_POINT ( 'NONE',  ( 20.94999999999999929, 64.35000000001146248, -42.80697314750249660 ) ) ;
#68655 = DIRECTION ( 'NONE',  ( 1.000000000000000000, -0.000000000000000000, -0.000000000000000000 ) ) ;
#68656 = VERTEX_POINT ( 'NONE', #114533 ) ;
#68657 = VECTOR ( 'NONE', #215359, 1000.000000000000000 ) ;
#68658 = DIRECTION ( 'NONE',  ( 0.000000000000000000, 0.000000000000000000, -1.000000000000000000 ) ) ;
#68659 = AXIS2_PLACEMENT_3D ( 'NONE', #170966, #250443, #151370 ) ;
#68660 = VERTEX_POINT ( 'NONE', #194090 ) ;
#68661 = CARTESIAN_POINT ( 'NONE',  ( -16.87331047859651179, 9.949999999999986855, -12.65000000000000213 ) ) ;
#68662 = CARTESIAN_POINT ( 'NONE',  ( -21.05000000000000071, 76.00000000001240608, -174.3231074845243427 ) ) ;
#68664 = ORIENTED_EDGE ( 'NONE', *, *, #132080, .T. ) ;
#68663 = DIRECTION ( 'NONE',  ( 0.000000000000000000, 0.000000000000000000, -1.000000000000000000 ) ) ;
#68665 = LINE ( 'NONE', #26991, #19935 ) ;
#68667 = FACE_OUTER_BOUND ( 'NONE', #55846, .T. ) ;
#68666 = UNCERTAINTY_MEASURE_WITH_UNIT (LENGTH_MEASURE( 1.000000000000000082E-05 ), #32308, 'distance_accuracy_value', 'NONE');
#68668 = CARTESIAN_POINT ( 'NONE',  ( -21.93340585972069334, 68.67585297715930892, -203.5231074845244166 ) ) ;
#68669 = DIRECTION ( 'NONE',  ( 0.000000000000000000, 0.000000000000000000, 1.000000000000000000 ) ) ;
#68670 = DIRECTION ( 'NONE',  ( 1.000000000000000000, 0.000000000000000000, 0.000000000000000000 ) ) ;
#68671 = CARTESIAN_POINT ( 'NONE',  ( -18.59999999999999787, 77.83585931145570669, -125.0186683157258045 ) ) ;
#68672 = CARTESIAN_POINT ( 'NONE',  ( 21.15000000000005542, 77.83551161375991967, -47.52760213295649550 ) ) ;
#68674 = ORIENTED_EDGE ( 'NONE', *, *, #234613, .T. ) ;
#68673 = CARTESIAN_POINT ( 'NONE',  ( 18.60000000000000142, 86.96699927712943179, -199.3055931863049466 ) ) ;
#68675 = ORIENTED_EDGE ( 'NONE', *, *, #116473, .T. ) ;
#68677 = CARTESIAN_POINT ( 'NONE',  ( -20.94999999999999929, 77.73625713160897988, -57.95445515550681392 ) ) ;
#68676 = DIRECTION ( 'NONE',  ( 1.000000000000000000, 0.000000000000000000, 0.000000000000000000 ) ) ;
#68679 = ORIENTED_EDGE ( 'NONE', *, *, #83916, .T. ) ;
#68678 = FACE_OUTER_BOUND ( 'NONE', #233939, .T. ) ;
#68680 = VERTEX_POINT ( 'NONE', #15449 ) ;
#68681 = CARTESIAN_POINT ( 'NONE',  ( -22.47007471830799119, 0.3230635261676482739, -230.0870367350772483 ) ) ;
#68682 = CARTESIAN_POINT ( 'NONE',  ( -20.85000000000000142, 86.58125133469155799, -209.3975964148341973 ) ) ;
#68683 = AXIS2_PLACEMENT_3D ( 'NONE', #233875, #155657, #172670 ) ;
#68684 = VECTOR ( 'NONE', #255928, 1000.000000000000000 ) ;
#68685 = DIRECTION ( 'NONE',  ( 0.000000000000000000, 0.9126074666063660468, 0.4088369013363524762 ) ) ;
#68686 = CARTESIAN_POINT ( 'NONE',  ( -23.25000000000000000, 4.350000000011156054, -179.7499999999999716 ) ) ;
#68687 = PLANE ( 'NONE',  #231778 ) ;
#68688 = CARTESIAN_POINT ( 'NONE',  ( 22.39999999999999503, 76.00000000001219291, -144.2731074845243313 ) ) ;
#68689 = DIRECTION ( 'NONE',  ( 1.000000000000000000, 3.265361837132813093E-16, -0.000000000000000000 ) ) ;
#68690 = ORIENTED_EDGE ( 'NONE', *, *, #51129, .T. ) ;
#68691 = ORIENTED_EDGE ( 'NONE', *, *, #98709, .T. ) ;
#68692 = EDGE_CURVE ( 'NONE', #81812, #141973, #94954, .T. ) ;
#68693 = CARTESIAN_POINT ( 'NONE',  ( -21.05000000000000071, 64.27836561112391678, -247.1251233467904171 ) ) ;
#68694 = CIRCLE ( 'NONE', #110372, 0.2000000000000000944 ) ;
#68695 = VECTOR ( 'NONE', #241236, 1000.000000000000000 ) ;
#68696 = ORIENTED_EDGE ( 'NONE', *, *, #3754, .F. ) ;
#68697 = FACE_OUTER_BOUND ( 'NONE', #123527, .T. ) ;
#68698 = EDGE_LOOP ( 'NONE', ( #40032, #209497, #208244, #30393 ) ) ;
#68699 = CARTESIAN_POINT ( 'NONE',  ( 21.05000000000000071, -4.656943609564678788, -233.1535107627236414 ) ) ;
#68700 = AXIS2_PLACEMENT_3D ( 'NONE', #157420, #182086, #221187 ) ;
#68701 = CARTESIAN_POINT ( 'NONE',  ( -21.98333005346336932, 76.00000000001170974, -76.89718281358099716 ) ) ;
#68702 = EDGE_CURVE ( 'NONE', #179923, #21183, #208518, .T. ) ;
#68703 = DIRECTION ( 'NONE',  ( 0.000000000000000000, 0.000000000000000000, 1.000000000000000000 ) ) ;
#68704 = ORIENTED_EDGE ( 'NONE', *, *, #84864, .F. ) ;
#68705 = CARTESIAN_POINT ( 'NONE',  ( -21.03571358705741190, 11.74999999999999645, -6.825106822058594425 ) ) ;
#68706 = ORIENTED_EDGE ( 'NONE', *, *, #93988, .F. ) ;
#68707 = EDGE_CURVE ( 'NONE', #179090, #76578, #91586, .T. ) ;
#68708 = FACE_OUTER_BOUND ( 'NONE', #39816, .T. ) ;
#68709 = EDGE_CURVE ( 'NONE', #118204, #52463, #120975, .T. ) ;
#68710 = DIRECTION ( 'NONE',  ( 1.000000000000000000, -0.000000000000000000, -0.000000000000000000 ) ) ;
#68711 = CARTESIAN_POINT ( 'NONE',  ( 18.45036689428327747, 8.829294088443328192, -245.4095986352067484 ) ) ;
#68712 = ORIENTED_EDGE ( 'NONE', *, *, #107060, .T. ) ;
#68713 = DIRECTION ( 'NONE',  ( 0.000000000000000000, 0.000000000000000000, 1.000000000000000000 ) ) ;
#68714 = ORIENTED_EDGE ( 'NONE', *, *, #106530, .T. ) ;
#68717 = ORIENTED_EDGE ( 'NONE', *, *, #43549, .T. ) ;
#68716 = CARTESIAN_POINT ( 'NONE',  ( 18.50016250449482058, 46.34703458179488678, -243.0587802416278009 ) ) ;
#68715 = DIRECTION ( 'NONE',  ( -1.000000000000000000, 0.000000000000000000, 0.000000000000000000 ) ) ;
#68718 = CARTESIAN_POINT ( 'NONE',  ( -21.55000000000000071, 7.150000000011155876, -88.25000000000005684 ) ) ;
#68720 = ORIENTED_EDGE ( 'NONE', *, *, #26137, .F. ) ;
#68719 = AXIS2_PLACEMENT_3D ( 'NONE', #18368, #178768, #222975 ) ;
#68721 = CARTESIAN_POINT ( 'NONE',  ( 20.94999999999999929, 1.115600667400684642E-11, -67.00000000000000000 ) ) ;
#68722 = EDGE_LOOP ( 'NONE', ( #133920, #255515, #99528, #26154, #221656 ) ) ;
#68723 = CIRCLE ( 'NONE', #52140, 12.97499999999999609 ) ;
#68724 = ADVANCED_FACE ( 'NONE', ( #177098 ), #38857, .F. ) ;
#68725 = LINE ( 'NONE', #145675, #70030 ) ;
#68726 = FACE_OUTER_BOUND ( 'NONE', #192592, .T. ) ;
#68727 = LINE ( 'NONE', #166569, #43627 ) ;
#68728 = AXIS2_PLACEMENT_3D ( 'NONE', #16085, #95584, #21222 ) ;
#68729 = CIRCLE ( 'NONE', #114515, 0.09999999999999939493 ) ;
#68730 = AXIS2_PLACEMENT_3D ( 'NONE', #26773, #145396, #164971 ) ;
#68731 = CARTESIAN_POINT ( 'NONE',  ( 21.05000000000000071, 76.00000000001215028, -138.4231074845243654 ) ) ;
#68732 = AXIS2_PLACEMENT_3D ( 'NONE', #158207, #137300, #197284 ) ;
#68733 = VERTEX_POINT ( 'NONE', #220046 ) ;
#68734 = DIRECTION ( 'NONE',  ( 0.000000000000000000, 0.000000000000000000, -1.000000000000000000 ) ) ;
#68735 = CARTESIAN_POINT ( 'NONE',  ( -16.89268316805465986, 9.951721813253337601, -188.3557524785454973 ) ) ;
#68736 = CARTESIAN_POINT ( 'NONE',  ( -12.93407622233968546, 66.58221053306007775, -154.6657229405475391 ) ) ;
#68737 = ORIENTED_EDGE ( 'NONE', *, *, #22818, .F. ) ;
#68738 = CARTESIAN_POINT ( 'NONE',  ( -23.15000000000000213, 1.148907358139439339E-11, -201.0000000000015064 ) ) ;
#68739 = ORIENTED_EDGE ( 'NONE', *, *, #179587, .T. ) ;
#68740 = CARTESIAN_POINT ( 'NONE',  ( 21.07928932188134397, 30.84304088367083097, -252.0482413927653340 ) ) ;
#68741 = ORIENTED_EDGE ( 'NONE', *, *, #7570, .T. ) ;
#68742 = CIRCLE ( 'NONE', #106130, 4.000000000000003553 ) ;
#68743 = ADVANCED_FACE ( 'NONE', ( #118392 ), #74868, .T. ) ;
#68744 = AXIS2_PLACEMENT_3D ( 'NONE', #149464, #12521, #93312 ) ;
#68745 = CARTESIAN_POINT ( 'NONE',  ( 21.05000000000000071, 76.10000000001174669, -81.17267829206912211 ) ) ;
#68746 = DIRECTION ( 'NONE',  ( 0.000000000000000000, 0.000000000000000000, -1.000000000000000000 ) ) ;
#68748 = ORIENTED_EDGE ( 'NONE', *, *, #17126, .T. ) ;
#68747 = CARTESIAN_POINT ( 'NONE',  ( -16.77180007708461673, 44.12235304356341459, -235.3048130856369653 ) ) ;
#68749 = CARTESIAN_POINT ( 'NONE',  ( -18.79999999999999716, 1.885425182446133885, -11.49641995933507843 ) ) ;
#68750 = CIRCLE ( 'NONE', #135366, 0.1000000000000017680 ) ;
#68751 = CIRCLE ( 'NONE', #156080, 0.09999999999999868716 ) ;
#68752 = CARTESIAN_POINT ( 'NONE',  ( -12.30589683808041102, 62.70378344720913333, -216.8024073824997231 ) ) ;
#68753 = DIRECTION ( 'NONE',  ( 2.952720810173288619E-16, -0.4721928772777346239, -0.8814952561688430555 ) ) ;
#68755 = EDGE_CURVE ( 'NONE', #235714, #115133, #145731, .T. ) ;
#68754 = ORIENTED_EDGE ( 'NONE', *, *, #168901, .T. ) ;
#68756 = DIRECTION ( 'NONE',  ( -1.000000000000000000, -0.000000000000000000, -0.000000000000000000 ) ) ;
#68757 = CARTESIAN_POINT ( 'NONE',  ( -12.25000000000000178, 26.54497872210690090, -232.9592037335782209 ) ) ;
#68758 = ORIENTED_EDGE ( 'NONE', *, *, #48281, .F. ) ;
#68759 = CARTESIAN_POINT ( 'NONE',  ( 21.05000000000000782, 1.643181256369374843, -230.7196533885927181 ) ) ;
#68760 = B_SPLINE_CURVE_WITH_KNOTS ( 'NONE', 3,
 ( #70756, #150277, #152870, #109835, #112435, #10756, #231107, #210252, #108569, #229794 ),
 .UNSPECIFIED., .F., .F.,
 ( 4, 3, 3, 4 ),
 ( 1.950915401637565782E-15, 8.145022132826850876E-06, 1.905645951092260044E-05, 2.061107371225642508E-05 ),
 .UNSPECIFIED. ) ;
#68761 = VERTEX_POINT ( 'NONE', #195375 ) ;
#68762 = DIRECTION ( 'NONE',  ( 2.952720810173288619E-16, -1.000000000000000000, 0.000000000000000000 ) ) ;
#68763 = CYLINDRICAL_SURFACE ( 'NONE', #197062, 0.1000000000000028644 ) ;
#68766 = ORIENTED_EDGE ( 'NONE', *, *, #255386, .F. ) ;
#68765 = EDGE_LOOP ( 'NONE', ( #139972, #107261, #35082, #133701, #154398, #165311, #91476, #72896, #123292, #201563, #229495, #99746 ) ) ;
#68764 = LINE ( 'NONE', #53041, #251246 ) ;
#68767 = AXIS2_PLACEMENT_3D ( 'NONE', #45254, #100062, #102628 ) ;
#68768 = CARTESIAN_POINT ( 'NONE',  ( -20.94999999999999929, -4.871452838297996024, -233.3782557782877518 ) ) ;
#68769 = CARTESIAN_POINT ( 'NONE',  ( -14.00000000000000178, 26.54497872210690090, -232.9592037335782209 ) ) ;
#68770 = AXIS2_PLACEMENT_3D ( 'NONE', #101368, #19320, #201797 ) ;
#68771 = DIRECTION ( 'NONE',  ( 1.000000000000000000, 0.000000000000000000, 0.000000000000000000 ) ) ;
#68773 = DIRECTION ( 'NONE',  ( 0.000000000000000000, 0.000000000000000000, 1.000000000000000000 ) ) ;
#68772 = CARTESIAN_POINT ( 'NONE',  ( 22.49066049874202022, 0.05634325154338429287, -88.84998776248292529 ) ) ;
#68774 = CARTESIAN_POINT ( 'NONE',  ( -23.25000000000000355, 11.75000000001113953, -176.7499999999999716 ) ) ;
#68775 = CONICAL_SURFACE ( 'NONE', #72905, 4.049999999999995381, 0.7853981633974604915 ) ;
#68776 = DIRECTION ( 'NONE',  ( 0.000000000000000000, 0.000000000000000000, -1.000000000000000000 ) ) ;
#68777 = DIRECTION ( 'NONE',  ( -1.000000000000000000, 0.000000000000000000, 0.000000000000000000 ) ) ;
#68778 = FACE_OUTER_BOUND ( 'NONE', #252782, .T. ) ;
#68779 = EDGE_LOOP ( 'NONE', ( #31613, #191894, #54276, #176329 ) ) ;
#68781 = ORIENTED_EDGE ( 'NONE', *, *, #101129, .F. ) ;
#68780 = VECTOR ( 'NONE', #79902, 1000.000000000000000 ) ;
#68782 = EDGE_CURVE ( 'NONE', #256147, #122770, #120642, .T. ) ;
#68783 = DIRECTION ( 'NONE',  ( 0.000000000000000000, 0.000000000000000000, -1.000000000000000000 ) ) ;
#68784 = AXIS2_PLACEMENT_3D ( 'NONE', #233413, #195566, #191726 ) ;
#68785 = EDGE_CURVE ( 'NONE', #151479, #189963, #175876, .T. ) ;
#68787 = ORIENTED_EDGE ( 'NONE', *, *, #126510, .F. ) ;
#68786 = CARTESIAN_POINT ( 'NONE',  ( -23.25000000000000000, 71.65000000001151648, -48.17310748452435831 ) ) ;
#68788 = VERTEX_POINT ( 'NONE', #79229 ) ;
#68789 = LINE ( 'NONE', #148321, #122641 ) ;
#68790 = ORIENTED_EDGE ( 'NONE', *, *, #181041, .T. ) ;
#68791 = DIRECTION ( 'NONE',  ( 1.000000000000000000, 0.000000000000000000, -0.000000000000000000 ) ) ;
#68792 = ADVANCED_FACE ( 'NONE', ( #81781 ), #156255, .T. ) ;
#68793 = EDGE_CURVE ( 'NONE', #239007, #12375, #139198, .T. ) ;
#68794 = AXIS2_PLACEMENT_3D ( 'NONE', #115681, #152265, #133945 ) ;
#68795 = VERTEX_POINT ( 'NONE', #101326 ) ;
#68796 = CIRCLE ( 'NONE', #14654, 0.1000000000000057648 ) ;
#68797 = ADVANCED_FACE ( 'NONE', ( #179654 ), #158819, .F. ) ;
#68798 = DIRECTION ( 'NONE',  ( 0.000000000000000000, 0.2128009952263403282, -0.9770955615653358350 ) ) ;
#68799 = DIRECTION ( 'NONE',  ( 0.000000000000000000, 0.000000000000000000, -1.000000000000000000 ) ) ;
#68800 = AXIS2_PLACEMENT_3D ( 'NONE', #157558, #197911, #16737 ) ;
#68801 = ADVANCED_FACE ( 'NONE', ( #161372, #57094, #40159 ), #37576, .F. ) ;
#68803 = EDGE_LOOP ( 'NONE', ( #71682, #160437, #227868, #103393, #23047 ) ) ;
#68802 = EDGE_LOOP ( 'NONE', ( #164621, #163357, #140945, #182619, #96247, #86918, #124388, #81927, #243555, #256273, #234209, #226251, #175603, #21046, #132265, #174405, #165963, #178075, #245679, #159914, #146447, #10229, #18931 ) ) ;
#68804 = VERTEX_POINT ( 'NONE', #140492 ) ;
#68807 = ADVANCED_FACE ( 'NONE', ( #88203 ), #205601, .F. ) ;
#68806 = EDGE_CURVE ( 'NONE', #237888, #48194, #253883, .T. ) ;
#68805 = DIRECTION ( 'NONE',  ( 0.000000000000000000, -1.000000000000000000, -6.982962677686266711E-15 ) ) ;
#68808 = VERTEX_POINT ( 'NONE', #182213 ) ;
#68809 = ORIENTED_EDGE ( 'NONE', *, *, #254041, .T. ) ;
#68810 = LINE ( 'NONE', #70109, #13709 ) ;
#68811 = DIRECTION ( 'NONE',  ( 0.000000000000000000, 1.000000000000000000, 0.000000000000000000 ) ) ;
#68812 = LINE ( 'NONE', #128783, #231143 ) ;
#68814 = VERTEX_POINT ( 'NONE', #66102 ) ;
#68813 = CARTESIAN_POINT ( 'NONE',  ( -23.15000000000000213, 85.50000000001232081, -160.1291383618718385 ) ) ;
#68816 = EDGE_CURVE ( 'NONE', #133581, #19091, #6114, .T. ) ;
#68815 = VECTOR ( 'NONE', #93108, 1000.000000000000000 ) ;
#68817 = CARTESIAN_POINT ( 'NONE',  ( -23.25000000000000000, 1.115600667400684642E-11, -100.5000000000000284 ) ) ;
#68818 = DIRECTION ( 'NONE',  ( 0.000000000000000000, 1.000000000000000000, 0.000000000000000000 ) ) ;
#68820 = VERTEX_POINT ( 'NONE', #221306 ) ;
#68819 = DIRECTION ( 'NONE',  ( 0.000000000000000000, 0.000000000000000000, -1.000000000000000000 ) ) ;
#68821 = CARTESIAN_POINT ( 'NONE',  ( -23.15000000000000213, 1.115600667400684642E-11, -134.0000000000000000 ) ) ;
#68822 = ORIENTED_EDGE ( 'NONE', *, *, #201783, .F. ) ;
#68823 = DIRECTION ( 'NONE',  ( 0.7071067811865475727, -0.7071067811865475727, -4.937700262164531476E-15 ) ) ;
#68824 = VERTEX_POINT ( 'NONE', #223875 ) ;
#68825 = DIRECTION ( 'NONE',  ( 1.000000000000000000, 0.000000000000000000, 0.000000000000000000 ) ) ;
#68827 = ADVANCED_FACE ( 'NONE', ( #4818 ), #83164, .F. ) ;
#68826 = DIRECTION ( 'NONE',  ( 1.000000000000000000, -0.000000000000000000, 0.000000000000000000 ) ) ;
#68828 = ORIENTED_EDGE ( 'NONE', *, *, #116386, .T. ) ;
#68830 = SPHERICAL_SURFACE ( 'NONE', #191582, 0.1000000000000000056 ) ;
#68829 = CARTESIAN_POINT ( 'NONE',  ( -21.05000000000000071, 60.94483358488582070, -234.0465764481390636 ) ) ;
#68831 = EDGE_CURVE ( 'NONE', #202762, #222218, #179104, .T. ) ;
#68832 = EDGE_CURVE ( 'NONE', #201062, #12214, #87292, .T. ) ;
#68833 = DIRECTION ( 'NONE',  ( -1.000000000000000000, -0.000000000000000000, -0.000000000000000000 ) ) ;
#68834 = AXIS2_PLACEMENT_3D ( 'NONE', #250628, #171156, #214087 ) ;
#68835 = DIRECTION ( 'NONE',  ( 0.000000000000000000, 0.000000000000000000, -1.000000000000000000 ) ) ;
#68836 = AXIS2_PLACEMENT_3D ( 'NONE', #151748, #166181, #47459 ) ;
#68837 = DIRECTION ( 'NONE',  ( -1.000000000000000000, -0.000000000000000000, 0.000000000000000000 ) ) ;
#68838 = VERTEX_POINT ( 'NONE', #83059 ) ;
#68839 = ORIENTED_EDGE ( 'NONE', *, *, #52888, .T. ) ;
#68840 = EDGE_CURVE ( 'NONE', #212150, #16688, #105780, .T. ) ;
#68841 = DIRECTION ( 'NONE',  ( 0.000000000000000000, -0.9651348961777157509, 0.2617529984165031243 ) ) ;
#68842 = DIRECTION ( 'NONE',  ( -0.7071067811865474617, -0.7071067811865474617, -0.000000000000000000 ) ) ;
#68843 = VERTEX_POINT ( 'NONE', #105182 ) ;
#68844 = LINE ( 'NONE', #191374, #118502 ) ;
#68845 = ORIENTED_EDGE ( 'NONE', *, *, #156886, .F. ) ;
#68846 = DIRECTION ( 'NONE',  ( 1.000000000000000000, -3.265361837132813093E-16, -2.280189983783949500E-30 ) ) ;
#68847 = ORIENTED_EDGE ( 'NONE', *, *, #44358, .T. ) ;
#68848 = CARTESIAN_POINT ( 'NONE',  ( 23.14999999999999858, 20.42498087366621817, -235.1829032864613396 ) ) ;
#68849 = ADVANCED_FACE ( 'NONE', ( #184761 ), #46524, .F. ) ;
#68850 = CARTESIAN_POINT ( 'NONE',  ( -23.15000000000000213, 74.00000000001199396, -115.7477294072863998 ) ) ;
#68851 = CARTESIAN_POINT ( 'NONE',  ( -16.87331047859651179, 66.05000000001187743, -90.37310748452438247 ) ) ;
#68852 = EDGE_CURVE ( 'NONE', #198075, #137562, #70767, .T. ) ;
#68853 = ORIENTED_EDGE ( 'NONE', *, *, #107267, .F. ) ;
#68854 = FACE_OUTER_BOUND ( 'NONE', #181702, .T. ) ;
#68855 =( NAMED_UNIT ( * ) SI_UNIT ( $, .STERADIAN. ) SOLID_ANGLE_UNIT ( ) );
#68856 = VECTOR ( 'NONE', #93186, 1000.000000000000000 ) ;
#68857 = ORIENTED_EDGE ( 'NONE', *, *, #64093, .F. ) ;
#68858 = ORIENTED_EDGE ( 'NONE', *, *, #198394, .F. ) ;
#68859 = ORIENTED_EDGE ( 'NONE', *, *, #109447, .F. ) ;
#68860 = CARTESIAN_POINT ( 'NONE',  ( -20.85000000000000142, -1.362429037182151470, -74.88888124792120493 ) ) ;
#68861 = CARTESIAN_POINT ( 'NONE',  ( -13.40000000000000036, -8.250000000000007105, 12.40000000000000391 ) ) ;
#68862 = CIRCLE ( 'NONE', #168840, 0.1000000000000028644 ) ;
#68863 = CARTESIAN_POINT ( 'NONE',  ( -21.08621493067320429, 0.05619483948720575828, -127.6507057088280845 ) ) ;
#68864 = CYLINDRICAL_SURFACE ( 'NONE', #73812, 4.000000000000000000 ) ;
#68865 = CARTESIAN_POINT ( 'NONE',  ( -20.64999999999999858, 68.66552716081216090, -214.3300732090495444 ) ) ;
#68866 = EDGE_CURVE ( 'NONE', #172097, #199454, #62367, .T. ) ;
#68868 = CARTESIAN_POINT ( 'NONE',  ( -21.46681500597178882, 1.115541036281197940E-11, -160.6424888405653633 ) ) ;
#68867 = CARTESIAN_POINT ( 'NONE',  ( -22.00411653962174441, 10.46655577783124969, -227.2920607449393344 ) ) ;
#68870 = ORIENTED_EDGE ( 'NONE', *, *, #179466, .F. ) ;
#68869 = DIRECTION ( 'NONE',  ( 0.000000000000000000, 0.000000000000000000, -1.000000000000000000 ) ) ;
#68871 = CARTESIAN_POINT ( 'NONE',  ( -18.59999999999999787, 18.14639373905162145, -237.6648341169113792 ) ) ;
#68872 = EDGE_LOOP ( 'NONE', ( #130327, #12284, #10693, #128189 ) ) ;
#68873 = CARTESIAN_POINT ( 'NONE',  ( -21.05000000000000071, 75.74389420791972327, -103.0580039261966050 ) ) ;
#68874 = VERTEX_POINT ( 'NONE', #143057 ) ;
#68875 = EDGE_LOOP ( 'NONE', ( #8784, #224060, #98636 ) ) ;
#68876 = CARTESIAN_POINT ( 'NONE',  ( 20.93284271247462414, 64.25000000001195133, -110.0379132551783243 ) ) ;
#68877 = FACE_OUTER_BOUND ( 'NONE', #123138, .T. ) ;
#68878 = DIRECTION ( 'NONE',  ( 1.000000000000000000, 0.000000000000000000, 0.000000000000000000 ) ) ;
#68879 = B_SPLINE_CURVE_WITH_KNOTS ( 'NONE', 3,
 ( #88266, #225214, #7472, #226496, #86982, #47869, #206964, #68740 ),
 .UNSPECIFIED., .F., .F.,
 ( 4, 2, 2, 4 ),
 ( 0.000000000000000000, 0.0001306511400391170414, 0.0001959767100586792214, 0.0002613022800782414013 ),
 .UNSPECIFIED. ) ;
#68880 = FACE_OUTER_BOUND ( 'NONE', #226400, .T. ) ;
#68881 = CIRCLE ( 'NONE', #131394, 2.600000000000001421 ) ;
#68882 = TOROIDAL_SURFACE ( 'NONE', #202142, 1.900000000000002576, 0.1000000000000000056 ) ;
#68883 = DIRECTION ( 'NONE',  ( 0.000000000000000000, 0.000000000000000000, 1.000000000000000000 ) ) ;
#68884 = ORIENTED_EDGE ( 'NONE', *, *, #179068, .T. ) ;
#68885 = ORIENTED_EDGE ( 'NONE', *, *, #172828, .F. ) ;
#68886 = LINE ( 'NONE', #32340, #103168 ) ;
#68887 = ORIENTED_EDGE ( 'NONE', *, *, #68958, .F. ) ;
#68888 = DIRECTION ( 'NONE',  ( 0.000000000000000000, 0.000000000000000000, -1.000000000000000000 ) ) ;
#68889 = CARTESIAN_POINT ( 'NONE',  ( -18.59999999999999787, -1.162701749926853712, -142.1000000000000227 ) ) ;
#68890 = VERTEX_POINT ( 'NONE', #45258 ) ;
#68891 = CARTESIAN_POINT ( 'NONE',  ( -20.54999999999999716, 84.73084112150731073, -112.6211822035085675 ) ) ;
#68892 = CARTESIAN_POINT ( 'NONE',  ( -16.87036670365548474, 51.72098459467785858, -231.8575261499355236 ) ) ;
#68893 = DIRECTION ( 'NONE',  ( 0.000000000000000000, -0.000000000000000000, 1.000000000000000000 ) ) ;
#68894 = CARTESIAN_POINT ( 'NONE',  ( 21.14999999999999858, 6.540656951712400691, -67.00000000000004263 ) ) ;
#68895 = ORIENTED_EDGE ( 'NONE', *, *, #97523, .T. ) ;
#68896 = DIRECTION ( 'NONE',  ( -1.000000000000000000, 0.000000000000000000, 0.000000000000000000 ) ) ;
#68897 = DIRECTION ( 'NONE',  ( 1.000000000000000000, 0.000000000000000000, 0.000000000000000000 ) ) ;
#68898 = DIRECTION ( 'NONE',  ( 0.000000000000000000, 1.000000000000000000, 0.000000000000000000 ) ) ;
#68899 = DIRECTION ( 'NONE',  ( 0.000000000000000000, 0.9770955615653551529, 0.2128009952262517601 ) ) ;
#68900 = EDGE_CURVE ( 'NONE', #61013, #15448, #241439, .T. ) ;
#68901 = CARTESIAN_POINT ( 'NONE',  ( 21.05000000000000071, 1.115600667400684642E-11, -200.9999999999999432 ) ) ;
#68902 = TOROIDAL_SURFACE ( 'NONE', #118959, 4.149999999999999467, 0.1000000000000000056 ) ;
#68903 = DIRECTION ( 'NONE',  ( 0.000000000000000000, 0.000000000000000000, -1.000000000000000000 ) ) ;
#68904 = EDGE_CURVE ( 'NONE', #169584, #39555, #166451, .T. ) ;
#68905 = AXIS2_PLACEMENT_3D ( 'NONE', #243466, #201768, #199224 ) ;
#68906 = AXIS2_PLACEMENT_3D ( 'NONE', #173818, #74704, #154245 ) ;
#68907 = VECTOR ( 'NONE', #226965, 1000.000000000000000 ) ;
#68908 = ORIENTED_EDGE ( 'NONE', *, *, #11219, .F. ) ;
#68909 = COLOUR_RGB ( '', 0.72549020, 0.75294118, 0.79215686) ;
#68910 = ADVANCED_FACE ( 'NONE', ( #23154 ), #86924, .F. ) ;
#68911 = CARTESIAN_POINT ( 'NONE',  ( 20.95512820512820440, 10.62384868371187707, -12.14999999999999858 ) ) ;
#68912 = EDGE_CURVE ( 'NONE', #1657, #230912, #158262, .T. ) ;
#68913 = ORIENTED_EDGE ( 'NONE', *, *, #252911, .T. ) ;
#68914 = CARTESIAN_POINT ( 'NONE',  ( 18.59999999999998366, 67.23127455305835554, -235.8551265064784559 ) ) ;
#68915 = DIRECTION ( 'NONE',  ( 0.000000000000000000, -0.000000000000000000, -1.000000000000000000 ) ) ;
#68917 = EDGE_CURVE ( 'NONE', #220002, #11174, #137351, .T. ) ;
#68916 = CARTESIAN_POINT ( 'NONE',  ( 18.49999999999999645, 76.00000000001267608, -203.5231074845243597 ) ) ;
#68918 = CARTESIAN_POINT ( 'NONE',  ( 20.19326291201646129, 65.84393901210839317, -162.2612456769175253 ) ) ;
#68919 = EDGE_LOOP ( 'NONE', ( #173677, #208001, #164407, #5174, #81016 ) ) ;
#68920 = CARTESIAN_POINT ( 'NONE',  ( -22.50000000000000000, 64.08545097430041437, -247.0723585184913986 ) ) ;
#68921 = CARTESIAN_POINT ( 'NONE',  ( 20.94999999999999929, 55.59258605799641373, -234.6589115948038966 ) ) ;
#68922 = DIRECTION ( 'NONE',  ( -1.000000000000000000, -3.439547145395919517E-14, 4.624352451196577991E-15 ) ) ;
#68923 = VECTOR ( 'NONE', #8765, 1000.000000000000000 ) ;
#68924 = DIRECTION ( 'NONE',  ( 0.000000000000000000, -1.000000000000000000, -6.982962677686265922E-15 ) ) ;
#68925 = MECHANICAL_DESIGN_GEOMETRIC_PRESENTATION_REPRESENTATION (  '', ( #23128 ), #135518 ) ;
#68926 = ADVANCED_FACE ( 'NONE', ( #43973 ), #124805, .F. ) ;
#68927 = VECTOR ( 'NONE', #35001, 1000.000000000000000 ) ;
#68928 = VERTEX_POINT ( 'NONE', #50367 ) ;
#68929 = ORIENTED_EDGE ( 'NONE', *, *, #125382, .T. ) ;
#68930 = CARTESIAN_POINT ( 'NONE',  ( 21.05000000000000071, 8.776282895303632259, -67.00000000000004263 ) ) ;
#68931 = DIRECTION ( 'NONE',  ( 1.000000000000000000, -0.000000000000000000, -0.000000000000000000 ) ) ;
#68932 = CARTESIAN_POINT ( 'NONE',  ( 18.79999999999999716, -11.75000000000000178, 0.000000000000000000 ) ) ;
#68933 = DIRECTION ( 'NONE',  ( 0.000000000000000000, -0.1350103645451945777, 0.9908441862701590219 ) ) ;
#68934 = DIRECTION ( 'NONE',  ( 0.000000000000000000, 0.9651348961777157509, -0.2617529984165031243 ) ) ;
#68935 = AXIS2_PLACEMENT_3D ( 'NONE', #21498, #44900, #203960 ) ;
#68936 = ORIENTED_EDGE ( 'NONE', *, *, #176169, .T. ) ;
#68937 = DIRECTION ( 'NONE',  ( -5.603264701231745086E-32, 0.2617529984165030132, 0.9651348961777158619 ) ) ;
#68938 = AXIS2_PLACEMENT_3D ( 'NONE', #214260, #117717, #19925 ) ;
#68939 = ITEM_DEFINED_TRANSFORMATION ( 'NONE', 'NONE', #19562,  #2425 ) ;
#68940 = AXIS2_PLACEMENT_3D ( 'NONE', #225796, #129295, #65458 ) ;
#68941 = ORIENTED_EDGE ( 'NONE', *, *, #107932, .F. ) ;
#68942 = FACE_OUTER_BOUND ( 'NONE', #135182, .T. ) ;
#68943 = EDGE_CURVE ( 'NONE', #116074, #235820, #53977, .T. ) ;
#68944 = CIRCLE ( 'NONE', #214653, 0.1000000000000024342 ) ;
#68945 = VERTEX_POINT ( 'NONE', #52951 ) ;
#68947 = VERTEX_POINT ( 'NONE', #212053 ) ;
#68946 = AXIS2_PLACEMENT_3D ( 'NONE', #224608, #45977, #206348 ) ;
#68948 = ORIENTED_EDGE ( 'NONE', *, *, #63288, .F. ) ;
#68949 = FACE_OUTER_BOUND ( 'NONE', #77115, .T. ) ;
#68950 = AXIS2_PLACEMENT_3D ( 'NONE', #118347, #154925, #157498 ) ;
#68951 = CARTESIAN_POINT ( 'NONE',  ( -21.05000000000000071, 69.25640205380744874, -247.7135141964517402 ) ) ;
#68952 = DIRECTION ( 'NONE',  ( 1.000000000000000000, 7.304098846218134667E-16, -4.607487905232622991E-31 ) ) ;
#68953 = EDGE_CURVE ( 'NONE', #226290, #204385, #79083, .T. ) ;
#68954 = CARTESIAN_POINT ( 'NONE',  ( 21.05000000000000071, -11.48912529306489994, -63.89999999999999858 ) ) ;
#68955 = CARTESIAN_POINT ( 'NONE',  ( -20.05000000000000426, 13.53887499352833146, -219.6971619212644669 ) ) ;
#68956 = LINE ( 'NONE', #148476, #232685 ) ;
#68957 = FACE_OUTER_BOUND ( 'NONE', #134748, .T. ) ;
#68958 = EDGE_CURVE ( 'NONE', #256823, #111166, #212410, .T. ) ;
#68960 = CARTESIAN_POINT ( 'NONE',  ( 23.14999999999999503, 11.65000000001116298, -126.9851942293460922 ) ) ;
#68959 = CARTESIAN_POINT ( 'NONE',  ( 20.95566103547454517, 65.38175234906483979, -95.39126729154378381 ) ) ;
#68961 = CARTESIAN_POINT ( 'NONE',  ( -20.85000000000000142, 77.16412189325330928, -128.8082593989527425 ) ) ;
#68962 = CARTESIAN_POINT ( 'NONE',  ( -16.87383368123029825, 9.950000000011138823, -113.1500000000000341 ) ) ;
#68963 = CARTESIAN_POINT ( 'NONE',  ( 22.49806830649814060, 0.07746431633666325811, -155.8501103451608856 ) ) ;
#68964 = CARTESIAN_POINT ( 'NONE',  ( 20.94999999999999574, 1.851028230152016674, -145.6539132694225032 ) ) ;
#68965 = EDGE_LOOP ( 'NONE', ( #126434, #32227, #133185 ) ) ;
#68966 = ORIENTED_EDGE ( 'NONE', *, *, #252765, .T. ) ;
#68967 = CARTESIAN_POINT ( 'NONE',  ( -20.85000000000000142, 11.75000000001115197, -93.71613433702194129 ) ) ;
#68968 = CARTESIAN_POINT ( 'NONE',  ( -21.14999999999999858, 64.25000000001269029, -203.5231074845244166 ) ) ;
#68970 = DIRECTION ( 'NONE',  ( 1.000000000000000000, -0.000000000000000000, -0.000000000000000000 ) ) ;
#68969 = DIRECTION ( 'NONE',  ( 0.000000000000000000, 0.000000000000000000, 1.000000000000000000 ) ) ;
#68971 = EDGE_CURVE ( 'NONE', #82535, #195496, #208203, .T. ) ;
#68972 = CARTESIAN_POINT ( 'NONE',  ( 20.95545211741311320, 39.25398227402024531, -236.7884260933929284 ) ) ;
#68973 = CARTESIAN_POINT ( 'NONE',  ( -20.54999999999999716, 68.85000000001186038, -90.67310748452435121 ) ) ;
#68974 = CARTESIAN_POINT ( 'NONE',  ( -23.25000000000000000, 11.75000000001115552, -100.5000000000000284 ) ) ;
#68975 = EDGE_CURVE ( 'NONE', #216709, #129965, #245704, .T. ) ;
#68976 = EDGE_CURVE ( 'NONE', #71999, #131991, #225710, .T. ) ;
#68977 = ORIENTED_EDGE ( 'NONE', *, *, #191899, .F. ) ;
#68978 = VERTEX_POINT ( 'NONE', #133776 ) ;
#68979 = CIRCLE ( 'NONE', #2286, 0.5000000000000004441 ) ;
#68980 = AXIS2_PLACEMENT_3D ( 'NONE', #155977, #219760, #198921 ) ;
#68981 = LINE ( 'NONE', #151067, #97006 ) ;
#68982 = ADVANCED_FACE ( 'NONE', ( #153391 ), #132460, .F. ) ;
#68983 = ORIENTED_EDGE ( 'NONE', *, *, #202132, .F. ) ;
#68984 = CARTESIAN_POINT ( 'NONE',  ( -20.54999999999999716, 7.150000000011155876, -121.6500000000000341 ) ) ;
#68985 = AXIS2_PLACEMENT_3D ( 'NONE', #41158, #4554, #200210 ) ;
#68986 = FACE_OUTER_BOUND ( 'NONE', #69369, .T. ) ;
#68987 = VECTOR ( 'NONE', #63930, 1000.000000000000000 ) ;
#68988 = EDGE_LOOP ( 'NONE', ( #248748, #148328, #51444, #30698 ) ) ;
#68989 = DIRECTION ( 'NONE',  ( -1.000000000000000000, -0.000000000000000000, -0.000000000000000000 ) ) ;
#68990 = EDGE_CURVE ( 'NONE', #169534, #142411, #249880, .T. ) ;
#68991 = ORIENTED_EDGE ( 'NONE', *, *, #150787, .T. ) ;
#68993 = AXIS2_PLACEMENT_3D ( 'NONE', #59128, #199976, #176565 ) ;
#68992 = CARTESIAN_POINT ( 'NONE',  ( 21.30000000000002558, 1.115650265596050101E-11, -71.05000000000003979 ) ) ;
#68995 = AXIS2_PLACEMENT_3D ( 'NONE', #161234, #4692, #62131 ) ;
#68994 = DIRECTION ( 'NONE',  ( 1.000000000000000000, 2.952720810173289112E-16, -0.000000000000000000 ) ) ;
#68996 = CARTESIAN_POINT ( 'NONE',  ( -18.35663730107557257, 64.52609257350039229, -60.27310748452440947 ) ) ;
#68997 = FACE_OUTER_BOUND ( 'NONE', #56444, .T. ) ;
#68998 = DIRECTION ( 'NONE',  ( 0.000000000000000000, -0.2128009952263485993, 0.9770955615653341697 ) ) ;
#68999 = AXIS2_PLACEMENT_3D ( 'NONE', #224103, #123740, #45475 ) ;
#69000 = CARTESIAN_POINT ( 'NONE',  ( -20.94999999999999929, 69.15387683765909799, -65.78538121767449809 ) ) ;
#69001 = LINE ( 'NONE', #205913, #28985 ) ;
#69003 = ORIENTED_EDGE ( 'NONE', *, *, #114407, .T. ) ;
#69002 = CARTESIAN_POINT ( 'NONE',  ( 18.43466021071417060, -0.7397809587360789640, -242.2185760212437629 ) ) ;
#69005 = CARTESIAN_POINT ( 'NONE',  ( 18.54999999999999716, 8.750000000011173285, -113.1500000000000341 ) ) ;
#69004 = LINE ( 'NONE', #144650, #236888 ) ;
#69006 = ORIENTED_EDGE ( 'NONE', *, *, #53151, .F. ) ;
#69008 = ORIENTED_EDGE ( 'NONE', *, *, #123801, .T. ) ;
#69007 = SPHERICAL_SURFACE ( 'NONE', #44349, 0.1000000000000000056 ) ;
#69009 = VERTEX_POINT ( 'NONE', #51645 ) ;
#69010 = CARTESIAN_POINT ( 'NONE',  ( -21.37071067811865532, 8.070710678129811910, -88.25000000000005684 ) ) ;
#69011 = DIRECTION ( 'NONE',  ( 1.000000000000000000, -0.000000000000000000, -0.000000000000000000 ) ) ;
#69012 = DIRECTION ( 'NONE',  ( -0.000000000000000000, -0.8814952561688432775, 0.4721928772777344019 ) ) ;
#69014 = FACE_OUTER_BOUND ( 'NONE', #7290, .T. ) ;
#69013 = CIRCLE ( 'NONE', #214720, 0.1000000000000028644 ) ;
#69015 = DIRECTION ( 'NONE',  ( 1.000000000000000000, 0.000000000000000000, 0.000000000000000000 ) ) ;
#69016 = DIRECTION ( 'NONE',  ( 1.000000000000000000, -3.469446951953718318E-14, 2.003086131649645455E-14 ) ) ;
#69017 = CARTESIAN_POINT ( 'NONE',  ( -16.77683809663752257, 51.60783545504968117, -231.9559722212415522 ) ) ;
#69018 = DIRECTION ( 'NONE',  ( 0.000000000000000000, 0.2617529984165024026, 0.9651348961777159730 ) ) ;
#69019 = ORIENTED_EDGE ( 'NONE', *, *, #16129, .F. ) ;
#69020 = VERTEX_POINT ( 'NONE', #111649 ) ;
#69021 = CARTESIAN_POINT ( 'NONE',  ( -21.05000000000000071, 30.43677443282725292, -239.5249545687858870 ) ) ;
#69022 = AXIS2_PLACEMENT_3D ( 'NONE', #74711, #56364, #52519 ) ;
#69023 = ORIENTED_EDGE ( 'NONE', *, *, #253975, .T. ) ;
#69024 = AXIS2_PLACEMENT_3D ( 'NONE', #34371, #14810, #177734 ) ;
#69025 = CARTESIAN_POINT ( 'NONE',  ( 20.94999999999999929, 79.19526988099229925, -196.1889237952725296 ) ) ;
#69026 = VERTEX_POINT ( 'NONE', #191220 ) ;
#69027 = DIRECTION ( 'NONE',  ( 0.000000000000000000, 0.000000000000000000, 1.000000000000000000 ) ) ;
#69028 = CARTESIAN_POINT ( 'NONE',  ( 21.00000000000000000, 9.749999999999998224, -21.15000000000000213 ) ) ;
#69029 = CARTESIAN_POINT ( 'NONE',  ( 20.94999999999999929, 77.16270174995010223, -128.6231074845242972 ) ) ;
#69030 = EDGE_CURVE ( 'NONE', #200569, #51404, #213305, .T. ) ;
#69031 = DIRECTION ( 'NONE',  ( -1.000000000000000000, 2.849773892568378313E-16, -7.728835255496647986E-17 ) ) ;
#69032 = DIRECTION ( 'NONE',  ( 1.000000000000000000, 1.186688945009010077E-16, 0.000000000000000000 ) ) ;
#69033 = ORIENTED_EDGE ( 'NONE', *, *, #237892, .F. ) ;
#69034 = B_SPLINE_CURVE_WITH_KNOTS ( 'NONE', 3,
 ( #61987, #25434, #64540, #82778, #202768, #24154, #224884, #81504, #205315, #184478, #85355, #101045, #5831, #244457, #46254, #219754, #22878, #103645, #7123, #159809, #141508, #183219, #239336, #164928, #65822, #144060 ),
 .UNSPECIFIED., .F., .F.,
 ( 4, 2, 2, 2, 2, 2, 2, 2, 2, 2, 2, 2, 4 ),
 ( 0.005476422646581339572, 0.006160811967703564394, 0.006845201288825788349, 0.007187395949386901628, 0.007529590609948013172, 0.007871785270509124716, 0.008213979931070237994, 0.008556174591631351273, 0.008898369252192462817, 0.009240563912753574360, 0.009582758573314687639, 0.01026714789443685175, 0.01095153721555902106 ),
 .UNSPECIFIED. ) ;
#69035 = CARTESIAN_POINT ( 'NONE',  ( -20.54999999999999716, 76.00000000001170974, -69.52310748452431710 ) ) ;
#69036 = EDGE_CURVE ( 'NONE', #11297, #24624, #222301, .T. ) ;
#69037 = EDGE_CURVE ( 'NONE', #185121, #3745, #231611, .T. ) ;
#69038 = CARTESIAN_POINT ( 'NONE',  ( -17.01473183483379970, 66.05000000001255955, -182.7731074845244734 ) ) ;
#69039 = DIRECTION ( 'NONE',  ( 0.000000000000000000, 0.000000000000000000, -1.000000000000000000 ) ) ;
#69040 = DIRECTION ( 'NONE',  ( 0.000000000000000000, -0.6728971962617102953, -0.7397360091702507301 ) ) ;
#69041 = ORIENTED_EDGE ( 'NONE', *, *, #223987, .F. ) ;
#69042 = AXIS2_PLACEMENT_3D ( 'NONE', #255776, #156752, #98001 ) ;
#69044 = LINE ( 'NONE', #28667, #235716 ) ;
#69043 = DIRECTION ( 'NONE',  ( 0.000000000000000000, 0.000000000000000000, -1.000000000000000000 ) ) ;
#69045 = ORIENTED_EDGE ( 'NONE', *, *, #138085, .F. ) ;
#69048 = ORIENTED_EDGE ( 'NONE', *, *, #138034, .T. ) ;
#69047 = CARTESIAN_POINT ( 'NONE',  ( -18.35668295345803713, 64.52683809664951298, -112.2731074845243739 ) ) ;
#69046 = DIRECTION ( 'NONE',  ( 1.000000000000000000, 0.000000000000000000, 0.000000000000000000 ) ) ;
#69049 = B_SPLINE_CURVE_WITH_KNOTS ( 'NONE', 3,
 ( #41687, #161643, #1235, #182482, #203316, #222863, #44247, #24702, #104189, #111933, #8961, #208469, #188884, #152355, #250143, #151049, #148478, #186323, #68959, #48081, #106762, #168081 ),
 .UNSPECIFIED., .F., .F.,
 ( 4, 3, 3, 3, 3, 3, 3, 4 ),
 ( 0.000000000000000000, 7.307836821080529321E-06, 4.161455748548037811E-05, 7.576591810648371868E-05, 0.0001098090429817550825, 0.0001438003617351050036, 0.0001777914035423659516, 0.0002117966137403016797 ),
 .UNSPECIFIED. ) ;
#69050 = ORIENTED_EDGE ( 'NONE', *, *, #250377, .F. ) ;
#69051 = CARTESIAN_POINT ( 'NONE',  ( -16.95709691156327992, 9.950000000011140600, -113.1600575625087117 ) ) ;
#69052 = DIRECTION ( 'NONE',  ( 1.000000000000000000, 0.000000000000000000, 0.000000000000000000 ) ) ;
#69053 = CYLINDRICAL_SURFACE ( 'NONE', #179169, 11.75000000000000178 ) ;
#69054 = AXIS2_PLACEMENT_3D ( 'NONE', #69935, #167755, #68636 ) ;
#69055 = EDGE_LOOP ( 'NONE', ( #148638, #3978, #192041, #4829 ) ) ;
#69056 = CARTESIAN_POINT ( 'NONE',  ( 11.60000000000000142, -8.250000000000005329, 15.00000000000000355 ) ) ;
#69057 = EDGE_CURVE ( 'NONE', #32249, #114550, #26728, .T. ) ;
#69058 = CARTESIAN_POINT ( 'NONE',  ( -18.79999999999999716, 1.410778198689825347, -7.973296578895943121 ) ) ;
#69060 = CYLINDRICAL_SURFACE ( 'NONE', #13350, 4.049999999999998046 ) ;
#69059 = CARTESIAN_POINT ( 'NONE',  ( -22.50000000000000000, 11.64987090376337875, 0.08251989087296193737 ) ) ;
#69062 = ORIENTED_EDGE ( 'NONE', *, *, #50886, .T. ) ;
#69061 = DIRECTION ( 'NONE',  ( 1.000000000000000000, 0.000000000000000000, 0.000000000000000000 ) ) ;
#69063 = ORIENTED_EDGE ( 'NONE', *, *, #183324, .F. ) ;
#69064 = CARTESIAN_POINT ( 'NONE',  ( 20.90000000000000213, 11.49641995933507843, 1.885425182446133885 ) ) ;
#69065 = CARTESIAN_POINT ( 'NONE',  ( -18.50000000000000000, -4.963776450181787148, -229.1688993039521449 ) ) ;
#69066 = VECTOR ( 'NONE', #216755, 1000.000000000000000 ) ;
#69067 = CARTESIAN_POINT ( 'NONE',  ( 23.14999999999999503, 11.65000000001116298, -79.15000000000004832 ) ) ;
#69068 = ORIENTED_EDGE ( 'NONE', *, *, #82356, .F. ) ;
#69069 = DIRECTION ( 'NONE',  ( 0.000000000000000000, 0.000000000000000000, -1.000000000000000000 ) ) ;
#69070 = EDGE_CURVE ( 'NONE', #201868, #182718, #49100, .T. ) ;
#69071 = DIRECTION ( 'NONE',  ( -1.000000000000000000, -3.265361837132813093E-16, 0.000000000000000000 ) ) ;
#69072 = DIRECTION ( 'NONE',  ( -1.000000000000000000, -2.885090398161910739E-16, -6.283419270304611573E-17 ) ) ;
#69073 = ADVANCED_FACE ( 'NONE', ( #256221 ), #219726, .T. ) ;
#69074 = EDGE_LOOP ( 'NONE', ( #50394, #78869, #237601, #145599 ) ) ;
#69075 = DIRECTION ( 'NONE',  ( 0.000000000000000000, 0.9942466578594195692, -0.1071148137998398919 ) ) ;
#69077 = EDGE_CURVE ( 'NONE', #68824, #95409, #78912, .T. ) ;
#69076 = ORIENTED_EDGE ( 'NONE', *, *, #158548, .T. ) ;
#69078 = DIRECTION ( 'NONE',  ( 0.000000000000000000, 0.2617529984165031243, 0.9651348961777157509 ) ) ;
#69079 = CYLINDRICAL_SURFACE ( 'NONE', #243921, 0.1000000000000028644 ) ;
#69080 = AXIS2_PLACEMENT_3D ( 'NONE', #124510, #129638, #89219 ) ;
#69081 = CIRCLE ( 'NONE', #60661, 0.09999999999999693856 ) ;
#69082 = AXIS2_PLACEMENT_3D ( 'NONE', #251556, #127778, #9108 ) ;
#69083 = ORIENTED_EDGE ( 'NONE', *, *, #101500, .F. ) ;
#69084 = ORIENTED_EDGE ( 'NONE', *, *, #143173, .T. ) ;
#69085 = FACE_OUTER_BOUND ( 'NONE', #17653, .T. ) ;
#69086 = VERTEX_POINT ( 'NONE', #95923 ) ;
#69088 = ORIENTED_EDGE ( 'NONE', *, *, #32016, .T. ) ;
#69087 = CARTESIAN_POINT ( 'NONE',  ( -21.12642695952773764, 6.375659922035164406, 0.09890328318936436602 ) ) ;
#69089 = EDGE_LOOP ( 'NONE', ( #101005, #211699, #8919, #141592, #105836 ) ) ;
#69092 = ADVANCED_FACE ( 'NONE', ( #17671 ), #257515, .T. ) ;
#69091 = ORIENTED_EDGE ( 'NONE', *, *, #96767, .T. ) ;
#69090 = ORIENTED_EDGE ( 'NONE', *, *, #106455, .F. ) ;
#69093 = CARTESIAN_POINT ( 'NONE',  ( -18.44204374631830134, -9.491036389587220512, -107.1262012702210455 ) ) ;
#69094 = ORIENTED_EDGE ( 'NONE', *, *, #127046, .T. ) ;
#69095 = CARTESIAN_POINT ( 'NONE',  ( -21.55000000000000426, 68.29142135624881860, -48.27310748452437394 ) ) ;
#69096 = CARTESIAN_POINT ( 'NONE',  ( -23.15000000000000213, 1.925233644870967487, -87.76975646687391475 ) ) ;
#69097 = VECTOR ( 'NONE', #206655, 1000.000000000000000 ) ;
#69098 = CARTESIAN_POINT ( 'NONE',  ( 18.59999999999999787, 11.75000000000000000, 6.000000000000001776 ) ) ;
#69099 = DIRECTION ( 'NONE',  ( -1.000000000000000000, -0.000000000000000000, -0.000000000000000000 ) ) ;
#69100 = CIRCLE ( 'NONE', #56415, 12.97499999999998366 ) ;
#69101 = VERTEX_POINT ( 'NONE', #176781 ) ;
#69102 = ORIENTED_EDGE ( 'NONE', *, *, #160379, .T. ) ;
#69103 = EDGE_CURVE ( 'NONE', #241932, #231975, #239100, .T. ) ;
#69104 = CARTESIAN_POINT ( 'NONE',  ( -23.15000000000000213, 74.00000000001151079, -48.74772940728643533 ) ) ;
#69106 = ORIENTED_EDGE ( 'NONE', *, *, #212081, .T. ) ;
#69105 = LINE ( 'NONE', #243863, #166026 ) ;
#69108 = DIRECTION ( 'NONE',  ( 0.000000000000000000, -0.2558827019434435912, 0.9667078373770033872 ) ) ;
#69107 = CIRCLE ( 'NONE', #27439, 0.1000000000000028644 ) ;
#69110 = ORIENTED_EDGE ( 'NONE', *, *, #205051, .T. ) ;
#69109 = DIRECTION ( 'NONE',  ( 1.000000000000000000, 0.000000000000000000, 0.000000000000000000 ) ) ;
#69111 = ORIENTED_EDGE ( 'NONE', *, *, #121247, .T. ) ;
#69112 = CARTESIAN_POINT ( 'NONE',  ( -18.50000000000000000, 66.65000000001229807, -157.6731074845244223 ) ) ;
#69113 = AXIS2_PLACEMENT_3D ( 'NONE', #113562, #54851, #176130 ) ;
#69114 = EDGE_CURVE ( 'NONE', #220040, #163227, #176571, .T. ) ;
#69115 = EDGE_CURVE ( 'NONE', #77390, #153546, #212794, .T. ) ;
#69116 = AXIS2_PLACEMENT_3D ( 'NONE', #28755, #127812, #67823 ) ;
#69117 = VERTEX_POINT ( 'NONE', #18957 ) ;
#69118 = CARTESIAN_POINT ( 'NONE',  ( -16.91256925476570672, 66.01426884188404642, -149.0554649955191735 ) ) ;
#69119 = CARTESIAN_POINT ( 'NONE',  ( 21.05000000000000071, 6.511710453938116316, -230.8991241839006534 ) ) ;
#69120 = EDGE_CURVE ( 'NONE', #179511, #11734, #22462, .T. ) ;
#69123 = ORIENTED_EDGE ( 'NONE', *, *, #21819, .F. ) ;
#69122 = ORIENTED_EDGE ( 'NONE', *, *, #154228, .T. ) ;
#69121 = CIRCLE ( 'NONE', #169100, 0.1000000000000028644 ) ;
#69124 = ORIENTED_EDGE ( 'NONE', *, *, #43435, .F. ) ;
#69126 = ADVANCED_FACE ( 'NONE', ( #175501 ), #55709, .T. ) ;
#69125 = CARTESIAN_POINT ( 'NONE',  ( -21.52071067811865746, 68.22071067813014622, -48.27310748452437394 ) ) ;
#69127 = ORIENTED_EDGE ( 'NONE', *, *, #232248, .T. ) ;
#69128 = VECTOR ( 'NONE', #82355, 1000.000000000000000 ) ;
#69129 = VERTEX_POINT ( 'NONE', #59338 ) ;
#69130 = CARTESIAN_POINT ( 'NONE',  ( -20.94999999999999929, 11.60000000001115161, -107.4282032302755852 ) ) ;
#69132 = EDGE_LOOP ( 'NONE', ( #39109, #11097, #136182, #121847 ) ) ;
#69131 = DIRECTION ( 'NONE',  ( 0.000000000000000000, -0.9126074666063769270, -0.4088369013363282733 ) ) ;
#69133 = LINE ( 'NONE', #148664, #115074 ) ;
#69134 = CIRCLE ( 'NONE', #160735, 0.1000000000000000056 ) ;
#69135 = EDGE_CURVE ( 'NONE', #237038, #118040, #60359, .T. ) ;
#69136 = AXIS2_PLACEMENT_3D ( 'NONE', #108359, #250421, #150067 ) ;
#69138 = CYLINDRICAL_SURFACE ( 'NONE', #148327, 0.09999999999999939493 ) ;
#69137 = CARTESIAN_POINT ( 'NONE',  ( 23.24999999999999645, 72.23597390491818260, -202.5022707907005497 ) ) ;
#69139 = CARTESIAN_POINT ( 'NONE',  ( -18.50000000000000000, 11.65000000001115588, -67.00000000000000000 ) ) ;
#69140 = FACE_OUTER_BOUND ( 'NONE', #137812, .T. ) ;
#69141 = EDGE_LOOP ( 'NONE', ( #57229, #14015, #123324 ) ) ;
#69142 = ORIENTED_EDGE ( 'NONE', *, *, #144515, .T. ) ;
#69143 = DIRECTION ( 'NONE',  ( 0.000000000000000000, 1.000000000000000000, 0.000000000000000000 ) ) ;
#69145 = EDGE_CURVE ( 'NONE', #21653, #55329, #76357, .T. ) ;
#69144 = CARTESIAN_POINT ( 'NONE',  ( -18.39418127959864790, 64.51609439831335635, -45.27310748452440947 ) ) ;
#69147 = EDGE_LOOP ( 'NONE', ( #490, #242180, #33112, #192003 ) ) ;
#69146 = B_SPLINE_CURVE_WITH_KNOTS ( 'NONE', 3,
 ( #160560, #41899, #49578, #127841, #187825, #87404, #206087, #245221 ),
 .UNSPECIFIED., .F., .F.,
 ( 4, 2, 2, 4 ),
 ( 0.000000000000000000, 9.550056980124257001E-05, 0.0001910011396024851400, 0.0003820022792049893620 ),
 .UNSPECIFIED. ) ;
#69148 = EDGE_CURVE ( 'NONE', #161999, #62202, #193315, .T. ) ;
#69149 = EDGE_CURVE ( 'NONE', #220754, #72588, #85334, .T. ) ;
#69150 = DIRECTION ( 'NONE',  ( 0.000000000000000000, -0.1350103645451835865, -0.9908441862701605762 ) ) ;
#69151 = ORIENTED_EDGE ( 'NONE', *, *, #111961, .F. ) ;
#69152 = ORIENTED_EDGE ( 'NONE', *, *, #181583, .F. ) ;
#69153 = EDGE_CURVE ( 'NONE', #176995, #132343, #143221, .T. ) ;
#69154 = CARTESIAN_POINT ( 'NONE',  ( -22.50000000000000000, 64.35000000001195986, -103.0231074845244024 ) ) ;
#69155 = DIRECTION ( 'NONE',  ( -1.000000000000000000, 0.000000000000000000, -0.000000000000000000 ) ) ;
#69156 = ORIENTED_EDGE ( 'NONE', *, *, #96598, .F. ) ;
#69157 = FACE_OUTER_BOUND ( 'NONE', #73942, .T. ) ;
#69158 = CARTESIAN_POINT ( 'NONE',  ( 21.05543885634738643, 8.775771046858691804, -112.6843844707147184 ) ) ;
#69160 = ORIENTED_EDGE ( 'NONE', *, *, #22886, .F. ) ;
#69159 = APPLICATION_CONTEXT ( 'automotive_design' ) ;
#69161 = DIRECTION ( 'NONE',  ( -1.000000000000000000, 0.000000000000000000, 0.000000000000000000 ) ) ;
#69162 = CARTESIAN_POINT ( 'NONE',  ( 21.05000000000000071, 1.115600667400684642E-11, -100.5000000000000426 ) ) ;
#69164 = DIRECTION ( 'NONE',  ( -1.000000000000000000, 0.000000000000000000, 0.000000000000000000 ) ) ;
#69163 = CARTESIAN_POINT ( 'NONE',  ( -21.05000000000000071, 1.162701749949165642, -75.00000000000004263 ) ) ;
#69165 = CARTESIAN_POINT ( 'NONE',  ( -23.15000000000000213, -11.39257802169451139, -97.42605042016811012 ) ) ;
#69166 = EDGE_CURVE ( 'NONE', #18425, #105519, #68223, .T. ) ;
#69167 = AXIS2_PLACEMENT_3D ( 'NONE', #149862, #228111, #132863 ) ;
#69168 = CARTESIAN_POINT ( 'NONE',  ( -23.25000000000000000, 1.115600667400684642E-11, -134.0000000000000284 ) ) ;
#69170 = EDGE_CURVE ( 'NONE', #123093, #3876, #102317, .T. ) ;
#69169 = DIRECTION ( 'NONE',  ( 0.000000000000000000, 0.000000000000000000, 1.000000000000000000 ) ) ;
#69171 = AXIS2_PLACEMENT_3D ( 'NONE', #1692, #126791, #42139 ) ;
#69172 = CARTESIAN_POINT ( 'NONE',  ( 23.25000000000000000, 69.45000000001157048, -57.17310748452436542 ) ) ;
#69173 = VECTOR ( 'NONE', #37418, 1000.000000000000000 ) ;
#69174 = AXIS2_PLACEMENT_3D ( 'NONE', #183216, #141506, #138901 ) ;
#69175 = EDGE_CURVE ( 'NONE', #40759, #228873, #130759, .T. ) ;
#69176 = ORIENTED_EDGE ( 'NONE', *, *, #61959, .F. ) ;
#69177 = CIRCLE ( 'NONE', #60743, 11.64999999999999325 ) ;
#69179 = ORIENTED_EDGE ( 'NONE', *, *, #40372, .F. ) ;
#69178 = EDGE_LOOP ( 'NONE', ( #76425, #216861, #101081, #167606, #27049 ) ) ;
#69180 = VERTEX_POINT ( 'NONE', #201450 ) ;
#69181 =( BOUNDED_SURFACE ( )  B_SPLINE_SURFACE ( 3, 2, ( 
 ( #38399, #94507, #134897 ),
 ( #98323, #56636, #177923 ),
 ( #60506, #175371, #257378 ),
 ( #78782, #40996, #59198 ),
 ( #138736, #218289, #219586 ),
 ( #119230, #194924, #214452 ) ),
 .UNSPECIFIED., .F., .F., .F. ) 
 B_SPLINE_SURFACE_WITH_KNOTS ( ( 4, 2, 4 ),
 ( 3, 3 ),
 ( 0.0001300404313046574028, 0.0003183318589266556425, 0.0005066232865486539364 ),
 ( 0.000000000000000000, 1.000000000000000000 ),
 .UNSPECIFIED. ) 
 GEOMETRIC_REPRESENTATION_ITEM ( )  RATIONAL_B_SPLINE_SURFACE ( (
 ( 1.000000000000000000, 0.7071067811865352493, 1.000000000000000000),
 ( 1.000000000000000000, 0.7625113560535959900, 1.000000000000000000),
 ( 1.000000000000000000, 0.8126073484694479321, 1.000000000000000000),
 ( 1.000000000000000000, 0.8923049332726290528, 1.000000000000000000),
 ( 1.000000000000000000, 0.9231914937774552410, 1.000000000000000000),
 ( 1.000000000000000000, 0.9238795325112713064, 1.000000000000000000) ) ) 
 REPRESENTATION_ITEM ( '' )  SURFACE ( )  );
#69182 = CYLINDRICAL_SURFACE ( 'NONE', #99310, 0.1000000000000124678 ) ;
#69183 = EDGE_CURVE ( 'NONE', #157880, #68456, #218218, .T. ) ;
#69184 = VECTOR ( 'NONE', #13329, 1000.000000000000000 ) ;
#69186 = DIRECTION ( 'NONE',  ( 2.952720810173289112E-16, -1.000000000000000000, 0.000000000000000000 ) ) ;
#69185 = CYLINDRICAL_SURFACE ( 'NONE', #41168, 0.1000000000000124678 ) ;
#69187 = ADVANCED_FACE ( 'NONE', ( #169758 ), #151641, .F. ) ;
#69188 = CARTESIAN_POINT ( 'NONE',  ( 23.14999999999999503, 64.35000000001197407, -115.1731074845243796 ) ) ;
#69189 = EDGE_LOOP ( 'NONE', ( #61424, #144326, #84576, #122176 ) ) ;
#69190 = CARTESIAN_POINT ( 'NONE',  ( -18.40000000000000213, 20.70659057908908096, -227.9750359040556873 ) ) ;
#69191 = ORIENTED_EDGE ( 'NONE', *, *, #45885, .F. ) ;
#69192 = CARTESIAN_POINT ( 'NONE',  ( -20.94999999999999929, 1.115600667400684642E-11, -167.4999999999999716 ) ) ;
#69193 = AXIS2_PLACEMENT_3D ( 'NONE', #192077, #13432, #154263 ) ;
#69194 = FACE_OUTER_BOUND ( 'NONE', #89985, .T. ) ;
#69195 = CARTESIAN_POINT ( 'NONE',  ( -21.04999999999998295, 1.543325666084004677, -230.7238449902075956 ) ) ;
#69196 = ORIENTED_EDGE ( 'NONE', *, *, #155085, .F. ) ;
#69197 = DIRECTION ( 'NONE',  ( 0.000000000000000000, 0.000000000000000000, -1.000000000000000000 ) ) ;
#69198 = CARTESIAN_POINT ( 'NONE',  ( -16.97683809663752186, 29.54312324717475136, -234.4517840742877013 ) ) ;
#69199 = ORIENTED_EDGE ( 'NONE', *, *, #30258, .F. ) ;
#69200 = EDGE_LOOP ( 'NONE', ( #73294, #80917, #43899, #105525 ) ) ;
#69201 = CARTESIAN_POINT ( 'NONE',  ( 18.50000000000000000, -9.399999999999998579, -6.999285677838848585 ) ) ;
#69202 = CARTESIAN_POINT ( 'NONE',  ( -22.37643362114956957, 0.4535211548021770844, -230.0445178328014606 ) ) ;
#69203 = AXIS2_PLACEMENT_3D ( 'NONE', #177195, #78050, #157642 ) ;
#69204 = LINE ( 'NONE', #7931, #127961 ) ;
#69205 = CARTESIAN_POINT ( 'NONE',  ( 21.14999999999999858, 11.65000000001115943, -33.60000000000000142 ) ) ;
#69206 = DIRECTION ( 'NONE',  ( 1.000000000000000000, 0.000000000000000000, 0.000000000000000000 ) ) ;
#69207 = DIRECTION ( 'NONE',  ( 1.000000000000000000, 0.000000000000000000, 0.000000000000000000 ) ) ;
#69208 = EDGE_LOOP ( 'NONE', ( #228431, #195043, #130396, #8316, #233271, #40362, #105056, #105214, #60410, #189327, #89773, #210410, #109340, #15652, #40397, #218545 ) ) ;
#69209 = FACE_OUTER_BOUND ( 'NONE', #4984, .T. ) ;
#69210 = CARTESIAN_POINT ( 'NONE',  ( 18.69999999999999929, -1.212568896937008089, -7.800000000000000711 ) ) ;
#69212 = FACE_OUTER_BOUND ( 'NONE', #154191, .T. ) ;
#69211 = CARTESIAN_POINT ( 'NONE',  ( -16.93433913041102912, 10.00597842153509376, -87.93536542739521167 ) ) ;
#69213 = DIRECTION ( 'NONE',  ( 1.000000000000000000, 0.000000000000000000, 0.000000000000000000 ) ) ;
#69214 = DIRECTION ( 'NONE',  ( 0.000000000000000000, 0.000000000000000000, 1.000000000000000000 ) ) ;
#69215 = EDGE_CURVE ( 'NONE', #236062, #30387, #130578, .T. ) ;
#69216 = CARTESIAN_POINT ( 'NONE',  ( 19.90000000000000924, 4.611773100472912112, 22.11686199900910665 ) ) ;
#69217 = CARTESIAN_POINT ( 'NONE',  ( -21.64999999999999858, 9.350000000011133849, -87.85000000000003695 ) ) ;
#69218 = CIRCLE ( 'NONE', #223118, 0.5000000000000013323 ) ;
#69221 = VERTEX_POINT ( 'NONE', #84025 ) ;
#69220 = AXIS2_PLACEMENT_3D ( 'NONE', #79068, #56928, #137767 ) ;
#69219 = CARTESIAN_POINT ( 'NONE',  ( 20.12500000000000000, 9.750000000011153745, -121.7500000000000426 ) ) ;
#69222 = EDGE_CURVE ( 'NONE', #116663, #202146, #105793, .T. ) ;
#69223 = AXIS2_PLACEMENT_3D ( 'NONE', #250498, #71890, #125438 ) ;
#69224 = AXIS2_PLACEMENT_3D ( 'NONE', #74703, #177643, #96753 ) ;
#69225 = CARTESIAN_POINT ( 'NONE',  ( -18.34374000495059676, 54.09900352584866567, -229.1663746252470446 ) ) ;
#69226 = FACE_OUTER_BOUND ( 'NONE', #242808, .T. ) ;
#69227 = AXIS2_PLACEMENT_3D ( 'NONE', #146149, #47036, #225664 ) ;
#69228 = EDGE_CURVE ( 'NONE', #75286, #222763, #39208, .T. ) ;
#69229 = AXIS2_PLACEMENT_3D ( 'NONE', #122753, #104422, #242668 ) ;
#69230 = VERTEX_POINT ( 'NONE', #141481 ) ;
#69231 = DIRECTION ( 'NONE',  ( 0.000000000000000000, -0.9908441862701596881, 0.1350103645451904977 ) ) ;
#69232 = PLANE ( 'NONE',  #166142 ) ;
#69233 = AXIS2_PLACEMENT_3D ( 'NONE', #147880, #207867, #108739 ) ;
#69234 = ORIENTED_EDGE ( 'NONE', *, *, #236942, .T. ) ;
#69236 = VERTEX_POINT ( 'NONE', #204021 ) ;
#69235 = DIRECTION ( 'NONE',  ( 0.000000000000000000, -0.2617529984165031243, -0.9651348961777157509 ) ) ;
#69237 = DIRECTION ( 'NONE',  ( 0.000000000000000000, 0.9999631594459055250, 0.008583690987131395445 ) ) ;
#69238 = DIRECTION ( 'NONE',  ( 1.000000000000000000, 2.952720810173289112E-16, -0.000000000000000000 ) ) ;
#69239 = ORIENTED_EDGE ( 'NONE', *, *, #206944, .T. ) ;
#69240 = APPLICATION_PROTOCOL_DEFINITION ( 'draft international standard', 'automotive_design', 1998, #37539 ) ;
#69241 = CARTESIAN_POINT ( 'NONE',  ( -20.91682497891422798, 65.67736539654923433, -63.96251168765719797 ) ) ;
#69242 = DIRECTION ( 'NONE',  ( -0.8660254037843746477, 0.000000000000000000, -0.5000000000001108003 ) ) ;
#69243 = CARTESIAN_POINT ( 'NONE',  ( -18.39999999999999858, 85.50000000001189449, -95.99103808782457747 ) ) ;
#69244 = ORIENTED_EDGE ( 'NONE', *, *, #138194, .F. ) ;
#69245 = CARTESIAN_POINT ( 'NONE',  ( 21.14999999999999858, 45.21086124044690280, -238.4331873168094091 ) ) ;
#69246 = CARTESIAN_POINT ( 'NONE',  ( -18.40000000000000213, 64.52683809664938508, -90.37310748452438247 ) ) ;
#69247 = VECTOR ( 'NONE', #200921, 1000.000000000000000 ) ;
#69248 = DIRECTION ( 'NONE',  ( -2.952720810173289112E-16, -1.000000000000000000, -6.982962677686266711E-15 ) ) ;
#69249 = ORIENTED_EDGE ( 'NONE', *, *, #40568, .F. ) ;
#69250 = ORIENTED_EDGE ( 'NONE', *, *, #208024, .F. ) ;
#69251 = CARTESIAN_POINT ( 'NONE',  ( 20.94999999999999574, 5.900000000011102586, -110.7190997646564483 ) ) ;
#69252 = EDGE_CURVE ( 'NONE', #134939, #197038, #150173, .T. ) ;
#69253 = FACE_OUTER_BOUND ( 'NONE', #68018, .T. ) ;
#69254 = FACE_OUTER_BOUND ( 'NONE', #44625, .T. ) ;
#69255 = FACE_OUTER_BOUND ( 'NONE', #75545, .T. ) ;
#69256 = EDGE_CURVE ( 'NONE', #226256, #219487, #205768, .T. ) ;
#69259 = CARTESIAN_POINT ( 'NONE',  ( 22.47110162079220785, -2.450980137404201731, -189.6107711856424203 ) ) ;
#69258 = CIRCLE ( 'NONE', #27589, 0.1000000000000185879 ) ;
#69257 = DIRECTION ( 'NONE',  ( -0.000000000000000000, -0.000000000000000000, 1.000000000000000000 ) ) ;
#69260 = FACE_OUTER_BOUND ( 'NONE', #67144, .T. ) ;
#69261 = DIRECTION ( 'NONE',  ( 0.000000000000000000, -0.8490545835447238510, -0.5283051335749973099 ) ) ;
#69262 = CARTESIAN_POINT ( 'NONE',  ( -18.40000000000000568, 46.93054509580812095, -255.3593361228640219 ) ) ;
#69263 = CIRCLE ( 'NONE', #165106, 0.09999999999999939493 ) ;
#69264 = AXIS2_PLACEMENT_3D ( 'NONE', #51742, #131301, #32232 ) ;
#69266 = ORIENTED_EDGE ( 'NONE', *, *, #78286, .T. ) ;
#69265 = DIRECTION ( 'NONE',  ( -0.000000000000000000, 0.1350103645451904977, 0.9908441862701597991 ) ) ;
#69267 = DIRECTION ( 'NONE',  ( 0.000000000000000000, -1.000000000000000000, 0.000000000000000000 ) ) ;
#69268 = CARTESIAN_POINT ( 'NONE',  ( -22.10000000000000497, 3.461118860469513336, 28.84309995045515507 ) ) ;
#69270 = CARTESIAN_POINT ( 'NONE',  ( -21.55000000000000071, 7.150000000011155876, -121.7500000000000426 ) ) ;
#69269 = DIRECTION ( 'NONE',  ( 1.000000000000000000, 0.000000000000000000, 0.000000000000000000 ) ) ;
#69271 =( BOUNDED_CURVE ( )  B_SPLINE_CURVE ( 3, ( #63108, #243039, #200072, #162248 ),
 .UNSPECIFIED., .F., .F. ) 
 B_SPLINE_CURVE_WITH_KNOTS ( ( 4, 4 ),
 ( 3.432212674861197854, 3.693332928900581624 ),
 .UNSPECIFIED. ) 
 CURVE ( )  GEOMETRIC_REPRESENTATION_ITEM ( )  RATIONAL_B_SPLINE_CURVE ( ( 1.000000000000000000, 0.9943260843901262636, 0.9943260843901262636, 1.000000000000000000 ) ) 
 REPRESENTATION_ITEM ( '' )  );
#69272 = EDGE_CURVE ( 'NONE', #59500, #194022, #128724, .T. ) ;
#69273 = ORIENTED_EDGE ( 'NONE', *, *, #57747, .T. ) ;
#69274 = DIRECTION ( 'NONE',  ( 2.952720810173289112E-16, -1.000000000000000000, 0.000000000000000000 ) ) ;
#69275 = CARTESIAN_POINT ( 'NONE',  ( 19.97071067695833690, 64.27928932305363219, -111.8468540517207117 ) ) ;
#69276 = DIRECTION ( 'NONE',  ( 1.000000000000000000, -0.000000000000000000, 0.000000000000000000 ) ) ;
#69277 = DIRECTION ( 'NONE',  ( 0.000000000000000000, 6.982962677686266711E-15, -1.000000000000000000 ) ) ;
#69278 = DIRECTION ( 'NONE',  ( 0.000000000000000000, 0.000000000000000000, 1.000000000000000000 ) ) ;
#69279 = EDGE_CURVE ( 'NONE', #235424, #164288, #70652, .T. ) ;
#69280 = VERTEX_POINT ( 'NONE', #145323 ) ;
#69281 = ORIENTED_EDGE ( 'NONE', *, *, #153128, .T. ) ;
#69282 = CARTESIAN_POINT ( 'NONE',  ( 20.95512820512820440, 67.12384868372375024, -90.87310748452436826 ) ) ;
#69283 = EDGE_CURVE ( 'NONE', #81676, #255363, #224860, .T. ) ;
#69284 = ORIENTED_EDGE ( 'NONE', *, *, #121148, .F. ) ;
#69285 = CARTESIAN_POINT ( 'NONE',  ( 21.05000000000000071, 65.27628289530437655, -95.35819391543677170 ) ) ;
#69286 = CIRCLE ( 'NONE', #214998, 0.09999999999999939493 ) ;
#69287 = ORIENTED_EDGE ( 'NONE', *, *, #100464, .T. ) ;
#69288 = CARTESIAN_POINT ( 'NONE',  ( 21.14999999999999858, 11.65000000000000391, -12.15000000000000036 ) ) ;
#69289 = AXIS2_PLACEMENT_3D ( 'NONE', #103942, #204340, #165228 ) ;
#69290 = DIRECTION ( 'NONE',  ( 1.000000000000000000, 0.000000000000000000, 0.000000000000000000 ) ) ;
#69292 = ORIENTED_EDGE ( 'NONE', *, *, #195152, .F. ) ;
#69291 = AXIS2_PLACEMENT_3D ( 'NONE', #123831, #45570, #188933 ) ;
#69293 = EDGE_CURVE ( 'NONE', #227995, #28763, #164090, .T. ) ;
#69294 = VECTOR ( 'NONE', #79233, 999.9999999999998863 ) ;
#69295 = DIRECTION ( 'NONE',  ( 0.000000000000000000, 6.982962677686266711E-15, -1.000000000000000000 ) ) ;
#69296 = AXIS2_PLACEMENT_3D ( 'NONE', #241971, #122030, #62065 ) ;
#69297 = CARTESIAN_POINT ( 'NONE',  ( -18.59999999999999787, 68.11287320386161070, -224.1382462126928488 ) ) ;
#69298 = CYLINDRICAL_SURFACE ( 'NONE', #133269, 0.1000000000000013933 ) ;
#69299 = LINE ( 'NONE', #246624, #234638 ) ;
#69300 = DIRECTION ( 'NONE',  ( -0.000000000000000000, 0.01283462868039629209, -0.9999176327611372095 ) ) ;
#69301 = CARTESIAN_POINT ( 'NONE',  ( -23.25000000000000000, 76.00000000001237765, -170.0231074845243597 ) ) ;
#69302 = VERTEX_POINT ( 'NONE', #81473 ) ;
#69304 = DIRECTION ( 'NONE',  ( 0.000000000000000000, 0.4646089985449745052, 0.8855159391400224678 ) ) ;
#69303 = CARTESIAN_POINT ( 'NONE',  ( 20.94999999999999929, -9.000000000000000000, -23.60603087734755690 ) ) ;
#69305 = ORIENTED_EDGE ( 'NONE', *, *, #104933, .T. ) ;
#69307 = ORIENTED_EDGE ( 'NONE', *, *, #206989, .F. ) ;
#69306 = DIRECTION ( 'NONE',  ( 1.000000000000000000, 0.000000000000000000, 0.000000000000000000 ) ) ;
#69308 = AXIS2_PLACEMENT_3D ( 'NONE', #115586, #238092, #16511 ) ;
#69309 = ORIENTED_EDGE ( 'NONE', *, *, #49354, .F. ) ;
#69310 = DIRECTION ( 'NONE',  ( 0.7071067811865493491, 0.6909108974501220191, 0.1504730267678052180 ) ) ;
#69311 = CIRCLE ( 'NONE', #252429, 0.2000000000000048683 ) ;
#69312 = CARTESIAN_POINT ( 'NONE',  ( 12.93279065517213766, 66.58230930894914934, -151.8815067877598608 ) ) ;
#69313 = VECTOR ( 'NONE', #120915, 999.9999999999998863 ) ;
#69314 = CARTESIAN_POINT ( 'NONE',  ( -20.94999999999999929, 6.846123162363745074, -171.2377262668498759 ) ) ;
#69315 = CARTESIAN_POINT ( 'NONE',  ( 20.95595624212458219, 65.37610879691791865, -128.8934745703975580 ) ) ;
#69316 = ORIENTED_EDGE ( 'NONE', *, *, #221565, .F. ) ;
#69317 = DIRECTION ( 'NONE',  ( 0.000000000000000000, -1.000000000000000000, 0.000000000000000000 ) ) ;
#69318 = CARTESIAN_POINT ( 'NONE',  ( 22.39999999999999503, 1.115600667400684642E-11, -126.2092204016266379 ) ) ;
#69319 = CIRCLE ( 'NONE', #31734, 0.1999999999999987899 ) ;
#69320 = ORIENTED_EDGE ( 'NONE', *, *, #212823, .F. ) ;
#69321 = CARTESIAN_POINT ( 'NONE',  ( -16.94275863006528482, 9.989496048678669027, -154.8916973820765861 ) ) ;
#69322 = VECTOR ( 'NONE', #235533, 1000.000000000000000 ) ;
#69323 = CARTESIAN_POINT ( 'NONE',  ( 20.95000000000000284, 16.98881331171930498, -224.4946931418895417 ) ) ;
#69324 = ORIENTED_EDGE ( 'NONE', *, *, #157483, .T. ) ;
#69325 = DIRECTION ( 'NONE',  ( 0.000000000000000000, -7.026728003956695223E-15, 1.000000000000000000 ) ) ;
#69326 = EDGE_CURVE ( 'NONE', #70529, #44319, #161060, .T. ) ;
#69327 = ORIENTED_EDGE ( 'NONE', *, *, #148271, .F. ) ;
#69328 = DIRECTION ( 'NONE',  ( 0.000000000000000000, 0.9651348961777189706, -0.2617529984164915779 ) ) ;
#69329 = ORIENTED_EDGE ( 'NONE', *, *, #48926, .T. ) ;
#69330 = DIRECTION ( 'NONE',  ( 1.000000000000000000, 0.000000000000000000, 0.000000000000000000 ) ) ;
#69331 = LINE ( 'NONE', #206265, #60691 ) ;
#69332 = CARTESIAN_POINT ( 'NONE',  ( 21.05000000000000071, 76.08561306081568887, -75.93686721833462627 ) ) ;
#69333 = EDGE_CURVE ( 'NONE', #123927, #181985, #197388, .T. ) ;
#69334 = CARTESIAN_POINT ( 'NONE',  ( 23.40000000000005187, 74.94272479589878344, -8.023107484524793165 ) ) ;
#69335 = AXIS2_PLACEMENT_3D ( 'NONE', #43704, #61989, #224886 ) ;
#69336 = AXIS2_PLACEMENT_3D ( 'NONE', #102690, #184815, #242219 ) ;
#69337 = EDGE_CURVE ( 'NONE', #9389, #74847, #89053, .T. ) ;
#69339 = EDGE_CURVE ( 'NONE', #133079, #78967, #35124, .T. ) ;
#69338 = AXIS2_PLACEMENT_3D ( 'NONE', #157384, #3058, #236876 ) ;
#69340 = TOROIDAL_SURFACE ( 'NONE', #240022, 0.4000000000000009104, 0.1000000000000000056 ) ;
#69341 = CARTESIAN_POINT ( 'NONE',  ( -21.05000000000000071, 1.115600667400684642E-11, -175.3999999999999773 ) ) ;
#69342 = CARTESIAN_POINT ( 'NONE',  ( 20.94999999999999574, 65.52661458509899717, -95.44445302027583011 ) ) ;
#69343 = ORIENTED_EDGE ( 'NONE', *, *, #84668, .T. ) ;
#69344 = DIRECTION ( 'NONE',  ( -1.000000000000000000, -2.952720810173289112E-16, 0.000000000000000000 ) ) ;
#69345 = EDGE_LOOP ( 'NONE', ( #221096, #8222, #251877, #137791 ) ) ;
#69347 = LINE ( 'NONE', #227106, #29619 ) ;
#69346 = DIRECTION ( 'NONE',  ( -1.000000000000000000, 1.646408749285562691E-14, 1.149681084847720908E-28 ) ) ;
#69348 = VECTOR ( 'NONE', #232980, 1000.000000000000000 ) ;
#69349 = ORIENTED_EDGE ( 'NONE', *, *, #56623, .F. ) ;
#69350 = DIRECTION ( 'NONE',  ( 1.000000000000000000, -3.265361837132813093E-16, -2.280189983783949500E-30 ) ) ;
#69351 = CARTESIAN_POINT ( 'NONE',  ( -20.85000000000000142, 7.783179459866048866, -245.3643104511423303 ) ) ;
#69352 = CYLINDRICAL_SURFACE ( 'NONE', #171005, 0.09999999999999691080 ) ;
#69353 = ORIENTED_EDGE ( 'NONE', *, *, #198549, .T. ) ;
#69355 = ORIENTED_EDGE ( 'NONE', *, *, #154632, .T. ) ;
#69354 = DIRECTION ( 'NONE',  ( 0.000000000000000000, 0.000000000000000000, 1.000000000000000000 ) ) ;
#69356 = EDGE_CURVE ( 'NONE', #29239, #5002, #43290, .T. ) ;
#69358 = CARTESIAN_POINT ( 'NONE',  ( 23.15000000000000213, 78.00142589229885459, -228.9845759368473637 ) ) ;
#69357 = VECTOR ( 'NONE', #226260, 1000.000000000000000 ) ;
#69359 = EDGE_CURVE ( 'NONE', #242362, #17438, #34945, .T. ) ;
#69361 = CARTESIAN_POINT ( 'NONE',  ( -16.94107738177415712, 65.98576071487597972, -190.9731074845244336 ) ) ;
#69360 = CARTESIAN_POINT ( 'NONE',  ( 23.14999999999999503, 11.65000000001116298, -45.65000000000000568 ) ) ;
#69362 = AXIS2_PLACEMENT_3D ( 'NONE', #192381, #57979, #187595 ) ;
#69364 = ORIENTED_EDGE ( 'NONE', *, *, #67864, .F. ) ;
#69363 = CARTESIAN_POINT ( 'NONE',  ( -16.87331047859649757, 9.950000000011138823, -154.8500000000000227 ) ) ;
#69365 = CIRCLE ( 'NONE', #56827, 0.1000000000000028644 ) ;
#69366 = ORIENTED_EDGE ( 'NONE', *, *, #231613, .F. ) ;
#69367 = DIRECTION ( 'NONE',  ( -0.000000000000000000, -0.000000000000000000, 1.000000000000000000 ) ) ;
#69368 = CARTESIAN_POINT ( 'NONE',  ( -21.05000000000000071, 46.59314322379660922, -243.1831726892433210 ) ) ;
#69369 = EDGE_LOOP ( 'NONE', ( #22012, #83508, #45741 ) ) ;
#69370 = DIRECTION ( 'NONE',  ( 0.000000000000000000, 0.000000000000000000, -1.000000000000000000 ) ) ;
#69371 = VERTEX_POINT ( 'NONE', #75766 ) ;
#69372 = ADVANCED_FACE ( 'NONE', ( #114880 ), #234829, .T. ) ;
#69373 = AXIS2_PLACEMENT_3D ( 'NONE', #84109, #46312, #164988 ) ;
#69375 = EDGE_CURVE ( 'NONE', #110098, #119594, #35384, .T. ) ;
#69374 = CARTESIAN_POINT ( 'NONE',  ( -18.46907102845854709, 85.47372736477545629, -29.34707274578775582 ) ) ;
#69376 = CARTESIAN_POINT ( 'NONE',  ( 21.14999999999999858, 0.000000000000000000, -12.15000000000000036 ) ) ;
#69377 = ADVANCED_FACE ( 'NONE', ( #112326 ), #250530, .F. ) ;
#69378 = VERTEX_POINT ( 'NONE', #151458 ) ;
#69379 = FACE_OUTER_BOUND ( 'NONE', #180669, .T. ) ;
#69380 = ORIENTED_EDGE ( 'NONE', *, *, #241422, .F. ) ;
#69381 = AXIS2_PLACEMENT_3D ( 'NONE', #51199, #130765, #210319 ) ;
#69382 = CIRCLE ( 'NONE', #15213, 0.1000000000000028644 ) ;
#69383 = CARTESIAN_POINT ( 'NONE',  ( 21.07928932188134397, 6.162520550847347955, -199.5566553493351307 ) ) ;
#69384 = CIRCLE ( 'NONE', #215122, 0.09999999999999108213 ) ;
#69385 = AXIS2_PLACEMENT_3D ( 'NONE', #199055, #200334, #21706 ) ;
#69386 = ORIENTED_EDGE ( 'NONE', *, *, #141157, .F. ) ;
#69387 = ORIENTED_EDGE ( 'NONE', *, *, #224295, .T. ) ;
#69388 = CARTESIAN_POINT ( 'NONE',  ( -21.05000000000000071, 60.94483358488582070, -234.0465764481390636 ) ) ;
#69389 = ADVANCED_FACE ( 'NONE', ( #190587 ), #233559, .T. ) ;
#69390 = EDGE_LOOP ( 'NONE', ( #5374, #5213, #69284, #237855 ) ) ;
#69391 = DIRECTION ( 'NONE',  ( 0.000000000000000000, -1.000000000000000000, -6.982962677686266711E-15 ) ) ;
#69392 = ORIENTED_EDGE ( 'NONE', *, *, #156373, .F. ) ;
#69394 = ORIENTED_EDGE ( 'NONE', *, *, #35605, .T. ) ;
#69393 = DIRECTION ( 'NONE',  ( 0.000000000000000000, -0.000000000000000000, 1.000000000000000000 ) ) ;
#69395 = DIRECTION ( 'NONE',  ( 0.000000000000000000, 0.000000000000000000, -1.000000000000000000 ) ) ;
#69396 = ORIENTED_EDGE ( 'NONE', *, *, #138889, .F. ) ;
#69397 = DIRECTION ( 'NONE',  ( 1.000000000000000000, 0.000000000000000000, 0.000000000000000000 ) ) ;
#69398 = VERTEX_POINT ( 'NONE', #210142 ) ;
#69402 = EDGE_CURVE ( 'NONE', #203889, #113415, #31026, .T. ) ;
#69401 = ORIENTED_EDGE ( 'NONE', *, *, #116113, .T. ) ;
#69400 = ORIENTED_EDGE ( 'NONE', *, *, #195611, .T. ) ;
#69399 = DIRECTION ( 'NONE',  ( -0.000000000000000000, 1.000000000000000000, 6.982962677686266711E-15 ) ) ;
#69403 = CARTESIAN_POINT ( 'NONE',  ( 20.94999999999999929, 71.00000000001180922, -81.42837350343744163 ) ) ;
#69404 = TOROIDAL_SURFACE ( 'NONE', #215133, 0.9750000000000019762, 0.1000000000000000056 ) ;
#69405 = DIRECTION ( 'NONE',  ( 1.000000000000000000, 0.000000000000000000, 0.000000000000000000 ) ) ;
#69406 = TOROIDAL_SURFACE ( 'NONE', #198557, 12.97499999999999787, 0.1000000000000000056 ) ;
#69407 = AXIS2_PLACEMENT_3D ( 'NONE', #180008, #202126, #1333 ) ;
#69408 = ORIENTED_EDGE ( 'NONE', *, *, #218311, .F. ) ;
#69409 = CIRCLE ( 'NONE', #98561, 0.2000000000000057288 ) ;
#69410 = EDGE_LOOP ( 'NONE', ( #244030, #60707, #186180, #69281 ) ) ;
#69411 = EDGE_CURVE ( 'NONE', #89282, #65312, #235007, .T. ) ;
#69412 = CARTESIAN_POINT ( 'NONE',  ( -21.07954640115405454, 69.67071230398777004, -203.5891151916643480 ) ) ;
#69413 = DIRECTION ( 'NONE',  ( 0.000000000000000000, 0.000000000000000000, -1.000000000000000000 ) ) ;
#69415 = ORIENTED_EDGE ( 'NONE', *, *, #195964, .T. ) ;
#69414 = DIRECTION ( 'NONE',  ( 2.952720810173289112E-16, -1.000000000000000000, 0.000000000000000000 ) ) ;
#69416 = ORIENTED_EDGE ( 'NONE', *, *, #68647, .F. ) ;
#69417 = DIRECTION ( 'NONE',  ( 1.000000000000000000, 0.000000000000000000, 0.000000000000000000 ) ) ;
#69418 = CARTESIAN_POINT ( 'NONE',  ( 21.72449340488910607, 10.28395627749111441, -20.84999999999999787 ) ) ;
#69420 = ORIENTED_EDGE ( 'NONE', *, *, #85633, .T. ) ;
#69419 = EDGE_CURVE ( 'NONE', #121003, #6765, #176750, .T. ) ;
#69421 = CARTESIAN_POINT ( 'NONE',  ( 18.49999999999999645, 18.11150788191476124, -237.7585516551410478 ) ) ;
#69422 = SPHERICAL_SURFACE ( 'NONE', #236575, 0.1000000000000000056 ) ;
#69423 = EDGE_CURVE ( 'NONE', #72990, #45011, #218403, .T. ) ;
#69424 = ORIENTED_EDGE ( 'NONE', *, *, #141188, .T. ) ;
#69426 = ORIENTED_EDGE ( 'NONE', *, *, #240656, .T. ) ;
#69425 = LINE ( 'NONE', #207653, #118055 ) ;
#69427 = CIRCLE ( 'NONE', #7042, 0.1000000000000072220 ) ;
#69428 = ADVANCED_FACE ( 'NONE', ( #176162 ), #133164, .F. ) ;
#69430 = ORIENTED_EDGE ( 'NONE', *, *, #56151, .F. ) ;
#69429 = ORIENTED_EDGE ( 'NONE', *, *, #164519, .T. ) ;
#69431 = ORIENTED_EDGE ( 'NONE', *, *, #150998, .T. ) ;
#69433 = EDGE_CURVE ( 'NONE', #218543, #249063, #226799, .T. ) ;
#69432 = CARTESIAN_POINT ( 'NONE',  ( 23.15000000000000213, 69.20602499728043711, -247.8456586332460176 ) ) ;
#69434 = ORIENTED_EDGE ( 'NONE', *, *, #162566, .F. ) ;
#69435 = ORIENTED_EDGE ( 'NONE', *, *, #141113, .T. ) ;
#69436 = CARTESIAN_POINT ( 'NONE',  ( -21.04999999999994387, 79.78873604695631627, -7.297728304630792806 ) ) ;
#69437 = ORIENTED_EDGE ( 'NONE', *, *, #208134, .T. ) ;
#69438 = CARTESIAN_POINT ( 'NONE',  ( -16.87036670365548474, 30.33914847462231279, -234.8334748671511818 ) ) ;
#69439 = CIRCLE ( 'NONE', #148538, 0.09999999999999939493 ) ;
#69440 = LINE ( 'NONE', #212795, #193957 ) ;
#69441 = ORIENTED_EDGE ( 'NONE', *, *, #188749, .F. ) ;
#69442 = EDGE_LOOP ( 'NONE', ( #166974, #207652, #147713, #168572 ) ) ;
#69443 = TOROIDAL_SURFACE ( 'NONE', #61032, 6.258578643762712446, 0.1000000000000000056 ) ;
#69444 = CYLINDRICAL_SURFACE ( 'NONE', #179615, 0.5000000000000004441 ) ;
#69445 = ORIENTED_EDGE ( 'NONE', *, *, #219405, .T. ) ;
#69446 = CIRCLE ( 'NONE', #161019, 7.799999999999998046 ) ;
#69447 = CIRCLE ( 'NONE', #173540, 0.1999999999999987899 ) ;
#69448 = EDGE_CURVE ( 'NONE', #64660, #49254, #85115, .T. ) ;
#69449 = ADVANCED_FACE ( 'NONE', ( #17085 ), #97588, .T. ) ;
#69450 = AXIS2_PLACEMENT_3D ( 'NONE', #117640, #197165, #18547 ) ;
#69451 = CARTESIAN_POINT ( 'NONE',  ( 18.59999999999998721, 6.846123162363745074, -70.73772626684986164 ) ) ;
#69452 = VERTEX_POINT ( 'NONE', #255621 ) ;
#69453 = EDGE_CURVE ( 'NONE', #128224, #200640, #83424, .T. ) ;
#69454 = DIRECTION ( 'NONE',  ( 0.000000000000000000, 1.000000000000000000, 0.000000000000000000 ) ) ;
#69456 = VERTEX_POINT ( 'NONE', #221662 ) ;
#69455 = DIRECTION ( 'NONE',  ( 3.265361837132813093E-16, 1.000000000000000000, 6.982962677686266711E-15 ) ) ;
#69457 = CARTESIAN_POINT ( 'NONE',  ( -20.94999999999999929, 74.83729825007408465, -128.4231074845243086 ) ) ;
#69458 = CARTESIAN_POINT ( 'NONE',  ( 20.94999999999999574, 64.37928932189353759, -143.3915241368653994 ) ) ;
#69459 = CARTESIAN_POINT ( 'NONE',  ( -16.91049119928365485, 12.40728329596000989, -211.2118950959028041 ) ) ;
#69460 = LINE ( 'NONE', #70755, #106875 ) ;
#69461 = CARTESIAN_POINT ( 'NONE',  ( -23.15000000000000213, 76.00000000001170974, -69.52310748452431710 ) ) ;
#69462 = CARTESIAN_POINT ( 'NONE',  ( 18.59999999999999076, 77.25000000001232081, -162.0231074845243313 ) ) ;
#69463 = CARTESIAN_POINT ( 'NONE',  ( -21.05000000000000426, 6.270085863700296080, -33.46513199698689078 ) ) ;
#69464 = CARTESIAN_POINT ( 'NONE',  ( 18.40916198585718888, 37.99112793787836750, -261.0419301676770374 ) ) ;
#69465 = DIRECTION ( 'NONE',  ( 0.000000000000000000, 0.4930308989875575865, 0.8700118002898125091 ) ) ;
#69466 = EDGE_CURVE ( 'NONE', #108089, #156778, #210072, .T. ) ;
#69467 = VECTOR ( 'NONE', #94231, 1000.000000000000000 ) ;
#69468 = VERTEX_POINT ( 'NONE', #78305 ) ;
#69469 = AXIS2_PLACEMENT_3D ( 'NONE', #163345, #180337, #38260 ) ;
#69470 = EDGE_CURVE ( 'NONE', #81117, #216222, #68403, .T. ) ;
#69472 = EDGE_LOOP ( 'NONE', ( #36635, #173422, #81213, #145850, #46826 ) ) ;
#69471 = CIRCLE ( 'NONE', #190276, 11.74999999999999645 ) ;
#69474 = EDGE_LOOP ( 'NONE', ( #189758, #240484, #201227, #132672 ) ) ;
#69473 = DIRECTION ( 'NONE',  ( -1.000000000000000000, 3.854941057726231589E-15, 1.927470528863115795E-15 ) ) ;
#69475 = CIRCLE ( 'NONE', #215201, 4.049999999999998046 ) ;
#69476 = ORIENTED_EDGE ( 'NONE', *, *, #246668, .T. ) ;
#69477 = CARTESIAN_POINT ( 'NONE',  ( -23.25000000000000000, 85.00000000001197975, -112.9170766071766820 ) ) ;
#69478 = CARTESIAN_POINT ( 'NONE',  ( -20.85000000000000142, 42.96960653111219131, -254.4772109693542745 ) ) ;
#69479 = AXIS2_PLACEMENT_3D ( 'NONE', #238010, #120668, #1957 ) ;
#69481 = CARTESIAN_POINT ( 'NONE',  ( -18.39999999999999858, 85.60000000001187459, -96.42291809330220076 ) ) ;
#69480 = CARTESIAN_POINT ( 'NONE',  ( 21.14999999999999858, 65.28660755661270798, -191.1731074845244223 ) ) ;
#69482 = EDGE_CURVE ( 'NONE', #89147, #124932, #139558, .T. ) ;
#69483 = ORIENTED_EDGE ( 'NONE', *, *, #136797, .F. ) ;
#69484 = ORIENTED_EDGE ( 'NONE', *, *, #20306, .T. ) ;
#69485 = CARTESIAN_POINT ( 'NONE',  ( -20.94999999999999929, -11.64999999998884483, -103.5000000000000426 ) ) ;
#69486 = CARTESIAN_POINT ( 'NONE',  ( -23.25000000000000000, 4.150000000011156764, -121.7500000000000426 ) ) ;
#69487 = EDGE_LOOP ( 'NONE', ( #193440, #106287, #177909, #171319 ) ) ;
#69488 = ORIENTED_EDGE ( 'NONE', *, *, #166570, .F. ) ;
#69489 = FACE_OUTER_BOUND ( 'NONE', #39197, .T. ) ;
#69490 = CARTESIAN_POINT ( 'NONE',  ( -16.85939591225059075, 9.905226478399006496, -180.4600682464689783 ) ) ;
#69491 = AXIS2_PLACEMENT_3D ( 'NONE', #160910, #180462, #85167 ) ;
#69492 = DIRECTION ( 'NONE',  ( 0.000000000000000000, -1.000000000000000000, 0.000000000000000000 ) ) ;
#69493 = CARTESIAN_POINT ( 'NONE',  ( -23.25000000000000000, 4.350000000011156054, -155.1500000000000057 ) ) ;
#69494 = AXIS2_PLACEMENT_3D ( 'NONE', #4470, #64465, #200119 ) ;
#69495 = ADVANCED_FACE ( 'NONE', ( #58728 ), #105975, .F. ) ;
#69496 = CARTESIAN_POINT ( 'NONE',  ( -20.94999999999999929, 64.25000000001232081, -163.0083017138704236 ) ) ;
#69498 = ORIENTED_EDGE ( 'NONE', *, *, #144208, .F. ) ;
#69497 = CARTESIAN_POINT ( 'NONE',  ( -20.85000000000000142, -1.164121893230052995, -74.91484808557160591 ) ) ;
#69500 = CARTESIAN_POINT ( 'NONE',  ( 23.14999999999999503, 64.35000000001218723, -143.5379132551783812 ) ) ;
#69499 = B_SPLINE_CURVE_WITH_KNOTS ( 'NONE', 3,
 ( #182903, #48507, #22544, #4231, #204994, #143751, #104598, #105887, #223281, #124212 ),
 .UNSPECIFIED., .F., .F.,
 ( 4, 3, 3, 4 ),
 ( 0.000000000000000000, 4.874959354401679605E-05, 9.785140065121436244E-05, 0.0001360444631935818385 ),
 .UNSPECIFIED. ) ;
#69501 = LINE ( 'NONE', #109870, #39823 ) ;
#69502 = DIRECTION ( 'NONE',  ( 0.000000000000000000, -1.000000000000000000, 0.000000000000000000 ) ) ;
#69503 = CARTESIAN_POINT ( 'NONE',  ( -18.59999999999999787, 61.95000000001234497, -164.5094124137634708 ) ) ;
#69504 = ORIENTED_EDGE ( 'NONE', *, *, #89513, .F. ) ;
#69505 = FACE_OUTER_BOUND ( 'NONE', #191293, .T. ) ;
#69506 = DIRECTION ( 'NONE',  ( 0.000000000000000000, -1.000000000000000000, 0.000000000000000000 ) ) ;
#69508 = CARTESIAN_POINT ( 'NONE',  ( -18.59999999999999787, 1.115600667400684642E-11, -108.4000000000000483 ) ) ;
#69507 = DIRECTION ( 'NONE',  ( 1.000000000000000000, 0.000000000000000000, 0.000000000000000000 ) ) ;
#69509 = DIRECTION ( 'NONE',  ( 0.000000000000000000, 0.9126074666063769270, 0.4088369013363280513 ) ) ;
#69510 = CARTESIAN_POINT ( 'NONE',  ( -16.77683809663752257, 30.19206623356022234, -234.8041291499450551 ) ) ;
#69511 = VECTOR ( 'NONE', #79696, 1000.000000000000000 ) ;
#69512 = CARTESIAN_POINT ( 'NONE',  ( -21.04999999999994387, 64.35000000001120668, -5.923107484524795296 ) ) ;
#69513 = DIRECTION ( 'NONE',  ( 0.000000000000000000, -0.000000000000000000, -1.000000000000000000 ) ) ;
#69514 = CARTESIAN_POINT ( 'NONE',  ( 18.60000000000000142, 85.32100840337338354, -129.2871692354463278 ) ) ;
#69515 = CARTESIAN_POINT ( 'NONE',  ( -21.14999999999999858, 69.45934304831089889, -136.5231074845243313 ) ) ;
#69516 = EDGE_LOOP ( 'NONE', ( #114174, #65453, #218884, #103061 ) ) ;
#69517 = ORIENTED_EDGE ( 'NONE', *, *, #150293, .T. ) ;
#69518 = ORIENTED_EDGE ( 'NONE', *, *, #60861, .F. ) ;
#69519 = EDGE_CURVE ( 'NONE', #169135, #194066, #185766, .T. ) ;
#69520 = CARTESIAN_POINT ( 'NONE',  ( 20.19326291201646129, 65.84393901210796685, -95.26124567692161804 ) ) ;
#69521 = CARTESIAN_POINT ( 'NONE',  ( -18.50000000000000000, 5.341242990002803559, -157.6933497935119419 ) ) ;
#69522 = VERTEX_POINT ( 'NONE', #242526 ) ;
#69523 = CIRCLE ( 'NONE', #215251, 0.09999999999998715472 ) ;
#69524 = VERTEX_POINT ( 'NONE', #120048 ) ;
#69525 = CIRCLE ( 'NONE', #132047, 2.000000000000001776 ) ;
#69526 = ADVANCED_FACE ( 'NONE', ( #101699 ), #68599, .T. ) ;
#69527 = ORIENTED_EDGE ( 'NONE', *, *, #98543, .F. ) ;
#69528 = CARTESIAN_POINT ( 'NONE',  ( 21.05000000000000071, 75.90220970870277029, -109.2809220950058346 ) ) ;
#69529 = ORIENTED_EDGE ( 'NONE', *, *, #174506, .F. ) ;
#69530 = VECTOR ( 'NONE', #113362, 1000.000000000000000 ) ;
#69531 = DIRECTION ( 'NONE',  ( 0.000000000000000000, -1.000000000000000000, 0.000000000000000000 ) ) ;
#69532 = DIRECTION ( 'NONE',  ( 1.000000000000000000, 0.000000000000000000, 0.000000000000000000 ) ) ;
#69533 = DIRECTION ( 'NONE',  ( 1.000000000000000000, 0.000000000000000000, 0.000000000000000000 ) ) ;
#69534 = DIRECTION ( 'NONE',  ( 0.000000000000000000, 0.9915357197604792727, -0.1298341882520475943 ) ) ;
#69535 = CARTESIAN_POINT ( 'NONE',  ( -23.25000000000000355, 11.75000000001113953, -76.25000000000004263 ) ) ;
#69537 = ORIENTED_EDGE ( 'NONE', *, *, #177970, .F. ) ;
#69536 = DIRECTION ( 'NONE',  ( 0.000000000000000000, 0.000000000000000000, 1.000000000000000000 ) ) ;
#69539 = PLANE ( 'NONE',  #237615 ) ;
#69538 = DIRECTION ( 'NONE',  ( -1.000000000000000000, -2.952720810173289112E-16, 0.000000000000000000 ) ) ;
#69540 = CARTESIAN_POINT ( 'NONE',  ( -16.92209698673574181, 9.949999999999983302, -20.78936443294790237 ) ) ;
#69541 = CIRCLE ( 'NONE', #161106, 0.09999999999999230338 ) ;
#69542 = ORIENTED_EDGE ( 'NONE', *, *, #68522, .F. ) ;
#69543 = DIRECTION ( 'NONE',  ( 1.000000000000000000, 0.000000000000000000, 0.000000000000000000 ) ) ;
#69544 = CARTESIAN_POINT ( 'NONE',  ( -13.22483237240078857, 9.436674251854006101, -115.6768619309992658 ) ) ;
#69545 = CARTESIAN_POINT ( 'NONE',  ( -20.64999999999999858, 71.75000000001156764, -57.17310748452435121 ) ) ;
#69546 = ORIENTED_EDGE ( 'NONE', *, *, #21054, .F. ) ;
#69547 = AXIS2_PLACEMENT_3D ( 'NONE', #253001, #95218, #73125 ) ;
#69548 = CARTESIAN_POINT ( 'NONE',  ( 20.94999999999999574, 1.250000000011155299, -74.90000000000004832 ) ) ;
#69549 = CARTESIAN_POINT ( 'NONE',  ( -22.94999999999999929, 6.841561409100513025, 9.675512259591560138 ) ) ;
#69550 = EDGE_LOOP ( 'NONE', ( #11944, #114245, #199166, #119790, #5291 ) ) ;
#69551 = CARTESIAN_POINT ( 'NONE',  ( 23.14999999999999858, 1.115600667400684642E-11, -67.00000000000000000 ) ) ;
#69552 = DIRECTION ( 'NONE',  ( 0.000000000000000000, -0.1575844902526687130, -0.9875055080513762684 ) ) ;
#69553 = DIRECTION ( 'NONE',  ( 0.000000000000000000, 0.000000000000000000, -1.000000000000000000 ) ) ;
#69554 = CARTESIAN_POINT ( 'NONE',  ( 20.94999999999999929, -8.730841121484171907, -76.59807471898437825 ) ) ;
#69555 = ORIENTED_EDGE ( 'NONE', *, *, #157157, .T. ) ;
#69556 = ORIENTED_EDGE ( 'NONE', *, *, #48663, .F. ) ;
#69557 = ADVANCED_FACE ( 'NONE', ( #138271 ), #251752, .T. ) ;
#69558 = DIRECTION ( 'NONE',  ( 1.000000000000000000, 0.000000000000000000, 0.000000000000000000 ) ) ;
#69559 = DIRECTION ( 'NONE',  ( 0.000000000000000000, 0.000000000000000000, 1.000000000000000000 ) ) ;
#69560 = FACE_OUTER_BOUND ( 'NONE', #120877, .T. ) ;
#69562 = DIRECTION ( 'NONE',  ( 0.000000000000000000, 0.000000000000000000, 1.000000000000000000 ) ) ;
#69561 = DIRECTION ( 'NONE',  ( -1.073024830501117725E-15, 0.000000000000000000, -1.000000000000000000 ) ) ;
#69563 = AXIS2_PLACEMENT_3D ( 'NONE', #192052, #77203, #75938 ) ;
#69564 = CIRCLE ( 'NONE', #19499, 2.100000000000004530 ) ;
#69565 = FACE_OUTER_BOUND ( 'NONE', #154198, .T. ) ;
#69567 = AXIS2_PLACEMENT_3D ( 'NONE', #215571, #197294, #55183 ) ;
#69566 = CARTESIAN_POINT ( 'NONE',  ( 20.94999999999999929, 74.16465844978819177, -191.9679561919613775 ) ) ;
#69568 = VECTOR ( 'NONE', #144188, 1000.000000000000000 ) ;
#69569 = DIRECTION ( 'NONE',  ( 0.000000000000000000, -6.454785026890510900E-15, 1.000000000000000000 ) ) ;
#69570 = VERTEX_POINT ( 'NONE', #80867 ) ;
#69571 = CARTESIAN_POINT ( 'NONE',  ( -21.65000000000000213, 9.950000000011138823, -46.25000000000000711 ) ) ;
#69572 = ORIENTED_EDGE ( 'NONE', *, *, #62482, .F. ) ;
#69573 = CARTESIAN_POINT ( 'NONE',  ( 18.39999999999999503, 11.47316190337363828, -158.2500000000000284 ) ) ;
#69574 = DIRECTION ( 'NONE',  ( 0.7071067811865463515, -0.7071067811865487940, 0.000000000000000000 ) ) ;
#69575 = DIRECTION ( 'NONE',  ( 0.000000000000000000, 0.000000000000000000, -1.000000000000000000 ) ) ;
#69576 = CARTESIAN_POINT ( 'NONE',  ( -16.87333278164142669, 66.11739021543317563, -123.3899396783716895 ) ) ;
#69577 = EDGE_CURVE ( 'NONE', #203988, #1139, #18521, .T. ) ;
#69578 = DIRECTION ( 'NONE',  ( -1.000000000000000000, -0.000000000000000000, -0.000000000000000000 ) ) ;
#69580 = ORIENTED_EDGE ( 'NONE', *, *, #119522, .F. ) ;
#69579 = CARTESIAN_POINT ( 'NONE',  ( 21.05000000000000071, 69.38854649060171198, -247.7638912529787376 ) ) ;
#69581 = FACE_OUTER_BOUND ( 'NONE', #127524, .T. ) ;
#69582 = CARTESIAN_POINT ( 'NONE',  ( -18.50000000000000000, 65.70711192142420032, -164.5651054685122574 ) ) ;
#69583 = DIRECTION ( 'NONE',  ( 0.000000000000000000, 0.000000000000000000, 1.000000000000000000 ) ) ;
#69584 = CARTESIAN_POINT ( 'NONE',  ( 18.49999999999999645, 43.08613539620618837, -254.3146655184800409 ) ) ;
#69585 = EDGE_CURVE ( 'NONE', #49440, #49697, #155910, .T. ) ;
#69586 = ORIENTED_EDGE ( 'NONE', *, *, #181630, .F. ) ;
#69587 = CARTESIAN_POINT ( 'NONE',  ( -15.75000000000000355, 66.65000000001229807, -153.1588398769083028 ) ) ;
#69588 = ORIENTED_EDGE ( 'NONE', *, *, #234361, .T. ) ;
#69589 = VECTOR ( 'NONE', #197170, 1000.000000000000000 ) ;
#69590 = AXIS2_PLACEMENT_3D ( 'NONE', #211610, #92922, #9538 ) ;
#69592 = VECTOR ( 'NONE', #82968, 1000.000000000000000 ) ;
#69591 = DIRECTION ( 'NONE',  ( 0.000000000000000000, 0.8814952561688430555, -0.4721928772777346239 ) ) ;
#69593 = ADVANCED_FACE ( 'NONE', ( #122602 ), #199582, .T. ) ;
#69594 = ORIENTED_EDGE ( 'NONE', *, *, #219815, .F. ) ;
#69595 = FACE_OUTER_BOUND ( 'NONE', #135083, .T. ) ;
#69596 = ORIENTED_EDGE ( 'NONE', *, *, #172612, .F. ) ;
#69598 = DIRECTION ( 'NONE',  ( 0.000000000000000000, 0.000000000000000000, -1.000000000000000000 ) ) ;
#69597 = CIRCLE ( 'NONE', #32183, 11.89999999999999858 ) ;
#69599 = CARTESIAN_POINT ( 'NONE',  ( -18.50000000000000000, 8.980461154494397746, -187.0187154576991304 ) ) ;
#69600 = DIRECTION ( 'NONE',  ( 0.000000000000000000, 0.000000000000000000, -1.000000000000000000 ) ) ;
#69601 = ORIENTED_EDGE ( 'NONE', *, *, #82564, .T. ) ;
#69602 = EDGE_CURVE ( 'NONE', #79411, #98538, #197569, .T. ) ;
#69603 = CARTESIAN_POINT ( 'NONE',  ( -16.87998658237743754, 9.949999999999985079, -12.86363956773800510 ) ) ;
#69604 = ADVANCED_FACE ( 'NONE', ( #117457 ), #182579, .T. ) ;
#69605 = CARTESIAN_POINT ( 'NONE',  ( -21.22070241538126112, 6.300705718653867748, -199.5265356483836570 ) ) ;
#69606 = DIRECTION ( 'NONE',  ( 0.000000000000000000, 1.000000000000000000, 0.000000000000000000 ) ) ;
#69607 = CARTESIAN_POINT ( 'NONE',  ( 18.59999999999996945, 10.33248238083634440, -72.59484654391314962 ) ) ;
#69608 = AXIS2_PLACEMENT_3D ( 'NONE', #46034, #107295, #162160 ) ;
#69609 = LINE ( 'NONE', #126997, #107338 ) ;
#69610 = ORIENTED_EDGE ( 'NONE', *, *, #131174, .F. ) ;
#69612 = ORIENTED_EDGE ( 'NONE', *, *, #170920, .T. ) ;
#69611 = DIRECTION ( 'NONE',  ( 1.000000000000000000, 0.000000000000000000, 0.000000000000000000 ) ) ;
#69613 = ORIENTED_EDGE ( 'NONE', *, *, #74716, .F. ) ;
#69614 = DIRECTION ( 'NONE',  ( 1.000000000000000000, 0.000000000000000000, 0.000000000000000000 ) ) ;
#69615 = ORIENTED_EDGE ( 'NONE', *, *, #28836, .F. ) ;
#69616 = CARTESIAN_POINT ( 'NONE',  ( -1.739115166359751801E-14, 64.35000000001230092, -157.7731074845244450 ) ) ;
#69617 = CARTESIAN_POINT ( 'NONE',  ( -23.15000000000000213, 6.683038871553167226, -212.1840060551439819 ) ) ;
#69618 = CARTESIAN_POINT ( 'NONE',  ( -18.50000000000000000, 31.94635157770352052, -238.7871412784868994 ) ) ;
#69619 = ORIENTED_EDGE ( 'NONE', *, *, #148272, .F. ) ;
#69620 = DIRECTION ( 'NONE',  ( 0.000000000000000000, 0.000000000000000000, 1.000000000000000000 ) ) ;
#69621 = CARTESIAN_POINT ( 'NONE',  ( 22.47071067811865319, 67.23127455305841238, -235.8551265064783991 ) ) ;
#69622 = AXIS2_PLACEMENT_3D ( 'NONE', #45165, #64728, #184669 ) ;
#69623 = DIRECTION ( 'NONE',  ( 0.000000000000000000, 0.000000000000000000, -1.000000000000000000 ) ) ;
#69624 = VERTEX_POINT ( 'NONE', #140871 ) ;
#69625 = EDGE_CURVE ( 'NONE', #36331, #190169, #22638, .T. ) ;
#69627 = ORIENTED_EDGE ( 'NONE', *, *, #8930, .F. ) ;
#69626 = DIRECTION ( 'NONE',  ( 0.8049926720990051576, -0.5932847527679298016, -4.142885285818778274E-15 ) ) ;
#69628 = CARTESIAN_POINT ( 'NONE',  ( 18.59999999999999076, 69.45000000001199680, -115.2731074845243455 ) ) ;
#69629 = FACE_OUTER_BOUND ( 'NONE', #148466, .T. ) ;
#69630 = AXIS2_PLACEMENT_3D ( 'NONE', #39790, #201388, #118003 ) ;
#69631 = TOROIDAL_SURFACE ( 'NONE', #240306, 0.2000000000000000111, 0.1000000000000000056 ) ;
#69632 = AXIS2_PLACEMENT_3D ( 'NONE', #60437, #20057, #237809 ) ;
#69633 = ORIENTED_EDGE ( 'NONE', *, *, #63496, .T. ) ;
#69635 = CARTESIAN_POINT ( 'NONE',  ( -20.94999999999999929, 87.75000000001212186, -133.6231074845242119 ) ) ;
#69634 = PRODUCT_DEFINITION_FORMATION_WITH_SPECIFIED_SOURCE ( 'ANY', '', #70236, .NOT_KNOWN. ) ;
#69637 = EDGE_CURVE ( 'NONE', #26511, #235569, #161739, .T. ) ;
#69636 = CARTESIAN_POINT ( 'NONE',  ( -17.27223548805945086, 42.80240007841014460, -235.4628745677799202 ) ) ;
#69638 = CARTESIAN_POINT ( 'NONE',  ( -23.15000000000000213, 86.43238724539048690, -209.5644480942280836 ) ) ;
#69640 = ORIENTED_EDGE ( 'NONE', *, *, #110843, .T. ) ;
#69639 = AXIS2_PLACEMENT_3D ( 'NONE', #31302, #93792, #91246 ) ;
#69641 = CARTESIAN_POINT ( 'NONE',  ( 22.39999999999999503, 76.10085836911117951, -181.7726746080137445 ) ) ;
#69642 = CIRCLE ( 'NONE', #215355, 0.09999999999999843736 ) ;
#69643 = CARTESIAN_POINT ( 'NONE',  ( -18.50000000000000000, 10.29270135741298375, -172.9573618871519614 ) ) ;
#69644 = ADVANCED_FACE ( 'NONE', ( #204669 ), #179670, .T. ) ;
#69645 = ORIENTED_EDGE ( 'NONE', *, *, #16092, .T. ) ;
#69646 = EDGE_CURVE ( 'NONE', #153155, #253265, #101686, .T. ) ;
#69647 = VECTOR ( 'NONE', #109634, 1000.000000000000000 ) ;
#69648 = EDGE_CURVE ( 'NONE', #189431, #231942, #230929, .T. ) ;
#69649 = CIRCLE ( 'NONE', #23874, 0.1999999999999987899 ) ;
#69650 = ORIENTED_EDGE ( 'NONE', *, *, #224111, .T. ) ;
#69651 = CARTESIAN_POINT ( 'NONE',  ( 21.53551880898956838, 69.21520223859636189, -203.6220772190960702 ) ) ;
#69652 = VECTOR ( 'NONE', #9498, 1000.000000000000000 ) ;
#69653 = ORIENTED_EDGE ( 'NONE', *, *, #182951, .F. ) ;
#69654 = AXIS2_PLACEMENT_3D ( 'NONE', #128030, #125462, #247956 ) ;
#69655 = DIRECTION ( 'NONE',  ( 0.000000000000000000, 0.000000000000000000, -1.000000000000000000 ) ) ;
#69656 = CARTESIAN_POINT ( 'NONE',  ( -16.85718274719422993, 9.976142314632891583, -79.56334633218253316 ) ) ;
#69659 = ADVANCED_FACE ( 'NONE', ( #9053 ), #203413, .F. ) ;
#69658 = VERTEX_POINT ( 'NONE', #186426 ) ;
#69657 = CARTESIAN_POINT ( 'NONE',  ( 19.58285714285715073, 9.015001489659738354, -142.4206528160817413 ) ) ;
#69660 = CARTESIAN_POINT ( 'NONE',  ( 20.85000000000000142, 11.75000000001115907, -127.2161343370219413 ) ) ;
#69662 = AXIS2_PLACEMENT_3D ( 'NONE', #27998, #227437, #156624 ) ;
#69661 = CARTESIAN_POINT ( 'NONE',  ( -23.25000000000000000, 0.000000000000000000, -33.50000000000000000 ) ) ;
#69663 = CARTESIAN_POINT ( 'NONE',  ( -20.94999999999999929, 79.11538813396778380, -196.3722783875038544 ) ) ;
#69664 = CARTESIAN_POINT ( 'NONE',  ( -16.87487986503753845, 22.97804876015371889, -230.9350448236104967 ) ) ;
#69665 = AXIS2_PLACEMENT_3D ( 'NONE', #171176, #92862, #55003 ) ;
#69666 = DIRECTION ( 'NONE',  ( 1.000000000000000000, 0.000000000000000000, 0.000000000000000000 ) ) ;
#69667 = EDGE_CURVE ( 'NONE', #38617, #45256, #81034, .T. ) ;
#69668 = CARTESIAN_POINT ( 'NONE',  ( -20.00857864376270001, 66.85000000001228670, -157.6731074845244223 ) ) ;
#69669 = EDGE_CURVE ( 'NONE', #42536, #213770, #7782, .T. ) ;
#69670 = DIRECTION ( 'NONE',  ( -0.000000000000000000, 1.000000000000000000, -0.000000000000000000 ) ) ;
#69672 = EDGE_LOOP ( 'NONE', ( #227161, #72180, #253255, #20654 ) ) ;
#69671 = CARTESIAN_POINT ( 'NONE',  ( -22.50000000000000000, 75.90000000001202807, -114.6726782920691221 ) ) ;
#69673 = CARTESIAN_POINT ( 'NONE',  ( 21.09793522318398828, 22.98180148693077740, -230.0583016547000739 ) ) ;
#69674 = VECTOR ( 'NONE', #1447, 1000.000000000000000 ) ;
#69675 = AXIS2_PLACEMENT_3D ( 'NONE', #20472, #176992, #221200 ) ;
#69677 = EDGE_CURVE ( 'NONE', #83539, #242544, #26215, .T. ) ;
#69676 = DIRECTION ( 'NONE',  ( 0.000000000000000000, 0.9126074666063772600, 0.4088369013363276627 ) ) ;
#69678 = CARTESIAN_POINT ( 'NONE',  ( -20.94999999999994600, 87.75000000001119815, -5.923107484524795296 ) ) ;
#69680 = EDGE_CURVE ( 'NONE', #28771, #152443, #139291, .T. ) ;
#69679 = DIRECTION ( 'NONE',  ( 0.000000000000000000, 0.000000000000000000, 1.000000000000000000 ) ) ;
#69681 = CARTESIAN_POINT ( 'NONE',  ( -23.25000000000000000, 76.00000000001170974, -69.52310748452431710 ) ) ;
#69682 = EDGE_CURVE ( 'NONE', #14406, #155813, #72713, .T. ) ;
#69683 = ORIENTED_EDGE ( 'NONE', *, *, #208940, .T. ) ;
#69684 = CARTESIAN_POINT ( 'NONE',  ( -22.59999999999999787, 64.25012875563515991, -69.58853707553808476 ) ) ;
#69685 = AXIS2_PLACEMENT_3D ( 'NONE', #164411, #169589, #89988 ) ;
#69686 = DIRECTION ( 'NONE',  ( 1.000000000000000000, 0.000000000000000000, -0.000000000000000000 ) ) ;
#69687 = VECTOR ( 'NONE', #256711, 1000.000000000000114 ) ;
#69688 = CARTESIAN_POINT ( 'NONE',  ( -21.05000000000000071, 62.82351852614503684, -207.2177435922979214 ) ) ;
#69689 = ORIENTED_EDGE ( 'NONE', *, *, #227667, .T. ) ;
#69690 = CARTESIAN_POINT ( 'NONE',  ( 23.14999999999999858, 71.00000000001230660, -157.6178414656113205 ) ) ;
#69691 = CARTESIAN_POINT ( 'NONE',  ( -16.93909480342659890, 9.993078364812696179, -79.60034701667237300 ) ) ;
#69692 = ORIENTED_EDGE ( 'NONE', *, *, #64624, .T. ) ;
#69693 = CARTESIAN_POINT ( 'NONE',  ( -16.86757978335472075, 66.03434962097831828, -190.9251028313569236 ) ) ;
#69694 = EDGE_CURVE ( 'NONE', #133079, #256777, #205968, .T. ) ;
#69695 = VERTEX_POINT ( 'NONE', #104282 ) ;
#69696 = EDGE_CURVE ( 'NONE', #150814, #180782, #147703, .T. ) ;
#69697 = FACE_OUTER_BOUND ( 'NONE', #54428, .T. ) ;
#69698 = VERTEX_POINT ( 'NONE', #129012 ) ;
#69699 = CIRCLE ( 'NONE', #115462, 0.1000000000000002554 ) ;
#69700 = DIRECTION ( 'NONE',  ( 1.000000000000000000, 0.000000000000000000, 0.000000000000000000 ) ) ;
#69701 = TOROIDAL_SURFACE ( 'NONE', #165372, 0.2000000000000000111, 0.1000000000000000056 ) ;
#69702 = DIRECTION ( 'NONE',  ( -1.000000000000000000, 0.000000000000000000, -0.000000000000000000 ) ) ;
#69703 = CIRCLE ( 'NONE', #98870, 4.300000000000035350 ) ;
#69704 = ORIENTED_EDGE ( 'NONE', *, *, #151870, .T. ) ;
#69706 = EDGE_CURVE ( 'NONE', #106227, #4597, #108162, .T. ) ;
#69705 = VERTEX_POINT ( 'NONE', #67747 ) ;
#69707 = CARTESIAN_POINT ( 'NONE',  ( 20.94999999999999929, 67.23127455305835554, -235.8551265064784559 ) ) ;
#69709 = ORIENTED_EDGE ( 'NONE', *, *, #3245, .T. ) ;
#69708 = LINE ( 'NONE', #244463, #184804 ) ;
#69710 = CARTESIAN_POINT ( 'NONE',  ( 20.73486653747088937, 52.51830411513114427, -233.9542054421835644 ) ) ;
#69711 = VERTEX_POINT ( 'NONE', #246386 ) ;
#69712 = AXIS2_PLACEMENT_3D ( 'NONE', #117216, #118517, #61081 ) ;
#69713 = VERTEX_POINT ( 'NONE', #109421 ) ;
#69714 = CARTESIAN_POINT ( 'NONE',  ( 23.24999999999999289, 11.75000000000000711, 11.75000000000000000 ) ) ;
#69715 = LINE ( 'NONE', #128391, #146958 ) ;
#69716 = DIRECTION ( 'NONE',  ( -1.000000000000000000, 0.000000000000000000, 0.000000000000000000 ) ) ;
#69717 = CARTESIAN_POINT ( 'NONE',  ( 21.05000000000000071, 64.35000000001195986, -110.0379132551783243 ) ) ;
#69718 = CARTESIAN_POINT ( 'NONE',  ( -18.40000000000000213, -9.499999999988851584, -74.03206939669971121 ) ) ;
#69719 = DIRECTION ( 'NONE',  ( 1.000000000000000000, 0.000000000000000000, 0.000000000000000000 ) ) ;
#69721 = ORIENTED_EDGE ( 'NONE', *, *, #158679, .T. ) ;
#69720 = EDGE_CURVE ( 'NONE', #86120, #35577, #47724, .T. ) ;
#69722 = CARTESIAN_POINT ( 'NONE',  ( -21.14999999999999858, 60.91865828504416669, -234.1430899377568551 ) ) ;
#69723 = CARTESIAN_POINT ( 'NONE',  ( -20.94999999999994600, 66.15000000001120384, -4.623107484524796362 ) ) ;
#69724 = LINE ( 'NONE', #227482, #111917 ) ;
#69725 = CARTESIAN_POINT ( 'NONE',  ( 18.54999999999999716, 33.06517536918362055, -220.7872234046467952 ) ) ;
#69726 = EDGE_CURVE ( 'NONE', #130308, #82909, #168176, .T. ) ;
#69727 = VERTEX_POINT ( 'NONE', #144699 ) ;
#69728 = CARTESIAN_POINT ( 'NONE',  ( 22.59999999999999432, 0.1008583691098678403, -55.25043287651065071 ) ) ;
#69729 = ORIENTED_EDGE ( 'NONE', *, *, #35803, .F. ) ;
#69730 = CARTESIAN_POINT ( 'NONE',  ( -18.50000000000000355, -7.631834139420990759, -210.1304494778855485 ) ) ;
#69732 = ORIENTED_EDGE ( 'NONE', *, *, #66364, .F. ) ;
#69731 = CIRCLE ( 'NONE', #90369, 11.65000000000000036 ) ;
#69733 = CARTESIAN_POINT ( 'NONE',  ( 23.15000000000000213, -9.499999999988844479, -157.6060308773475640 ) ) ;
#69734 = LINE ( 'NONE', #209220, #231384 ) ;
#69735 = ORIENTED_EDGE ( 'NONE', *, *, #15108, .T. ) ;
#69736 = ORIENTED_EDGE ( 'NONE', *, *, #240800, .T. ) ;
#69739 = ORIENTED_EDGE ( 'NONE', *, *, #247540, .T. ) ;
#69738 = ADVANCED_FACE ( 'NONE', ( #45620 ), #1924, .T. ) ;
#69737 = DIRECTION ( 'NONE',  ( 0.000000000000000000, 0.9915357197604971473, -0.1298341882519111479 ) ) ;
#69740 = VERTEX_POINT ( 'NONE', #11644 ) ;
#69741 = DIRECTION ( 'NONE',  ( -1.000000000000000000, -2.885090398161910739E-16, -6.283419270304611573E-17 ) ) ;
#69742 = EDGE_CURVE ( 'NONE', #64377, #173790, #247466, .T. ) ;
#69743 = FACE_OUTER_BOUND ( 'NONE', #184883, .T. ) ;
#69744 = ORIENTED_EDGE ( 'NONE', *, *, #53434, .T. ) ;
#69745 = DIRECTION ( 'NONE',  ( 0.000000000000000000, 0.000000000000000000, -1.000000000000000000 ) ) ;
#69746 = EDGE_CURVE ( 'NONE', #216222, #188358, #235183, .T. ) ;
#69747 = DIRECTION ( 'NONE',  ( -1.000000000000000000, 0.000000000000000000, 0.000000000000000000 ) ) ;
#69748 = AXIS2_PLACEMENT_3D ( 'NONE', #196845, #23391, #58613 ) ;
#69749 = AXIS2_PLACEMENT_3D ( 'NONE', #199089, #76566, #257716 ) ;
#69750 = VECTOR ( 'NONE', #49777, 1000.000000000000000 ) ;
#69751 = AXIS2_PLACEMENT_3D ( 'NONE', #65025, #10209, #29797 ) ;
#69752 = VERTEX_POINT ( 'NONE', #72914 ) ;
#69753 = ADVANCED_FACE ( 'NONE', ( #71616 ), #213674, .T. ) ;
#69756 = EDGE_CURVE ( 'NONE', #242536, #247150, #89426, .T. ) ;
#69755 = EDGE_CURVE ( 'NONE', #141218, #5530, #172876, .T. ) ;
#69754 = LINE ( 'NONE', #134814, #89106 ) ;
#69757 = DIRECTION ( 'NONE',  ( 5.421010862427554711E-16, 1.000000000000000000, 1.023556919514279895E-14 ) ) ;
#69758 = CARTESIAN_POINT ( 'NONE',  ( -18.40000000000000213, 11.47316190337364183, -54.39142135623731633 ) ) ;
#69760 = ORIENTED_EDGE ( 'NONE', *, *, #121032, .T. ) ;
#69759 = DIRECTION ( 'NONE',  ( 1.000000000000000000, 0.000000000000000000, -0.000000000000000000 ) ) ;
#69761 = DIRECTION ( 'NONE',  ( -1.000000000000000000, 2.952720810173289112E-16, 2.061873921506763405E-30 ) ) ;
#69762 = FACE_OUTER_BOUND ( 'NONE', #107223, .T. ) ;
#69765 = CARTESIAN_POINT ( 'NONE',  ( -17.27223548803355513, 60.22175817953561960, -222.1770843993087396 ) ) ;
#69764 = AXIS2_PLACEMENT_3D ( 'NONE', #86290, #224538, #167177 ) ;
#69763 = DIRECTION ( 'NONE',  ( -3.265361837132813093E-16, 1.000000000000000000, 0.000000000000000000 ) ) ;
#69766 = CARTESIAN_POINT ( 'NONE',  ( -21.05000000000000071, 5.849999999999952571, -10.13249722427796762 ) ) ;
#69767 = DIRECTION ( 'NONE',  ( 0.000000000000000000, 0.2617529984164955192, 0.9651348961777178603 ) ) ;
#69768 = AXIS2_PLACEMENT_3D ( 'NONE', #102904, #245007, #246299 ) ;
#69769 = DIRECTION ( 'NONE',  ( -2.342056488767301376E-15, 0.1350103645451974088, -0.9908441862701587999 ) ) ;
#69770 = CARTESIAN_POINT ( 'NONE',  ( -20.64999999999999858, 85.00000000001159606, -60.12913836187181715 ) ) ;
#69771 = EDGE_CURVE ( 'NONE', #188971, #91651, #248963, .T. ) ;
#69772 = EDGE_CURVE ( 'NONE', #146292, #83438, #201855, .T. ) ;
#69773 = ORIENTED_EDGE ( 'NONE', *, *, #80936, .T. ) ;
#69774 = CIRCLE ( 'NONE', #215504, 0.1000000000000054040 ) ;
#69775 = ORIENTED_EDGE ( 'NONE', *, *, #65716, .T. ) ;
#69776 = ADVANCED_FACE ( 'NONE', ( #251504 ), #131570, .T. ) ;
#69777 = VERTEX_POINT ( 'NONE', #32513 ) ;
#69778 = EDGE_CURVE ( 'NONE', #103174, #66550, #60381, .T. ) ;
#69779 = DIRECTION ( 'NONE',  ( 0.000000000000000000, -0.4999999999999689138, 0.8660254037844565822 ) ) ;
#69780 = CYLINDRICAL_SURFACE ( 'NONE', #102693, 0.09999999999999939493 ) ;
#69781 = ADVANCED_FACE ( 'NONE', ( #194134 ), #10343, .T. ) ;
#69782 = ORIENTED_EDGE ( 'NONE', *, *, #88190, .F. ) ;
#69783 =( NAMED_UNIT ( * ) SI_UNIT ( $, .STERADIAN. ) SOLID_ANGLE_UNIT ( ) );
#69784 = CARTESIAN_POINT ( 'NONE',  ( -23.25000000000000000, 11.75000000001115552, -126.9851942293460922 ) ) ;
#69785 = CARTESIAN_POINT ( 'NONE',  ( 20.89878130938411616, 10.32747123227773045, -206.5774032850248716 ) ) ;
#69786 = CIRCLE ( 'NONE', #40771, 7.800000000000005151 ) ;
#69787 = LINE ( 'NONE', #174048, #182962 ) ;
#69788 = ORIENTED_EDGE ( 'NONE', *, *, #123269, .T. ) ;
#69789 = ORIENTED_EDGE ( 'NONE', *, *, #209202, .T. ) ;
#69790 = CARTESIAN_POINT ( 'NONE',  ( -16.87368910959167678, 9.961273816702552963, -46.11249309664059837 ) ) ;
#69791 = DIRECTION ( 'NONE',  ( -0.000000000000000000, 0.8660254037844377084, 0.5000000000000016653 ) ) ;
#69792 = ORIENTED_EDGE ( 'NONE', *, *, #77058, .F. ) ;
#69793 = ADVANCED_FACE ( 'NONE', ( #15495 ), #27104, .T. ) ;
#69794 = FACE_OUTER_BOUND ( 'NONE', #24755, .T. ) ;
#69796 = ORIENTED_EDGE ( 'NONE', *, *, #237778, .T. ) ;
#69795 = DIRECTION ( 'NONE',  ( -1.000000000000000000, 0.000000000000000000, 0.000000000000000000 ) ) ;
#69797 = CARTESIAN_POINT ( 'NONE',  ( 21.05000000000000071, 74.95298800634525094, -207.3836470692357636 ) ) ;
#69798 = AXIS2_PLACEMENT_3D ( 'NONE', #113823, #31761, #151709 ) ;
#69800 = VERTEX_POINT ( 'NONE', #33797 ) ;
#69799 = DIRECTION ( 'NONE',  ( -0.000000000000000000, 0.8660254037844411501, 0.4999999999999956701 ) ) ;
#69801 = PRESENTATION_STYLE_ASSIGNMENT (( #151912 ) ) ;
#69802 = DIRECTION ( 'NONE',  ( -1.000000000000000000, -0.000000000000000000, -0.000000000000000000 ) ) ;
#69803 = CARTESIAN_POINT ( 'NONE',  ( 18.59999999999999076, 64.25000000001250555, -178.6731074845244507 ) ) ;
#69804 = CARTESIAN_POINT ( 'NONE',  ( -20.94999999999999929, 69.16514130714681130, -247.7543978865853660 ) ) ;
#69805 = CIRCLE ( 'NONE', #253118, 12.87499999999999822 ) ;
#69806 = EDGE_CURVE ( 'NONE', #30941, #154018, #243545, .T. ) ;
#69808 = FACE_OUTER_BOUND ( 'NONE', #207628, .T. ) ;
#69807 = DIRECTION ( 'NONE',  ( 0.000000000000000000, 0.2128009952263604232, -0.9770955615653316162 ) ) ;
#69809 = CARTESIAN_POINT ( 'NONE',  ( -23.15000000000000213, 76.00000000001216449, -140.5231074845243597 ) ) ;
#69810 = CARTESIAN_POINT ( 'NONE',  ( -18.59999999999999787, 85.48068669529138219, -163.0819923157664562 ) ) ;
#69811 = AXIS2_PLACEMENT_3D ( 'NONE', #246999, #68382, #147924 ) ;
#69812 = AXIS2_PLACEMENT_3D ( 'NONE', #64952, #201909, #246174 ) ;
#69813 = DIRECTION ( 'NONE',  ( 0.000000000000000000, 0.8490545835447252943, 0.5283051335749947564 ) ) ;
#69814 = DIRECTION ( 'NONE',  ( 1.000000000000000000, -0.000000000000000000, -0.000000000000000000 ) ) ;
#69816 = ORIENTED_EDGE ( 'NONE', *, *, #255381, .F. ) ;
#69815 = AXIS2_PLACEMENT_3D ( 'NONE', #247604, #68994, #169398 ) ;
#69817 = VERTEX_POINT ( 'NONE', #174609 ) ;
#69818 = LINE ( 'NONE', #91917, #163871 ) ;
#69819 = TOROIDAL_SURFACE ( 'NONE', #190623, 11.65000000000000036, 0.1000000000000000056 ) ;
#69820 = ORIENTED_EDGE ( 'NONE', *, *, #115174, .F. ) ;
#69821 = CARTESIAN_POINT ( 'NONE',  ( -18.50000000000000000, 9.250000000011157297, -188.7499999999999716 ) ) ;
#69822 = EDGE_LOOP ( 'NONE', ( #216683, #242981, #16726, #175868 ) ) ;
#69823 = ADVANCED_FACE ( 'NONE', ( #31232 ), #153759, .F. ) ;
#69825 = CARTESIAN_POINT ( 'NONE',  ( 23.24999999999999645, 68.28935379556426710, -213.7087130192904567 ) ) ;
#69824 = VECTOR ( 'NONE', #136503, 1000.000000000000000 ) ;
#69826 = DIRECTION ( 'NONE',  ( -1.000000000000000000, 0.000000000000000000, 0.000000000000000000 ) ) ;
#69827 = ORIENTED_EDGE ( 'NONE', *, *, #64552, .T. ) ;
#69828 = DIRECTION ( 'NONE',  ( 0.000000000000000000, -0.2128009952263602012, 0.9770955615653315052 ) ) ;
#69829 = CIRCLE ( 'NONE', #132172, 4.049999999999998046 ) ;
#69830 = EDGE_CURVE ( 'NONE', #208704, #59112, #66362, .T. ) ;
#69831 = ORIENTED_EDGE ( 'NONE', *, *, #45998, .T. ) ;
#69832 = ORIENTED_EDGE ( 'NONE', *, *, #71784, .T. ) ;
#69833 = AXIS2_PLACEMENT_3D ( 'NONE', #128412, #207968, #89269 ) ;
#69834 = ORIENTED_EDGE ( 'NONE', *, *, #79182, .F. ) ;
#69836 = DIRECTION ( 'NONE',  ( -1.000000000000000000, 0.000000000000000000, -0.000000000000000000 ) ) ;
#69835 = AXIS2_PLACEMENT_3D ( 'NONE', #177547, #216627, #135 ) ;
#69837 = CARTESIAN_POINT ( 'NONE',  ( 21.05000000000000071, 10.62950747927180295, -41.12797939999666141 ) ) ;
#69838 = DIRECTION ( 'NONE',  ( 0.000000000000000000, 0.000000000000000000, -1.000000000000000000 ) ) ;
#69839 = AXIS2_PLACEMENT_3D ( 'NONE', #206358, #167254, #222028 ) ;
#69840 = CARTESIAN_POINT ( 'NONE',  ( 22.59999999999999432, -3.092988775432913506, -228.1437074281570858 ) ) ;
#69841 = CARTESIAN_POINT ( 'NONE',  ( -20.64999999999999858, -8.999999999988844479, -124.1060308773475924 ) ) ;
#69842 = COLOUR_RGB ( '', 0.08235294, 0.09019608, 0.10196078) ;
#69844 = DIRECTION ( 'NONE',  ( -1.020425574104004196E-15, -0.2617529984165031243, -0.9651348961777157509 ) ) ;
#69843 = DIRECTION ( 'NONE',  ( -1.000000000000000000, -0.000000000000000000, -0.000000000000000000 ) ) ;
#69845 = CARTESIAN_POINT ( 'NONE',  ( -12.84409460144753368, 9.410682294279109072, -82.43114344194833620 ) ) ;
#69847 = ORIENTED_EDGE ( 'NONE', *, *, #88043, .T. ) ;
#69846 = CARTESIAN_POINT ( 'NONE',  ( -21.14999999999999858, 6.540656951712397138, -134.0000000000000000 ) ) ;
#69849 = DIRECTION ( 'NONE',  ( 0.000000000000000000, -6.688090509790120484E-15, 1.000000000000000000 ) ) ;
#69848 = CARTESIAN_POINT ( 'NONE',  ( -20.94999999999999929, 76.00000000001173817, -73.52310748452431710 ) ) ;
#69850 = CIRCLE ( 'NONE', #86358, 0.09999999999999939493 ) ;
#69851 = FACE_OUTER_BOUND ( 'NONE', #27065, .T. ) ;
#69852 = ORIENTED_EDGE ( 'NONE', *, *, #179428, .T. ) ;
#69853 = CARTESIAN_POINT ( 'NONE',  ( 20.95052659398289308, 10.47982436779105875, -74.57523875586565509 ) ) ;
#69854 = DIRECTION ( 'NONE',  ( 0.000000000000000000, -0.3427706569149636118, 0.9394191166662962944 ) ) ;
#69855 = DIRECTION ( 'NONE',  ( -1.000000000000000000, 0.000000000000000000, 0.000000000000000000 ) ) ;
#69856 = ORIENTED_EDGE ( 'NONE', *, *, #46431, .T. ) ;
#69857 = LINE ( 'NONE', #249758, #53776 ) ;
#69858 = AXIS2_PLACEMENT_3D ( 'NONE', #247121, #59814, #140657 ) ;
#69859 = DIRECTION ( 'NONE',  ( 0.7071067811865474617, 0.7071067811865474617, 0.000000000000000000 ) ) ;
#69860 = CARTESIAN_POINT ( 'NONE',  ( 15.06592377766031277, 66.58221053305965142, -87.66572294054748227 ) ) ;
#69861 = AXIS2_PLACEMENT_3D ( 'NONE', #186186, #128782, #242289 ) ;
#69863 = ORIENTED_EDGE ( 'NONE', *, *, #149257, .F. ) ;
#69862 = VECTOR ( 'NONE', #59540, 1000.000000000000000 ) ;
#69864 = ORIENTED_EDGE ( 'NONE', *, *, #27578, .F. ) ;
#69865 = CARTESIAN_POINT ( 'NONE',  ( -18.40000000000000213, 64.66825945288670141, -90.37310748452438247 ) ) ;
#69866 = CARTESIAN_POINT ( 'NONE',  ( -18.53317502108577131, 10.32263460347359540, -173.0605957968672328 ) ) ;
#69867 = FACE_OUTER_BOUND ( 'NONE', #10612, .T. ) ;
#69868 = CYLINDRICAL_SURFACE ( 'NONE', #63579, 0.09999999999998898659 ) ;
#69869 = EDGE_LOOP ( 'NONE', ( #30491, #87417, #7517, #238928, #31517, #165659, #116952, #92870, #64880, #112698, #97136, #143300 ) ) ;
#69870 = DIRECTION ( 'NONE',  ( 0.000000000000000000, 0.000000000000000000, 1.000000000000000000 ) ) ;
#69871 = CIRCLE ( 'NONE', #198839, 0.4000000000000010214 ) ;
#69873 = ADVANCED_FACE ( 'NONE', ( #37621 ), #256592, .F. ) ;
#69872 = CARTESIAN_POINT ( 'NONE',  ( 18.59999999999999076, 10.49142135624846439, -91.75000000000005684 ) ) ;
#69874 = VECTOR ( 'NONE', #171822, 1000.000000000000000 ) ;
#69875 = CARTESIAN_POINT ( 'NONE',  ( -18.59999999999999787, 74.75000000001261924, -195.5231074845243597 ) ) ;
#69876 = CARTESIAN_POINT ( 'NONE',  ( -18.50000000000000000, 1.866714910068465239, -78.75267524628205251 ) ) ;
#69877 = TOROIDAL_SURFACE ( 'NONE', #253008, 0.2000000000000000111, 0.1000000000000000056 ) ;
#69878 = ORIENTED_EDGE ( 'NONE', *, *, #207870, .F. ) ;
#69879 = CARTESIAN_POINT ( 'NONE',  ( 20.94788355080264353, 10.30207779524867462, -38.98955207167824000 ) ) ;
#69880 = AXIS2_PLACEMENT_3D ( 'NONE', #248386, #37070, #121733 ) ;
#69882 = ORIENTED_EDGE ( 'NONE', *, *, #218124, .F. ) ;
#69881 = LINE ( 'NONE', #108971, #212723 ) ;
#69883 = DIRECTION ( 'NONE',  ( 0.000000000000000000, 1.000000000000000000, 0.000000000000000000 ) ) ;
#69884 = DIRECTION ( 'NONE',  ( -1.000000000000000000, -0.000000000000000000, -0.000000000000000000 ) ) ;
#69885 = CARTESIAN_POINT ( 'NONE',  ( 11.60000000000006182, 66.35000000001119247, -23.62310748452479103 ) ) ;
#69886 = EDGE_CURVE ( 'NONE', #87571, #210308, #97778, .T. ) ;
#69887 = FACE_OUTER_BOUND ( 'NONE', #127431, .T. ) ;
#69888 = DIRECTION ( 'NONE',  ( 2.952720810173289112E-16, 1.000000000000000000, 6.938893903907222067E-15 ) ) ;
#69889 = VECTOR ( 'NONE', #128736, 1000.000000000000000 ) ;
#69890 = SPHERICAL_SURFACE ( 'NONE', #80149, 0.1000000000000000056 ) ;
#69891 = CYLINDRICAL_SURFACE ( 'NONE', #69622, 0.1000000000000028644 ) ;
#69892 = EDGE_CURVE ( 'NONE', #1615, #20493, #18696, .T. ) ;
#69893 = ORIENTED_EDGE ( 'NONE', *, *, #100861, .F. ) ;
#69894 = DIRECTION ( 'NONE',  ( 1.000000000000000000, 0.000000000000000000, 0.000000000000000000 ) ) ;
#69895 = CARTESIAN_POINT ( 'NONE',  ( 21.05000000000000071, 1.115600667400684642E-11, -167.4999999999999716 ) ) ;
#69896 = CARTESIAN_POINT ( 'NONE',  ( -20.64999999999999858, 85.00000000001197975, -112.9170766071766820 ) ) ;
#69897 = CIRCLE ( 'NONE', #215600, 0.5000000000000004441 ) ;
#69898 = AXIS2_PLACEMENT_3D ( 'NONE', #103477, #162219, #83892 ) ;
#69899 = DIRECTION ( 'NONE',  ( -1.000000000000000000, 0.000000000000000000, 0.000000000000000000 ) ) ;
#69900 = CIRCLE ( 'NONE', #173978, 0.1000000000000016431 ) ;
#69901 = CARTESIAN_POINT ( 'NONE',  ( 20.94999999999999574, 1.261786168576181755, -175.5864989635454378 ) ) ;
#69902 = EDGE_CURVE ( 'NONE', #133238, #252010, #164457, .T. ) ;
#69903 = VECTOR ( 'NONE', #34826, 1000.000000000000000 ) ;
#69904 = CARTESIAN_POINT ( 'NONE',  ( 12.60873083341397383, 9.389571634557567492, -185.3176407123691547 ) ) ;
#69905 = ORIENTED_EDGE ( 'NONE', *, *, #179880, .T. ) ;
#69906 = ORIENTED_EDGE ( 'NONE', *, *, #146910, .T. ) ;
#69907 = LINE ( 'NONE', #150704, #10088 ) ;
#69908 = EDGE_CURVE ( 'NONE', #37087, #5080, #156104, .T. ) ;
#69909 = CARTESIAN_POINT ( 'NONE',  ( -16.94107738177414291, 63.04990807712500356, -213.0142932718104021 ) ) ;
#69910 = DIRECTION ( 'NONE',  ( 1.000000000000000000, -1.541976423090492636E-14, 0.000000000000000000 ) ) ;
#69911 = ADVANCED_FACE ( 'NONE', ( #161416 ), #257878, .F. ) ;
#69912 = CARTESIAN_POINT ( 'NONE',  ( -16.87331047859651179, 66.05000000001157900, -56.87310748452438958 ) ) ;
#69913 = EDGE_CURVE ( 'NONE', #135260, #7751, #137965, .T. ) ;
#69914 = DIRECTION ( 'NONE',  ( 0.000000000000000000, 0.000000000000000000, 1.000000000000000000 ) ) ;
#69915 = CIRCLE ( 'NONE', #111588, 0.09999999999999820144 ) ;
#69916 = CARTESIAN_POINT ( 'NONE',  ( -18.50000000000000000, -0.5844187615853587703, -242.4893126442242703 ) ) ;
#69917 = EDGE_CURVE ( 'NONE', #50997, #61093, #64496, .T. ) ;
#69918 = DIRECTION ( 'NONE',  ( 0.000000000000000000, 0.000000000000000000, -1.000000000000000000 ) ) ;
#69919 = AXIS2_PLACEMENT_3D ( 'NONE', #154324, #172605, #211700 ) ;
#69920 = DIRECTION ( 'NONE',  ( 1.000000000000000000, 0.000000000000000000, 0.000000000000000000 ) ) ;
#69921 = EDGE_LOOP ( 'NONE', ( #38215, #46448, #150540, #60458, #19996 ) ) ;
#69922 = DIRECTION ( 'NONE',  ( -4.408576920032447355E-17, -0.1350103645451945777, 0.9908441862701589109 ) ) ;
#69923 = ORIENTED_EDGE ( 'NONE', *, *, #20655, .T. ) ;
#69924 = DIRECTION ( 'NONE',  ( 1.000000000000000000, 0.000000000000000000, 0.000000000000000000 ) ) ;
#69926 = EDGE_CURVE ( 'NONE', #169929, #97822, #168927, .T. ) ;
#69925 = DIRECTION ( 'NONE',  ( 0.2834754621636439431, -0.08203050052812088655, -0.9554646300801588055 ) ) ;
#69927 = LINE ( 'NONE', #211996, #66036 ) ;
#69928 = CARTESIAN_POINT ( 'NONE',  ( 22.57320508075688537, 11.65000000001115588, -100.5000000000000284 ) ) ;
#69929 = CARTESIAN_POINT ( 'NONE',  ( 18.54271179734060127, 85.62408429011053101, -62.78214263182413646 ) ) ;
#69930 = DIRECTION ( 'NONE',  ( 1.000000000000000000, 0.000000000000000000, 0.000000000000000000 ) ) ;
#69931 = ORIENTED_EDGE ( 'NONE', *, *, #217302, .T. ) ;
#69932 = EDGE_CURVE ( 'NONE', #97655, #99793, #197758, .T. ) ;
#69933 = FACE_OUTER_BOUND ( 'NONE', #92118, .T. ) ;
#69934 = CARTESIAN_POINT ( 'NONE',  ( 21.05000000000000071, 67.23127455305841238, -235.8551265064783991 ) ) ;
#69935 = CARTESIAN_POINT ( 'NONE',  ( 18.59999999999999787, 87.75000000001250555, -178.6731074845242802 ) ) ;
#69936 = CARTESIAN_POINT ( 'NONE',  ( -20.65000000000000568, 7.250000000011138646, -54.35000000000000142 ) ) ;
#69937 = CIRCLE ( 'NONE', #107323, 0.1999999999999987899 ) ;
#69938 = AXIS2_PLACEMENT_3D ( 'NONE', #80392, #41333, #200385 ) ;
#69939 = CARTESIAN_POINT ( 'NONE',  ( -22.57320508075686405, 11.75000000001115552, -167.5000000000000000 ) ) ;
#69940 = ORIENTED_EDGE ( 'NONE', *, *, #179457, .F. ) ;
#69941 = CARTESIAN_POINT ( 'NONE',  ( -16.79814274880124358, 9.949272542688458287, -79.65243303704804134 ) ) ;
#69943 = EDGE_CURVE ( 'NONE', #55595, #256235, #81820, .T. ) ;
#69942 = CARTESIAN_POINT ( 'NONE',  ( -20.64999999999999858, 68.85000000001151932, -48.37310748452436826 ) ) ;
#69944 = ORIENTED_EDGE ( 'NONE', *, *, #142423, .F. ) ;
#69945 = VERTEX_POINT ( 'NONE', #76713 ) ;
#69946 = LINE ( 'NONE', #167768, #122395 ) ;
#69947 = FACE_OUTER_BOUND ( 'NONE', #157673, .T. ) ;
#69948 = ORIENTED_EDGE ( 'NONE', *, *, #11210, .F. ) ;
#69949 = VECTOR ( 'NONE', #77988, 1000.000000000000114 ) ;
#69950 = CARTESIAN_POINT ( 'NONE',  ( 20.96077737575330247, 64.37609936600661342, -42.88231552741775943 ) ) ;
#69951 = DIRECTION ( 'NONE',  ( 0.000000000000000000, -1.000000000000000000, 0.000000000000000000 ) ) ;
#69952 = AXIS2_PLACEMENT_3D ( 'NONE', #171318, #142399, #60287 ) ;
#69953 = ORIENTED_EDGE ( 'NONE', *, *, #153141, .F. ) ;
#69954 = EDGE_CURVE ( 'NONE', #131991, #160738, #157596, .T. ) ;
#69955 = CIRCLE ( 'NONE', #207328, 3.900000000000000799 ) ;
#69956 = LINE ( 'NONE', #149497, #193814 ) ;
#69957 = EDGE_LOOP ( 'NONE', ( #32593, #46685, #36149, #91588, #155320, #130481, #73360, #87173, #85042 ) ) ;
#69958 = CARTESIAN_POINT ( 'NONE',  ( 21.13461538461538325, 10.61458296203669249, -79.35000000000005116 ) ) ;
#69959 = DIRECTION ( 'NONE',  ( 1.000000000000000000, 0.000000000000000000, 0.000000000000000000 ) ) ;
#69963 = EDGE_CURVE ( 'NONE', #201799, #69997, #160384, .T. ) ;
#69962 = ORIENTED_EDGE ( 'NONE', *, *, #59960, .T. ) ;
#69961 =( BOUNDED_SURFACE ( )  B_SPLINE_SURFACE ( 3, 2, ( 
 ( #105898, #169797, #249307 ),
 ( #228462, #8121, #109768 ),
 ( #184168, #66803, #49803 ),
 ( #5519, #146324, #85044 ),
 ( #143757, #244138, #246711 ),
 ( #225838, #47218, #126773 ),
 ( #87628, #147620, #227150 ),
 ( #65507, #48517, #155362 ),
 ( #17123, #34134, #150207 ),
 ( #211449, #171087, #212744 ) ),
 .UNSPECIFIED., .F., .F., .F. ) 
 B_SPLINE_SURFACE_WITH_KNOTS ( ( 4, 2, 2, 2, 4 ),
 ( 3, 3 ),
 ( 0.0001836757140119083063, 0.0004000170051583575893, 0.0005081876507315822309, 0.0005622729735181946058, 0.0006163582963048068724 ),
 ( 0.000000000000000000, 1.000000000000000000 ),
 .UNSPECIFIED. ) 
 GEOMETRIC_REPRESENTATION_ITEM ( )  RATIONAL_B_SPLINE_SURFACE ( (
 ( 1.000000000000000000, 0.7071067811865425767, 1.000000000000000000),
 ( 1.000000000000000000, 0.6461995200036771969, 1.000000000000000000),
 ( 1.000000000000000000, 0.5776453529540377385, 1.000000000000000000),
 ( 1.000000000000000000, 0.4585233068356288633, 1.000000000000000000),
 ( 1.000000000000000000, 0.4154092989930812663, 1.000000000000000000),
 ( 1.000000000000000000, 0.3550093145840674258, 1.000000000000000000),
 ( 1.000000000000000000, 0.3354498651685111632, 1.000000000000000000),
 ( 1.000000000000000000, 0.3060347992257030914, 1.000000000000000000),
 ( 1.000000000000000000, 0.2963555829626022819, 1.000000000000000000),
 ( 1.000000000000000000, 0.2966190024560417804, 1.000000000000000000) ) ) 
 REPRESENTATION_ITEM ( '' )  SURFACE ( )  );
#69960 = CARTESIAN_POINT ( 'NONE',  ( 21.05000000000000071, 14.05000000001115623, -94.98630492923912527 ) ) ;
#69964 = DIRECTION ( 'NONE',  ( -1.000000000000000000, 0.000000000000000000, -0.000000000000000000 ) ) ;
#69965 = DIRECTION ( 'NONE',  ( 0.000000000000000000, -0.6035730884107395333, -0.7973076739542406255 ) ) ;
#69966 = DIRECTION ( 'NONE',  ( 0.000000000000000000, 0.9654727137038715545, -0.2605042016806676242 ) ) ;
#69967 = CARTESIAN_POINT ( 'NONE',  ( -16.77308656112214891, 66.05000000001228955, -157.3729142928221165 ) ) ;
#69968 = CARTESIAN_POINT ( 'NONE',  ( -21.05000000000000426, 64.40000000001161595, -62.59490425424885274 ) ) ;
#69969 = EDGE_CURVE ( 'NONE', #126077, #153125, #47904, .T. ) ;
#69970 = LINE ( 'NONE', #189896, #234703 ) ;
#69971 = CARTESIAN_POINT ( 'NONE',  ( 18.59999999999998721, 69.06610602788578035, -132.7374616501508342 ) ) ;
#69972 = EDGE_CURVE ( 'NONE', #139316, #28102, #118680, .T. ) ;
#69974 = VERTEX_POINT ( 'NONE', #136687 ) ;
#69973 = CARTESIAN_POINT ( 'NONE',  ( 18.49362639424904131, 86.88399968321819244, -199.4661394926152411 ) ) ;
#69975 = ORIENTED_EDGE ( 'NONE', *, *, #74158, .F. ) ;
#69977 = CARTESIAN_POINT ( 'NONE',  ( -12.60829076262180592, 9.389529397477891948, -84.81710791289371798 ) ) ;
#69976 = CARTESIAN_POINT ( 'NONE',  ( 18.49999999999998934, 6.550000000000000711, -21.15000000000000213 ) ) ;
#69979 = ORIENTED_EDGE ( 'NONE', *, *, #145774, .T. ) ;
#69978 = CARTESIAN_POINT ( 'NONE',  ( -23.25000000000000000, 76.00000000001126921, -203.5231074845248997 ) ) ;
#69980 = ORIENTED_EDGE ( 'NONE', *, *, #50722, .F. ) ;
#69981 = CARTESIAN_POINT ( 'NONE',  ( -16.77732147262506146, 66.05403306739390246, -182.6866162412485437 ) ) ;
#69982 = EDGE_CURVE ( 'NONE', #254397, #163777, #218786, .T. ) ;
#69983 = DIRECTION ( 'NONE',  ( -2.827886303505249259E-16, -0.8660254037844378194, -0.5000000000000016653 ) ) ;
#69984 = AXIS2_PLACEMENT_3D ( 'NONE', #903, #79175, #160042 ) ;
#69985 =( BOUNDED_CURVE ( )  B_SPLINE_CURVE ( 3, ( #59644, #41422, #40150, #175797 ),
 .UNSPECIFIED., .F., .F. ) 
 B_SPLINE_CURVE_WITH_KNOTS ( ( 4, 4 ),
 ( 0.3000847527772386725, 0.5517402753107893965 ),
 .UNSPECIFIED. ) 
 CURVE ( )  GEOMETRIC_REPRESENTATION_ITEM ( )  RATIONAL_B_SPLINE_CURVE ( ( 1.000000000000000000, 0.9947294176030464508, 0.9947294176030464508, 1.000000000000000000 ) ) 
 REPRESENTATION_ITEM ( '' )  );
#69986 = EDGE_CURVE ( 'NONE', #10818, #226600, #2112, .T. ) ;
#69987 = DIRECTION ( 'NONE',  ( -1.000000000000000000, 0.000000000000000000, -0.000000000000000000 ) ) ;
#69989 = CARTESIAN_POINT ( 'NONE',  ( -21.05000000000000071, 68.59681812508419796, -224.1344059333694361 ) ) ;
#69988 = TOROIDAL_SURFACE ( 'NONE', #215685, 12.77499999999999858, 0.1000000000000000056 ) ;
#69990 = FACE_OUTER_BOUND ( 'NONE', #246121, .T. ) ;
#69991 = DIRECTION ( 'NONE',  ( -1.000000000000000000, 0.000000000000000000, 0.000000000000000000 ) ) ;
#69992 = ORIENTED_EDGE ( 'NONE', *, *, #225709, .F. ) ;
#69993 = ORIENTED_EDGE ( 'NONE', *, *, #110290, .F. ) ;
#69994 = LINE ( 'NONE', #89518, #114854 ) ;
#69995 = VECTOR ( 'NONE', #126758, 999.9999999999998863 ) ;
#69996 = CIRCLE ( 'NONE', #198963, 3.900000000000004796 ) ;
#69997 = VERTEX_POINT ( 'NONE', #47839 ) ;
#69998 = DIRECTION ( 'NONE',  ( 1.000000000000000000, 0.000000000000000000, 0.000000000000000000 ) ) ;
#69999 = ORIENTED_EDGE ( 'NONE', *, *, #170157, .F. ) ;
#70001 = FACE_OUTER_BOUND ( 'NONE', #140337, .T. ) ;
#70000 = TOROIDAL_SURFACE ( 'NONE', #86510, 0.6000000000000009770, 0.1000000000000000056 ) ;
#70002 =( BOUNDED_SURFACE ( )  B_SPLINE_SURFACE ( 3, 2, ( 
 ( #80005, #179172, #218243 ),
 ( #42207, #220828, #96993 ),
 ( #22663, #181714, #82570 ),
 ( #159586, #239120, #235254 ),
 ( #197412, #216963, #139989 ),
 ( #219536, #136129, #117872 ) ),
 .UNSPECIFIED., .F., .F., .F. ) 
 B_SPLINE_SURFACE_WITH_KNOTS ( ( 4, 2, 4 ),
 ( 3, 3 ),
 ( 1.570796326794895448, 2.356194490192343505, 3.141592653589791784 ),
 ( 0.000000000000000000, 1.000000000000000000 ),
 .UNSPECIFIED. ) 
 GEOMETRIC_REPRESENTATION_ITEM ( )  RATIONAL_B_SPLINE_SURFACE ( (
 ( 1.000000000000000000, 0.7071067811865352493, 1.000000000000000000),
 ( 1.000000000000000000, 0.6611148371775558141, 1.000000000000000000),
 ( 1.000000000000000000, 0.6092287576700777807, 1.000000000000000000),
 ( 1.000000000000000000, 0.5278258667052361242, 1.000000000000000000),
 ( 1.000000000000000000, 0.4993418825338509226, 1.000000000000000000),
 ( 1.000000000000000000, 0.5000000000000260902, 1.000000000000000000) ) ) 
 REPRESENTATION_ITEM ( '' )  SURFACE ( )  );
#70003 = EDGE_CURVE ( 'NONE', #154676, #163656, #147893, .T. ) ;
#70004 = AXIS2_PLACEMENT_3D ( 'NONE', #65386, #45824, #131778 ) ;
#70005 = DIRECTION ( 'NONE',  ( -0.000000000000000000, -0.000000000000000000, 1.000000000000000000 ) ) ;
#70006 = DIRECTION ( 'NONE',  ( 1.000000000000000000, 0.000000000000000000, 0.000000000000000000 ) ) ;
#70007 = ADVANCED_FACE ( 'NONE', ( #162689 ), #25740, .T. ) ;
#70008 = ORIENTED_EDGE ( 'NONE', *, *, #16127, .F. ) ;
#70009 = EDGE_CURVE ( 'NONE', #62433, #22716, #6209, .T. ) ;
#70010 = DIRECTION ( 'NONE',  ( 1.000000000000000000, 0.000000000000000000, 0.000000000000000000 ) ) ;
#70011 = VERTEX_POINT ( 'NONE', #206945 ) ;
#70012 = CARTESIAN_POINT ( 'NONE',  ( -16.97048361161166596, 66.05000000001150795, -49.16422314009399486 ) ) ;
#70013 = CARTESIAN_POINT ( 'NONE',  ( -16.88328101497759448, 9.950352834230013599, -87.85117951492932775 ) ) ;
#70014 = CARTESIAN_POINT ( 'NONE',  ( -20.85000000000000142, 77.83585931145600512, -158.5186683157258187 ) ) ;
#70015 = VERTEX_POINT ( 'NONE', #247342 ) ;
#70016 = FACE_OUTER_BOUND ( 'NONE', #131672, .T. ) ;
#70017 = AXIS2_PLACEMENT_3D ( 'NONE', #21202, #56426, #116430 ) ;
#70018 = EDGE_LOOP ( 'NONE', ( #175966, #246224 ) ) ;
#70021 = ORIENTED_EDGE ( 'NONE', *, *, #137671, .F. ) ;
#70020 = CARTESIAN_POINT ( 'NONE',  ( 18.58222699835054570, 46.46797214202639026, -243.0846070113367432 ) ) ;
#70019 = DIRECTION ( 'NONE',  ( -1.000000000000000000, -0.000000000000000000, -0.000000000000000000 ) ) ;
#70022 = AXIS2_PLACEMENT_3D ( 'NONE', #196093, #174005, #16191 ) ;
#70023 = ORIENTED_EDGE ( 'NONE', *, *, #225698, .T. ) ;
#70024 = AXIS2_PLACEMENT_3D ( 'NONE', #47941, #170527, #173088 ) ;
#70025 = CARTESIAN_POINT ( 'NONE',  ( 5.900000000000060751, 64.25000000001119815, -21.92310748452479174 ) ) ;
#70026 = ORIENTED_EDGE ( 'NONE', *, *, #165015, .T. ) ;
#70027 = TOROIDAL_SURFACE ( 'NONE', #128279, 12.77500000000000036, 0.1000000000000000056 ) ;
#70028 = CIRCLE ( 'NONE', #136619, 0.09999999999999553690 ) ;
#70029 = DIRECTION ( 'NONE',  ( -0.000000000000000000, 1.000000000000000000, -0.000000000000000000 ) ) ;
#70030 = VECTOR ( 'NONE', #226485, 1000.000000000000114 ) ;
#70031 = CARTESIAN_POINT ( 'NONE',  ( 20.95000000000005258, 65.25000000001119815, -4.423107484524790856 ) ) ;
#70032 = CARTESIAN_POINT ( 'NONE',  ( -18.41431012584569515, 54.11435837739090715, -229.1438153579562993 ) ) ;
#70033 = CARTESIAN_POINT ( 'NONE',  ( -16.92778301347232883, 65.99905508317726799, -123.9516255924936274 ) ) ;
#70034 = ADVANCED_FACE ( 'NONE', ( #64852 ), #28343, .F. ) ;
#70035 = VERTEX_POINT ( 'NONE', #106531 ) ;
#70036 = FACE_OUTER_BOUND ( 'NONE', #156452, .T. ) ;
#70037 = CARTESIAN_POINT ( 'NONE',  ( -20.64999999999999858, 4.250000000011156409, -121.6500000000000341 ) ) ;
#70038 = CARTESIAN_POINT ( 'NONE',  ( 18.50000972452444969, 10.29326151435342851, -139.4592822510414862 ) ) ;
#70039 = ORIENTED_EDGE ( 'NONE', *, *, #234793, .F. ) ;
#70040 = DIRECTION ( 'NONE',  ( 1.000000000000000000, 0.000000000000000000, 0.000000000000000000 ) ) ;
#70041 = VERTEX_POINT ( 'NONE', #8743 ) ;
#70043 = CIRCLE ( 'NONE', #94956, 0.09999999999999939493 ) ;
#70042 = DIRECTION ( 'NONE',  ( -0.000000000000000000, -0.000000000000000000, -1.000000000000000000 ) ) ;
#70044 = ORIENTED_EDGE ( 'NONE', *, *, #199859, .T. ) ;
#70045 = CLOSED_SHELL ( 'NONE', ( #31416, #72148, #13180, #182625, #187317, #78204, #229293, #77655, #236123, #171953, #250748, #51690, #254646, #198358, #134691, #155607, #243864, #86274, #117461, #246817, #202243, #174936, #212779, #176402, #160561, #59116, #194141, #113215, #215299, #53261, #225929, #73540, #137377, #81269, #24742, #149155, #135635, #40063, #107032, #235455, #184903, #129351, #90376, #180318, #86144, #116587, #12009, #220399, #124330, #121447, #29144, #238935, #254504, #129716, #249231, #83999, #100747, #13819, #15931, #129930, #256309, #85116, #256475, #34266, #73016, #99823, #255296, #200370, #169811, #99110, #175376, #223605, #179503, #223116, #21125, #97049, #222962, #59546, #7382, #42390, #221832, #107669, #149252, #45544, #85211, #116805, #228710, #225636, #137065, #126759, #242551, #239356, #202473, #74908, #138292, #72039, #175500, #225175, #124343, #212007, #243527, #257793, #129413, #79867, #238948, #20290, #18838, #194282, #86520, #76728, #104564, #53785, #187045, #130018, #144334, #123487, #10446, #776, #22009, #126726, #8380, #54130, #76739, #218398, #93899, #253378, #211631, #57511, #142524, #35398, #37807, #235152, #186251, #88541, #29858, #179763, #142912, #172936, #96423, #245531, #226727, #196246, #212718, #68849, #97544, #245705, #220221, #24202, #9917, #213130, #98446, #249139, #80017, #118821, #7665, #232917, #27360, #67410, #40180, #213940, #246838, #134088, #222757, #8376, #143804, #203893, #139915, #214533, #206926, #76860, #156601, #97924, #1349, #109670, #180587, #249726, #199213, #200376, #221314, #229344, #232234, #236524, #65937, #130072, #100188, #114629, #51069, #147995, #145783, #60373, #79436, #205551, #170705, #14348, #181773, #103581, #187195, #178923, #111457, #243969, #107336, #78648, #196553, #139658, #49039, #27469, #176514, #154927, #137412, #71860, #104151, #107143, #236729, #160466, #249955, #193265, #56107, #94964, #122998, #113457, #57992, #60013, #61094, #138304, #28945, #159171, #94377, #43532, #213238, #182716, #164927, #81860, #74509, #247194, #214915, #243926, #129898, #175139, #152850, #124814, #87532, #27958, #131602, #46296, #146625, #20845, #226555, #77811, #83800, #123432, #220132, #232435, #213920, #41952, #254197, #175972, #48213, #88822, #153325, #90208, #63874, #211100, #100408, #172422, #165143, #203092, #19048, #226061, #193180, #190760, #62880, #55469, #103487, #248264, #59871, #190187, #131772, #90791, #133616, #111097, #117415, #113756, #189610, #50374, #27085, #67036, #37045, #156683, #80070, #132099, #251239, #130101, #7899, #44491, #212483, #239267, #34040, #16292, #56721, #165778, #61921, #176030, #153804, #141291, #197174, #99308, #192423, #115033, #247445, #59594, #21776, #141852, #73751, #251981, #2308, #7411, #43641, #168661, #195973, #5889, #50774, #156060, #977, #77055, #218138, #117276, #205275, #65943, #225122, #229006, #67441, #94529, #2539, #61965, #20460, #188939, #247490, #13580, #243333, #92318, #242171, #55085, #222146, #164216, #51197, #50273, #235937, #227371, #219442, #74794, #27580, #216329, #212194, #66486, #176825, #38122, #246344, #18657, #93612, #115310, #197544, #203570, #41718, #80328, #239792, #48724, #142033, #158250, #22502, #48573, #83363, #168347, #65895, #128270, #173417, #204537, #111995, #5992, #94126, #209422, #47778, #42661, #117260, #132716, #195446, #82996, #203662, #171532, #139601, #179776, #82066, #65548, #19816, #57361, #183096, #14982, #152969, #137394, #199369, #155076, #211366, #35093, #98182, #125876, #13050, #47849, #245857, #176510, #257104, #84118, #207155, #179180, #185686, #35385, #246044, #23263, #149692, #185826, #77736, #160002, #188857, #247512, #78197, #234802, #211044, #103279, #65474, #101616, #96151, #20193, #246057, #175297, #99721, #244855, #131758, #46554, #64071, #17191, #185730, #180052, #158537, #215124, #157137, #151368, #256913, #226043, #76331, #44873, #118441, #18557, #119143, #187781, #33824, #157204, #198730, #154776, #62923, #93178, #254828, #121720, #75617, #164217, #17628, #32596, #171457, #34361, #163161, #17098, #76338, #145409, #41016, #37054, #55880, #107057, #207190, #255523, #28961, #27314 ) ) ;
#70046 = CARTESIAN_POINT ( 'NONE',  ( 20.94999999999997442, -1.263275465206102233, -208.9018646667463770 ) ) ;
#70047 = DIRECTION ( 'NONE',  ( -1.000000000000000000, -0.000000000000000000, 0.000000000000000000 ) ) ;
#70049 = EDGE_LOOP ( 'NONE', ( #186143, #231127, #108246, #229429 ) ) ;
#70048 = CARTESIAN_POINT ( 'NONE',  ( 18.52928932188133970, 10.27928932189250411, -58.15000000000000568 ) ) ;
#70050 = CARTESIAN_POINT ( 'NONE',  ( 18.59999999999999787, -1.835341550213255957, -45.05515129256298223 ) ) ;
#70051 = ORIENTED_EDGE ( 'NONE', *, *, #183764, .T. ) ;
#70052 = DIRECTION ( 'NONE',  ( 0.000000000000000000, 0.000000000000000000, -1.000000000000000000 ) ) ;
#70053 = VECTOR ( 'NONE', #197768, 1000.000000000000000 ) ;
#70054 = EDGE_CURVE ( 'NONE', #192900, #7521, #44015, .T. ) ;
#70055 = CARTESIAN_POINT ( 'NONE',  ( -16.85722902420155478, 9.950000000011169021, -113.2655474737703116 ) ) ;
#70056 = AXIS2_PLACEMENT_3D ( 'NONE', #130288, #91172, #31248 ) ;
#70057 = ORIENTED_EDGE ( 'NONE', *, *, #106856, .F. ) ;
#70058 = FACE_OUTER_BOUND ( 'NONE', #118252, .T. ) ;
#70060 = EDGE_CURVE ( 'NONE', #213743, #158833, #39583, .T. ) ;
#70059 = CARTESIAN_POINT ( 'NONE',  ( -21.52071067811865746, 7.779289321892505882, -54.65000000000000568 ) ) ;
#70061 = CIRCLE ( 'NONE', #249132, 0.4999999999999944489 ) ;
#70062 = EDGE_LOOP ( 'NONE', ( #168485, #83130, #103917, #133232 ) ) ;
#70063 = FACE_OUTER_BOUND ( 'NONE', #111814, .T. ) ;
#70064 = VERTEX_POINT ( 'NONE', #246079 ) ;
#70065 = AXIS2_PLACEMENT_3D ( 'NONE', #116293, #159273, #215366 ) ;
#70066 = ADVANCED_FACE ( 'NONE', ( #222627 ), #218587, .T. ) ;
#70067 = DIRECTION ( 'NONE',  ( 1.000000000000000000, 0.000000000000000000, 0.000000000000000000 ) ) ;
#70069 = ADVANCED_FACE ( 'NONE', ( #67427 ), #123557, .T. ) ;
#70068 = LINE ( 'NONE', #105277, #238779 ) ;
#70070 = CIRCLE ( 'NONE', #136670, 0.09999999999999963085 ) ;
#70073 = VERTEX_POINT ( 'NONE', #144368 ) ;
#70072 = VERTEX_POINT ( 'NONE', #242208 ) ;
#70071 = CARTESIAN_POINT ( 'NONE',  ( 21.05000000000000071, 1.162701749949165642, -41.60000000000000142 ) ) ;
#70074 = DIRECTION ( 'NONE',  ( 1.000000000000000000, 0.000000000000000000, 0.000000000000000000 ) ) ;
#70075 = CIRCLE ( 'NONE', #3392, 0.1000000000000001860 ) ;
#70076 = DIRECTION ( 'NONE',  ( 0.000000000000000000, -0.2617529984165152257, -0.9651348961777124202 ) ) ;
#70077 = CIRCLE ( 'NONE', #186779, 0.09999999999999990841 ) ;
#70078 = DIRECTION ( 'NONE',  ( 1.000000000000000000, 0.000000000000000000, 0.000000000000000000 ) ) ;
#70079 = AXIS2_PLACEMENT_3D ( 'NONE', #218118, #198568, #99451 ) ;
#70081 = DIRECTION ( 'NONE',  ( -1.000000000000000000, -2.952720810173289112E-16, 0.000000000000000000 ) ) ;
#70080 = DIRECTION ( 'NONE',  ( 0.000000000000000000, -0.5000000000000014433, 0.8660254037844378194 ) ) ;
#70082 = DIRECTION ( 'NONE',  ( -0.7071067811865474617, 0.7071067811865474617, 4.937700262164531476E-15 ) ) ;
#70083 = CYLINDRICAL_SURFACE ( 'NONE', #15347, 0.09999999999998898659 ) ;
#70084 = DIRECTION ( 'NONE',  ( 0.000000000000000000, 0.000000000000000000, 1.000000000000000000 ) ) ;
#70085 = AXIS2_PLACEMENT_3D ( 'NONE', #169509, #166933, #89911 ) ;
#70086 = SPHERICAL_SURFACE ( 'NONE', #88258, 0.1000000000000000056 ) ;
#70087 = EDGE_CURVE ( 'NONE', #226630, #20661, #53898, .T. ) ;
#70088 = EDGE_CURVE ( 'NONE', #214056, #13993, #244768, .T. ) ;
#70089 = ORIENTED_EDGE ( 'NONE', *, *, #113638, .T. ) ;
#70090 = EDGE_LOOP ( 'NONE', ( #127446, #117218, #235479, #130164 ) ) ;
#70091 = DIRECTION ( 'NONE',  ( 1.000000000000000000, 0.000000000000000000, 0.000000000000000000 ) ) ;
#70093 = EDGE_LOOP ( 'NONE', ( #170773, #186986, #8441, #90342 ) ) ;
#70092 = CARTESIAN_POINT ( 'NONE',  ( 21.05000000000000071, 10.48443348965288635, -174.9568058014918961 ) ) ;
#70094 = ORIENTED_EDGE ( 'NONE', *, *, #205337, .F. ) ;
#70095 = CARTESIAN_POINT ( 'NONE',  ( 18.39999999999999858, -9.499999999988842703, -141.0320693966996828 ) ) ;
#70096 = ORIENTED_EDGE ( 'NONE', *, *, #71219, .F. ) ;
#70097 = CARTESIAN_POINT ( 'NONE',  ( 22.47007471830800895, 33.50241300269675548, -242.5051845127899810 ) ) ;
#70098 = AXIS2_PLACEMENT_3D ( 'NONE', #15758, #129585, #209109 ) ;
#70099 = EDGE_CURVE ( 'NONE', #257642, #173164, #101876, .T. ) ;
#70100 = ORIENTED_EDGE ( 'NONE', *, *, #149399, .T. ) ;
#70101 = CARTESIAN_POINT ( 'NONE',  ( 18.52928932188133970, 10.27928932189249878, -125.2085786437627206 ) ) ;
#70102 = DIRECTION ( 'NONE',  ( -0.7071067811865388020, 0.7071067811865561215, 0.000000000000000000 ) ) ;
#70103 = EDGE_CURVE ( 'NONE', #16002, #249989, #135202, .T. ) ;
#70105 = ORIENTED_EDGE ( 'NONE', *, *, #248422, .F. ) ;
#70104 = ORIENTED_EDGE ( 'NONE', *, *, #129670, .F. ) ;
#70106 = ORIENTED_EDGE ( 'NONE', *, *, #180508, .F. ) ;
#70107 = EDGE_LOOP ( 'NONE', ( #17802, #197434, #117077, #88610 ) ) ;
#70108 = EDGE_LOOP ( 'NONE', ( #120378, #142118, #150522, #168990 ) ) ;
#70109 = CARTESIAN_POINT ( 'NONE',  ( -20.94999999999999929, 1.750000000011155743, -45.16951155790164307 ) ) ;
#70110 = CARTESIAN_POINT ( 'NONE',  ( 21.11701782572533048, 43.45044756046340240, -234.7603190085133633 ) ) ;
#70111 = CARTESIAN_POINT ( 'NONE',  ( -12.26136940704872025, 9.351403174152810749, -184.4795304368384734 ) ) ;
#70113 = ORIENTED_EDGE ( 'NONE', *, *, #184710, .F. ) ;
#70112 = DIRECTION ( 'NONE',  ( 0.000000000000000000, 0.000000000000000000, -1.000000000000000000 ) ) ;
#70114 = CARTESIAN_POINT ( 'NONE',  ( -23.15000000000000213, 85.00000000001222134, -145.8170766071767446 ) ) ;
#70115 = ADVANCED_FACE ( 'NONE', ( #187393 ), #166562, .F. ) ;
#70116 = PLANE ( 'NONE',  #236693 ) ;
#70118 = ORIENTED_EDGE ( 'NONE', *, *, #85466, .F. ) ;
#70117 = DIRECTION ( 'NONE',  ( -1.000000000000000000, 0.000000000000000000, -0.000000000000000000 ) ) ;
#70119 = DIRECTION ( 'NONE',  ( -1.000000000000000000, 0.000000000000000000, 0.000000000000000000 ) ) ;
#70120 = ORIENTED_EDGE ( 'NONE', *, *, #120521, .T. ) ;
#70121 = CARTESIAN_POINT ( 'NONE',  ( -23.15000000000000213, 76.00000000001172396, -71.62310748452431142 ) ) ;
#70122 = B_SPLINE_CURVE_WITH_KNOTS ( 'NONE', 3,
 ( #239749, #23291, #162789, #242298, #104054, #140632, #218876, #220185, #63663, #143194 ),
 .UNSPECIFIED., .F., .F.,
 ( 4, 3, 3, 4 ),
 ( 0.000000000000000000, 0.0002000000000008585893, 0.001000000000082977483, 0.001967863649483336721 ),
 .UNSPECIFIED. ) ;
#70123 = VERTEX_POINT ( 'NONE', #83100 ) ;
#70124 = DIRECTION ( 'NONE',  ( -1.000000000000000000, 1.836970198721029934E-16, 1.282749433769087757E-30 ) ) ;
#70126 = EDGE_CURVE ( 'NONE', #145746, #278, #127215, .T. ) ;
#70125 = ORIENTED_EDGE ( 'NONE', *, *, #142531, .F. ) ;
#70127 = AXIS2_PLACEMENT_3D ( 'NONE', #90083, #246596, #147507 ) ;
#70128 = AXIS2_PLACEMENT_3D ( 'NONE', #121533, #143622, #203603 ) ;
#70130 = DIRECTION ( 'NONE',  ( 1.000000000000000000, 0.000000000000000000, 0.000000000000000000 ) ) ;
#70129 = CARTESIAN_POINT ( 'NONE',  ( 21.05000000000000071, 76.00000000001267608, -203.5231074845243597 ) ) ;
#70131 = VECTOR ( 'NONE', #228932, 1000.000000000000000 ) ;
#70132 = DIRECTION ( 'NONE',  ( -4.448008912761043807E-16, 1.000000000000000000, 0.000000000000000000 ) ) ;
#70133 = B_SPLINE_CURVE_WITH_KNOTS ( 'NONE', 3,
 ( #243531, #161451, #140572, #25775 ),
 .UNSPECIFIED., .F., .F.,
 ( 4, 4 ),
 ( 0.000000000000000000, 7.713889350926964386E-05 ),
 .UNSPECIFIED. ) ;
#70134 = CARTESIAN_POINT ( 'NONE',  ( 20.94999999999999574, -1.162701749926853712, -75.10000000000003695 ) ) ;
#70135 = CARTESIAN_POINT ( 'NONE',  ( 20.94999999999999929, 74.63912941282058000, -195.4501095574334215 ) ) ;
#70136 = ORIENTED_EDGE ( 'NONE', *, *, #6400, .F. ) ;
#70137 = ORIENTED_EDGE ( 'NONE', *, *, #48714, .F. ) ;
#70138 = DIRECTION ( 'NONE',  ( 0.000000000000000000, -1.000000000000000000, -0.000000000000000000 ) ) ;
#70139 = CARTESIAN_POINT ( 'NONE',  ( 23.14999999999998437, 76.00000000001267608, -203.5231074845243597 ) ) ;
#70140 = ORIENTED_EDGE ( 'NONE', *, *, #158617, .F. ) ;
#70141 = PLANE ( 'NONE',  #155915 ) ;
#70142 = ORIENTED_EDGE ( 'NONE', *, *, #19451, .T. ) ;
#70143 = ADVANCED_FACE ( 'NONE', ( #90825 ), #129948, .F. ) ;
#70144 = CARTESIAN_POINT ( 'NONE',  ( -22.39999999999999858, -0.1008583690875575894, -55.25043287651065782 ) ) ;
#70145 = CARTESIAN_POINT ( 'NONE',  ( -20.85000000000000142, -1.135018845899022466, -74.71697688343232358 ) ) ;
#70146 = CARTESIAN_POINT ( 'NONE',  ( 21.14999999999999858, 1.115600667400684642E-11, -45.65000000000000568 ) ) ;
#70147 = AXIS2_PLACEMENT_3D ( 'NONE', #117960, #137505, #119264 ) ;
#70148 = ORIENTED_EDGE ( 'NONE', *, *, #202262, .T. ) ;
#70149 = AXIS2_PLACEMENT_3D ( 'NONE', #9, #83375, #102950 ) ;
#70150 = DIRECTION ( 'NONE',  ( 2.952720810173289112E-16, 1.000000000000000000, 6.982962677686266711E-15 ) ) ;
#70151 = VERTEX_POINT ( 'NONE', #110398 ) ;
#70152 = AXIS2_PLACEMENT_3D ( 'NONE', #164061, #23289, #27147 ) ;
#70153 = ORIENTED_EDGE ( 'NONE', *, *, #160574, .T. ) ;
#70154 = ORIENTED_EDGE ( 'NONE', *, *, #232700, .F. ) ;
#70155 = CARTESIAN_POINT ( 'NONE',  ( -23.25000000000000000, 71.65000000001228386, -157.8731074845243825 ) ) ;
#70156 = DIRECTION ( 'NONE',  ( 1.000000000000000000, -0.000000000000000000, -0.000000000000000000 ) ) ;
#70157 = DIRECTION ( 'NONE',  ( 0.000000000000000000, -6.652207440891554563E-15, 1.000000000000000000 ) ) ;
#70158 = CARTESIAN_POINT ( 'NONE',  ( -21.05000000000000071, -0.2561057920810652089, -133.9651035583277121 ) ) ;
#70159 = DIRECTION ( 'NONE',  ( 0.000000000000000000, 0.4999999999999478195, -0.8660254037844686836 ) ) ;
#70161 = CARTESIAN_POINT ( 'NONE',  ( 21.14999999999999858, 8.786607556600111835, -12.25000000000000000 ) ) ;
#70160 = CARTESIAN_POINT ( 'NONE',  ( -14.00000000000000178, 66.15000000001204228, -119.7731074845243739 ) ) ;
#70163 = VERTEX_POINT ( 'NONE', #149561 ) ;
#70162 = DIRECTION ( 'NONE',  ( 0.000000000000000000, 0.000000000000000000, -1.000000000000000000 ) ) ;
#70164 = CARTESIAN_POINT ( 'NONE',  ( -20.94999999999999929, 76.00000000001247713, -174.1231074845243540 ) ) ;
#70165 = EDGE_LOOP ( 'NONE', ( #35517, #172010, #135972, #207198 ) ) ;
#70166 = CARTESIAN_POINT ( 'NONE',  ( -20.64999999999999858, 63.46669608621377279, -222.0380013001639270 ) ) ;
#70167 = VERTEX_POINT ( 'NONE', #10024 ) ;
#70168 = ORIENTED_EDGE ( 'NONE', *, *, #124089, .T. ) ;
#70169 = CARTESIAN_POINT ( 'NONE',  ( 20.85000000000000142, 64.25000000001195133, -109.8069731475024753 ) ) ;
#70170 = CARTESIAN_POINT ( 'NONE',  ( -20.94999999999999929, -1.135018845899022466, -108.2169768834323662 ) ) ;
#70171 = CARTESIAN_POINT ( 'NONE',  ( -16.89268316805465986, 66.04827818676933759, -48.66735500597884823 ) ) ;
#70172 = DIRECTION ( 'NONE',  ( -0.000000000000000000, 6.982962677686266711E-15, -1.000000000000000000 ) ) ;
#70173 = CIRCLE ( 'NONE', #178496, 0.09999999999999939493 ) ;
#70174 = VECTOR ( 'NONE', #246443, 1000.000000000000000 ) ;
#70175 = VECTOR ( 'NONE', #84951, 1000.000000000000000 ) ;
#70176 = DIRECTION ( 'NONE',  ( 1.000000000000000000, 3.265361837132813093E-16, -0.000000000000000000 ) ) ;
#70177 = VERTEX_POINT ( 'NONE', #131248 ) ;
#70178 = ORIENTED_EDGE ( 'NONE', *, *, #129936, .F. ) ;
#70179 = DIRECTION ( 'NONE',  ( 1.000000000000000000, -2.952720810173289112E-16, -2.061873921506763405E-30 ) ) ;
#70180 = ORIENTED_EDGE ( 'NONE', *, *, #69954, .F. ) ;
#70181 = CARTESIAN_POINT ( 'NONE',  ( -18.39999999999999858, -9.499999999988849808, -107.4992856778388841 ) ) ;
#70182 = DIRECTION ( 'NONE',  ( 0.000000000000000000, -6.938893903907222067E-15, 1.000000000000000000 ) ) ;
#70183 = ORIENTED_EDGE ( 'NONE', *, *, #208089, .F. ) ;
#70184 = AXIS2_PLACEMENT_3D ( 'NONE', #233790, #50002, #129551 ) ;
#70185 = CARTESIAN_POINT ( 'NONE',  ( -21.64999999999999858, 11.10425270649115603, -208.0484446391143649 ) ) ;
#70186 = DIRECTION ( 'NONE',  ( 0.000000000000000000, 0.000000000000000000, -1.000000000000000000 ) ) ;
#70187 = DIRECTION ( 'NONE',  ( 0.000000000000000000, 0.000000000000000000, -1.000000000000000000 ) ) ;
#70188 = ORIENTED_EDGE ( 'NONE', *, *, #34414, .T. ) ;
#70189 = FACE_OUTER_BOUND ( 'NONE', #249576, .T. ) ;
#70190 = CARTESIAN_POINT ( 'NONE',  ( -21.00857864376268935, 11.60000000001115161, -140.9282032302755852 ) ) ;
#70191 = DIRECTION ( 'NONE',  ( 0.000000000000000000, 0.000000000000000000, -1.000000000000000000 ) ) ;
#70192 = FACE_OUTER_BOUND ( 'NONE', #73493, .T. ) ;
#70194 = ADVANCED_FACE ( 'NONE', ( #54269 ), #239647, .F. ) ;
#70193 = DIRECTION ( 'NONE',  ( 0.000000000000000000, 0.8814952561688428334, -0.4721928772777348460 ) ) ;
#70195 = CIRCLE ( 'NONE', #136786, 0.09999999999999949207 ) ;
#70196 = CARTESIAN_POINT ( 'NONE',  ( -21.05439746398122836, 57.72057112225034814, -226.0333164516449074 ) ) ;
#70197 = CIRCLE ( 'NONE', #36880, 0.09999999999999939493 ) ;
#70198 = CIRCLE ( 'NONE', #3508, 0.09999999999999939493 ) ;
#70199 = ORIENTED_EDGE ( 'NONE', *, *, #155694, .F. ) ;
#70200 = CIRCLE ( 'NONE', #36889, 14.20833333333333748 ) ;
#70201 = CARTESIAN_POINT ( 'NONE',  ( 22.50000000000000000, -2.381330705637465961, -189.5959759702857923 ) ) ;
#70202 = ADVANCED_FACE ( 'NONE', ( #209501 ), #114751, .T. ) ;
#70203 = VERTEX_POINT ( 'NONE', #50406 ) ;
#70204 = DIRECTION ( 'NONE',  ( 0.000000000000000000, 0.8660254037844420383, -0.4999999999999943379 ) ) ;
#70205 = DIRECTION ( 'NONE',  ( 0.000000000000000000, 0.03181660087583048496, -0.9994937237965570986 ) ) ;
#70206 = CARTESIAN_POINT ( 'NONE',  ( 22.39999999999999503, 64.25000000001269029, -203.5231074845244166 ) ) ;
#70207 = CARTESIAN_POINT ( 'NONE',  ( 20.97565083910961548, 65.52538259873351478, -162.4451643079358973 ) ) ;
#70208 = AXIS2_PLACEMENT_3D ( 'NONE', #99352, #78516, #1547 ) ;
#70209 = EDGE_CURVE ( 'NONE', #238726, #206520, #217729, .T. ) ;
#70210 = ORIENTED_EDGE ( 'NONE', *, *, #227679, .T. ) ;
#70211 = CARTESIAN_POINT ( 'NONE',  ( -23.15000000000000213, 76.00000000001234923, -165.8731074845243825 ) ) ;
#70212 = DIRECTION ( 'NONE',  ( -3.265361837132813093E-16, -1.000000000000000000, 7.445645354460596589E-46 ) ) ;
#70213 = CARTESIAN_POINT ( 'NONE',  ( -20.94999999999999929, 78.48087866980282001, -232.8271061603568910 ) ) ;
#70214 = DIRECTION ( 'NONE',  ( -1.000000000000000000, -0.000000000000000000, -0.000000000000000000 ) ) ;
#70215 = AXIS2_PLACEMENT_3D ( 'NONE', #112276, #250473, #251764 ) ;
#70216 = CARTESIAN_POINT ( 'NONE',  ( 13.40000000000005898, 64.35000000001120668, -23.62310748452479103 ) ) ;
#70217 = CIRCLE ( 'NONE', #20121, 0.6000000000000015321 ) ;
#70218 = AXIS2_PLACEMENT_3D ( 'NONE', #34009, #229607, #10565 ) ;
#70220 = ORIENTED_EDGE ( 'NONE', *, *, #211029, .F. ) ;
#70219 = AXIS2_PLACEMENT_3D ( 'NONE', #125273, #48295, #185241 ) ;
#70221 = ORIENTED_EDGE ( 'NONE', *, *, #194813, .F. ) ;
#70222 = DIRECTION ( 'NONE',  ( 0.000000000000000000, 0.000000000000000000, -1.000000000000000000 ) ) ;
#70223 = AXIS2_PLACEMENT_3D ( 'NONE', #183529, #47837, #145666 ) ;
#70224 = DIRECTION ( 'NONE',  ( 0.000000000000000000, 6.938893903907229955E-15, -1.000000000000000000 ) ) ;
#70226 = EDGE_CURVE ( 'NONE', #174804, #56502, #92121, .T. ) ;
#70225 = DIRECTION ( 'NONE',  ( 0.7071067811865475727, 0.7071067811865475727, 4.937700262164531476E-15 ) ) ;
#70227 = CARTESIAN_POINT ( 'NONE',  ( -21.93340585972067558, 68.67585297715902470, -170.0231074845244166 ) ) ;
#70228 = EDGE_CURVE ( 'NONE', #4224, #179208, #249921, .T. ) ;
#70229 = CIRCLE ( 'NONE', #207586, 0.09999999999999939493 ) ;
#70230 = ORIENTED_EDGE ( 'NONE', *, *, #81122, .T. ) ;
#70231 = CARTESIAN_POINT ( 'NONE',  ( 20.94999999999999929, 67.12338541492553645, -195.1380270056797599 ) ) ;
#70232 = ADVANCED_FACE ( 'NONE', ( #234186 ), #231289, .T. ) ;
#70233 = CARTESIAN_POINT ( 'NONE',  ( -23.25000000000000000, -3.275978944802464099, -228.2735455795363748 ) ) ;
#70234 = ORIENTED_EDGE ( 'NONE', *, *, #118793, .T. ) ;
#70235 = CARTESIAN_POINT ( 'NONE',  ( -20.64999999999999858, 76.00000000001259082, -190.6481074845243597 ) ) ;
#70236 = PRODUCT ( 'Fixed End Mounting Bracket', 'Fixed End Mounting Bracket', '', ( #100313 ) ) ;
#70237 = AXIS2_PLACEMENT_3D ( 'NONE', #142335, #64096, #186625 ) ;
#70238 = CLOSED_SHELL ( 'NONE', ( #156038, #151986, #165286, #181173, #146567, #207141, #249737, #205129, #18393, #44650, #133858, #120687, #223274, #6449, #128237, #30548, #132912, #225481, #199328, #251166, #105409, #90641, #147609, #216265, #18409, #17482, #192662, #116996, #10778, #196810, #62403, #106446, #16128, #201043, #113839, #163083, #161744, #254672, #162233, #205281, #242621, #91417, #26779, #113582, #111580, #127960, #205772, #227763, #140719, #172187, #236461, #59799, #170825, #243974, #153698, #196579, #245799, #241565, #19371, #23255, #212151, #3662, #136327, #191387, #208938, #152479, #173711, #58190, #129451, #12907, #177928, #118972, #71449, #253888, #131366, #9865, #140709, #224927, #104081, #243341, #225738, #140622, #71109, #240405, #187385, #40796, #203202, #90873, #220736, #162076, #126135, #239465, #176225, #14445, #169993, #17552, #219992, #93244, #49901, #226583, #36319, #67331, #221472, #163281, #230359, #254607, #87071, #188957, #108193, #128620, #110308, #28749, #213422, #205385, #9438, #39809, #96174, #80471, #140876, #156329, #82434, #210405, #28583, #241645, #57259, #216479, #64113, #125527, #120207, #72999, #101243, #97025, #190102, #83958, #129697, #207316, #245022, #109985, #52330, #79855, #58180, #221057, #8076, #257676, #102523, #62659, #231135, #251882, #199868, #181607, #232372, #222181, #162131, #39959, #148593, #150214, #723, #37610, #165890, #109978, #215486, #142594, #105914, #169005, #140769, #193877, #165182, #81565, #58961, #49395, #185634, #178632, #188665, #220859, #11782, #72615, #60559, #25431, #42081, #117702, #212759, #89176, #175527, #247333, #256135, #67455, #245990, #218963, #100151, #121508, #91360, #215715, #190450, #102046, #80806, #127688, #119727, #199554, #1730, #36489, #62224, #13470, #111695, #12189, #236541, #90217, #247793, #9359, #114692, #103946, #199131, #226484, #41365, #6154, #84769, #169053, #87690, #65026, #120079, #240797, #186487, #87227, #31235, #182973, #168629, #96005, #931, #133012, #85615, #244815, #220009, #59356, #123072, #216318, #79889, #202435, #249432, #38096, #136429, #33912, #98722, #89208, #195214, #160506, #204508, #103026, #102403, #234356, #89417, #210163, #180895, #248202, #83738, #112719, #143124, #178962, #205746, #75569, #245451, #208831, #75444, #77561, #152142, #115003, #55591, #128217, #175903, #252383, #43983, #172380, #197018, #254688, #200389, #142712, #8674, #94029, #3009, #241790, #10245, #196793, #121018, #208080, #226909, #78302, #18102, #28568, #42535, #1572, #24061, #174012, #28563, #10877, #253470, #125097, #133275, #139995, #48519, #186563, #123860, #231152, #41745, #168119, #151789, #165499, #79172, #69372, #46915, #118317, #188310, #206747, #237929, #147128, #211542, #105023, #5477, #150560, #15204, #255558, #122162, #232861, #43113, #149571, #210523, #175100, #206671, #222796, #198429, #39262, #112868, #231015, #66970, #133228, #223131, #215980, #185027, #244029, #54972, #96299, #249509, #251307, #62011, #88497, #162105, #136233, #84808, #237779, #200684, #133456, #158047, #63798, #53413, #133854, #66526, #140066, #89660, #52134, #110244, #208461, #186593, #218767, #121445, #195674, #46438, #57492, #145845, #84008, #78179, #229672, #79036, #148754, #80899, #72417, #99409, #70534, #50121, #231661, #241013, #208269, #37120, #76359, #250561, #54446, #66825, #148092, #108452, #255947, #82684, #115628, #227992, #38258, #96190, #141692, #209556, #5638, #6081, #122112, #214565, #158480, #160784, #215383, #164492, #87923, #23694, #188899, #239224, #61209, #67231, #191276, #226732, #222364, #156149, #24318, #239898, #90190, #29694, #62118, #239918, #142235, #102811, #108812, #232910, #65876, #12901, #228208, #62045, #20515, #196655, #143696, #137067, #42648, #241644, #135258, #160098, #60910, #112611, #100813, #74549, #65348, #183445, #223860, #98614, #104690, #155015, #135009, #16457, #59139, #91971, #129482, #179861, #138032, #110862, #114493, #32102, #217089, #121943, #2742, #51556, #48195, #88127, #171155, #128298, #187810, #32018, #180009, #12167, #26673, #151350, #67159, #26238, #170925, #113540, #137183, #252828, #55245, #138360, #119977, #219783, #26375 ) ) ;
#70239 = EDGE_CURVE ( 'NONE', #211510, #160294, #2290, .T. ) ;
#70240 = ORIENTED_EDGE ( 'NONE', *, *, #80755, .T. ) ;
#70241 = ORIENTED_EDGE ( 'NONE', *, *, #158202, .F. ) ;
#70242 = VERTEX_POINT ( 'NONE', #191255 ) ;
#70243 = DIRECTION ( 'NONE',  ( 0.000000000000000000, -1.000000000000000000, -6.982962677686266711E-15 ) ) ;
#70244 = CARTESIAN_POINT ( 'NONE',  ( 18.50000000000000000, 86.35479209693714608, -75.76656650145046967 ) ) ;
#70245 = LINE ( 'NONE', #113189, #244927 ) ;
#70246 = CARTESIAN_POINT ( 'NONE',  ( 18.39999999999999858, -9.499999999988842703, -140.6001893912220737 ) ) ;
#70248 = AXIS2_PLACEMENT_3D ( 'NONE', #145177, #190455, #230863 ) ;
#70247 = DIRECTION ( 'NONE',  ( -1.000000000000000000, -0.000000000000000000, -0.000000000000000000 ) ) ;
#70249 = DIRECTION ( 'NONE',  ( 0.000000000000000000, 0.2534589355813222089, 0.9673461469267261581 ) ) ;
#70250 = DIRECTION ( 'NONE',  ( 1.000000000000000000, 0.000000000000000000, 0.000000000000000000 ) ) ;
#70251 = AXIS2_PLACEMENT_3D ( 'NONE', #209849, #113301, #228129 ) ;
#70252 = EDGE_CURVE ( 'NONE', #149752, #237399, #63103, .T. ) ;
#70254 = DIRECTION ( 'NONE',  ( -1.000000000000000000, 0.000000000000000000, 0.000000000000000000 ) ) ;
#70253 = LINE ( 'NONE', #11544, #166056 ) ;
#70255 = PLANE ( 'NONE',  #62911 ) ;
#70256 = AXIS2_PLACEMENT_3D ( 'NONE', #42970, #122514, #102910 ) ;
#70257 = PLANE ( 'NONE',  #197830 ) ;
#70258 = FACE_OUTER_BOUND ( 'NONE', #89301, .T. ) ;
#70259 = CARTESIAN_POINT ( 'NONE',  ( 20.95561247346651967, 18.82560383811837568, -227.9789827151014947 ) ) ;
#70260 = EDGE_LOOP ( 'NONE', ( #32196, #231480, #200876, #161073 ) ) ;
#70261 = ORIENTED_EDGE ( 'NONE', *, *, #31082, .F. ) ;
#70262 = CARTESIAN_POINT ( 'NONE',  ( -18.58744394320964233, -9.566385154548546765, -40.32284805387602944 ) ) ;
#70263 = LINE ( 'NONE', #148491, #228642 ) ;
#70264 = CARTESIAN_POINT ( 'NONE',  ( -13.54036565897076372, 13.16206247923560113, -217.0199023716218960 ) ) ;
#70265 = AXIS2_PLACEMENT_3D ( 'NONE', #129759, #48932, #26840 ) ;
#70266 = SPHERICAL_SURFACE ( 'NONE', #60330, 0.1000000000000000056 ) ;
#70267 = CYLINDRICAL_SURFACE ( 'NONE', #133252, 0.1000000000000018374 ) ;
#70268 = LINE ( 'NONE', #245018, #148214 ) ;
#70269 = AXIS2_PLACEMENT_3D ( 'NONE', #50844, #144822, #204794 ) ;
#70270 = VERTEX_POINT ( 'NONE', #171699 ) ;
#70271 = ORIENTED_EDGE ( 'NONE', *, *, #11876, .F. ) ;
#70272 = TOROIDAL_SURFACE ( 'NONE', #41042, 0.2000000000000000111, 0.1000000000000000056 ) ;
#70273 = AXIS2_PLACEMENT_3D ( 'NONE', #110260, #114108, #172862 ) ;
#70274 = DIRECTION ( 'NONE',  ( -0.000000000000000000, -0.000000000000000000, 1.000000000000000000 ) ) ;
#70275 = ORIENTED_EDGE ( 'NONE', *, *, #250133, .F. ) ;
#70276 = DIRECTION ( 'NONE',  ( 1.000000000000000000, 0.000000000000000000, 0.000000000000000000 ) ) ;
#70277 = LINE ( 'NONE', #136283, #692 ) ;
#70278 = ADVANCED_FACE ( 'NONE', ( #174282 ), #84412, .T. ) ;
#70279 = EDGE_CURVE ( 'NONE', #156295, #104826, #202053, .T. ) ;
#70280 = EDGE_LOOP ( 'NONE', ( #199623, #238604, #130410 ) ) ;
#70281 = DIRECTION ( 'NONE',  ( 1.000000000000000000, -0.000000000000000000, -0.000000000000000000 ) ) ;
#70282 = ORIENTED_EDGE ( 'NONE', *, *, #1968, .T. ) ;
#70283 = ADVANCED_FACE ( 'NONE', ( #56814 ), #257554, .T. ) ;
#70285 = EDGE_CURVE ( 'NONE', #43985, #203363, #693, .T. ) ;
#70284 = LINE ( 'NONE', #230622, #99695 ) ;
#70286 = DIRECTION ( 'NONE',  ( 1.000000000000000000, 0.000000000000000000, 0.000000000000000000 ) ) ;
#70288 = CARTESIAN_POINT ( 'NONE',  ( 23.24999999999999645, 5.600000000011153389, -155.0947339810869323 ) ) ;
#70287 = VECTOR ( 'NONE', #204300, 1000.000000000000000 ) ;
#70289 = DIRECTION ( 'NONE',  ( 0.7071067811865475727, -0.7071067811865475727, 0.000000000000000000 ) ) ;
#70290 = DIRECTION ( 'NONE',  ( -0.000000000000000000, 1.000000000000000000, -0.000000000000000000 ) ) ;
#70291 = CARTESIAN_POINT ( 'NONE',  ( 20.94999999999999929, 45.77234354862702048, -239.5513518621457365 ) ) ;
#70292 = ADVANCED_FACE ( 'NONE', ( #76392 ), #60678, .T. ) ;
#70293 = CARTESIAN_POINT ( 'NONE',  ( -22.39999999999999858, 64.18196446391819165, -247.0985338183330668 ) ) ;
#70294 = CARTESIAN_POINT ( 'NONE',  ( 18.54999999999999716, 67.25000000001185185, -93.77310748452437394 ) ) ;
#70295 = ORIENTED_EDGE ( 'NONE', *, *, #70985, .T. ) ;
#70296 = DIRECTION ( 'NONE',  ( -1.000000000000000000, -6.649824375826082804E-14, -1.991473509853015959E-14 ) ) ;
#70297 = EDGE_LOOP ( 'NONE', ( #209590, #79354, #23600, #76546 ) ) ;
#70299 = VERTEX_POINT ( 'NONE', #217187 ) ;
#70298 = FACE_OUTER_BOUND ( 'NONE', #181741, .T. ) ;
#70300 = ADVANCED_FACE ( 'NONE', ( #214626 ), #196353, .F. ) ;
#70301 = ORIENTED_EDGE ( 'NONE', *, *, #21347, .T. ) ;
#70302 = CARTESIAN_POINT ( 'NONE',  ( -18.59999999999999787, 51.38014393322265505, -230.1906178717505611 ) ) ;
#70304 = EDGE_CURVE ( 'NONE', #13565, #16741, #41166, .T. ) ;
#70303 = EDGE_CURVE ( 'NONE', #139213, #212713, #48102, .T. ) ;
#70305 = DIRECTION ( 'NONE',  ( 0.000000000000000000, -1.000000000000000000, 0.000000000000000000 ) ) ;
#70306 = CARTESIAN_POINT ( 'NONE',  ( 21.05000000000000071, 62.99095723518624368, -207.1734234082435080 ) ) ;
#70307 = DIRECTION ( 'NONE',  ( 0.000000000000000000, -0.000000000000000000, 1.000000000000000000 ) ) ;
#70308 = FACE_OUTER_BOUND ( 'NONE', #176237, .T. ) ;
#70309 = DIRECTION ( 'NONE',  ( 1.000000000000000000, -1.646408749285562060E-14, -1.073024830501232702E-15 ) ) ;
#70310 = CARTESIAN_POINT ( 'NONE',  ( 18.39999999999999858, -9.682403433465241349, -207.6568433774127413 ) ) ;
#70311 = CARTESIAN_POINT ( 'NONE',  ( -16.79363873026997922, 51.61582291306198300, -231.9490907809428961 ) ) ;
#70312 = ADVANCED_FACE ( 'NONE', ( #176815 ), #39766, .T. ) ;
#70313 = DIRECTION ( 'NONE',  ( 0.000000000000000000, 6.982962677686266711E-15, -1.000000000000000000 ) ) ;
#70314 = AXIS2_PLACEMENT_3D ( 'NONE', #185040, #68970, #27291 ) ;
#70315 = ORIENTED_EDGE ( 'NONE', *, *, #144830, .F. ) ;
#70316 = EDGE_LOOP ( 'NONE', ( #108487, #120675, #18070, #96907 ) ) ;
#70317 = AXIS2_PLACEMENT_3D ( 'NONE', #185536, #207680, #51130 ) ;
#70318 = CARTESIAN_POINT ( 'NONE',  ( -16.94445028196808778, 9.992063609708889516, -180.1073301784184366 ) ) ;
#70319 = EDGE_CURVE ( 'NONE', #192243, #158502, #193855, .T. ) ;
#70320 = AXIS2_PLACEMENT_3D ( 'NONE', #6690, #84912, #223161 ) ;
#70321 = EDGE_CURVE ( 'NONE', #43558, #225791, #180653, .T. ) ;
#70322 = VERTEX_POINT ( 'NONE', #101052 ) ;
#70323 = LINE ( 'NONE', #149843, #146555 ) ;
#70324 = ORIENTED_EDGE ( 'NONE', *, *, #236536, .T. ) ;
#70325 = CARTESIAN_POINT ( 'NONE',  ( 18.33996824403465808, -9.569639859431823936, -40.31906563751653039 ) ) ;
#70326 = EDGE_CURVE ( 'NONE', #208846, #41312, #56285, .T. ) ;
#70327 = VECTOR ( 'NONE', #6967, 1000.000000000000000 ) ;
#70328 = CARTESIAN_POINT ( 'NONE',  ( -16.91049119928364775, 9.950000000011138823, -180.1182796068091250 ) ) ;
#70329 = DIRECTION ( 'NONE',  ( 0.000000000000000000, 0.000000000000000000, -1.000000000000000000 ) ) ;
#70330 = CARTESIAN_POINT ( 'NONE',  ( -20.85000000000000142, 77.83585931145498193, -24.41866831572578533 ) ) ;
#70331 = LINE ( 'NONE', #49451, #49737 ) ;
#70332 = ORIENTED_EDGE ( 'NONE', *, *, #138813, .F. ) ;
#70333 = EDGE_CURVE ( 'NONE', #170452, #87006, #227162, .T. ) ;
#70334 = LINE ( 'NONE', #187699, #120272 ) ;
#70335 = AXIS2_PLACEMENT_3D ( 'NONE', #82262, #125285, #5294 ) ;
#70336 = DIRECTION ( 'NONE',  ( 0.000000000000000000, 0.9126074666063768159, 0.4088369013363282178 ) ) ;
#70338 = VECTOR ( 'NONE', #216175, 1000.000000000000000 ) ;
#70337 = CARTESIAN_POINT ( 'NONE',  ( -18.59999999999999787, -1.835341550213255957, -45.15515129256298366 ) ) ;
#70339 = CARTESIAN_POINT ( 'NONE',  ( 18.50000000000000000, -9.399999999999998579, -7.297259759663296208 ) ) ;
#70340 = DIRECTION ( 'NONE',  ( 1.000000000000000000, 0.000000000000000000, 0.000000000000000000 ) ) ;
#70341 = ORIENTED_EDGE ( 'NONE', *, *, #43529, .F. ) ;
#70343 = DIRECTION ( 'NONE',  ( 1.000000000000000000, 0.000000000000000000, 0.000000000000000000 ) ) ;
#70342 = CARTESIAN_POINT ( 'NONE',  ( 21.08198257630413508, 61.09658931423916073, -234.2666139183525615 ) ) ;
#70344 = EDGE_LOOP ( 'NONE', ( #82923, #180315, #92043, #224348 ) ) ;
#70347 = ORIENTED_EDGE ( 'NONE', *, *, #208091, .T. ) ;
#70346 = CARTESIAN_POINT ( 'NONE',  ( 22.60000000000000142, 64.25043287652275126, -136.6239658536230763 ) ) ;
#70345 = DIRECTION ( 'NONE',  ( -1.000000000000000000, 0.000000000000000000, -0.000000000000000000 ) ) ;
#70348 = CIRCLE ( 'NONE', #45358, 11.80000000000000782 ) ;
#70349 = CARTESIAN_POINT ( 'NONE',  ( 22.45305468355011058, 76.10085836911173374, -114.7726746080140288 ) ) ;
#70350 = DIRECTION ( 'NONE',  ( 0.000000000000000000, 0.8814952561688428334, -0.4721928772777350125 ) ) ;
#70351 = DIRECTION ( 'NONE',  ( 0.000000000000000000, 0.000000000000000000, -1.000000000000000000 ) ) ;
#70352 = EDGE_LOOP ( 'NONE', ( #23029, #165674, #149243, #143538 ) ) ;
#70353 = DIRECTION ( 'NONE',  ( -0.000000000000000000, 0.4721928772777345684, 0.8814952561688429444 ) ) ;
#70354 = DIRECTION ( 'NONE',  ( 0.000000000000000000, -6.982962677686266711E-15, 1.000000000000000000 ) ) ;
#70356 = DIRECTION ( 'NONE',  ( 0.000000000000000000, -0.2128009952263601456, 0.9770955615653316162 ) ) ;
#70355 = DIRECTION ( 'NONE',  ( 1.000000000000000000, -0.000000000000000000, -0.000000000000000000 ) ) ;
#70358 = ORIENTED_EDGE ( 'NONE', *, *, #215198, .T. ) ;
#70357 = FACE_OUTER_BOUND ( 'NONE', #49422, .T. ) ;
#70359 = EDGE_LOOP ( 'NONE', ( #141866, #187877, #33487, #217256 ) ) ;
#70360 = DIRECTION ( 'NONE',  ( -0.000000000000000000, 6.982962677686266711E-15, -1.000000000000000000 ) ) ;
#70361 = FACE_OUTER_BOUND ( 'NONE', #82152, .T. ) ;
#70362 = AXIS2_PLACEMENT_3D ( 'NONE', #215009, #91230, #35138 ) ;
#70363 = CIRCLE ( 'NONE', #45190, 7.900000000000000355 ) ;
#70364 = DIRECTION ( 'NONE',  ( 0.000000000000000000, 0.000000000000000000, 1.000000000000000000 ) ) ;
#70365 = ORIENTED_EDGE ( 'NONE', *, *, #193486, .F. ) ;
#70366 = DIRECTION ( 'NONE',  ( 0.000000000000000000, 0.000000000000000000, -1.000000000000000000 ) ) ;
#70367 = DIRECTION ( 'NONE',  ( 0.000000000000000000, 0.000000000000000000, -1.000000000000000000 ) ) ;
#70368 = DIRECTION ( 'NONE',  ( 0.000000000000000000, -6.982962677686266711E-15, 1.000000000000000000 ) ) ;
#70369 = AXIS2_PLACEMENT_3D ( 'NONE', #89639, #242300, #63665 ) ;
#70370 = VERTEX_POINT ( 'NONE', #58108 ) ;
#70371 = CARTESIAN_POINT ( 'NONE',  ( 20.97107704358301916, 60.90557777443898146, -225.2713797486721887 ) ) ;
#70372 = EDGE_CURVE ( 'NONE', #77802, #212831, #77143, .T. ) ;
#70373 = VERTEX_POINT ( 'NONE', #118108 ) ;
#70374 = TOROIDAL_SURFACE ( 'NONE', #182788, 0.2000000000000000111, 0.1000000000000000056 ) ;
#70376 = AXIS2_PLACEMENT_3D ( 'NONE', #39384, #19804, #178899 ) ;
#70375 = DIRECTION ( 'NONE',  ( 0.000000000000000000, 0.9908441862701791170, -0.1350103645450472789 ) ) ;
#70378 = EDGE_CURVE ( 'NONE', #101254, #44131, #122946, .T. ) ;
#70377 = PLANE ( 'NONE',  #110654 ) ;
#70379 = AXIS2_PLACEMENT_3D ( 'NONE', #191560, #71604, #108148 ) ;
#70380 = ORIENTED_EDGE ( 'NONE', *, *, #245879, .F. ) ;
#70381 = VERTEX_POINT ( 'NONE', #16465 ) ;
#70382 = AXIS2_PLACEMENT_3D ( 'NONE', #239240, #60584, #33707 ) ;
#70383 = EDGE_CURVE ( 'NONE', #75395, #4930, #178102, .T. ) ;
#70384 = CARTESIAN_POINT ( 'NONE',  ( -20.54999999999999716, 1.115600667400684642E-11, -169.4000000000000625 ) ) ;
#70385 = EDGE_LOOP ( 'NONE', ( #19992, #237081, #100657, #233698, #17691 ) ) ;
#70388 = EDGE_CURVE ( 'NONE', #185684, #168941, #10521, .T. ) ;
#70387 = VERTEX_POINT ( 'NONE', #39879 ) ;
#70386 = CARTESIAN_POINT ( 'NONE',  ( 22.45463910399148588, 26.02743911761160689, -254.3139371331799623 ) ) ;
#70389 = ORIENTED_EDGE ( 'NONE', *, *, #162242, .F. ) ;
#70390 = CIRCLE ( 'NONE', #220766, 2.000000000000002665 ) ;
#70391 = AXIS2_PLACEMENT_3D ( 'NONE', #31131, #174514, #251419 ) ;
#70394 = EDGE_LOOP ( 'NONE', ( #169325, #4050, #221303, #236829, #246086 ) ) ;
#70393 = ORIENTED_EDGE ( 'NONE', *, *, #54521, .T. ) ;
#70392 = CARTESIAN_POINT ( 'NONE',  ( -20.85000000000000142, 7.070967871809997973, -171.2465642218683115 ) ) ;
#70395 = CARTESIAN_POINT ( 'NONE',  ( 18.59999999999999787, -9.849999999999994316, 30.09999999999999076 ) ) ;
#70397 = ORIENTED_EDGE ( 'NONE', *, *, #5441, .T. ) ;
#70396 = AXIS2_PLACEMENT_3D ( 'NONE', #237030, #153701, #17965 ) ;
#70398 = CARTESIAN_POINT ( 'NONE',  ( 23.14999999999999858, 67.44464249442897597, -214.0562211244547655 ) ) ;
#70399 = CYLINDRICAL_SURFACE ( 'NONE', #57571, 0.09999999999999939493 ) ;
#70400 = DIRECTION ( 'NONE',  ( 0.000000000000000000, -6.467318590049456648E-15, 1.000000000000000000 ) ) ;
#70401 = ADVANCED_FACE ( 'NONE', ( #241895 ), #46361, .T. ) ;
#70402 = CIRCLE ( 'NONE', #20310, 12.87499999999999822 ) ;
#70403 = CARTESIAN_POINT ( 'NONE',  ( -22.50000000000094147, 25.98655542988606726, -254.2226763854396552 ) ) ;
#70406 = EDGE_CURVE ( 'NONE', #932, #168498, #247836, .T. ) ;
#70405 = ORIENTED_EDGE ( 'NONE', *, *, #21428, .F. ) ;
#70404 = AXIS2_PLACEMENT_3D ( 'NONE', #171930, #149781, #72818 ) ;
#70407 = CIRCLE ( 'NONE', #103655, 0.1000000000000004496 ) ;
#70408 = ORIENTED_EDGE ( 'NONE', *, *, #16209, .T. ) ;
#70409 = AXIS2_PLACEMENT_3D ( 'NONE', #48271, #192931, #30024 ) ;
#70410 = EDGE_LOOP ( 'NONE', ( #212076, #1396, #161691, #174411 ) ) ;
#70411 = CARTESIAN_POINT ( 'NONE',  ( 20.94999999999999574, 74.83729825007431202, -162.0231074845243597 ) ) ;
#70413 = ORIENTED_EDGE ( 'NONE', *, *, #95887, .T. ) ;
#70412 = DIRECTION ( 'NONE',  ( -0.000000000000000000, 1.000000000000000000, 0.000000000000000000 ) ) ;
#70414 = CARTESIAN_POINT ( 'NONE',  ( 21.14999999999999858, 76.00000000001271871, -210.0637644362255969 ) ) ;
#70416 = ORIENTED_EDGE ( 'NONE', *, *, #2874, .T. ) ;
#70415 = CARTESIAN_POINT ( 'NONE',  ( 18.50000000000000000, 78.21920797885123022, -231.3255576768048911 ) ) ;
#70417 = AXIS2_PLACEMENT_3D ( 'NONE', #124292, #79984, #142543 ) ;
#70418 = ORIENTED_EDGE ( 'NONE', *, *, #36955, .T. ) ;
#70419 = CARTESIAN_POINT ( 'NONE',  ( -18.50000000000000000, 80.78317333349157536, -192.9003134612048882 ) ) ;
#70420 = ADVANCED_FACE ( 'NONE', ( #87939 ), #38032, .F. ) ;
#70421 = ORIENTED_EDGE ( 'NONE', *, *, #204337, .T. ) ;
#70422 = CARTESIAN_POINT ( 'NONE',  ( -16.92570016628982543, 66.04121104227236572, -149.1437581545634430 ) ) ;
#70423 = CARTESIAN_POINT ( 'NONE',  ( 18.59999999999999432, 77.16270174994990327, -94.92310748452430857 ) ) ;
#70424 = EDGE_CURVE ( 'NONE', #101287, #12212, #221044, .T. ) ;
#70425 = CIRCLE ( 'NONE', #120483, 0.1000000000000028644 ) ;
#70427 = EDGE_LOOP ( 'NONE', ( #102076, #135568, #165334 ) ) ;
#70426 = VERTEX_POINT ( 'NONE', #226151 ) ;
#70428 = ORIENTED_EDGE ( 'NONE', *, *, #183640, .F. ) ;
#70429 = CARTESIAN_POINT ( 'NONE',  ( -18.35235881385853318, 13.17903599427090633, -207.5965789609904846 ) ) ;
#70430 = VERTEX_POINT ( 'NONE', #121962 ) ;
#70431 = ORIENTED_EDGE ( 'NONE', *, *, #194607, .F. ) ;
#70432 = DIRECTION ( 'NONE',  ( 0.000000000000000000, -0.9126074666063660468, -0.4088369013363524762 ) ) ;
#70434 = ORIENTED_EDGE ( 'NONE', *, *, #36684, .F. ) ;
#70433 = DIRECTION ( 'NONE',  ( 0.000000000000000000, 0.9908441862701605762, 0.1350103645451835310 ) ) ;
#70435 = LINE ( 'NONE', #151231, #77437 ) ;
#70437 = CARTESIAN_POINT ( 'NONE',  ( -18.40000000000000213, 5.650000000011139001, -146.6500000000000341 ) ) ;
#70436 = DIRECTION ( 'NONE',  ( 0.000000000000000000, 1.000000000000000000, 6.938893903907222067E-15 ) ) ;
#70438 = EDGE_CURVE ( 'NONE', #13347, #213820, #110452, .T. ) ;
#70439 = CARTESIAN_POINT ( 'NONE',  ( 22.39999999999999503, 1.115600667400684642E-11, -55.35042919245524473 ) ) ;
#70440 = CARTESIAN_POINT ( 'NONE',  ( -13.12432614554022869, 62.11595298889567118, -218.6870723643518772 ) ) ;
#70441 = VERTEX_POINT ( 'NONE', #145362 ) ;
#70442 = CIRCLE ( 'NONE', #249475, 12.97499999999999076 ) ;
#70443 = EDGE_CURVE ( 'NONE', #126094, #44687, #256142, .T. ) ;
#70444 = AXIS2_PLACEMENT_3D ( 'NONE', #244094, #9338, #4199 ) ;
#70445 = ORIENTED_EDGE ( 'NONE', *, *, #236743, .F. ) ;
#70446 = CARTESIAN_POINT ( 'NONE',  ( -20.94999999999999929, -11.64999999998884483, -170.3999999999999773 ) ) ;
#70447 = DIRECTION ( 'NONE',  ( -1.000000000000000000, -0.000000000000000000, -0.000000000000000000 ) ) ;
#70448 = TOROIDAL_SURFACE ( 'NONE', #103689, 0.6000000000000006439, 0.1000000000000000056 ) ;
#70450 = EDGE_CURVE ( 'NONE', #193873, #149301, #73092, .T. ) ;
#70449 = VERTEX_POINT ( 'NONE', #63255 ) ;
#70451 = AXIS2_PLACEMENT_3D ( 'NONE', #192311, #250975, #231448 ) ;
#70452 = CARTESIAN_POINT ( 'NONE',  ( -20.54999999999999716, 9.350000000011156942, -88.25000000000005684 ) ) ;
#70453 = CARTESIAN_POINT ( 'NONE',  ( -20.94999999999999929, 64.25000000001263345, -196.5083017138704236 ) ) ;
#70454 = ORIENTED_EDGE ( 'NONE', *, *, #94419, .T. ) ;
#70455 = VERTEX_POINT ( 'NONE', #82784 ) ;
#70456 = CARTESIAN_POINT ( 'NONE',  ( -0.000000000000000000, -11.25000000000000000, 10.10000000000000142 ) ) ;
#70457 = DIRECTION ( 'NONE',  ( 0.000000000000000000, 0.9673461469267252699, -0.2534589355813257061 ) ) ;
#70458 = VERTEX_POINT ( 'NONE', #47533 ) ;
#70459 = PLANE ( 'NONE',  #80470 ) ;
#70460 = VERTEX_POINT ( 'NONE', #127093 ) ;
#70461 = ADVANCED_FACE ( 'NONE', ( #107523 ), #201483, .F. ) ;
#70462 = CARTESIAN_POINT ( 'NONE',  ( 20.94999999999999574, 1.835341550235567887, -45.05515129256298223 ) ) ;
#70463 = CARTESIAN_POINT ( 'NONE',  ( 18.39999999999999503, 55.18266668263805030, -231.5853321237989633 ) ) ;
#70465 = CARTESIAN_POINT ( 'NONE',  ( 20.73486653747088937, 7.750000000011182166, -143.2500000000000284 ) ) ;
#70464 = DIRECTION ( 'NONE',  ( 1.000000000000000000, 0.000000000000000000, 0.000000000000000000 ) ) ;
#70466 = CARTESIAN_POINT ( 'NONE',  ( -16.95709691156326215, 9.950000000011138823, -87.83994243749135933 ) ) ;
#70468 = AXIS2_PLACEMENT_3D ( 'NONE', #250117, #68934, #148460 ) ;
#70467 = CARTESIAN_POINT ( 'NONE',  ( -14.00000000000000178, 66.15000000001258229, -186.7731074845244166 ) ) ;
#70469 = DIRECTION ( 'NONE',  ( 0.000000000000000000, 0.2617529984162567103, 0.9651348961777825863 ) ) ;
#70471 = EDGE_CURVE ( 'NONE', #102565, #3257, #139666, .T. ) ;
#70470 = CARTESIAN_POINT ( 'NONE',  ( -21.10000000000000142, -11.64999999999999858, 11.89999999999999680 ) ) ;
#70472 = AXIS2_PLACEMENT_3D ( 'NONE', #17421, #136059, #233903 ) ;
#70474 = ORIENTED_EDGE ( 'NONE', *, *, #43645, .F. ) ;
#70473 = DIRECTION ( 'NONE',  ( 0.000000000000000000, 0.000000000000000000, -1.000000000000000000 ) ) ;
#70475 = AXIS2_PLACEMENT_3D ( 'NONE', #146299, #49772, #126744 ) ;
#70477 = EDGE_LOOP ( 'NONE', ( #175820, #45166, #236457, #164916 ) ) ;
#70476 = ORIENTED_EDGE ( 'NONE', *, *, #79494, .F. ) ;
#70478 = ORIENTED_EDGE ( 'NONE', *, *, #200564, .T. ) ;
#70480 = EDGE_CURVE ( 'NONE', #15261, #135372, #14876, .T. ) ;
#70479 = DIRECTION ( 'NONE',  ( 0.000000000000000000, 0.1298341882519953583, 0.9915357197604861561 ) ) ;
#70481 = FACE_OUTER_BOUND ( 'NONE', #215145, .T. ) ;
#70483 = FACE_OUTER_BOUND ( 'NONE', #240295, .T. ) ;
#70482 = DIRECTION ( 'NONE',  ( 1.000000000000000000, -0.000000000000000000, -0.000000000000000000 ) ) ;
#70484 = DIRECTION ( 'NONE',  ( 1.000000000000000000, 0.000000000000000000, 0.000000000000000000 ) ) ;
#70485 = EDGE_LOOP ( 'NONE', ( #2025, #9443, #115537, #40172 ) ) ;
#70486 = FACE_OUTER_BOUND ( 'NONE', #191448, .T. ) ;
#70487 = ORIENTED_EDGE ( 'NONE', *, *, #2110, .F. ) ;
#70488 = CARTESIAN_POINT ( 'NONE',  ( -18.59999999999999787, 74.16465844978819177, -191.9679561919613775 ) ) ;
#70489 = DIRECTION ( 'NONE',  ( 1.000000000000000000, 0.000000000000000000, 0.000000000000000000 ) ) ;
#70490 = CARTESIAN_POINT ( 'NONE',  ( -21.05000000000000071, 1.371682548295136472, -230.7621968047018584 ) ) ;
#70491 = ORIENTED_EDGE ( 'NONE', *, *, #230696, .T. ) ;
#70492 = DIRECTION ( 'NONE',  ( 0.000000000000000000, 6.982962677686266711E-15, -1.000000000000000000 ) ) ;
#70493 = CARTESIAN_POINT ( 'NONE',  ( 18.59999999999998366, 76.00000000001170974, -69.52310748452431710 ) ) ;
#70494 = VERTEX_POINT ( 'NONE', #207938 ) ;
#70495 = EDGE_LOOP ( 'NONE', ( #124187, #163688, #178657, #68074, #225567 ) ) ;
#70496 = DIRECTION ( 'NONE',  ( 0.000000000000000000, -0.1298341882520022694, -0.9915357197604853789 ) ) ;
#70497 = FACE_OUTER_BOUND ( 'NONE', #243674, .T. ) ;
#70498 = CARTESIAN_POINT ( 'NONE',  ( 18.39999999999999503, 64.25000000001159606, -56.87310748452440379 ) ) ;
#70499 = CARTESIAN_POINT ( 'NONE',  ( 20.95392731769792150, 67.11693852082284195, -61.00087950495308320 ) ) ;
#70500 = CARTESIAN_POINT ( 'NONE',  ( 20.94999999999999929, 76.00000000001237765, -170.0231074845243597 ) ) ;
#70501 = DIRECTION ( 'NONE',  ( 1.000000000000000000, 0.000000000000000000, 0.000000000000000000 ) ) ;
#70502 = EDGE_LOOP ( 'NONE', ( #209049, #575, #16363, #120134 ) ) ;
#70503 = CARTESIAN_POINT ( 'NONE',  ( 23.14999999999999858, 10.71906255309368383, -222.4921384173655383 ) ) ;
#70504 = CARTESIAN_POINT ( 'NONE',  ( -16.87331047859649757, 66.05000000001224691, -149.1731074845244223 ) ) ;
#70506 = CARTESIAN_POINT ( 'NONE',  ( -20.94684162708999864, 11.74999999080544022, -174.3416440060701973 ) ) ;
#70505 = DIRECTION ( 'NONE',  ( 0.000000000000000000, 0.000000000000000000, -1.000000000000000000 ) ) ;
#70507 = CARTESIAN_POINT ( 'NONE',  ( 23.14999999999999858, 1.115600667400684642E-11, -67.00000000000000000 ) ) ;
#70508 = DIRECTION ( 'NONE',  ( 0.000000000000000000, -1.000000000000000000, 0.000000000000000000 ) ) ;
#70509 = AXIS2_PLACEMENT_3D ( 'NONE', #84280, #45214, #163874 ) ;
#70510 = VECTOR ( 'NONE', #181405, 1000.000000000000000 ) ;
#70511 = DIRECTION ( 'NONE',  ( -0.000000000000000000, 0.000000000000000000, 1.000000000000000000 ) ) ;
#70512 = DIRECTION ( 'NONE',  ( 0.000000000000000000, 0.000000000000000000, 1.000000000000000000 ) ) ;
#70513 = AXIS2_PLACEMENT_3D ( 'NONE', #23088, #98707, #178314 ) ;
#70514 = VECTOR ( 'NONE', #107614, 1000.000000000000227 ) ;
#70516 = ORIENTED_EDGE ( 'NONE', *, *, #195646, .F. ) ;
#70515 = DIRECTION ( 'NONE',  ( -1.000000000000000000, 0.000000000000000000, 0.000000000000000000 ) ) ;
#70517 = ADVANCED_FACE ( 'NONE', ( #190949 ), #231351, .F. ) ;
#70518 = DIRECTION ( 'NONE',  ( 0.000000000000000000, 7.086529944415886769E-15, -1.000000000000000000 ) ) ;
#70519 = EDGE_CURVE ( 'NONE', #212171, #232077, #150521, .T. ) ;
#70521 = EDGE_CURVE ( 'NONE', #247339, #250368, #48835, .T. ) ;
#70520 = AXIS2_PLACEMENT_3D ( 'NONE', #20791, #83277, #199428 ) ;
#70523 = AXIS2_PLACEMENT_3D ( 'NONE', #163622, #4525, #162350 ) ;
#70522 = LINE ( 'NONE', #110895, #229743 ) ;
#70524 = ORIENTED_EDGE ( 'NONE', *, *, #191298, .F. ) ;
#70525 = CIRCLE ( 'NONE', #249569, 0.09999999999999939493 ) ;
#70526 = CYLINDRICAL_SURFACE ( 'NONE', #230582, 0.09999999999999939493 ) ;
#70527 = CARTESIAN_POINT ( 'NONE',  ( -18.50000000000000000, -9.400000000000005684, -40.38204184817266906 ) ) ;
#70528 = DIRECTION ( 'NONE',  ( 0.000000000000000000, -1.000000000000000000, 0.000000000000000000 ) ) ;
#70529 = VERTEX_POINT ( 'NONE', #91822 ) ;
#70530 = CARTESIAN_POINT ( 'NONE',  ( -17.04295772865462411, 65.97510057475010115, -56.87310748452439668 ) ) ;
#70532 = EDGE_LOOP ( 'NONE', ( #1906, #75531, #68111, #208930 ) ) ;
#70531 = DIRECTION ( 'NONE',  ( 1.000000000000000000, 0.000000000000000000, 0.000000000000000000 ) ) ;
#70533 = CARTESIAN_POINT ( 'NONE',  ( -23.15000000000000213, 10.74948822439028895, -222.3968794097801549 ) ) ;
#70534 = ADVANCED_FACE ( 'NONE', ( #209192 ), #211781, .F. ) ;
#70535 = DIRECTION ( 'NONE',  ( 0.000000000000000000, 0.1495327102803586661, -0.9887567792719350601 ) ) ;
#70536 = EDGE_LOOP ( 'NONE', ( #152638, #144019, #152432, #61980 ) ) ;
#70537 = CARTESIAN_POINT ( 'NONE',  ( 21.14999999999999858, 11.65000000001115943, -79.15000000000004832 ) ) ;
#70538 = APPLICATION_PROTOCOL_DEFINITION ( 'draft international standard', 'automotive_design', 1998, #205831 ) ;
#70539 = CARTESIAN_POINT ( 'NONE',  ( 21.15000000000005187, 76.00000000001119815, -36.02310748452479316 ) ) ;
#70540 = CARTESIAN_POINT ( 'NONE',  ( -21.51976009735018991, 69.08954155835347422, -203.5231074845243882 ) ) ;
#70541 = CARTESIAN_POINT ( 'NONE',  ( -18.40000000000000568, 85.50000000001192291, -96.02374538734412113 ) ) ;
#70542 = ORIENTED_EDGE ( 'NONE', *, *, #182490, .F. ) ;
#70543 = DIRECTION ( 'NONE',  ( 1.000000000000000000, -0.000000000000000000, -0.000000000000000000 ) ) ;
#70544 = CARTESIAN_POINT ( 'NONE',  ( 13.99999999999999822, 47.91805600923871822, -233.7139610577891631 ) ) ;
#70545 = CIRCLE ( 'NONE', #107911, 0.1000000000000031558 ) ;
#70546 = CARTESIAN_POINT ( 'NONE',  ( 20.95083306685154056, 8.916842641901356004, -175.9773248532583239 ) ) ;
#70547 = EDGE_CURVE ( 'NONE', #40998, #208239, #53400, .T. ) ;
#70548 = ORIENTED_EDGE ( 'NONE', *, *, #8991, .T. ) ;
#70550 = EDGE_CURVE ( 'NONE', #131243, #248676, #93892, .T. ) ;
#70549 = B_SPLINE_CURVE_WITH_KNOTS ( 'NONE', 3,
 ( #83663, #76649, #14143, #33732, #114501, #216155 ),
 .UNSPECIFIED., .F., .F.,
 ( 4, 2, 4 ),
 ( 0.000000000000000000, 0.0001895189928937408147, 0.0003790379857874816294 ),
 .UNSPECIFIED. ) ;
#70551 = AXIS2_PLACEMENT_3D ( 'NONE', #171473, #209270, #136126 ) ;
#70552 = EDGE_LOOP ( 'NONE', ( #226646, #110523, #85493, #20118 ) ) ;
#70553 = FACE_OUTER_BOUND ( 'NONE', #138825, .T. ) ;
#70554 = CARTESIAN_POINT ( 'NONE',  ( 18.41416235934318379, 85.50000000001188027, -96.42291809330222918 ) ) ;
#70555 = CARTESIAN_POINT ( 'NONE',  ( -23.15000000000000213, 87.41227409416113403, -39.02310748452423894 ) ) ;
#70556 = CARTESIAN_POINT ( 'NONE',  ( 21.04105312098506531, 8.875332623054768888, -146.3285067472120602 ) ) ;
#70557 = EDGE_CURVE ( 'NONE', #229612, #91602, #112675, .T. ) ;
#70559 = DIRECTION ( 'NONE',  ( 0.000000000000000000, 0.000000000000000000, -1.000000000000000000 ) ) ;
#70558 = DIRECTION ( 'NONE',  ( 0.000000000000000000, -0.9999631594459053030, -0.008583690987162452199 ) ) ;
#70561 = CARTESIAN_POINT ( 'NONE',  ( -21.10320863425827298, 75.97497774878530663, -176.4233848709835684 ) ) ;
#70560 = TOROIDAL_SURFACE ( 'NONE', #249599, 0.2000000000000000111, 0.1000000000000000056 ) ;
#70562 = DIRECTION ( 'NONE',  ( 0.000000000000000000, -0.8814952561688438326, 0.4721928772777334582 ) ) ;
#70563 = DIRECTION ( 'NONE',  ( 0.000000000000000000, -6.467318590049456648E-15, 1.000000000000000000 ) ) ;
#70564 = CIRCLE ( 'NONE', #174636, 0.1000000000000028644 ) ;
#70565 = ORIENTED_EDGE ( 'NONE', *, *, #239466, .F. ) ;
#70567 = ORIENTED_EDGE ( 'NONE', *, *, #153924, .T. ) ;
#70566 = CARTESIAN_POINT ( 'NONE',  ( 12.42718393586867087, 62.77476515014583924, -216.4875458411300713 ) ) ;
#70568 = LINE ( 'NONE', #127946, #143450 ) ;
#70569 = VECTOR ( 'NONE', #202671, 1000.000000000000000 ) ;
#70570 = LINE ( 'NONE', #170973, #49379 ) ;
#70572 = FACE_OUTER_BOUND ( 'NONE', #77109, .T. ) ;
#70571 = SPHERICAL_SURFACE ( 'NONE', #138466, 0.1000000000000000056 ) ;
#70573 = VERTEX_POINT ( 'NONE', #193506 ) ;
#70574 = DIRECTION ( 'NONE',  ( -2.915501640297154283E-16, -0.4088369013363279403, 0.9126074666063770380 ) ) ;
#70575 = CARTESIAN_POINT ( 'NONE',  ( 23.14999999999999503, 35.97645343225767789, -235.9694016464868298 ) ) ;
#70576 = FACE_OUTER_BOUND ( 'NONE', #126309, .T. ) ;
#70577 = DIRECTION ( 'NONE',  ( 1.000000000000000000, 0.000000000000000000, 0.000000000000000000 ) ) ;
#70578 = ORIENTED_EDGE ( 'NONE', *, *, #94539, .F. ) ;
#70579 = TOROIDAL_SURFACE ( 'NONE', #224648, 0.2000000000000000111, 0.1000000000000000056 ) ;
#70580 = ORIENTED_EDGE ( 'NONE', *, *, #70333, .T. ) ;
#70581 = EDGE_CURVE ( 'NONE', #89267, #7014, #123132, .T. ) ;
#70582 = LINE ( 'NONE', #11886, #26157 ) ;
#70583 = EDGE_LOOP ( 'NONE', ( #256837, #22973, #144649, #219792, #84746 ) ) ;
#70584 = CARTESIAN_POINT ( 'NONE',  ( -20.94999999999999929, 12.80863705670245700, -205.3010250813005655 ) ) ;
#70585 = AXIS2_PLACEMENT_3D ( 'NONE', #164106, #87110, #226621 ) ;
#70586 = DIRECTION ( 'NONE',  ( 0.000000000000000000, 0.000000000000000000, -1.000000000000000000 ) ) ;
#70587 = AXIS2_PLACEMENT_3D ( 'NONE', #134031, #97450, #17936 ) ;
#70588 = CIRCLE ( 'NONE', #78892, 0.1000000000000000749 ) ;
#70589 = AXIS2_PLACEMENT_3D ( 'NONE', #59798, #115961, #58520 ) ;
#70590 = ADVANCED_FACE ( 'NONE', ( #50115 ), #85656, .F. ) ;
#70591 = CYLINDRICAL_SURFACE ( 'NONE', #63946, 0.5000000000000004441 ) ;
#70592 = ORIENTED_EDGE ( 'NONE', *, *, #65047, .F. ) ;
#70593 = CARTESIAN_POINT ( 'NONE',  ( 21.05000000000000071, 8.776282895292474961, 0.000000000000000000 ) ) ;
#70594 = EDGE_CURVE ( 'NONE', #149638, #28763, #202238, .T. ) ;
#70596 = EDGE_CURVE ( 'NONE', #245608, #145681, #73269, .T. ) ;
#70595 = DIRECTION ( 'NONE',  ( 0.000000000000000000, 0.9126074666064841745, 0.4088369013360889648 ) ) ;
#70597 = CARTESIAN_POINT ( 'NONE',  ( -23.15000000000000213, 76.00000000001172396, -71.52310748452431710 ) ) ;
#70598 = CARTESIAN_POINT ( 'NONE',  ( 18.49999999999998934, 69.45000000001222418, -148.7731074845244166 ) ) ;
#70599 = CARTESIAN_POINT ( 'NONE',  ( 18.59999999999999787, -1.736705739456431807, -112.0174225876237699 ) ) ;
#70600 = DIRECTION ( 'NONE',  ( 1.000000000000000000, 0.000000000000000000, 0.000000000000000000 ) ) ;
#70601 = DIRECTION ( 'NONE',  ( -0.000000000000000000, -0.000000000000000000, 1.000000000000000000 ) ) ;
#70602 = VERTEX_POINT ( 'NONE', #134773 ) ;
#70604 = SPHERICAL_SURFACE ( 'NONE', #10146, 0.1000000000000000056 ) ;
#70603 = CARTESIAN_POINT ( 'NONE',  ( -18.59999999999999787, 78.48087866980282001, -232.8271061603568910 ) ) ;
#70605 = AXIS2_PLACEMENT_3D ( 'NONE', #9168, #84812, #169572 ) ;
#70606 = ORIENTED_EDGE ( 'NONE', *, *, #190639, .F. ) ;
#70608 = ORIENTED_EDGE ( 'NONE', *, *, #219147, .T. ) ;
#70607 = CARTESIAN_POINT ( 'NONE',  ( 20.94999999999999929, 64.75617845954087670, -200.4736850529726269 ) ) ;
#70609 = EDGE_CURVE ( 'NONE', #99805, #135741, #10697, .T. ) ;
#70610 = EDGE_LOOP ( 'NONE', ( #96326, #181103, #164513, #106128 ) ) ;
#70611 = CARTESIAN_POINT ( 'NONE',  ( -18.40000000000000213, 11.48667500176882861, -91.25000000000005684 ) ) ;
#70612 = ADVANCED_FACE ( 'NONE', ( #95660 ), #19056, .T. ) ;
#70613 = CARTESIAN_POINT ( 'NONE',  ( -18.39999999999999858, 11.47316190337362762, -176.8259460668079441 ) ) ;
#70614 = FACE_OUTER_BOUND ( 'NONE', #191922, .T. ) ;
#70615 = CARTESIAN_POINT ( 'NONE',  ( -21.78635804494510708, 60.41499726328847686, -234.1090742605158539 ) ) ;
#70616 = ORIENTED_EDGE ( 'NONE', *, *, #233721, .T. ) ;
#70617 = CYLINDRICAL_SURFACE ( 'NONE', #205487, 0.09999999999999543976 ) ;
#70619 = EDGE_CURVE ( 'NONE', #74897, #139488, #206513, .T. ) ;
#70618 = CARTESIAN_POINT ( 'NONE',  ( -23.25000000000000000, 76.00000000001197975, -107.0731074845243143 ) ) ;
#70620 = VERTEX_POINT ( 'NONE', #175255 ) ;
#70621 = AXIS2_PLACEMENT_3D ( 'NONE', #130256, #113273, #230664 ) ;
#70622 = CARTESIAN_POINT ( 'NONE',  ( -16.94052228080551359, 9.986279733109993728, -154.8903755026694569 ) ) ;
#70623 = EDGE_CURVE ( 'NONE', #28041, #146870, #23381, .T. ) ;
#70624 = CARTESIAN_POINT ( 'NONE',  ( -16.87036670365548474, 30.35820049718185487, -234.7353065400981507 ) ) ;
#70625 = ORIENTED_EDGE ( 'NONE', *, *, #6367, .T. ) ;
#70626 = CARTESIAN_POINT ( 'NONE',  ( 20.85000000000000142, 76.00000000001213607, -136.5231074845243313 ) ) ;
#70627 = ADVANCED_FACE ( 'NONE', ( #117800 ), #14985, .F. ) ;
#70628 = EDGE_CURVE ( 'NONE', #120433, #129506, #23185, .T. ) ;
#70629 = CIRCLE ( 'NONE', #187137, 0.09999999999999939493 ) ;
#70630 = EDGE_LOOP ( 'NONE', ( #98173, #168089, #16462 ) ) ;
#70631 = CARTESIAN_POINT ( 'NONE',  ( -23.25000000000000355, 5.650000000011139001, -121.3500000000000369 ) ) ;
#70632 = VERTEX_POINT ( 'NONE', #216890 ) ;
#70633 = CARTESIAN_POINT ( 'NONE',  ( 21.05000000000000071, 76.08561306081638520, -176.4368672183346405 ) ) ;
#70634 = ADVANCED_FACE ( 'NONE', ( #78661 ), #77375, .T. ) ;
#70635 = DIRECTION ( 'NONE',  ( 1.000000000000000000, -0.000000000000000000, -0.000000000000000000 ) ) ;
#70636 = DIRECTION ( 'NONE',  ( -3.265361837132813093E-16, 1.000000000000000000, -0.000000000000000000 ) ) ;
#70637 = DIRECTION ( 'NONE',  ( -1.000000000000000000, 0.000000000000000000, -0.000000000000000000 ) ) ;
#70638 = ADVANCED_FACE ( 'NONE', ( #198616 ), #158256, .T. ) ;
#70639 = CIRCLE ( 'NONE', #53864, 0.6000000000000033085 ) ;
#70640 = ADVANCED_FACE ( 'NONE', ( #55227 ), #237749, .T. ) ;
#70641 = AXIS2_PLACEMENT_3D ( 'NONE', #1388, #217861, #118803 ) ;
#70642 = ADVANCED_FACE ( 'NONE', ( #219452 ), #74862, .F. ) ;
#70643 = CARTESIAN_POINT ( 'NONE',  ( -21.05000000000000071, 67.63082410804655353, -211.8415745842588649 ) ) ;
#70644 = DIRECTION ( 'NONE',  ( 0.000000000000000000, 0.000000000000000000, -1.000000000000000000 ) ) ;
#70645 = VERTEX_POINT ( 'NONE', #138613 ) ;
#70647 = CARTESIAN_POINT ( 'NONE',  ( -18.59999999999999787, 65.50527602196416410, -248.6645148362614748 ) ) ;
#70646 = AXIS2_PLACEMENT_3D ( 'NONE', #198698, #154475, #59148 ) ;
#70648 = ORIENTED_EDGE ( 'NONE', *, *, #41232, .F. ) ;
#70650 = CARTESIAN_POINT ( 'NONE',  ( -22.59999999999999787, 11.64957080755595520, -33.40000000000000568 ) ) ;
#70649 = CARTESIAN_POINT ( 'NONE',  ( 20.94999999999999929, 71.14953271029224879, -90.98884007552265984 ) ) ;
#70651 = ORIENTED_EDGE ( 'NONE', *, *, #122964, .F. ) ;
#70652 = LINE ( 'NONE', #51016, #80853 ) ;
#70653 = DIRECTION ( 'NONE',  ( -1.000000000000000000, -0.000000000000000000, -0.000000000000000000 ) ) ;
#70654 = CARTESIAN_POINT ( 'NONE',  ( -21.05000000000000071, 36.02367271998545561, -235.8812521208699309 ) ) ;
#70655 = CARTESIAN_POINT ( 'NONE',  ( 20.95325940946048249, 59.05480421347601805, -225.7998712302227773 ) ) ;
#70656 = ORIENTED_EDGE ( 'NONE', *, *, #93223, .T. ) ;
#70658 = ORIENTED_EDGE ( 'NONE', *, *, #82777, .T. ) ;
#70657 = DIRECTION ( 'NONE',  ( 1.000000000000000000, 0.000000000000000000, -0.000000000000000000 ) ) ;
#70659 = ADVANCED_FACE ( 'NONE', ( #40870 ), #120413, .F. ) ;
#70661 = CARTESIAN_POINT ( 'NONE',  ( 21.05000000000000071, 69.16514130714681130, -247.7543978865853660 ) ) ;
#70660 = DIRECTION ( 'NONE',  ( -0.000000000000000000, 6.982962677686266711E-15, -1.000000000000000000 ) ) ;
#70663 = EDGE_LOOP ( 'NONE', ( #218608, #247151, #251992, #4193, #99139, #120905, #107335, #164417, #151501, #217158, #81588, #36603, #194518, #221195, #248378, #59505 ) ) ;
#70662 = CYLINDRICAL_SURFACE ( 'NONE', #36447, 0.09999999999999781286 ) ;
#70664 = AXIS2_PLACEMENT_3D ( 'NONE', #242158, #24431, #162641 ) ;
#70665 = VERTEX_POINT ( 'NONE', #197324 ) ;
#70666 = DIRECTION ( 'NONE',  ( 1.000000000000000000, 0.000000000000000000, 0.000000000000000000 ) ) ;
#70667 = DIRECTION ( 'NONE',  ( 0.000000000000000000, 0.000000000000000000, 1.000000000000000000 ) ) ;
#70668 = ORIENTED_EDGE ( 'NONE', *, *, #50873, .F. ) ;
#70669 = ORIENTED_EDGE ( 'NONE', *, *, #147323, .F. ) ;
#70670 = CARTESIAN_POINT ( 'NONE',  ( 23.24999999999999289, 21.13195309841794867, -243.6318585593223816 ) ) ;
#70671 = CARTESIAN_POINT ( 'NONE',  ( 20.95512820512820440, 18.90192396791320562, -227.9871466877642661 ) ) ;
#70672 = ORIENTED_EDGE ( 'NONE', *, *, #156874, .F. ) ;
#70673 = CARTESIAN_POINT ( 'NONE',  ( 21.05000000000000071, -11.48912529306490349, -69.90000000000004832 ) ) ;
#70674 = CIRCLE ( 'NONE', #28995, 0.09999999999999986677 ) ;
#70675 = EDGE_CURVE ( 'NONE', #129332, #68660, #185669, .T. ) ;
#70676 = VECTOR ( 'NONE', #237206, 1000.000000000000000 ) ;
#70677 = ORIENTED_EDGE ( 'NONE', *, *, #130194, .T. ) ;
#70678 = AXIS2_PLACEMENT_3D ( 'NONE', #86549, #166159, #245658 ) ;
#70679 = AXIS2_PLACEMENT_3D ( 'NONE', #177278, #16902, #199400 ) ;
#70681 = EDGE_CURVE ( 'NONE', #129072, #246378, #139855, .T. ) ;
#70680 = CARTESIAN_POINT ( 'NONE',  ( 18.59999999999999076, 10.24999999999999822, -24.75000000000000000 ) ) ;
#70682 = ORIENTED_EDGE ( 'NONE', *, *, #170043, .F. ) ;
#70683 = CIRCLE ( 'NONE', #153923, 6.329289321881367059 ) ;
#70684 = VERTEX_POINT ( 'NONE', #99496 ) ;
#70685 = CARTESIAN_POINT ( 'NONE',  ( 20.11144452914042091, 18.77466987908303508, -228.7020108391373014 ) ) ;
#70686 = ORIENTED_EDGE ( 'NONE', *, *, #7748, .F. ) ;
#70687 = DIRECTION ( 'NONE',  ( 1.000000000000000000, -0.000000000000000000, -0.000000000000000000 ) ) ;
#70688 = ORIENTED_EDGE ( 'NONE', *, *, #105881, .F. ) ;
#70690 = VERTEX_POINT ( 'NONE', #179098 ) ;
#70689 = DIRECTION ( 'NONE',  ( -0.7071067811865474617, 0.7071067811865474617, 5.142139384388980375E-15 ) ) ;
#70691 = APPLICATION_CONTEXT ( 'automotive_design' ) ;
#70692 = ORIENTED_EDGE ( 'NONE', *, *, #254286, .T. ) ;
#70693 = CARTESIAN_POINT ( 'NONE',  ( -18.59999999999999787, -1.835859311432481045, -145.5044391687985694 ) ) ;
#70694 = AXIS2_PLACEMENT_3D ( 'NONE', #242372, #105403, #183703 ) ;
#70695 = VERTEX_POINT ( 'NONE', #21303 ) ;
#70698 = ORIENTED_EDGE ( 'NONE', *, *, #171325, .F. ) ;
#70697 = ORIENTED_EDGE ( 'NONE', *, *, #25762, .F. ) ;
#70696 = DIRECTION ( 'NONE',  ( -0.000000000000000000, -0.4088369013363281623, 0.9126074666063771490 ) ) ;
#70700 = DIRECTION ( 'NONE',  ( 0.000000000000000000, -0.2128009952263485993, 0.9770955615653341697 ) ) ;
#70699 = AXIS2_PLACEMENT_3D ( 'NONE', #17077, #168805, #114871 ) ;
#70701 = EDGE_CURVE ( 'NONE', #96084, #200838, #218250, .T. ) ;
#70702 = CARTESIAN_POINT ( 'NONE',  ( 21.05000000000000071, 0.6736784609442970639, -212.7825231506076875 ) ) ;
#70703 = VERTEX_POINT ( 'NONE', #65521 ) ;
#70704 = AXIS2_PLACEMENT_3D ( 'NONE', #7269, #86796, #63388 ) ;
#70705 = CARTESIAN_POINT ( 'NONE',  ( 21.05995757104869526, 8.775389244732430427, -45.69490512299120866 ) ) ;
#70706 = VERTEX_POINT ( 'NONE', #62964 ) ;
#70707 = CARTESIAN_POINT ( 'NONE',  ( -21.04999999999960281, 69.65527659592207499, -203.5378253410476077 ) ) ;
#70708 =( BOUNDED_SURFACE ( )  B_SPLINE_SURFACE ( 3, 2, ( 
 ( #18948, #137599, #239299 ),
 ( #180609, #179342, #61947 ),
 ( #60634, #98449, #123202 ),
 ( #202730, #159766, #59331 ) ),
 .UNSPECIFIED., .F., .F., .F. ) 
 B_SPLINE_SURFACE_WITH_KNOTS ( ( 4, 4 ),
 ( 3, 3 ),
 ( 0.0008258556059633768206, 0.0009616864997632988948 ),
 ( 0.000000000000000000, 1.000000000000000000 ),
 .UNSPECIFIED. ) 
 GEOMETRIC_REPRESENTATION_ITEM ( )  RATIONAL_B_SPLINE_SURFACE ( (
 ( 1.000000000000000000, 0.9152888060719411856, 1.000000000000000000),
 ( 1.000000000000000000, 0.9327727094137941988, 1.000000000000000000),
 ( 1.000000000000000000, 0.9369023509258418425, 1.000000000000000000),
 ( 1.000000000000000000, 0.9246339933864583527, 1.000000000000000000) ) ) 
 REPRESENTATION_ITEM ( '' )  SURFACE ( )  );
#70710 = ORIENTED_EDGE ( 'NONE', *, *, #125621, .T. ) ;
#70709 = FACE_BOUND ( 'NONE', #212064, .T. ) ;
#70711 = FACE_OUTER_BOUND ( 'NONE', #112878, .T. ) ;
#70712 = EDGE_LOOP ( 'NONE', ( #5845, #199412, #123317, #185358 ) ) ;
#70713 = CARTESIAN_POINT ( 'NONE',  ( -23.25000000000000000, 6.933893972137497030, -104.2856458343736250 ) ) ;
#70714 = CARTESIAN_POINT ( 'NONE',  ( -21.65000000000000213, 7.708578643773852157, -54.65000000000000568 ) ) ;
#70715 = ORIENTED_EDGE ( 'NONE', *, *, #125252, .T. ) ;
#70716 = CARTESIAN_POINT ( 'NONE',  ( 18.47654891039379166, 85.46527494839392602, -62.39713157932961707 ) ) ;
#70717 = DIRECTION ( 'NONE',  ( -1.000000000000000000, 0.000000000000000000, -0.000000000000000000 ) ) ;
#70718 = ORIENTED_EDGE ( 'NONE', *, *, #174064, .T. ) ;
#70720 = ORIENTED_EDGE ( 'NONE', *, *, #207778, .T. ) ;
#70719 = DIRECTION ( 'NONE',  ( -2.561896900575096011E-15, -0.5907332058517279494, 0.8068669527897025517 ) ) ;
#70721 = CIRCLE ( 'NONE', #166403, 0.09999999999999939493 ) ;
#70722 = CARTESIAN_POINT ( 'NONE',  ( -23.25000000000000000, 1.115651490242849210E-11, -96.35000000000003695 ) ) ;
#70724 = ORIENTED_EDGE ( 'NONE', *, *, #71165, .T. ) ;
#70723 = EDGE_LOOP ( 'NONE', ( #212757, #6979, #190958, #185886, #146566, #205523, #209305, #232031, #10107, #6005, #190937, #33792, #9834, #208219, #134644, #71602, #115926, #114970 ) ) ;
#70725 = ORIENTED_EDGE ( 'NONE', *, *, #153100, .T. ) ;
#70726 = FACE_OUTER_BOUND ( 'NONE', #197287, .T. ) ;
#70727 = ORIENTED_EDGE ( 'NONE', *, *, #171023, .F. ) ;
#70728 = VERTEX_POINT ( 'NONE', #25146 ) ;
#70729 = DIRECTION ( 'NONE',  ( 0.000000000000000000, 0.000000000000000000, -1.000000000000000000 ) ) ;
#70730 = VECTOR ( 'NONE', #89013, 1000.000000000000000 ) ;
#70731 = ORIENTED_EDGE ( 'NONE', *, *, #217665, .T. ) ;
#70732 = FACE_OUTER_BOUND ( 'NONE', #201248, .T. ) ;
#70733 = CARTESIAN_POINT ( 'NONE',  ( -21.05000000000000071, 14.05000000001115623, -139.5136950707610026 ) ) ;
#70734 = EDGE_CURVE ( 'NONE', #111271, #88487, #222010, .T. ) ;
#70735 = ORIENTED_EDGE ( 'NONE', *, *, #13130, .F. ) ;
#70736 = ADVANCED_FACE ( 'NONE', ( #185486 ), #106519, .F. ) ;
#70737 = VERTEX_POINT ( 'NONE', #225854 ) ;
#70738 = CYLINDRICAL_SURFACE ( 'NONE', #121379, 0.09999999999998898659 ) ;
#70740 = VERTEX_POINT ( 'NONE', #142488 ) ;
#70739 = VECTOR ( 'NONE', #6712, 1000.000000000000000 ) ;
#70741 = CIRCLE ( 'NONE', #208104, 0.09999999999999939493 ) ;
#70742 = EDGE_CURVE ( 'NONE', #47961, #199368, #248214, .T. ) ;
#70743 = DIRECTION ( 'NONE',  ( 0.000000000000000000, -0.8814952561688476074, 0.4721928772777262417 ) ) ;
#70744 = ORIENTED_EDGE ( 'NONE', *, *, #29106, .T. ) ;
#70745 = AXIS2_PLACEMENT_3D ( 'NONE', #8580, #50247, #151963 ) ;
#70746 = SPHERICAL_SURFACE ( 'NONE', #25386, 0.1000000000000000056 ) ;
#70749 = EDGE_CURVE ( 'NONE', #60391, #117855, #94066, .T. ) ;
#70748 = ORIENTED_EDGE ( 'NONE', *, *, #25557, .F. ) ;
#70747 = FACE_OUTER_BOUND ( 'NONE', #39926, .T. ) ;
#70750 = DIRECTION ( 'NONE',  ( -0.7071067811865474617, -0.7071067811865474617, -0.000000000000000000 ) ) ;
#70751 = CARTESIAN_POINT ( 'NONE',  ( 20.99142135623731065, 64.40000000001218439, -143.4513107147999165 ) ) ;
#70752 = EDGE_CURVE ( 'NONE', #168869, #72318, #105915, .T. ) ;
#70754 = CIRCLE ( 'NONE', #237329, 0.09999999999999939493 ) ;
#70753 = DIRECTION ( 'NONE',  ( 0.000000000000000000, 1.000000000000000000, 6.982962677686266711E-15 ) ) ;
#70755 = CARTESIAN_POINT ( 'NONE',  ( 18.49999999999999645, -2.275048162540885155, -230.1697641654749305 ) ) ;
#70756 = CARTESIAN_POINT ( 'NONE',  ( -16.89268316805466341, 66.04827818677011919, -157.3788599630699707 ) ) ;
#70757 = DIRECTION ( 'NONE',  ( 1.000000000000000000, -0.000000000000000000, -0.000000000000000000 ) ) ;
#70758 = CARTESIAN_POINT ( 'NONE',  ( -21.05000000000000426, 6.477046381801002894, -33.60000000000000853 ) ) ;
#70759 = CARTESIAN_POINT ( 'NONE',  ( 18.33683296300444709, 38.25517547545369723, -261.1960221343530293 ) ) ;
#70760 = ADVANCED_FACE ( 'NONE', ( #224598 ), #244389, .T. ) ;
#70761 = DIRECTION ( 'NONE',  ( 1.000000000000000000, 0.000000000000000000, 0.000000000000000000 ) ) ;
#70762 = ORIENTED_EDGE ( 'NONE', *, *, #93294, .F. ) ;
#70763 = AXIS2_PLACEMENT_3D ( 'NONE', #20446, #99931, #94820 ) ;
#70764 = AXIS2_PLACEMENT_3D ( 'NONE', #137563, #38491, #15079 ) ;
#70765 = AXIS2_PLACEMENT_3D ( 'NONE', #212863, #158065, #34250 ) ;
#70766 = AXIS2_PLACEMENT_3D ( 'NONE', #76184, #93188, #252255 ) ;
#70767 = CIRCLE ( 'NONE', #224843, 3.999999999999999112 ) ;
#70768 = EDGE_LOOP ( 'NONE', ( #150298, #82783, #204071, #138539 ) ) ;
#70769 = ORIENTED_EDGE ( 'NONE', *, *, #20263, .T. ) ;
#70770 = EDGE_LOOP ( 'NONE', ( #165642, #239667, #114976, #203945 ) ) ;
#70771 = AXIS2_PLACEMENT_3D ( 'NONE', #135188, #234295, #236865 ) ;
#70773 = EDGE_CURVE ( 'NONE', #118880, #194069, #245473, .T. ) ;
#70772 = CARTESIAN_POINT ( 'NONE',  ( -17.73285935861198581, 65.14201819622113021, -92.78166929430516063 ) ) ;
#70774 = DIRECTION ( 'NONE',  ( 0.2834754621636439431, -0.2834754621636535465, -0.9161240771326838450 ) ) ;
#70776 = DIRECTION ( 'NONE',  ( 0.000000000000000000, 0.000000000000000000, -1.000000000000000000 ) ) ;
#70775 = CARTESIAN_POINT ( 'NONE',  ( -21.04999999999994387, 76.00000000001119815, -31.87310748452479459 ) ) ;
#70777 = ORIENTED_EDGE ( 'NONE', *, *, #33221, .F. ) ;
#70778 = EDGE_LOOP ( 'NONE', ( #122034, #38973, #207224, #24172 ) ) ;
#70779 = SURFACE_STYLE_FILL_AREA ( #231130 ) ;
#70780 = FACE_OUTER_BOUND ( 'NONE', #200322, .T. ) ;
#70781 = CARTESIAN_POINT ( 'NONE',  ( 23.14999999999999503, 11.65000000001116298, -121.8500000000000369 ) ) ;
#70782 = ORIENTED_EDGE ( 'NONE', *, *, #53689, .F. ) ;
#70783 = VERTEX_POINT ( 'NONE', #203763 ) ;
#70784 = DIRECTION ( 'NONE',  ( 0.000000000000000000, 0.9875055080513743810, -0.1575844902526802316 ) ) ;
#70785 = DIRECTION ( 'NONE',  ( 0.000000000000000000, -0.9126074666063771490, -0.4088369013363278293 ) ) ;
#70786 = DIRECTION ( 'NONE',  ( -1.000000000000000000, -0.000000000000000000, -0.000000000000000000 ) ) ;
#70787 = DIRECTION ( 'NONE',  ( -0.000000000000000000, -2.891205793294679805E-16, 1.000000000000000000 ) ) ;
#70789 = ORIENTED_EDGE ( 'NONE', *, *, #206023, .F. ) ;
#70788 = CARTESIAN_POINT ( 'NONE',  ( -20.54999999999999716, 68.75000000001205080, -124.2731074845243455 ) ) ;
#70790 = DIRECTION ( 'NONE',  ( 0.000000000000000000, -1.000000000000000000, -6.837150591533219968E-15 ) ) ;
#70791 = LINE ( 'NONE', #128172, #52434 ) ;
#70792 = CARTESIAN_POINT ( 'NONE',  ( 20.85000000000000142, 0.000000000000000000, -33.50000000000000000 ) ) ;
#70793 = CARTESIAN_POINT ( 'NONE',  ( 20.73486653747088582, 52.72272256579930172, -234.4105091754867658 ) ) ;
#70794 = EDGE_LOOP ( 'NONE', ( #2386, #168270, #158662, #211959 ) ) ;
#70795 = CARTESIAN_POINT ( 'NONE',  ( 13.88638282980484284, 66.54257354752293452, -84.52306561612435587 ) ) ;
#70796 = CIRCLE ( 'NONE', #216511, 0.09999999999999820144 ) ;
#70797 = CARTESIAN_POINT ( 'NONE',  ( 23.25000000000000000, 87.75000000001246292, -181.7731074845242745 ) ) ;
#70799 = CARTESIAN_POINT ( 'NONE',  ( -17.22361732159831504, 65.65484434140957148, -114.3938920103915109 ) ) ;
#70798 = LINE ( 'NONE', #231154, #7631 ) ;
#70800 = DIRECTION ( 'NONE',  ( 1.000000000000000000, 7.304098846218133681E-16, -4.607487905232622991E-31 ) ) ;
#70801 = CIRCLE ( 'NONE', #179133, 0.1000000000000072220 ) ;
#70802 = CARTESIAN_POINT ( 'NONE',  ( 18.79999999999999005, 8.000000000000000000, 1.212568896937007867 ) ) ;
#70803 = CARTESIAN_POINT ( 'NONE',  ( -21.37071067811865532, 67.92928932189292368, -57.27310748452438105 ) ) ;
#70804 = DIRECTION ( 'NONE',  ( 0.000000000000000000, -7.304098846218112382E-15, 1.000000000000000000 ) ) ;
#70805 = FACE_OUTER_BOUND ( 'NONE', #175668, .T. ) ;
#70806 = DIRECTION ( 'NONE',  ( 1.186688945009010077E-16, 1.000000000000000000, 6.982962677686266711E-15 ) ) ;
#70808 = VERTEX_POINT ( 'NONE', #104621 ) ;
#70807 = AXIS2_PLACEMENT_3D ( 'NONE', #36507, #174753, #56008 ) ;
#70809 = EDGE_CURVE ( 'NONE', #170116, #242049, #85059, .T. ) ;
#70810 = VERTEX_POINT ( 'NONE', #146338 ) ;
#70811 =( BOUNDED_SURFACE ( )  B_SPLINE_SURFACE ( 3, 2, ( 
 ( #165715, #146122, #41920 ),
 ( #65303, #125287, #221780 ),
 ( #202254, #143553, #164416 ),
 ( #6610, #83554, #121463 ) ),
 .UNSPECIFIED., .F., .F., .F. ) 
 B_SPLINE_SURFACE_WITH_KNOTS ( ( 4, 4 ),
 ( 3, 3 ),
 ( 0.0002700421466196637442, 0.0004789321604330607179 ),
 ( 0.000000000000000000, 1.000000000000000000 ),
 .UNSPECIFIED. ) 
 GEOMETRIC_REPRESENTATION_ITEM ( )  RATIONAL_B_SPLINE_SURFACE ( (
 ( 1.000000000000000000, 0.7071067811865475727, 1.000000000000000000),
 ( 1.000000000000000000, 0.7163411249511738577, 1.000000000000000000),
 ( 1.000000000000000000, 0.7221957104842052777, 1.000000000000000000),
 ( 1.000000000000000000, 0.7250110520819876836, 1.000000000000000000) ) ) 
 REPRESENTATION_ITEM ( '' )  SURFACE ( )  );
#70812 = ORIENTED_EDGE ( 'NONE', *, *, #201933, .T. ) ;
#70813 = DIRECTION ( 'NONE',  ( 1.000000000000000000, 0.000000000000000000, 0.000000000000000000 ) ) ;
#70814 = DIRECTION ( 'NONE',  ( -1.000000000000000000, -1.794895427898102820E-16, -3.909090864890033875E-17 ) ) ;
#70815 = VERTEX_POINT ( 'NONE', #27733 ) ;
#70816 = ADVANCED_FACE ( 'NONE', ( #180350 ), #81219, .T. ) ;
#70817 = CIRCLE ( 'NONE', #129051, 0.09999999999999742428 ) ;
#70818 = ORIENTED_EDGE ( 'NONE', *, *, #255539, .F. ) ;
#70819 = VECTOR ( 'NONE', #113351, 1000.000000000000114 ) ;
#70820 = EDGE_CURVE ( 'NONE', #208002, #224260, #127399, .T. ) ;
#70821 = EDGE_CURVE ( 'NONE', #239499, #15247, #88930, .T. ) ;
#70822 = ORIENTED_EDGE ( 'NONE', *, *, #4982, .F. ) ;
#70823 = CARTESIAN_POINT ( 'NONE',  ( -21.65000000000000213, 68.29142135624915966, -90.67310748452436542 ) ) ;
#70824 = CONICAL_SURFACE ( 'NONE', #212457, 7.750000000000026645, 0.7853981633974531640 ) ;
#70825 = EDGE_LOOP ( 'NONE', ( #55930, #100609, #110248, #56515 ) ) ;
#70826 = CYLINDRICAL_SURFACE ( 'NONE', #242853, 0.8750000000000007772 ) ;
#70827 = DIRECTION ( 'NONE',  ( 0.000000000000000000, 0.2128009952263485993, -0.9770955615653341697 ) ) ;
#70828 = DIRECTION ( 'NONE',  ( 0.000000000000000000, 0.000000000000000000, -1.000000000000000000 ) ) ;
#70829 = DIRECTION ( 'NONE',  ( 0.000000000000000000, 0.000000000000000000, -1.000000000000000000 ) ) ;
#70830 = FACE_OUTER_BOUND ( 'NONE', #123890, .T. ) ;
#70832 = ORIENTED_EDGE ( 'NONE', *, *, #82070, .T. ) ;
#70831 = DIRECTION ( 'NONE',  ( 0.000000000000000000, -0.000000000000000000, 1.000000000000000000 ) ) ;
#70834 = CARTESIAN_POINT ( 'NONE',  ( 20.97462148592268250, 8.874737576461731337, -79.25464433173107182 ) ) ;
#70833 = CARTESIAN_POINT ( 'NONE',  ( 20.95576188350343116, 65.39101945504820890, -61.91187376177009583 ) ) ;
#70835 = ADVANCED_FACE ( 'NONE', ( #207635 ), #148940, .T. ) ;
#70836 = DIRECTION ( 'NONE',  ( 0.000000000000000000, 0.000000000000000000, -1.000000000000000000 ) ) ;
#70837 = ORIENTED_EDGE ( 'NONE', *, *, #19434, .F. ) ;
#70838 = DIRECTION ( 'NONE',  ( 0.000000000000000000, -1.000000000000000000, -6.352154140967427193E-15 ) ) ;
#70839 = CARTESIAN_POINT ( 'NONE',  ( -16.97048361161167307, 66.05000000001180638, -82.66422314009398065 ) ) ;
#70841 = EDGE_CURVE ( 'NONE', #133882, #13363, #223073, .T. ) ;
#70840 = CARTESIAN_POINT ( 'NONE',  ( 21.05000000000000426, -0.08561306079281312542, -60.58624026618976188 ) ) ;
#70842 = ORIENTED_EDGE ( 'NONE', *, *, #211172, .T. ) ;
#70843 = LINE ( 'NONE', #90366, #200090 ) ;
#70844 = PRODUCT_DEFINITION ( 'UNKNOWN', '', #28130, #154952 ) ;
#70845 = AXIS2_PLACEMENT_3D ( 'NONE', #95911, #223248, #240274 ) ;
#70846 = AXIS2_PLACEMENT_3D ( 'NONE', #86299, #87592, #6791 ) ;
#70847 = CARTESIAN_POINT ( 'NONE',  ( -18.40000000000000213, 70.35000000001224407, -149.1731074845243938 ) ) ;
#70848 = ORIENTED_EDGE ( 'NONE', *, *, #186406, .T. ) ;
#70849 = DIRECTION ( 'NONE',  ( 1.000000000000000000, 0.000000000000000000, 0.000000000000000000 ) ) ;
#70850 = EDGE_CURVE ( 'NONE', #201537, #119534, #29023, .T. ) ;
#70851 = CARTESIAN_POINT ( 'NONE',  ( 18.49999999999999645, 77.16270174994961906, -61.42310748452431568 ) ) ;
#70852 = DIRECTION ( 'NONE',  ( 7.304098846218134667E-16, 1.000000000000000000, 6.982962677686266711E-15 ) ) ;
#70853 = EDGE_CURVE ( 'NONE', #201727, #123059, #9402, .T. ) ;
#70854 = ORIENTED_EDGE ( 'NONE', *, *, #198946, .T. ) ;
#70855 = ADVANCED_FACE ( 'NONE', ( #190640 ), #181587, .F. ) ;
#70856 = ORIENTED_EDGE ( 'NONE', *, *, #108037, .T. ) ;
#70857 = FACE_OUTER_BOUND ( 'NONE', #201891, .T. ) ;
#70858 = DIRECTION ( 'NONE',  ( 0.000000000000000000, -0.2617529984165031243, -0.9651348961777157509 ) ) ;
#70859 = DIRECTION ( 'NONE',  ( 0.000000000000000000, -1.000000000000000000, 0.000000000000000000 ) ) ;
#70861 = DIRECTION ( 'NONE',  ( 0.000000000000000000, -1.000000000000000000, 0.000000000000000000 ) ) ;
#70860 = CIRCLE ( 'NONE', #220684, 0.1000000000000013933 ) ;
#70862 = AXIS2_PLACEMENT_3D ( 'NONE', #185868, #144158, #202861 ) ;
#70865 = CARTESIAN_POINT ( 'NONE',  ( 23.24999999999999289, 69.35000000001151932, -48.37310748452436826 ) ) ;
#70864 = AXIS2_PLACEMENT_3D ( 'NONE', #7593, #89679, #88387 ) ;
#70863 = CARTESIAN_POINT ( 'NONE',  ( -21.14999999999999858, 1.115600667400684642E-11, -94.24142135623733907 ) ) ;
#70866 = CARTESIAN_POINT ( 'NONE',  ( 21.07933241753356768, 6.328645948390904330, -167.4066204095806540 ) ) ;
#70867 = CARTESIAN_POINT ( 'NONE',  ( -23.15000000000000213, -8.999999999988846255, -43.39396912265245021 ) ) ;
#70868 = CARTESIAN_POINT ( 'NONE',  ( 20.85000000000000142, 68.92903212821255465, -32.27654326265606954 ) ) ;
#70869 = ORIENTED_EDGE ( 'NONE', *, *, #35503, .F. ) ;
#70870 = CARTESIAN_POINT ( 'NONE',  ( 23.24999999999999645, 64.25000000001224976, -149.1731074845244507 ) ) ;
#70872 = VERTEX_POINT ( 'NONE', #12005 ) ;
#70871 = DIRECTION ( 'NONE',  ( 0.000000000000000000, -0.1568667991644863147, -0.9876197685951252359 ) ) ;
#70873 = AXIS2_PLACEMENT_3D ( 'NONE', #27251, #247546, #188851 ) ;
#70874 = DIRECTION ( 'NONE',  ( 2.952720810173290098E-16, 0.9651348961777149738, -0.2617529984165062884 ) ) ;
#70875 = DIRECTION ( 'NONE',  ( 1.000000000000000000, 0.000000000000000000, 0.000000000000000000 ) ) ;
#70876 = DIRECTION ( 'NONE',  ( -1.000000000000000000, 2.952720810173289112E-16, 2.061873921506763405E-30 ) ) ;
#70877 = DIRECTION ( 'NONE',  ( -1.000000000000000000, -0.000000000000000000, -0.000000000000000000 ) ) ;
#70878 = CARTESIAN_POINT ( 'NONE',  ( 20.87155475150661132, 11.75000000001115907, -194.0955865291576004 ) ) ;
#70880 = ORIENTED_EDGE ( 'NONE', *, *, #218294, .F. ) ;
#70879 = CARTESIAN_POINT ( 'NONE',  ( 21.05000000000000071, 7.244009986534929446, -211.6437749090809177 ) ) ;
#70881 = DIRECTION ( 'NONE',  ( 0.000000000000000000, -1.000000000000000000, -6.982962677686265922E-15 ) ) ;
#70882 = DIRECTION ( 'NONE',  ( -0.000000000000000000, 6.982962677686266711E-15, -1.000000000000000000 ) ) ;
#70883 = DIRECTION ( 'NONE',  ( 0.000000000000000000, -7.086529944415886769E-15, 1.000000000000000000 ) ) ;
#70884 = CARTESIAN_POINT ( 'NONE',  ( 20.94999999999999929, 74.63912941282028157, -161.9501095574334215 ) ) ;
#70885 = ORIENTED_EDGE ( 'NONE', *, *, #12463, .T. ) ;
#70886 = FACE_OUTER_BOUND ( 'NONE', #94640, .T. ) ;
#70888 = VERTEX_POINT ( 'NONE', #31579 ) ;
#70887 = VECTOR ( 'NONE', #48997, 1000.000000000000114 ) ;
#70889 = EDGE_CURVE ( 'NONE', #107985, #238512, #224576, .T. ) ;
#70890 = AXIS2_PLACEMENT_3D ( 'NONE', #255082, #15267, #256357 ) ;
#70891 = DIRECTION ( 'NONE',  ( 1.000000000000000000, 0.000000000000000000, 0.000000000000000000 ) ) ;
#70892 = ORIENTED_EDGE ( 'NONE', *, *, #206020, .T. ) ;
#70893 = CARTESIAN_POINT ( 'NONE',  ( 18.59999999999999787, -1.263275465206102233, -74.90186466674640542 ) ) ;
#70894 = ORIENTED_EDGE ( 'NONE', *, *, #141754, .F. ) ;
#70895 = CARTESIAN_POINT ( 'NONE',  ( 20.99999999999999645, 9.750000000011137757, -143.2500000000000284 ) ) ;
#70896 = DIRECTION ( 'NONE',  ( 0.000000000000000000, 0.000000000000000000, 1.000000000000000000 ) ) ;
#70897 = EDGE_CURVE ( 'NONE', #123919, #169080, #64842, .T. ) ;
#70898 = FACE_OUTER_BOUND ( 'NONE', #201632, .T. ) ;
#70899 = ORIENTED_EDGE ( 'NONE', *, *, #57963, .T. ) ;
#70900 = EDGE_CURVE ( 'NONE', #213658, #150739, #168536, .T. ) ;
#70901 = CARTESIAN_POINT ( 'NONE',  ( -16.93710578446424009, 9.949999999999983302, -12.91880398379939265 ) ) ;
#70902 = PLANE ( 'NONE',  #32627 ) ;
#70903 = LINE ( 'NONE', #74767, #66564 ) ;
#70904 = EDGE_CURVE ( 'NONE', #148979, #103023, #243917, .T. ) ;
#70905 = DIRECTION ( 'NONE',  ( -0.000000000000000000, 1.000000000000000000, 6.982962677686266711E-15 ) ) ;
#70907 = CARTESIAN_POINT ( 'NONE',  ( -16.83558968593875349, 9.949999999999983302, -20.83769481238317667 ) ) ;
#70906 = AXIS2_PLACEMENT_3D ( 'NONE', #45240, #222569, #204297 ) ;
#70908 = ORIENTED_EDGE ( 'NONE', *, *, #14700, .T. ) ;
#70909 = DIRECTION ( 'NONE',  ( -7.304098846218134667E-16, 1.000000000000000000, 6.982962677686267499E-15 ) ) ;
#70910 = ORIENTED_EDGE ( 'NONE', *, *, #43515, .T. ) ;
#70912 = ORIENTED_EDGE ( 'NONE', *, *, #194834, .T. ) ;
#70911 = CARTESIAN_POINT ( 'NONE',  ( 22.39999999999999503, 64.25313205997782973, -247.2214437328673853 ) ) ;
#70913 = EDGE_CURVE ( 'NONE', #31696, #179904, #228480, .T. ) ;
#70914 = ORIENTED_EDGE ( 'NONE', *, *, #129223, .F. ) ;
#70915 = DIRECTION ( 'NONE',  ( 1.000000000000000000, 1.541880601228652843E-16, 2.878400969107353907E-16 ) ) ;
#70916 = EDGE_CURVE ( 'NONE', #197652, #228950, #135759, .T. ) ;
#70917 = ORIENTED_EDGE ( 'NONE', *, *, #85576, .F. ) ;
#70918 = DIRECTION ( 'NONE',  ( -1.000000000000000000, -0.000000000000000000, -0.000000000000000000 ) ) ;
#70919 = FACE_OUTER_BOUND ( 'NONE', #152514, .T. ) ;
#70920 = CARTESIAN_POINT ( 'NONE',  ( 20.94999999999999929, 56.22462877935074488, -228.0203483467521721 ) ) ;
#70921 = VECTOR ( 'NONE', #230833, 1000.000000000000000 ) ;
#70922 = ORIENTED_EDGE ( 'NONE', *, *, #174852, .T. ) ;
#70923 = CARTESIAN_POINT ( 'NONE',  ( -16.94275863009466576, 66.01050395134967630, -123.9148048665654898 ) ) ;
#70924 = DIRECTION ( 'NONE',  ( 2.952720810173289112E-16, 1.000000000000000000, 6.530723674265620862E-15 ) ) ;
#70925 = CARTESIAN_POINT ( 'NONE',  ( -21.14999999999999858, 11.65000000001115588, -73.78386566297820082 ) ) ;
#70926 = EDGE_LOOP ( 'NONE', ( #72670, #181058, #181268, #70324 ) ) ;
#70928 = ORIENTED_EDGE ( 'NONE', *, *, #223844, .T. ) ;
#70927 = CARTESIAN_POINT ( 'NONE',  ( 20.94999999999999574, -11.39257802169451672, -70.07394957983198935 ) ) ;
#70929 = DIRECTION ( 'NONE',  ( -0.5735764363510466035, 0.8191520442889914655, 0.000000000000000000 ) ) ;
#70930 = DIRECTION ( 'NONE',  ( 0.000000000000000000, 1.000000000000000000, 0.000000000000000000 ) ) ;
#70931 = AXIS2_PLACEMENT_3D ( 'NONE', #10275, #169379, #128935 ) ;
#70932 = EDGE_CURVE ( 'NONE', #256624, #85343, #77476, .T. ) ;
#70934 = EDGE_CURVE ( 'NONE', #46286, #230427, #222872, .T. ) ;
#70933 = AXIS2_PLACEMENT_3D ( 'NONE', #38844, #214897, #118379 ) ;
#70935 = EDGE_LOOP ( 'NONE', ( #236222, #49253, #214010, #10371 ) ) ;
#70936 = DIRECTION ( 'NONE',  ( 0.000000000000000000, 1.000000000000000000, 6.982962677686266711E-15 ) ) ;
#70937 = FACE_BOUND ( 'NONE', #234940, .T. ) ;
#70938 = DIRECTION ( 'NONE',  ( 1.000000000000000000, 0.000000000000000000, 0.000000000000000000 ) ) ;
#70939 = ORIENTED_EDGE ( 'NONE', *, *, #51116, .F. ) ;
#70940 = FACE_OUTER_BOUND ( 'NONE', #225279, .T. ) ;
#70941 = CIRCLE ( 'NONE', #37598, 0.09999999999999939493 ) ;
#70942 = ADVANCED_FACE ( 'NONE', ( #104200 ), #83336, .F. ) ;
#70943 = CARTESIAN_POINT ( 'NONE',  ( -22.39999999999999858, -2.500503813844232592, -189.5187041743089367 ) ) ;
#70944 = CIRCLE ( 'NONE', #224834, 0.1000000000000033362 ) ;
#70945 = CIRCLE ( 'NONE', #45958, 0.1000000000000028644 ) ;
#70946 = DIRECTION ( 'NONE',  ( -1.000000000000000000, -0.000000000000000000, -0.000000000000000000 ) ) ;
#70947 = EDGE_CURVE ( 'NONE', #185852, #247118, #224154, .T. ) ;
#70948 = EDGE_CURVE ( 'NONE', #131663, #253340, #225426, .T. ) ;
#70949 = CIRCLE ( 'NONE', #216662, 4.099999999999992539 ) ;
#70950 = AXIS2_PLACEMENT_3D ( 'NONE', #236055, #155275, #139512 ) ;
#70951 = CIRCLE ( 'NONE', #116704, 0.09999999999999609201 ) ;
#70952 = VERTEX_POINT ( 'NONE', #25977 ) ;
#70954 = LINE ( 'NONE', #150472, #190472 ) ;
#70953 = AXIS2_PLACEMENT_3D ( 'NONE', #214415, #215689, #115318 ) ;
#70955 = AXIS2_PLACEMENT_3D ( 'NONE', #249124, #71772, #191732 ) ;
#70956 = ADVANCED_FACE ( 'NONE', ( #3838 ), #6396, .F. ) ;
#70957 = ORIENTED_EDGE ( 'NONE', *, *, #82411, .T. ) ;
#70958 = CARTESIAN_POINT ( 'NONE',  ( -16.91049119928363353, 9.950000000011137047, -188.3817203931907898 ) ) ;
#70959 = CARTESIAN_POINT ( 'NONE',  ( -20.05000000000000426, 9.250000000011157297, -155.2500000000000284 ) ) ;
#70961 = ORIENTED_EDGE ( 'NONE', *, *, #27146, .F. ) ;
#70960 = CARTESIAN_POINT ( 'NONE',  ( 14.77516762759921143, 24.96309550270879285, -232.5807238286745928 ) ) ;
#70962 = EDGE_CURVE ( 'NONE', #228369, #181257, #164987, .T. ) ;
#70963 = CARTESIAN_POINT ( 'NONE',  ( -21.05000000000000071, 85.51932773110404185, -62.55013110796492271 ) ) ;
#70964 = FACE_BOUND ( 'NONE', #120590, .T. ) ;
#70965 = DIRECTION ( 'NONE',  ( 0.000000000000000000, 0.000000000000000000, -1.000000000000000000 ) ) ;
#70966 = CARTESIAN_POINT ( 'NONE',  ( 18.39999999999997371, 64.52683809664901560, -45.27310748452439526 ) ) ;
#70967 = EDGE_CURVE ( 'NONE', #257108, #190470, #215069, .T. ) ;
#70968 = DIRECTION ( 'NONE',  ( 0.000000000000000000, -1.000000000000000000, 0.000000000000000000 ) ) ;
#70969 = CARTESIAN_POINT ( 'NONE',  ( -23.25000000000000000, 1.115600667400684642E-11, -108.4000000000000483 ) ) ;
#70970 = CIRCLE ( 'NONE', #66840, 2.100000000000004530 ) ;
#70972 = ORIENTED_EDGE ( 'NONE', *, *, #236881, .F. ) ;
#70971 = DIRECTION ( 'NONE',  ( -3.265361837132813093E-16, -1.000000000000000000, 7.445645354460596589E-46 ) ) ;
#70973 = DIRECTION ( 'NONE',  ( 0.000000000000000000, -1.000000000000000000, 0.000000000000000000 ) ) ;
#70974 = DIRECTION ( 'NONE',  ( 1.000000000000000000, 0.000000000000000000, 0.000000000000000000 ) ) ;
#70975 = CARTESIAN_POINT ( 'NONE',  ( 18.59999999999999076, -1.149570369564537842, -108.3159124845020074 ) ) ;
#70976 = CARTESIAN_POINT ( 'NONE',  ( -23.15000000000000213, 13.96869538424788360, -210.3925794786331949 ) ) ;
#70977 = EDGE_LOOP ( 'NONE', ( #103379, #170510, #254737 ) ) ;
#70978 = TOROIDAL_SURFACE ( 'NONE', #229176, 12.77500000000000036, 0.1000000000000000056 ) ;
#70979 = DIRECTION ( 'NONE',  ( 0.000000000000000000, 1.000000000000000000, 0.000000000000000000 ) ) ;
#70980 = AXIS2_PLACEMENT_3D ( 'NONE', #169175, #206985, #8786 ) ;
#70981 = FACE_OUTER_BOUND ( 'NONE', #174302, .T. ) ;
#70982 = ORIENTED_EDGE ( 'NONE', *, *, #25351, .F. ) ;
#70983 = AXIS2_PLACEMENT_3D ( 'NONE', #46271, #163675, #107535 ) ;
#70985 = EDGE_CURVE ( 'NONE', #245055, #143179, #126344, .T. ) ;
#70984 = DIRECTION ( 'NONE',  ( 0.000000000000000000, 0.000000000000000000, -1.000000000000000000 ) ) ;
#70986 = DIRECTION ( 'NONE',  ( 1.000000000000000000, 0.000000000000000000, 0.000000000000000000 ) ) ;
#70987 = VERTEX_POINT ( 'NONE', #84605 ) ;
#70988 = DIRECTION ( 'NONE',  ( -1.073024830501117725E-15, 0.000000000000000000, 1.000000000000000000 ) ) ;
#70989 = ORIENTED_EDGE ( 'NONE', *, *, #107291, .F. ) ;
#70990 = DIRECTION ( 'NONE',  ( 1.000000000000000000, 0.000000000000000000, 0.000000000000000000 ) ) ;
#70992 = VERTEX_POINT ( 'NONE', #204591 ) ;
#70991 = DIRECTION ( 'NONE',  ( -1.186688945009010077E-16, -1.000000000000000000, -6.982962677686266711E-15 ) ) ;
#70993 = AXIS2_PLACEMENT_3D ( 'NONE', #51266, #30471, #68306 ) ;
#70994 = SPHERICAL_SURFACE ( 'NONE', #239844, 0.1000000000000000056 ) ;
#70995 = ORIENTED_EDGE ( 'NONE', *, *, #227537, .T. ) ;
#70996 = TOROIDAL_SURFACE ( 'NONE', #216712, 0.2000000000000000111, 0.1000000000000000056 ) ;
#70997 = DIRECTION ( 'NONE',  ( 0.000000000000000000, -1.000000000000000000, 0.000000000000000000 ) ) ;
#70998 = ORIENTED_EDGE ( 'NONE', *, *, #109099, .F. ) ;
#70999 = ORIENTED_EDGE ( 'NONE', *, *, #148500, .T. ) ;
#71000 = CYLINDRICAL_SURFACE ( 'NONE', #194426, 11.79999999999999005 ) ;
#71001 = VERTEX_POINT ( 'NONE', #87202 ) ;
#71002 = EDGE_CURVE ( 'NONE', #246004, #102227, #102596, .T. ) ;
#71003 = DIRECTION ( 'NONE',  ( 0.000000000000000000, -1.000000000000000000, 0.000000000000000000 ) ) ;
#71004 = CIRCLE ( 'NONE', #216715, 0.1000000000000045158 ) ;
#71005 = ORIENTED_EDGE ( 'NONE', *, *, #52470, .F. ) ;
#71006 = CIRCLE ( 'NONE', #191820, 0.1000000000000002554 ) ;
#71007 = ORIENTED_EDGE ( 'NONE', *, *, #54517, .F. ) ;
#71008 = DIRECTION ( 'NONE',  ( -3.265361837132813093E-16, -1.000000000000000000, -7.086529944415894657E-15 ) ) ;
#71009 = CARTESIAN_POINT ( 'NONE',  ( -18.42637059832564361, 38.00040471499162464, -261.0434343050587813 ) ) ;
#71010 = ORIENTED_EDGE ( 'NONE', *, *, #92792, .T. ) ;
#71011 = CYLINDRICAL_SURFACE ( 'NONE', #233711, 0.5000000000000014433 ) ;
#71012 = CARTESIAN_POINT ( 'NONE',  ( -12.60206096961793776, 66.61031399435691469, -187.8502639781731034 ) ) ;
#71013 = CARTESIAN_POINT ( 'NONE',  ( 18.39999999999999858, -9.499999999999998224, -7.032069396699667685 ) ) ;
#71014 = ORIENTED_EDGE ( 'NONE', *, *, #256324, .F. ) ;
#71015 = CARTESIAN_POINT ( 'NONE',  ( 20.85000000000000142, 1.115600667400684642E-11, -167.5000000000000284 ) ) ;
#71016 = LINE ( 'NONE', #11017, #94431 ) ;
#71017 = DIRECTION ( 'NONE',  ( -1.000000000000000000, -0.000000000000000000, -0.000000000000000000 ) ) ;
#71018 = VECTOR ( 'NONE', #239431, 1000.000000000000000 ) ;
#71019 = DIRECTION ( 'NONE',  ( 1.000000000000000000, 0.000000000000000000, 0.000000000000000000 ) ) ;
#71020 = ORIENTED_EDGE ( 'NONE', *, *, #141925, .T. ) ;
#71021 = CARTESIAN_POINT ( 'NONE',  ( 18.53317502108576420, 10.32263460347359896, -106.0605957968672470 ) ) ;
#71022 = VERTEX_POINT ( 'NONE', #226721 ) ;
#71023 = FACE_OUTER_BOUND ( 'NONE', #131799, .T. ) ;
#71024 = EDGE_LOOP ( 'NONE', ( #23995, #194880, #34976, #247472 ) ) ;
#71025 = CARTESIAN_POINT ( 'NONE',  ( -20.64999999999999858, 4.350000000011156054, -155.1500000000000057 ) ) ;
#71026 = CARTESIAN_POINT ( 'NONE',  ( -23.39999999999994529, 77.83551161375991967, -47.52760213295649550 ) ) ;
#71027 = ORIENTED_EDGE ( 'NONE', *, *, #14664, .T. ) ;
#71028 = ORIENTED_EDGE ( 'NONE', *, *, #78606, .F. ) ;
#71029 = CARTESIAN_POINT ( 'NONE',  ( 20.05000000000002913, 9.775875410973618784, -211.8174516384118817 ) ) ;
#71030 = CARTESIAN_POINT ( 'NONE',  ( 20.94999999999999574, -1.162701749926853712, -108.5000000000000426 ) ) ;
#71031 = ORIENTED_EDGE ( 'NONE', *, *, #60001, .F. ) ;
#71032 = DIRECTION ( 'NONE',  ( 0.000000000000000000, 0.8660254037844384856, -0.5000000000000003331 ) ) ;
#71033 = CARTESIAN_POINT ( 'NONE',  ( -18.55807992284872299, 65.67101464000481315, -63.94043916224792667 ) ) ;
#71034 = VERTEX_POINT ( 'NONE', #27288 ) ;
#71035 = AXIS2_PLACEMENT_3D ( 'NONE', #28281, #69959, #246011 ) ;
#71036 = AXIS2_PLACEMENT_3D ( 'NONE', #79725, #159312, #40672 ) ;
#71037 = EDGE_CURVE ( 'NONE', #198432, #88303, #23571, .T. ) ;
#71038 = CIRCLE ( 'NONE', #116801, 0.09999999999999939493 ) ;
#71039 = VERTEX_POINT ( 'NONE', #85905 ) ;
#71040 = VECTOR ( 'NONE', #243374, 1000.000000000000000 ) ;
#71041 = LINE ( 'NONE', #170167, #230597 ) ;
#71042 = EDGE_CURVE ( 'NONE', #26109, #216892, #186335, .T. ) ;
#71043 = CARTESIAN_POINT ( 'NONE',  ( -16.77732147278574715, 22.98807097893278595, -230.9449972797045803 ) ) ;
#71044 = EDGE_CURVE ( 'NONE', #57597, #227768, #48089, .T. ) ;
#71045 = LINE ( 'NONE', #87988, #176046 ) ;
#71047 = ORIENTED_EDGE ( 'NONE', *, *, #182099, .T. ) ;
#71046 = DIRECTION ( 'NONE',  ( 0.000000000000000000, -6.938893903907222067E-15, 1.000000000000000000 ) ) ;
#71048 = DIRECTION ( 'NONE',  ( 0.000000000000000000, -1.000000000000000000, -7.272083257015735086E-15 ) ) ;
#71049 = VECTOR ( 'NONE', #2814, 1000.000000000000000 ) ;
#71050 = DIRECTION ( 'NONE',  ( -1.000000000000000000, -2.952720810173289112E-16, 0.000000000000000000 ) ) ;
#71051 = CARTESIAN_POINT ( 'NONE',  ( -21.64999999999999858, 9.350000000011133849, -143.2500000000000284 ) ) ;
#71053 = CARTESIAN_POINT ( 'NONE',  ( -23.25000000000000000, 64.25000000001229239, -157.8731074845244393 ) ) ;
#71052 = DIRECTION ( 'NONE',  ( 0.000000000000000000, 1.000000000000000000, 0.000000000000000000 ) ) ;
#71054 = DIRECTION ( 'NONE',  ( 0.000000000000000000, -8.326672684688666480E-14, 1.000000000000000000 ) ) ;
#71055 = CARTESIAN_POINT ( 'NONE',  ( -18.50000000000000711, 11.65000000001115232, -174.5148057706539930 ) ) ;
#71056 = EDGE_CURVE ( 'NONE', #250008, #43046, #252455, .T. ) ;
#71057 = CARTESIAN_POINT ( 'NONE',  ( 20.85000000000000142, 77.83585931145526615, -58.01866831572577610 ) ) ;
#71058 = DIRECTION ( 'NONE',  ( 1.000000000000000000, 1.541880601228652843E-16, 2.878400969107353907E-16 ) ) ;
#71059 = ORIENTED_EDGE ( 'NONE', *, *, #1968, .F. ) ;
#71060 = ORIENTED_EDGE ( 'NONE', *, *, #186283, .F. ) ;
#71061 = ORIENTED_EDGE ( 'NONE', *, *, #42350, .F. ) ;
#71062 = EDGE_CURVE ( 'NONE', #198608, #177524, #44258, .T. ) ;
#71063 = AXIS2_PLACEMENT_3D ( 'NONE', #114123, #211969, #152009 ) ;
#71064 = DIRECTION ( 'NONE',  ( 0.000000000000000000, 0.000000000000000000, -1.000000000000000000 ) ) ;
#71065 = CARTESIAN_POINT ( 'NONE',  ( 20.04142135623730070, 52.91185528119410009, -244.1460391050142675 ) ) ;
#71066 = ORIENTED_EDGE ( 'NONE', *, *, #163402, .F. ) ;
#71067 = CIRCLE ( 'NONE', #62858, 0.1000000000000054040 ) ;
#71068 = DIRECTION ( 'NONE',  ( -1.000000000000000000, 2.952720810173289112E-16, 2.061873921506763405E-30 ) ) ;
#71069 = CARTESIAN_POINT ( 'NONE',  ( 21.14999999999999503, -2.576749817950531707, -189.6385361693310756 ) ) ;
#71070 = CIRCLE ( 'NONE', #195977, 0.1000000000000028644 ) ;
#71071 = CARTESIAN_POINT ( 'NONE',  ( -28.12018973533754362, 11.62642356364895413, -347.0000000000001137 ) ) ;
#71072 = ORIENTED_EDGE ( 'NONE', *, *, #227368, .F. ) ;
#71073 = EDGE_LOOP ( 'NONE', ( #57313, #69416, #238141, #27125 ) ) ;
#71074 = DIRECTION ( 'NONE',  ( 0.000000000000000000, 0.1298341882519953583, 0.9915357197604861561 ) ) ;
#71075 = CARTESIAN_POINT ( 'NONE',  ( -20.64999999999999858, 85.00000000001253397, -179.4170766071767389 ) ) ;
#71076 = ORIENTED_EDGE ( 'NONE', *, *, #111677, .F. ) ;
#71077 = CIRCLE ( 'NONE', #54295, 0.09999999999999892308 ) ;
#71078 = CARTESIAN_POINT ( 'NONE',  ( -20.85000000000000142, 14.80545736607782814, -235.9842437978701639 ) ) ;
#71080 = VERTEX_POINT ( 'NONE', #145897 ) ;
#71079 = DIRECTION ( 'NONE',  ( 1.000000000000000000, 0.000000000000000000, 0.000000000000000000 ) ) ;
#71081 = DIRECTION ( 'NONE',  ( 0.000000000000000000, -0.9654727137038715545, 0.2605042016806676242 ) ) ;
#71082 = FACE_OUTER_BOUND ( 'NONE', #76735, .T. ) ;
#71085 = EDGE_CURVE ( 'NONE', #182894, #13509, #206687, .T. ) ;
#71084 = ORIENTED_EDGE ( 'NONE', *, *, #74838, .F. ) ;
#71083 = LINE ( 'NONE', #209281, #193736 ) ;
#71086 = CARTESIAN_POINT ( 'NONE',  ( 23.14999999999999858, 36.65892442174935439, -249.5511627012433848 ) ) ;
#71087 = CARTESIAN_POINT ( 'NONE',  ( -20.94999999999999929, 67.23127455305841238, -235.8551265064783991 ) ) ;
#71088 = CARTESIAN_POINT ( 'NONE',  ( 23.25000000000000000, 9.028068219309963283, -211.6732836666006961 ) ) ;
#71090 = CARTESIAN_POINT ( 'NONE',  ( 21.09546886439552438, 8.878553113026056209, -179.7370938505546007 ) ) ;
#71089 = DIRECTION ( 'NONE',  ( 0.000000000000000000, 0.000000000000000000, 1.000000000000000000 ) ) ;
#71091 = CARTESIAN_POINT ( 'NONE',  ( -20.64999999999999858, 4.250000000011156409, -88.15000000000004832 ) ) ;
#71092 = AXIS2_PLACEMENT_3D ( 'NONE', #72503, #152048, #12536 ) ;
#71093 = LINE ( 'NONE', #149354, #218427 ) ;
#71094 = CARTESIAN_POINT ( 'NONE',  ( 21.05000000000000071, 1.434803724213256082, -230.7796651547878355 ) ) ;
#71095 = CARTESIAN_POINT ( 'NONE',  ( -20.94999999999999929, 11.65000000001115588, -74.01480577065404987 ) ) ;
#71096 = CIRCLE ( 'NONE', #16935, 0.09999999999999939493 ) ;
#71097 = ORIENTED_EDGE ( 'NONE', *, *, #48281, .T. ) ;
#71098 = ADVANCED_FACE ( 'NONE', ( #203325 ), #127640, .T. ) ;
#71100 = CYLINDRICAL_SURFACE ( 'NONE', #226373, 0.09999999999998898659 ) ;
#71099 = CIRCLE ( 'NONE', #100654, 0.1000000000000008937 ) ;
#71101 = VERTEX_POINT ( 'NONE', #142052 ) ;
#71103 = CYLINDRICAL_SURFACE ( 'NONE', #14641, 0.09999999999998898659 ) ;
#71102 = AXIS2_PLACEMENT_3D ( 'NONE', #246, #84885, #83604 ) ;
#71104 = EDGE_LOOP ( 'NONE', ( #108206, #166985, #124183, #225464, #16621 ) ) ;
#71105 = CARTESIAN_POINT ( 'NONE',  ( -23.15000000000000213, 54.14029358995846053, -238.9803212882090691 ) ) ;
#71106 = CARTESIAN_POINT ( 'NONE',  ( 20.94999999999999929, 5.000000000011153745, -188.5947339810868755 ) ) ;
#71107 = AXIS2_PLACEMENT_3D ( 'NONE', #237594, #155520, #159353 ) ;
#71109 = ADVANCED_FACE ( 'NONE', ( #221571 ), #146962, .T. ) ;
#71108 = CIRCLE ( 'NONE', #237692, 0.1000000000000028644 ) ;
#71110 = VERTEX_POINT ( 'NONE', #243509 ) ;
#71111 = CARTESIAN_POINT ( 'NONE',  ( 21.97500000000000497, 51.97441255244040548, -232.0063394385699667 ) ) ;
#71112 = EDGE_CURVE ( 'NONE', #56965, #181257, #189939, .T. ) ;
#71114 = ORIENTED_EDGE ( 'NONE', *, *, #41052, .T. ) ;
#71113 = AXIS2_PLACEMENT_3D ( 'NONE', #168033, #44205, #247531 ) ;
#71115 = CIRCLE ( 'NONE', #54526, 0.09999999999999911737 ) ;
#71116 = AXIS2_PLACEMENT_3D ( 'NONE', #32354, #253918, #115708 ) ;
#71117 = ORIENTED_EDGE ( 'NONE', *, *, #188842, .T. ) ;
#71118 = TOROIDAL_SURFACE ( 'NONE', #216835, 0.2000000000000000111, 0.1000000000000000056 ) ;
#71119 = AXIS2_PLACEMENT_3D ( 'NONE', #190118, #32351, #168019 ) ;
#71120 = CARTESIAN_POINT ( 'NONE',  ( -20.00857864376270001, 9.350000000011156942, -79.35000000000005116 ) ) ;
#71121 = CARTESIAN_POINT ( 'NONE',  ( 20.95512820512820085, 10.62384868372303615, -41.16491356908760935 ) ) ;
#71122 = CARTESIAN_POINT ( 'NONE',  ( -20.54999999999999716, 9.350000000011156942, -121.6500000000000341 ) ) ;
#71123 = DIRECTION ( 'NONE',  ( 0.000000000000000000, 0.7106264324241517993, -0.7035695228903270371 ) ) ;
#71124 = LINE ( 'NONE', #150641, #127442 ) ;
#71125 = EDGE_CURVE ( 'NONE', #224041, #194487, #223932, .T. ) ;
#71127 = CARTESIAN_POINT ( 'NONE',  ( -20.94999999999999929, -11.64999999998884306, -164.4000000000000057 ) ) ;
#71126 = CARTESIAN_POINT ( 'NONE',  ( -20.94999999999999929, 1.115600667400684642E-11, -67.00000000000000000 ) ) ;
#71128 = CARTESIAN_POINT ( 'NONE',  ( 18.50000000000010303, 10.37342005529087530, -58.26578812462643953 ) ) ;
#71130 = EDGE_LOOP ( 'NONE', ( #114662, #147892, #166605, #69555 ) ) ;
#71129 = DIRECTION ( 'NONE',  ( 3.469446951953635015E-14, 6.982962677686266711E-15, -1.000000000000000000 ) ) ;
#71132 = CARTESIAN_POINT ( 'NONE',  ( -22.57320508075687115, 11.75000000001115552, -100.5000000000000284 ) ) ;
#71131 = CARTESIAN_POINT ( 'NONE',  ( 18.59999999999997655, -1.164121893230052995, -141.9148480855716343 ) ) ;
#71133 = CARTESIAN_POINT ( 'NONE',  ( -18.59999999999999787, 1.115600667400684642E-11, -33.50000000000000000 ) ) ;
#71134 = ORIENTED_EDGE ( 'NONE', *, *, #90257, .T. ) ;
#71135 = DIRECTION ( 'NONE',  ( -1.000000000000000000, -0.000000000000000000, -0.000000000000000000 ) ) ;
#71136 = DIRECTION ( 'NONE',  ( 0.000000000000000000, -1.000000000000000000, 0.000000000000000000 ) ) ;
#71138 = EDGE_CURVE ( 'NONE', #209692, #208323, #27670, .T. ) ;
#71137 = DIRECTION ( 'NONE',  ( -1.000000000000000000, 0.000000000000000000, 0.000000000000000000 ) ) ;
#71140 = EDGE_CURVE ( 'NONE', #203407, #208166, #173436, .T. ) ;
#71139 = ORIENTED_EDGE ( 'NONE', *, *, #132307, .T. ) ;
#71141 = AXIS2_PLACEMENT_3D ( 'NONE', #95072, #234581, #252855 ) ;
#71142 = DIRECTION ( 'NONE',  ( 1.000000000000000000, -7.136802563874199107E-16, -1.554319503706925307E-16 ) ) ;
#71143 = CARTESIAN_POINT ( 'NONE',  ( 20.94999999999999574, 87.48912529308769592, -66.42310748452423752 ) ) ;
#71144 = ORIENTED_EDGE ( 'NONE', *, *, #226009, .T. ) ;
#71145 = ORIENTED_EDGE ( 'NONE', *, *, #139454, .T. ) ;
#71146 = EDGE_CURVE ( 'NONE', #133539, #11282, #15158, .T. ) ;
#71147 = CARTESIAN_POINT ( 'NONE',  ( 21.05000000000000071, 1.115600667400684642E-11, -167.5000000000000284 ) ) ;
#71148 = CARTESIAN_POINT ( 'NONE',  ( -18.50016250449483124, 10.29766095125282988, -172.9743663933276139 ) ) ;
#71149 = CARTESIAN_POINT ( 'NONE',  ( -21.55000000000000426, 68.29142135624984178, -182.3731074845244109 ) ) ;
#71151 = EDGE_CURVE ( 'NONE', #64097, #163036, #182269, .T. ) ;
#71150 = DIRECTION ( 'NONE',  ( 1.000000000000000000, 0.000000000000000000, 0.000000000000000000 ) ) ;
#71152 = ORIENTED_EDGE ( 'NONE', *, *, #49673, .F. ) ;
#71153 = EDGE_CURVE ( 'NONE', #71514, #196401, #25752, .T. ) ;
#71154 = FACE_OUTER_BOUND ( 'NONE', #41625, .T. ) ;
#71155 = CARTESIAN_POINT ( 'NONE',  ( -20.94999999999999929, 86.19075908668452257, -209.4719249499869136 ) ) ;
#71156 = CARTESIAN_POINT ( 'NONE',  ( 20.46382478191414833, 8.901379558713770734, -75.54572809488314533 ) ) ;
#71158 = B_SPLINE_CURVE_WITH_KNOTS ( 'NONE', 3,
 ( #252934, #234670, #133016, #36497, #79423, #159013, #14369, #53467 ),
 .UNSPECIFIED., .F., .F.,
 ( 4, 2, 2, 4 ),
 ( 0.000000000000000000, 0.0001049670497870003278, 0.0002099340995740006557, 0.0004198681991479968120 ),
 .UNSPECIFIED. ) ;
#71157 = LINE ( 'NONE', #112831, #70131 ) ;
#71159 = VERTEX_POINT ( 'NONE', #143110 ) ;
#71160 = PLANE ( 'NONE',  #188437 ) ;
#71161 = TOROIDAL_SURFACE ( 'NONE', #25380, 0.4000000000000009104, 0.1000000000000000056 ) ;
#71163 = ORIENTED_EDGE ( 'NONE', *, *, #63780, .T. ) ;
#71162 = CARTESIAN_POINT ( 'NONE',  ( 21.05000000000000071, 1.115600667400684642E-11, -100.5000000000000426 ) ) ;
#71165 = EDGE_CURVE ( 'NONE', #220497, #101456, #91336, .T. ) ;
#71164 = FACE_OUTER_BOUND ( 'NONE', #168299, .T. ) ;
#71166 = CARTESIAN_POINT ( 'NONE',  ( -18.59999999999999787, -1.164121893230052995, -108.4148480855716485 ) ) ;
#71167 = CARTESIAN_POINT ( 'NONE',  ( 21.14999999999999858, 8.786607556600111835, -12.35000000000000320 ) ) ;
#71168 = EDGE_CURVE ( 'NONE', #141902, #156342, #194256, .T. ) ;
#71169 = ORIENTED_EDGE ( 'NONE', *, *, #12250, .T. ) ;
#71170 = DIRECTION ( 'NONE',  ( 0.000000000000000000, -0.9651348961777158619, 0.2617529984165028467 ) ) ;
#71171 = CARTESIAN_POINT ( 'NONE',  ( -21.14999999999999858, 76.10000000001203091, -114.6726782920691079 ) ) ;
#71172 = CARTESIAN_POINT ( 'NONE',  ( 23.14999999999999503, 61.95000000001194707, -108.5368025552853197 ) ) ;
#71173 = ORIENTED_EDGE ( 'NONE', *, *, #201513, .T. ) ;
#71174 = DIRECTION ( 'NONE',  ( 0.000000000000000000, 0.000000000000000000, 1.000000000000000000 ) ) ;
#71175 = AXIS2_PLACEMENT_3D ( 'NONE', #197070, #231099, #18448 ) ;
#71176 = CARTESIAN_POINT ( 'NONE',  ( 21.14999999999999858, 11.65000000001116298, -155.7499999999999716 ) ) ;
#71177 = LINE ( 'NONE', #30772, #100454 ) ;
#71178 = DIRECTION ( 'NONE',  ( -0.000000000000000000, 1.265107689135680095E-16, -1.000000000000000000 ) ) ;
#71179 = ADVANCED_FACE ( 'NONE', ( #225208 ), #166574, .T. ) ;
#71181 = AXIS2_PLACEMENT_3D ( 'NONE', #147092, #90979, #226631 ) ;
#71180 = CARTESIAN_POINT ( 'NONE',  ( 21.05000000000000071, 6.540656951712402467, -167.4999999999999716 ) ) ;
#71183 = DIRECTION ( 'NONE',  ( -0.000000000000000000, 0.9887567792719327286, 0.1495327102803745423 ) ) ;
#71182 = VECTOR ( 'NONE', #214752, 1000.000000000000000 ) ;
#71184 = VERTEX_POINT ( 'NONE', #105241 ) ;
#71185 = ORIENTED_EDGE ( 'NONE', *, *, #61126, .T. ) ;
#71186 = CARTESIAN_POINT ( 'NONE',  ( 20.94999999999999574, 70.44746257310249860, -228.4383880063670347 ) ) ;
#71187 = FACE_OUTER_BOUND ( 'NONE', #176195, .T. ) ;
#71188 = CARTESIAN_POINT ( 'NONE',  ( 18.59999999999999076, 64.35000000001220144, -145.1731074845244507 ) ) ;
#71189 = DIRECTION ( 'NONE',  ( -0.000000000000000000, 1.000000000000000000, 6.352154140967427193E-15 ) ) ;
#71190 = CARTESIAN_POINT ( 'NONE',  ( -17.01473183483382101, 66.05000000001157900, -56.77310748452439526 ) ) ;
#71191 = LINE ( 'NONE', #248522, #213473 ) ;
#71192 = ADVANCED_FACE ( 'NONE', ( #64869 ), #46577, .F. ) ;
#71193 = CARTESIAN_POINT ( 'NONE',  ( -23.15000000000000213, 2.000000000011154189, -187.7753780772378889 ) ) ;
#71194 = AXIS2_PLACEMENT_3D ( 'NONE', #49147, #148251, #254683 ) ;
#71195 = CARTESIAN_POINT ( 'NONE',  ( -16.93230518875208190, 10.00075036143099716, -113.0757783481015366 ) ) ;
#71196 = EDGE_CURVE ( 'NONE', #114288, #158981, #256507, .T. ) ;
#71197 = CARTESIAN_POINT ( 'NONE',  ( -20.94999999999999929, 7.021664781911246322, -137.8335654018973457 ) ) ;
#71198 = VERTEX_POINT ( 'NONE', #186110 ) ;
#71199 = DIRECTION ( 'NONE',  ( 0.000000000000000000, 0.9553114395363172529, -0.2956011730204217702 ) ) ;
#71200 = EDGE_CURVE ( 'NONE', #1255, #235463, #81748, .T. ) ;
#71201 = EDGE_CURVE ( 'NONE', #199913, #45747, #177506, .T. ) ;
#71202 = ORIENTED_EDGE ( 'NONE', *, *, #226340, .T. ) ;
#71203 = CARTESIAN_POINT ( 'NONE',  ( 23.14999999999998437, 76.00000000001237765, -170.0231074845243597 ) ) ;
#71204 = CARTESIAN_POINT ( 'NONE',  ( -20.94999999999999929, -11.39257802169451317, -63.92605042016806749 ) ) ;
#71205 = CARTESIAN_POINT ( 'NONE',  ( 21.13920837816993270, 8.783247050131068434, -79.25000000000004263 ) ) ;
#71206 = CARTESIAN_POINT ( 'NONE',  ( -22.45305610364635385, -3.275978944802467652, -228.2735455795363748 ) ) ;
#71207 = ADVANCED_FACE ( 'NONE', ( #162709 ), #28357, .T. ) ;
#71208 = FACE_OUTER_BOUND ( 'NONE', #135780, .T. ) ;
#71209 = ORIENTED_EDGE ( 'NONE', *, *, #197435, .T. ) ;
#71210 = CARTESIAN_POINT ( 'NONE',  ( -16.93583594267724379, 22.92587748271144221, -230.8406021309349399 ) ) ;
#71211 = CIRCLE ( 'NONE', #443, 0.1000000000000121764 ) ;
#71212 = DIRECTION ( 'NONE',  ( 1.000000000000000000, 0.000000000000000000, 0.000000000000000000 ) ) ;
#71213 = TOROIDAL_SURFACE ( 'NONE', #46059, 0.4000000000000009104, 0.1000000000000000056 ) ;
#71214 = CIRCLE ( 'NONE', #137816, 11.65000000000000746 ) ;
#71215 = CARTESIAN_POINT ( 'NONE',  ( 18.59999999999999076, 69.55000000001207638, -126.5060803140843291 ) ) ;
#71216 = LINE ( 'NONE', #150735, #14690 ) ;
#71217 = AXIS2_PLACEMENT_3D ( 'NONE', #141057, #220592, #58907 ) ;
#71218 = CARTESIAN_POINT ( 'NONE',  ( -22.49999999999999645, 11.74956712350054744, -167.3991416309012550 ) ) ;
#71219 = EDGE_CURVE ( 'NONE', #57263, #105021, #2665, .T. ) ;
#71220 = AXIS2_PLACEMENT_3D ( 'NONE', #166130, #43578, #206499 ) ;
#71221 = EDGE_CURVE ( 'NONE', #195076, #253894, #119213, .T. ) ;
#71222 = ORIENTED_EDGE ( 'NONE', *, *, #181183, .F. ) ;
#71223 = FACE_OUTER_BOUND ( 'NONE', #56176, .T. ) ;
#71224 = DIRECTION ( 'NONE',  ( 0.000000000000000000, 0.000000000000000000, -1.000000000000000000 ) ) ;
#71225 = ORIENTED_EDGE ( 'NONE', *, *, #96418, .T. ) ;
#71226 = EDGE_CURVE ( 'NONE', #167295, #181396, #22496, .T. ) ;
#71227 = VERTEX_POINT ( 'NONE', #32192 ) ;
#71228 = CARTESIAN_POINT ( 'NONE',  ( 18.59999999999999432, -1.162701749926855266, -75.10000000000003695 ) ) ;
#71229 = CARTESIAN_POINT ( 'NONE',  ( 20.95512828230154767, 11.26953735574613447, -211.0340866196924026 ) ) ;
#71230 = AXIS2_PLACEMENT_3D ( 'NONE', #246279, #169347, #25953 ) ;
#71231 = ORIENTED_EDGE ( 'NONE', *, *, #89002, .T. ) ;
#71232 = CARTESIAN_POINT ( 'NONE',  ( 20.46382478191415188, 39.33264809402798079, -236.7398086741081613 ) ) ;
#71233 = CARTESIAN_POINT ( 'NONE',  ( -20.00857864376270001, 22.34215363070824623, -231.2750834139128528 ) ) ;
#71234 = ORIENTED_EDGE ( 'NONE', *, *, #8409, .T. ) ;
#71235 = EDGE_CURVE ( 'NONE', #59075, #16193, #88260, .T. ) ;
#71236 = ADVANCED_FACE ( 'NONE', ( #70036 ), #181749, .T. ) ;
#71237 = DIRECTION ( 'NONE',  ( 0.000000000000000000, 0.8660254037844411501, 0.4999999999999956701 ) ) ;
#71238 = ADVANCED_FACE ( 'NONE', ( #229092 ), #133830, .T. ) ;
#71239 = EDGE_LOOP ( 'NONE', ( #106216, #134075 ) ) ;
#71240 = CARTESIAN_POINT ( 'NONE',  ( -20.54999999999999716, 1.115600667400684642E-11, -146.9749999999999943 ) ) ;
#71241 = DIRECTION ( 'NONE',  ( 0.000000000000000000, 0.000000000000000000, 1.000000000000000000 ) ) ;
#71242 = VECTOR ( 'NONE', #185668, 1000.000000000000000 ) ;
#71244 = ORIENTED_EDGE ( 'NONE', *, *, #202457, .T. ) ;
#71243 = LINE ( 'NONE', #133754, #258084 ) ;
#71245 = EDGE_CURVE ( 'NONE', #249371, #41329, #56264, .T. ) ;
#71246 = CYLINDRICAL_SURFACE ( 'NONE', #211445, 11.80000000000000426 ) ;
#71248 = CARTESIAN_POINT ( 'NONE',  ( 18.50000000000000000, 85.50000000001240608, -163.4229180933022576 ) ) ;
#71247 = UNCERTAINTY_MEASURE_WITH_UNIT (LENGTH_MEASURE( 1.000000000000000082E-05 ), #148376, 'distance_accuracy_value', 'NONE');
#71249 = PLANE ( 'NONE',  #116872 ) ;
#71250 = CARTESIAN_POINT ( 'NONE',  ( -16.79270642812249292, 66.05375578307356932, -157.3620407630891123 ) ) ;
#71251 = EDGE_CURVE ( 'NONE', #248097, #217199, #167859, .T. ) ;
#71252 = DIRECTION ( 'NONE',  ( 0.000000000000000000, 6.982962677686266711E-15, -1.000000000000000000 ) ) ;
#71253 = CIRCLE ( 'NONE', #54656, 0.5000000000000004441 ) ;
#71255 = B_SPLINE_CURVE_WITH_KNOTS ( 'NONE', 3,
 ( #71261, #251135, #188608, #231607, #8698, #171660, #50361, #69977, #149515, #191214, #246029, #206898, #52947, #27005, #111644, #89499, #247293, #9980, #129912, #186053, #7399, #249874, #11270, #67386, #86920, #166516, #167801, #209459, #169094, #248589 ),
 .UNSPECIFIED., .F., .F.,
 ( 4, 2, 2, 2, 2, 2, 2, 2, 2, 2, 2, 2, 2, 2, 4 ),
 ( 0.000000000000000000, 0.0003422764154113355664, 0.0006845528308226711328, 0.001026829246234006862, 0.001369105661645342266, 0.002053658492468009387, 0.002738211323290676725, 0.003080487738702010828, 0.003422764154113344063, 0.003765040569524678166, 0.004107316984936011835, 0.004449593400347345504, 0.004791869815758679173, 0.005134146231170016311, 0.005476422646581353450 ),
 .UNSPECIFIED. ) ;
#71254 = DIRECTION ( 'NONE',  ( 0.000000000000000000, 0.5341055959866798375, -0.8454177738465836756 ) ) ;
#71256 = CARTESIAN_POINT ( 'NONE',  ( 23.04999999999999716, 8.822561741677553471, -87.85000000000003695 ) ) ;
#71258 = ORIENTED_EDGE ( 'NONE', *, *, #24298, .F. ) ;
#71257 = LINE ( 'NONE', #171656, #65472 ) ;
#71259 = VERTEX_POINT ( 'NONE', #173011 ) ;
#71261 = CARTESIAN_POINT ( 'NONE',  ( -12.25000000000000178, 9.350000000011139178, -83.75000000000004263 ) ) ;
#71260 = CARTESIAN_POINT ( 'NONE',  ( 21.05000000000000071, 1.360870587203197646, -108.5729979270909951 ) ) ;
#71262 = ORIENTED_EDGE ( 'NONE', *, *, #91537, .F. ) ;
#71263 = VECTOR ( 'NONE', #200510, 1000.000000000000000 ) ;
#71264 = ORIENTED_EDGE ( 'NONE', *, *, #181323, .T. ) ;
#71265 = CARTESIAN_POINT ( 'NONE',  ( 23.25000000000000000, 6.550000000011156231, -112.8500000000000369 ) ) ;
#71266 = CARTESIAN_POINT ( 'NONE',  ( 11.60000000000006004, 67.75000000001118394, -23.62310748452479103 ) ) ;
#71267 = CIRCLE ( 'NONE', #133778, 0.09999999999999939493 ) ;
#71268 = DIRECTION ( 'NONE',  ( 1.000000000000000000, 0.000000000000000000, 0.000000000000000000 ) ) ;
#71269 = CIRCLE ( 'NONE', #112754, 0.1000000000000054040 ) ;
#71270 = CARTESIAN_POINT ( 'NONE',  ( 19.86930884467575353, 11.68691006698223411, -58.23922263893884121 ) ) ;
#71271 = EDGE_CURVE ( 'NONE', #4242, #212844, #89976, .T. ) ;
#71272 = LINE ( 'NONE', #229049, #102549 ) ;
#71273 = CARTESIAN_POINT ( 'NONE',  ( -16.94445028196807002, 51.64060657411747712, -231.8906364537310196 ) ) ;
#71274 = CARTESIAN_POINT ( 'NONE',  ( 21.05000000000000071, 17.11694853917244075, -224.3781540347815451 ) ) ;
#71275 = ADVANCED_FACE ( 'NONE', ( #109121 ), #89560, .T. ) ;
#71276 = EDGE_LOOP ( 'NONE', ( #167438, #247113, #182920, #68857 ) ) ;
#71277 = ORIENTED_EDGE ( 'NONE', *, *, #137245, .T. ) ;
#71278 = DIRECTION ( 'NONE',  ( -1.000000000000000000, 3.854941057726231589E-15, 0.000000000000000000 ) ) ;
#71279 = CIRCLE ( 'NONE', #204530, 12.87499999999999822 ) ;
#71280 = ORIENTED_EDGE ( 'NONE', *, *, #79484, .T. ) ;
#71281 = CARTESIAN_POINT ( 'NONE',  ( 21.14999999999999858, 64.35000000001195986, -102.9231074845243938 ) ) ;
#71283 = EDGE_LOOP ( 'NONE', ( #101448, #4661, #122487, #209742 ) ) ;
#71282 = AXIS2_PLACEMENT_3D ( 'NONE', #171047, #210133, #26689 ) ;
#71284 = CARTESIAN_POINT ( 'NONE',  ( -21.52071067811865746, 7.779289321892505882, -79.35000000000005116 ) ) ;
#71285 = AXIS2_PLACEMENT_3D ( 'NONE', #10633, #69330, #45903 ) ;
#71286 = AXIS2_PLACEMENT_3D ( 'NONE', #58622, #2500, #82018 ) ;
#71287 = PLANE ( 'NONE',  #197041 ) ;
#71288 = ADVANCED_FACE ( 'NONE', ( #10034 ), #50422, .F. ) ;
#71289 = CARTESIAN_POINT ( 'NONE',  ( 18.49999999999998934, 6.550000000011156231, -54.75000000000000000 ) ) ;
#71290 = ORIENTED_EDGE ( 'NONE', *, *, #10641, .F. ) ;
#71291 = AXIS2_PLACEMENT_3D ( 'NONE', #55581, #38629, #118165 ) ;
#71293 = CIRCLE ( 'NONE', #192104, 0.09999999999999543976 ) ;
#71292 = CARTESIAN_POINT ( 'NONE',  ( -20.64999999999999858, 2.000000000011154189, -87.27537807723794572 ) ) ;
#71294 = EDGE_LOOP ( 'NONE', ( #232753, #185975, #245934, #192593 ) ) ;
#71295 = CARTESIAN_POINT ( 'NONE',  ( 20.95512820512820440, 67.12384868372396340, -127.9644784893834100 ) ) ;
#71296 = DIRECTION ( 'NONE',  ( 1.000000000000000000, -7.304098846218134667E-16, 4.607487905232622991E-31 ) ) ;
#71297 = ORIENTED_EDGE ( 'NONE', *, *, #241672, .T. ) ;
#71298 = DIRECTION ( 'NONE',  ( 0.000000000000000000, 0.000000000000000000, 1.000000000000000000 ) ) ;
#71299 = ORIENTED_EDGE ( 'NONE', *, *, #42546, .T. ) ;
#71302 = ORIENTED_EDGE ( 'NONE', *, *, #182170, .F. ) ;
#71301 = DIRECTION ( 'NONE',  ( 1.000000000000000000, 0.000000000000000000, 0.000000000000000000 ) ) ;
#71300 = CYLINDRICAL_SURFACE ( 'NONE', #128448, 0.09999999999999939493 ) ;
#71303 = EDGE_CURVE ( 'NONE', #125623, #46813, #248557, .T. ) ;
#71304 = AXIS2_PLACEMENT_3D ( 'NONE', #211958, #230219, #68589 ) ;
#71305 = CARTESIAN_POINT ( 'NONE',  ( -21.14999999999999858, 11.75000000001115552, -134.0000000000000284 ) ) ;
#71306 = TOROIDAL_SURFACE ( 'NONE', #171107, 7.800000000000000711, 0.1000000000000000056 ) ;
#71308 = ORIENTED_EDGE ( 'NONE', *, *, #142536, .F. ) ;
#71307 = AXIS2_PLACEMENT_3D ( 'NONE', #99647, #144891, #236607 ) ;
#71309 = CIRCLE ( 'NONE', #217009, 7.899999999999990585 ) ;
#71310 = CYLINDRICAL_SURFACE ( 'NONE', #71194, 0.5000000000000014433 ) ;
#71311 = ORIENTED_EDGE ( 'NONE', *, *, #152456, .F. ) ;
#71312 = DIRECTION ( 'NONE',  ( 0.000000000000000000, 0.000000000000000000, -1.000000000000000000 ) ) ;
#71313 = VERTEX_POINT ( 'NONE', #111705 ) ;
#71314 = CARTESIAN_POINT ( 'NONE',  ( 21.04999999999913030, 18.82942951893005201, -229.9355821828612534 ) ) ;
#71315 = DIRECTION ( 'NONE',  ( -0.000000000000000000, 1.000000000000000000, 6.982962677686266711E-15 ) ) ;
#71316 = CARTESIAN_POINT ( 'NONE',  ( 18.50211644919734866, 67.49401193140447219, -195.5283494629371148 ) ) ;
#71317 = CARTESIAN_POINT ( 'NONE',  ( -16.27683809663751191, 11.10425270649114715, -208.0484446391143365 ) ) ;
#71318 = ORIENTED_EDGE ( 'NONE', *, *, #178063, .T. ) ;
#71319 = DIRECTION ( 'NONE',  ( -1.000000000000000000, 0.000000000000000000, 0.000000000000000000 ) ) ;
#71320 = CARTESIAN_POINT ( 'NONE',  ( 18.49505816908823874, 86.88289224156976331, -199.4521454443379582 ) ) ;
#71321 = SPHERICAL_SURFACE ( 'NONE', #226089, 0.1000000000000000056 ) ;
#71322 = VERTEX_POINT ( 'NONE', #118123 ) ;
#71323 = CARTESIAN_POINT ( 'NONE',  ( -21.76363531954647357, 0.09900187429944841411, 7.012936547871741588 ) ) ;
#71324 = EDGE_LOOP ( 'NONE', ( #95732, #154813, #207958, #150374, #139594 ) ) ;
#71325 = CARTESIAN_POINT ( 'NONE',  ( 23.15000000000000213, -8.596261682231833845, -143.4501275171502925 ) ) ;
#71326 = VERTEX_POINT ( 'NONE', #15187 ) ;
#71327 = CARTESIAN_POINT ( 'NONE',  ( -23.15000000000000213, 4.150000000011156764, -79.35000000000005116 ) ) ;
#71328 = DIRECTION ( 'NONE',  ( 0.000000000000000000, 0.000000000000000000, 1.000000000000000000 ) ) ;
#71330 = ORIENTED_EDGE ( 'NONE', *, *, #24165, .F. ) ;
#71329 = CARTESIAN_POINT ( 'NONE',  ( -16.83558968593869309, 44.14671151211591393, -235.2939007918319021 ) ) ;
#71331 = DIRECTION ( 'NONE',  ( 0.000000000000000000, 0.000000000000000000, 1.000000000000000000 ) ) ;
#71332 = EDGE_LOOP ( 'NONE', ( #203692, #90786, #127964, #113936 ) ) ;
#71333 = AXIS2_PLACEMENT_3D ( 'NONE', #127432, #105256, #222660 ) ;
#71334 = CARTESIAN_POINT ( 'NONE',  ( -20.87155475150660777, 36.12098300858677646, -235.9333785785471775 ) ) ;
#71335 = EDGE_CURVE ( 'NONE', #91812, #106067, #165175, .T. ) ;
#71336 = CARTESIAN_POINT ( 'NONE',  ( -16.88705144915408951, 9.950000000011193890, -113.4309785947120872 ) ) ;
#71337 = VERTEX_POINT ( 'NONE', #115547 ) ;
#71338 = CARTESIAN_POINT ( 'NONE',  ( 21.53699400380723361, 69.21228820682206617, -203.5231074845244166 ) ) ;
#71339 = CARTESIAN_POINT ( 'NONE',  ( -18.59999999999999787, -10.80884033489985363, 5.900000000000001243 ) ) ;
#71340 = ORIENTED_EDGE ( 'NONE', *, *, #234889, .F. ) ;
#71341 = CARTESIAN_POINT ( 'NONE',  ( 20.85000000000000142, 87.65000000001214175, -136.5231074845242745 ) ) ;
#71342 = ORIENTED_EDGE ( 'NONE', *, *, #36326, .T. ) ;
#71344 = CARTESIAN_POINT ( 'NONE',  ( -23.15000000000000213, 1.115600667400684642E-11, -167.5000000000000284 ) ) ;
#71343 = VECTOR ( 'NONE', #144195, 1000.000000000000000 ) ;
#71345 = CARTESIAN_POINT ( 'NONE',  ( 21.05000000000000071, 85.00000000001207923, -126.6291383618717816 ) ) ;
#71346 = EDGE_CURVE ( 'NONE', #199368, #156063, #158558, .T. ) ;
#71347 = ADVANCED_FACE ( 'NONE', ( #98507 ), #257568, .F. ) ;
#71350 = ORIENTED_EDGE ( 'NONE', *, *, #4704, .T. ) ;
#71349 = ORIENTED_EDGE ( 'NONE', *, *, #92732, .F. ) ;
#71348 = CARTESIAN_POINT ( 'NONE',  ( 23.14999999999999858, 5.499999999999998224, -12.40526601891309788 ) ) ;
#71351 = DIRECTION ( 'NONE',  ( 0.000000000000000000, 0.000000000000000000, 1.000000000000000000 ) ) ;
#71352 = CARTESIAN_POINT ( 'NONE',  ( 20.94999999999999574, 39.29335463311362275, -236.8946393634874994 ) ) ;
#71353 = CARTESIAN_POINT ( 'NONE',  ( 20.94999999999999929, 1.115600667400684642E-11, -167.4999999999999716 ) ) ;
#71355 = DIRECTION ( 'NONE',  ( 1.000000000000000000, -0.000000000000000000, -0.000000000000000000 ) ) ;
#71354 = CARTESIAN_POINT ( 'NONE',  ( 22.47110162079220785, 0.02879741281384913879, -88.85006406331571327 ) ) ;
#71356 = LINE ( 'NONE', #36074, #148803 ) ;
#71357 = FACE_OUTER_BOUND ( 'NONE', #144186, .T. ) ;
#71358 = AXIS2_PLACEMENT_3D ( 'NONE', #23686, #26237, #221823 ) ;
#71359 = ADVANCED_FACE ( 'NONE', ( #235491 ), #6952, .T. ) ;
#71360 = DIRECTION ( 'NONE',  ( 1.000000000000000000, 0.000000000000000000, 0.000000000000000000 ) ) ;
#71361 = AXIS2_PLACEMENT_3D ( 'NONE', #175612, #16539, #230437 ) ;
#71362 = DIRECTION ( 'NONE',  ( 0.000000000000000000, 0.9876197685951241256, 0.1568667991644932258 ) ) ;
#71364 = ORIENTED_EDGE ( 'NONE', *, *, #181960, .T. ) ;
#71363 = CIRCLE ( 'NONE', #125510, 0.09999999999998464284 ) ;
#71365 = EDGE_LOOP ( 'NONE', ( #90038, #143693, #241980 ) ) ;
#71366 = EDGE_CURVE ( 'NONE', #114547, #50189, #52734, .T. ) ;
#71367 = LINE ( 'NONE', #153503, #120890 ) ;
#71369 = VERTEX_POINT ( 'NONE', #80238 ) ;
#71368 = EDGE_CURVE ( 'NONE', #37986, #201109, #55540, .T. ) ;
#71370 = VERTEX_POINT ( 'NONE', #76415 ) ;
#71371 = CARTESIAN_POINT ( 'NONE',  ( 23.40000000000005542, 74.16448838626247664, -47.52760213295649550 ) ) ;
#71372 = VERTEX_POINT ( 'NONE', #119417 ) ;
#71373 = CARTESIAN_POINT ( 'NONE',  ( 21.04116576186320842, 43.56632586560215259, -234.8146366772427029 ) ) ;
#71374 = ADVANCED_FACE ( 'NONE', ( #179398 ), #34769, .T. ) ;
#71375 = ORIENTED_EDGE ( 'NONE', *, *, #102918, .F. ) ;
#71376 = EDGE_CURVE ( 'NONE', #215584, #208846, #86030, .T. ) ;
#71377 = VECTOR ( 'NONE', #116514, 1000.000000000000000 ) ;
#71378 = CARTESIAN_POINT ( 'NONE',  ( 21.05000000000000071, 5.500000000011153745, -88.09473398108696074 ) ) ;
#71379 = DIRECTION ( 'NONE',  ( 0.000000000000000000, -0.1568667991644863147, -0.9876197685951252359 ) ) ;
#71381 = VERTEX_POINT ( 'NONE', #97228 ) ;
#71380 = ORIENTED_EDGE ( 'NONE', *, *, #45155, .F. ) ;
#71382 = ORIENTED_EDGE ( 'NONE', *, *, #142347, .T. ) ;
#71383 = VERTEX_POINT ( 'NONE', #238058 ) ;
#71384 = EDGE_LOOP ( 'NONE', ( #20776, #240758, #1365 ) ) ;
#71385 = CARTESIAN_POINT ( 'NONE',  ( -20.65000000000000568, 64.19947762500697763, -225.4487242757812737 ) ) ;
#71386 = DIRECTION ( 'NONE',  ( -5.603264701231743991E-32, 0.2128009952263606175, -0.9770955615653316162 ) ) ;
#71387 = CARTESIAN_POINT ( 'NONE',  ( -15.66061380678752180, 9.360723793997193454, -184.8139271946066913 ) ) ;
#71389 = ORIENTED_EDGE ( 'NONE', *, *, #108187, .F. ) ;
#71388 = DIRECTION ( 'NONE',  ( 0.000000000000000000, 0.000000000000000000, -1.000000000000000000 ) ) ;
#71390 = DIRECTION ( 'NONE',  ( -0.000000000000000000, -2.891205793294679805E-16, 1.000000000000000000 ) ) ;
#71391 = CARTESIAN_POINT ( 'NONE',  ( -20.54999999999999716, -9.499999999988846255, -191.1060308773475356 ) ) ;
#71393 = ORIENTED_EDGE ( 'NONE', *, *, #9330, .F. ) ;
#71392 = CARTESIAN_POINT ( 'NONE',  ( -18.40000000000000213, 62.48575673152180343, -209.5207689439494345 ) ) ;
#71394 = CARTESIAN_POINT ( 'NONE',  ( -23.15000000000000213, 76.00000000001242029, -166.0231074845243597 ) ) ;
#71395 = EDGE_LOOP ( 'NONE', ( #129659, #161432, #58806, #137711 ) ) ;
#71396 = FACE_OUTER_BOUND ( 'NONE', #40864, .T. ) ;
#71398 = EDGE_CURVE ( 'NONE', #34286, #79153, #119391, .T. ) ;
#71397 = EDGE_LOOP ( 'NONE', ( #183946, #249693, #104069, #49045 ) ) ;
#71399 = CARTESIAN_POINT ( 'NONE',  ( 20.85000000000000142, 45.93315328338058379, -256.6017782078560003 ) ) ;
#71400 = CARTESIAN_POINT ( 'NONE',  ( 20.94999999999999929, -9.500000000000001776, -9.893969122652443104 ) ) ;
#71401 = CIRCLE ( 'NONE', #75500, 0.1000000000000028644 ) ;
#71402 = CIRCLE ( 'NONE', #204638, 0.09999999999998898659 ) ;
#71403 = AXIS2_PLACEMENT_3D ( 'NONE', #177009, #238223, #15354 ) ;
#71404 = ORIENTED_EDGE ( 'NONE', *, *, #75838, .F. ) ;
#71406 = DIRECTION ( 'NONE',  ( 0.000000000000000000, 0.000000000000000000, 1.000000000000000000 ) ) ;
#71405 = CARTESIAN_POINT ( 'NONE',  ( -21.93340585900940454, 76.00000000001273293, -210.8472545066297812 ) ) ;
#71407 = LINE ( 'NONE', #153541, #180864 ) ;
#71408 = DIRECTION ( 'NONE',  ( -1.000000000000000000, -0.000000000000000000, -0.000000000000000000 ) ) ;
#71409 = CARTESIAN_POINT ( 'NONE',  ( -20.54999999999999716, 1.115600667400684642E-11, -200.9999999999999432 ) ) ;
#71410 = ORIENTED_EDGE ( 'NONE', *, *, #11715, .T. ) ;
#71411 = EDGE_LOOP ( 'NONE', ( #206859, #112957, #241737, #107551 ) ) ;
#71412 = EDGE_CURVE ( 'NONE', #111684, #20030, #231837, .T. ) ;
#71413 = CARTESIAN_POINT ( 'NONE',  ( 21.05000000000000071, 8.876614585087102327, -8.385080478844674445 ) ) ;
#71414 = DIRECTION ( 'NONE',  ( 0.000000000000000000, 0.2617529984165152257, 0.9651348961777124202 ) ) ;
#71415 = ORIENTED_EDGE ( 'NONE', *, *, #90035, .F. ) ;
#71416 = LINE ( 'NONE', #173113, #22644 ) ;
#71417 = VERTEX_POINT ( 'NONE', #36035 ) ;
#71418 = LINE ( 'NONE', #89657, #106571 ) ;
#71419 = CARTESIAN_POINT ( 'NONE',  ( -20.85000000000000142, -1.164121893241208960, -41.41484808557160591 ) ) ;
#71420 = CIRCLE ( 'NONE', #167287, 0.1000000000000052097 ) ;
#71421 = CYLINDRICAL_SURFACE ( 'NONE', #174131, 0.1000000000000072220 ) ;
#71422 = EDGE_LOOP ( 'NONE', ( #34132, #93622, #37467, #211239 ) ) ;
#71423 = CARTESIAN_POINT ( 'NONE',  ( -16.80100426158790228, 66.05684947961644582, -190.8401617316903582 ) ) ;
#71424 =( LENGTH_UNIT ( ) NAMED_UNIT ( * ) SI_UNIT ( .MILLI., .METRE. ) );
#71425 = ADVANCED_FACE ( 'NONE', ( #157275 ), #215916, .F. ) ;
#71426 = ORIENTED_EDGE ( 'NONE', *, *, #64693, .F. ) ;
#71427 = ORIENTED_EDGE ( 'NONE', *, *, #237285, .F. ) ;
#71428 = ORIENTED_EDGE ( 'NONE', *, *, #228046, .F. ) ;
#71429 = CARTESIAN_POINT ( 'NONE',  ( 22.57320508075688537, 64.25000000001213607, -136.5231074845243882 ) ) ;
#71430 = CARTESIAN_POINT ( 'NONE',  ( 12.84233041328156588, 66.58946139148270049, -54.09041948738352090 ) ) ;
#71431 = CARTESIAN_POINT ( 'NONE',  ( -23.49999999999994316, 79.88763423575340994, -7.282924647898262549 ) ) ;
#71432 = CARTESIAN_POINT ( 'NONE',  ( -18.40000000000000213, 70.35000000001187459, -90.37310748452433984 ) ) ;
#71433 = DIRECTION ( 'NONE',  ( 0.000000000000000000, -0.2128009952263603677, 0.9770955615653313941 ) ) ;
#71434 = VECTOR ( 'NONE', #80930, 1000.000000000000114 ) ;
#71435 = EDGE_CURVE ( 'NONE', #220754, #116282, #77664, .T. ) ;
#71437 = FACE_OUTER_BOUND ( 'NONE', #1444, .T. ) ;
#71436 = CARTESIAN_POINT ( 'NONE',  ( -22.47071067811866385, 10.68684811775433907, -226.8807012965928323 ) ) ;
#71439 = ORIENTED_EDGE ( 'NONE', *, *, #222613, .F. ) ;
#71438 = DIRECTION ( 'NONE',  ( 0.000000000000000000, 0.9126074666063771490, 0.4088369013363281623 ) ) ;
#71440 = DIRECTION ( 'NONE',  ( -1.073024830501117725E-15, 6.982962677686266711E-15, -1.000000000000000000 ) ) ;
#71441 = ORIENTED_EDGE ( 'NONE', *, *, #205150, .F. ) ;
#71442 = CARTESIAN_POINT ( 'NONE',  ( -14.23072895065543086, 9.455987233623899257, -149.0115311668978393 ) ) ;
#71443 = VERTEX_POINT ( 'NONE', #234205 ) ;
#71444 = ORIENTED_EDGE ( 'NONE', *, *, #18581, .F. ) ;
#71445 = CARTESIAN_POINT ( 'NONE',  ( 20.94999999999999929, 1.115624548013267999E-11, -199.0999999999999375 ) ) ;
#71446 = AXIS2_PLACEMENT_3D ( 'NONE', #178897, #182728, #220554 ) ;
#71447 = FACE_OUTER_BOUND ( 'NONE', #87526, .T. ) ;
#71449 = ADVANCED_FACE ( 'NONE', ( #16478 ), #37320, .T. ) ;
#71448 = LINE ( 'NONE', #169285, #41909 ) ;
#71450 = EDGE_CURVE ( 'NONE', #211300, #233201, #176832, .T. ) ;
#71451 = FACE_OUTER_BOUND ( 'NONE', #250924, .T. ) ;
#71452 = AXIS2_PLACEMENT_3D ( 'NONE', #114246, #174268, #33468 ) ;
#71453 = CARTESIAN_POINT ( 'NONE',  ( 20.94999675878240808, 18.34775554461856828, -236.8759397601555179 ) ) ;
#71454 = VECTOR ( 'NONE', #14407, 1000.000000000000000 ) ;
#71455 = ORIENTED_EDGE ( 'NONE', *, *, #75336, .F. ) ;
#71456 = VERTEX_POINT ( 'NONE', #217200 ) ;
#71457 = EDGE_CURVE ( 'NONE', #163426, #79894, #235905, .T. ) ;
#71458 = AXIS2_PLACEMENT_3D ( 'NONE', #222821, #204551, #181159 ) ;
#71459 = CARTESIAN_POINT ( 'NONE',  ( 23.15000000000000213, -11.64999999998884483, -100.5000000000000284 ) ) ;
#71460 = ORIENTED_EDGE ( 'NONE', *, *, #248130, .F. ) ;
#71461 = CARTESIAN_POINT ( 'NONE',  ( -21.64999999999999858, 52.95562111564758823, -234.1965973584252652 ) ) ;
#71462 = ORIENTED_EDGE ( 'NONE', *, *, #226015, .T. ) ;
#71463 = DIRECTION ( 'NONE',  ( 0.000000000000000000, -1.000000000000000000, 0.000000000000000000 ) ) ;
#71464 = CARTESIAN_POINT ( 'NONE',  ( -21.05000000000000071, 11.60000000001115339, -60.07179676972449300 ) ) ;
#71465 = CARTESIAN_POINT ( 'NONE',  ( 21.05000000000005400, 67.65000000001118963, -25.06452884076210452 ) ) ;
#71466 = CARTESIAN_POINT ( 'NONE',  ( 21.08804281139604342, 65.37816569817111656, -157.6731075171456098 ) ) ;
#71467 = ORIENTED_EDGE ( 'NONE', *, *, #90739, .F. ) ;
#71468 = FACE_OUTER_BOUND ( 'NONE', #104222, .T. ) ;
#71470 = FACE_OUTER_BOUND ( 'NONE', #11449, .T. ) ;
#71469 = VECTOR ( 'NONE', #184272, 1000.000000000000000 ) ;
#71471 = DIRECTION ( 'NONE',  ( 0.000000000000000000, -0.9126074666063660468, -0.4088369013363524762 ) ) ;
#71472 = DIRECTION ( 'NONE',  ( 1.000000000000000000, 0.000000000000000000, 0.000000000000000000 ) ) ;
#71473 = DIRECTION ( 'NONE',  ( 0.000000000000000000, 0.7397360091702777085, -0.6728971962616808744 ) ) ;
#71474 = AXIS2_PLACEMENT_3D ( 'NONE', #171984, #169416, #111982 ) ;
#71475 = DIRECTION ( 'NONE',  ( -2.602085213965226419E-14, 0.2617529984165031243, 0.9651348961777157509 ) ) ;
#71476 = ORIENTED_EDGE ( 'NONE', *, *, #144500, .T. ) ;
#71477 = VECTOR ( 'NONE', #130673, 1000.000000000000000 ) ;
#71478 = DIRECTION ( 'NONE',  ( 0.000000000000000000, -7.109473446599835262E-15, 1.000000000000000000 ) ) ;
#71479 = VERTEX_POINT ( 'NONE', #202791 ) ;
#71480 = EDGE_CURVE ( 'NONE', #256542, #183369, #40325, .T. ) ;
#71481 = CARTESIAN_POINT ( 'NONE',  ( -23.25000000000000000, -1.736705739456431807, -145.5174225876237699 ) ) ;
#71482 = EDGE_CURVE ( 'NONE', #233023, #164661, #123481, .T. ) ;
#71483 = AXIS2_PLACEMENT_3D ( 'NONE', #69358, #75464, #247968 ) ;
#71484 = PLANE ( 'NONE',  #141821 ) ;
#71485 = CARTESIAN_POINT ( 'NONE',  ( -16.83794479845801817, 66.07364258066029095, -82.32666278030205831 ) ) ;
#71486 = DIRECTION ( 'NONE',  ( -1.000000000000000000, -0.000000000000000000, -0.000000000000000000 ) ) ;
#71487 = DIRECTION ( 'NONE',  ( 0.7071067811865463515, 0.7071067811865487940, 4.937700262164540154E-15 ) ) ;
#71488 = CARTESIAN_POINT ( 'NONE',  ( 20.97107704358301916, 67.12452184799103350, -161.4641342551351784 ) ) ;
#71489 = ORIENTED_EDGE ( 'NONE', *, *, #235357, .T. ) ;
#71490 = DIRECTION ( 'NONE',  ( 2.952720810173289112E-16, -1.000000000000000000, 0.000000000000000000 ) ) ;
#71491 = DIRECTION ( 'NONE',  ( 0.000000000000000000, -0.8814952561688513821, 0.4721928772777189698 ) ) ;
#71492 = CARTESIAN_POINT ( 'NONE',  ( 21.46681500593592773, 10.36690126540559653, -227.6878377563196523 ) ) ;
#71493 = DIRECTION ( 'NONE',  ( 0.000000000000000000, 0.9998779222360096863, -0.01562500000001061998 ) ) ;
#71494 = EDGE_CURVE ( 'NONE', #126765, #166239, #219775, .T. ) ;
#71495 = AXIS2_PLACEMENT_3D ( 'NONE', #220907, #102221, #36602 ) ;
#71496 = AXIS2_PLACEMENT_3D ( 'NONE', #135600, #36555, #235990 ) ;
#71497 = LINE ( 'NONE', #14081, #228141 ) ;
#71498 = CIRCLE ( 'NONE', #213111, 0.2000000000000057288 ) ;
#71499 = AXIS2_PLACEMENT_3D ( 'NONE', #228257, #246515, #130421 ) ;
#71500 = ORIENTED_EDGE ( 'NONE', *, *, #244745, .F. ) ;
#71501 = VERTEX_POINT ( 'NONE', #84073 ) ;
#71502 = LINE ( 'NONE', #166761, #25082 ) ;
#71503 = CARTESIAN_POINT ( 'NONE',  ( 20.73486653747088582, 68.75000000001205080, -127.2731074845243597 ) ) ;
#71504 = CARTESIAN_POINT ( 'NONE',  ( -21.05000000000000071, -4.990442493977163885, -233.3018263216538628 ) ) ;
#71505 = DIRECTION ( 'NONE',  ( 0.000000000000000000, -0.9126074666063771490, -0.4088369013363281623 ) ) ;
#71506 =( BOUNDED_SURFACE ( )  B_SPLINE_SURFACE ( 3, 2, ( 
 ( #94205, #75943, #211606 ),
 ( #73404, #254540, #212887 ),
 ( #13409, #155512, #172526 ),
 ( #195905, #95495, #253278 ),
 ( #115066, #232468, #215443 ),
 ( #15994, #92919, #154241 ) ),
 .UNSPECIFIED., .F., .F., .F. ) 
 B_SPLINE_SURFACE_WITH_KNOTS ( ( 4, 2, 4 ),
 ( 3, 3 ),
 ( 0.0001792624049599645341, 0.0003686986002124761691, 0.0005581347954649877770 ),
 ( 0.000000000000000000, 1.000000000000000000 ),
 .UNSPECIFIED. ) 
 GEOMETRIC_REPRESENTATION_ITEM ( )  RATIONAL_B_SPLINE_SURFACE ( (
 ( 1.000000000000000000, 0.9238795325112807433, 1.000000000000000000),
 ( 1.000000000000000000, 0.9229318695232904268, 1.000000000000000000),
 ( 1.000000000000000000, 0.8926288119238101615, 1.000000000000000000),
 ( 1.000000000000000000, 0.8123777807263494743, 1.000000000000000000),
 ( 1.000000000000000000, 0.7629087100937503862, 1.000000000000000000),
 ( 1.000000000000000000, 0.7071067811865467956, 1.000000000000000000) ) ) 
 REPRESENTATION_ITEM ( '' )  SURFACE ( )  );
#71507 = ORIENTED_EDGE ( 'NONE', *, *, #148607, .T. ) ;
#71508 = FACE_OUTER_BOUND ( 'NONE', #161384, .T. ) ;
#71509 = DIRECTION ( 'NONE',  ( 1.000000000000000000, 0.000000000000000000, 0.000000000000000000 ) ) ;
#71510 = VERTEX_POINT ( 'NONE', #106238 ) ;
#71511 = CARTESIAN_POINT ( 'NONE',  ( -20.64999999999999858, 76.00000000001267608, -203.5231074845243597 ) ) ;
#71512 = EDGE_CURVE ( 'NONE', #140913, #126382, #120716, .T. ) ;
#71513 = AXIS2_PLACEMENT_3D ( 'NONE', #96692, #116310, #234966 ) ;
#71514 = VERTEX_POINT ( 'NONE', #181954 ) ;
#71516 = VERTEX_POINT ( 'NONE', #162401 ) ;
#71515 =( BOUNDED_SURFACE ( )  B_SPLINE_SURFACE ( 3, 2, ( 
 ( #57795, #158242, #156945 ),
 ( #36998, #115221, #55214 ),
 ( #95648, #137333, #93081 ),
 ( #153111, #59063, #254684 ),
 ( #233886, #53958, #214326 ),
 ( #255962, #35717, #176499 ) ),
 .UNSPECIFIED., .F., .F., .F. ) 
 B_SPLINE_SURFACE_WITH_KNOTS ( ( 4, 2, 4 ),
 ( 3, 3 ),
 ( 0.0001792624049599545865, 0.0003686986002124574124, 0.0005581347954649602382 ),
 ( 0.000000000000000000, 1.000000000000000000 ),
 .UNSPECIFIED. ) 
 GEOMETRIC_REPRESENTATION_ITEM ( )  RATIONAL_B_SPLINE_SURFACE ( (
 ( 1.000000000000000000, 0.9238795325112828527, 1.000000000000000000),
 ( 1.000000000000000000, 0.9229318695241007786, 1.000000000000000000),
 ( 1.000000000000000000, 0.8926288119227357987, 1.000000000000000000),
 ( 1.000000000000000000, 0.8123777807274511487, 1.000000000000000000),
 ( 1.000000000000000000, 0.7629087100929119458, 1.000000000000000000),
 ( 1.000000000000000000, 0.7071067811865475727, 1.000000000000000000) ) ) 
 REPRESENTATION_ITEM ( '' )  SURFACE ( )  );
#71517 = ADVANCED_FACE ( 'NONE', ( #245778 ), #131859, .T. ) ;
#71518 = VERTEX_POINT ( 'NONE', #164951 ) ;
#71519 = CARTESIAN_POINT ( 'NONE',  ( 18.59999999999999076, 11.65000000000000391, -24.85000000000000142 ) ) ;
#71520 = FACE_BOUND ( 'NONE', #105761, .T. ) ;
#71521 = CARTESIAN_POINT ( 'NONE',  ( 21.08804281139618908, 10.62183430185229938, -112.8499999673788494 ) ) ;
#71522 = CIRCLE ( 'NONE', #67210, 0.09999999999999949207 ) ;
#71523 = DIRECTION ( 'NONE',  ( 0.000000000000000000, 0.9915357197604862671, -0.1298341882519953583 ) ) ;
#71524 = FACE_OUTER_BOUND ( 'NONE', #164254, .T. ) ;
#71525 = EDGE_CURVE ( 'NONE', #75919, #196737, #183238, .T. ) ;
#71526 = CARTESIAN_POINT ( 'NONE',  ( 18.49999999999999645, 1.835341550235567887, -78.55515129256302487 ) ) ;
#71527 = CARTESIAN_POINT ( 'NONE',  ( -16.94107738177415712, 10.01423928513662176, -12.55000000000000249 ) ) ;
#71529 = DIRECTION ( 'NONE',  ( 1.000000000000000000, 0.000000000000000000, 0.000000000000000000 ) ) ;
#71528 = DIRECTION ( 'NONE',  ( 0.000000000000000000, 0.1144908148674362580, 0.9934243067848653741 ) ) ;
#71530 = DIRECTION ( 'NONE',  ( 0.000000000000000000, -0.8814952561688423893, 0.4721928772777359007 ) ) ;
#71531 = EDGE_CURVE ( 'NONE', #114189, #131422, #23753, .T. ) ;
#71532 = CARTESIAN_POINT ( 'NONE',  ( 18.59999999999999076, 65.75000000001196554, -111.7731074845243739 ) ) ;
#71533 = DIRECTION ( 'NONE',  ( -1.000000000000000000, -3.265361837132813093E-16, 0.000000000000000000 ) ) ;
#71534 = CARTESIAN_POINT ( 'NONE',  ( 20.95462737510932882, 18.78654564892814349, -228.0014245997133742 ) ) ;
#71535 = EDGE_LOOP ( 'NONE', ( #191029, #241294, #22520, #22596 ) ) ;
#71536 = CARTESIAN_POINT ( 'NONE',  ( 18.49999999999998934, 33.69766839675186532, -236.3369293616048026 ) ) ;
#71537 = DIRECTION ( 'NONE',  ( 0.000000000000000000, -0.03181660087583042251, 0.9994937237965568766 ) ) ;
#71538 =( BOUNDED_CURVE ( )  B_SPLINE_CURVE ( 3, ( #246154, #209594, #49227, #29702 ),
 .UNSPECIFIED., .F., .F. ) 
 B_SPLINE_CURVE_WITH_KNOTS ( ( 4, 4 ),
 ( 1.570796326794896558, 3.141592653589793116 ),
 .UNSPECIFIED. ) 
 CURVE ( )  GEOMETRIC_REPRESENTATION_ITEM ( )  RATIONAL_B_SPLINE_CURVE ( ( 1.000000000000000000, 0.8047378541243649375, 0.8047378541243649375, 1.000000000000000000 ) ) 
 REPRESENTATION_ITEM ( '' )  );
#71539 = EDGE_CURVE ( 'NONE', #196694, #20109, #236722, .T. ) ;
#71540 = CIRCLE ( 'NONE', #167218, 4.299999999999970512 ) ;
#71542 = ADVANCED_FACE ( 'NONE', ( #3286 ), #145379, .F. ) ;
#71541 = EDGE_CURVE ( 'NONE', #221590, #217985, #185798, .T. ) ;
#71543 = DIRECTION ( 'NONE',  ( 1.000000000000000000, 0.000000000000000000, 0.000000000000000000 ) ) ;
#71544 = CYLINDRICAL_SURFACE ( 'NONE', #54127, 0.1000000000000028644 ) ;
#71545 = CARTESIAN_POINT ( 'NONE',  ( 20.04142135623730070, 16.02417409648693081, -219.3605785455116006 ) ) ;
#71546 = VERTEX_POINT ( 'NONE', #82805 ) ;
#71547 = VERTEX_POINT ( 'NONE', #42432 ) ;
#71548 = FACE_OUTER_BOUND ( 'NONE', #6809, .T. ) ;
#71549 = EDGE_LOOP ( 'NONE', ( #257552, #121159, #27165, #88410 ) ) ;
#71550 = CARTESIAN_POINT ( 'NONE',  ( 21.76363531954645936, 68.98706345214041846, -136.6221093588237920 ) ) ;
#71551 = CARTESIAN_POINT ( 'NONE',  ( 21.00000000000000000, 14.02742277431099538, -219.5907614236512870 ) ) ;
#71552 = TOROIDAL_SURFACE ( 'NONE', #200711, 0.2000000000000000111, 0.1000000000000000056 ) ;
#71553 = CIRCLE ( 'NONE', #25739, 1.900000000000012790 ) ;
#71554 = EDGE_CURVE ( 'NONE', #217421, #145230, #101069, .T. ) ;
#71555 = ADVANCED_FACE ( 'NONE', ( #204066 ), #161113, .F. ) ;
#71556 = AXIS2_PLACEMENT_3D ( 'NONE', #7703, #147196, #109334 ) ;
#71557 = ORIENTED_EDGE ( 'NONE', *, *, #199435, .F. ) ;
#71558 = DIRECTION ( 'NONE',  ( -1.000000000000000000, 0.000000000000000000, 0.000000000000000000 ) ) ;
#71559 = EDGE_CURVE ( 'NONE', #13430, #230269, #184500, .T. ) ;
#71560 = ORIENTED_EDGE ( 'NONE', *, *, #205901, .T. ) ;
#71561 = CARTESIAN_POINT ( 'NONE',  ( -23.25000000000000000, 36.65892442174935439, -249.5511627012433848 ) ) ;
#71562 = CARTESIAN_POINT ( 'NONE',  ( -21.05000000000000071, 87.48912529308842068, -167.0231074845242745 ) ) ;
#71563 = DIRECTION ( 'NONE',  ( -0.000000000000000000, -0.000000000000000000, -1.000000000000000000 ) ) ;
#71564 = CARTESIAN_POINT ( 'NONE',  ( 18.59999999999999787, -9.749999999999996447, 31.50000000000000000 ) ) ;
#71565 = DIRECTION ( 'NONE',  ( 2.952720810173289605E-16, 1.000000000000000000, 7.086529944415894657E-15 ) ) ;
#71566 = ADVANCED_FACE ( 'NONE', ( #46272 ), #81526, .T. ) ;
#71567 = DIRECTION ( 'NONE',  ( -0.000000000000000000, -6.982962677686266711E-15, 1.000000000000000000 ) ) ;
#71568 = AXIS2_PLACEMENT_3D ( 'NONE', #185021, #106755, #88460 ) ;
#71569 = CARTESIAN_POINT ( 'NONE',  ( 21.05000000000000071, -0.09999999998884338825, -100.5000000000000284 ) ) ;
#71570 = DIRECTION ( 'NONE',  ( 1.000000000000000000, -0.000000000000000000, -0.000000000000000000 ) ) ;
#71573 = ORIENTED_EDGE ( 'NONE', *, *, #199354, .F. ) ;
#71572 = ADVANCED_FACE ( 'NONE', ( #205342 ), #207955, .F. ) ;
#71571 = CARTESIAN_POINT ( 'NONE',  ( 18.39999999999999858, -0.9152171842606988683, -242.2974985173726452 ) ) ;
#71574 = CARTESIAN_POINT ( 'NONE',  ( -20.94999999999999929, 64.40000000001249703, -176.9513107147999449 ) ) ;
#71575 = VERTEX_POINT ( 'NONE', #192240 ) ;
#71576 = ORIENTED_EDGE ( 'NONE', *, *, #139490, .F. ) ;
#71577 = VERTEX_POINT ( 'NONE', #111405 ) ;
#71578 = CARTESIAN_POINT ( 'NONE',  ( 21.05000000000000071, 67.44464249442897597, -214.0562211244547655 ) ) ;
#71579 = CARTESIAN_POINT ( 'NONE',  ( -18.59999999999999787, 11.65000000001115232, -141.0148057706540214 ) ) ;
#71580 = CARTESIAN_POINT ( 'NONE',  ( 22.44352723754029810, 75.99072290496846449, -81.17282882987304049 ) ) ;
#71581 = CARTESIAN_POINT ( 'NONE',  ( -20.85000000000000142, 77.16412189325330928, -128.6082593989527254 ) ) ;
#71582 = DIRECTION ( 'NONE',  ( 0.000000000000000000, 0.000000000000000000, -1.000000000000000000 ) ) ;
#71583 = EDGE_CURVE ( 'NONE', #221113, #205489, #206869, .T. ) ;
#71584 = DIRECTION ( 'NONE',  ( 1.000000000000000000, 3.265361837132813093E-16, -0.000000000000000000 ) ) ;
#71585 = CARTESIAN_POINT ( 'NONE',  ( -20.54999999999999716, 76.00000000001212186, -134.5231074845243313 ) ) ;
#71586 = DIRECTION ( 'NONE',  ( 1.000000000000000000, 0.000000000000000000, 0.000000000000000000 ) ) ;
#71587 = VECTOR ( 'NONE', #144980, 1000.000000000000000 ) ;
#71588 = AXIS2_PLACEMENT_3D ( 'NONE', #73753, #152013, #112854 ) ;
#71589 = LINE ( 'NONE', #49433, #226777 ) ;
#71590 = EDGE_CURVE ( 'NONE', #60627, #177453, #71016, .T. ) ;
#71591 = EDGE_LOOP ( 'NONE', ( #59152, #172160 ) ) ;
#71592 = VERTEX_POINT ( 'NONE', #210504 ) ;
#71593 = ORIENTED_EDGE ( 'NONE', *, *, #153902, .F. ) ;
#71594 = DIRECTION ( 'NONE',  ( -1.000000000000000000, 0.000000000000000000, 0.000000000000000000 ) ) ;
#71595 = ORIENTED_EDGE ( 'NONE', *, *, #141471, .F. ) ;
#71596 = CARTESIAN_POINT ( 'NONE',  ( -20.64999999999999858, 7.150000000011155876, -146.3500000000000227 ) ) ;
#71597 = DIRECTION ( 'NONE',  ( 6.938893903907224433E-15, -1.000000000000000000, -2.891205793294679805E-16 ) ) ;
#71598 = CARTESIAN_POINT ( 'NONE',  ( -20.85000000000000142, 62.86885547537413288, -207.0505773246641752 ) ) ;
#71599 = EDGE_CURVE ( 'NONE', #209282, #253747, #244270, .T. ) ;
#71600 = LINE ( 'NONE', #131550, #168898 ) ;
#71601 = CARTESIAN_POINT ( 'NONE',  ( -21.05000000000000071, 36.65892442174935439, -249.5511627012433848 ) ) ;
#71602 = ORIENTED_EDGE ( 'NONE', *, *, #227089, .T. ) ;
#71603 = AXIS2_PLACEMENT_3D ( 'NONE', #111589, #189840, #149450 ) ;
#71604 = DIRECTION ( 'NONE',  ( 1.000000000000000000, 2.952720810173289112E-16, -0.000000000000000000 ) ) ;
#71605 = DIRECTION ( 'NONE',  ( -1.000000000000000000, 0.000000000000000000, 0.000000000000000000 ) ) ;
#71606 = DIRECTION ( 'NONE',  ( 0.000000000000000000, -1.000000000000000000, -0.000000000000000000 ) ) ;
#71607 = CARTESIAN_POINT ( 'NONE',  ( -21.04999999999999716, 6.307425219576570541, -134.0168198683856815 ) ) ;
#71608 = CARTESIAN_POINT ( 'NONE',  ( -20.94999999999999929, -12.41227409413852811, -164.5000000000000000 ) ) ;
#71609 = ORIENTED_EDGE ( 'NONE', *, *, #42460, .T. ) ;
#71611 = FACE_OUTER_BOUND ( 'NONE', #180376, .T. ) ;
#71610 = FACE_OUTER_BOUND ( 'NONE', #139794, .T. ) ;
#71612 = ORIENTED_EDGE ( 'NONE', *, *, #149677, .F. ) ;
#71615 = EDGE_LOOP ( 'NONE', ( #28298, #227045, #250911, #48987, #112882, #207904, #74338, #89133, #213347, #31482, #176139, #92330, #24481, #253463, #71209, #44068 ) ) ;
#71614 = CARTESIAN_POINT ( 'NONE',  ( -16.87683809663752399, 51.08261412647723887, -232.2799364306433461 ) ) ;
#71613 = DIRECTION ( 'NONE',  ( 0.000000000000000000, 1.000000000000000000, 0.000000000000000000 ) ) ;
#71616 = FACE_OUTER_BOUND ( 'NONE', #3724, .T. ) ;
#71617 = CARTESIAN_POINT ( 'NONE',  ( -18.50000000000000000, 85.41908450282512888, -96.19319967749882494 ) ) ;
#71618 = ORIENTED_EDGE ( 'NONE', *, *, #250059, .T. ) ;
#71619 = CARTESIAN_POINT ( 'NONE',  ( -21.05000000000000071, 76.25610579210417939, -103.0580039261966050 ) ) ;
#71620 = AXIS2_PLACEMENT_3D ( 'NONE', #236169, #21006, #22277 ) ;
#71621 = CARTESIAN_POINT ( 'NONE',  ( -21.14999999999999858, -0.09999999999999939493, 11.64957080754479968 ) ) ;
#71622 = DIRECTION ( 'NONE',  ( 5.603264701231745086E-32, 7.172728831056619538E-15, -1.000000000000000000 ) ) ;
#71624 = ORIENTED_EDGE ( 'NONE', *, *, #133439, .T. ) ;
#71623 = CARTESIAN_POINT ( 'NONE',  ( -21.05000000000000071, 1.261786168576181755, -75.08649896354552311 ) ) ;
#71625 = B_SPLINE_CURVE_WITH_KNOTS ( 'NONE', 3,
 ( #171604, #33381, #67330, #107739, #170336, #231554, #189849, #206846, #11218, #50314, #32084, #88144, #90731, #249827, #71205, #132442 ),
 .UNSPECIFIED., .F., .F.,
 ( 4, 3, 3, 3, 3, 4 ),
 ( 0.000000000000000000, 2.372700795693552043E-05, 5.739057815867001201E-05, 9.073899019179670509E-05, 0.0001243544287365731219, 0.0001585386695601224125 ),
 .UNSPECIFIED. ) ;
#71626 = AXIS2_PLACEMENT_3D ( 'NONE', #29787, #28513, #49307 ) ;
#71627 = ORIENTED_EDGE ( 'NONE', *, *, #171013, .F. ) ;
#71628 = AXIS2_PLACEMENT_3D ( 'NONE', #221034, #70990, #211765 ) ;
#71629 = LINE ( 'NONE', #69065, #168620 ) ;
#71630 = CARTESIAN_POINT ( 'NONE',  ( -23.15000000000000213, 35.97645343225767789, -235.9694016464868298 ) ) ;
#71632 = EDGE_LOOP ( 'NONE', ( #11773, #52486, #26893, #182306, #119232 ) ) ;
#71631 = AXIS2_PLACEMENT_3D ( 'NONE', #140741, #23398, #238554 ) ;
#71633 = CARTESIAN_POINT ( 'NONE',  ( 18.59999999999999076, 74.16465844978745281, -91.46795619196133487 ) ) ;
#71634 = AXIS2_PLACEMENT_3D ( 'NONE', #91031, #131435, #187589 ) ;
#71635 = DIRECTION ( 'NONE',  ( 0.000000000000000000, -0.9856811345164829818, -0.1686199900910294314 ) ) ;
#71636 = DIRECTION ( 'NONE',  ( -1.000000000000000000, 0.000000000000000000, 0.000000000000000000 ) ) ;
#71637 = EDGE_LOOP ( 'NONE', ( #115351, #83252, #25941, #198606 ) ) ;
#71638 = CARTESIAN_POINT ( 'NONE',  ( 23.14999999999999503, 11.65000000001116298, -93.48519422934610645 ) ) ;
#71639 = TOROIDAL_SURFACE ( 'NONE', #54853, 0.2000000000000000111, 0.1000000000000000056 ) ;
#71640 = CARTESIAN_POINT ( 'NONE',  ( -18.59999999999999787, 64.35000000001150511, -48.27310748452440237 ) ) ;
#71641 = VECTOR ( 'NONE', #13694, 1000.000000000000000 ) ;
#71642 = EDGE_CURVE ( 'NONE', #186173, #183267, #19446, .T. ) ;
#71643 = ORIENTED_EDGE ( 'NONE', *, *, #102474, .T. ) ;
#71644 = CIRCLE ( 'NONE', #50749, 0.1000000000000033223 ) ;
#71645 = CARTESIAN_POINT ( 'NONE',  ( -37.88850191057539973, -10.64999999999999325, 31.50000000000000000 ) ) ;
#71646 = CARTESIAN_POINT ( 'NONE',  ( -18.34374000495060386, 64.52683809664941350, -93.77310748452440237 ) ) ;
#71647 = AXIS2_PLACEMENT_3D ( 'NONE', #153423, #188647, #132533 ) ;
#71648 = ORIENTED_EDGE ( 'NONE', *, *, #106783, .T. ) ;
#71649 = ORIENTED_EDGE ( 'NONE', *, *, #44948, .T. ) ;
#71650 = AXIS2_PLACEMENT_3D ( 'NONE', #208429, #209690, #132735 ) ;
#71651 = DIRECTION ( 'NONE',  ( 0.000000000000000000, -1.000000000000000000, 0.000000000000000000 ) ) ;
#71652 = VERTEX_POINT ( 'NONE', #93113 ) ;
#71654 = ORIENTED_EDGE ( 'NONE', *, *, #86685, .F. ) ;
#71653 = LINE ( 'NONE', #136727, #92828 ) ;
#71655 = TOROIDAL_SURFACE ( 'NONE', #4972, 0.2000000000000000111, 0.1000000000000000056 ) ;
#71656 = ORIENTED_EDGE ( 'NONE', *, *, #167361, .F. ) ;
#71657 = EDGE_CURVE ( 'NONE', #137714, #121616, #148624, .T. ) ;
#71658 = EDGE_CURVE ( 'NONE', #158295, #156870, #227700, .T. ) ;
#71661 = ORIENTED_EDGE ( 'NONE', *, *, #149373, .T. ) ;
#71660 = ORIENTED_EDGE ( 'NONE', *, *, #171973, .F. ) ;
#71659 = LINE ( 'NONE', #151186, #172024 ) ;
#71662 = DIRECTION ( 'NONE',  ( -1.000000000000000000, 7.492892343619937423E-30, -1.073024830501117725E-15 ) ) ;
#71663 = ORIENTED_EDGE ( 'NONE', *, *, #11425, .F. ) ;
#71664 = DIRECTION ( 'NONE',  ( 0.000000000000000000, -6.769652589177795712E-15, 1.000000000000000000 ) ) ;
#71665 = CARTESIAN_POINT ( 'NONE',  ( -1.739115166359751801E-14, 62.49201502323813173, -208.8221019049098857 ) ) ;
#71666 = VECTOR ( 'NONE', #1918, 1000.000000000000000 ) ;
#71667 = CIRCLE ( 'NONE', #59136, 0.09999999999999178990 ) ;
#71668 = AXIS2_PLACEMENT_3D ( 'NONE', #50041, #166178, #27951 ) ;
#71669 = DIRECTION ( 'NONE',  ( 1.000000000000000000, 0.000000000000000000, 0.000000000000000000 ) ) ;
#71671 = CARTESIAN_POINT ( 'NONE',  ( -22.45354308602216165, 25.93539154016570691, -254.3551730728916311 ) ) ;
#71670 = AXIS2_PLACEMENT_3D ( 'NONE', #143259, #37770, #196806 ) ;
#71672 = ORIENTED_EDGE ( 'NONE', *, *, #172597, .T. ) ;
#71673 = ORIENTED_EDGE ( 'NONE', *, *, #254499, .F. ) ;
#71674 = EDGE_LOOP ( 'NONE', ( #112542, #171555, #200699, #168832 ) ) ;
#71675 = ADVANCED_FACE ( 'NONE', ( #91838 ), #33194, .F. ) ;
#71676 = LINE ( 'NONE', #12993, #174898 ) ;
#71679 = ORIENTED_EDGE ( 'NONE', *, *, #223798, .T. ) ;
#71678 = ADVANCED_FACE ( 'NONE', ( #50130 ), #230064, .F. ) ;
#71677 = CARTESIAN_POINT ( 'NONE',  ( -21.05000000000000071, 0.000000000000000000, -7.900000000000000355 ) ) ;
#71680 = CARTESIAN_POINT ( 'NONE',  ( 23.14999999999999503, 2.272311100394802885, -217.9150152700588592 ) ) ;
#71682 = ORIENTED_EDGE ( 'NONE', *, *, #73348, .T. ) ;
#71681 = CARTESIAN_POINT ( 'NONE',  ( 18.42555734704283665, 78.24001024381558977, -231.5466501076114980 ) ) ;
#71683 = EDGE_LOOP ( 'NONE', ( #78241, #27992, #80291, #89584 ) ) ;
#71684 = DIRECTION ( 'NONE',  ( -6.938893903907222856E-15, -1.000000000000000000, -6.982962677686266711E-15 ) ) ;
#71685 = EDGE_CURVE ( 'NONE', #162952, #151569, #250896, .T. ) ;
#71686 = VERTEX_POINT ( 'NONE', #188368 ) ;
#71687 = ADVANCED_FACE ( 'NONE', ( #147962 ), #110110, .T. ) ;
#71688 = CARTESIAN_POINT ( 'NONE',  ( 21.15000000000005542, 87.50449464844290048, -34.18759587077607165 ) ) ;
#71689 = DIRECTION ( 'NONE',  ( 1.000000000000000000, -0.000000000000000000, 0.000000000000000000 ) ) ;
#71690 = AXIS2_PLACEMENT_3D ( 'NONE', #39041, #182398, #41615 ) ;
#71692 = EDGE_LOOP ( 'NONE', ( #216607, #237355, #81471, #28460 ) ) ;
#71691 = VERTEX_POINT ( 'NONE', #211796 ) ;
#71693 = EDGE_LOOP ( 'NONE', ( #226607, #34630, #202256 ) ) ;
#71694 = DIRECTION ( 'NONE',  ( -0.000000000000000000, -1.000000000000000000, -0.000000000000000000 ) ) ;
#71696 = ORIENTED_EDGE ( 'NONE', *, *, #99475, .F. ) ;
#71695 = EDGE_CURVE ( 'NONE', #230675, #242544, #108820, .T. ) ;
#71697 = ORIENTED_EDGE ( 'NONE', *, *, #128426, .F. ) ;
#71699 = ORIENTED_EDGE ( 'NONE', *, *, #141792, .T. ) ;
#71698 = CARTESIAN_POINT ( 'NONE',  ( 20.94999999999999929, 36.65892442174935439, -249.5511627012433848 ) ) ;
#71700 = CARTESIAN_POINT ( 'NONE',  ( -19.99999999999999645, 1.249999999999999334, 21.90000000000000213 ) ) ;
#71702 = CARTESIAN_POINT ( 'NONE',  ( -20.85000000000000142, 11.65000000001115232, -200.9999999999999432 ) ) ;
#71701 = DIRECTION ( 'NONE',  ( -7.304098846218134667E-16, 1.000000000000000000, 6.982962677686267499E-15 ) ) ;
#71703 = DIRECTION ( 'NONE',  ( 1.000000000000000000, 0.000000000000000000, 0.000000000000000000 ) ) ;
#71704 = DIRECTION ( 'NONE',  ( 1.000000000000000000, -0.000000000000000000, -0.000000000000000000 ) ) ;
#71705 = ORIENTED_EDGE ( 'NONE', *, *, #4415, .F. ) ;
#71707 = ADVANCED_FACE ( 'NONE', ( #168851 ), #173797, .F. ) ;
#71706 = VERTEX_POINT ( 'NONE', #227481 ) ;
#71708 = CARTESIAN_POINT ( 'NONE',  ( 18.41832399655378083, 85.68240326668595230, -96.36626386449687232 ) ) ;
#71709 = DIRECTION ( 'NONE',  ( -1.000000000000000000, 0.000000000000000000, 0.000000000000000000 ) ) ;
#71710 = PLANE ( 'NONE',  #178551 ) ;
#71711 = EDGE_LOOP ( 'NONE', ( #3388, #96024, #74150, #161170 ) ) ;
#71712 = AXIS2_PLACEMENT_3D ( 'NONE', #70544, #229594, #210040 ) ;
#71713 = CARTESIAN_POINT ( 'NONE',  ( 21.05000000000000071, 0.09779029131994770863, -161.2421853895238542 ) ) ;
#71714 = DIRECTION ( 'NONE',  ( -0.000000000000000000, -6.982962677686266711E-15, 1.000000000000000000 ) ) ;
#71715 = ORIENTED_EDGE ( 'NONE', *, *, #160734, .T. ) ;
#71716 = ORIENTED_EDGE ( 'NONE', *, *, #184909, .F. ) ;
#71717 = DIRECTION ( 'NONE',  ( 1.000000000000000000, 0.000000000000000000, 0.000000000000000000 ) ) ;
#71718 = DIRECTION ( 'NONE',  ( -1.000000000000000000, 0.000000000000000000, 0.000000000000000000 ) ) ;
#71719 = ORIENTED_EDGE ( 'NONE', *, *, #44960, .T. ) ;
#71720 = DIRECTION ( 'NONE',  ( -1.000000000000000000, 7.304098846218163263E-16, -4.217023435051627211E-16 ) ) ;
#71721 = ORIENTED_EDGE ( 'NONE', *, *, #254431, .F. ) ;
#71722 = CARTESIAN_POINT ( 'NONE',  ( 18.47135592147663274, -9.471088613254405431, -140.6835949398439993 ) ) ;
#71723 = DIRECTION ( 'NONE',  ( 0.000000000000000000, -6.938893903907222067E-15, 1.000000000000000000 ) ) ;
#71725 = CARTESIAN_POINT ( 'NONE',  ( -21.05000000000000782, -1.244299762474067705, -194.8241018385128314 ) ) ;
#71724 = LINE ( 'NONE', #151260, #86367 ) ;
#71726 = CARTESIAN_POINT ( 'NONE',  ( -18.59999999999999787, 77.16270174995010223, -128.4231074845242802 ) ) ;
#71727 = DIRECTION ( 'NONE',  ( -0.000000000000000000, -1.000000000000000000, 0.000000000000000000 ) ) ;
#71728 = CYLINDRICAL_SURFACE ( 'NONE', #128121, 0.09999999999999939493 ) ;
#71729 = CARTESIAN_POINT ( 'NONE',  ( -20.54999999999999716, 74.00000000001254818, -183.2477294072864709 ) ) ;
#71730 = AXIS2_PLACEMENT_3D ( 'NONE', #83293, #162888, #80733 ) ;
#71732 = EDGE_LOOP ( 'NONE', ( #7562, #184806, #208867, #178696 ) ) ;
#71731 = DIRECTION ( 'NONE',  ( 0.000000000000000000, 8.673617379883787770E-15, -1.000000000000000000 ) ) ;
#71733 = VECTOR ( 'NONE', #252084, 1000.000000000000000 ) ;
#71734 = EDGE_CURVE ( 'NONE', #81173, #217285, #247041, .T. ) ;
#71736 = VERTEX_POINT ( 'NONE', #128397 ) ;
#71735 = ORIENTED_EDGE ( 'NONE', *, *, #98158, .F. ) ;
#71737 = ORIENTED_EDGE ( 'NONE', *, *, #204115, .F. ) ;
#71738 = EDGE_CURVE ( 'NONE', #142512, #87114, #19628, .T. ) ;
#71739 = CARTESIAN_POINT ( 'NONE',  ( 22.49066049874202022, 0.05634325153222827925, 11.65001223751710313 ) ) ;
#71740 = CARTESIAN_POINT ( 'NONE',  ( -20.00857864376270001, 63.74333919030581086, -212.9951329171253747 ) ) ;
#71741 = ADVANCED_FACE ( 'NONE', ( #150536 ), #95678, .F. ) ;
#71742 = ADVANCED_FACE ( 'NONE', ( #74880 ), #66189, .T. ) ;
#71744 = CARTESIAN_POINT ( 'NONE',  ( -23.25000000000000000, 76.00000000001267608, -203.5231074845243597 ) ) ;
#71743 = LINE ( 'NONE', #109549, #161979 ) ;
#71745 = DIRECTION ( 'NONE',  ( -0.000000000000000000, 0.000000000000000000, 1.000000000000000000 ) ) ;
#71746 = ORIENTED_EDGE ( 'NONE', *, *, #19680, .F. ) ;
#71747 = CARTESIAN_POINT ( 'NONE',  ( 22.00411653962175862, 68.74655713164172255, -69.62214559032500460 ) ) ;
#71748 = ORIENTED_EDGE ( 'NONE', *, *, #136889, .T. ) ;
#71749 = ORIENTED_EDGE ( 'NONE', *, *, #179705, .F. ) ;
#71750 = CARTESIAN_POINT ( 'NONE',  ( -21.05000000000000071, 0.05132743234157015333, 6.300183336267757284 ) ) ;
#71752 = VECTOR ( 'NONE', #115595, 1000.000000000000000 ) ;
#71751 = CARTESIAN_POINT ( 'NONE',  ( -18.59999999999999787, 64.25000000001233502, -163.0083017138704236 ) ) ;
#71753 = ADVANCED_FACE ( 'NONE', ( #77392 ), #186219, .T. ) ;
#71754 = CIRCLE ( 'NONE', #217445, 0.09999999999998898659 ) ;
#71755 = LINE ( 'NONE', #30070, #212371 ) ;
#71756 = VERTEX_POINT ( 'NONE', #237769 ) ;
#71757 = EDGE_CURVE ( 'NONE', #74028, #64043, #127959, .T. ) ;
#71758 = EDGE_CURVE ( 'NONE', #2383, #217847, #152928, .T. ) ;
#71759 = FACE_OUTER_BOUND ( 'NONE', #102750, .T. ) ;
#71760 = ORIENTED_EDGE ( 'NONE', *, *, #200757, .T. ) ;
#71761 = ORIENTED_EDGE ( 'NONE', *, *, #160406, .F. ) ;
#71762 = DIRECTION ( 'NONE',  ( -0.000000000000000000, -0.000000000000000000, 1.000000000000000000 ) ) ;
#71763 = CARTESIAN_POINT ( 'NONE',  ( -16.85718274719427967, 9.976142314632875596, -54.43665366781746684 ) ) ;
#71764 = EDGE_CURVE ( 'NONE', #65641, #117652, #133532, .T. ) ;
#71766 = CARTESIAN_POINT ( 'NONE',  ( -21.05000000000000071, -1.162701749926853712, -175.5999999999999659 ) ) ;
#71765 = B_SPLINE_CURVE_WITH_KNOTS ( 'NONE', 3,
 ( #185029, #83328, #162925, #5075, #84597, #243722, #65079, #245002, #224146, #6389 ),
 .UNSPECIFIED., .F., .F.,
 ( 4, 2, 2, 2, 4 ),
 ( 0.000000000000000000, 3.990160268013353780E-05, 7.980320536026707561E-05, 0.0001596064107205310341, 0.0003192128214410546957 ),
 .UNSPECIFIED. ) ;
#71767 = DIRECTION ( 'NONE',  ( 1.000000000000000000, 0.000000000000000000, 0.000000000000000000 ) ) ;
#71768 = CYLINDRICAL_SURFACE ( 'NONE', #85920, 0.09999999999999939493 ) ;
#71769 = DIRECTION ( 'NONE',  ( 0.000000000000000000, -7.189901751995769991E-15, 1.000000000000000000 ) ) ;
#71770 = ORIENTED_EDGE ( 'NONE', *, *, #61184, .T. ) ;
#71771 = CARTESIAN_POINT ( 'NONE',  ( -20.54999999999999716, -9.399999999988848387, -177.3939691226524076 ) ) ;
#71772 = DIRECTION ( 'NONE',  ( 0.000000000000000000, -0.8814952561688430555, 0.4721928772777346239 ) ) ;
#71773 = EDGE_CURVE ( 'NONE', #130997, #157258, #236479, .T. ) ;
#71776 = CARTESIAN_POINT ( 'NONE',  ( 23.04999999999999716, 67.17743825834568838, -127.2731074845243597 ) ) ;
#71775 = VECTOR ( 'NONE', #24776, 1000.000000000000000 ) ;
#71774 = FACE_OUTER_BOUND ( 'NONE', #120124, .T. ) ;
#71778 = FACE_OUTER_BOUND ( 'NONE', #137731, .T. ) ;
#71777 = VECTOR ( 'NONE', #158147, 1000.000000000000000 ) ;
#71779 = VECTOR ( 'NONE', #96796, 1000.000000000000000 ) ;
#71780 = DIRECTION ( 'NONE',  ( -2.252264143451594314E-15, 0.1298341882520054891, 0.9915357197604850459 ) ) ;
#71781 = DIRECTION ( 'NONE',  ( -1.000000000000000000, 0.000000000000000000, 0.000000000000000000 ) ) ;
#71782 = DIRECTION ( 'NONE',  ( -0.000000000000000000, 1.000000000000000000, 6.982962677686266711E-15 ) ) ;
#71783 = EDGE_CURVE ( 'NONE', #97122, #233908, #202952, .T. ) ;
#71784 = EDGE_CURVE ( 'NONE', #140921, #104099, #98680, .T. ) ;
#71786 = ORIENTED_EDGE ( 'NONE', *, *, #106408, .F. ) ;
#71785 = CARTESIAN_POINT ( 'NONE',  ( 19.75857864376268935, 54.48300931968434213, -228.8005724072070564 ) ) ;
#71787 = ADVANCED_FACE ( 'NONE', ( #213061 ), #69701, .T. ) ;
#71788 = DIRECTION ( 'NONE',  ( 0.000000000000000000, -0.2617529984165036239, -0.9651348961777156399 ) ) ;
#71789 = EDGE_CURVE ( 'NONE', #243260, #194615, #82127, .T. ) ;
#71790 = EDGE_CURVE ( 'NONE', #8771, #12190, #82513, .T. ) ;
#71791 = CYLINDRICAL_SURFACE ( 'NONE', #11633, 0.09999999999998898659 ) ;
#71792 = CARTESIAN_POINT ( 'NONE',  ( -20.54999999999999716, 38.42191493408704872, -250.4955484557988541 ) ) ;
#71793 = FACE_OUTER_BOUND ( 'NONE', #49162, .T. ) ;
#71794 = CIRCLE ( 'NONE', #221588, 0.09999999999998898659 ) ;
#71795 = CARTESIAN_POINT ( 'NONE',  ( 23.14999999999999858, 76.00000000001170974, -69.52310748452431710 ) ) ;
#71796 = DIRECTION ( 'NONE',  ( 0.000000000000000000, 0.000000000000000000, -1.000000000000000000 ) ) ;
#71797 = DIRECTION ( 'NONE',  ( 1.000000000000000000, -7.304098846218134667E-16, 0.000000000000000000 ) ) ;
#71798 = EDGE_LOOP ( 'NONE', ( #149770, #203282, #199894, #187733 ) ) ;
#71799 = DIRECTION ( 'NONE',  ( 1.000000000000000000, 0.000000000000000000, 0.000000000000000000 ) ) ;
#71800 = ORIENTED_EDGE ( 'NONE', *, *, #134276, .T. ) ;
#71801 = DIRECTION ( 'NONE',  ( 0.000000000000000000, -1.000000000000000000, -6.982962677686266711E-15 ) ) ;
#71802 = CIRCLE ( 'NONE', #55002, 0.1000000000000066530 ) ;
#71803 = CYLINDRICAL_SURFACE ( 'NONE', #121195, 11.80000000000000426 ) ;
#71804 = EDGE_LOOP ( 'NONE', ( #145429, #207875, #256911, #173690 ) ) ;
#71805 = DIRECTION ( 'NONE',  ( 0.000000000000000000, -1.000000000000000000, -0.000000000000000000 ) ) ;
#71806 = CIRCLE ( 'NONE', #109177, 0.09999999999999939493 ) ;
#71807 = PRODUCT_CONTEXT ( 'NONE', #195588, 'mechanical' ) ;
#71808 = CARTESIAN_POINT ( 'NONE',  ( -21.05000000000000071, 69.66772772607649244, -136.4855714212387170 ) ) ;
#71809 = LINE ( 'NONE', #50912, #23362 ) ;
#71811 = AXIS2_PLACEMENT_3D ( 'NONE', #53636, #94031, #250540 ) ;
#71810 = CARTESIAN_POINT ( 'NONE',  ( -21.05000000000000071, 87.65000000001163016, -66.52310748452423184 ) ) ;
#71812 = ORIENTED_EDGE ( 'NONE', *, *, #168388, .F. ) ;
#71813 = AXIS2_PLACEMENT_3D ( 'NONE', #190645, #195785, #254419 ) ;
#71814 = CARTESIAN_POINT ( 'NONE',  ( 23.24999999999999645, 8.822561741677553471, -188.3499999999999659 ) ) ;
#71815 = CIRCLE ( 'NONE', #134134, 0.1000000000000028644 ) ;
#71816 = VECTOR ( 'NONE', #115835, 1000.000000000000000 ) ;
#71817 = CARTESIAN_POINT ( 'NONE',  ( -18.40000000000000213, 5.650000000011139001, -180.1499999999999773 ) ) ;
#71818 = ORIENTED_EDGE ( 'NONE', *, *, #249901, .T. ) ;
#71819 = ORIENTED_EDGE ( 'NONE', *, *, #209243, .T. ) ;
#71821 = AXIS2_PLACEMENT_3D ( 'NONE', #26868, #106349, #4685 ) ;
#71820 = DIRECTION ( 'NONE',  ( -1.000000000000000000, -0.000000000000000000, -0.000000000000000000 ) ) ;
#71822 = CARTESIAN_POINT ( 'NONE',  ( -20.54999999999999716, 76.00000000001126921, -203.5231074845248997 ) ) ;
#71823 = DIRECTION ( 'NONE',  ( 0.000000000000000000, -6.530723674265620862E-15, 1.000000000000000000 ) ) ;
#71824 = EDGE_CURVE ( 'NONE', #161922, #99797, #32107, .T. ) ;
#71825 = DIRECTION ( 'NONE',  ( 1.000000000000000000, -0.000000000000000000, -0.000000000000000000 ) ) ;
#71827 = CARTESIAN_POINT ( 'NONE',  ( -18.40000000000000213, 64.52683809665026615, -145.8229367329901436 ) ) ;
#71826 = LINE ( 'NONE', #230906, #257536 ) ;
#71828 = AXIS2_PLACEMENT_3D ( 'NONE', #73846, #153395, #232913 ) ;
#71829 = VECTOR ( 'NONE', #215058, 1000.000000000000000 ) ;
#71830 = CARTESIAN_POINT ( 'NONE',  ( -21.08376601933334271, 75.93622398908254922, -176.3650547558000881 ) ) ;
#71831 = EDGE_CURVE ( 'NONE', #257097, #232829, #215430, .T. ) ;
#71832 = LINE ( 'NONE', #86209, #14529 ) ;
#71834 = DIRECTION ( 'NONE',  ( -1.000000000000000000, -2.952720810173289112E-16, 0.000000000000000000 ) ) ;
#71833 = AXIS2_PLACEMENT_3D ( 'NONE', #118593, #64684, #177296 ) ;
#71835 = VERTEX_POINT ( 'NONE', #180371 ) ;
#71837 = EDGE_LOOP ( 'NONE', ( #117808, #235938, #198686, #84985 ) ) ;
#71836 = FACE_OUTER_BOUND ( 'NONE', #61281, .T. ) ;
#71838 = CARTESIAN_POINT ( 'NONE',  ( 21.08884785362045378, 69.64280663258713844, -170.0728905795912453 ) ) ;
#71839 = AXIS2_PLACEMENT_3D ( 'NONE', #242874, #65512, #223295 ) ;
#71840 = CARTESIAN_POINT ( 'NONE',  ( -21.14999999999999858, -1.391858308744747807, -194.6091531227727955 ) ) ;
#71842 = FACE_OUTER_BOUND ( 'NONE', #54110, .T. ) ;
#71841 = CARTESIAN_POINT ( 'NONE',  ( -21.05000000000000071, 5.265981236333565222E-16, 4.299999999999956302 ) ) ;
#71843 = VECTOR ( 'NONE', #256134, 1000.000000000000000 ) ;
#71844 = ADVANCED_FACE ( 'NONE', ( #205035 ), #42154, .F. ) ;
#71845 = EDGE_CURVE ( 'NONE', #43634, #204747, #207066, .T. ) ;
#71846 = ORIENTED_EDGE ( 'NONE', *, *, #236942, .F. ) ;
#71847 = DIRECTION ( 'NONE',  ( 0.000000000000000000, 0.000000000000000000, 1.000000000000000000 ) ) ;
#71848 = CARTESIAN_POINT ( 'NONE',  ( -16.97683809663752186, 66.05000000001264482, -194.2731074845244166 ) ) ;
#71849 = CARTESIAN_POINT ( 'NONE',  ( -21.05000000000000071, 87.48912529308798014, -100.0231074845242318 ) ) ;
#71851 = DIRECTION ( 'NONE',  ( -1.000000000000000000, 0.000000000000000000, 0.000000000000000000 ) ) ;
#71850 = AXIS2_PLACEMENT_3D ( 'NONE', #7210, #107607, #148029 ) ;
#71852 = ORIENTED_EDGE ( 'NONE', *, *, #211752, .F. ) ;
#71853 = VERTEX_POINT ( 'NONE', #60404 ) ;
#71854 = CARTESIAN_POINT ( 'NONE',  ( -23.25000000000000000, 68.97833521811203639, -132.6895420826271277 ) ) ;
#71855 = EDGE_LOOP ( 'NONE', ( #36950, #41885, #247020, #222584 ) ) ;
#71856 = CARTESIAN_POINT ( 'NONE',  ( 21.05000000000000071, 76.00000000001170974, -69.52310748452431710 ) ) ;
#71857 = CIRCLE ( 'NONE', #26063, 0.1000000000000060701 ) ;
#71858 = DIRECTION ( 'NONE',  ( 0.000000000000000000, 0.000000000000000000, 1.000000000000000000 ) ) ;
#71859 = AXIS2_PLACEMENT_3D ( 'NONE', #179537, #19154, #2145 ) ;
#71860 = ADVANCED_FACE ( 'NONE', ( #241620 ), #26439, .F. ) ;
#71861 = DIRECTION ( 'NONE',  ( 0.000000000000000000, 0.6728388485993177515, -0.7397890806274072251 ) ) ;
#71862 = EDGE_LOOP ( 'NONE', ( #188718, #131825, #50612, #126405 ) ) ;
#71863 = CARTESIAN_POINT ( 'NONE',  ( -18.59999999999999787, 76.00000000001126921, -203.5231074845248997 ) ) ;
#71864 = LINE ( 'NONE', #92682, #170327 ) ;
#71865 = FACE_OUTER_BOUND ( 'NONE', #210375, .T. ) ;
#71866 = CARTESIAN_POINT ( 'NONE',  ( -23.25000000000000000, 73.40000000001185754, -89.79848556176223440 ) ) ;
#71867 = ADVANCED_FACE ( 'NONE', ( #104638 ), #123865, .T. ) ;
#71868 = FACE_OUTER_BOUND ( 'NONE', #192285, .T. ) ;
#71869 = LINE ( 'NONE', #151409, #144782 ) ;
#71871 = ORIENTED_EDGE ( 'NONE', *, *, #92766, .F. ) ;
#71870 = ADVANCED_FACE ( 'NONE', ( #199947 ), #123680, .F. ) ;
#71872 = VECTOR ( 'NONE', #223714, 1000.000000000000000 ) ;
#71874 = DIRECTION ( 'NONE',  ( 0.000000000000000000, 1.000000000000000000, 0.000000000000000000 ) ) ;
#71873 = FACE_OUTER_BOUND ( 'NONE', #77838, .T. ) ;
#71875 = VERTEX_POINT ( 'NONE', #143792 ) ;
#71877 = ORIENTED_EDGE ( 'NONE', *, *, #219815, .T. ) ;
#71876 = LINE ( 'NONE', #73175, #252401 ) ;
#71878 = ORIENTED_EDGE ( 'NONE', *, *, #45512, .T. ) ;
#71879 = CARTESIAN_POINT ( 'NONE',  ( 20.95000000000005258, 64.35000000001119247, -5.923107484524795296 ) ) ;
#71880 = CARTESIAN_POINT ( 'NONE',  ( 18.56308993302888055, 65.61930884468753788, -78.28388484558554694 ) ) ;
#71881 = FACE_OUTER_BOUND ( 'NONE', #97232, .T. ) ;
#71882 = VECTOR ( 'NONE', #190511, 1000.000000000000000 ) ;
#71883 = VERTEX_POINT ( 'NONE', #162106 ) ;
#71884 = FACE_OUTER_BOUND ( 'NONE', #93610, .T. ) ;
#71885 = B_SPLINE_CURVE_WITH_KNOTS ( 'NONE', 3,
 ( #167252, #206357, #208910, #70716, #111095, #171120, #245486, #195794, #34165, #15879 ),
 .UNSPECIFIED., .F., .F.,
 ( 4, 2, 2, 2, 4 ),
 ( 0.000000000000000000, 0.0001584437871624896237, 0.0002376656807437438411, 0.0002772766275343796776, 0.0003168875743250154598 ),
 .UNSPECIFIED. ) ;
#71886 = CARTESIAN_POINT ( 'NONE',  ( 18.49999999999999289, 10.44006789215405639, -158.7671177488814465 ) ) ;
#71887 = EDGE_CURVE ( 'NONE', #86347, #131422, #21320, .T. ) ;
#71888 = VERTEX_POINT ( 'NONE', #184200 ) ;
#71889 = EDGE_CURVE ( 'NONE', #82836, #91161, #194618, .T. ) ;
#71890 = DIRECTION ( 'NONE',  ( 1.000000000000000000, 0.000000000000000000, 0.000000000000000000 ) ) ;
#71891 = CARTESIAN_POINT ( 'NONE',  ( 18.59999999999999076, 7.128833340094563376, -233.7327013124401276 ) ) ;
#71892 = EDGE_CURVE ( 'NONE', #54287, #7235, #242899, .T. ) ;
#71893 = ORIENTED_EDGE ( 'NONE', *, *, #134753, .T. ) ;
#71894 = DIRECTION ( 'NONE',  ( 1.000000000000000000, 0.000000000000000000, 0.000000000000000000 ) ) ;
#71895 = VECTOR ( 'NONE', #57994, 1000.000000000000000 ) ;
#71896 = EDGE_LOOP ( 'NONE', ( #92362, #32079, #170504, #80104 ) ) ;
#71897 = CARTESIAN_POINT ( 'NONE',  ( 18.49999999999999289, 65.70729864261004138, -97.56574559737244101 ) ) ;
#71898 = ORIENTED_EDGE ( 'NONE', *, *, #93179, .T. ) ;
#71899 = DIRECTION ( 'NONE',  ( -2.952720810173289112E-16, 1.000000000000000000, -0.000000000000000000 ) ) ;
#71900 = DIRECTION ( 'NONE',  ( 0.000000000000000000, 0.000000000000000000, 1.000000000000000000 ) ) ;
#71901 = CARTESIAN_POINT ( 'NONE',  ( 18.49999999999999289, 6.649999999999999467, -21.35000000000000142 ) ) ;
#71902 = ADVANCED_FACE ( 'NONE', ( #103370 ), #182949, .F. ) ;
#71903 = DIRECTION ( 'NONE',  ( 1.000000000000000000, 0.000000000000000000, 0.000000000000000000 ) ) ;
#71904 = EDGE_CURVE ( 'NONE', #14880, #252820, #11443, .T. ) ;
#71906 = CIRCLE ( 'NONE', #113409, 0.09999999999999939493 ) ;
#71905 = CARTESIAN_POINT ( 'NONE',  ( -22.42357213249529124, 0.09908696401271366305, -25.82706761364006454 ) ) ;
#71907 = CARTESIAN_POINT ( 'NONE',  ( 18.59999999999999432, -1.835859311432484375, -212.5044391687984842 ) ) ;
#71908 = DIRECTION ( 'NONE',  ( -1.000000000000000000, 0.000000000000000000, 0.000000000000000000 ) ) ;
#71909 = ORIENTED_EDGE ( 'NONE', *, *, #87523, .T. ) ;
#71910 = DIRECTION ( 'NONE',  ( 1.000000000000000000, 0.000000000000000000, 0.000000000000000000 ) ) ;
#71912 = VERTEX_POINT ( 'NONE', #125525 ) ;
#71911 = AXIS2_PLACEMENT_3D ( 'NONE', #86263, #82407, #2884 ) ;
#71914 = DIRECTION ( 'NONE',  ( 0.000000000000000000, -0.000000000000000000, -1.000000000000000000 ) ) ;
#71913 = CARTESIAN_POINT ( 'NONE',  ( 22.39999999999999858, 68.20922040163857503, -103.1231074845243540 ) ) ;
#71915 = VERTEX_POINT ( 'NONE', #105935 ) ;
#71916 = CARTESIAN_POINT ( 'NONE',  ( -20.94999999999999929, 76.00000000001142553, -36.02310748452432421 ) ) ;
#71917 = DIRECTION ( 'NONE',  ( 1.000000000000000000, 0.000000000000000000, 0.000000000000000000 ) ) ;
#71919 = CARTESIAN_POINT ( 'NONE',  ( -23.25000000000000000, 76.00000000001244871, -170.0231074845243597 ) ) ;
#71918 = AXIS2_PLACEMENT_3D ( 'NONE', #186234, #6289, #25885 ) ;
#71920 = DIRECTION ( 'NONE',  ( -0.000000000000000000, 0.000000000000000000, 1.000000000000000000 ) ) ;
#71921 = ORIENTED_EDGE ( 'NONE', *, *, #143997, .T. ) ;
#71923 = ORIENTED_EDGE ( 'NONE', *, *, #47240, .T. ) ;
#71922 = LINE ( 'NONE', #156621, #67916 ) ;
#71925 = CARTESIAN_POINT ( 'NONE',  ( -18.59999999999999787, -1.687074390091559906, 12.81457296654165212 ) ) ;
#71924 = CARTESIAN_POINT ( 'NONE',  ( 21.14999999999999858, -1.391858308744748696, -194.6091531227727955 ) ) ;
#71927 = VERTEX_POINT ( 'NONE', #79939 ) ;
#71926 = DIRECTION ( 'NONE',  ( 1.000000000000000000, 0.000000000000000000, 0.000000000000000000 ) ) ;
#71928 = TOROIDAL_SURFACE ( 'NONE', #101066, 11.65000000000000036, 0.1000000000000000056 ) ;
#71929 = CIRCLE ( 'NONE', #105172, 0.1999999999999987899 ) ;
#71930 = ORIENTED_EDGE ( 'NONE', *, *, #77455, .T. ) ;
#71931 = CARTESIAN_POINT ( 'NONE',  ( 21.05000000000000071, 71.00000000001151079, -47.92837350343745584 ) ) ;
#71932 = CARTESIAN_POINT ( 'NONE',  ( 21.05000000000000071, 67.22371735104076151, -94.53551510600442498 ) ) ;
#71933 = VERTEX_POINT ( 'NONE', #159531 ) ;
#71934 = FACE_OUTER_BOUND ( 'NONE', #86813, .T. ) ;
#71935 = ORIENTED_EDGE ( 'NONE', *, *, #33729, .T. ) ;
#71936 = AXIS2_PLACEMENT_3D ( 'NONE', #99124, #18325, #39202 ) ;
#71937 = CARTESIAN_POINT ( 'NONE',  ( -18.39999999999999858, -9.499999999988849808, -107.1001893912220879 ) ) ;
#71938 = CARTESIAN_POINT ( 'NONE',  ( 20.12499999999999645, 18.89374182079812314, -228.4160025464828152 ) ) ;
#71939 = ORIENTED_EDGE ( 'NONE', *, *, #152785, .F. ) ;
#71940 = DIRECTION ( 'NONE',  ( 0.000000000000000000, -1.000000000000000000, -0.000000000000000000 ) ) ;
#71941 = AXIS2_PLACEMENT_3D ( 'NONE', #96016, #158600, #218518 ) ;
#71942 = VECTOR ( 'NONE', #143658, 1000.000000000000000 ) ;
#71943 = VECTOR ( 'NONE', #187490, 1000.000000000000000 ) ;
#71944 = EDGE_CURVE ( 'NONE', #115688, #41243, #177851, .T. ) ;
#71945 = ORIENTED_EDGE ( 'NONE', *, *, #151220, .T. ) ;
#71946 = DIRECTION ( 'NONE',  ( 0.000000000000000000, 0.000000000000000000, -1.000000000000000000 ) ) ;
#71947 = ORIENTED_EDGE ( 'NONE', *, *, #215185, .F. ) ;
#71948 = ORIENTED_EDGE ( 'NONE', *, *, #4404, .F. ) ;
#71949 = CARTESIAN_POINT ( 'NONE',  ( 20.77766267348356166, 18.75573362213343387, -228.1071430829227324 ) ) ;
#71950 = ORIENTED_EDGE ( 'NONE', *, *, #215419, .T. ) ;
#71951 = DIRECTION ( 'NONE',  ( -1.000000000000000000, -0.000000000000000000, 0.000000000000000000 ) ) ;
#71953 = EDGE_CURVE ( 'NONE', #69371, #68201, #36389, .T. ) ;
#71952 = EDGE_LOOP ( 'NONE', ( #158001, #102993, #227804, #79500 ) ) ;
#71955 = ORIENTED_EDGE ( 'NONE', *, *, #135745, .F. ) ;
#71954 = LINE ( 'NONE', #151508, #18223 ) ;
#71956 = ORIENTED_EDGE ( 'NONE', *, *, #145568, .T. ) ;
#71957 = ADVANCED_FACE ( 'NONE', ( #146353 ), #157006, .T. ) ;
#71958 = DIRECTION ( 'NONE',  ( 0.000000000000000000, -1.000000000000000000, 0.000000000000000000 ) ) ;
#71959 = ADVANCED_FACE ( 'NONE', ( #231069 ), #107099, .T. ) ;
#71960 = ORIENTED_EDGE ( 'NONE', *, *, #169563, .F. ) ;
#71963 = VERTEX_POINT ( 'NONE', #32889 ) ;
#71962 = ORIENTED_EDGE ( 'NONE', *, *, #203732, .F. ) ;
#71961 = CARTESIAN_POINT ( 'NONE',  ( 20.94999999999999929, 87.48912529308749697, -39.12310748452424747 ) ) ;
#71965 = DIRECTION ( 'NONE',  ( -0.000000000000000000, 1.000000000000000000, 6.982962677686266711E-15 ) ) ;
#71964 = CIRCLE ( 'NONE', #92787, 11.74999999999999645 ) ;
#71966 = EDGE_LOOP ( 'NONE', ( #85606, #44228, #248628 ) ) ;
#71967 = AXIS2_PLACEMENT_3D ( 'NONE', #131666, #172124, #114675 ) ;
#71968 = CARTESIAN_POINT ( 'NONE',  ( 20.94999999999999929, 69.35000000001228670, -157.8731074845244109 ) ) ;
#71969 = ORIENTED_EDGE ( 'NONE', *, *, #62322, .T. ) ;
#71970 = ADVANCED_FACE ( 'NONE', ( #148960 ), #227185, .T. ) ;
#71971 = CARTESIAN_POINT ( 'NONE',  ( -14.00000000000000178, 47.91805600923872532, -233.7139610577891631 ) ) ;
#71972 = AXIS2_PLACEMENT_3D ( 'NONE', #4307, #102108, #162135 ) ;
#71974 = EDGE_LOOP ( 'NONE', ( #251773, #105357, #107370, #229864 ) ) ;
#71973 = CYLINDRICAL_SURFACE ( 'NONE', #153585, 0.09999999999999939493 ) ;
#71975 = CARTESIAN_POINT ( 'NONE',  ( -20.54999999999999716, 26.13474583767463244, -241.1910018098189141 ) ) ;
#71976 = EDGE_LOOP ( 'NONE', ( #59073, #2635, #241097, #40754 ) ) ;
#71977 = CARTESIAN_POINT ( 'NONE',  ( 20.95512820512820085, 65.37615131630002452, -95.35819391543677170 ) ) ;
#71978 = AXIS2_PLACEMENT_3D ( 'NONE', #217346, #161261, #221201 ) ;
#71979 = EDGE_LOOP ( 'NONE', ( #76953, #126470, #140526, #144481 ) ) ;
#71980 = DIRECTION ( 'NONE',  ( 0.000000000000000000, 0.5000000000000078826, -0.8660254037844340447 ) ) ;
#71981 = CARTESIAN_POINT ( 'NONE',  ( 20.46382478191414833, 67.09862044130898084, -60.97737938964129967 ) ) ;
#71982 = CIRCLE ( 'NONE', #125940, 0.09999999999998898659 ) ;
#71983 = AXIS2_PLACEMENT_3D ( 'NONE', #55905, #61060, #139299 ) ;
#71985 = ORIENTED_EDGE ( 'NONE', *, *, #137904, .T. ) ;
#71984 = VECTOR ( 'NONE', #28752, 1000.000000000000000 ) ;
#71987 = VERTEX_POINT ( 'NONE', #69421 ) ;
#71986 = CARTESIAN_POINT ( 'NONE',  ( 18.39999999999997371, 64.25000000001210765, -127.2731074845243882 ) ) ;
#71988 = DIRECTION ( 'NONE',  ( 0.000000000000000000, 6.938893903907270030E-14, 1.000000000000000000 ) ) ;
#71989 = AXIS2_PLACEMENT_3D ( 'NONE', #204339, #15149, #94667 ) ;
#71991 = ORIENTED_EDGE ( 'NONE', *, *, #107357, .T. ) ;
#71990 = ORIENTED_EDGE ( 'NONE', *, *, #110712, .F. ) ;
#71992 = ORIENTED_EDGE ( 'NONE', *, *, #141183, .T. ) ;
#71993 = DIRECTION ( 'NONE',  ( 0.000000000000000000, 0.9736512643735623085, 0.2280421351061316382 ) ) ;
#71995 = VERTEX_POINT ( 'NONE', #108528 ) ;
#71994 = ADVANCED_FACE ( 'NONE', ( #190661 ), #136287, .F. ) ;
#71996 = ORIENTED_EDGE ( 'NONE', *, *, #245974, .F. ) ;
#71997 = EDGE_CURVE ( 'NONE', #24454, #208529, #244455, .T. ) ;
#71998 = CARTESIAN_POINT ( 'NONE',  ( 20.94999999999999929, -1.349153571964892606, -74.78749733558989021 ) ) ;
#71999 = VERTEX_POINT ( 'NONE', #229757 ) ;
#72000 = LINE ( 'NONE', #152844, #206471 ) ;
#72001 = CIRCLE ( 'NONE', #105257, 0.09999999999999538425 ) ;
#72002 = LINE ( 'NONE', #133248, #89877 ) ;
#72003 = ORIENTED_EDGE ( 'NONE', *, *, #17983, .T. ) ;
#72005 = EDGE_CURVE ( 'NONE', #97978, #245888, #28017, .T. ) ;
#72004 = ORIENTED_EDGE ( 'NONE', *, *, #13473, .T. ) ;
#72006 = AXIS2_PLACEMENT_3D ( 'NONE', #98509, #178120, #257570 ) ;
#72007 = CARTESIAN_POINT ( 'NONE',  ( 16.87683809663749557, 66.05000000001257376, -182.6731074845244223 ) ) ;
#72008 = ORIENTED_EDGE ( 'NONE', *, *, #190236, .T. ) ;
#72009 = AXIS2_PLACEMENT_3D ( 'NONE', #92471, #255346, #172056 ) ;
#72010 = CIRCLE ( 'NONE', #38686, 0.09999999999999939493 ) ;
#72011 = CIRCLE ( 'NONE', #159495, 0.1000000000000124678 ) ;
#72012 = TOROIDAL_SURFACE ( 'NONE', #155617, 0.2000000000000000111, 0.1000000000000000056 ) ;
#72013 = CARTESIAN_POINT ( 'NONE',  ( 23.14999999999999858, 76.00000000001190870, -103.0231074845243029 ) ) ;
#72014 = ORIENTED_EDGE ( 'NONE', *, *, #121309, .F. ) ;
#72015 = PLANE ( 'NONE',  #187700 ) ;
#72017 = ORIENTED_EDGE ( 'NONE', *, *, #99272, .T. ) ;
#72016 = CARTESIAN_POINT ( 'NONE',  ( 18.59999999999999076, 69.45000000001181206, -81.77310748452434552 ) ) ;
#72018 = DIRECTION ( 'NONE',  ( -1.000000000000000000, -2.952720810173289112E-16, 0.000000000000000000 ) ) ;
#72019 = DIRECTION ( 'NONE',  ( -0.7071067811865302533, 0.6909108974501196876, 0.1504730267679053324 ) ) ;
#72020 = CARTESIAN_POINT ( 'NONE',  ( 20.95203847575071521, 65.49893946073807172, -128.9560361359008027 ) ) ;
#72021 = CARTESIAN_POINT ( 'NONE',  ( -23.15000000000000213, 64.35000000001218723, -143.5379132551784096 ) ) ;
#72022 = DIRECTION ( 'NONE',  ( 1.000000000000000000, 0.000000000000000000, 0.000000000000000000 ) ) ;
#72023 = FACE_OUTER_BOUND ( 'NONE', #186409, .T. ) ;
#72024 = DIRECTION ( 'NONE',  ( 0.000000000000000000, 0.000000000000000000, 1.000000000000000000 ) ) ;
#72025 = LINE ( 'NONE', #191987, #228280 ) ;
#72026 = CARTESIAN_POINT ( 'NONE',  ( 18.48413544395656416, 37.98663424106526065, -261.2259154368716736 ) ) ;
#72027 = DIRECTION ( 'NONE',  ( 0.000000000000000000, 0.1298341882520022972, 0.9915357197604853789 ) ) ;
#72028 = VECTOR ( 'NONE', #191580, 1000.000000000000000 ) ;
#72030 = ORIENTED_EDGE ( 'NONE', *, *, #206876, .F. ) ;
#72029 = AXIS2_PLACEMENT_3D ( 'NONE', #60951, #140481, #187343 ) ;
#72031 = AXIS2_PLACEMENT_3D ( 'NONE', #132908, #110759, #29975 ) ;
#72032 = EDGE_CURVE ( 'NONE', #172976, #222651, #140404, .T. ) ;
#72034 = EDGE_LOOP ( 'NONE', ( #49404, #62528, #168167, #112933 ) ) ;
#72033 = ORIENTED_EDGE ( 'NONE', *, *, #102296, .T. ) ;
#72036 = ORIENTED_EDGE ( 'NONE', *, *, #254524, .F. ) ;
#72035 = EDGE_CURVE ( 'NONE', #122419, #253828, #66838, .T. ) ;
#72037 = DIRECTION ( 'NONE',  ( -1.000000000000000000, 0.000000000000000000, -0.000000000000000000 ) ) ;
#72038 = DIRECTION ( 'NONE',  ( 1.000000000000000000, -7.049440681616512959E-16, 1.911869773728117674E-16 ) ) ;
#72039 = ADVANCED_FACE ( 'NONE', ( #210213 ), #27747, .F. ) ;
#72040 = EDGE_CURVE ( 'NONE', #87677, #29148, #160902, .T. ) ;
#72041 = DIRECTION ( 'NONE',  ( 2.952720810173289112E-16, 1.000000000000000000, 6.530723674265620862E-15 ) ) ;
#72042 = EDGE_LOOP ( 'NONE', ( #65757, #93715, #176719, #189250 ) ) ;
#72043 = ORIENTED_EDGE ( 'NONE', *, *, #206297, .F. ) ;
#72044 =( NAMED_UNIT ( * ) SI_UNIT ( $, .STERADIAN. ) SOLID_ANGLE_UNIT ( ) );
#72045 = CARTESIAN_POINT ( 'NONE',  ( 18.59999999999999787, -9.321008403350148797, -40.73593824907786143 ) ) ;
#72046 = CYLINDRICAL_SURFACE ( 'NONE', #109824, 0.09999999999999982514 ) ;
#72047 = DIRECTION ( 'NONE',  ( -0.000000000000000000, -1.000000000000000000, -0.000000000000000000 ) ) ;
#72048 = AXIS2_PLACEMENT_3D ( 'NONE', #40357, #100260, #19478 ) ;
#72049 = ORIENTED_EDGE ( 'NONE', *, *, #93162, .F. ) ;
#72050 = ORIENTED_EDGE ( 'NONE', *, *, #247429, .F. ) ;
#72051 = EDGE_CURVE ( 'NONE', #111107, #143411, #127576, .T. ) ;
#72052 = CARTESIAN_POINT ( 'NONE',  ( -22.50000000000000000, 0.1000000000111554016, -92.70922040162662370 ) ) ;
#72054 = EDGE_CURVE ( 'NONE', #206496, #88538, #71885, .T. ) ;
#72053 = ADVANCED_FACE ( 'NONE', ( #91539 ), #109798, .T. ) ;
#72055 = DIRECTION ( 'NONE',  ( 1.000000000000000000, -7.304098846218134667E-16, -4.639676173203993355E-30 ) ) ;
#72056 = VECTOR ( 'NONE', #80134, 1000.000000000000000 ) ;
#72057 = LINE ( 'NONE', #151608, #212148 ) ;
#72058 = EDGE_LOOP ( 'NONE', ( #189544, #142035, #29508 ) ) ;
#72059 = EDGE_CURVE ( 'NONE', #112516, #76379, #197032, .T. ) ;
#72060 = DIRECTION ( 'NONE',  ( -0.000000000000000000, -0.000000000000000000, -1.000000000000000000 ) ) ;
#72061 = CARTESIAN_POINT ( 'NONE',  ( -18.50000000000000000, 66.75000000001151079, -48.27310748452438816 ) ) ;
#72062 = DIRECTION ( 'NONE',  ( 1.000000000000000000, 0.000000000000000000, -0.000000000000000000 ) ) ;
#72063 = DIRECTION ( 'NONE',  ( -1.000000000000000000, 0.000000000000000000, 0.000000000000000000 ) ) ;
#72064 = ORIENTED_EDGE ( 'NONE', *, *, #136992, .F. ) ;
#72065 = DIRECTION ( 'NONE',  ( 1.000000000000000000, 0.000000000000000000, 0.000000000000000000 ) ) ;
#72066 = LINE ( 'NONE', #92886, #136117 ) ;
#72067 = ADVANCED_FACE ( 'NONE', ( #75822 ), #237464, .T. ) ;
#72069 = CARTESIAN_POINT ( 'NONE',  ( 23.14999999999999858, 76.00000000001126921, -203.5231074845248997 ) ) ;
#72068 = DIRECTION ( 'NONE',  ( -1.000000000000000000, 7.304098846218134667E-16, 4.217023435051625732E-16 ) ) ;
#72070 = DIRECTION ( 'NONE',  ( 0.000000000000000000, -7.026728003956686545E-15, 1.000000000000000000 ) ) ;
#72071 = CARTESIAN_POINT ( 'NONE',  ( -16.84981964351500849, 9.917318234109957942, -54.13039838598031395 ) ) ;
#72072 = DIRECTION ( 'NONE',  ( 1.000000000000000000, -7.304098846218134667E-16, -0.000000000000000000 ) ) ;
#72073 = LINE ( 'NONE', #169923, #76979 ) ;
#72074 = CARTESIAN_POINT ( 'NONE',  ( 18.43709777086140278, 85.68240343348880117, -163.3662641071115615 ) ) ;
#72075 = CARTESIAN_POINT ( 'NONE',  ( 21.33487959338958362, 6.725558151922348848, -33.50000000000000000 ) ) ;
#72076 = EDGE_CURVE ( 'NONE', #168569, #203210, #17155, .T. ) ;
#72077 = EDGE_CURVE ( 'NONE', #172330, #69117, #190522, .T. ) ;
#72078 = ORIENTED_EDGE ( 'NONE', *, *, #253030, .F. ) ;
#72079 = AXIS2_PLACEMENT_3D ( 'NONE', #202358, #219348, #224479 ) ;
#72080 = ORIENTED_EDGE ( 'NONE', *, *, #168381, .T. ) ;
#72081 = ORIENTED_EDGE ( 'NONE', *, *, #59346, .T. ) ;
#72082 = EDGE_CURVE ( 'NONE', #244309, #103352, #189923, .T. ) ;
#72083 = DIRECTION ( 'NONE',  ( 0.000000000000000000, 0.000000000000000000, -1.000000000000000000 ) ) ;
#72084 = DIRECTION ( 'NONE',  ( 0.000000000000000000, -0.000000000000000000, -1.000000000000000000 ) ) ;
#72085 = ORIENTED_EDGE ( 'NONE', *, *, #110445, .F. ) ;
#72086 = CARTESIAN_POINT ( 'NONE',  ( 23.40000000000005187, 76.00000000001119815, -31.87310748452479459 ) ) ;
#72087 = EDGE_CURVE ( 'NONE', #220201, #54789, #256970, .T. ) ;
#72088 = ORIENTED_EDGE ( 'NONE', *, *, #26997, .F. ) ;
#72089 = EDGE_CURVE ( 'NONE', #87043, #136449, #57520, .T. ) ;
#72090 = VERTEX_POINT ( 'NONE', #38006 ) ;
#72091 = DIRECTION ( 'NONE',  ( -0.000000000000000000, -0.7397360091702755991, -0.6728971962616832059 ) ) ;
#72092 = ORIENTED_EDGE ( 'NONE', *, *, #165015, .F. ) ;
#72093 = CIRCLE ( 'NONE', #251113, 0.5000000000000004441 ) ;
#72094 = CARTESIAN_POINT ( 'NONE',  ( 23.24999999999999645, 67.23581240663841641, -214.2531594801197627 ) ) ;
#72095 = DIRECTION ( 'NONE',  ( 0.000000000000000000, 0.000000000000000000, -1.000000000000000000 ) ) ;
#72096 = DIRECTION ( 'NONE',  ( -1.000000000000000000, 2.952720810173289112E-16, 2.061873921506763405E-30 ) ) ;
#72097 = AXIS2_PLACEMENT_3D ( 'NONE', #14696, #53788, #250697 ) ;
#72098 = FACE_OUTER_BOUND ( 'NONE', #142215, .T. ) ;
#72099 = DIRECTION ( 'NONE',  ( 0.000000000000000000, -1.000000000000000000, 0.000000000000000000 ) ) ;
#72101 = VERTEX_POINT ( 'NONE', #251879 ) ;
#72100 = CARTESIAN_POINT ( 'NONE',  ( 18.59999999999999787, -1.835859311432481045, -112.0044391687985694 ) ) ;
#72103 = DIRECTION ( 'NONE',  ( 0.000000000000000000, -0.2599159095383244966, 0.9656312546561787169 ) ) ;
#72102 = FACE_OUTER_BOUND ( 'NONE', #103652, .T. ) ;
#72104 = EDGE_CURVE ( 'NONE', #190072, #51901, #44750, .T. ) ;
#72105 = DIRECTION ( 'NONE',  ( 0.000000000000000000, 0.000000000000000000, -1.000000000000000000 ) ) ;
#72106 = DIRECTION ( 'NONE',  ( 0.000000000000000000, -6.982962677686266711E-15, 1.000000000000000000 ) ) ;
#72107 = CARTESIAN_POINT ( 'NONE',  ( -13.77178122865953824, 9.456028260519072859, -115.5111980350657745 ) ) ;
#72108 = CARTESIAN_POINT ( 'NONE',  ( 23.24999999999999289, 69.35000000001156195, -57.17310748452436542 ) ) ;
#72109 = VERTEX_POINT ( 'NONE', #96631 ) ;
#72110 = AXIS2_PLACEMENT_3D ( 'NONE', #16872, #96369, #117244 ) ;
#72111 = SURFACE_STYLE_FILL_AREA ( #175098 ) ;
#72113 = SPHERICAL_SURFACE ( 'NONE', #100094, 0.1000000000000000056 ) ;
#72112 = CIRCLE ( 'NONE', #251129, 0.2000000000000057288 ) ;
#72114 = CIRCLE ( 'NONE', #130341, 0.09999999999999939493 ) ;
#72115 = CARTESIAN_POINT ( 'NONE',  ( -20.94999999999999929, 87.39257802171759693, -99.94915790469229933 ) ) ;
#72116 = ORIENTED_EDGE ( 'NONE', *, *, #256300, .F. ) ;
#72117 = DIRECTION ( 'NONE',  ( 1.000000000000000000, 2.952720810173289112E-16, -0.000000000000000000 ) ) ;
#72118 = CIRCLE ( 'NONE', #76176, 0.09999999999999939493 ) ;
#72119 = DIRECTION ( 'NONE',  ( 0.000000000000000000, 0.2128009952263604232, -0.9770955615653316162 ) ) ;
#72120 = DIRECTION ( 'NONE',  ( -1.000000000000000000, -3.295974604355953674E-13, 0.000000000000000000 ) ) ;
#72121 = ORIENTED_EDGE ( 'NONE', *, *, #79590, .T. ) ;
#72122 = VERTEX_POINT ( 'NONE', #113658 ) ;
#72123 = AXIS2_PLACEMENT_3D ( 'NONE', #26589, #7002, #185648 ) ;
#72124 = AXIS2_PLACEMENT_3D ( 'NONE', #246693, #224560, #48497 ) ;
#72125 = AXIS2_PLACEMENT_3D ( 'NONE', #7715, #31156, #225439 ) ;
#72126 = CIRCLE ( 'NONE', #147122, 0.1000000000000000472 ) ;
#72127 = LINE ( 'NONE', #169973, #198437 ) ;
#72128 = CARTESIAN_POINT ( 'NONE',  ( 21.05000000000000071, 5.850000000011156942, -123.8675027757221159 ) ) ;
#72129 = EDGE_CURVE ( 'NONE', #173624, #72705, #223230, .T. ) ;
#72130 = CARTESIAN_POINT ( 'NONE',  ( 20.92356734117541706, 65.68026841930954163, -164.4725740131889893 ) ) ;
#72131 = CARTESIAN_POINT ( 'NONE',  ( -23.15000000000000213, 33.22109292269086467, -247.7096104798602312 ) ) ;
#72133 = LINE ( 'NONE', #49980, #25150 ) ;
#72132 = DIRECTION ( 'NONE',  ( 1.000000000000000000, -1.335000415235278971E-16, 2.979993593738921214E-16 ) ) ;
#72134 = DIRECTION ( 'NONE',  ( 1.000000000000000000, -7.304098846218134667E-16, -4.217023435051626718E-16 ) ) ;
#72135 = ADVANCED_FACE ( 'NONE', ( #217870 ), #174973, .T. ) ;
#72136 = FACE_OUTER_BOUND ( 'NONE', #42043, .T. ) ;
#72137 = DIRECTION ( 'NONE',  ( 0.000000000000000000, -1.000000000000000000, -6.982962677686265922E-15 ) ) ;
#72138 = EDGE_LOOP ( 'NONE', ( #63652, #251855, #139215, #109778 ) ) ;
#72139 = DIRECTION ( 'NONE',  ( 0.000000000000000000, -0.1350103645451945777, 0.9908441862701590219 ) ) ;
#72141 = ORIENTED_EDGE ( 'NONE', *, *, #145311, .F. ) ;
#72140 = LINE ( 'NONE', #34311, #129674 ) ;
#72142 = DIRECTION ( 'NONE',  ( 0.000000000000000000, 0.000000000000000000, -1.000000000000000000 ) ) ;
#72143 = DIRECTION ( 'NONE',  ( -0.7071067811865475727, 0.7071067811865475727, 4.937700262164531476E-15 ) ) ;
#72145 = DIRECTION ( 'NONE',  ( 0.000000000000000000, -0.8777080977375132376, 0.4791956752371582251 ) ) ;
#72144 = DIRECTION ( 'NONE',  ( -1.000000000000000000, -1.394253735153569469E-16, -2.602809386958778209E-16 ) ) ;
#72146 = DIRECTION ( 'NONE',  ( 1.000000000000000000, 0.000000000000000000, 0.000000000000000000 ) ) ;
#72147 = ADVANCED_FACE ( 'NONE', ( #193216 ), #137760, .F. ) ;
#72148 = ADVANCED_FACE ( 'NONE', ( #78375 ), #85841, .T. ) ;
#72149 = CARTESIAN_POINT ( 'NONE',  ( 20.85000000106584750, 11.75000000001115907, -194.1555046564733971 ) ) ;
#72151 = ORIENTED_EDGE ( 'NONE', *, *, #205081, .T. ) ;
#72150 = DIRECTION ( 'NONE',  ( -0.000000000000000000, -0.000000000000000000, 1.000000000000000000 ) ) ;
#72152 = CARTESIAN_POINT ( 'NONE',  ( 20.90000000000000213, -1.885425182446133885, -11.49641995933507843 ) ) ;
#72153 = CARTESIAN_POINT ( 'NONE',  ( 21.05000000000000071, 24.17260720300848575, -252.6908294531417027 ) ) ;
#72154 = CARTESIAN_POINT ( 'NONE',  ( 22.48660254037843842, 11.75000000001115907, -66.95000000000003126 ) ) ;
#72155 = DIRECTION ( 'NONE',  ( 0.000000000000000000, -1.000000000000000000, 6.938893903907270030E-14 ) ) ;
#72156 = VERTEX_POINT ( 'NONE', #53687 ) ;
#72157 = CARTESIAN_POINT ( 'NONE',  ( -18.59999999999999787, 11.62724406944293598, -220.3181830240302190 ) ) ;
#72158 = VERTEX_POINT ( 'NONE', #215325 ) ;
#72159 = CARTESIAN_POINT ( 'NONE',  ( -17.05016517656038744, 66.05000000000937632, -90.35040948852557108 ) ) ;
#72160 = ORIENTED_EDGE ( 'NONE', *, *, #226076, .T. ) ;
#72161 = CARTESIAN_POINT ( 'NONE',  ( 18.39999999999997371, 33.92263863280957281, -235.0698407953532296 ) ) ;
#72162 = ORIENTED_EDGE ( 'NONE', *, *, #214482, .F. ) ;
#72163 = EDGE_CURVE ( 'NONE', #175143, #155422, #219126, .T. ) ;
#72164 = FACE_OUTER_BOUND ( 'NONE', #78849, .T. ) ;
#72165 = CARTESIAN_POINT ( 'NONE',  ( 21.05000000000000071, 70.15000000001198543, -113.1556047088022581 ) ) ;
#72166 = AXIS2_PLACEMENT_3D ( 'NONE', #187118, #64569, #145388 ) ;
#72167 = VECTOR ( 'NONE', #9458, 1000.000000000000000 ) ;
#72168 = DIRECTION ( 'NONE',  ( -2.252264143451594314E-15, -0.1298341882520124002, -0.9915357197604841577 ) ) ;
#72169 = ORIENTED_EDGE ( 'NONE', *, *, #169041, .T. ) ;
#72170 = AXIS2_PLACEMENT_3D ( 'NONE', #104464, #5362, #184022 ) ;
#72171 = DIRECTION ( 'NONE',  ( 0.000000000000000000, 0.000000000000000000, -1.000000000000000000 ) ) ;
#72172 = B_SPLINE_CURVE_WITH_KNOTS ( 'NONE', 3,
 ( #20247, #97151, #120644, #198866, #159752, #16402, #137589, #195039, #55465, #239287 ),
 .UNSPECIFIED., .F., .F.,
 ( 4, 3, 3, 4 ),
 ( 7.632826238681696029E-06, 4.756916949875625587E-05, 9.484459048150268483E-05, 0.0001435500935099809469 ),
 .UNSPECIFIED. ) ;
#72173 = VECTOR ( 'NONE', #244471, 1000.000000000000000 ) ;
#72174 = CARTESIAN_POINT ( 'NONE',  ( 18.49999999999999289, 69.35000000001151932, -48.17310748452437252 ) ) ;
#72175 = CIRCLE ( 'NONE', #34767, 0.1000000000000009354 ) ;
#72176 = CIRCLE ( 'NONE', #1221, 0.09999999999999971412 ) ;
#72177 = DIRECTION ( 'NONE',  ( 1.000000000000000000, -0.000000000000000000, -0.000000000000000000 ) ) ;
#72178 = FACE_OUTER_BOUND ( 'NONE', #88075, .T. ) ;
#72180 = ORIENTED_EDGE ( 'NONE', *, *, #220594, .F. ) ;
#72179 = ADVANCED_FACE ( 'NONE', ( #126157 ), #85722, .F. ) ;
#72181 = CARTESIAN_POINT ( 'NONE',  ( -18.44204374631838661, 85.49103638961042861, -129.8969062143032716 ) ) ;
#72182 = VERTEX_POINT ( 'NONE', #121407 ) ;
#72184 = EDGE_LOOP ( 'NONE', ( #222760, #149009, #199551, #61403 ) ) ;
#72183 = CARTESIAN_POINT ( 'NONE',  ( -18.59999999999999787, 77.83534155023700407, -191.9679561919613491 ) ) ;
#72185 = VECTOR ( 'NONE', #162065, 1000.000000000000000 ) ;
#72186 = ORIENTED_EDGE ( 'NONE', *, *, #217958, .T. ) ;
#72187 = DIRECTION ( 'NONE',  ( 1.000000000000000000, 0.000000000000000000, 0.000000000000000000 ) ) ;
#72188 = DIRECTION ( 'NONE',  ( -0.000000000000000000, 0.000000000000000000, -1.000000000000000000 ) ) ;
#72189 = LINE ( 'NONE', #167445, #197551 ) ;
#72190 = DIRECTION ( 'NONE',  ( 2.827886303505249259E-16, -0.8660254037844411501, -0.4999999999999956701 ) ) ;
#72191 = EDGE_LOOP ( 'NONE', ( #201449, #245682, #53417, #203860 ) ) ;
#72192 = CARTESIAN_POINT ( 'NONE',  ( 18.59999999999999432, -9.480686695267811714, -140.9411151687579036 ) ) ;
#72193 = EDGE_CURVE ( 'NONE', #127544, #74110, #252442, .T. ) ;
#72194 = VERTEX_POINT ( 'NONE', #39289 ) ;
#72195 = AXIS2_PLACEMENT_3D ( 'NONE', #217151, #82758, #183197 ) ;
#72197 = ORIENTED_EDGE ( 'NONE', *, *, #143324, .T. ) ;
#72196 = DIRECTION ( 'NONE',  ( -1.000000000000000000, -0.000000000000000000, -0.000000000000000000 ) ) ;
#72199 = EDGE_CURVE ( 'NONE', #127135, #139652, #94235, .T. ) ;
#72198 = DIRECTION ( 'NONE',  ( 0.000000000000000000, 1.224646799142015331E-16, 1.000000000000000000 ) ) ;
#72200 = DIRECTION ( 'NONE',  ( -0.7071067811865474617, -0.6909108974501236844, -0.1504730267678055788 ) ) ;
#72201 = AXIS2_PLACEMENT_3D ( 'NONE', #108822, #149267, #110114 ) ;
#72202 = CIRCLE ( 'NONE', #217900, 0.09999999999999939493 ) ;
#72203 = ORIENTED_EDGE ( 'NONE', *, *, #174534, .T. ) ;
#72204 = CIRCLE ( 'NONE', #188697, 1.749999999999998002 ) ;
#72205 = VECTOR ( 'NONE', #175534, 1000.000000000000000 ) ;
#72206 = FACE_OUTER_BOUND ( 'NONE', #138059, .T. ) ;
#72207 = EDGE_CURVE ( 'NONE', #245468, #23492, #119197, .T. ) ;
#72208 = CARTESIAN_POINT ( 'NONE',  ( -20.86777300164945004, 18.41441690808118281, -236.9991004306322964 ) ) ;
#72209 = ORIENTED_EDGE ( 'NONE', *, *, #95518, .F. ) ;
#72210 = CARTESIAN_POINT ( 'NONE',  ( -20.54999999999999716, 76.00000000001190870, -103.0231074845243029 ) ) ;
#72211 = EDGE_CURVE ( 'NONE', #176891, #168958, #144108, .T. ) ;
#72212 = FACE_OUTER_BOUND ( 'NONE', #53086, .T. ) ;
#72213 = ADVANCED_FACE ( 'NONE', ( #80935 ), #206674, .F. ) ;
#72214 = CARTESIAN_POINT ( 'NONE',  ( -20.94999999999999929, 5.850000000011105428, -110.6324972242780120 ) ) ;
#72215 = ADVANCED_FACE ( 'NONE', ( #7510 ), #247393, .F. ) ;
#72216 = AXIS2_PLACEMENT_3D ( 'NONE', #44020, #103967, #151806 ) ;
#72217 = AXIS2_PLACEMENT_3D ( 'NONE', #214580, #136305, #193748 ) ;
#72218 = AXIS2_PLACEMENT_3D ( 'NONE', #238089, #218510, #58155 ) ;
#72219 = ORIENTED_EDGE ( 'NONE', *, *, #209227, .F. ) ;
#72220 = DIRECTION ( 'NONE',  ( -1.000000000000000000, 0.000000000000000000, 0.000000000000000000 ) ) ;
#72221 = ORIENTED_EDGE ( 'NONE', *, *, #23448, .F. ) ;
#72222 = CARTESIAN_POINT ( 'NONE',  ( -18.43569575749026512, -9.519327731081288491, -174.4729763765592736 ) ) ;
#72224 = EDGE_CURVE ( 'NONE', #237722, #106114, #257074, .T. ) ;
#72223 = DIRECTION ( 'NONE',  ( 0.000000000000000000, 0.000000000000000000, -1.000000000000000000 ) ) ;
#72227 = ORIENTED_EDGE ( 'NONE', *, *, #78351, .T. ) ;
#72226 = DIRECTION ( 'NONE',  ( 1.000000000000000000, -0.000000000000000000, 0.000000000000000000 ) ) ;
#72225 =( BOUNDED_SURFACE ( )  B_SPLINE_SURFACE ( 3, 2, ( 
 ( #33584, #250015, #191357 ),
 ( #32280, #246168, #212188 ),
 ( #109206, #227886, #10127 ),
 ( #251284, #49241, #89642 ) ),
 .UNSPECIFIED., .F., .F., .F. ) 
 B_SPLINE_SURFACE_WITH_KNOTS ( ( 4, 4 ),
 ( 3, 3 ),
 ( 0.0008258556059633741101, 0.0009616864997632823065 ),
 ( 0.000000000000000000, 1.000000000000000000 ),
 .UNSPECIFIED. ) 
 GEOMETRIC_REPRESENTATION_ITEM ( )  RATIONAL_B_SPLINE_SURFACE ( (
 ( 1.000000000000000000, 0.9152888060719235330, 1.000000000000000000),
 ( 1.000000000000000000, 0.9327727094137976405, 1.000000000000000000),
 ( 1.000000000000000000, 0.9369023509258225246, 1.000000000000000000),
 ( 1.000000000000000000, 0.9246339933864551330, 1.000000000000000000) ) ) 
 REPRESENTATION_ITEM ( '' )  SURFACE ( )  );
#72228 = DIRECTION ( 'NONE',  ( 1.000000000000000000, 0.000000000000000000, 0.000000000000000000 ) ) ;
#72229 = CARTESIAN_POINT ( 'NONE',  ( 20.94999999999999929, -4.656943609564680564, -233.1535107627236414 ) ) ;
#72230 = DIRECTION ( 'NONE',  ( 0.000000000000000000, -6.982962677686266711E-15, 1.000000000000000000 ) ) ;
#72231 = CARTESIAN_POINT ( 'NONE',  ( -16.87435696428308063, 22.97806136355487183, -230.9350573516298368 ) ) ;
#72232 = PLANE ( 'NONE',  #43652 ) ;
#72233 = DIRECTION ( 'NONE',  ( -1.000000000000000000, 0.000000000000000000, 0.000000000000000000 ) ) ;
#72234 = CARTESIAN_POINT ( 'NONE',  ( 20.85000000000000142, 76.00000000001213607, -136.5231074845243313 ) ) ;
#72236 = VERTEX_POINT ( 'NONE', #166620 ) ;
#72235 = DIRECTION ( 'NONE',  ( -0.000000000000000000, 0.000000000000000000, 1.000000000000000000 ) ) ;
#72237 = CARTESIAN_POINT ( 'NONE',  ( -22.50000000000000000, 76.00000000001169553, -75.77310748452431710 ) ) ;
#72238 = VECTOR ( 'NONE', #23791, 1000.000000000000000 ) ;
#72239 = CARTESIAN_POINT ( 'NONE',  ( 23.14999999999999858, 5.499999999999998224, -21.09473398108690390 ) ) ;
#72240 = DIRECTION ( 'NONE',  ( 0.000000000000000000, 0.9651348961777157509, -0.2617529984165031243 ) ) ;
#72241 = DIRECTION ( 'NONE',  ( -1.000000000000000000, 0.000000000000000000, -0.000000000000000000 ) ) ;
#72242 = ORIENTED_EDGE ( 'NONE', *, *, #146552, .T. ) ;
#72243 = FACE_OUTER_BOUND ( 'NONE', #113639, .T. ) ;
#72244 = DIRECTION ( 'NONE',  ( 0.000000000000000000, -1.000000000000000000, 0.000000000000000000 ) ) ;
#72245 = ORIENTED_EDGE ( 'NONE', *, *, #72261, .F. ) ;
#72246 = AXIS2_PLACEMENT_3D ( 'NONE', #7104, #218765, #5810 ) ;
#72248 = ADVANCED_FACE ( 'NONE', ( #246130 ), #67480, .T. ) ;
#72247 = DIRECTION ( 'NONE',  ( -1.000000000000000000, 0.000000000000000000, 0.000000000000000000 ) ) ;
#72249 = VECTOR ( 'NONE', #153990, 1000.000000000000000 ) ;
#72250 = VECTOR ( 'NONE', #34223, 1000.000000000000000 ) ;
#72251 = PLANE ( 'NONE',  #151480 ) ;
#72252 = ORIENTED_EDGE ( 'NONE', *, *, #175685, .T. ) ;
#72253 = LINE ( 'NONE', #95643, #256645 ) ;
#72254 = EDGE_LOOP ( 'NONE', ( #13999, #230751, #191195, #214583 ) ) ;
#72256 = EDGE_CURVE ( 'NONE', #161970, #109286, #31740, .T. ) ;
#72255 = DIRECTION ( 'NONE',  ( 0.000000000000000000, 0.9910827722268049644, 0.1332476588733589318 ) ) ;
#72258 = VERTEX_POINT ( 'NONE', #99210 ) ;
#72257 = CARTESIAN_POINT ( 'NONE',  ( 21.53752568622128294, 75.90102553874136504, -143.3099153590727610 ) ) ;
#72259 = DIRECTION ( 'NONE',  ( 1.000000000000000000, 0.000000000000000000, -0.000000000000000000 ) ) ;
#72260 = ORIENTED_EDGE ( 'NONE', *, *, #162043, .F. ) ;
#72261 = EDGE_CURVE ( 'NONE', #9997, #147041, #111378, .T. ) ;
#72262 = DIRECTION ( 'NONE',  ( 1.000000000000000000, 0.000000000000000000, -0.000000000000000000 ) ) ;
#72263 = EDGE_CURVE ( 'NONE', #138091, #107290, #107892, .T. ) ;
#72264 = ORIENTED_EDGE ( 'NONE', *, *, #77889, .T. ) ;
#72266 = EDGE_LOOP ( 'NONE', ( #127334, #114967, #152587, #63543, #89216 ) ) ;
#72265 = ORIENTED_EDGE ( 'NONE', *, *, #69279, .T. ) ;
#72268 = DIRECTION ( 'NONE',  ( 0.000000000000000000, 0.9126074666063772600, 0.4088369013363274962 ) ) ;
#72267 = AXIS2_PLACEMENT_3D ( 'NONE', #94259, #212938, #12191 ) ;
#72269 = EDGE_LOOP ( 'NONE', ( #243177, #32290 ) ) ;
#72270 = DIRECTION ( 'NONE',  ( 1.000000000000000000, 0.000000000000000000, 0.000000000000000000 ) ) ;
#72271 = ORIENTED_EDGE ( 'NONE', *, *, #55736, .T. ) ;
#72272 = AXIS2_PLACEMENT_3D ( 'NONE', #61958, #200184, #180618 ) ;
#72273 = AXIS2_PLACEMENT_3D ( 'NONE', #254519, #193304, #14684 ) ;
#72274 = AXIS2_PLACEMENT_3D ( 'NONE', #199276, #158885, #161446 ) ;
#72275 = ORIENTED_EDGE ( 'NONE', *, *, #98367, .T. ) ;
#72276 = EDGE_CURVE ( 'NONE', #256668, #252315, #98297, .T. ) ;
#72277 = DIRECTION ( 'NONE',  ( -1.000000000000000000, -0.000000000000000000, -0.000000000000000000 ) ) ;
#72278 = SPHERICAL_SURFACE ( 'NONE', #205587, 0.1000000000000000056 ) ;
#72279 = CARTESIAN_POINT ( 'NONE',  ( 18.39999999999999858, -0.8467571797981052750, -242.2246066262668194 ) ) ;
#72280 = ORIENTED_EDGE ( 'NONE', *, *, #93887, .F. ) ;
#72281 = ADVANCED_FACE ( 'NONE', ( #187450 ), #145723, .T. ) ;
#72282 = CARTESIAN_POINT ( 'NONE',  ( -21.14999999999999503, 64.25000000001209344, -129.6039602385655769 ) ) ;
#72283 = FACE_OUTER_BOUND ( 'NONE', #53138, .T. ) ;
#72284 = CARTESIAN_POINT ( 'NONE',  ( 21.14999999999999858, 6.550000000000000711, -12.15000000000000036 ) ) ;
#72285 = CIRCLE ( 'NONE', #14033, 0.09999999999999439892 ) ;
#72286 = EDGE_LOOP ( 'NONE', ( #83101, #257140, #213709, #163791 ) ) ;
#72287 = TOROIDAL_SURFACE ( 'NONE', #76344, 0.2000000000000000111, 0.1000000000000000056 ) ;
#72288 = CARTESIAN_POINT ( 'NONE',  ( 23.14999999999999503, 64.35000000001222986, -148.6731074845244507 ) ) ;
#72289 = DIRECTION ( 'NONE',  ( -1.000000000000000000, -0.000000000000000000, -0.000000000000000000 ) ) ;
#72290 = DIRECTION ( 'NONE',  ( 1.734723475976757112E-13, 0.9999176327611370985, 0.01283462868040226822 ) ) ;
#72291 = AXIS2_PLACEMENT_3D ( 'NONE', #35650, #175172, #254630 ) ;
#72292 = FACE_OUTER_BOUND ( 'NONE', #123070, .T. ) ;
#72293 = ORIENTED_EDGE ( 'NONE', *, *, #246868, .F. ) ;
#72294 = FACE_OUTER_BOUND ( 'NONE', #241548, .T. ) ;
#72295 = ORIENTED_EDGE ( 'NONE', *, *, #30938, .F. ) ;
#72296 = LINE ( 'NONE', #30610, #164935 ) ;
#72297 = EDGE_LOOP ( 'NONE', ( #41377, #94309, #253285, #37124, #13683, #57585, #110760, #160222, #80307, #156075, #229222, #24677 ) ) ;
#72298 = CARTESIAN_POINT ( 'NONE',  ( -12.24999999999999822, 26.10487691728824799, -233.2906712717671951 ) ) ;
#72299 = FACE_OUTER_BOUND ( 'NONE', #35376, .T. ) ;
#72300 = ADVANCED_FACE ( 'NONE', ( #106588 ), #19232, .F. ) ;
#72302 = ORIENTED_EDGE ( 'NONE', *, *, #110941, .T. ) ;
#72301 = VECTOR ( 'NONE', #162499, 1000.000000000000000 ) ;
#72303 = ORIENTED_EDGE ( 'NONE', *, *, #204546, .T. ) ;
#72304 = LINE ( 'NONE', #46287, #136413 ) ;
#72305 = EDGE_CURVE ( 'NONE', #72705, #1104, #53112, .T. ) ;
#72306 = DIRECTION ( 'NONE',  ( 6.938893903907224433E-15, -1.000000000000000000, -2.891205793294679805E-16 ) ) ;
#72307 = VERTEX_POINT ( 'NONE', #12672 ) ;
#72308 = ADVANCED_FACE ( 'NONE', ( #230411 ), #171754, .F. ) ;
#72309 = VERTEX_POINT ( 'NONE', #227836 ) ;
#72310 = CARTESIAN_POINT ( 'NONE',  ( -21.05000000000000071, 1.115600667400684642E-11, -67.00000000000000000 ) ) ;
#72311 = AXIS2_PLACEMENT_3D ( 'NONE', #139474, #100335, #37848 ) ;
#72312 = CIRCLE ( 'NONE', #47323, 0.09999999999999939493 ) ;
#72313 = CIRCLE ( 'NONE', #222101, 0.1000000000000013933 ) ;
#72314 = DIRECTION ( 'NONE',  ( -2.812466655313719426E-14, 0.1350103645451904977, 0.9908441862701596881 ) ) ;
#72315 = VECTOR ( 'NONE', #119950, 1000.000000000000000 ) ;
#72316 = VERTEX_POINT ( 'NONE', #93453 ) ;
#72317 = EDGE_CURVE ( 'NONE', #60618, #197578, #231628, .T. ) ;
#72318 = VERTEX_POINT ( 'NONE', #33543 ) ;
#72319 = DIRECTION ( 'NONE',  ( 1.000000000000000000, -0.000000000000000000, -0.000000000000000000 ) ) ;
#72320 =( BOUNDED_SURFACE ( )  B_SPLINE_SURFACE ( 3, 2, ( 
 ( #175444, #94587, #213248 ),
 ( #253654, #136262, #37211 ),
 ( #116726, #58013, #137556 ),
 ( #217088, #181848, #200127 ),
 ( #123160, #1898, #121885 ),
 ( #24080, #243095, #5745 ) ),
 .UNSPECIFIED., .F., .F., .F. ) 
 B_SPLINE_SURFACE_WITH_KNOTS ( ( 4, 2, 4 ),
 ( 3, 3 ),
 ( 0.0001300404313046710908, 0.0003183318589266752666, 0.0005066232865486794152 ),
 ( 0.000000000000000000, 1.000000000000000000 ),
 .UNSPECIFIED. ) 
 GEOMETRIC_REPRESENTATION_ITEM ( )  RATIONAL_B_SPLINE_SURFACE ( (
 ( 1.000000000000000000, 0.7071067811865475727, 1.000000000000000000),
 ( 1.000000000000000000, 0.7625113560543049784, 1.000000000000000000),
 ( 1.000000000000000000, 0.8126073484684088744, 1.000000000000000000),
 ( 1.000000000000000000, 0.8923049332736880945, 1.000000000000000000),
 ( 1.000000000000000000, 0.9231914937766396712, 1.000000000000000000),
 ( 1.000000000000000000, 0.9238795325112915124, 1.000000000000000000) ) ) 
 REPRESENTATION_ITEM ( '' )  SURFACE ( )  );
#72321 = CARTESIAN_POINT ( 'NONE',  ( 18.59999999999999787, -1.835341550213255957, -179.1551512925629197 ) ) ;
#72322 = FACE_OUTER_BOUND ( 'NONE', #109707, .T. ) ;
#72324 = ORIENTED_EDGE ( 'NONE', *, *, #63261, .F. ) ;
#72323 = CARTESIAN_POINT ( 'NONE',  ( 23.14999999999999858, 67.55989888862310977, -211.9120700681549465 ) ) ;
#72325 = LINE ( 'NONE', #134819, #161894 ) ;
#72326 = CARTESIAN_POINT ( 'NONE',  ( -20.64999999999999858, 0.000000000000000000, -33.50000000000000000 ) ) ;
#72328 = ADVANCED_FACE ( 'NONE', ( #71357 ), #249977, .F. ) ;
#72327 = DIRECTION ( 'NONE',  ( 0.000000000000000000, 0.9788861828082167094, 0.2044060691544132835 ) ) ;
#72329 = AXIS2_PLACEMENT_3D ( 'NONE', #146867, #67357, #105146 ) ;
#72330 = B_SPLINE_CURVE_WITH_KNOTS ( 'NONE', 3,
 ( #20132, #200047, #18827, #218290, #82621, #81339, #201319, #61820, #141348, #40997 ),
 .UNSPECIFIED., .F., .F.,
 ( 4, 3, 3, 4 ),
 ( 1.551583845779545699E-17, 0.0002000000000002884074, 0.001000000000045107602, 0.001967863649472132576 ),
 .UNSPECIFIED. ) ;
#72332 = DIRECTION ( 'NONE',  ( 1.000000000000000000, 0.000000000000000000, 0.000000000000000000 ) ) ;
#72331 = CARTESIAN_POINT ( 'NONE',  ( 21.14999999999999858, -0.09999999998884338825, -55.35042919245524473 ) ) ;
#72333 = CARTESIAN_POINT ( 'NONE',  ( -18.59999999999999787, 19.02280865327213277, -233.3540837620168986 ) ) ;
#72334 = CARTESIAN_POINT ( 'NONE',  ( -16.94107738177415712, 65.98576071487495653, -56.97310748452439810 ) ) ;
#72335 = CIRCLE ( 'NONE', #176399, 0.09999999999999954758 ) ;
#72336 = DIRECTION ( 'NONE',  ( 0.000000000000000000, 0.000000000000000000, -1.000000000000000000 ) ) ;
#72338 = CARTESIAN_POINT ( 'NONE',  ( 23.14999999999999503, 64.35000000001218723, -143.5379132551783812 ) ) ;
#72337 = CIRCLE ( 'NONE', #172329, 0.09999999999999939493 ) ;
#72339 = VERTEX_POINT ( 'NONE', #72644 ) ;
#72340 = CIRCLE ( 'NONE', #155745, 0.09999999999999939493 ) ;
#72341 = ADVANCED_FACE ( 'NONE', ( #173053 ), #208297, .F. ) ;
#72342 = AXIS2_PLACEMENT_3D ( 'NONE', #78410, #200938, #57555 ) ;
#72343 = ORIENTED_EDGE ( 'NONE', *, *, #30628, .F. ) ;
#72344 = CYLINDRICAL_SURFACE ( 'NONE', #31888, 0.1000000000000070832 ) ;
#72345 = ADVANCED_FACE ( 'NONE', ( #190006 ), #51745, .F. ) ;
#72346 = CARTESIAN_POINT ( 'NONE',  ( -23.15000000000000213, 40.18490544642472884, -251.4399342103543233 ) ) ;
#72347 = ORIENTED_EDGE ( 'NONE', *, *, #239019, .T. ) ;
#72348 = AXIS2_PLACEMENT_3D ( 'NONE', #233905, #133521, #214346 ) ;
#72349 = CARTESIAN_POINT ( 'NONE',  ( -23.15000000000000213, 6.307392164054360428, -220.9841382799134522 ) ) ;
#72350 = VECTOR ( 'NONE', #61059, 1000.000000000000000 ) ;
#72351 = CARTESIAN_POINT ( 'NONE',  ( 18.52928932188133970, 10.27928932189250411, -58.15000000000000568 ) ) ;
#72352 = CIRCLE ( 'NONE', #43126, 0.1000000000000008937 ) ;
#72353 = PRODUCT ( 'Snap Open Cable Crossbars 12', 'Snap Open Cable Crossbars 12', '', ( #133060 ) ) ;
#72354 = CARTESIAN_POINT ( 'NONE',  ( -23.25000000000000000, 1.115600667400684642E-11, -67.00000000000000000 ) ) ;
#72355 = ORIENTED_EDGE ( 'NONE', *, *, #177166, .F. ) ;
#72356 = EDGE_LOOP ( 'NONE', ( #33422, #244447, #45383, #194394 ) ) ;
#72357 = AXIS2_PLACEMENT_3D ( 'NONE', #4880, #66170, #244794 ) ;
#72358 = ADVANCED_FACE ( 'NONE', ( #253810 ), #32235, .F. ) ;
#72359 = CARTESIAN_POINT ( 'NONE',  ( 21.14999999999999858, 60.09787988008869775, -221.2279614330287245 ) ) ;
#72360 = CARTESIAN_POINT ( 'NONE',  ( 22.50000000000000000, -3.181516632163039482, -228.0962854788089942 ) ) ;
#72362 = ADVANCED_FACE ( 'NONE', ( #131306 ), #132604, .F. ) ;
#72361 = VERTEX_POINT ( 'NONE', #53050 ) ;
#72363 = DIRECTION ( 'NONE',  ( 0.000000000000000000, 0.1350103645451904977, 0.9908441862701596881 ) ) ;
#72365 = ORIENTED_EDGE ( 'NONE', *, *, #3451, .F. ) ;
#72364 = DIRECTION ( 'NONE',  ( 0.000000000000000000, 0.2128009952263485993, -0.9770955615653341697 ) ) ;
#72366 = CARTESIAN_POINT ( 'NONE',  ( -21.07933241753356413, 75.90662040959291801, -142.8517534329040473 ) ) ;
#72367 = AXIS2_PLACEMENT_3D ( 'NONE', #245286, #189156, #66641 ) ;
#72369 = ORIENTED_EDGE ( 'NONE', *, *, #87040, .T. ) ;
#72368 = DIRECTION ( 'NONE',  ( 1.713247197920696300E-14, 0.6046243595031879359, 0.7965107556683461709 ) ) ;
#72370 = CARTESIAN_POINT ( 'NONE',  ( -18.52643265882458579, 10.31973158071402530, -72.55053347133545572 ) ) ;
#72371 = CARTESIAN_POINT ( 'NONE',  ( -16.92989507731676113, 9.950000000011135270, -87.61749893061021055 ) ) ;
#72372 = CYLINDRICAL_SURFACE ( 'NONE', #56822, 0.09999999999999804878 ) ;
#72373 = AXIS2_PLACEMENT_3D ( 'NONE', #81876, #226531, #200577 ) ;
#72374 = EDGE_CURVE ( 'NONE', #70665, #88995, #115093, .T. ) ;
#72376 = CARTESIAN_POINT ( 'NONE',  ( 21.05000000000000071, 8.776282895303626930, -179.6499999999999773 ) ) ;
#72375 = CARTESIAN_POINT ( 'NONE',  ( 21.05000000000000071, 84.73084112150679914, -45.62118220350859588 ) ) ;
#72377 = CARTESIAN_POINT ( 'NONE',  ( -20.64999999999999858, 76.00000000001170974, -69.52310748452431710 ) ) ;
#72378 = CARTESIAN_POINT ( 'NONE',  ( 23.25000000000000000, 84.59626168225550202, -179.4732350016745954 ) ) ;
#72379 = CARTESIAN_POINT ( 'NONE',  ( 21.05000000000000071, 1.316055977212907901, -230.7323992127457473 ) ) ;
#72380 = CARTESIAN_POINT ( 'NONE',  ( 20.94999999999999929, 82.09643798151613225, -215.4278993322501208 ) ) ;
#72381 = ADVANCED_FACE ( 'NONE', ( #153497 ), #73613, .T. ) ;
#72382 = CIRCLE ( 'NONE', #184780, 0.1000000000000028644 ) ;
#72384 = ORIENTED_EDGE ( 'NONE', *, *, #2745, .F. ) ;
#72383 = VECTOR ( 'NONE', #257251, 1000.000000000000114 ) ;
#72385 = FACE_OUTER_BOUND ( 'NONE', #91259, .T. ) ;
#72386 = AXIS2_PLACEMENT_3D ( 'NONE', #176703, #217071, #99684 ) ;
#72387 = VERTEX_POINT ( 'NONE', #213399 ) ;
#72388 = CARTESIAN_POINT ( 'NONE',  ( 22.39999999999999858, 7.790779598384538929, -167.3999999999999773 ) ) ;
#72389 = EDGE_LOOP ( 'NONE', ( #96729, #135267, #135666, #90869 ) ) ;
#72390 = EDGE_CURVE ( 'NONE', #111166, #25855, #177666, .T. ) ;
#72391 = CYLINDRICAL_SURFACE ( 'NONE', #110990, 2.000000000000001776 ) ;
#72392 = EDGE_CURVE ( 'NONE', #185818, #97895, #248694, .T. ) ;
#72393 = ORIENTED_EDGE ( 'NONE', *, *, #106949, .T. ) ;
#72394 = CARTESIAN_POINT ( 'NONE',  ( -21.07954763557547651, 30.85583369947000421, -252.0786915620676325 ) ) ;
#72395 =( LENGTH_UNIT ( ) NAMED_UNIT ( * ) SI_UNIT ( .MILLI., .METRE. ) );
#72396 = ADVANCED_FACE ( 'NONE', ( #15231 ), #70083, .T. ) ;
#72397 = AXIS2_PLACEMENT_3D ( 'NONE', #88919, #228466, #49807 ) ;
#72398 = VECTOR ( 'NONE', #168494, 1000.000000000000000 ) ;
#72399 = EDGE_LOOP ( 'NONE', ( #253521, #198814, #75314, #256080 ) ) ;
#72400 = TOROIDAL_SURFACE ( 'NONE', #197279, 12.97499999999999609, 0.1000000000000000056 ) ;
#72401 = AXIS2_PLACEMENT_3D ( 'NONE', #72323, #28075, #90571 ) ;
#72402 = ORIENTED_EDGE ( 'NONE', *, *, #79648, .F. ) ;
#72403 = DIRECTION ( 'NONE',  ( 0.000000000000000000, 1.000000000000000000, 0.000000000000000000 ) ) ;
#72404 = CARTESIAN_POINT ( 'NONE',  ( -16.79184697841823493, 66.05123833835317271, -56.86896521392187509 ) ) ;
#72405 = DIRECTION ( 'NONE',  ( -1.000000000000000000, -0.000000000000000000, 0.000000000000000000 ) ) ;
#72406 = CARTESIAN_POINT ( 'NONE',  ( 33.30000000000001137, 3.332938107839120701, -347.0000000000001137 ) ) ;
#72407 = SPHERICAL_SURFACE ( 'NONE', #256563, 0.1000000000000000056 ) ;
#72409 = DIRECTION ( 'NONE',  ( 0.000000000000000000, -0.000000000000000000, 1.000000000000000000 ) ) ;
#72408 = DIRECTION ( 'NONE',  ( 0.000000000000000000, 1.734723475976805517E-14, -1.000000000000000000 ) ) ;
#72410 = CARTESIAN_POINT ( 'NONE',  ( 23.14999999999999503, 61.95000000001218154, -142.0368025552853624 ) ) ;
#72412 = EDGE_LOOP ( 'NONE', ( #98745, #7828, #383, #57922, #22672, #202648, #205328, #92835, #250013 ) ) ;
#72411 = CARTESIAN_POINT ( 'NONE',  ( -20.85000000000000142, 10.33248238083634440, -139.5948465439131780 ) ) ;
#72414 = CARTESIAN_POINT ( 'NONE',  ( 20.84999999999999787, 11.75000000001116085, -127.0808527540413166 ) ) ;
#72413 = CARTESIAN_POINT ( 'NONE',  ( 20.74625933824090396, 8.882913521095439080, -75.55517102412177621 ) ) ;
#72415 = EDGE_CURVE ( 'NONE', #9008, #117471, #152729, .T. ) ;
#72416 = DIRECTION ( 'NONE',  ( -1.073024830501117725E-15, 0.000000000000000000, 1.000000000000000000 ) ) ;
#72417 = ADVANCED_FACE ( 'NONE', ( #219824 ), #65201, .F. ) ;
#72418 = ORIENTED_EDGE ( 'NONE', *, *, #160584, .T. ) ;
#72419 = DIRECTION ( 'NONE',  ( -0.000000000000000000, -0.000000000000000000, 1.000000000000000000 ) ) ;
#72420 = DIRECTION ( 'NONE',  ( 0.000000000000000000, -1.000000000000000000, 0.000000000000000000 ) ) ;
#72421 = CARTESIAN_POINT ( 'NONE',  ( 20.94999999999999929, 46.45388641681647357, -243.1520440498138385 ) ) ;
#72422 = ORIENTED_EDGE ( 'NONE', *, *, #134239, .F. ) ;
#72423 = B_SPLINE_CURVE_WITH_KNOTS ( 'NONE', 3,
 ( #145983, #187709, #144693, #165573, #245094, #48168, #169452 ),
 .UNSPECIFIED., .F., .F.,
 ( 4, 3, 4 ),
 ( 0.000000000000000000, 0.0007844235214594318627, 0.001767853679404347454 ),
 .UNSPECIFIED. ) ;
#72424 = CARTESIAN_POINT ( 'NONE',  ( 23.24999999999999645, 67.23127455305841238, -235.8551265064783991 ) ) ;
#72425 = DIRECTION ( 'NONE',  ( 0.000000000000000000, 0.6728971962616792091, -0.7397360091702790408 ) ) ;
#72426 = DIRECTION ( 'NONE',  ( 0.5932847527679310229, 0.8049926720990042694, 5.621233785078285907E-15 ) ) ;
#72427 = ORIENTED_EDGE ( 'NONE', *, *, #178239, .T. ) ;
#72428 = ORIENTED_EDGE ( 'NONE', *, *, #253693, .F. ) ;
#72429 = CIRCLE ( 'NONE', #10043, 0.09999999999999843736 ) ;
#72430 = DIRECTION ( 'NONE',  ( 0.000000000000000000, -1.000000000000000000, 0.000000000000000000 ) ) ;
#72431 = DIRECTION ( 'NONE',  ( -1.000000000000000000, -0.000000000000000000, -0.000000000000000000 ) ) ;
#72432 = PLANE ( 'NONE',  #19971 ) ;
#72433 = CARTESIAN_POINT ( 'NONE',  ( 18.52928932188133970, 10.27928932188134858, -24.65000000000000213 ) ) ;
#72434 = ORIENTED_EDGE ( 'NONE', *, *, #20963, .T. ) ;
#72435 = CARTESIAN_POINT ( 'NONE',  ( 14.11444803880196730, 46.48141361689233975, -234.7877205119061728 ) ) ;
#72436 = CARTESIAN_POINT ( 'NONE',  ( -22.49544290803737212, 64.25012976215484173, -170.0884194437827261 ) ) ;
#72437 = CARTESIAN_POINT ( 'NONE',  ( 23.40000000000005187, 87.50449464844290048, -37.85861909827351468 ) ) ;
#72438 = CIRCLE ( 'NONE', #93256, 0.09999999999999939493 ) ;
#72439 = ADVANCED_FACE ( 'NONE', ( #96018 ), #31915, .T. ) ;
#72441 = ORIENTED_EDGE ( 'NONE', *, *, #7601, .F. ) ;
#72440 = AXIS2_PLACEMENT_3D ( 'NONE', #147209, #170680, #127654 ) ;
#72442 = CARTESIAN_POINT ( 'NONE',  ( 23.14999999999999503, 31.49702336731128582, -233.4564499823349877 ) ) ;
#72443 = AXIS2_PLACEMENT_3D ( 'NONE', #221786, #43188, #103135 ) ;
#72445 = ORIENTED_EDGE ( 'NONE', *, *, #166863, .T. ) ;
#72444 = CARTESIAN_POINT ( 'NONE',  ( -21.44999999999999929, 7.350000000011155166, -54.65000000000000568 ) ) ;
#72446 = FACE_OUTER_BOUND ( 'NONE', #32612, .T. ) ;
#72447 = DIRECTION ( 'NONE',  ( -0.000000000000000000, 1.000000000000000000, -0.000000000000000000 ) ) ;
#72448 = DIRECTION ( 'NONE',  ( 0.000000000000000000, 0.000000000000000000, -1.000000000000000000 ) ) ;
#72449 = LINE ( 'NONE', #148121, #34535 ) ;
#72450 = DIRECTION ( 'NONE',  ( 0.000000000000000000, -0.9915357197604892647, 0.1298341882519715440 ) ) ;
#72451 = ORIENTED_EDGE ( 'NONE', *, *, #63068, .F. ) ;
#72452 = CARTESIAN_POINT ( 'NONE',  ( 21.06277459767449756, 8.872862438268244389, -12.20399919235636155 ) ) ;
#72453 = CARTESIAN_POINT ( 'NONE',  ( 18.59999999999999787, -8.350000000000004974, 10.52591260281975138 ) ) ;
#72454 = DIRECTION ( 'NONE',  ( 0.000000000000000000, 0.000000000000000000, -1.000000000000000000 ) ) ;
#72455 = ORIENTED_EDGE ( 'NONE', *, *, #248985, .T. ) ;
#72456 = CARTESIAN_POINT ( 'NONE',  ( -23.15000000000000213, 64.35000000001275566, -215.2731074845244450 ) ) ;
#72457 = DIRECTION ( 'NONE',  ( 0.000000000000000000, -0.2128009952263744675, 0.9770955615653283965 ) ) ;
#72458 = CARTESIAN_POINT ( 'NONE',  ( 20.94999999999999929, -12.41227409414968541, -30.50000000000000000 ) ) ;
#72459 = DIRECTION ( 'NONE',  ( 0.000000000000000000, 1.000000000000000000, 0.000000000000000000 ) ) ;
#72460 = AXIS2_PLACEMENT_3D ( 'NONE', #140151, #219695, #81449 ) ;
#72461 = EDGE_CURVE ( 'NONE', #231975, #28041, #195167, .T. ) ;
#72462 = CYLINDRICAL_SURFACE ( 'NONE', #42509, 0.09999999999999881206 ) ;
#72463 = TOROIDAL_SURFACE ( 'NONE', #30778, 11.90000000000000213, 0.1000000000000000056 ) ;
#72465 = ORIENTED_EDGE ( 'NONE', *, *, #225709, .T. ) ;
#72464 = VECTOR ( 'NONE', #42710, 1000.000000000000000 ) ;
#72466 = ORIENTED_EDGE ( 'NONE', *, *, #161091, .F. ) ;
#72467 = AXIS2_PLACEMENT_3D ( 'NONE', #91192, #52040, #170780 ) ;
#72468 = CARTESIAN_POINT ( 'NONE',  ( 23.24999999999999645, 1.115600667400684642E-11, -167.4999999999999716 ) ) ;
#72469 = CARTESIAN_POINT ( 'NONE',  ( -17.11825945287481687, 65.95000000001201101, -115.6731074845243796 ) ) ;
#72470 = CARTESIAN_POINT ( 'NONE',  ( -20.97625342178432817, 38.23914636359209851, -236.1324109475626187 ) ) ;
#72471 = DIRECTION ( 'NONE',  ( 0.000000000000000000, -0.4999999999999088507, 0.8660254037844913322 ) ) ;
#72472 = CARTESIAN_POINT ( 'NONE',  ( -21.14999999999999858, 11.75000000001115552, -33.60000000000000142 ) ) ;
#72473 = CIRCLE ( 'NONE', #93296, 0.5999999999999968692 ) ;
#72474 = CIRCLE ( 'NONE', #130712, 0.09999999999998898659 ) ;
#72475 = FACE_OUTER_BOUND ( 'NONE', #251593, .T. ) ;
#72476 = CIRCLE ( 'NONE', #193275, 0.5000000000000004441 ) ;
#72477 = CARTESIAN_POINT ( 'NONE',  ( 20.94999999999999929, 10.38178547072394764, -39.00784536388417223 ) ) ;
#72478 = VECTOR ( 'NONE', #158221, 1000.000000000000000 ) ;
#72479 = CARTESIAN_POINT ( 'NONE',  ( -13.40000000000000213, -8.350000000000004974, 19.04142135623731491 ) ) ;
#72480 = VERTEX_POINT ( 'NONE', #176879 ) ;
#72481 = DIRECTION ( 'NONE',  ( 0.000000000000000000, 0.000000000000000000, -1.000000000000000000 ) ) ;
#72482 = AXIS2_PLACEMENT_3D ( 'NONE', #122631, #17109, #200860 ) ;
#72483 = ORIENTED_EDGE ( 'NONE', *, *, #232254, .T. ) ;
#72484 = CYLINDRICAL_SURFACE ( 'NONE', #230301, 0.5000000000000008882 ) ;
#72485 = CARTESIAN_POINT ( 'NONE',  ( 21.05000000000000071, 10.47338541491290265, -7.578654464248540279 ) ) ;
#72486 = FACE_OUTER_BOUND ( 'NONE', #17127, .T. ) ;
#72488 = AXIS2_PLACEMENT_3D ( 'NONE', #248975, #46889, #187724 ) ;
#72487 = DIRECTION ( 'NONE',  ( 1.000000000000000000, -0.000000000000000000, -0.000000000000000000 ) ) ;
#72489 = CARTESIAN_POINT ( 'NONE',  ( -21.05000000000000071, 69.29912324054878070, -228.2305608266744343 ) ) ;
#72490 = CARTESIAN_POINT ( 'NONE',  ( 18.40000000000000213, 85.50000000001166711, -62.60095763519380796 ) ) ;
#72491 = AXIS2_PLACEMENT_3D ( 'NONE', #221933, #107139, #141153 ) ;
#72492 = DIRECTION ( 'NONE',  ( 2.952720810173289112E-16, -1.000000000000000000, 0.000000000000000000 ) ) ;
#72493 = ORIENTED_EDGE ( 'NONE', *, *, #148438, .F. ) ;
#72495 = CARTESIAN_POINT ( 'NONE',  ( -16.93909480342659890, 22.95463988730850957, -230.8736442518436434 ) ) ;
#72494 = CIRCLE ( 'NONE', #147491, 0.4000000000000010214 ) ;
#72496 = CARTESIAN_POINT ( 'NONE',  ( 21.00000000000000000, 66.25000000001223555, -148.7731074845244450 ) ) ;
#72498 = ADVANCED_FACE ( 'NONE', ( #159882 ), #16517, .T. ) ;
#72497 = DIRECTION ( 'NONE',  ( 1.000000000000000000, 0.000000000000000000, -0.000000000000000000 ) ) ;
#72499 = CARTESIAN_POINT ( 'NONE',  ( -20.94999999999999929, 1.115600667400684642E-11, -62.90000000000001279 ) ) ;
#72500 = DIRECTION ( 'NONE',  ( -3.265361837132813093E-16, 1.000000000000000000, 0.000000000000000000 ) ) ;
#72501 = EDGE_LOOP ( 'NONE', ( #190436, #29049, #216500, #159421 ) ) ;
#72502 = CARTESIAN_POINT ( 'NONE',  ( -21.14999999999994174, 84.00000000001119815, -34.86056257560453986 ) ) ;
#72504 = EDGE_CURVE ( 'NONE', #14704, #134939, #118167, .T. ) ;
#72503 = CARTESIAN_POINT ( 'NONE',  ( -23.25000000000000355, 64.19947762500697763, -225.4487242757812737 ) ) ;
#72505 = ORIENTED_EDGE ( 'NONE', *, *, #33141, .F. ) ;
#72506 = ORIENTED_EDGE ( 'NONE', *, *, #112733, .T. ) ;
#72508 = EDGE_CURVE ( 'NONE', #51580, #47266, #196409, .T. ) ;
#72507 = DIRECTION ( 'NONE',  ( -1.000000000000000000, 0.000000000000000000, 0.000000000000000000 ) ) ;
#72509 = CARTESIAN_POINT ( 'NONE',  ( 21.05000000000000071, 11.16079915604378492, -211.0041093385139561 ) ) ;
#72510 = VECTOR ( 'NONE', #192021, 1000.000000000000000 ) ;
#72511 = VERTEX_POINT ( 'NONE', #120764 ) ;
#72512 = DIRECTION ( 'NONE',  ( 0.000000000000000000, 7.993605777301153912E-15, -1.000000000000000000 ) ) ;
#72513 = CARTESIAN_POINT ( 'NONE',  ( -16.87683809663750978, 9.950000000011137047, -147.4023640181965220 ) ) ;
#72514 = VECTOR ( 'NONE', #92083, 1000.000000000000114 ) ;
#72515 = ADVANCED_FACE ( 'NONE', ( #17758 ), #76459, .T. ) ;
#72517 = ORIENTED_EDGE ( 'NONE', *, *, #26394, .T. ) ;
#72516 = VECTOR ( 'NONE', #11261, 1000.000000000000000 ) ;
#72519 = CARTESIAN_POINT ( 'NONE',  ( 18.59999999999999432, -9.480686695267811714, -174.4411151687578752 ) ) ;
#72518 = VECTOR ( 'NONE', #195720, 1000.000000000000000 ) ;
#72520 = AXIS2_PLACEMENT_3D ( 'NONE', #119839, #199367, #39010 ) ;
#72521 = ORIENTED_EDGE ( 'NONE', *, *, #152497, .T. ) ;
#72522 = FACE_OUTER_BOUND ( 'NONE', #12700, .T. ) ;
#72524 = EDGE_CURVE ( 'NONE', #26818, #114870, #239404, .T. ) ;
#72523 = CYLINDRICAL_SURFACE ( 'NONE', #92032, 0.09999999999999939493 ) ;
#72526 = ORIENTED_EDGE ( 'NONE', *, *, #12477, .T. ) ;
#72525 = CARTESIAN_POINT ( 'NONE',  ( 13.40000000000005898, 67.75000000001118394, -21.02310748452479316 ) ) ;
#72527 = DIRECTION ( 'NONE',  ( -1.000000000000000000, 0.000000000000000000, 0.000000000000000000 ) ) ;
#72528 = AXIS2_PLACEMENT_3D ( 'NONE', #82993, #162588, #242094 ) ;
#72529 = DIRECTION ( 'NONE',  ( 0.000000000000000000, 0.000000000000000000, 1.000000000000000000 ) ) ;
#72530 = CARTESIAN_POINT ( 'NONE',  ( -18.39999999999999858, 85.50000000001168132, -62.92291809330220786 ) ) ;
#72531 = CARTESIAN_POINT ( 'NONE',  ( -20.64999999999999858, 78.50726470275243685, -228.6618886302502176 ) ) ;
#72532 = AXIS2_PLACEMENT_3D ( 'NONE', #17795, #253841, #210880 ) ;
#72533 = DIRECTION ( 'NONE',  ( -3.469446951953635015E-14, 1.000000000000000000, 0.000000000000000000 ) ) ;
#72534 = DIRECTION ( 'NONE',  ( 0.000000000000000000, 0.9999176327611370985, -0.01283462868041289687 ) ) ;
#72535 = CIRCLE ( 'NONE', #26751, 0.09999999999998304689 ) ;
#72537 = VERTEX_POINT ( 'NONE', #80284 ) ;
#72536 = CARTESIAN_POINT ( 'NONE',  ( 18.49999999999999289, 10.20857864377385127, -54.85000000000000142 ) ) ;
#72538 = ORIENTED_EDGE ( 'NONE', *, *, #132290, .F. ) ;
#72540 = CARTESIAN_POINT ( 'NONE',  ( 23.14999999999998437, 80.05000000001268745, -203.5231074845243313 ) ) ;
#72539 = PLANE ( 'NONE',  #120579 ) ;
#72541 = CIRCLE ( 'NONE', #26754, 0.09999999999999939493 ) ;
#72543 = ORIENTED_EDGE ( 'NONE', *, *, #209217, .F. ) ;
#72542 = CYLINDRICAL_SURFACE ( 'NONE', #105856, 0.1000000000000028644 ) ;
#72544 = ORIENTED_EDGE ( 'NONE', *, *, #32710, .T. ) ;
#72545 = CARTESIAN_POINT ( 'NONE',  ( -21.00023020733502221, 1.495312417593689602, -230.7149783752102508 ) ) ;
#72546 = CARTESIAN_POINT ( 'NONE',  ( -22.50000000000000000, 55.89093952297024970, -232.7795287750844579 ) ) ;
#72547 = AXIS2_PLACEMENT_3D ( 'NONE', #40220, #63596, #118461 ) ;
#72548 = DIRECTION ( 'NONE',  ( 0.000000000000000000, 0.4088369013363281623, -0.9126074666063771490 ) ) ;
#72549 = FACE_OUTER_BOUND ( 'NONE', #25738, .T. ) ;
#72550 = LINE ( 'NONE', #42391, #42953 ) ;
#72551 = AXIS2_PLACEMENT_3D ( 'NONE', #154565, #20167, #197496 ) ;
#72552 = CARTESIAN_POINT ( 'NONE',  ( -19.89999999999999858, 1.350000000000000089, 16.60000000000000142 ) ) ;
#72553 = CARTESIAN_POINT ( 'NONE',  ( -16.97683809663752186, 66.15000000001255387, -183.4254715027207396 ) ) ;
#72554 = CIRCLE ( 'NONE', #118344, 0.09999999999999530098 ) ;
#72555 = EDGE_LOOP ( 'NONE', ( #169930, #145772, #203598 ) ) ;
#72556 = ORIENTED_EDGE ( 'NONE', *, *, #198648, .T. ) ;
#72557 = DIRECTION ( 'NONE',  ( 1.000000000000000000, 1.394253735153569469E-16, 2.602809386958778209E-16 ) ) ;
#72558 = VERTEX_POINT ( 'NONE', #99851 ) ;
#72559 = LINE ( 'NONE', #131225, #230137 ) ;
#72560 = ORIENTED_EDGE ( 'NONE', *, *, #241944, .F. ) ;
#72562 = CIRCLE ( 'NONE', #230788, 4.099999999999996980 ) ;
#72561 = DIRECTION ( 'NONE',  ( 0.000000000000000000, -0.1686199900910313187, 0.9856811345164828708 ) ) ;
#72563 = AXIS2_PLACEMENT_3D ( 'NONE', #133208, #154101, #75802 ) ;
#72564 = EDGE_CURVE ( 'NONE', #103201, #224509, #20374, .T. ) ;
#72565 = CIRCLE ( 'NONE', #39453, 0.8750000000000007772 ) ;
#72566 = CARTESIAN_POINT ( 'NONE',  ( -21.44999999999999929, 7.150000000011155876, -79.35000000000005116 ) ) ;
#72567 = CARTESIAN_POINT ( 'NONE',  ( -15.73854595235692244, 66.64858632091065260, -119.5427639169754315 ) ) ;
#72568 = ORIENTED_EDGE ( 'NONE', *, *, #119656, .T. ) ;
#72569 =( REPRESENTATION_RELATIONSHIP ('NONE','NONE', #36900, #90142 ) REPRESENTATION_RELATIONSHIP_WITH_TRANSFORMATION ( #59580 )SHAPE_REPRESENTATION_RELATIONSHIP( ) );
#72571 = EDGE_CURVE ( 'NONE', #197089, #118463, #56869, .T. ) ;
#72570 = CARTESIAN_POINT ( 'NONE',  ( -20.90000000000000213, 8.000000000000000000, -1.212568896937008089 ) ) ;
#72572 = EDGE_LOOP ( 'NONE', ( #30102, #159717, #186017, #51117 ) ) ;
#72573 = CARTESIAN_POINT ( 'NONE',  ( -20.54999999999999716, 7.150000000011155876, -121.6500000000000341 ) ) ;
#72574 = CARTESIAN_POINT ( 'NONE',  ( 21.04999999999999716, 8.894723818389232761, -108.9870843231514783 ) ) ;
#72575 = EDGE_CURVE ( 'NONE', #183349, #116714, #11043, .T. ) ;
#72576 = EDGE_CURVE ( 'NONE', #202387, #175179, #48630, .T. ) ;
#72577 = ORIENTED_EDGE ( 'NONE', *, *, #253733, .T. ) ;
#72578 = CARTESIAN_POINT ( 'NONE',  ( -20.85000000000000142, 36.22724532936083364, -235.9903003947922286 ) ) ;
#72579 = ORIENTED_EDGE ( 'NONE', *, *, #26774, .T. ) ;
#72582 = ORIENTED_EDGE ( 'NONE', *, *, #49799, .F. ) ;
#72581 = SPHERICAL_SURFACE ( 'NONE', #122092, 0.1000000000000000056 ) ;
#72580 = DIRECTION ( 'NONE',  ( 0.000000000000000000, -0.9770955615653291737, -0.2128009952263710536 ) ) ;
#72583 = TOROIDAL_SURFACE ( 'NONE', #138595, 0.2000000000000000111, 0.1000000000000000056 ) ;
#72584 = VECTOR ( 'NONE', #54230, 1000.000000000000114 ) ;
#72585 = DIRECTION ( 'NONE',  ( 0.000000000000000000, 1.000000000000000000, 6.982962677686266711E-15 ) ) ;
#72586 = VECTOR ( 'NONE', #188104, 1000.000000000000000 ) ;
#72587 = ORIENTED_EDGE ( 'NONE', *, *, #184829, .T. ) ;
#72588 = VERTEX_POINT ( 'NONE', #79007 ) ;
#72590 = EDGE_CURVE ( 'NONE', #159923, #217493, #44376, .T. ) ;
#72589 = LINE ( 'NONE', #172997, #3341 ) ;
#72591 = EDGE_LOOP ( 'NONE', ( #103716, #43059, #104997, #94919 ) ) ;
#72592 = EDGE_CURVE ( 'NONE', #11610, #147404, #19426, .T. ) ;
#72593 = CARTESIAN_POINT ( 'NONE',  ( 18.59999999999999787, -14.35849056603774976, -0.4952830188679671064 ) ) ;
#72594 = DIRECTION ( 'NONE',  ( 0.000000000000000000, -6.982962677686266711E-15, 1.000000000000000000 ) ) ;
#72595 = DIRECTION ( 'NONE',  ( -0.000000000000000000, 0.1350103645451807555, 0.9908441862701610203 ) ) ;
#72596 = CARTESIAN_POINT ( 'NONE',  ( -23.15000000000000213, 73.50000000001229239, -156.7984855617622770 ) ) ;
#72597 = EDGE_CURVE ( 'NONE', #41537, #226810, #198475, .T. ) ;
#72598 = LINE ( 'NONE', #191269, #189367 ) ;
#72599 = ORIENTED_EDGE ( 'NONE', *, *, #72787, .F. ) ;
#72600 = CARTESIAN_POINT ( 'NONE',  ( -16.93906926870270624, 44.02196362656498252, -235.2816881676999401 ) ) ;
#72601 = CARTESIAN_POINT ( 'NONE',  ( -21.05315837517722244, 64.24999999299802766, -109.8647514757331294 ) ) ;
#72602 = CARTESIAN_POINT ( 'NONE',  ( 21.08035267497491105, 6.331706839794169817, -33.41731137522386774 ) ) ;
#72603 = ORIENTED_EDGE ( 'NONE', *, *, #179540, .F. ) ;
#72604 = DIRECTION ( 'NONE',  ( 1.000000000000000000, 0.000000000000000000, 0.000000000000000000 ) ) ;
#72605 = VERTEX_POINT ( 'NONE', #101109 ) ;
#72606 = DIRECTION ( 'NONE',  ( 1.000000000000000000, 0.000000000000000000, 0.000000000000000000 ) ) ;
#72607 = EDGE_LOOP ( 'NONE', ( #235326, #161901, #232381, #157702, #21292, #229433, #180593, #62430, #211410, #250564, #152268, #100186, #111103, #244382, #4986, #230974, #13336, #35678, #229741, #206561, #49285, #153285, #99192, #46247, #65915, #152231, #236707 ) ) ;
#72608 = ADVANCED_FACE ( 'NONE', ( #180718 ), #2049, .T. ) ;
#72609 = CIRCLE ( 'NONE', #205859, 0.09999999999999749367 ) ;
#72610 = FACE_OUTER_BOUND ( 'NONE', #91794, .T. ) ;
#72611 = CARTESIAN_POINT ( 'NONE',  ( -18.40000000000000213, 64.25000000001256240, -182.6731074845244507 ) ) ;
#72612 = EDGE_CURVE ( 'NONE', #251611, #5997, #111002, .T. ) ;
#72614 = ORIENTED_EDGE ( 'NONE', *, *, #71435, .F. ) ;
#72613 = CARTESIAN_POINT ( 'NONE',  ( -20.94999999999999929, 1.736257131608553550, -112.0686523290175245 ) ) ;
#72615 = ADVANCED_FACE ( 'NONE', ( #182000 ), #42471, .T. ) ;
#72616 = EDGE_LOOP ( 'NONE', ( #240219, #120544, #209909, #176222 ) ) ;
#72617 = EDGE_CURVE ( 'NONE', #129900, #11577, #256692, .T. ) ;
#72618 = DIRECTION ( 'NONE',  ( 0.000000000000000000, -6.982962677686266711E-15, 1.000000000000000000 ) ) ;
#72619 = CARTESIAN_POINT ( 'NONE',  ( -16.85697194749131711, 9.908543714134740554, -113.4350042676143602 ) ) ;
#72620 = ORIENTED_EDGE ( 'NONE', *, *, #42667, .F. ) ;
#72621 = DIRECTION ( 'NONE',  ( -0.000000000000000000, -0.2128009952263604232, 0.9770955615653316162 ) ) ;
#72622 = CARTESIAN_POINT ( 'NONE',  ( -23.15000000000000213, 64.35000000001180354, -81.67310748452439384 ) ) ;
#72623 = ORIENTED_EDGE ( 'NONE', *, *, #119763, .T. ) ;
#72625 = CARTESIAN_POINT ( 'NONE',  ( -23.25000000000000000, 68.11287320386161070, -224.1382462126928488 ) ) ;
#72624 = CIRCLE ( 'NONE', #135121, 0.5000000000000004441 ) ;
#72626 = VERTEX_POINT ( 'NONE', #205384 ) ;
#72627 = VECTOR ( 'NONE', #31055, 1000.000000000000114 ) ;
#72628 = AXIS2_PLACEMENT_3D ( 'NONE', #92222, #114366, #34857 ) ;
#72629 = CARTESIAN_POINT ( 'NONE',  ( 13.77030915526558630, 9.456007326080463571, -118.9886334941467965 ) ) ;
#72630 = CARTESIAN_POINT ( 'NONE',  ( -20.64999999999999858, 19.91953773510093839, -237.8616849742533077 ) ) ;
#72631 = EDGE_CURVE ( 'NONE', #167145, #238889, #221103, .T. ) ;
#72632 = EDGE_CURVE ( 'NONE', #212292, #208213, #144281, .T. ) ;
#72635 = ORIENTED_EDGE ( 'NONE', *, *, #75259, .T. ) ;
#72634 = ORIENTED_EDGE ( 'NONE', *, *, #87008, .T. ) ;
#72633 = CARTESIAN_POINT ( 'NONE',  ( -21.14999999999999858, 30.68987205111127281, -252.2252246220829193 ) ) ;
#72636 = CARTESIAN_POINT ( 'NONE',  ( 21.30000000000002558, 0.000000000000000000, 0.000000000000000000 ) ) ;
#72637 = CARTESIAN_POINT ( 'NONE',  ( -22.39999999999999858, 64.35000000001166143, -69.62310748452439668 ) ) ;
#72639 = EDGE_CURVE ( 'NONE', #121457, #61914, #15822, .T. ) ;
#72638 = DIRECTION ( 'NONE',  ( -0.000000000000000000, 1.000000000000000000, 6.982962677686267499E-15 ) ) ;
#72640 = AXIS2_PLACEMENT_3D ( 'NONE', #125451, #146278, #225797 ) ;
#72642 = CARTESIAN_POINT ( 'NONE',  ( -14.11361717019515893, 66.54257354752263609, -51.02306561612434876 ) ) ;
#72641 = DIRECTION ( 'NONE',  ( 1.000000000000000000, 0.000000000000000000, 0.000000000000000000 ) ) ;
#72643 = FACE_OUTER_BOUND ( 'NONE', #186946, .T. ) ;
#72644 = CARTESIAN_POINT ( 'NONE',  ( -23.15000000000000213, 10.69888912757691024, -235.6450824654141059 ) ) ;
#72645 = CARTESIAN_POINT ( 'NONE',  ( -21.05000000000000071, -11.48912529306489994, -97.40000000000004832 ) ) ;
#72646 = AXIS2_PLACEMENT_3D ( 'NONE', #151243, #173411, #15596 ) ;
#72647 = CARTESIAN_POINT ( 'NONE',  ( -23.25000000000000000, 0.000000000000000000, -4.049999999999998934 ) ) ;
#72648 = VECTOR ( 'NONE', #195084, 1000.000000000000000 ) ;
#72649 = VERTEX_POINT ( 'NONE', #224949 ) ;
#72650 = EDGE_LOOP ( 'NONE', ( #122072, #185603, #23543, #192937 ) ) ;
#72651 = AXIS2_PLACEMENT_3D ( 'NONE', #7484, #206977, #88279 ) ;
#72652 = FACE_OUTER_BOUND ( 'NONE', #68564, .T. ) ;
#72653 = CIRCLE ( 'NONE', #139242, 5.000000000000000888 ) ;
#72655 = EDGE_LOOP ( 'NONE', ( #96325, #189651, #100486 ) ) ;
#72654 = DIRECTION ( 'NONE',  ( -0.000000000000000000, 0.9126074666063770380, 0.4088369013363281068 ) ) ;
#72656 = EDGE_LOOP ( 'NONE', ( #247641, #233122, #95763 ) ) ;
#72657 = CARTESIAN_POINT ( 'NONE',  ( -20.54999999999999716, 76.00000000001143974, -38.02310748452432421 ) ) ;
#72658 = ORIENTED_EDGE ( 'NONE', *, *, #159760, .F. ) ;
#72659 = CARTESIAN_POINT ( 'NONE',  ( 21.46681500591742520, 33.85532080845636216, -243.2929468148404908 ) ) ;
#72660 = AXIS2_PLACEMENT_3D ( 'NONE', #132032, #92894, #134577 ) ;
#72661 = EDGE_CURVE ( 'NONE', #154428, #241341, #119378, .T. ) ;
#72662 = ORIENTED_EDGE ( 'NONE', *, *, #22304, .F. ) ;
#72663 = CIRCLE ( 'NONE', #35274, 0.09999999999999913125 ) ;
#72664 = PRESENTATION_STYLE_ASSIGNMENT (( #154769 ) ) ;
#72666 = ADVANCED_FACE ( 'NONE', ( #85415 ), #45046, .F. ) ;
#72665 = DIRECTION ( 'NONE',  ( 0.000000000000000000, -0.9126074666063660468, -0.4088369013363524762 ) ) ;
#72667 = CIRCLE ( 'NONE', #81004, 0.1000000000000073330 ) ;
#72669 = EDGE_LOOP ( 'NONE', ( #46250, #101909, #234838, #231925 ) ) ;
#72668 = ORIENTED_EDGE ( 'NONE', *, *, #88881, .F. ) ;
#72670 = ORIENTED_EDGE ( 'NONE', *, *, #122468, .F. ) ;
#72671 = VERTEX_POINT ( 'NONE', #46316 ) ;
#72672 = ORIENTED_EDGE ( 'NONE', *, *, #154914, .T. ) ;
#72673 = EDGE_CURVE ( 'NONE', #26640, #73948, #187152, .T. ) ;
#72675 = LINE ( 'NONE', #174364, #176230 ) ;
#72674 = AXIS2_PLACEMENT_3D ( 'NONE', #16472, #236762, #173001 ) ;
#72676 = PLANE ( 'NONE',  #57345 ) ;
#72677 = DIRECTION ( 'NONE',  ( 1.000000000000000000, 0.000000000000000000, 0.000000000000000000 ) ) ;
#72680 = EDGE_CURVE ( 'NONE', #69777, #24915, #104976, .T. ) ;
#72679 = EDGE_LOOP ( 'NONE', ( #10990, #49029, #17371, #210125 ) ) ;
#72678 = CARTESIAN_POINT ( 'NONE',  ( 18.39999999999999503, 14.17280543801757986, -210.8598471598932349 ) ) ;
#72681 = LINE ( 'NONE', #29708, #144815 ) ;
#72682 = CARTESIAN_POINT ( 'NONE',  ( -18.50000000000000000, 6.846123162352588665, -37.23772626684986164 ) ) ;
#72684 = ORIENTED_EDGE ( 'NONE', *, *, #214145, .F. ) ;
#72683 = DIRECTION ( 'NONE',  ( 1.073024830501117725E-15, -0.000000000000000000, -1.000000000000000000 ) ) ;
#72685 = CARTESIAN_POINT ( 'NONE',  ( -23.25000000000000000, -11.48912529306489994, -164.4000000000000057 ) ) ;
#72686 = ORIENTED_EDGE ( 'NONE', *, *, #16107, .F. ) ;
#72687 = VECTOR ( 'NONE', #231986, 1000.000000000000000 ) ;
#72688 = EDGE_CURVE ( 'NONE', #30925, #162306, #227508, .T. ) ;
#72689 = CARTESIAN_POINT ( 'NONE',  ( 20.94999999999999574, 11.62071067812981795, -127.1315833476590740 ) ) ;
#72690 = ORIENTED_EDGE ( 'NONE', *, *, #88758, .F. ) ;
#72691 = CIRCLE ( 'NONE', #39383, 0.09999999999998898659 ) ;
#72692 = DIRECTION ( 'NONE',  ( 0.000000000000000000, -8.881784197000685330E-16, -1.000000000000000000 ) ) ;
#72693 = CARTESIAN_POINT ( 'NONE',  ( -18.50000000000000000, 74.16465844978715438, -57.96795619196135618 ) ) ;
#72694 = VERTEX_POINT ( 'NONE', #24221 ) ;
#72696 = CARTESIAN_POINT ( 'NONE',  ( -18.50000000000000355, -9.419084502802135717, -140.8299078070255064 ) ) ;
#72695 = DIRECTION ( 'NONE',  ( 0.000000000000000000, -1.000000000000000000, -6.352154140967427193E-15 ) ) ;
#72697 = DIRECTION ( 'NONE',  ( 2.694716079187272946E-16, -1.000000000000000000, 0.000000000000000000 ) ) ;
#72698 = EDGE_CURVE ( 'NONE', #48752, #24784, #84113, .T. ) ;
#72699 = DIRECTION ( 'NONE',  ( 0.000000000000000000, 0.000000000000000000, -1.000000000000000000 ) ) ;
#72700 = ADVANCED_FACE ( 'NONE', ( #184544 ), #206694, .F. ) ;
#72701 = VERTEX_POINT ( 'NONE', #243233 ) ;
#72702 = ORIENTED_EDGE ( 'NONE', *, *, #244760, .F. ) ;
#72703 = CARTESIAN_POINT ( 'NONE',  ( 18.49999999999999289, 58.01113881014391893, -224.9619361160449387 ) ) ;
#72704 = DIRECTION ( 'NONE',  ( 0.000000000000000000, 0.000000000000000000, 1.000000000000000000 ) ) ;
#72705 = VERTEX_POINT ( 'NONE', #204110 ) ;
#72706 = DIRECTION ( 'NONE',  ( -1.000000000000000000, -0.000000000000000000, -0.000000000000000000 ) ) ;
#72707 = ORIENTED_EDGE ( 'NONE', *, *, #130000, .F. ) ;
#72708 = EDGE_CURVE ( 'NONE', #215387, #105012, #173599, .T. ) ;
#72709 = DIRECTION ( 'NONE',  ( 1.000000000000000000, 0.000000000000000000, 0.000000000000000000 ) ) ;
#72710 = DIRECTION ( 'NONE',  ( 1.000000000000000000, -0.000000000000000000, -0.000000000000000000 ) ) ;
#72711 = DIRECTION ( 'NONE',  ( 1.000000000000000000, 0.000000000000000000, 0.000000000000000000 ) ) ;
#72712 = CIRCLE ( 'NONE', #189393, 0.1000000000000055844 ) ;
#72713 = CIRCLE ( 'NONE', #201676, 0.09999999999999938105 ) ;
#72714 = ORIENTED_EDGE ( 'NONE', *, *, #17399, .T. ) ;
#72715 = CARTESIAN_POINT ( 'NONE',  ( -20.64999999999999858, 78.50726470275243685, -228.6618886302502176 ) ) ;
#72716 = FILL_AREA_STYLE ('',( #171825 ) ) ;
#72717 = AXIS2_PLACEMENT_3D ( 'NONE', #52639, #115195, #132190 ) ;
#72718 = EDGE_CURVE ( 'NONE', #79888, #200654, #65894, .T. ) ;
#72719 = VERTEX_POINT ( 'NONE', #81570 ) ;
#72720 = ORIENTED_EDGE ( 'NONE', *, *, #136347, .F. ) ;
#72721 = ORIENTED_EDGE ( 'NONE', *, *, #20814, .F. ) ;
#72722 = AXIS2_PLACEMENT_3D ( 'NONE', #151800, #253430, #16145 ) ;
#72723 = EDGE_CURVE ( 'NONE', #130445, #224041, #181735, .T. ) ;
#72724 = CARTESIAN_POINT ( 'NONE',  ( 20.94999999999999929, 7.128833340094563376, -233.7327013124401276 ) ) ;
#72725 = DIRECTION ( 'NONE',  ( -7.304098846218134667E-16, 0.4088369013363281068, -0.9126074666063770380 ) ) ;
#72726 = AXIS2_PLACEMENT_3D ( 'NONE', #20422, #75274, #217298 ) ;
#72727 = DIRECTION ( 'NONE',  ( 0.000000000000000000, -0.5000000000000016653, 0.8660254037844377084 ) ) ;
#72728 = LINE ( 'NONE', #180790, #240563 ) ;
#72729 = CARTESIAN_POINT ( 'NONE',  ( -18.59999999999999787, -9.499999999988849808, -75.10000000000003695 ) ) ;
#72731 = CARTESIAN_POINT ( 'NONE',  ( 21.05000000000005400, 73.94408376456904364, -49.16694968567509250 ) ) ;
#72730 = DIRECTION ( 'NONE',  ( -1.000000000000000000, 0.000000000000000000, 0.000000000000000000 ) ) ;
#72732 = EDGE_CURVE ( 'NONE', #158852, #252820, #186200, .T. ) ;
#72734 = EDGE_LOOP ( 'NONE', ( #66997, #9098, #116797, #180651, #185936 ) ) ;
#72733 = LINE ( 'NONE', #231789, #6611 ) ;
#72735 = FACE_OUTER_BOUND ( 'NONE', #81372, .T. ) ;
#72736 = ORIENTED_EDGE ( 'NONE', *, *, #246037, .F. ) ;
#72737 = AXIS2_PLACEMENT_3D ( 'NONE', #224785, #25345, #243076 ) ;
#72738 = DIRECTION ( 'NONE',  ( 0.000000000000000000, -0.9856811345164832039, -0.1686199900910280158 ) ) ;
#72739 = ADVANCED_FACE ( 'NONE', ( #227529 ), #211135, .F. ) ;
#72740 = VERTEX_POINT ( 'NONE', #188406 ) ;
#72741 = ORIENTED_EDGE ( 'NONE', *, *, #161868, .F. ) ;
#72742 = DIRECTION ( 'NONE',  ( -4.391705002472929091E-16, 1.000000000000000000, 0.000000000000000000 ) ) ;
#72743 = AXIS2_PLACEMENT_3D ( 'NONE', #21672, #221129, #101144 ) ;
#72744 = CARTESIAN_POINT ( 'NONE',  ( -16.93230518875208190, 10.00075036143099894, -46.07577834810150108 ) ) ;
#72745 = CARTESIAN_POINT ( 'NONE',  ( -16.93935632781549572, 66.01526950028642204, -48.63344673581409694 ) ) ;
#72746 = AXIS2_PLACEMENT_3D ( 'NONE', #202991, #81728, #40109 ) ;
#72747 = DIRECTION ( 'NONE',  ( -0.000000000000000000, 0.000000000000000000, -1.000000000000000000 ) ) ;
#72748 = CIRCLE ( 'NONE', #89258, 0.1000000000000028644 ) ;
#72749 = CARTESIAN_POINT ( 'NONE',  ( 23.15000000000000213, 23.45160524131172153, -253.2535058871250726 ) ) ;
#72750 = VERTEX_POINT ( 'NONE', #230101 ) ;
#72751 = ORIENTED_EDGE ( 'NONE', *, *, #21132, .F. ) ;
#72752 = DIRECTION ( 'NONE',  ( 0.000000000000000000, 0.000000000000000000, 1.000000000000000000 ) ) ;
#72754 = EDGE_CURVE ( 'NONE', #231809, #112979, #19614, .T. ) ;
#72753 = ORIENTED_EDGE ( 'NONE', *, *, #209491, .F. ) ;
#72755 = DIRECTION ( 'NONE',  ( 7.304098846218134667E-16, 0.4088369013363281068, -0.9126074666063770380 ) ) ;
#72756 = CARTESIAN_POINT ( 'NONE',  ( -18.59999999999999787, 1.115600667400684642E-11, -100.5000000000000426 ) ) ;
#72757 = ORIENTED_EDGE ( 'NONE', *, *, #206753, .F. ) ;
#72758 = FACE_OUTER_BOUND ( 'NONE', #62696, .T. ) ;
#72760 = CIRCLE ( 'NONE', #93567, 0.1000000000000028644 ) ;
#72759 = DIRECTION ( 'NONE',  ( 1.000000000000000000, 3.265361837132813093E-16, -0.000000000000000000 ) ) ;
#72761 = CARTESIAN_POINT ( 'NONE',  ( -21.05000000000000782, 6.100991474439140028, -199.6040273627268107 ) ) ;
#72762 = CARTESIAN_POINT ( 'NONE',  ( 21.06089410995835109, 65.27470446788869651, -157.8207267534812104 ) ) ;
#72763 = VERTEX_POINT ( 'NONE', #128439 ) ;
#72764 = CARTESIAN_POINT ( 'NONE',  ( 23.14999999999999858, 71.22429906543317202, -191.6743393804784148 ) ) ;
#72765 = CARTESIAN_POINT ( 'NONE',  ( -16.93433913041102912, 65.99402157848805928, -115.5877420571292049 ) ) ;
#72766 = DIRECTION ( 'NONE',  ( 0.000000000000000000, 1.000000000000000000, -1.224646799147353207E-16 ) ) ;
#72767 = AXIS2_PLACEMENT_3D ( 'NONE', #102117, #4318, #1748 ) ;
#72768 = LINE ( 'NONE', #36190, #37356 ) ;
#72769 = CARTESIAN_POINT ( 'NONE',  ( -20.94684162445269848, 57.68176035244419353, -226.1764194146458635 ) ) ;
#72770 = VECTOR ( 'NONE', #92511, 1000.000000000000000 ) ;
#72771 = AXIS2_PLACEMENT_3D ( 'NONE', #237159, #79340, #158924 ) ;
#72772 = ORIENTED_EDGE ( 'NONE', *, *, #76734, .F. ) ;
#72773 = VECTOR ( 'NONE', #62851, 1000.000000000000000 ) ;
#72775 = ADVANCED_FACE ( 'NONE', ( #131003 ), #207997, .T. ) ;
#72774 = CARTESIAN_POINT ( 'NONE',  ( 21.08804281139606118, 10.62183430184116339, -12.34999996737854566 ) ) ;
#72776 = ORIENTED_EDGE ( 'NONE', *, *, #13214, .T. ) ;
#72777 = CARTESIAN_POINT ( 'NONE',  ( -2.995603634470891112E-16, 87.75000000001199396, -115.2731074845242176 ) ) ;
#72778 = CARTESIAN_POINT ( 'NONE',  ( -20.94999999999999929, 0.6656436123793491033, -212.6810495496487476 ) ) ;
#72779 = CARTESIAN_POINT ( 'NONE',  ( -16.80469485234340610, 66.05784833687079072, -82.21314064059320970 ) ) ;
#72780 = LINE ( 'NONE', #170618, #143794 ) ;
#72781 = PLANE ( 'NONE',  #153038 ) ;
#72782 = VERTEX_POINT ( 'NONE', #249677 ) ;
#72783 = DIRECTION ( 'NONE',  ( 0.000000000000000000, 0.2617529984165031243, 0.9651348961777157509 ) ) ;
#72784 = CARTESIAN_POINT ( 'NONE',  ( 20.94999999999999574, 18.18127959618848521, -237.5711165786817389 ) ) ;
#72785 = LINE ( 'NONE', #152317, #60645 ) ;
#72786 = CARTESIAN_POINT ( 'NONE',  ( 21.14999999999999858, 10.71339244341104013, -79.35000000000005116 ) ) ;
#72787 = EDGE_CURVE ( 'NONE', #191564, #16721, #248545, .T. ) ;
#72788 = CIRCLE ( 'NONE', #256032, 0.09999999999999939493 ) ;
#72789 = CYLINDRICAL_SURFACE ( 'NONE', #244682, 0.8750000000000007772 ) ;
#72790 = ORIENTED_EDGE ( 'NONE', *, *, #151220, .F. ) ;
#72791 = EDGE_LOOP ( 'NONE', ( #153003, #79241, #52437, #30197 ) ) ;
#72792 = FACE_OUTER_BOUND ( 'NONE', #192560, .T. ) ;
#72793 = CARTESIAN_POINT ( 'NONE',  ( 20.85000000000000142, 64.35000000001218723, -143.3069731475025037 ) ) ;
#72795 = CARTESIAN_POINT ( 'NONE',  ( -23.25000000000000000, 1.115600667400684642E-11, -100.5000000000000284 ) ) ;
#72794 = AXIS2_PLACEMENT_3D ( 'NONE', #194357, #191791, #253009 ) ;
#72796 = CARTESIAN_POINT ( 'NONE',  ( 22.57320508075687115, 11.75000000001115552, -33.50000000000000000 ) ) ;
#72797 = EDGE_LOOP ( 'NONE', ( #97019, #256956, #43378, #88594 ) ) ;
#72798 = LINE ( 'NONE', #152332, #59637 ) ;
#72799 = DIRECTION ( 'NONE',  ( 0.000000000000000000, 0.000000000000000000, -1.000000000000000000 ) ) ;
#72800 = ORIENTED_EDGE ( 'NONE', *, *, #7528, .F. ) ;
#72801 = LINE ( 'NONE', #134016, #38098 ) ;
#72802 = DIRECTION ( 'NONE',  ( 1.186688945009009831E-16, -1.000000000000000000, 0.000000000000000000 ) ) ;
#72803 = AXIS2_PLACEMENT_3D ( 'NONE', #235165, #173953, #253423 ) ;
#72804 = AXIS2_PLACEMENT_3D ( 'NONE', #142450, #85018, #6796 ) ;
#72805 = ORIENTED_EDGE ( 'NONE', *, *, #82829, .F. ) ;
#72807 = ORIENTED_EDGE ( 'NONE', *, *, #76890, .F. ) ;
#72806 = DIRECTION ( 'NONE',  ( -1.000000000000000000, 0.000000000000000000, 0.000000000000000000 ) ) ;
#72808 = EDGE_LOOP ( 'NONE', ( #48634, #252100, #130184, #158287 ) ) ;
#72809 = DIRECTION ( 'NONE',  ( 0.000000000000000000, -0.2617529984165032908, -0.9651348961777156399 ) ) ;
#72810 = CARTESIAN_POINT ( 'NONE',  ( -21.44999999999999929, 29.28400589394459530, -237.3759593473670293 ) ) ;
#72811 = DIRECTION ( 'NONE',  ( 1.000000000000000000, 0.000000000000000000, 0.000000000000000000 ) ) ;
#72812 = DIRECTION ( 'NONE',  ( 0.000000000000000000, -0.4088369013363280513, 0.9126074666063769270 ) ) ;
#72813 = DIRECTION ( 'NONE',  ( 0.000000000000000000, 0.000000000000000000, 1.000000000000000000 ) ) ;
#72814 = DIRECTION ( 'NONE',  ( -1.000000000000000000, 0.000000000000000000, -0.000000000000000000 ) ) ;
#72815 = EDGE_CURVE ( 'NONE', #144794, #136985, #244441, .T. ) ;
#72816 = DIRECTION ( 'NONE',  ( 2.879366945564059217E-14, -0.6052030477779082318, -0.7960711469211348978 ) ) ;
#72818 = DIRECTION ( 'NONE',  ( 0.000000000000000000, -0.9553114395362733990, 0.2956011730205631016 ) ) ;
#72817 = CARTESIAN_POINT ( 'NONE',  ( 20.94999999999999574, 10.47338541492405994, -108.0786544642485865 ) ) ;
#72819 = CYLINDRICAL_SURFACE ( 'NONE', #154524, 0.1000000000000070832 ) ;
#72820 = CARTESIAN_POINT ( 'NONE',  ( 21.05000000000000071, 1.148907358139439339E-11, -201.0000000000015064 ) ) ;
#72821 = CARTESIAN_POINT ( 'NONE',  ( -20.94999999999999929, 1.115600667400684642E-11, -67.00000000000004263 ) ) ;
#72823 = CARTESIAN_POINT ( 'NONE',  ( -21.05000000000000071, 1.115600667400684642E-11, -134.0000000000000284 ) ) ;
#72822 = CIRCLE ( 'NONE', #218502, 0.1000000000000106498 ) ;
#72824 = ORIENTED_EDGE ( 'NONE', *, *, #176735, .T. ) ;
#72825 = VECTOR ( 'NONE', #9329, 1000.000000000000000 ) ;
#72826 = CARTESIAN_POINT ( 'NONE',  ( -18.46154800491006398, -9.480206274242036102, -40.15745083838135798 ) ) ;
#72827 = DIRECTION ( 'NONE',  ( 0.000000000000000000, -1.000000000000000000, -6.352154140967427193E-15 ) ) ;
#72829 = CARTESIAN_POINT ( 'NONE',  ( 20.05000000000002913, 7.250000000011171508, -154.8500000000000227 ) ) ;
#72828 = CIRCLE ( 'NONE', #206070, 0.09999999999999123479 ) ;
#72830 = CIRCLE ( 'NONE', #147818, 0.09999999999999939493 ) ;
#72831 = DIRECTION ( 'NONE',  ( -0.000000000000000000, 0.4791956752371485107, 0.8777080977375185666 ) ) ;
#72833 = EDGE_CURVE ( 'NONE', #213752, #120974, #213104, .T. ) ;
#72832 = DIRECTION ( 'NONE',  ( 1.000000000000000000, 0.000000000000000000, 0.000000000000000000 ) ) ;
#72834 = DIRECTION ( 'NONE',  ( -0.000000000000000000, 0.9126074666063770380, 0.4088369013363281068 ) ) ;
#72835 = VERTEX_POINT ( 'NONE', #11060 ) ;
#72836 = ORIENTED_EDGE ( 'NONE', *, *, #161557, .F. ) ;
#72837 = EDGE_CURVE ( 'NONE', #189461, #192398, #136090, .T. ) ;
#72838 = FACE_OUTER_BOUND ( 'NONE', #71535, .T. ) ;
#72839 = ORIENTED_EDGE ( 'NONE', *, *, #196100, .T. ) ;
#72840 = CARTESIAN_POINT ( 'NONE',  ( 21.05000000000000071, 70.60000000001149090, -45.91707660717680284 ) ) ;
#72841 = DIRECTION ( 'NONE',  ( 0.000000000000000000, 0.8490545835447254053, 0.5283051335749948674 ) ) ;
#72842 = EDGE_CURVE ( 'NONE', #251542, #30528, #50170, .T. ) ;
#72843 = CIRCLE ( 'NONE', #97721, 0.09999999999998898659 ) ;
#72844 = VECTOR ( 'NONE', #153775, 1000.000000000000000 ) ;
#72845 = TOROIDAL_SURFACE ( 'NONE', #101823, 11.90000000000000391, 0.1000000000000000056 ) ;
#72846 = VECTOR ( 'NONE', #105470, 1000.000000000000000 ) ;
#72847 = EDGE_LOOP ( 'NONE', ( #67425, #173209, #162790, #112674 ) ) ;
#72848 = DIRECTION ( 'NONE',  ( -0.000000000000000000, -6.982962677686266711E-15, 1.000000000000000000 ) ) ;
#72849 = ORIENTED_EDGE ( 'NONE', *, *, #248251, .F. ) ;
#72850 = EDGE_CURVE ( 'NONE', #76616, #34898, #118321, .T. ) ;
#72851 = CARTESIAN_POINT ( 'NONE',  ( -20.54999999999999716, -8.999999999988844479, -124.5060308773475839 ) ) ;
#72852 = CARTESIAN_POINT ( 'NONE',  ( 20.95512828230159030, 67.12384868768677393, -124.3206772190210074 ) ) ;
#72854 = CIRCLE ( 'NONE', #172831, 11.64999999999999325 ) ;
#72853 = DIRECTION ( 'NONE',  ( 1.000000000000000000, 3.265361837132813093E-16, -0.000000000000000000 ) ) ;
#72856 = CARTESIAN_POINT ( 'NONE',  ( -16.87683809663752399, 21.23804903844422043, -79.65000000000004832 ) ) ;
#72855 = AXIS2_PLACEMENT_3D ( 'NONE', #175785, #140473, #197884 ) ;
#72857 = DIRECTION ( 'NONE',  ( 0.000000000000000000, 0.1350103645451904977, -0.9908441862701596881 ) ) ;
#72859 = AXIS2_PLACEMENT_3D ( 'NONE', #216840, #236411, #173925 ) ;
#72858 = LINE ( 'NONE', #28621, #240481 ) ;
#72860 = EDGE_CURVE ( 'NONE', #146300, #63364, #73087, .T. ) ;
#72861 = DIRECTION ( 'NONE',  ( 1.000000000000000000, -0.000000000000000000, -0.000000000000000000 ) ) ;
#72862 = CARTESIAN_POINT ( 'NONE',  ( -22.39999999999999858, 64.25313205997782973, -247.2214437328673853 ) ) ;
#72864 = ORIENTED_EDGE ( 'NONE', *, *, #179618, .F. ) ;
#72863 = CARTESIAN_POINT ( 'NONE',  ( -20.64999999999999858, 1.115600667400684642E-11, -200.9999999999999432 ) ) ;
#72866 = DIRECTION ( 'NONE',  ( 1.000000000000000000, 7.049440681616512959E-16, -1.911869773728115455E-16 ) ) ;
#72865 = LINE ( 'NONE', #12884, #145296 ) ;
#72867 = AXIS2_PLACEMENT_3D ( 'NONE', #75916, #57616, #135864 ) ;
#72868 = EDGE_LOOP ( 'NONE', ( #74593, #221773, #145715, #95195 ) ) ;
#72870 = ORIENTED_EDGE ( 'NONE', *, *, #190772, .F. ) ;
#72869 = DIRECTION ( 'NONE',  ( 0.000000000000000000, 0.2128009952263485993, -0.9770955615653341697 ) ) ;
#72871 = ORIENTED_EDGE ( 'NONE', *, *, #135989, .T. ) ;
#72872 = DIRECTION ( 'NONE',  ( 0.5932847527679310229, 0.8049926720990042694, 5.621233785078285907E-15 ) ) ;
#72873 = LINE ( 'NONE', #87246, #117854 ) ;
#72874 = CIRCLE ( 'NONE', #202018, 0.09999999999999693856 ) ;
#72875 = CIRCLE ( 'NONE', #97747, 0.09999999999998898659 ) ;
#72876 = DIRECTION ( 'NONE',  ( 0.000000000000000000, -6.467318590049456648E-15, 1.000000000000000000 ) ) ;
#72877 = CARTESIAN_POINT ( 'NONE',  ( 18.39999999999999858, -9.500000000000000000, -7.032069396699673014 ) ) ;
#72878 = CARTESIAN_POINT ( 'NONE',  ( 20.94999999999999574, 1.261786168565025568, -8.086498963545480478 ) ) ;
#72879 = VECTOR ( 'NONE', #212756, 1000.000000000000000 ) ;
#72880 = DIRECTION ( 'NONE',  ( 0.000000000000000000, 0.000000000000000000, 1.000000000000000000 ) ) ;
#72881 = CIRCLE ( 'NONE', #102036, 7.791421356237317575 ) ;
#72882 = CARTESIAN_POINT ( 'NONE',  ( -16.91256925476571027, 12.42391174447540081, -211.1203373714319014 ) ) ;
#72883 = EDGE_CURVE ( 'NONE', #221901, #187906, #165351, .T. ) ;
#72884 = CARTESIAN_POINT ( 'NONE',  ( -22.59999999999999787, 11.36146383068193444, -198.4232501820394816 ) ) ;
#72885 = EDGE_LOOP ( 'NONE', ( #170916, #91452, #247658, #157186, #81616 ) ) ;
#72886 = ORIENTED_EDGE ( 'NONE', *, *, #29103, .T. ) ;
#72887 = DIRECTION ( 'NONE',  ( -0.000000000000000000, -6.982962677686266711E-15, 1.000000000000000000 ) ) ;
#72888 = EDGE_LOOP ( 'NONE', ( #214491, #254100, #183515 ) ) ;
#72889 = SPHERICAL_SURFACE ( 'NONE', #5070, 0.1000000000000000056 ) ;
#72890 = VERTEX_POINT ( 'NONE', #54032 ) ;
#72891 = DIRECTION ( 'NONE',  ( 0.000000000000000000, 0.000000000000000000, 1.000000000000000000 ) ) ;
#72892 = ADVANCED_FACE ( 'NONE', ( #30646 ), #133571, .T. ) ;
#72893 = DIRECTION ( 'NONE',  ( -1.020425574104004196E-15, 6.982962677686266711E-15, -1.000000000000000000 ) ) ;
#72894 = DIRECTION ( 'NONE',  ( 1.000000000000000000, 0.000000000000000000, 0.000000000000000000 ) ) ;
#72895 = CARTESIAN_POINT ( 'NONE',  ( 22.24259225415828922, 75.90093411655990963, -211.0150453550897680 ) ) ;
#72896 = ORIENTED_EDGE ( 'NONE', *, *, #204674, .T. ) ;
#72898 = EDGE_CURVE ( 'NONE', #225466, #17954, #11229, .T. ) ;
#72897 = DIRECTION ( 'NONE',  ( -1.000000000000000000, -0.000000000000000000, -0.000000000000000000 ) ) ;
#72899 = VECTOR ( 'NONE', #41427, 1000.000000000000000 ) ;
#72900 = CARTESIAN_POINT ( 'NONE',  ( 13.99999999999999822, 66.15000000001258229, -186.7731074845244450 ) ) ;
#72901 = AXIS2_PLACEMENT_3D ( 'NONE', #208243, #105221, #46564 ) ;
#72902 = CYLINDRICAL_SURFACE ( 'NONE', #150558, 0.09999999999999939493 ) ;
#72903 = CARTESIAN_POINT ( 'NONE',  ( -20.94999999999994600, 87.75000000001119815, -4.623107484524796362 ) ) ;
#72904 = EDGE_CURVE ( 'NONE', #67839, #86769, #68472, .T. ) ;
#72905 = AXIS2_PLACEMENT_3D ( 'NONE', #143735, #230670, #170741 ) ;
#72906 = EDGE_LOOP ( 'NONE', ( #20521, #144534, #126974 ) ) ;
#72908 = DIRECTION ( 'NONE',  ( -3.265361837132813586E-16, 0.9770955615653357240, 0.2128009952263412996 ) ) ;
#72907 = PLANE ( 'NONE',  #83294 ) ;
#72909 = VERTEX_POINT ( 'NONE', #60440 ) ;
#72912 = ORIENTED_EDGE ( 'NONE', *, *, #151544, .F. ) ;
#72911 = DIRECTION ( 'NONE',  ( 0.000000000000000000, 0.000000000000000000, -1.000000000000000000 ) ) ;
#72910 = DIRECTION ( 'NONE',  ( 0.000000000000000000, 6.982962677686266711E-15, -1.000000000000000000 ) ) ;
#72913 = EDGE_CURVE ( 'NONE', #118880, #125620, #214390, .T. ) ;
#72914 = CARTESIAN_POINT ( 'NONE',  ( -20.54999999999999716, 85.00000000001149658, -45.51707660717670478 ) ) ;
#72915 = AXIS2_PLACEMENT_3D ( 'NONE', #154088, #114914, #131907 ) ;
#72916 = CARTESIAN_POINT ( 'NONE',  ( 21.14999999999999503, 1.148907358139439339E-11, -201.0000000000015064 ) ) ;
#72917 = CIRCLE ( 'NONE', #218598, 12.87499999999999467 ) ;
#72918 = ORIENTED_EDGE ( 'NONE', *, *, #195040, .F. ) ;
#72919 = CARTESIAN_POINT ( 'NONE',  ( 23.04999999999999716, 67.17743825834540417, -82.17310748452437963 ) ) ;
#72921 = EDGE_CURVE ( 'NONE', #165093, #151955, #240369, .T. ) ;
#72920 = FACE_OUTER_BOUND ( 'NONE', #254478, .T. ) ;
#72922 = CARTESIAN_POINT ( 'NONE',  ( -21.05000000000000071, 7.128833340094563376, -233.7327013124401276 ) ) ;
#72924 = ORIENTED_EDGE ( 'NONE', *, *, #107757, .T. ) ;
#72923 = DIRECTION ( 'NONE',  ( 0.000000000000000000, 0.8814952561688430555, -0.4721928772777346239 ) ) ;
#72925 = AXIS2_PLACEMENT_3D ( 'NONE', #13362, #113735, #208981 ) ;
#72926 = EDGE_CURVE ( 'NONE', #40304, #120532, #158311, .T. ) ;
#72927 = EDGE_CURVE ( 'NONE', #206343, #230076, #115291, .T. ) ;
#72928 = AXIS2_PLACEMENT_3D ( 'NONE', #30382, #89040, #225955 ) ;
#72929 = VERTEX_POINT ( 'NONE', #177858 ) ;
#72930 = CYLINDRICAL_SURFACE ( 'NONE', #245198, 0.1000000000000124678 ) ;
#72931 = CARTESIAN_POINT ( 'NONE',  ( 18.47073956224748770, -9.471729412460723196, -74.10868575281796211 ) ) ;
#72932 = SPHERICAL_SURFACE ( 'NONE', #2143, 0.1000000000000000056 ) ;
#72933 = CARTESIAN_POINT ( 'NONE',  ( -18.59999999999999787, 11.64999999999999680, -21.35000000000000142 ) ) ;
#72934 = EDGE_LOOP ( 'NONE', ( #241309, #238129, #154777, #234126 ) ) ;
#72935 = DIRECTION ( 'NONE',  ( -1.000000000000000000, -1.652117596168391700E-15, -1.153667551319263085E-29 ) ) ;
#72936 = EDGE_CURVE ( 'NONE', #163036, #223382, #256028, .T. ) ;
#72937 = LINE ( 'NONE', #75495, #1603 ) ;
#72938 = CARTESIAN_POINT ( 'NONE',  ( 20.85000000000000142, 7.675662554762638479, -241.7139905447625381 ) ) ;
#72939 = AXIS2_PLACEMENT_3D ( 'NONE', #132244, #211793, #129673 ) ;
#72940 = EDGE_LOOP ( 'NONE', ( #215392, #168128, #190308, #85780 ) ) ;
#72941 = CARTESIAN_POINT ( 'NONE',  ( 20.87631937322885278, 59.10889048783243993, -225.7987040349840697 ) ) ;
#72942 = ADVANCED_FACE ( 'NONE', ( #138669 ), #119516, .F. ) ;
#72943 = LINE ( 'NONE', #151173, #251315 ) ;
#72944 = ORIENTED_EDGE ( 'NONE', *, *, #160425, .F. ) ;
#72945 = CARTESIAN_POINT ( 'NONE',  ( -23.25000000000000000, 67.23127455305835554, -235.8551265064784559 ) ) ;
#72946 = CARTESIAN_POINT ( 'NONE',  ( -23.25000000000000000, 68.97833521811179480, -99.18954208262705663 ) ) ;
#72947 = CIRCLE ( 'NONE', #218643, 0.09999999999999939493 ) ;
#72948 = VERTEX_POINT ( 'NONE', #38338 ) ;
#72949 = VECTOR ( 'NONE', #208160, 1000.000000000000114 ) ;
#72950 = EDGE_LOOP ( 'NONE', ( #160845, #226507, #155347, #36909, #223444 ) ) ;
#72951 = CARTESIAN_POINT ( 'NONE',  ( -21.45000000000000284, 68.29142135624984178, -182.2731074845244166 ) ) ;
#72952 = ORIENTED_EDGE ( 'NONE', *, *, #103292, .F. ) ;
#72954 = ORIENTED_EDGE ( 'NONE', *, *, #250921, .F. ) ;
#72953 = DIRECTION ( 'NONE',  ( -1.000000000000000000, 0.000000000000000000, 0.000000000000000000 ) ) ;
#72955 = ADVANCED_FACE ( 'NONE', ( #40925 ), #86204, .T. ) ;
#72956 = EDGE_CURVE ( 'NONE', #49183, #79239, #136108, .T. ) ;
#72957 = ORIENTED_EDGE ( 'NONE', *, *, #148933, .T. ) ;
#72960 = EDGE_LOOP ( 'NONE', ( #180258, #207085, #31545, #183311 ) ) ;
#72959 = VERTEX_POINT ( 'NONE', #96969 ) ;
#72958 = DIRECTION ( 'NONE',  ( -1.000000000000000000, 3.854941057726231589E-15, 0.000000000000000000 ) ) ;
#72962 = EDGE_CURVE ( 'NONE', #125125, #43174, #223581, .T. ) ;
#72961 = CARTESIAN_POINT ( 'NONE',  ( 21.05000000000000071, 6.350000000000004974, -9.843822089683129661 ) ) ;
#72963 = ORIENTED_EDGE ( 'NONE', *, *, #13854, .F. ) ;
#72964 = CARTESIAN_POINT ( 'NONE',  ( -22.50000000000000000, 11.75000000001115552, -167.4999999999999716 ) ) ;
#72965 = CARTESIAN_POINT ( 'NONE',  ( -20.94999999999999929, 1.736257131608553550, -45.06865232901750318 ) ) ;
#72966 = LINE ( 'NONE', #131616, #93025 ) ;
#72967 = CARTESIAN_POINT ( 'NONE',  ( 18.59999999999999787, 64.14105355761505223, -250.1147034356626193 ) ) ;
#72968 = DIRECTION ( 'NONE',  ( -1.000000000000000000, -2.952720810173289112E-16, 0.000000000000000000 ) ) ;
#72969 = ORIENTED_EDGE ( 'NONE', *, *, #285, .F. ) ;
#72970 = EDGE_LOOP ( 'NONE', ( #166366, #35497, #174007, #199531 ) ) ;
#72971 = ORIENTED_EDGE ( 'NONE', *, *, #61826, .T. ) ;
#72972 = CYLINDRICAL_SURFACE ( 'NONE', #187325, 0.09999999999999939493 ) ;
#72973 = VECTOR ( 'NONE', #226714, 1000.000000000000000 ) ;
#72974 =( BOUNDED_SURFACE ( )  B_SPLINE_SURFACE ( 3, 2, ( 
 ( #143350, #181222, #179934 ),
 ( #220344, #203340, #243741 ),
 ( #219030, #121274, #241194 ),
 ( #139492, #84619, #159096 ) ),
 .UNSPECIFIED., .F., .F., .F. ) 
 B_SPLINE_SURFACE_WITH_KNOTS ( ( 4, 4 ),
 ( 3, 3 ),
 ( 0.0008258556059633821332, 0.0009616864997633045326 ),
 ( 0.000000000000000000, 1.000000000000000000 ),
 .UNSPECIFIED. ) 
 GEOMETRIC_REPRESENTATION_ITEM ( )  RATIONAL_B_SPLINE_SURFACE ( (
 ( 1.000000000000000000, 0.9152888060719758245, 1.000000000000000000),
 ( 1.000000000000000000, 0.9327727094137872044, 1.000000000000000000),
 ( 1.000000000000000000, 0.9369023509258540550, 1.000000000000000000),
 ( 1.000000000000000000, 0.9246339933864557992, 1.000000000000000000) ) ) 
 REPRESENTATION_ITEM ( '' )  SURFACE ( )  );
#72976 = ORIENTED_EDGE ( 'NONE', *, *, #33807, .T. ) ;
#72975 = CARTESIAN_POINT ( 'NONE',  ( -20.85000000000000142, 1.115600667400684642E-11, -208.8999999999999488 ) ) ;
#72977 = DIRECTION ( 'NONE',  ( -1.000000000000000000, -0.000000000000000000, -0.000000000000000000 ) ) ;
#72979 = VERTEX_POINT ( 'NONE', #141276 ) ;
#72978 = FACE_OUTER_BOUND ( 'NONE', #157253, .T. ) ;
#72980 = EDGE_LOOP ( 'NONE', ( #218372, #227498, #43448 ) ) ;
#72981 = CARTESIAN_POINT ( 'NONE',  ( -18.49999999999999645, -0.6211011429738022560, -242.4105644729049232 ) ) ;
#72982 = EDGE_CURVE ( 'NONE', #154033, #135761, #252815, .T. ) ;
#72983 = ORIENTED_EDGE ( 'NONE', *, *, #165912, .F. ) ;
#72984 = CARTESIAN_POINT ( 'NONE',  ( -16.89797118371622275, 66.02361927736751568, -149.0858141169672706 ) ) ;
#72986 = EDGE_CURVE ( 'NONE', #254423, #100756, #202753, .T. ) ;
#72985 = DIRECTION ( 'NONE',  ( 0.000000000000000000, -0.000000000000000000, 1.000000000000000000 ) ) ;
#72987 = B_SPLINE_CURVE_WITH_KNOTS ( 'NONE', 3,
 ( #236949, #115722, #183083, #235653, #197813, #56995 ),
 .UNSPECIFIED., .F., .F.,
 ( 4, 2, 4 ),
 ( 0.000000000000000000, 0.0001496588209255806561, 0.0002993176418511613122 ),
 .UNSPECIFIED. ) ;
#72990 = VERTEX_POINT ( 'NONE', #63013 ) ;
#72989 = ORIENTED_EDGE ( 'NONE', *, *, #66424, .F. ) ;
#72988 = VECTOR ( 'NONE', #218495, 1000.000000000000000 ) ;
#72991 = VECTOR ( 'NONE', #196839, 1000.000000000000000 ) ;
#72992 = VERTEX_POINT ( 'NONE', #66877 ) ;
#72993 = DIRECTION ( 'NONE',  ( -0.000000000000000000, 0.9126074666063770380, 0.4088369013363281068 ) ) ;
#72994 = ORIENTED_EDGE ( 'NONE', *, *, #40001, .F. ) ;
#72995 = EDGE_LOOP ( 'NONE', ( #236793, #210182, #30274, #40662 ) ) ;
#72996 = FACE_OUTER_BOUND ( 'NONE', #233762, .T. ) ;
#72999 = ADVANCED_FACE ( 'NONE', ( #220808 ), #81273, .F. ) ;
#72998 = ORIENTED_EDGE ( 'NONE', *, *, #131888, .F. ) ;
#72997 = CARTESIAN_POINT ( 'NONE',  ( -20.85000000000000142, 7.675662554762638479, -241.7139905447625381 ) ) ;
#73000 = DIRECTION ( 'NONE',  ( 0.000000000000000000, -0.2617529984165152257, -0.9651348961777124202 ) ) ;
#73001 = CARTESIAN_POINT ( 'NONE',  ( 23.25000000000000000, -8.596261682231828516, -158.0498724828497359 ) ) ;
#73002 = DIRECTION ( 'NONE',  ( 0.000000000000000000, 1.776356839400250267E-15, 1.000000000000000000 ) ) ;
#73003 = CARTESIAN_POINT ( 'NONE',  ( 20.73486653747090003, 68.75000000001196554, -115.6731074845243512 ) ) ;
#73004 = ORIENTED_EDGE ( 'NONE', *, *, #168746, .T. ) ;
#73005 = EDGE_CURVE ( 'NONE', #244528, #177284, #5587, .T. ) ;
#73006 = ORIENTED_EDGE ( 'NONE', *, *, #151316, .T. ) ;
#73007 = CARTESIAN_POINT ( 'NONE',  ( 18.48197441911431937, 85.51795479471547878, -96.13289584231789320 ) ) ;
#73008 = CARTESIAN_POINT ( 'NONE',  ( -23.15000000000000213, 1.115600667400684642E-11, -100.5000000000000426 ) ) ;
#73009 = CARTESIAN_POINT ( 'NONE',  ( 20.73486653747088226, 63.54522198573869929, -221.7484608313106094 ) ) ;
#73010 = ADVANCED_FACE ( 'NONE', ( #121735 ), #99656, .T. ) ;
#73011 = TOROIDAL_SURFACE ( 'NONE', #102155, 4.099999999999999645, 0.1000000000000000056 ) ;
#73012 = EDGE_LOOP ( 'NONE', ( #13586, #78234, #7350, #20148 ) ) ;
#73013 = LINE ( 'NONE', #244204, #215350 ) ;
#73014 = AXIS2_PLACEMENT_3D ( 'NONE', #133652, #228909, #91956 ) ;
#73015 = AXIS2_PLACEMENT_3D ( 'NONE', #209121, #229975, #250815 ) ;
#73016 = ADVANCED_FACE ( 'NONE', ( #43462 ), #102116, .F. ) ;
#73017 = DIRECTION ( 'NONE',  ( 1.000000000000000000, 0.000000000000000000, 0.000000000000000000 ) ) ;
#73018 = CYLINDRICAL_SURFACE ( 'NONE', #255039, 0.1000000000000026007 ) ;
#73020 = EDGE_CURVE ( 'NONE', #21693, #20940, #103407, .T. ) ;
#73019 = EDGE_CURVE ( 'NONE', #223792, #46071, #181695, .T. ) ;
#73021 = VERTEX_POINT ( 'NONE', #125563 ) ;
#73022 = ORIENTED_EDGE ( 'NONE', *, *, #170397, .T. ) ;
#73023 = MECHANICAL_DESIGN_GEOMETRIC_PRESENTATION_REPRESENTATION (  '', ( #206075 ), #147824 ) ;
#73024 = CARTESIAN_POINT ( 'NONE',  ( -23.25000000000000000, 87.65000000001172964, -72.62310748452422615 ) ) ;
#73025 = CARTESIAN_POINT ( 'NONE',  ( -21.14999999999999858, 69.45934304831114048, -169.9231074845244223 ) ) ;
#73026 = ORIENTED_EDGE ( 'NONE', *, *, #48272, .F. ) ;
#73027 = DIRECTION ( 'NONE',  ( -3.265361837132813093E-16, 1.000000000000000000, 0.000000000000000000 ) ) ;
#73028 = EDGE_LOOP ( 'NONE', ( #197897, #72302, #163091, #19728 ) ) ;
#73029 = CARTESIAN_POINT ( 'NONE',  ( 18.54271179734065456, -9.624084290087184357, -140.7409648527008983 ) ) ;
#73030 = CARTESIAN_POINT ( 'NONE',  ( -18.39999999999999858, 11.47316190337362762, -143.3259460668079726 ) ) ;
#73032 = LINE ( 'NONE', #170868, #170191 ) ;
#73031 = DIRECTION ( 'NONE',  ( 0.000000000000000000, -0.4088369013363783999, 0.9126074666063545004 ) ) ;
#73033 = DIRECTION ( 'NONE',  ( -0.000000000000000000, 0.4791956752371484551, 0.8777080977375184556 ) ) ;
#73034 = DIRECTION ( 'NONE',  ( -1.000000000000000000, -2.952720810173289112E-16, 0.000000000000000000 ) ) ;
#73035 = CARTESIAN_POINT ( 'NONE',  ( 21.09696443733127325, 65.27599011609339641, -90.78832995747616508 ) ) ;
#73037 = EDGE_LOOP ( 'NONE', ( #165488, #130423, #142646, #240095 ) ) ;
#73036 = CARTESIAN_POINT ( 'NONE',  ( 18.69999999999999929, -10.80884033489985363, 5.900000000000001243 ) ) ;
#73038 = EDGE_CURVE ( 'NONE', #213344, #64533, #163417, .T. ) ;
#73039 = ADVANCED_FACE ( 'NONE', ( #100817 ), #44552, .F. ) ;
#73040 = AXIS2_PLACEMENT_3D ( 'NONE', #80564, #256609, #160165 ) ;
#73042 = ORIENTED_EDGE ( 'NONE', *, *, #12503, .T. ) ;
#73041 = VERTEX_POINT ( 'NONE', #124294 ) ;
#73043 = ORIENTED_EDGE ( 'NONE', *, *, #35409, .T. ) ;
#73044 = ADVANCED_FACE ( 'NONE', ( #203813 ), #199980, .T. ) ;
#73045 = CARTESIAN_POINT ( 'NONE',  ( -16.77977881697927387, 60.94561573421638201, -221.0316353316906088 ) ) ;
#73046 = CARTESIAN_POINT ( 'NONE',  ( -18.59999999999999787, 68.97833521811131163, -32.28954208262708647 ) ) ;
#73047 =( BOUNDED_SURFACE ( )  B_SPLINE_SURFACE ( 3, 2, ( 
 ( #68433, #51395, #69728 ),
 ( #130971, #151843, #228798 ),
 ( #227486, #48856, #128402 ),
 ( #207959, #171421, #250901 ) ),
 .UNSPECIFIED., .F., .F., .F. ) 
 B_SPLINE_SURFACE_WITH_KNOTS ( ( 4, 4 ),
 ( 3, 3 ),
 ( -2.710505431213761085E-20, 0.0003124336600439509004 ),
 ( 0.000000000000000000, 1.000000000000000000 ),
 .UNSPECIFIED. ) 
 GEOMETRIC_REPRESENTATION_ITEM ( )  RATIONAL_B_SPLINE_SURFACE ( (
 ( 1.000000000000000000, 0.7071067811865229258, 1.000000000000000000),
 ( 1.000000000000000000, 0.7089187706049977500, 1.000000000000000000),
 ( 1.000000000000000000, 0.7039288185052062774, 1.000000000000000000),
 ( 1.000000000000000000, 0.7040654476015933971, 1.000000000000000000) ) ) 
 REPRESENTATION_ITEM ( '' )  SURFACE ( )  );
#73049 = CYLINDRICAL_SURFACE ( 'NONE', #157278, 0.1000000000000106914 ) ;
#73048 = DIRECTION ( 'NONE',  ( 0.000000000000000000, 0.1350103645451945777, -0.9908441862701589109 ) ) ;
#73050 = CARTESIAN_POINT ( 'NONE',  ( -23.15000000000000213, 1.115600667400684642E-11, -33.50000000000000000 ) ) ;
#73051 = EDGE_LOOP ( 'NONE', ( #24524, #16438, #73245, #171886, #19536 ) ) ;
#73052 = CIRCLE ( 'NONE', #97913, 2.000000000000001776 ) ;
#73053 = DIRECTION ( 'NONE',  ( 1.000000000000000000, 0.000000000000000000, 0.000000000000000000 ) ) ;
#73054 = AXIS2_PLACEMENT_3D ( 'NONE', #119655, #199183, #64791 ) ;
#73055 = CIRCLE ( 'NONE', #210395, 0.1000000000000005468 ) ;
#73056 = EDGE_CURVE ( 'NONE', #129974, #103686, #15528, .T. ) ;
#73057 = ORIENTED_EDGE ( 'NONE', *, *, #251875, .T. ) ;
#73058 = ORIENTED_EDGE ( 'NONE', *, *, #202811, .F. ) ;
#73059 = CARTESIAN_POINT ( 'NONE',  ( -21.04999999999999716, 69.45934304831042994, -69.52310748452438816 ) ) ;
#73060 = FACE_OUTER_BOUND ( 'NONE', #247929, .T. ) ;
#73061 = DIRECTION ( 'NONE',  ( 0.000000000000000000, 0.9126074666063774821, 0.4088369013363270521 ) ) ;
#73062 = CARTESIAN_POINT ( 'NONE',  ( 18.39999999999999858, -9.399999999988843058, -88.75000000000004263 ) ) ;
#73063 = VECTOR ( 'NONE', #141524, 1000.000000000000000 ) ;
#73064 = LINE ( 'NONE', #112172, #251080 ) ;
#73065 = ORIENTED_EDGE ( 'NONE', *, *, #103265, .T. ) ;
#73066 = ORIENTED_EDGE ( 'NONE', *, *, #73873, .F. ) ;
#73067 = DIRECTION ( 'NONE',  ( 0.000000000000000000, -6.467318590049456648E-15, 1.000000000000000000 ) ) ;
#73068 = VECTOR ( 'NONE', #111252, 999.9999999999998863 ) ;
#73069 = CARTESIAN_POINT ( 'NONE',  ( -21.14999999999994174, 83.97335046823651794, -34.66234602115918051 ) ) ;
#73070 = CARTESIAN_POINT ( 'NONE',  ( -21.05000000000000071, 1.835341550235567887, -45.05515129256298223 ) ) ;
#73071 = ADVANCED_FACE ( 'NONE', ( #145111 ), #194604, .T. ) ;
#73072 = CYLINDRICAL_SURFACE ( 'NONE', #231295, 0.09999999999998898659 ) ;
#73073 = FACE_OUTER_BOUND ( 'NONE', #69147, .T. ) ;
#73074 = AXIS2_PLACEMENT_3D ( 'NONE', #120932, #223828, #200440 ) ;
#73075 = DIRECTION ( 'NONE',  ( -0.7070776581709311559, 4.937903618720164857E-15, -0.7071359030027479786 ) ) ;
#73076 = DIRECTION ( 'NONE',  ( 0.000000000000000000, 0.000000000000000000, 1.000000000000000000 ) ) ;
#73077 = CARTESIAN_POINT ( 'NONE',  ( -16.92507428761699018, 66.05000000001224691, -149.2365049441459917 ) ) ;
#73079 = CARTESIAN_POINT ( 'NONE',  ( -20.54999999999999716, -8.730841121484173684, -76.59807471898437825 ) ) ;
#73078 = CARTESIAN_POINT ( 'NONE',  ( -22.47120815636973745, 0.02890382190389122891, 11.64993198875349734 ) ) ;
#73080 = DIRECTION ( 'NONE',  ( 0.000000000000000000, -0.000000000000000000, 1.000000000000000000 ) ) ;
#73082 = EDGE_CURVE ( 'NONE', #168942, #35313, #180409, .T. ) ;
#73081 = CARTESIAN_POINT ( 'NONE',  ( -18.59999999999999787, 1.750000000011155743, -112.1695115579016857 ) ) ;
#73083 = PLANE ( 'NONE',  #124652 ) ;
#73084 = DIRECTION ( 'NONE',  ( 2.952720810173288619E-16, -1.000000000000000000, 0.000000000000000000 ) ) ;
#73086 = ORIENTED_EDGE ( 'NONE', *, *, #131137, .T. ) ;
#73085 = DIRECTION ( 'NONE',  ( 0.000000000000000000, -0.1298341882520022694, -0.9915357197604853789 ) ) ;
#73087 =( BOUNDED_CURVE ( )  B_SPLINE_CURVE ( 3, ( #72334, #132284, #33232, #192279 ),
 .UNSPECIFIED., .F., .F. ) 
 B_SPLINE_CURVE_WITH_KNOTS ( ( 4, 4 ),
 ( 0.3000847527772380618, 0.5497968875596825900 ),
 .UNSPECIFIED. ) 
 CURVE ( )  GEOMETRIC_REPRESENTATION_ITEM ( )  RATIONAL_B_SPLINE_CURVE ( ( 1.000000000000000000, 0.9948104011409419911, 0.9948104011409419911, 1.000000000000000000 ) ) 
 REPRESENTATION_ITEM ( '' )  );
#73089 = ADVANCED_FACE ( 'NONE', ( #128145 ), #234486, .T. ) ;
#73088 = CARTESIAN_POINT ( 'NONE',  ( -18.79999999999999716, 0.000000000000000000, 0.000000000000000000 ) ) ;
#73091 = VECTOR ( 'NONE', #60016, 1000.000000000000000 ) ;
#73090 = FACE_OUTER_BOUND ( 'NONE', #24757, .T. ) ;
#73092 = CIRCLE ( 'NONE', #218775, 0.09999999999999031886 ) ;
#73093 = DIRECTION ( 'NONE',  ( 0.000000000000000000, 0.2128009952263603677, -0.9770955615653313941 ) ) ;
#73094 = VECTOR ( 'NONE', #195408, 1000.000000000000000 ) ;
#73095 = CARTESIAN_POINT ( 'NONE',  ( -21.14999999999999858, 4.136903274969358613, -245.4596299165286268 ) ) ;
#73096 = CARTESIAN_POINT ( 'NONE',  ( 21.00000000000000000, 6.238071963501339745, 11.95857864376269042 ) ) ;
#73097 = CARTESIAN_POINT ( 'NONE',  ( -18.50000000000000000, 79.11538813396778380, -196.3722783875038544 ) ) ;
#73098 = FACE_OUTER_BOUND ( 'NONE', #92255, .T. ) ;
#73099 = LINE ( 'NONE', #250405, #23965 ) ;
#73100 = AXIS2_PLACEMENT_3D ( 'NONE', #256936, #20982, #155359 ) ;
#73101 = VECTOR ( 'NONE', #179849, 1000.000000000000000 ) ;
#73102 = ORIENTED_EDGE ( 'NONE', *, *, #68276, .T. ) ;
#73103 = CARTESIAN_POINT ( 'NONE',  ( -23.15000000000000213, 86.27712145182582049, -209.5223386573213702 ) ) ;
#73105 = VERTEX_POINT ( 'NONE', #31636 ) ;
#73104 = CARTESIAN_POINT ( 'NONE',  ( -23.25000000000000000, 11.75000000001115552, -112.6500000000000341 ) ) ;
#73106 = DIRECTION ( 'NONE',  ( 1.000000000000000000, -0.000000000000000000, -0.000000000000000000 ) ) ;
#73107 = LINE ( 'NONE', #53506, #250332 ) ;
#73108 = AXIS2_PLACEMENT_3D ( 'NONE', #248383, #96965, #20056 ) ;
#73109 = VERTEX_POINT ( 'NONE', #186841 ) ;
#73110 = DIRECTION ( 'NONE',  ( 1.000000000000000000, 0.000000000000000000, 0.000000000000000000 ) ) ;
#73111 = CIRCLE ( 'NONE', #64690, 0.1000000000000033223 ) ;
#73112 = SHAPE_DEFINITION_REPRESENTATION ( #226236, #61981 ) ;
#73113 = FACE_OUTER_BOUND ( 'NONE', #102049, .T. ) ;
#73114 = CARTESIAN_POINT ( 'NONE',  ( 22.49231231312462853, 64.35001509633437422, -69.58416037212577976 ) ) ;
#73115 = AXIS2_PLACEMENT_3D ( 'NONE', #91173, #31249, #207293 ) ;
#73116 = ORIENTED_EDGE ( 'NONE', *, *, #255004, .F. ) ;
#73117 = CARTESIAN_POINT ( 'NONE',  ( 21.05000000000000071, 64.35000000001249987, -177.0379132551784096 ) ) ;
#73118 = CARTESIAN_POINT ( 'NONE',  ( 18.49999999999998934, 66.44571689960341132, -213.7280413126916017 ) ) ;
#73119 = PLANE ( 'NONE',  #170208 ) ;
#73120 = ORIENTED_EDGE ( 'NONE', *, *, #207460, .F. ) ;
#73121 = AXIS2_PLACEMENT_3D ( 'NONE', #20024, #237766, #196078 ) ;
#73122 = ORIENTED_EDGE ( 'NONE', *, *, #242921, .T. ) ;
#73123 = DIRECTION ( 'NONE',  ( 1.000000000000000000, 0.000000000000000000, 0.000000000000000000 ) ) ;
#73124 = DIRECTION ( 'NONE',  ( 0.000000000000000000, 0.000000000000000000, -1.000000000000000000 ) ) ;
#73125 = DIRECTION ( 'NONE',  ( 0.000000000000000000, 0.000000000000000000, -1.000000000000000000 ) ) ;
#73126 = DIRECTION ( 'NONE',  ( 1.000000000000000000, -0.000000000000000000, 0.000000000000000000 ) ) ;
#73127 = ADVANCED_FACE ( 'NONE', ( #210255 ), #13332, .F. ) ;
#73129 = CARTESIAN_POINT ( 'NONE',  ( -22.39999999999999858, 64.25000000001215028, -136.6231074845243825 ) ) ;
#73128 = CARTESIAN_POINT ( 'NONE',  ( -20.54999999999999716, 53.08776555244186568, -234.2469744149522626 ) ) ;
#73130 = CARTESIAN_POINT ( 'NONE',  ( -21.05000000000000071, -0.09999999998884338825, -160.9593430482987344 ) ) ;
#73131 = CARTESIAN_POINT ( 'NONE',  ( -16.94445028196808778, 9.992063609708889516, -113.1073301784184792 ) ) ;
#73132 = CARTESIAN_POINT ( 'NONE',  ( 22.39999999999999503, 55.96127771274635876, -232.9022175645438892 ) ) ;
#73133 = ORIENTED_EDGE ( 'NONE', *, *, #12419, .T. ) ;
#73134 = AXIS2_PLACEMENT_3D ( 'NONE', #237205, #157708, #160257 ) ;
#73136 = VERTEX_POINT ( 'NONE', #87703 ) ;
#73135 = DIRECTION ( 'NONE',  ( -1.000000000000000000, 0.000000000000000000, 0.000000000000000000 ) ) ;
#73137 = CIRCLE ( 'NONE', #106390, 0.09999999999999949207 ) ;
#73138 = DIRECTION ( 'NONE',  ( -7.304098846218134667E-16, -1.000000000000000000, 0.000000000000000000 ) ) ;
#73139 = CARTESIAN_POINT ( 'NONE',  ( -18.50000000000000000, 7.021664781911246322, -70.63356540189728605 ) ) ;
#73141 = DIRECTION ( 'NONE',  ( 0.000000000000000000, 0.000000000000000000, -1.000000000000000000 ) ) ;
#73140 = LINE ( 'NONE', #127948, #201036 ) ;
#73142 = ORIENTED_EDGE ( 'NONE', *, *, #225705, .T. ) ;
#73143 = CARTESIAN_POINT ( 'NONE',  ( -23.25000000000000000, 1.115600667400684642E-11, -108.4000000000000483 ) ) ;
#73145 = ADVANCED_FACE ( 'NONE', ( #49875 ), #248077, .T. ) ;
#73144 = DIRECTION ( 'NONE',  ( 0.2834754621636439431, 0.2834754621636471628, 0.9161240771326858434 ) ) ;
#73146 = PLANE ( 'NONE',  #241032 ) ;
#73147 = CARTESIAN_POINT ( 'NONE',  ( 12.93279065517212523, 13.06253445771513100, -216.7219835687084526 ) ) ;
#73148 = ORIENTED_EDGE ( 'NONE', *, *, #239166, .F. ) ;
#73149 = ORIENTED_EDGE ( 'NONE', *, *, #42570, .F. ) ;
#73150 = ADVANCED_FACE ( 'NONE', ( #171164 ), #236026, .T. ) ;
#73151 = LINE ( 'NONE', #246610, #42700 ) ;
#73152 = ORIENTED_EDGE ( 'NONE', *, *, #240170, .F. ) ;
#73153 = CARTESIAN_POINT ( 'NONE',  ( -20.85000000000000142, 74.93036000061670165, -233.6816308724374949 ) ) ;
#73154 = VECTOR ( 'NONE', #222096, 1000.000000000000114 ) ;
#73155 = CARTESIAN_POINT ( 'NONE',  ( 23.04999999999999716, 10.58889512527366428, -208.1606840254082158 ) ) ;
#73156 = FACE_OUTER_BOUND ( 'NONE', #214156, .T. ) ;
#73157 = ADVANCED_FACE ( 'NONE', ( #15925 ), #95429, .T. ) ;
#73158 = AXIS2_PLACEMENT_3D ( 'NONE', #115448, #154619, #114169 ) ;
#73159 = ADVANCED_FACE ( 'NONE', ( #133274 ), #148608, .T. ) ;
#73160 = ORIENTED_EDGE ( 'NONE', *, *, #16767, .T. ) ;
#73161 = CARTESIAN_POINT ( 'NONE',  ( -21.05000000000000426, 38.23914636435921466, -236.1324109481172968 ) ) ;
#73162 = EDGE_CURVE ( 'NONE', #203670, #70299, #217918, .T. ) ;
#73163 = CARTESIAN_POINT ( 'NONE',  ( 21.05000000000000071, 85.00000000001251976, -179.9170766071767389 ) ) ;
#73164 = DIRECTION ( 'NONE',  ( 0.000000000000000000, 0.000000000000000000, 1.000000000000000000 ) ) ;
#73165 = DIRECTION ( 'NONE',  ( 1.000000000000000000, 0.000000000000000000, 0.000000000000000000 ) ) ;
#73166 = CARTESIAN_POINT ( 'NONE',  ( 23.14999999999999147, 76.00000000001195133, -103.0231074845243171 ) ) ;
#73168 = DIRECTION ( 'NONE',  ( 0.000000000000000000, 0.000000000000000000, 1.000000000000000000 ) ) ;
#73167 = CARTESIAN_POINT ( 'NONE',  ( -23.25000000000000355, 64.25000000001207923, -123.8731074845243683 ) ) ;
#73169 = EDGE_CURVE ( 'NONE', #41677, #169820, #215237, .T. ) ;
#73170 = CARTESIAN_POINT ( 'NONE',  ( -16.77308656112215246, 66.05000000001226113, -149.1733006762267451 ) ) ;
#73171 = ORIENTED_EDGE ( 'NONE', *, *, #46014, .T. ) ;
#73173 = CARTESIAN_POINT ( 'NONE',  ( -20.54999999999999716, 2.500000000011154633, -87.27537807723794572 ) ) ;
#73172 = DIRECTION ( 'NONE',  ( -1.000000000000000000, -7.304098846218164250E-16, 4.217023435051628197E-16 ) ) ;
#73174 = ORIENTED_EDGE ( 'NONE', *, *, #70701, .T. ) ;
#73176 = EDGE_LOOP ( 'NONE', ( #257847, #175698, #107217, #180344 ) ) ;
#73175 = CARTESIAN_POINT ( 'NONE',  ( 18.50000000000000000, -9.399999999988843058, -174.4992856778388273 ) ) ;
#73177 = CIRCLE ( 'NONE', #239550, 0.09999999999999939493 ) ;
#73178 = VERTEX_POINT ( 'NONE', #56284 ) ;
#73179 = CIRCLE ( 'NONE', #48192, 11.79999999999999716 ) ;
#73180 = CARTESIAN_POINT ( 'NONE',  ( -23.49999999999994316, 74.94272479589878344, -3.123107484524795474 ) ) ;
#73181 = EDGE_CURVE ( 'NONE', #93396, #230638, #217567, .T. ) ;
#73182 = CARTESIAN_POINT ( 'NONE',  ( 12.60873083341399159, 66.61042836546585022, -152.2054667721552335 ) ) ;
#73183 = CARTESIAN_POINT ( 'NONE',  ( -23.15000000000000213, 76.00000000001192291, -105.0231074845243029 ) ) ;
#73184 = CARTESIAN_POINT ( 'NONE',  ( 20.95262331984766746, 65.49584273722216210, -128.9622191549310912 ) ) ;
#73185 = EDGE_LOOP ( 'NONE', ( #169174, #70651, #229012, #145686 ) ) ;
#73186 = CARTESIAN_POINT ( 'NONE',  ( -18.40000000000000213, 40.40436687347765599, -235.2865959907995546 ) ) ;
#73187 = CARTESIAN_POINT ( 'NONE',  ( 21.30000000000002558, 76.00000000001237765, -170.0231074845243597 ) ) ;
#73188 = ORIENTED_EDGE ( 'NONE', *, *, #103117, .T. ) ;
#73190 = EDGE_CURVE ( 'NONE', #203969, #66968, #111362, .T. ) ;
#73189 = DIRECTION ( 'NONE',  ( 1.000000000000000000, 0.000000000000000000, -0.000000000000000000 ) ) ;
#73192 = CIRCLE ( 'NONE', #160486, 0.1000000000000020595 ) ;
#73191 = DIRECTION ( 'NONE',  ( -0.000000000000000000, 6.982962677686266711E-15, -1.000000000000000000 ) ) ;
#73193 = ORIENTED_EDGE ( 'NONE', *, *, #202996, .T. ) ;
#73195 = CARTESIAN_POINT ( 'NONE',  ( -23.15000000000000213, 11.65000000001115588, -112.7500000000000284 ) ) ;
#73194 = CIRCLE ( 'NONE', #243838, 0.09999999999998898659 ) ;
#73196 = AXIS2_PLACEMENT_3D ( 'NONE', #42265, #121808, #57946 ) ;
#73197 = AXIS2_PLACEMENT_3D ( 'NONE', #58781, #176210, #95371 ) ;
#73198 = ORIENTED_EDGE ( 'NONE', *, *, #63372, .T. ) ;
#73199 = CARTESIAN_POINT ( 'NONE',  ( 18.49505832270841310, -9.438028062771731896, -141.1984731748938771 ) ) ;
#73200 = ORIENTED_EDGE ( 'NONE', *, *, #239506, .T. ) ;
#73201 = DIRECTION ( 'NONE',  ( -1.000000000000000000, -0.000000000000000000, -0.000000000000000000 ) ) ;
#73202 = DIRECTION ( 'NONE',  ( 0.000000000000000000, 0.000000000000000000, 1.000000000000000000 ) ) ;
#73203 = CARTESIAN_POINT ( 'NONE',  ( 20.85000000000000142, 7.021664781911246322, -171.3335654018973173 ) ) ;
#73204 = DIRECTION ( 'NONE',  ( -0.000000000000000000, -0.000000000000000000, 1.000000000000000000 ) ) ;
#73206 = B_SPLINE_CURVE_WITH_KNOTS ( 'NONE', 3,
 ( #166076, #186917, #245589, #66938, #146459, #225977, #47357, #8266, #68229, #147774, #227293, #48654, #251994, #197148, #55057, #56345 ),
 .UNSPECIFIED., .F., .F.,
 ( 4, 3, 3, 3, 3, 4 ),
 ( 0.000000000000000000, 1.810570668010637698E-05, 2.740575833571996995E-05, 4.256816319435940987E-05, 5.213463471026038941E-05, 6.641585710717883072E-05 ),
 .UNSPECIFIED. ) ;
#73205 = CARTESIAN_POINT ( 'NONE',  ( 18.44208962362722204, -9.552340496897459232, -73.84217305546387422 ) ) ;
#73207 = DIRECTION ( 'NONE',  ( -1.000000000000000000, -7.304098846218105085E-16, -4.217023435051676515E-16 ) ) ;
#73208 = EDGE_LOOP ( 'NONE', ( #20874, #254774, #29818, #252036 ) ) ;
#73209 = DIRECTION ( 'NONE',  ( -1.000000000000000000, -0.000000000000000000, 0.000000000000000000 ) ) ;
#73210 = AXIS2_PLACEMENT_3D ( 'NONE', #78968, #41187, #215923 ) ;
#73211 = ORIENTED_EDGE ( 'NONE', *, *, #146693, .F. ) ;
#73214 = ORIENTED_EDGE ( 'NONE', *, *, #113570, .T. ) ;
#73213 = CARTESIAN_POINT ( 'NONE',  ( -18.50000000000000000, 74.36282728704149747, -91.44095411905230719 ) ) ;
#73212 = DIRECTION ( 'NONE',  ( 1.000000000000000000, -0.000000000000000000, -0.000000000000000000 ) ) ;
#73215 = EDGE_CURVE ( 'NONE', #204820, #190865, #102970, .T. ) ;
#73216 = VERTEX_POINT ( 'NONE', #38050 ) ;
#73217 = DIRECTION ( 'NONE',  ( 1.000000000000000000, -2.952720810173289112E-16, -2.061873921506763405E-30 ) ) ;
#73218 = AXIS2_PLACEMENT_3D ( 'NONE', #226792, #87269, #127712 ) ;
#73219 = CARTESIAN_POINT ( 'NONE',  ( -21.05000000000000071, 74.14897176987174987, -191.8691942151018850 ) ) ;
#73220 = DIRECTION ( 'NONE',  ( 1.000000000000000000, 0.000000000000000000, 0.000000000000000000 ) ) ;
#73221 = CARTESIAN_POINT ( 'NONE',  ( 20.95575313997065336, 58.98169444576728893, -225.7211617421326650 ) ) ;
#73222 = VERTEX_POINT ( 'NONE', #176277 ) ;
#73224 = ORIENTED_EDGE ( 'NONE', *, *, #75333, .F. ) ;
#73223 = DIRECTION ( 'NONE',  ( 1.000000000000000000, 0.000000000000000000, 0.000000000000000000 ) ) ;
#73225 = CIRCLE ( 'NONE', #106462, 0.1000000000000028644 ) ;
#73226 = EDGE_CURVE ( 'NONE', #211171, #205125, #107259, .T. ) ;
#73227 = EDGE_CURVE ( 'NONE', #150102, #57757, #140568, .T. ) ;
#73228 = CIRCLE ( 'NONE', #19008, 0.09999999999999990841 ) ;
#73230 = CARTESIAN_POINT ( 'NONE',  ( 18.49999999999999289, 15.39038045630036855, -223.0585967715782090 ) ) ;
#73229 = CARTESIAN_POINT ( 'NONE',  ( -18.59999999999999787, 63.74333919030581086, -212.9951329171253747 ) ) ;
#73231 = VECTOR ( 'NONE', #77011, 1000.000000000000000 ) ;
#73232 = CIRCLE ( 'NONE', #77277, 0.09999999999998898659 ) ;
#73234 = ORIENTED_EDGE ( 'NONE', *, *, #47098, .F. ) ;
#73233 = FACE_OUTER_BOUND ( 'NONE', #241154, .T. ) ;
#73235 = EDGE_CURVE ( 'NONE', #53868, #105637, #155269, .T. ) ;
#73236 = ADVANCED_FACE ( 'NONE', ( #58840 ), #215415, .F. ) ;
#73237 = ORIENTED_EDGE ( 'NONE', *, *, #216847, .T. ) ;
#73238 = EDGE_CURVE ( 'NONE', #243786, #239652, #53732, .T. ) ;
#73239 = ADVANCED_FACE ( 'NONE', ( #214093 ), #21058, .F. ) ;
#73240 = CYLINDRICAL_SURFACE ( 'NONE', #76923, 5.000000000000004441 ) ;
#73241 = VECTOR ( 'NONE', #67474, 1000.000000000000000 ) ;
#73242 = PLANE ( 'NONE',  #192925 ) ;
#73243 = VERTEX_POINT ( 'NONE', #180117 ) ;
#73244 = DIRECTION ( 'NONE',  ( 0.000000000000000000, 1.000000000000000000, 0.000000000000000000 ) ) ;
#73245 = ORIENTED_EDGE ( 'NONE', *, *, #38502, .F. ) ;
#73246 = CIRCLE ( 'NONE', #48256, 0.1000000000000124678 ) ;
#73247 = EDGE_CURVE ( 'NONE', #17738, #244686, #207241, .T. ) ;
#73248 = CARTESIAN_POINT ( 'NONE',  ( 18.59999999999999432, 68.22930980752001062, -227.7331931781284879 ) ) ;
#73249 = VECTOR ( 'NONE', #125088, 999.9999999999998863 ) ;
#73251 = VERTEX_POINT ( 'NONE', #24907 ) ;
#73250 = CIRCLE ( 'NONE', #56595, 0.09999999999999158173 ) ;
#73252 = DIRECTION ( 'NONE',  ( 0.000000000000000000, 0.000000000000000000, 1.000000000000000000 ) ) ;
#73253 = CARTESIAN_POINT ( 'NONE',  ( -23.25000000000000000, 6.933893972137497030, -137.7856458343736108 ) ) ;
#73254 = ADVANCED_FACE ( 'NONE', ( #181410 ), #40636, .F. ) ;
#73255 = ORIENTED_EDGE ( 'NONE', *, *, #224874, .T. ) ;
#73256 = ORIENTED_EDGE ( 'NONE', *, *, #98166, .T. ) ;
#73257 = CARTESIAN_POINT ( 'NONE',  ( 20.12518398540832365, 18.88802431391419034, -228.7156777160730030 ) ) ;
#73258 = ORIENTED_EDGE ( 'NONE', *, *, #177290, .F. ) ;
#73259 = DIRECTION ( 'NONE',  ( 0.000000000000000000, -0.5000000000000016653, 0.8660254037844377084 ) ) ;
#73260 = ORIENTED_EDGE ( 'NONE', *, *, #7249, .T. ) ;
#73262 = EDGE_LOOP ( 'NONE', ( #46638, #191232, #255751, #5199 ) ) ;
#73261 = CARTESIAN_POINT ( 'NONE',  ( 19.97071067811864609, 11.72071067812981404, -188.8499999999999659 ) ) ;
#73263 = EDGE_CURVE ( 'NONE', #195708, #219226, #44459, .T. ) ;
#73264 = EDGE_CURVE ( 'NONE', #215277, #187182, #244627, .T. ) ;
#73265 = ORIENTED_EDGE ( 'NONE', *, *, #224912, .F. ) ;
#73266 = AXIS2_PLACEMENT_3D ( 'NONE', #187707, #152442, #231970 ) ;
#73267 = CARTESIAN_POINT ( 'NONE',  ( -20.15000000000000568, 11.68541875934721297, -210.9921969175020706 ) ) ;
#73268 = ORIENTED_EDGE ( 'NONE', *, *, #166495, .F. ) ;
#73269 = CIRCLE ( 'NONE', #173241, 11.80000000000000959 ) ;
#73272 = ORIENTED_EDGE ( 'NONE', *, *, #217282, .T. ) ;
#73271 = ORIENTED_EDGE ( 'NONE', *, *, #122973, .T. ) ;
#73270 = CARTESIAN_POINT ( 'NONE',  ( -16.93226657140833069, 66.00045617728716252, -56.94439437355077871 ) ) ;
#73273 = AXIS2_PLACEMENT_3D ( 'NONE', #189083, #129111, #10451 ) ;
#73274 = VECTOR ( 'NONE', #68710, 1000.000000000000000 ) ;
#73275 = ORIENTED_EDGE ( 'NONE', *, *, #88420, .T. ) ;
#73276 = AXIS2_PLACEMENT_3D ( 'NONE', #158892, #100141, #117179 ) ;
#73277 = ADVANCED_BREP_SHAPE_REPRESENTATION ( '', ( #191235, #2425 ), #131439 ) ;
#73278 = CARTESIAN_POINT ( 'NONE',  ( -18.40000000000000213, 8.822561741677553471, -143.2500000000000284 ) ) ;
#73279 = ORIENTED_EDGE ( 'NONE', *, *, #88844, .T. ) ;
#73280 = CARTESIAN_POINT ( 'NONE',  ( 18.52928932188133970, 65.72071067813062939, -111.7731074845243739 ) ) ;
#73282 = ORIENTED_EDGE ( 'NONE', *, *, #82021, .T. ) ;
#73281 = CARTESIAN_POINT ( 'NONE',  ( 22.47071067811865319, 7.720074744509199505, -167.4009075452973434 ) ) ;
#73283 = DIRECTION ( 'NONE',  ( 1.000000000000000000, -0.000000000000000000, -0.000000000000000000 ) ) ;
#73284 = ORIENTED_EDGE ( 'NONE', *, *, #174325, .F. ) ;
#73285 = TOROIDAL_SURFACE ( 'NONE', #210620, 0.2000000000000000111, 0.1000000000000000056 ) ;
#73286 = AXIS2_PLACEMENT_3D ( 'NONE', #180796, #64682, #222446 ) ;
#73287 = ORIENTED_EDGE ( 'NONE', *, *, #220206, .T. ) ;
#73288 = CARTESIAN_POINT ( 'NONE',  ( -18.50000000000000000, 11.65000000001115232, -55.25000000000004974 ) ) ;
#73289 = DIRECTION ( 'NONE',  ( -0.000000000000000000, -0.9887567792719339499, -0.1495327102803676589 ) ) ;
#73290 = AXIS2_PLACEMENT_3D ( 'NONE', #214812, #96135, #142640 ) ;
#73291 = ORIENTED_EDGE ( 'NONE', *, *, #164098, .T. ) ;
#73293 = ORIENTED_EDGE ( 'NONE', *, *, #59413, .F. ) ;
#73292 = LINE ( 'NONE', #119788, #122348 ) ;
#73295 = ORIENTED_EDGE ( 'NONE', *, *, #114926, .F. ) ;
#73294 = ORIENTED_EDGE ( 'NONE', *, *, #229644, .T. ) ;
#73296 = EDGE_LOOP ( 'NONE', ( #168482, #196756, #174304, #29440 ) ) ;
#73297 = DIRECTION ( 'NONE',  ( 1.000000000000000000, 0.000000000000000000, 0.000000000000000000 ) ) ;
#73298 = ORIENTED_EDGE ( 'NONE', *, *, #53815, .T. ) ;
#73299 = ORIENTED_EDGE ( 'NONE', *, *, #50169, .F. ) ;
#73300 = CARTESIAN_POINT ( 'NONE',  ( 20.95443524775735256, 18.84365912742161697, -229.9358607224024524 ) ) ;
#73301 = CIRCLE ( 'NONE', #248243, 0.1000000000000002831 ) ;
#73302 = ORIENTED_EDGE ( 'NONE', *, *, #70209, .F. ) ;
#73303 = CARTESIAN_POINT ( 'NONE',  ( 18.39999999999999503, 70.35000000001230092, -157.3731074845244109 ) ) ;
#73304 = DIRECTION ( 'NONE',  ( 1.000000000000000000, 0.000000000000000000, 0.000000000000000000 ) ) ;
#73305 = B_SPLINE_CURVE_WITH_KNOTS ( 'NONE', 3,
 ( #172177, #113436, #192986, #92574, #213821, #14367 ),
 .UNSPECIFIED., .F., .F.,
 ( 4, 2, 4 ),
 ( 1.138412281109779656E-18, 0.0001569047307838638433, 0.0003138094615677265481 ),
 .UNSPECIFIED. ) ;
#73306 = VERTEX_POINT ( 'NONE', #221766 ) ;
#73307 = EDGE_CURVE ( 'NONE', #171657, #217875, #100527, .T. ) ;
#73308 = EDGE_LOOP ( 'NONE', ( #12824, #67267, #159169, #80672 ) ) ;
#73309 = CYLINDRICAL_SURFACE ( 'NONE', #33908, 0.1000000000000070832 ) ;
#73310 = EDGE_CURVE ( 'NONE', #132836, #111853, #84815, .T. ) ;
#73311 = VERTEX_POINT ( 'NONE', #241374 ) ;
#73312 = AXIS2_PLACEMENT_3D ( 'NONE', #171519, #166388, #189766 ) ;
#73313 = CIRCLE ( 'NONE', #235763, 0.1999999999999987899 ) ;
#73314 = TOROIDAL_SURFACE ( 'NONE', #239694, 0.2000000000000000111, 0.1000000000000000056 ) ;
#73315 = AXIS2_PLACEMENT_3D ( 'NONE', #194636, #135889, #191699 ) ;
#73316 = EDGE_CURVE ( 'NONE', #39283, #23611, #119756, .T. ) ;
#73317 = CARTESIAN_POINT ( 'NONE',  ( 15.74999999999999645, 12.70026017068886226, -215.3766613508543628 ) ) ;
#73318 = EDGE_CURVE ( 'NONE', #130629, #142489, #198842, .T. ) ;
#73319 = ORIENTED_EDGE ( 'NONE', *, *, #210169, .F. ) ;
#73320 = EDGE_LOOP ( 'NONE', ( #73717, #100503, #45365, #97436 ) ) ;
#73321 = CARTESIAN_POINT ( 'NONE',  ( 21.05000000000000071, 36.65892442174472876, -249.5511627012454596 ) ) ;
#73323 = VERTEX_POINT ( 'NONE', #243916 ) ;
#73322 = CARTESIAN_POINT ( 'NONE',  ( 18.46082813847984383, 85.48074965091987565, -162.9387373818086644 ) ) ;
#73324 = DIRECTION ( 'NONE',  ( 2.952720810173289112E-16, 1.000000000000000000, 1.261617073437673512E-14 ) ) ;
#73325 = DIRECTION ( 'NONE',  ( -1.000000000000000000, -0.000000000000000000, -0.000000000000000000 ) ) ;
#73326 = CARTESIAN_POINT ( 'NONE',  ( 20.95052659398289308, 65.52017563223218133, -128.9478687286587615 ) ) ;
#73327 = DIRECTION ( 'NONE',  ( 0.000000000000000000, -1.000000000000000000, 0.000000000000000000 ) ) ;
#73328 = CARTESIAN_POINT ( 'NONE',  ( -17.11825945287481332, 9.949999999999983302, -20.75000000000000000 ) ) ;
#73329 = CARTESIAN_POINT ( 'NONE',  ( 21.87500000000000355, 66.25000000001199396, -115.3731074845243683 ) ) ;
#73330 = CARTESIAN_POINT ( 'NONE',  ( 21.05000000000000071, -9.400000000000000355, -23.60603087734755690 ) ) ;
#73331 = CARTESIAN_POINT ( 'NONE',  ( 22.47071067811865319, 10.68684811775432664, -226.8807012965928323 ) ) ;
#73332 = CARTESIAN_POINT ( 'NONE',  ( 18.39999999999999858, 37.99112772578903474, -261.0419300540665404 ) ) ;
#73333 = CARTESIAN_POINT ( 'NONE',  ( 22.50000000000000000, 75.90000000001222702, -148.1726782920690937 ) ) ;
#73334 = DIRECTION ( 'NONE',  ( 0.000000000000000000, 0.000000000000000000, -1.000000000000000000 ) ) ;
#73335 = EDGE_LOOP ( 'NONE', ( #46547, #240616, #13487, #212118 ) ) ;
#73336 = ADVANCED_FACE ( 'NONE', ( #45726 ), #101814, .T. ) ;
#73337 = EDGE_CURVE ( 'NONE', #81187, #100947, #104388, .T. ) ;
#73339 = ORIENTED_EDGE ( 'NONE', *, *, #4967, .T. ) ;
#73338 = ORIENTED_EDGE ( 'NONE', *, *, #31839, .F. ) ;
#73340 = AXIS2_PLACEMENT_3D ( 'NONE', #118022, #77585, #18918 ) ;
#73341 = EDGE_LOOP ( 'NONE', ( #250607, #153516, #243227, #123490 ) ) ;
#73342 = CARTESIAN_POINT ( 'NONE',  ( -21.08621493067320429, 0.05619483948720407906, -94.15070570882809875 ) ) ;
#73343 = FACE_OUTER_BOUND ( 'NONE', #33209, .T. ) ;
#73345 = LINE ( 'NONE', #51148, #169603 ) ;
#73344 = DIRECTION ( 'NONE',  ( -0.000000000000000000, 1.000000000000000000, 6.982962677686267499E-15 ) ) ;
#73346 = ORIENTED_EDGE ( 'NONE', *, *, #45591, .T. ) ;
#73347 = ORIENTED_EDGE ( 'NONE', *, *, #121852, .F. ) ;
#73348 = EDGE_CURVE ( 'NONE', #38351, #182549, #136274, .T. ) ;
#73349 = DIRECTION ( 'NONE',  ( 1.000000000000000000, -0.000000000000000000, 0.000000000000000000 ) ) ;
#73350 = CARTESIAN_POINT ( 'NONE',  ( -16.87851181299898329, 9.950042924018893231, -180.1498564846330623 ) ) ;
#73351 = EDGE_CURVE ( 'NONE', #224073, #235880, #28193, .T. ) ;
#73352 = FACE_OUTER_BOUND ( 'NONE', #194796, .T. ) ;
#73353 = ORIENTED_EDGE ( 'NONE', *, *, #38107, .F. ) ;
#73354 = EDGE_LOOP ( 'NONE', ( #86464, #113260, #52812 ) ) ;
#73355 = AXIS2_PLACEMENT_3D ( 'NONE', #44731, #124272, #141258 ) ;
#73356 = DIRECTION ( 'NONE',  ( 0.000000000000000000, 0.4088369013363311599, -0.9126074666063757057 ) ) ;
#73357 = CARTESIAN_POINT ( 'NONE',  ( 22.39999999999999858, 75.90000000001219860, -144.3138870828976792 ) ) ;
#73358 = CARTESIAN_POINT ( 'NONE',  ( -20.54999999999999716, 1.115600667400684642E-11, -180.4749999999999659 ) ) ;
#73360 = ORIENTED_EDGE ( 'NONE', *, *, #150171, .T. ) ;
#73359 = FACE_OUTER_BOUND ( 'NONE', #47781, .T. ) ;
#73361 = DIRECTION ( 'NONE',  ( 0.000000000000000000, -0.4999999999999088507, -0.8660254037844913322 ) ) ;
#73362 = EDGE_CURVE ( 'NONE', #30919, #43391, #219684, .T. ) ;
#73363 = CARTESIAN_POINT ( 'NONE',  ( -20.94999999999999929, 72.06821323333463170, -225.0920403225231610 ) ) ;
#73364 = CARTESIAN_POINT ( 'NONE',  ( -20.54999999999999716, 76.00000000001126921, -203.5231074845248997 ) ) ;
#73365 = VERTEX_POINT ( 'NONE', #143534 ) ;
#73366 = DIRECTION ( 'NONE',  ( 1.000000000000000000, 0.000000000000000000, 0.000000000000000000 ) ) ;
#73367 = CARTESIAN_POINT ( 'NONE',  ( -18.40000000000000213, 11.41458325961093756, -180.1499999999999488 ) ) ;
#73368 = EDGE_CURVE ( 'NONE', #89147, #36696, #65566, .T. ) ;
#73369 = CARTESIAN_POINT ( 'NONE',  ( -23.15000000000000213, 31.89597452117651244, -238.9192857152811769 ) ) ;
#73371 = DIRECTION ( 'NONE',  ( 1.000000000000000000, -0.000000000000000000, -0.000000000000000000 ) ) ;
#73370 = FACE_OUTER_BOUND ( 'NONE', #217977, .T. ) ;
#73372 = DIRECTION ( 'NONE',  ( 0.000000000000000000, 1.000000000000000000, 0.000000000000000000 ) ) ;
#73373 = TOROIDAL_SURFACE ( 'NONE', #60656, 0.4000000000000017431, 0.1000000000000000056 ) ;
#73375 = EDGE_CURVE ( 'NONE', #1130, #35113, #78030, .T. ) ;
#73374 = DIRECTION ( 'NONE',  ( -1.000000000000000000, -0.000000000000000000, -0.000000000000000000 ) ) ;
#73376 = LINE ( 'NONE', #96726, #180592 ) ;
#73377 = CIRCLE ( 'NONE', #85202, 0.5000000000000004441 ) ;
#73378 = CARTESIAN_POINT ( 'NONE',  ( 18.59999999999999432, 74.26374286841520700, -191.9544551555068779 ) ) ;
#73379 = VECTOR ( 'NONE', #186290, 1000.000000000000000 ) ;
#73380 = ORIENTED_EDGE ( 'NONE', *, *, #124571, .T. ) ;
#73381 = AXIS2_PLACEMENT_3D ( 'NONE', #250283, #191630, #172067 ) ;
#73382 = B_SPLINE_CURVE_WITH_KNOTS ( 'NONE', 3,
 ( #224274, #144726, #226846, #126466, #7816, #203443, #24831 ),
 .UNSPECIFIED., .F., .F.,
 ( 4, 3, 4 ),
 ( 3.469446951953614189E-18, 3.882884552234413058E-05, 5.798605692158429121E-05 ),
 .UNSPECIFIED. ) ;
#73383 = EDGE_LOOP ( 'NONE', ( #187326, #232818, #36674, #89967 ) ) ;
#73384 = CARTESIAN_POINT ( 'NONE',  ( -18.59999999999999787, 6.846123162363745074, -104.2377262668499043 ) ) ;
#73385 = DIRECTION ( 'NONE',  ( -1.000000000000000000, 0.000000000000000000, 0.000000000000000000 ) ) ;
#73386 = ORIENTED_EDGE ( 'NONE', *, *, #252822, .T. ) ;
#73387 = ADVANCED_FACE ( 'NONE', ( #26178 ), #211324, .T. ) ;
#73388 = DIRECTION ( 'NONE',  ( 1.000000000000000000, 0.000000000000000000, 0.000000000000000000 ) ) ;
#73389 = ORIENTED_EDGE ( 'NONE', *, *, #44048, .T. ) ;
#73390 = EDGE_CURVE ( 'NONE', #16272, #152584, #159274, .T. ) ;
#73391 = ORIENTED_EDGE ( 'NONE', *, *, #103570, .F. ) ;
#73392 = CARTESIAN_POINT ( 'NONE',  ( 22.47071067811865319, 7.720074744509199505, -66.90090754529744288 ) ) ;
#73393 = ORIENTED_EDGE ( 'NONE', *, *, #172646, .F. ) ;
#73394 =( BOUNDED_SURFACE ( )  B_SPLINE_SURFACE ( 3, 2, ( 
 ( #41081, #179308, #163579 ),
 ( #219678, #203974, #61905 ),
 ( #239261, #244380, #123167 ),
 ( #184410, #612, #222231 ) ),
 .UNSPECIFIED., .F., .F., .T. ) 
 B_SPLINE_SURFACE_WITH_KNOTS ( ( 4, 4 ),
 ( 3, 3 ),
 ( 0.0006461284895274055275, 0.0007503702773986016886 ),
 ( 0.000000000000000000, 1.000000000000000000 ),
 .UNSPECIFIED. ) 
 GEOMETRIC_REPRESENTATION_ITEM ( )  RATIONAL_B_SPLINE_SURFACE ( (
 ( 1.000000000000000000, 0.7071067811865475727, 1.000000000000000000),
 ( 1.000000000000000000, 0.7076476444648701625, 1.000000000000000000),
 ( 1.000000000000000000, 0.7075727925191833689, 1.000000000000000000),
 ( 1.000000000000000000, 0.7071067811865475727, 1.000000000000000000) ) ) 
 REPRESENTATION_ITEM ( '' )  SURFACE ( )  );
#73395 = CARTESIAN_POINT ( 'NONE',  ( 21.13614978966381841, 1.115648815929779806E-11, -161.0008952981661707 ) ) ;
#73396 = AXIS2_PLACEMENT_3D ( 'NONE', #105205, #139221, #218766 ) ;
#73397 = DIRECTION ( 'NONE',  ( -1.000000000000000000, -3.265361837132813093E-16, 0.000000000000000000 ) ) ;
#73398 = DIRECTION ( 'NONE',  ( 0.000000000000000000, -0.000000000000000000, -1.000000000000000000 ) ) ;
#73399 = LINE ( 'NONE', #159034, #66640 ) ;
#73400 = CARTESIAN_POINT ( 'NONE',  ( 23.24999999999999645, 20.70829660003285611, -234.6540061327600597 ) ) ;
#73403 = ORIENTED_EDGE ( 'NONE', *, *, #139381, .F. ) ;
#73402 = CARTESIAN_POINT ( 'NONE',  ( -16.96982749440706328, 29.78781364502790652, -234.5828580218738750 ) ) ;
#73401 = VECTOR ( 'NONE', #17037, 1000.000000000000000 ) ;
#73405 = CARTESIAN_POINT ( 'NONE',  ( -20.94999999999999929, -11.39257802169451317, -97.42605042016811012 ) ) ;
#73404 = CARTESIAN_POINT ( 'NONE',  ( 21.07954763557415490, 6.170303673189042826, -199.5887535105479174 ) ) ;
#73406 = CARTESIAN_POINT ( 'NONE',  ( 18.49999999999999645, -1.637172712959225507, -145.5821533654720383 ) ) ;
#73407 = CARTESIAN_POINT ( 'NONE',  ( 12.93225390519045170, 66.58234804117104488, -121.1643200920839263 ) ) ;
#73408 = VECTOR ( 'NONE', #14180, 1000.000000000000000 ) ;
#73409 = LINE ( 'NONE', #31717, #14744 ) ;
#73410 = DIRECTION ( 'NONE',  ( -3.265361837132813093E-16, 1.000000000000000000, -0.000000000000000000 ) ) ;
#73412 = EDGE_LOOP ( 'NONE', ( #79918, #73569, #127773, #196208 ) ) ;
#73411 = VECTOR ( 'NONE', #54674, 1000.000000000000000 ) ;
#73413 = CARTESIAN_POINT ( 'NONE',  ( -23.15000000000000213, 4.350000000011156054, -45.85000000000000142 ) ) ;
#73414 = ORIENTED_EDGE ( 'NONE', *, *, #35201, .F. ) ;
#73415 = DIRECTION ( 'NONE',  ( 1.000000000000000000, 0.000000000000000000, 0.000000000000000000 ) ) ;
#73416 = ORIENTED_EDGE ( 'NONE', *, *, #195409, .F. ) ;
#73417 = FACE_OUTER_BOUND ( 'NONE', #28145, .T. ) ;
#73418 = CIRCLE ( 'NONE', #40284, 11.74999999999999289 ) ;
#73419 = AXIS2_PLACEMENT_3D ( 'NONE', #74092, #17920, #97437 ) ;
#73420 = CYLINDRICAL_SURFACE ( 'NONE', #81969, 0.09999999999999939493 ) ;
#73421 = FACE_OUTER_BOUND ( 'NONE', #33506, .T. ) ;
#73422 = EDGE_LOOP ( 'NONE', ( #200388, #83075, #8885, #19682, #113186, #107848 ) ) ;
#73423 = ORIENTED_EDGE ( 'NONE', *, *, #162823, .T. ) ;
#73424 = DIRECTION ( 'NONE',  ( 0.000000000000000000, -0.9998779222360104635, -0.01562499999996343723 ) ) ;
#73425 = DIRECTION ( 'NONE',  ( -0.000000000000000000, -0.000000000000000000, 1.000000000000000000 ) ) ;
#73426 = FACE_OUTER_BOUND ( 'NONE', #128387, .T. ) ;
#73427 = LINE ( 'NONE', #151686, #169582 ) ;
#73428 = ADVANCED_FACE ( 'NONE', ( #49584 ), #245226, .T. ) ;
#73429 = AXIS2_PLACEMENT_3D ( 'NONE', #138332, #13287, #137077 ) ;
#73431 = CARTESIAN_POINT ( 'NONE',  ( 18.59999999999999432, 80.78317333349157536, -192.9003134612048882 ) ) ;
#73430 = FACE_OUTER_BOUND ( 'NONE', #183677, .T. ) ;
#73432 = DIRECTION ( 'NONE',  ( 1.000000000000000000, 0.000000000000000000, 0.000000000000000000 ) ) ;
#73433 = CARTESIAN_POINT ( 'NONE',  ( 20.94999999999999574, 72.05339752741123505, -225.0867394276846483 ) ) ;
#73434 = CARTESIAN_POINT ( 'NONE',  ( -20.94999999999999929, -11.64999999998884483, -103.4000000000000341 ) ) ;
#73435 = EDGE_LOOP ( 'NONE', ( #200285, #64246, #218878, #187830, #70416, #221343 ) ) ;
#73436 = CARTESIAN_POINT ( 'NONE',  ( 23.25000000000000000, -8.729782940176418649, -238.4538547387928986 ) ) ;
#73438 = EDGE_LOOP ( 'NONE', ( #200582, #226461, #21252, #212897 ) ) ;
#73437 = CARTESIAN_POINT ( 'NONE',  ( 17.74533788810829904, 10.81849979148194940, -56.68637732505243321 ) ) ;
#73439 = DIRECTION ( 'NONE',  ( -1.000000000000000000, 0.000000000000000000, -0.000000000000000000 ) ) ;
#73440 = DIRECTION ( 'NONE',  ( -1.000000000000000000, 0.000000000000000000, 0.000000000000000000 ) ) ;
#73442 = DIRECTION ( 'NONE',  ( -1.000000000000000000, -0.000000000000000000, -0.000000000000000000 ) ) ;
#73441 = LINE ( 'NONE', #152987, #8660 ) ;
#73443 = ADVANCED_FACE ( 'NONE', ( #91285 ), #149993, .F. ) ;
#73444 = DIRECTION ( 'NONE',  ( 1.000000000000000000, 0.000000000000000000, 0.000000000000000000 ) ) ;
#73446 = ORIENTED_EDGE ( 'NONE', *, *, #34626, .T. ) ;
#73445 = CARTESIAN_POINT ( 'NONE',  ( -15.75000000000000355, 62.59162599727320497, -217.2417264603073477 ) ) ;
#73447 = CARTESIAN_POINT ( 'NONE',  ( 18.59999999999999076, 8.433899723187009201, -209.4150263691077782 ) ) ;
#73448 = CARTESIAN_POINT ( 'NONE',  ( -23.15000000000000213, 4.350000000011156054, -155.2500000000000284 ) ) ;
#73449 = CARTESIAN_POINT ( 'NONE',  ( 33.80000000000000426, 3.175288713399626594, 33.00000000000000000 ) ) ;
#73450 = DIRECTION ( 'NONE',  ( 0.000000000000000000, 0.000000000000000000, -1.000000000000000000 ) ) ;
#73452 = CARTESIAN_POINT ( 'NONE',  ( -18.56579813702275672, 10.33025634372637391, -139.5870929282639281 ) ) ;
#73451 = SHAPE_REPRESENTATION ( 'Snap Open Cable Crossbars 13', ( #2425 ), #227278 ) ;
#73453 = ORIENTED_EDGE ( 'NONE', *, *, #190307, .T. ) ;
#73454 = CARTESIAN_POINT ( 'NONE',  ( 18.41789779300693652, -7.785976411356864801, -209.8926135142695273 ) ) ;
#73455 = AXIS2_PLACEMENT_3D ( 'NONE', #129006, #130265, #52006 ) ;
#73456 = EDGE_CURVE ( 'NONE', #218579, #92785, #148789, .T. ) ;
#73458 = EDGE_CURVE ( 'NONE', #84528, #125683, #15719, .T. ) ;
#73457 = ORIENTED_EDGE ( 'NONE', *, *, #39055, .T. ) ;
#73459 = AXIS2_PLACEMENT_3D ( 'NONE', #45530, #125078, #46794 ) ;
#73460 = DIRECTION ( 'NONE',  ( 0.000000000000000000, 0.000000000000000000, 1.000000000000000000 ) ) ;
#73461 = VERTEX_POINT ( 'NONE', #30046 ) ;
#73462 = CARTESIAN_POINT ( 'NONE',  ( 20.94999999999999929, 1.115600667400684642E-11, -167.5000000000000284 ) ) ;
#73463 = VERTEX_POINT ( 'NONE', #169576 ) ;
#73464 = VECTOR ( 'NONE', #173034, 1000.000000000000114 ) ;
#73465 = DIRECTION ( 'NONE',  ( 0.7071067811865474617, 0.7071067811865474617, 0.000000000000000000 ) ) ;
#73466 = EDGE_CURVE ( 'NONE', #132466, #186768, #23908, .T. ) ;
#73468 = EDGE_CURVE ( 'NONE', #74301, #128415, #232187, .T. ) ;
#73467 = CARTESIAN_POINT ( 'NONE',  ( -20.94999999999999929, 74.83729825007360148, -61.62310748452433273 ) ) ;
#73469 = ORIENTED_EDGE ( 'NONE', *, *, #241848, .T. ) ;
#73470 = AXIS2_PLACEMENT_3D ( 'NONE', #110826, #67851, #187826 ) ;
#73472 = CIRCLE ( 'NONE', #48490, 2.000000000000001776 ) ;
#73471 = FACE_OUTER_BOUND ( 'NONE', #37551, .T. ) ;
#73473 = DIRECTION ( 'NONE',  ( 0.000000000000000000, 6.982962677686267499E-15, -1.000000000000000000 ) ) ;
#73474 = CIRCLE ( 'NONE', #173464, 0.1000000000000028644 ) ;
#73475 = DIRECTION ( 'NONE',  ( -1.000000000000000000, 0.000000000000000000, 0.000000000000000000 ) ) ;
#73476 = CARTESIAN_POINT ( 'NONE',  ( 21.53551880898956838, 6.608334920795639000, -199.4594853955832434 ) ) ;
#73477 = LINE ( 'NONE', #12211, #248667 ) ;
#73478 = ORIENTED_EDGE ( 'NONE', *, *, #6689, .F. ) ;
#73479 = FACE_OUTER_BOUND ( 'NONE', #257190, .T. ) ;
#73480 = EDGE_LOOP ( 'NONE', ( #32584, #109280, #192956 ) ) ;
#73482 = EDGE_LOOP ( 'NONE', ( #252614, #111497, #229190, #118189, #174121, #109295, #129728 ) ) ;
#73481 = DIRECTION ( 'NONE',  ( 1.000000000000000000, -0.000000000000000000, 0.000000000000000000 ) ) ;
#73483 = EDGE_LOOP ( 'NONE', ( #121765, #169178, #18770, #256325 ) ) ;
#73484 = CARTESIAN_POINT ( 'NONE',  ( -20.00857864376270001, 52.31097543990284038, -232.5130202284001371 ) ) ;
#73485 = ADVANCED_FACE ( 'NONE', ( #131683 ), #50835, .T. ) ;
#73486 = LINE ( 'NONE', #53892, #54934 ) ;
#73487 = DIRECTION ( 'NONE',  ( 0.000000000000000000, 0.000000000000000000, -1.000000000000000000 ) ) ;
#73488 = CARTESIAN_POINT ( 'NONE',  ( 18.59999999999999076, 14.05000000001116689, -139.5136950707610026 ) ) ;
#73490 = ORIENTED_EDGE ( 'NONE', *, *, #251535, .F. ) ;
#73489 = CIRCLE ( 'NONE', #248412, 7.720710678118663850 ) ;
#73491 = CARTESIAN_POINT ( 'NONE',  ( 18.59999999999999076, 10.20857864377385127, -88.35000000000003695 ) ) ;
#73492 = DIRECTION ( 'NONE',  ( 0.000000000000000000, -1.000000000000000000, -6.982962677686266711E-15 ) ) ;
#73493 = EDGE_LOOP ( 'NONE', ( #212046, #241573, #115891, #78689 ) ) ;
#73495 = ORIENTED_EDGE ( 'NONE', *, *, #256880, .T. ) ;
#73494 = CARTESIAN_POINT ( 'NONE',  ( 21.05000000000000071, 82.57900542960499024, -215.5587758314583766 ) ) ;
#73496 = DIRECTION ( 'NONE',  ( -1.000000000000000000, -2.952720810173289112E-16, 0.000000000000000000 ) ) ;
#73498 = ADVANCED_FACE ( 'NONE', ( #186533 ), #71728, .T. ) ;
#73497 = DIRECTION ( 'NONE',  ( 0.000000000000000000, 0.000000000000000000, -1.000000000000000000 ) ) ;
#73499 = DIRECTION ( 'NONE',  ( 1.000000000000000000, 0.000000000000000000, 0.000000000000000000 ) ) ;
#73500 = AXIS2_PLACEMENT_3D ( 'NONE', #26551, #30402, #188185 ) ;
#73501 = EDGE_LOOP ( 'NONE', ( #111642, #79221, #52281, #257730 ) ) ;
#73502 = AXIS2_PLACEMENT_3D ( 'NONE', #48945, #131054, #250984 ) ;
#73503 = AXIS2_PLACEMENT_3D ( 'NONE', #62586, #99109, #59990 ) ;
#73504 = AXIS2_PLACEMENT_3D ( 'NONE', #39023, #76839, #140667 ) ;
#73505 = ORIENTED_EDGE ( 'NONE', *, *, #252470, .T. ) ;
#73506 = CARTESIAN_POINT ( 'NONE',  ( 20.94999999999999929, 21.98309897467606433, -231.7335930323676791 ) ) ;
#73507 = DIRECTION ( 'NONE',  ( 0.7071359030027126735, -0.6232856014206268336, 0.3338770338706537610 ) ) ;
#73508 = ORIENTED_EDGE ( 'NONE', *, *, #205604, .F. ) ;
#73509 = CYLINDRICAL_SURFACE ( 'NONE', #162877, 0.5000000000000004441 ) ;
#73510 = CARTESIAN_POINT ( 'NONE',  ( 18.59999999999999432, 16.50669723772569952, -240.7258389668962479 ) ) ;
#73511 = DIRECTION ( 'NONE',  ( -1.000000000000000000, -0.000000000000000000, -0.000000000000000000 ) ) ;
#73512 = ADVANCED_FACE ( 'NONE', ( #247777 ), #90498, .T. ) ;
#73513 = AXIS2_PLACEMENT_3D ( 'NONE', #194936, #191095, #230190 ) ;
#73514 = AXIS2_PLACEMENT_3D ( 'NONE', #41630, #201971, #22059 ) ;
#73515 = AXIS2_PLACEMENT_3D ( 'NONE', #15816, #94020, #18350 ) ;
#73516 = ORIENTED_EDGE ( 'NONE', *, *, #124426, .F. ) ;
#73517 = DIRECTION ( 'NONE',  ( 1.000000000000000000, 0.000000000000000000, 0.000000000000000000 ) ) ;
#73518 = EDGE_CURVE ( 'NONE', #101582, #112033, #11420, .T. ) ;
#73519 = VECTOR ( 'NONE', #124796, 1000.000000000000000 ) ;
#73520 = EDGE_CURVE ( 'NONE', #204695, #46891, #6046, .T. ) ;
#73521 = ORIENTED_EDGE ( 'NONE', *, *, #184504, .T. ) ;
#73522 = CARTESIAN_POINT ( 'NONE',  ( -20.94999999999999929, 11.65000000001115232, -60.21613433702190576 ) ) ;
#73523 = CARTESIAN_POINT ( 'NONE',  ( -18.50000000000000000, 0.8650195716890449749, -212.6652626294507229 ) ) ;
#73525 = EDGE_LOOP ( 'NONE', ( #62663, #215578, #83084, #28313 ) ) ;
#73524 = CARTESIAN_POINT ( 'NONE',  ( 15.52844286134408769, 25.54333932933833751, -232.9607505220590440 ) ) ;
#73526 = DIRECTION ( 'NONE',  ( -1.000000000000000000, -0.000000000000000000, -0.000000000000000000 ) ) ;
#73527 = CARTESIAN_POINT ( 'NONE',  ( -21.05000000000000071, -11.75000000000000000, -30.59999999999999432 ) ) ;
#73529 = ADVANCED_FACE ( 'NONE', ( #86101 ), #147396, .T. ) ;
#73528 = LINE ( 'NONE', #52637, #97688 ) ;
#73530 = EDGE_CURVE ( 'NONE', #20565, #138502, #223775, .T. ) ;
#73531 = CARTESIAN_POINT ( 'NONE',  ( 21.04999999999999716, 6.496686585779318790, -33.51465611851394755 ) ) ;
#73532 = CARTESIAN_POINT ( 'NONE',  ( 21.05000000000000071, 7.525330762710603416, -212.0571253909869256 ) ) ;
#73533 = CARTESIAN_POINT ( 'NONE',  ( 21.08884785362045378, 6.357193367436396514, -66.95021690493318545 ) ) ;
#73535 = ORIENTED_EDGE ( 'NONE', *, *, #32166, .T. ) ;
#73534 = CYLINDRICAL_SURFACE ( 'NONE', #181795, 0.09999999999999939493 ) ;
#73536 = EDGE_CURVE ( 'NONE', #167673, #209133, #55971, .T. ) ;
#73537 = EDGE_CURVE ( 'NONE', #108030, #252270, #177261, .T. ) ;
#73538 = AXIS2_PLACEMENT_3D ( 'NONE', #70437, #211191, #52098 ) ;
#73540 = ADVANCED_FACE ( 'NONE', ( #212526 ), #18150, .T. ) ;
#73539 = EDGE_CURVE ( 'NONE', #154576, #183114, #43479, .T. ) ;
#73541 = DIRECTION ( 'NONE',  ( -0.7070776581708965169, 0.7071359030027827286, 4.937903618720407826E-15 ) ) ;
#73542 = CARTESIAN_POINT ( 'NONE',  ( -18.44232395689959247, 85.55228255706151685, -62.68085549971750936 ) ) ;
#73543 = SPHERICAL_SURFACE ( 'NONE', #213889, 0.1000000000000000056 ) ;
#73544 = AXIS2_PLACEMENT_3D ( 'NONE', #140044, #176650, #155809 ) ;
#73545 = EDGE_LOOP ( 'NONE', ( #200005, #70692, #132195, #96330 ) ) ;
#73546 = DIRECTION ( 'NONE',  ( 1.000000000000000000, 0.000000000000000000, 0.000000000000000000 ) ) ;
#73547 = EDGE_CURVE ( 'NONE', #45859, #200649, #192950, .T. ) ;
#73548 = DIRECTION ( 'NONE',  ( 0.000000000000000000, 1.000000000000000000, -6.308085367188393199E-16 ) ) ;
#73549 = CARTESIAN_POINT ( 'NONE',  ( 20.94999999999999929, 4.999999999999997335, -12.40526601891309788 ) ) ;
#73550 = TOROIDAL_SURFACE ( 'NONE', #160844, 0.2000000000000000111, 0.1000000000000000056 ) ;
#73551 = EDGE_LOOP ( 'NONE', ( #167939, #71444, #231036, #162083 ) ) ;
#73552 = EDGE_CURVE ( 'NONE', #76812, #82079, #74450, .T. ) ;
#73553 = ADVANCED_FACE ( 'NONE', ( #157713 ), #78216, .F. ) ;
#73554 = AXIS2_PLACEMENT_3D ( 'NONE', #138361, #163105, #256996 ) ;
#73555 = AXIS2_PLACEMENT_3D ( 'NONE', #131000, #69763, #187149 ) ;
#73556 = SPHERICAL_SURFACE ( 'NONE', #164292, 0.1000000000000000056 ) ;
#73557 = CARTESIAN_POINT ( 'NONE',  ( -21.46681500593047431, 60.61285123220599758, -234.0601523988342194 ) ) ;
#73558 = EDGE_CURVE ( 'NONE', #26051, #107789, #58543, .T. ) ;
#73559 = ORIENTED_EDGE ( 'NONE', *, *, #248933, .F. ) ;
#73560 = CARTESIAN_POINT ( 'NONE',  ( 18.59999999999999076, 1.835341550235567887, -45.15515129256298366 ) ) ;
#73561 = EDGE_LOOP ( 'NONE', ( #14712, #234322, #45990, #189799 ) ) ;
#73563 = EDGE_LOOP ( 'NONE', ( #99448, #194916, #103238, #258070 ) ) ;
#73562 = CARTESIAN_POINT ( 'NONE',  ( -15.75000000000000355, 9.850000000011133849, -150.7500000000000284 ) ) ;
#73564 = EDGE_CURVE ( 'NONE', #198292, #257935, #190686, .T. ) ;
#73565 = DIRECTION ( 'NONE',  ( -1.000000000000000000, 9.012599976028471648E-15, 6.882867235861662930E-14 ) ) ;
#73566 = VERTEX_POINT ( 'NONE', #174715 ) ;
#73567 = DIRECTION ( 'NONE',  ( 0.000000000000000000, 1.000000000000000000, 0.000000000000000000 ) ) ;
#73568 = VERTEX_POINT ( 'NONE', #215068 ) ;
#73570 = ORIENTED_EDGE ( 'NONE', *, *, #62932, .F. ) ;
#73569 = ORIENTED_EDGE ( 'NONE', *, *, #235317, .F. ) ;
#73571 = DIRECTION ( 'NONE',  ( -1.000000000000000000, 0.000000000000000000, 0.000000000000000000 ) ) ;
#73573 = ORIENTED_EDGE ( 'NONE', *, *, #53537, .F. ) ;
#73572 = CARTESIAN_POINT ( 'NONE',  ( 21.05193202509564898, 10.72393601970834354, -146.1725346033257722 ) ) ;
#73574 = CARTESIAN_POINT ( 'NONE',  ( 20.94999999999999929, 65.70711192142346135, -64.06510546851221477 ) ) ;
#73576 = ORIENTED_EDGE ( 'NONE', *, *, #190314, .T. ) ;
#73575 = AXIS2_PLACEMENT_3D ( 'NONE', #149097, #10860, #73424 ) ;
#73577 = VECTOR ( 'NONE', #107508, 1000.000000000000000 ) ;
#73578 = CIRCLE ( 'NONE', #194382, 0.1999999999999945155 ) ;
#73579 = ORIENTED_EDGE ( 'NONE', *, *, #152964, .T. ) ;
#73580 = CARTESIAN_POINT ( 'NONE',  ( -18.50000000000000000, 77.63717271298224887, -91.44095411905229298 ) ) ;
#73581 = CARTESIAN_POINT ( 'NONE',  ( 21.12642695952774119, 75.90109671682233738, -75.89876740655950016 ) ) ;
#73582 = CARTESIAN_POINT ( 'NONE',  ( 20.94999999999999574, 74.16465844978819177, -191.8679561919614116 ) ) ;
#73583 = ORIENTED_EDGE ( 'NONE', *, *, #230229, .T. ) ;
#73584 = AXIS2_PLACEMENT_3D ( 'NONE', #114223, #193764, #75128 ) ;
#73585 = FACE_OUTER_BOUND ( 'NONE', #166907, .T. ) ;
#73586 = CIRCLE ( 'NONE', #215207, 0.09999999999999939493 ) ;
#73587 = CARTESIAN_POINT ( 'NONE',  ( 21.11344571971309136, 65.38212097649309840, -57.27708659212506603 ) ) ;
#73588 = DIRECTION ( 'NONE',  ( -0.000000000000000000, 1.000000000000000000, -0.000000000000000000 ) ) ;
#73589 = VERTEX_POINT ( 'NONE', #255426 ) ;
#73590 = DIRECTION ( 'NONE',  ( -1.000000000000000000, -0.000000000000000000, 0.000000000000000000 ) ) ;
#73591 = CARTESIAN_POINT ( 'NONE',  ( 22.59999999999999432, 0.1000000000111554016, -55.35042919245524473 ) ) ;
#73592 = CARTESIAN_POINT ( 'NONE',  ( -22.57320508075687115, 64.25000000001215028, -136.5231074845243597 ) ) ;
#73593 = B_SPLINE_CURVE_WITH_KNOTS ( 'NONE', 3,
 ( #19184, #196529, #257734, #218651, #80398, #40066, #239523 ),
 .UNSPECIFIED., .F., .F.,
 ( 4, 3, 4 ),
 ( 0.000000000000000000, 1.860045280645939271E-05, 5.251155757305736512E-05 ),
 .UNSPECIFIED. ) ;
#73594 = ORIENTED_EDGE ( 'NONE', *, *, #129172, .F. ) ;
#73595 = CARTESIAN_POINT ( 'NONE',  ( -16.91049119928363709, 14.16575171929611798, -219.2860664115342786 ) ) ;
#73596 = EDGE_LOOP ( 'NONE', ( #35722, #113133, #107363, #191507 ) ) ;
#73597 = DIRECTION ( 'NONE',  ( -7.304098846218134667E-16, 0.4088369013363281068, -0.9126074666063770380 ) ) ;
#73598 = ORIENTED_EDGE ( 'NONE', *, *, #179678, .T. ) ;
#73599 = CIRCLE ( 'NONE', #219306, 0.09999999999999939493 ) ;
#73600 = AXIS2_PLACEMENT_3D ( 'NONE', #57921, #137462, #136157 ) ;
#73601 = AXIS2_PLACEMENT_3D ( 'NONE', #63156, #222217, #219666 ) ;
#73602 = CARTESIAN_POINT ( 'NONE',  ( 22.88900146558018989, 8.703904791123973084, -154.8500000000000227 ) ) ;
#73603 = ORIENTED_EDGE ( 'NONE', *, *, #79417, .F. ) ;
#73604 = ORIENTED_EDGE ( 'NONE', *, *, #52839, .F. ) ;
#73605 = DIRECTION ( 'NONE',  ( 1.000000000000000000, -0.000000000000000000, -0.000000000000000000 ) ) ;
#73606 = DIRECTION ( 'NONE',  ( -0.000000000000000000, 0.6132151058540549204, -0.7899159663865520375 ) ) ;
#73607 = VERTEX_POINT ( 'NONE', #36465 ) ;
#73608 = ORIENTED_EDGE ( 'NONE', *, *, #9246, .T. ) ;
#73609 = CARTESIAN_POINT ( 'NONE',  ( -18.59999999999999787, 77.83534155023598089, -57.86795619196132634 ) ) ;
#73610 = CARTESIAN_POINT ( 'NONE',  ( -18.56579813702276027, 65.66974365629646115, -63.93601455626048136 ) ) ;
#73611 = EDGE_LOOP ( 'NONE', ( #132670, #153250, #42070, #57557 ) ) ;
#73612 = EDGE_CURVE ( 'NONE', #133691, #179534, #244804, .T. ) ;
#73613 = TOROIDAL_SURFACE ( 'NONE', #219317, 0.2000000000000000111, 0.1000000000000000056 ) ;
#73614 = EDGE_CURVE ( 'NONE', #67516, #129211, #211506, .T. ) ;
#73615 = ORIENTED_EDGE ( 'NONE', *, *, #79383, .F. ) ;
#73616 = PLANE ( 'NONE',  #35176 ) ;
#73617 = ADVANCED_FACE ( 'NONE', ( #216346 ), #74167, .T. ) ;
#73618 = CYLINDRICAL_SURFACE ( 'NONE', #126316, 12.87499999999999822 ) ;
#73619 = ADVANCED_FACE ( 'NONE', ( #117261 ), #80668, .T. ) ;
#73620 = CARTESIAN_POINT ( 'NONE',  ( 18.49999999999999645, 76.00000000001126921, -203.5231074845248997 ) ) ;
#73622 = VERTEX_POINT ( 'NONE', #22018 ) ;
#73621 = FACE_OUTER_BOUND ( 'NONE', #127484, .T. ) ;
#73623 = CIRCLE ( 'NONE', #252453, 1.749999999999999778 ) ;
#73624 = DIRECTION ( 'NONE',  ( -4.408576920032448588E-17, 0.8490545835447252943, 0.5283051335749948674 ) ) ;
#73625 = CARTESIAN_POINT ( 'NONE',  ( -22.59999999999999787, 12.58798907299599001, -223.3278890275437050 ) ) ;
#73626 = CARTESIAN_POINT ( 'NONE',  ( -18.59999999999999787, 43.08613539620618837, -254.3146655184800409 ) ) ;
#73628 = LINE ( 'NONE', #153179, #224310 ) ;
#73627 = DIRECTION ( 'NONE',  ( 0.000000000000000000, -6.652207440891554563E-15, 1.000000000000000000 ) ) ;
#73630 = CIRCLE ( 'NONE', #77666, 11.75000000000000355 ) ;
#73629 = DIRECTION ( 'NONE',  ( 0.000000000000000000, 0.000000000000000000, -1.000000000000000000 ) ) ;
#73631 = AXIS2_PLACEMENT_3D ( 'NONE', #198607, #1684, #19998 ) ;
#73632 = DIRECTION ( 'NONE',  ( -1.000000000000000000, -2.952720810173289112E-16, 0.000000000000000000 ) ) ;
#73633 = CYLINDRICAL_SURFACE ( 'NONE', #164321, 12.87499999999999822 ) ;
#73634 = DIRECTION ( 'NONE',  ( -1.000000000000000000, -0.000000000000000000, -0.000000000000000000 ) ) ;
#73636 = ORIENTED_EDGE ( 'NONE', *, *, #73316, .T. ) ;
#73635 = TOROIDAL_SURFACE ( 'NONE', #211160, 0.2000000000000000111, 0.1000000000000000056 ) ;
#73637 = EDGE_CURVE ( 'NONE', #201851, #140921, #61942, .T. ) ;
#73638 = EDGE_CURVE ( 'NONE', #11990, #60888, #223952, .T. ) ;
#73640 = EDGE_LOOP ( 'NONE', ( #160978, #173554 ) ) ;
#73639 = DIRECTION ( 'NONE',  ( 1.000000000000000000, 2.952720810173289112E-16, -0.000000000000000000 ) ) ;
#73641 = DIRECTION ( 'NONE',  ( 0.000000000000000000, 0.000000000000000000, -1.000000000000000000 ) ) ;
#73642 = CIRCLE ( 'NONE', #36231, 4.000000000000002665 ) ;
#73643 = CARTESIAN_POINT ( 'NONE',  ( -33.30000000000001137, 3.332938107839112263, 33.00000000000000000 ) ) ;
#73644 = ORIENTED_EDGE ( 'NONE', *, *, #57623, .F. ) ;
#73645 = SURFACE_STYLE_USAGE ( .BOTH. , #151895 ) ;
#73646 = EDGE_CURVE ( 'NONE', #224589, #209479, #3715, .T. ) ;
#73647 = DIRECTION ( 'NONE',  ( 0.000000000000000000, 0.000000000000000000, 1.000000000000000000 ) ) ;
#73648 = EDGE_CURVE ( 'NONE', #101456, #187411, #221460, .T. ) ;
#73649 = DIRECTION ( 'NONE',  ( 0.000000000000000000, 0.8496786552930157832, 0.5273008465188090410 ) ) ;
#73650 = ORIENTED_EDGE ( 'NONE', *, *, #84640, .T. ) ;
#73651 = VERTEX_POINT ( 'NONE', #239774 ) ;
#73652 = FACE_OUTER_BOUND ( 'NONE', #112474, .T. ) ;
#73653 = CARTESIAN_POINT ( 'NONE',  ( 18.39999999999998082, 11.47316190337362585, -42.75000000000000000 ) ) ;
#73654 = CIRCLE ( 'NONE', #52760, 11.65000000000000036 ) ;
#73655 = CARTESIAN_POINT ( 'NONE',  ( 21.17356465864818915, 0.09891124102502621418, -94.07719687375829665 ) ) ;
#73657 = ORIENTED_EDGE ( 'NONE', *, *, #184695, .F. ) ;
#73656 = CARTESIAN_POINT ( 'NONE',  ( -16.97683809663752186, 44.86297841676466902, -235.0825981793917094 ) ) ;
#73658 = CARTESIAN_POINT ( 'NONE',  ( -23.25000000000000000, 0.000000000000000000, -33.50000000000000000 ) ) ;
#73659 = EDGE_CURVE ( 'NONE', #37719, #85479, #28376, .T. ) ;
#73661 = EDGE_LOOP ( 'NONE', ( #42480, #150220, #144732, #35758 ) ) ;
#73660 = CARTESIAN_POINT ( 'NONE',  ( -18.59999999999999787, -1.835859311432481045, -78.50443916879852679 ) ) ;
#73662 = CARTESIAN_POINT ( 'NONE',  ( -21.04999999999999716, 10.27539803298866516, -228.0704349406337030 ) ) ;
#73663 = DIRECTION ( 'NONE',  ( 0.000000000000000000, 0.000000000000000000, -1.000000000000000000 ) ) ;
#73664 = CARTESIAN_POINT ( 'NONE',  ( 11.60000000000006182, 67.65000000001118963, -16.98168612828748891 ) ) ;
#73665 = EDGE_CURVE ( 'NONE', #127337, #99016, #222754, .T. ) ;
#73666 = DIRECTION ( 'NONE',  ( 0.000000000000000000, -1.000000000000000000, 0.000000000000000000 ) ) ;
#73668 = CARTESIAN_POINT ( 'NONE',  ( 20.12481660106788084, 9.526343992285099205, -108.7261416690930815 ) ) ;
#73667 = DIRECTION ( 'NONE',  ( 1.000000000000000000, 0.000000000000000000, 0.000000000000000000 ) ) ;
#73669 = LINE ( 'NONE', #235268, #91266 ) ;
#73671 = EDGE_CURVE ( 'NONE', #201752, #227236, #240725, .T. ) ;
#73670 = CARTESIAN_POINT ( 'NONE',  ( 18.59999999999999076, 65.79142135624910281, -81.67310748452439384 ) ) ;
#73672 = DIRECTION ( 'NONE',  ( 0.000000000000000000, 0.000000000000000000, -1.000000000000000000 ) ) ;
#73673 = CIRCLE ( 'NONE', #102844, 0.09999999999999939493 ) ;
#73674 = AXIS2_PLACEMENT_3D ( 'NONE', #120513, #202587, #103463 ) ;
#73675 = LINE ( 'NONE', #35822, #76549 ) ;
#73676 = AXIS2_PLACEMENT_3D ( 'NONE', #165541, #245062, #126396 ) ;
#73678 = DIRECTION ( 'NONE',  ( 0.000000000000000000, 0.000000000000000000, -1.000000000000000000 ) ) ;
#73677 = AXIS2_PLACEMENT_3D ( 'NONE', #133626, #213161, #167646 ) ;
#73679 = ORIENTED_EDGE ( 'NONE', *, *, #103315, .F. ) ;
#73680 = EDGE_CURVE ( 'NONE', #37930, #56204, #44143, .T. ) ;
#73681 = DIRECTION ( 'NONE',  ( 0.000000000000000000, -1.000000000000000000, -5.551115123125777653E-14 ) ) ;
#73682 = VERTEX_POINT ( 'NONE', #4975 ) ;
#73683 = VERTEX_POINT ( 'NONE', #101492 ) ;
#73684 = LINE ( 'NONE', #232744, #106952 ) ;
#73685 = ADVANCED_FACE ( 'NONE', ( #201929 ), #164087, .F. ) ;
#73686 = EDGE_LOOP ( 'NONE', ( #3452, #86524, #67860, #109998 ) ) ;
#73687 = EDGE_CURVE ( 'NONE', #22291, #201039, #107452, .T. ) ;
#73688 = AXIS2_PLACEMENT_3D ( 'NONE', #119247, #183072, #100903 ) ;
#73689 = CARTESIAN_POINT ( 'NONE',  ( -21.14999999999999858, 30.68987205111127636, -252.2252246220829193 ) ) ;
#73690 = SHAPE_REPRESENTATION_RELATIONSHIP ( 'NONE' , 'NONE' ,  #108449, #194461 ) ;
#73691 = CIRCLE ( 'NONE', #177912, 0.1000000000000028644 ) ;
#73692 = EDGE_LOOP ( 'NONE', ( #168265, #12945, #736, #66213 ) ) ;
#73693 = ORIENTED_EDGE ( 'NONE', *, *, #54937, .T. ) ;
#73694 = DIRECTION ( 'NONE',  ( -0.000000000000000000, -0.9910827722268039652, 0.1332476588733665090 ) ) ;
#73695 = CARTESIAN_POINT ( 'NONE',  ( 23.14999999999999858, 71.00000000001199396, -114.9283735034374274 ) ) ;
#73696 = AXIS2_PLACEMENT_3D ( 'NONE', #212045, #76346, #249869 ) ;
#73697 = DIRECTION ( 'NONE',  ( 1.000000000000000000, 0.000000000000000000, 0.000000000000000000 ) ) ;
#73698 = CARTESIAN_POINT ( 'NONE',  ( -21.05000000000000071, 1.115600667400684642E-11, -167.4999999999999716 ) ) ;
#73699 = CARTESIAN_POINT ( 'NONE',  ( -18.50000000000000000, 11.50215294792677057, -198.5972978622482970 ) ) ;
#73700 = ADVANCED_FACE ( 'NONE', ( #224038 ), #45415, .F. ) ;
#73701 = DIRECTION ( 'NONE',  ( 1.000000000000000000, 0.000000000000000000, 0.000000000000000000 ) ) ;
#73702 = CARTESIAN_POINT ( 'NONE',  ( 18.49999999999999289, 10.23906162413259402, -58.25439743459697439 ) ) ;
#73704 = EDGE_LOOP ( 'NONE', ( #55029, #80829, #63989, #19236, #24849 ) ) ;
#73703 = SPHERICAL_SURFACE ( 'NONE', #223088, 0.1000000000000000056 ) ;
#73706 = DIRECTION ( 'NONE',  ( -1.000000000000000000, 0.000000000000000000, 0.000000000000000000 ) ) ;
#73705 = CARTESIAN_POINT ( 'NONE',  ( 23.14999999999999503, 6.450000000000001066, -21.15000000000000213 ) ) ;
#73707 = DIRECTION ( 'NONE',  ( -0.000000000000000000, -0.000000000000000000, 1.000000000000000000 ) ) ;
#73708 = VERTEX_POINT ( 'NONE', #79392 ) ;
#73709 = CARTESIAN_POINT ( 'NONE',  ( -18.46093223321767596, -9.480682968263407062, -174.5845505139266436 ) ) ;
#73710 = CARTESIAN_POINT ( 'NONE',  ( 21.09706851349341861, 8.775842513484549912, -146.2355662163996612 ) ) ;
#73711 = FACE_OUTER_BOUND ( 'NONE', #108888, .T. ) ;
#73712 = ORIENTED_EDGE ( 'NONE', *, *, #14035, .F. ) ;
#73713 = DIRECTION ( 'NONE',  ( 0.000000000000000000, 0.000000000000000000, -1.000000000000000000 ) ) ;
#73714 = TOROIDAL_SURFACE ( 'NONE', #219414, 0.6000000000000004219, 0.1000000000000000056 ) ;
#73715 = DIRECTION ( 'NONE',  ( 0.000000000000000000, 1.734723475976757554E-14, -1.000000000000000000 ) ) ;
#73716 = CARTESIAN_POINT ( 'NONE',  ( -18.49499033040906681, 78.22449947793296587, -231.3784013806107112 ) ) ;
#73717 = ORIENTED_EDGE ( 'NONE', *, *, #215843, .T. ) ;
#73718 = ORIENTED_EDGE ( 'NONE', *, *, #205689, .T. ) ;
#73719 = FACE_OUTER_BOUND ( 'NONE', #224976, .T. ) ;
#73720 = DIRECTION ( 'NONE',  ( 0.000000000000000000, -0.9915357197604853789, 0.1298341882520022694 ) ) ;
#73721 = DIRECTION ( 'NONE',  ( -0.000000000000000000, -6.982962677686266711E-15, 1.000000000000000000 ) ) ;
#73722 = ORIENTED_EDGE ( 'NONE', *, *, #234061, .T. ) ;
#73723 = AXIS2_PLACEMENT_3D ( 'NONE', #151658, #253280, #214170 ) ;
#73724 = CARTESIAN_POINT ( 'NONE',  ( 13.54556439290364622, 46.53556350520270257, -234.7709563976631273 ) ) ;
#73725 = CARTESIAN_POINT ( 'NONE',  ( 20.94999999999999574, -1.851028230129704522, -179.1539132694224463 ) ) ;
#73726 = VECTOR ( 'NONE', #149455, 1000.000000000000114 ) ;
#73727 = CARTESIAN_POINT ( 'NONE',  ( 21.12642695952774474, 0.09890328320052040045, -127.6243400779648596 ) ) ;
#73728 = DIRECTION ( 'NONE',  ( 0.000000000000000000, -0.2128009952263403282, 0.9770955615653358350 ) ) ;
#73729 = AXIS2_PLACEMENT_3D ( 'NONE', #118399, #14183, #96242 ) ;
#73730 = CARTESIAN_POINT ( 'NONE',  ( -23.25000000000000000, 2.000000000011154189, -180.7246219227620543 ) ) ;
#73731 = PRESENTATION_LAYER_ASSIGNMENT (  '', '', ( #7067 ) ) ;
#73733 = EDGE_LOOP ( 'NONE', ( #212463, #183220, #182239, #163729 ) ) ;
#73732 = CARTESIAN_POINT ( 'NONE',  ( -21.44999999999999929, 7.150000000011155876, -112.7500000000000284 ) ) ;
#73734 = CARTESIAN_POINT ( 'NONE',  ( -23.25000000000000000, 79.24821784679178904, -196.3217825494968736 ) ) ;
#73735 = DIRECTION ( 'NONE',  ( 0.000000000000000000, -6.938893903907222067E-15, 1.000000000000000000 ) ) ;
#73736 = CARTESIAN_POINT ( 'NONE',  ( 22.50000000000000000, 1.115600667400684642E-11, -134.0000000000000000 ) ) ;
#73737 = CARTESIAN_POINT ( 'NONE',  ( -20.64999999999999858, 84.73084112150711178, -79.12118220350858167 ) ) ;
#73738 = CIRCLE ( 'NONE', #61250, 0.09999999999998898659 ) ;
#73739 = EDGE_CURVE ( 'NONE', #81327, #54263, #158979, .T. ) ;
#73740 = CARTESIAN_POINT ( 'NONE',  ( 20.85000000000000142, 43.62273694548321856, -253.2814864317374770 ) ) ;
#73742 = ORIENTED_EDGE ( 'NONE', *, *, #196385, .F. ) ;
#73741 = DIRECTION ( 'NONE',  ( 0.000000000000000000, 0.8814952561688432775, -0.4721928772777344019 ) ) ;
#73743 = CARTESIAN_POINT ( 'NONE',  ( -23.15000000000000213, 4.350000000011156054, -79.25000000000004263 ) ) ;
#73744 = DIRECTION ( 'NONE',  ( 0.000000000000000000, 0.000000000000000000, -1.000000000000000000 ) ) ;
#73745 = CARTESIAN_POINT ( 'NONE',  ( 23.14999999999998437, 31.85509083104287598, -238.8280249686205536 ) ) ;
#73746 = ORIENTED_EDGE ( 'NONE', *, *, #224436, .F. ) ;
#73747 = CARTESIAN_POINT ( 'NONE',  ( -23.15000000000000213, 71.85000000001203091, -114.7731074845243313 ) ) ;
#73748 = DIRECTION ( 'NONE',  ( -0.000000000000000000, -1.000000000000000000, -0.000000000000000000 ) ) ;
#73750 = EDGE_CURVE ( 'NONE', #227495, #200926, #178208, .T. ) ;
#73749 = CARTESIAN_POINT ( 'NONE',  ( -18.59999999999999787, 1.835341550224411922, -11.55515129256298046 ) ) ;
#73751 = ADVANCED_FACE ( 'NONE', ( #46682 ), #107960, .F. ) ;
#73752 = CARTESIAN_POINT ( 'NONE',  ( 18.79999999999999716, 5.488301202077012775, 16.50000000000000000 ) ) ;
#73753 = CARTESIAN_POINT ( 'NONE',  ( -20.85000000000000142, -1.164121893230052995, -74.91484808557160591 ) ) ;
#73754 = TOROIDAL_SURFACE ( 'NONE', #186152, 0.4000000000000015210, 0.1000000000000000056 ) ;
#73755 = CARTESIAN_POINT ( 'NONE',  ( -23.25000000000000000, 1.115600667400684642E-11, -203.0999999999999375 ) ) ;
#73756 = AXIS2_PLACEMENT_3D ( 'NONE', #3618, #62327, #141847 ) ;
#73757 = ORIENTED_EDGE ( 'NONE', *, *, #160036, .F. ) ;
#73758 = ORIENTED_EDGE ( 'NONE', *, *, #134141, .F. ) ;
#73759 = AXIS2_PLACEMENT_3D ( 'NONE', #199727, #238832, #253242 ) ;
#73760 = CARTESIAN_POINT ( 'NONE',  ( 21.05000000000000071, 5.000000000011153745, -55.09473398108690390 ) ) ;
#73761 = LINE ( 'NONE', #34633, #133149 ) ;
#73762 = AXIS2_PLACEMENT_3D ( 'NONE', #120356, #104572, #221949 ) ;
#73763 = EDGE_CURVE ( 'NONE', #246499, #226147, #67544, .T. ) ;
#73764 =( BOUNDED_SURFACE ( )  B_SPLINE_SURFACE ( 3, 2, ( 
 ( #176987, #218629, #79113 ),
 ( #2150, #158706, #238198 ),
 ( #59536, #82948, #225040 ),
 ( #205490, #102512, #84209 ) ),
 .UNSPECIFIED., .F., .F., .F. ) 
 B_SPLINE_SURFACE_WITH_KNOTS ( ( 4, 4 ),
 ( 3, 3 ),
 ( 4.712388980384689674, 6.283185307179586232 ),
 ( 0.000000000000000000, 1.000000000000000000 ),
 .UNSPECIFIED. ) 
 GEOMETRIC_REPRESENTATION_ITEM ( )  RATIONAL_B_SPLINE_SURFACE ( (
 ( 1.000000000000000000, 0.7071067811865444641, 1.000000000000000000),
 ( 1.000000000000000000, 0.7389971855006018941, 1.000000000000000000),
 ( 1.000000000000000000, 0.7651312202474049862, 1.000000000000000000),
 ( 1.000000000000000000, 0.7644017236018784134, 1.000000000000000000) ) ) 
 REPRESENTATION_ITEM ( '' )  SURFACE ( )  );
#73765 = FACE_OUTER_BOUND ( 'NONE', #63590, .T. ) ;
#73766 = CYLINDRICAL_SURFACE ( 'NONE', #205582, 0.1000000000000053763 ) ;
#73767 = CIRCLE ( 'NONE', #231983, 0.5000000000000004441 ) ;
#73768 = VECTOR ( 'NONE', #133289, 1000.000000000000000 ) ;
#73769 = FACE_OUTER_BOUND ( 'NONE', #194177, .T. ) ;
#73770 = CARTESIAN_POINT ( 'NONE',  ( -20.94999999999999929, 76.00000000001170974, -69.52310748452431710 ) ) ;
#73771 = DIRECTION ( 'NONE',  ( 1.000000000000000000, 0.000000000000000000, 0.000000000000000000 ) ) ;
#73772 = DIRECTION ( 'NONE',  ( 1.000000000000000000, 0.000000000000000000, -0.000000000000000000 ) ) ;
#73773 = VECTOR ( 'NONE', #219211, 1000.000000000000000 ) ;
#73774 = CIRCLE ( 'NONE', #36367, 0.09999999999999781286 ) ;
#73775 = ORIENTED_EDGE ( 'NONE', *, *, #23580, .T. ) ;
#73776 = DIRECTION ( 'NONE',  ( 1.000000000000000000, 0.000000000000000000, -0.000000000000000000 ) ) ;
#73777 = VERTEX_POINT ( 'NONE', #49263 ) ;
#73778 = EDGE_CURVE ( 'NONE', #175343, #90665, #209361, .T. ) ;
#73779 = DIRECTION ( 'NONE',  ( 0.000000000000000000, 1.000000000000000000, 6.853228547068871147E-15 ) ) ;
#73781 = EDGE_CURVE ( 'NONE', #125880, #136260, #24092, .T. ) ;
#73780 = B_SPLINE_CURVE_WITH_KNOTS ( 'NONE', 3,
 ( #116429, #78563, #158157, #40767, #120313, #21201 ),
 .UNSPECIFIED., .F., .F.,
 ( 4, 2, 4 ),
 ( 0.000000000000000000, 0.0001568709654583424031, 0.0003137419309166848062 ),
 .UNSPECIFIED. ) ;
#73782 = CARTESIAN_POINT ( 'NONE',  ( 20.73486653747088937, 7.750000000000025757, -12.65000000000000568 ) ) ;
#73784 = ORIENTED_EDGE ( 'NONE', *, *, #2855, .F. ) ;
#73783 = LINE ( 'NONE', #54177, #216060 ) ;
#73785 = DIRECTION ( 'NONE',  ( 1.000000000000000000, 0.000000000000000000, 0.000000000000000000 ) ) ;
#73786 = CARTESIAN_POINT ( 'NONE',  ( 21.05095171578076574, 21.99704254906454537, -231.7411790891100907 ) ) ;
#73787 = CARTESIAN_POINT ( 'NONE',  ( 18.39999999999999858, 85.50000000001166711, -62.92291809330219365 ) ) ;
#73788 = CARTESIAN_POINT ( 'NONE',  ( -20.94999999999999929, -11.48912529306490349, -170.5999999999999659 ) ) ;
#73789 = ORIENTED_EDGE ( 'NONE', *, *, #150359, .F. ) ;
#73790 = DIRECTION ( 'NONE',  ( -1.000000000000000000, -0.000000000000000000, -0.000000000000000000 ) ) ;
#73791 = DIRECTION ( 'NONE',  ( 0.000000000000000000, 0.000000000000000000, 1.000000000000000000 ) ) ;
#73792 = CARTESIAN_POINT ( 'NONE',  ( -18.69999999999999929, -11.65000000000000036, -15.00000000000000000 ) ) ;
#73793 = AXIS2_PLACEMENT_3D ( 'NONE', #189698, #167589, #69767 ) ;
#73795 = ADVANCED_FACE ( 'NONE', ( #169256 ), #71421, .T. ) ;
#73794 = FACE_OUTER_BOUND ( 'NONE', #159355, .T. ) ;
#73796 = DIRECTION ( 'NONE',  ( -4.391705002472931063E-16, -0.9651348961777154178, 0.2617529984165040680 ) ) ;
#73797 = VERTEX_POINT ( 'NONE', #188772 ) ;
#73798 = AXIS2_PLACEMENT_3D ( 'NONE', #41227, #39938, #58165 ) ;
#73799 = CARTESIAN_POINT ( 'NONE',  ( -22.39999999999999858, 76.10085836911093793, -148.2726746080136877 ) ) ;
#73800 = CARTESIAN_POINT ( 'NONE',  ( -16.78493832629887805, 66.05416425680772363, -90.35915846542016538 ) ) ;
#73801 = ORIENTED_EDGE ( 'NONE', *, *, #253395, .F. ) ;
#73802 = VERTEX_POINT ( 'NONE', #7574 ) ;
#73803 = FACE_OUTER_BOUND ( 'NONE', #27070, .T. ) ;
#73804 = CARTESIAN_POINT ( 'NONE',  ( -20.94999999999999929, 48.04585786805223080, -246.4610531646956417 ) ) ;
#73805 = VECTOR ( 'NONE', #8435, 1000.000000000000227 ) ;
#73806 = AXIS2_PLACEMENT_3D ( 'NONE', #424, #203776, #22590 ) ;
#73807 = EDGE_CURVE ( 'NONE', #154034, #39515, #199029, .T. ) ;
#73808 = ORIENTED_EDGE ( 'NONE', *, *, #73019, .F. ) ;
#73810 = AXIS2_PLACEMENT_3D ( 'NONE', #215403, #195868, #176307 ) ;
#73809 = CARTESIAN_POINT ( 'NONE',  ( 18.79999999999999716, 7.900000000000000355, -1.212568896937008089 ) ) ;
#73811 = CARTESIAN_POINT ( 'NONE',  ( 23.24999999999999645, 11.75000000001113953, -109.7500000000000426 ) ) ;
#73812 = AXIS2_PLACEMENT_3D ( 'NONE', #25884, #148387, #105362 ) ;
#73813 = ORIENTED_EDGE ( 'NONE', *, *, #177621, .T. ) ;
#73814 = CIRCLE ( 'NONE', #194624, 0.1000000000000001860 ) ;
#73815 = ADVANCED_FACE ( 'NONE', ( #145785 ), #226602, .F. ) ;
#73816 = ORIENTED_EDGE ( 'NONE', *, *, #163374, .T. ) ;
#73817 = DIRECTION ( 'NONE',  ( -0.000000000000000000, 1.000000000000000000, 0.000000000000000000 ) ) ;
#73818 = LINE ( 'NONE', #50344, #204455 ) ;
#73820 = ORIENTED_EDGE ( 'NONE', *, *, #118543, .F. ) ;
#73819 = CARTESIAN_POINT ( 'NONE',  ( -21.05000000000000071, -11.39257802169451672, -70.07394957983198935 ) ) ;
#73821 = DIRECTION ( 'NONE',  ( -1.000000000000000000, -0.000000000000000000, -0.000000000000000000 ) ) ;
#73823 = LINE ( 'NONE', #131188, #49023 ) ;
#73822 = UNCERTAINTY_MEASURE_WITH_UNIT (LENGTH_MEASURE( 1.000000000000000082E-05 ), #175605, 'distance_accuracy_value', 'NONE');
#73824 = ADVANCED_FACE ( 'NONE', ( #47973 ), #109228, .T. ) ;
#73826 = EDGE_CURVE ( 'NONE', #126775, #209328, #232373, .T. ) ;
#73825 = CARTESIAN_POINT ( 'NONE',  ( -20.91682497891423154, 65.67736539654967487, -130.9625116876572406 ) ) ;
#73827 = AXIS2_PLACEMENT_3D ( 'NONE', #80641, #222727, #239748 ) ;
#73828 = CARTESIAN_POINT ( 'NONE',  ( 18.59999999999999787, 86.87366311306882949, -199.3414869250131858 ) ) ;
#73829 = DIRECTION ( 'NONE',  ( 1.000000000000000000, 0.000000000000000000, 0.000000000000000000 ) ) ;
#73830 = CIRCLE ( 'NONE', #23940, 11.64999999999999325 ) ;
#73831 = DIRECTION ( 'NONE',  ( 1.000000000000000000, 0.000000000000000000, 0.000000000000000000 ) ) ;
#73832 = CARTESIAN_POINT ( 'NONE',  ( 23.14999999999999858, 71.18691588786271041, -148.4646252410481964 ) ) ;
#73834 = VERTEX_POINT ( 'NONE', #149678 ) ;
#73833 = DIRECTION ( 'NONE',  ( 2.895190717381441586E-16, -0.1335171055202867274, 0.9910465087640865089 ) ) ;
#73835 = ORIENTED_EDGE ( 'NONE', *, *, #16202, .F. ) ;
#73837 = CARTESIAN_POINT ( 'NONE',  ( -16.83558968593868244, 51.60763312609429221, -231.9514998304251492 ) ) ;
#73836 = CARTESIAN_POINT ( 'NONE',  ( 18.69999999999999929, -14.27107483842559432, -0.5438473119858313609 ) ) ;
#73839 = ORIENTED_EDGE ( 'NONE', *, *, #221568, .T. ) ;
#73838 = CARTESIAN_POINT ( 'NONE',  ( 21.04999999999999716, 8.871279686006802834, -75.55862899514100661 ) ) ;
#73840 = ORIENTED_EDGE ( 'NONE', *, *, #18487, .F. ) ;
#73841 = DIRECTION ( 'NONE',  ( 1.000000000000000000, 0.000000000000000000, -0.000000000000000000 ) ) ;
#73842 = DIRECTION ( 'NONE',  ( -1.000000000000000000, 0.000000000000000000, 0.000000000000000000 ) ) ;
#73843 = AXIS2_PLACEMENT_3D ( 'NONE', #149157, #68322, #46172 ) ;
#73844 = EDGE_CURVE ( 'NONE', #37194, #241978, #186218, .T. ) ;
#73845 = EDGE_CURVE ( 'NONE', #26557, #138331, #88366, .T. ) ;
#73846 = CARTESIAN_POINT ( 'NONE',  ( 18.79999999999999716, 1.212568896937007645, -8.000000000000000000 ) ) ;
#73847 = DIRECTION ( 'NONE',  ( 0.000000000000000000, 1.000000000000000000, 0.000000000000000000 ) ) ;
#73848 = DIRECTION ( 'NONE',  ( 1.000000000000000000, 0.000000000000000000, 0.000000000000000000 ) ) ;
#73849 = ADVANCED_FACE ( 'NONE', ( #209626 ), #166681, .T. ) ;
#73850 = CARTESIAN_POINT ( 'NONE',  ( 20.94999999999999929, 54.26566224370346703, -236.3486064386993633 ) ) ;
#73851 = CARTESIAN_POINT ( 'NONE',  ( -16.97683809663752186, 66.05000000001203375, -116.4254715027206828 ) ) ;
#73853 = VERTEX_POINT ( 'NONE', #68850 ) ;
#73852 = EDGE_CURVE ( 'NONE', #200814, #99245, #226093, .T. ) ;
#73854 = ORIENTED_EDGE ( 'NONE', *, *, #229800, .T. ) ;
#73855 = CARTESIAN_POINT ( 'NONE',  ( 21.05000000000000071, 30.84076144264166786, -252.2514173861790709 ) ) ;
#73856 = AXIS2_PLACEMENT_3D ( 'NONE', #36537, #116057, #71797 ) ;
#73857 = VECTOR ( 'NONE', #183695, 1000.000000000000000 ) ;
#73858 = VERTEX_POINT ( 'NONE', #208366 ) ;
#73860 = EDGE_CURVE ( 'NONE', #189704, #197589, #119956, .T. ) ;
#73859 = AXIS2_PLACEMENT_3D ( 'NONE', #18665, #99459, #193468 ) ;
#73862 = DIRECTION ( 'NONE',  ( 0.000000000000000000, 0.000000000000000000, -1.000000000000000000 ) ) ;
#73861 = TOROIDAL_SURFACE ( 'NONE', #244683, 0.2000000000000000111, 0.1000000000000000056 ) ;
#73864 = EDGE_CURVE ( 'NONE', #34141, #26557, #161240, .T. ) ;
#73863 = ORIENTED_EDGE ( 'NONE', *, *, #47471, .F. ) ;
#73865 = DIRECTION ( 'NONE',  ( -3.469446951953635015E-14, 1.000000000000000000, 0.000000000000000000 ) ) ;
#73866 =( BOUNDED_SURFACE ( )  B_SPLINE_SURFACE ( 3, 2, ( 
 ( #165854, #8056, #227079 ),
 ( #191851, #189259, #250495 ),
 ( #68016, #146258, #187975 ),
 ( #9324, #167155, #88838 ),
 ( #249235, #71886, #32782 ),
 ( #48448, #130550, #168460 ) ),
 .UNSPECIFIED., .F., .F., .T. ) 
 B_SPLINE_SURFACE_WITH_KNOTS ( ( 4, 2, 4 ),
 ( 3, 3 ),
 ( 3.141592653589793116, 3.926990816987241395, 4.712388980384689674 ),
 ( 0.000000000000000000, 1.000000000000000000 ),
 .UNSPECIFIED. ) 
 GEOMETRIC_REPRESENTATION_ITEM ( )  RATIONAL_B_SPLINE_SURFACE ( (
 ( 1.000000000000000000, 0.9238795325112820755, 1.000000000000000000),
 ( 1.000000000000000000, 0.9240297172239489987, 1.000000000000000000),
 ( 1.000000000000000000, 0.9038128468044698272, 1.000000000000000000),
 ( 1.000000000000000000, 0.8282379607644166919, 1.000000000000000000),
 ( 1.000000000000000000, 0.7727932973495217350, 1.000000000000000000),
 ( 1.000000000000000000, 0.7071067811865475727, 1.000000000000000000) ) ) 
 REPRESENTATION_ITEM ( '' )  SURFACE ( )  );
#73867 = DIRECTION ( 'NONE',  ( 1.000000000000000000, 0.000000000000000000, -0.000000000000000000 ) ) ;
#73868 = ADVANCED_FACE ( 'NONE', ( #192640 ), #160901, .T. ) ;
#73869 = DIRECTION ( 'NONE',  ( 3.469446951953635015E-14, -0.2128009952263604232, 0.9770955615653316162 ) ) ;
#73870 = VERTEX_POINT ( 'NONE', #198718 ) ;
#73871 = DIRECTION ( 'NONE',  ( 3.265361837132813093E-16, 0.4088369013363281068, -0.9126074666063770380 ) ) ;
#73872 = ORIENTED_EDGE ( 'NONE', *, *, #153955, .T. ) ;
#73873 = EDGE_CURVE ( 'NONE', #217763, #236784, #103157, .T. ) ;
#73874 = FACE_OUTER_BOUND ( 'NONE', #10953, .T. ) ;
#73875 = ADVANCED_FACE ( 'NONE', ( #12738 ), #51809, .T. ) ;
#73876 = DIRECTION ( 'NONE',  ( 0.000000000000000000, 0.2868887416115947775, -0.9579639084728169829 ) ) ;
#73877 = AXIS2_PLACEMENT_3D ( 'NONE', #140860, #136996, #220401 ) ;
#73879 = EDGE_LOOP ( 'NONE', ( #103990, #181048, #198055, #151528 ) ) ;
#73878 = EDGE_CURVE ( 'NONE', #236713, #199664, #161642, .T. ) ;
#73880 = CARTESIAN_POINT ( 'NONE',  ( -21.05000000000000071, 6.400000000011158541, -110.4304246300616086 ) ) ;
#73881 = ORIENTED_EDGE ( 'NONE', *, *, #29389, .T. ) ;
#73883 = ORIENTED_EDGE ( 'NONE', *, *, #95749, .T. ) ;
#73882 = CARTESIAN_POINT ( 'NONE',  ( 22.49231231312462853, 55.97148680618423100, -232.8646322987703456 ) ) ;
#73884 = CARTESIAN_POINT ( 'NONE',  ( 18.49999999999999289, 65.50857864377418593, -44.67310748452439384 ) ) ;
#73885 = EDGE_LOOP ( 'NONE', ( #218824, #149737, #92237, #63376 ) ) ;
#73886 = ORIENTED_EDGE ( 'NONE', *, *, #9559, .T. ) ;
#73887 = CARTESIAN_POINT ( 'NONE',  ( -20.85000000000000142, 11.65000000001115232, -160.7161343370219129 ) ) ;
#73888 = ORIENTED_EDGE ( 'NONE', *, *, #139886, .T. ) ;
#73889 = EDGE_CURVE ( 'NONE', #102120, #156136, #36572, .T. ) ;
#73890 = DIRECTION ( 'NONE',  ( 1.000000000000000000, -0.000000000000000000, -0.000000000000000000 ) ) ;
#73891 = CARTESIAN_POINT ( 'NONE',  ( 21.04999999999999716, 69.70076908992476206, -69.62154498452436258 ) ) ;
#73892 = CARTESIAN_POINT ( 'NONE',  ( 20.85000000000000142, 46.07463622722161745, -256.5801648492221148 ) ) ;
#73893 = DIRECTION ( 'NONE',  ( 0.000000000000000000, -7.086529944415894657E-15, 1.000000000000000000 ) ) ;
#73894 = FACE_OUTER_BOUND ( 'NONE', #59721, .T. ) ;
#73895 = ORIENTED_EDGE ( 'NONE', *, *, #229633, .T. ) ;
#73896 = DIRECTION ( 'NONE',  ( 0.000000000000000000, 0.9126074666063772600, 0.4088369013363274962 ) ) ;
#73897 = CARTESIAN_POINT ( 'NONE',  ( -21.05000000000000071, 64.40000000001194280, -109.9513107147998880 ) ) ;
#73898 = CARTESIAN_POINT ( 'NONE',  ( -20.94999999999999929, -1.164121893230052995, -74.71484808557160306 ) ) ;
#73899 = AXIS2_PLACEMENT_3D ( 'NONE', #163430, #146402, #246801 ) ;
#73900 = ORIENTED_EDGE ( 'NONE', *, *, #200496, .F. ) ;
#73901 = LINE ( 'NONE', #232965, #105377 ) ;
#73902 = ORIENTED_EDGE ( 'NONE', *, *, #210611, .F. ) ;
#73903 = CARTESIAN_POINT ( 'NONE',  ( -21.22070241538126112, 33.92349738987645935, -243.6870831740097003 ) ) ;
#73904 = ORIENTED_EDGE ( 'NONE', *, *, #168008, .T. ) ;
#73905 = DIRECTION ( 'NONE',  ( -0.000000000000000000, 0.1298341882520009927, 0.9915357197604854900 ) ) ;
#73906 = LINE ( 'NONE', #72611, #172787 ) ;
#73908 = ORIENTED_EDGE ( 'NONE', *, *, #151545, .T. ) ;
#73907 = CYLINDRICAL_SURFACE ( 'NONE', #48954, 0.5000000000000004441 ) ;
#73909 = DIRECTION ( 'NONE',  ( -0.000000000000000000, -6.982962677686266711E-15, 1.000000000000000000 ) ) ;
#73910 = ORIENTED_EDGE ( 'NONE', *, *, #192730, .T. ) ;
#73911 = AXIS2_PLACEMENT_3D ( 'NONE', #167713, #227646, #49015 ) ;
#73912 = CARTESIAN_POINT ( 'NONE',  ( -20.85000000106542117, 36.17380055357438096, -235.9616714914856459 ) ) ;
#73913 = CARTESIAN_POINT ( 'NONE',  ( -16.84981964351502626, 9.917318234110025443, -113.3696016140195439 ) ) ;
#73914 = ORIENTED_EDGE ( 'NONE', *, *, #146087, .T. ) ;
#73915 = VECTOR ( 'NONE', #127982, 1000.000000000000000 ) ;
#73916 = EDGE_CURVE ( 'NONE', #66589, #5531, #20097, .T. ) ;
#73917 = DIRECTION ( 'NONE',  ( 1.000000000000000000, 0.000000000000000000, 0.000000000000000000 ) ) ;
#73918 = CARTESIAN_POINT ( 'NONE',  ( -20.87155475150660777, 11.75000000001115197, -194.0955865291576004 ) ) ;
#73919 = ORIENTED_EDGE ( 'NONE', *, *, #76213, .T. ) ;
#73920 = LINE ( 'NONE', #212129, #148996 ) ;
#73921 = AXIS2_PLACEMENT_3D ( 'NONE', #193766, #252437, #235440 ) ;
#73922 = AXIS2_PLACEMENT_3D ( 'NONE', #203186, #243599, #226585 ) ;
#73923 = EDGE_CURVE ( 'NONE', #114232, #220305, #174317, .T. ) ;
#73924 = ORIENTED_EDGE ( 'NONE', *, *, #59631, .T. ) ;
#73925 = PRODUCT_DEFINITION_FORMATION_WITH_SPECIFIED_SOURCE ( 'ANY', '', #86733, .NOT_KNOWN. ) ;
#73927 = FACE_OUTER_BOUND ( 'NONE', #232671, .T. ) ;
#73926 = AXIS2_PLACEMENT_3D ( 'NONE', #173391, #233340, #229471 ) ;
#73928 = VECTOR ( 'NONE', #166396, 1000.000000000000000 ) ;
#73929 = ORIENTED_EDGE ( 'NONE', *, *, #99429, .T. ) ;
#73930 = DIRECTION ( 'NONE',  ( 0.000000000000000000, 0.9126074666063660468, 0.4088369013363524762 ) ) ;
#73931 = CARTESIAN_POINT ( 'NONE',  ( -22.48479450179659977, 0.04699158119804078271, -155.8500015537483421 ) ) ;
#73932 = PLANE ( 'NONE',  #85691 ) ;
#73934 = CARTESIAN_POINT ( 'NONE',  ( -13.11924609551134857, 66.56831044948742715, -51.24381745228831875 ) ) ;
#73933 = DIRECTION ( 'NONE',  ( -0.000000000000000000, -6.982962677686266711E-15, 1.000000000000000000 ) ) ;
#73936 = EDGE_CURVE ( 'NONE', #250542, #193798, #140967, .T. ) ;
#73935 = CARTESIAN_POINT ( 'NONE',  ( 21.14999999999999858, 11.75000000000000711, -12.15000000000000036 ) ) ;
#73937 = DIRECTION ( 'NONE',  ( 0.000000000000000000, -0.8660254037844377084, -0.5000000000000016653 ) ) ;
#73938 = AXIS2_PLACEMENT_3D ( 'NONE', #257776, #218686, #41381 ) ;
#73939 = FACE_OUTER_BOUND ( 'NONE', #233590, .T. ) ;
#73940 = LINE ( 'NONE', #33546, #75824 ) ;
#73941 = AXIS2_PLACEMENT_3D ( 'NONE', #171430, #226184, #69737 ) ;
#73942 = EDGE_LOOP ( 'NONE', ( #61083, #17569, #64652, #19432 ) ) ;
#73943 = EDGE_LOOP ( 'NONE', ( #107509, #95286, #2274, #201938 ) ) ;
#73945 = DIRECTION ( 'NONE',  ( 0.000000000000000000, 0.8814952561688438326, -0.4721928772777331806 ) ) ;
#73944 = VECTOR ( 'NONE', #234922, 1000.000000000000000 ) ;
#73946 = VECTOR ( 'NONE', #15188, 1000.000000000000000 ) ;
#73948 = VERTEX_POINT ( 'NONE', #159607 ) ;
#73947 = DIRECTION ( 'NONE',  ( 1.000000000000000000, 0.000000000000000000, 0.000000000000000000 ) ) ;
#73949 = AXIS2_PLACEMENT_3D ( 'NONE', #63891, #43051, #143422 ) ;
#73950 = EDGE_LOOP ( 'NONE', ( #29460, #249069, #108520, #76096 ) ) ;
#73951 = DIRECTION ( 'NONE',  ( 1.000000000000000000, 0.000000000000000000, 0.000000000000000000 ) ) ;
#73952 = VERTEX_POINT ( 'NONE', #173118 ) ;
#73953 = CARTESIAN_POINT ( 'NONE',  ( -18.59999999999999787, 77.83585931145526615, -58.01866831572577610 ) ) ;
#73954 = ORIENTED_EDGE ( 'NONE', *, *, #9995, .F. ) ;
#73955 = PRESENTATION_STYLE_ASSIGNMENT (( #17776 ) ) ;
#73956 = CYLINDRICAL_SURFACE ( 'NONE', #98876, 11.74999999999999645 ) ;
#73959 = ORIENTED_EDGE ( 'NONE', *, *, #102477, .T. ) ;
#73958 = VERTEX_POINT ( 'NONE', #252589 ) ;
#73957 = AXIS2_PLACEMENT_3D ( 'NONE', #63684, #4973, #68507 ) ;
#73960 = ORIENTED_EDGE ( 'NONE', *, *, #198243, .T. ) ;
#73961 = AXIS2_PLACEMENT_3D ( 'NONE', #230913, #108382, #73135 ) ;
#73962 = AXIS2_PLACEMENT_3D ( 'NONE', #205492, #223767, #85518 ) ;
#73963 = EDGE_LOOP ( 'NONE', ( #256699, #247467, #166690, #65777 ) ) ;
#73964 = EDGE_LOOP ( 'NONE', ( #181787, #230052, #222693, #159838, #86336 ) ) ;
#73965 = CARTESIAN_POINT ( 'NONE',  ( -21.04999999999994387, 66.15000000001114699, -51.02310748452479316 ) ) ;
#73966 = CARTESIAN_POINT ( 'NONE',  ( -23.15000000000000213, 11.65000000001115588, -188.8499999999999659 ) ) ;
#73968 = EDGE_LOOP ( 'NONE', ( #45665, #220118, #221230, #2582 ) ) ;
#73967 = CARTESIAN_POINT ( 'NONE',  ( -17.22361732159832215, 65.65484434140988412, -158.6523229586572938 ) ) ;
#73969 = CARTESIAN_POINT ( 'NONE',  ( -20.07928932188135107, 66.77928932189291800, -57.17310748452438673 ) ) ;
#73970 = CARTESIAN_POINT ( 'NONE',  ( 21.53752568617682428, 6.786807874514932060, -167.4010255387155155 ) ) ;
#73972 = EDGE_LOOP ( 'NONE', ( #196215, #53172, #114834, #150559 ) ) ;
#73971 = CARTESIAN_POINT ( 'NONE',  ( 20.95017935633852346, 10.47548927963648246, -141.5774397973904968 ) ) ;
#73973 = DIRECTION ( 'NONE',  ( 1.000000000000000000, 0.000000000000000000, 0.000000000000000000 ) ) ;
#73974 = ORIENTED_EDGE ( 'NONE', *, *, #91523, .T. ) ;
#73975 = DIRECTION ( 'NONE',  ( 0.000000000000000000, 1.000000000000000000, 0.000000000000000000 ) ) ;
#73976 = EDGE_CURVE ( 'NONE', #257053, #3812, #61845, .T. ) ;
#73978 = ORIENTED_EDGE ( 'NONE', *, *, #57231, .T. ) ;
#73977 = DIRECTION ( 'NONE',  ( -0.000000000000000000, -0.3427706569149635007, 0.9394191166662961834 ) ) ;
#73979 = VECTOR ( 'NONE', #67556, 1000.000000000000000 ) ;
#73980 = CARTESIAN_POINT ( 'NONE',  ( -21.05000000000000071, 18.27574494880468592, -237.6039235467692947 ) ) ;
#73981 = CARTESIAN_POINT ( 'NONE',  ( -20.94999999999999929, 14.05000000001115623, -161.9863049292391111 ) ) ;
#73982 = ADVANCED_FACE ( 'NONE', ( #92234 ), #120503, .F. ) ;
#73983 = AXIS2_PLACEMENT_3D ( 'NONE', #61440, #220525, #199693 ) ;
#73984 = EDGE_LOOP ( 'NONE', ( #18187, #228850, #171916, #97868 ) ) ;
#73986 = DIRECTION ( 'NONE',  ( -0.000000000000000000, 0.4791956752371485107, 0.8777080977375185666 ) ) ;
#73985 = DIRECTION ( 'NONE',  ( -1.000000000000000000, -0.000000000000000000, -0.000000000000000000 ) ) ;
#73987 = AXIS2_PLACEMENT_3D ( 'NONE', #149114, #108684, #12177 ) ;
#73988 = CARTESIAN_POINT ( 'NONE',  ( 21.05000000000000071, 77.16270174994961906, -61.42310748452431568 ) ) ;
#73989 = B_SPLINE_CURVE_WITH_KNOTS ( 'NONE', 3,
 ( #69297, #148831, #147533, #247908, #110976, #87539, #27626, #49716, #129257, #130527, #48423, #207524, #108412, #28921, #189235, #30176, #210089, #228363, #131815 ),
 .UNSPECIFIED., .F., .F.,
 ( 4, 3, 3, 3, 3, 3, 4 ),
 ( 0.000000000000000000, 2.646747978908489188E-05, 5.271166642128679745E-05, 9.008788829884017187E-05, 0.0001426648776561119315, 0.0001897378458659873231, 0.0001917382627806427315 ),
 .UNSPECIFIED. ) ;
#73990 = FACE_OUTER_BOUND ( 'NONE', #130822, .T. ) ;
#73991 = ORIENTED_EDGE ( 'NONE', *, *, #52719, .F. ) ;
#73992 = ORIENTED_EDGE ( 'NONE', *, *, #222061, .F. ) ;
#73993 = CIRCLE ( 'NONE', #61496, 12.87499999999999822 ) ;
#73994 = ADVANCED_FACE ( 'NONE', ( #212213 ), #251305, .T. ) ;
#73995 = CARTESIAN_POINT ( 'NONE',  ( -21.04999999999999716, 0.01485563490459204140, -127.6556409579560949 ) ) ;
#73996 = DIRECTION ( 'NONE',  ( 0.000000000000000000, 0.000000000000000000, -1.000000000000000000 ) ) ;
#73997 = EDGE_LOOP ( 'NONE', ( #143488, #18095, #191936 ) ) ;
#73998 = DIRECTION ( 'NONE',  ( 0.000000000000000000, 0.9126074666063775931, 0.4088369013363268301 ) ) ;
#73999 = ORIENTED_EDGE ( 'NONE', *, *, #178725, .T. ) ;
#74000 = DIRECTION ( 'NONE',  ( -0.000000000000000000, 1.000000000000000000, 6.982962677686266711E-15 ) ) ;
#74001 = DIRECTION ( 'NONE',  ( 0.000000000000000000, -0.9908441862701596881, -0.1350103645451904977 ) ) ;
#74002 = EDGE_CURVE ( 'NONE', #118767, #99245, #128477, .T. ) ;
#74003 = AXIS2_PLACEMENT_3D ( 'NONE', #255341, #214981, #117180 ) ;
#74004 = AXIS2_PLACEMENT_3D ( 'NONE', #114726, #194288, #174745 ) ;
#74005 = VECTOR ( 'NONE', #18822, 1000.000000000000000 ) ;
#74006 = ORIENTED_EDGE ( 'NONE', *, *, #67020, .T. ) ;
#74007 = EDGE_CURVE ( 'NONE', #104053, #82065, #4490, .T. ) ;
#74008 = CIRCLE ( 'NONE', #86971, 4.000000000000003553 ) ;
#74009 = CARTESIAN_POINT ( 'NONE',  ( -16.85312841634287651, 66.08639382269238638, -190.6259343512319049 ) ) ;
#74010 = SURFACE_SIDE_STYLE ('',( #257675 ) ) ;
#74011 = VECTOR ( 'NONE', #250948, 1000.000000000000000 ) ;
#74012 = VERTEX_POINT ( 'NONE', #100856 ) ;
#74013 = ORIENTED_EDGE ( 'NONE', *, *, #146156, .T. ) ;
#74014 = ORIENTED_EDGE ( 'NONE', *, *, #243846, .T. ) ;
#74015 = DIRECTION ( 'NONE',  ( 0.000000000000000000, -0.000000000000000000, 1.000000000000000000 ) ) ;
#74016 = CARTESIAN_POINT ( 'NONE',  ( 15.70340296795548163, 66.64411154550899141, -53.23446458774640178 ) ) ;
#74017 = CYLINDRICAL_SURFACE ( 'NONE', #221623, 0.1000000000000013933 ) ;
#74018 = LINE ( 'NONE', #173132, #23754 ) ;
#74019 = CARTESIAN_POINT ( 'NONE',  ( 12.68104795156995124, 66.60346600605809897, -118.6171677053510791 ) ) ;
#74020 = EDGE_CURVE ( 'NONE', #168498, #131079, #130280, .T. ) ;
#74022 = CARTESIAN_POINT ( 'NONE',  ( 18.49999999999999289, -0.1830918614494220220, -222.4987906021368360 ) ) ;
#74021 = CARTESIAN_POINT ( 'NONE',  ( -23.25000000000000000, -9.599999999988845900, -57.10603087734755690 ) ) ;
#74024 = ORIENTED_EDGE ( 'NONE', *, *, #95046, .F. ) ;
#74023 = LINE ( 'NONE', #137788, #64864 ) ;
#74025 = LINE ( 'NONE', #114397, #87386 ) ;
#74026 = EDGE_LOOP ( 'NONE', ( #215767, #12029, #16615, #44783 ) ) ;
#74027 = CARTESIAN_POINT ( 'NONE',  ( 20.85000000000000142, 7.070967871798842452, -37.24656422186831151 ) ) ;
#74028 = VERTEX_POINT ( 'NONE', #3069 ) ;
#74029 = ORIENTED_EDGE ( 'NONE', *, *, #98709, .F. ) ;
#74030 = CIRCLE ( 'NONE', #28229, 0.1000000000000054040 ) ;
#74031 = DIRECTION ( 'NONE',  ( 1.000000000000000000, 0.000000000000000000, 0.000000000000000000 ) ) ;
#74032 = CYLINDRICAL_SURFACE ( 'NONE', #204363, 0.09999999999999939493 ) ;
#74033 = CYLINDRICAL_SURFACE ( 'NONE', #171074, 0.1000000000000026007 ) ;
#74034 = CARTESIAN_POINT ( 'NONE',  ( 20.84999999999998721, 18.41524492703432614, -237.0006385043383546 ) ) ;
#74035 = ORIENTED_EDGE ( 'NONE', *, *, #222822, .F. ) ;
#74036 = VERTEX_POINT ( 'NONE', #64357 ) ;
#74037 = PLANE ( 'NONE',  #257252 ) ;
#74038 = ORIENTED_EDGE ( 'NONE', *, *, #165133, .T. ) ;
#74039 = CARTESIAN_POINT ( 'NONE',  ( 20.94999999999999929, 76.00000000001212186, -134.6231074845243256 ) ) ;
#74040 = FACE_OUTER_BOUND ( 'NONE', #79890, .T. ) ;
#74041 = ORIENTED_EDGE ( 'NONE', *, *, #89850, .F. ) ;
#74042 = DIRECTION ( 'NONE',  ( 1.000000000000000000, 0.000000000000000000, 0.000000000000000000 ) ) ;
#74043 = CARTESIAN_POINT ( 'NONE',  ( -20.94999999999999929, 11.63687328911525753, -60.17824078667513987 ) ) ;
#74044 = CARTESIAN_POINT ( 'NONE',  ( 21.05000000000000071, 87.65000000001268177, -203.5231074845243029 ) ) ;
#74045 = CARTESIAN_POINT ( 'NONE',  ( 21.13461538461538680, 65.38541703798675542, -157.6731074845244223 ) ) ;
#74046 = ORIENTED_EDGE ( 'NONE', *, *, #177386, .F. ) ;
#74047 = DIRECTION ( 'NONE',  ( 0.000000000000000000, 0.2716869542551192951, -0.9623856809447951521 ) ) ;
#74048 = CARTESIAN_POINT ( 'NONE',  ( 20.94999999999999929, 1.115600667400684642E-11, -167.5000000000000284 ) ) ;
#74049 = AXIS2_PLACEMENT_3D ( 'NONE', #184677, #243371, #244653 ) ;
#74051 = VECTOR ( 'NONE', #6002, 1000.000000000000000 ) ;
#74050 = DIRECTION ( 'NONE',  ( -1.000000000000000000, 0.000000000000000000, 0.000000000000000000 ) ) ;
#74052 = CIRCLE ( 'NONE', #40734, 7.899999999999990585 ) ;
#74053 = ADVANCED_FACE ( 'NONE', ( #123047 ), #44790, .F. ) ;
#74054 = VERTEX_POINT ( 'NONE', #124331 ) ;
#74055 = CARTESIAN_POINT ( 'NONE',  ( -18.50000000000000000, 76.00000000001213607, -136.5231074845243313 ) ) ;
#74056 = ORIENTED_EDGE ( 'NONE', *, *, #46303, .F. ) ;
#74057 = DIRECTION ( 'NONE',  ( -0.000000000000000000, -0.4721928772777346794, -0.8814952561688431665 ) ) ;
#74058 = EDGE_CURVE ( 'NONE', #37588, #101180, #2956, .T. ) ;
#74059 = DIRECTION ( 'NONE',  ( 2.952720810173288619E-16, 0.4088369013363286064, -0.9126074666063768159 ) ) ;
#74060 = CARTESIAN_POINT ( 'NONE',  ( -20.94999999999999929, -4.735542975717121905, -233.2463119243910796 ) ) ;
#74061 = DIRECTION ( 'NONE',  ( 0.000000000000000000, 0.6728971962617102953, 0.7397360091702507301 ) ) ;
#74062 = DIRECTION ( 'NONE',  ( 1.000000000000000000, 0.000000000000000000, 0.000000000000000000 ) ) ;
#74063 = CARTESIAN_POINT ( 'NONE',  ( 21.05000000000000071, 77.16270174995034381, -162.1231074845243540 ) ) ;
#74064 = VERTEX_POINT ( 'NONE', #202577 ) ;
#74065 = FACE_OUTER_BOUND ( 'NONE', #9161, .T. ) ;
#74066 = CARTESIAN_POINT ( 'NONE',  ( 22.39999999999999503, 64.25000000001213607, -136.6231074845243825 ) ) ;
#74067 = EDGE_CURVE ( 'NONE', #140417, #991, #25243, .T. ) ;
#74068 = TOROIDAL_SURFACE ( 'NONE', #174027, 0.6000000000000017542, 0.1000000000000000056 ) ;
#74069 = EDGE_CURVE ( 'NONE', #89706, #206520, #63051, .T. ) ;
#74070 = LINE ( 'NONE', #96143, #193403 ) ;
#74071 = DIRECTION ( 'NONE',  ( 0.000000000000000000, -1.000000000000000000, -6.982962677686266711E-15 ) ) ;
#74072 = DIRECTION ( 'NONE',  ( -1.000000000000000000, 0.000000000000000000, -0.000000000000000000 ) ) ;
#74073 = CIRCLE ( 'NONE', #165828, 0.1000000000000024342 ) ;
#74074 = EDGE_LOOP ( 'NONE', ( #66529, #228058, #21417, #113350 ) ) ;
#74075 = ORIENTED_EDGE ( 'NONE', *, *, #151681, .F. ) ;
#74076 = CARTESIAN_POINT ( 'NONE',  ( 20.85000000000000142, -1.736705739456431807, -78.51742258762372728 ) ) ;
#74077 = DIRECTION ( 'NONE',  ( -1.000000000000000000, 0.000000000000000000, 0.000000000000000000 ) ) ;
#74078 = CARTESIAN_POINT ( 'NONE',  ( -20.64999999999999858, 85.40000000001221281, -146.4170766071767389 ) ) ;
#74079 = DIRECTION ( 'NONE',  ( 0.000000000000000000, 0.8814952561688428334, -0.4721928772777350125 ) ) ;
#74080 = DIRECTION ( 'NONE',  ( 0.000000000000000000, 6.505213034913742890E-15, -1.000000000000000000 ) ) ;
#74081 = ADVANCED_FACE ( 'NONE', ( #186887 ), #184288, .F. ) ;
#74082 = ORIENTED_EDGE ( 'NONE', *, *, #48142, .T. ) ;
#74083 = CARTESIAN_POINT ( 'NONE',  ( -20.94999999999999929, 87.29603075034775372, -173.0710066441881452 ) ) ;
#74084 = ADVANCED_FACE ( 'NONE', ( #203853 ), #181734, .T. ) ;
#74085 = DIRECTION ( 'NONE',  ( -1.000000000000000000, -0.000000000000000000, -0.000000000000000000 ) ) ;
#74086 = ORIENTED_EDGE ( 'NONE', *, *, #108693, .T. ) ;
#74087 = CARTESIAN_POINT ( 'NONE',  ( -23.49999999999994316, 76.00000000001119815, -36.02310748452479316 ) ) ;
#74088 = CARTESIAN_POINT ( 'NONE',  ( 20.73486653747088582, 7.250000000011182166, -87.85000000000003695 ) ) ;
#74089 = TOROIDAL_SURFACE ( 'NONE', #211428, 0.2000000000000000111, 0.1000000000000000056 ) ;
#74090 = CIRCLE ( 'NONE', #194873, 0.1000000000000028644 ) ;
#74091 = VERTEX_POINT ( 'NONE', #220845 ) ;
#74092 = CARTESIAN_POINT ( 'NONE',  ( 23.14999999999998792, 64.35000000001166143, -69.52310748452440237 ) ) ;
#74093 = EDGE_CURVE ( 'NONE', #188385, #154893, #53478, .T. ) ;
#74094 = ORIENTED_EDGE ( 'NONE', *, *, #232926, .F. ) ;
#74095 = EDGE_CURVE ( 'NONE', #118431, #20419, #117964, .T. ) ;
#74096 = CARTESIAN_POINT ( 'NONE',  ( -16.97048361161167662, 9.950000000011137047, -154.3588843444304075 ) ) ;
#74097 = EDGE_CURVE ( 'NONE', #57112, #170896, #27827, .T. ) ;
#74098 = CARTESIAN_POINT ( 'NONE',  ( -18.59999999999999787, 11.65000000001115232, -174.5148057706539930 ) ) ;
#74099 = CARTESIAN_POINT ( 'NONE',  ( -18.59999999999999787, 11.65000000001115232, -112.7500000000000284 ) ) ;
#74100 = CARTESIAN_POINT ( 'NONE',  ( 21.17356465864818205, 75.90108875899855434, -176.4459106107660773 ) ) ;
#74101 = CARTESIAN_POINT ( 'NONE',  ( -20.54999999999999716, 62.08591502004791352, -248.5699171172615820 ) ) ;
#74102 = DIRECTION ( 'NONE',  ( 0.000000000000000000, 0.000000000000000000, -1.000000000000000000 ) ) ;
#74103 = DIRECTION ( 'NONE',  ( 0.000000000000000000, 6.982962677686266711E-15, -1.000000000000000000 ) ) ;
#74104 = CARTESIAN_POINT ( 'NONE',  ( 18.59999999999999076, 45.93315328338058379, -256.6017782078560003 ) ) ;
#74107 = CARTESIAN_POINT ( 'NONE',  ( -23.25000000000000000, -1.851617760457748618, -78.60318971960367662 ) ) ;
#74106 = CIRCLE ( 'NONE', #219799, 0.3999999999999975797 ) ;
#74105 = CYLINDRICAL_SURFACE ( 'NONE', #141264, 0.1000000000000028644 ) ;
#74108 = DIRECTION ( 'NONE',  ( 1.000000000000000000, -0.000000000000000000, -0.000000000000000000 ) ) ;
#74109 = FACE_OUTER_BOUND ( 'NONE', #28767, .T. ) ;
#74110 = VERTEX_POINT ( 'NONE', #242977 ) ;
#74111 = AXIS2_PLACEMENT_3D ( 'NONE', #161194, #201585, #219868 ) ;
#74112 = CARTESIAN_POINT ( 'NONE',  ( -20.95000000000000639, 11.75000000001115019, -93.71613433702195550 ) ) ;
#74113 = TOROIDAL_SURFACE ( 'NONE', #190619, 0.2000000000000000111, 0.1000000000000000056 ) ;
#74114 = DIRECTION ( 'NONE',  ( 0.000000000000000000, 0.000000000000000000, -1.000000000000000000 ) ) ;
#74115 = CYLINDRICAL_SURFACE ( 'NONE', #132645, 0.1000000000000028644 ) ;
#74116 = AXIS2_PLACEMENT_3D ( 'NONE', #8210, #86412, #147711 ) ;
#74117 = VERTEX_POINT ( 'NONE', #66915 ) ;
#74118 = CARTESIAN_POINT ( 'NONE',  ( -21.64999999999999858, 10.05000000001113847, -188.3499999999999659 ) ) ;
#74119 = DIRECTION ( 'NONE',  ( -1.000000000000000000, 1.207181226542539700E-16, -2.694675058168174199E-16 ) ) ;
#74120 = AXIS2_PLACEMENT_3D ( 'NONE', #124371, #8276, #164774 ) ;
#74121 = CARTESIAN_POINT ( 'NONE',  ( -21.64999999999999858, 66.65000000001207070, -123.8731074845243683 ) ) ;
#74122 = ORIENTED_EDGE ( 'NONE', *, *, #82305, .F. ) ;
#74123 = ADVANCED_FACE ( 'NONE', ( #164738 ), #141319, .F. ) ;
#74124 = DIRECTION ( 'NONE',  ( 0.000000000000000000, 0.4930308989875575865, 0.8700118002898125091 ) ) ;
#74125 = ORIENTED_EDGE ( 'NONE', *, *, #42026, .F. ) ;
#74126 = FACE_OUTER_BOUND ( 'NONE', #118827, .T. ) ;
#74127 = CARTESIAN_POINT ( 'NONE',  ( -23.15000000000000213, 4.350000000011156054, -146.3500000000000227 ) ) ;
#74128 = CIRCLE ( 'NONE', #90820, 0.1000000000000028644 ) ;
#74129 = TOROIDAL_SURFACE ( 'NONE', #190643, 11.70000000000000107, 0.1000000000000000056 ) ;
#74130 =( GEOMETRIC_REPRESENTATION_CONTEXT ( 3 ) GLOBAL_UNCERTAINTY_ASSIGNED_CONTEXT ( ( #2310 ) ) GLOBAL_UNIT_ASSIGNED_CONTEXT ( ( #192241, #52698, #93114 ) ) REPRESENTATION_CONTEXT ( 'NONE', 'WORKASPACE' ) );
#74131 = ORIENTED_EDGE ( 'NONE', *, *, #102538, .F. ) ;
#74132 = CARTESIAN_POINT ( 'NONE',  ( 18.59999999999999076, 68.51069317435826633, -224.1259271199053842 ) ) ;
#74133 = ADVANCED_FACE ( 'NONE', ( #222108 ), #111122, .F. ) ;
#74134 = ORIENTED_EDGE ( 'NONE', *, *, #54532, .T. ) ;
#74135 = DIRECTION ( 'NONE',  ( 2.168404344971008868E-16, 0.000000000000000000, 1.000000000000000000 ) ) ;
#74136 = DIRECTION ( 'NONE',  ( 0.000000000000000000, 0.000000000000000000, 1.000000000000000000 ) ) ;
#74138 = DIRECTION ( 'NONE',  ( 0.000000000000000000, 0.000000000000000000, -1.000000000000000000 ) ) ;
#74137 = UNCERTAINTY_MEASURE_WITH_UNIT (LENGTH_MEASURE( 1.000000000000000082E-05 ), #63371, 'distance_accuracy_value', 'NONE');
#74139 = EDGE_CURVE ( 'NONE', #72694, #184776, #107619, .T. ) ;
#74140 = FACE_OUTER_BOUND ( 'NONE', #231370, .T. ) ;
#74141 = CARTESIAN_POINT ( 'NONE',  ( -16.80468759584938709, 9.942153675134134616, -12.69001886620163688 ) ) ;
#74142 = LINE ( 'NONE', #115803, #20859 ) ;
#74143 = LINE ( 'NONE', #153707, #147007 ) ;
#74144 = DIRECTION ( 'NONE',  ( 0.000000000000000000, -1.000000000000000000, 0.000000000000000000 ) ) ;
#74145 = EDGE_CURVE ( 'NONE', #183734, #242007, #157561, .T. ) ;
#74147 = VERTEX_POINT ( 'NONE', #51174 ) ;
#74146 = FACE_OUTER_BOUND ( 'NONE', #111235, .T. ) ;
#74149 = CARTESIAN_POINT ( 'NONE',  ( 18.59999999999999432, 77.26178616857710324, -128.4366085209788366 ) ) ;
#74148 = DIRECTION ( 'NONE',  ( 1.000000000000000000, 7.304098846218163263E-16, -4.217023435051627211E-16 ) ) ;
#74150 = ORIENTED_EDGE ( 'NONE', *, *, #60307, .F. ) ;
#74151 = ORIENTED_EDGE ( 'NONE', *, *, #242800, .F. ) ;
#74152 = AXIS2_PLACEMENT_3D ( 'NONE', #138701, #20092, #39674 ) ;
#74153 = VERTEX_POINT ( 'NONE', #69510 ) ;
#74154 = PLANE ( 'NONE',  #211556 ) ;
#74155 = CIRCLE ( 'NONE', #174119, 0.09999999999999939493 ) ;
#74156 = CONICAL_SURFACE ( 'NONE', #253171, 4.049999999999998046, 0.7853981633974604915 ) ;
#74157 = FACE_OUTER_BOUND ( 'NONE', #11025, .T. ) ;
#74158 = EDGE_CURVE ( 'NONE', #133901, #133788, #188157, .T. ) ;
#74159 = CLOSED_SHELL ( 'NONE', ( #94218, #62465, #47386, #99100, #213142, #254130, #117392, #86339, #49445, #46607, #146865, #111811, #248673, #92957, #87688, #38455, #56909, #20475, #248974, #42179, #238951, #251575, #239058, #57618, #87054, #124520, #147134, #10876, #178103, #187078, #53979, #180277, #81436, #8671, #15480, #117195, #203207, #19609, #47706, #206529, #62777, #211083, #11497, #245189, #8680, #103172, #159580, #155666, #241050, #223531, #107720, #252718, #243128, #19801, #188620, #66082, #76722, #41, #1654, #34112, #43697, #68301, #84406, #30154, #84419, #111716, #53209, #165302, #33829, #257919, #90752, #197376, #90397, #5188, #122658, #224102, #128441, #106426, #38299, #143878, #175190, #115957, #31171, #241697, #57590, #18078, #36959, #94571, #214026, #16443, #179700, #206314, #45910, #123519, #219630, #200550, #136581, #43311, #217156, #202370, #211654, #166819, #183, #62264, #190506, #68618, #109026, #37256, #141285, #250334, #154704, #96617, #171761, #20002, #159192, #21656, #148560, #31178, #13160, #220755, #170083, #253042, #207171, #154268, #211053, #174047, #257600, #179895, #216507, #164476, #80796, #193836, #1461, #252965, #22928, #234852, #171957, #55098, #155773, #89987, #209077, #244291, #173408, #88454, #240625, #46885, #219067, #200978, #251026, #237764, #100790, #9119, #32935, #48792, #245145, #123813, #253806, #195979, #101160, #4370, #234431, #102105, #84654, #255607, #113887, #226508, #1778, #207399, #135297, #77996, #40184, #88982, #193446, #89173, #206546, #246249, #241885, #256052, #230326, #228145, #142634, #93782, #124069, #253958, #111605, #9751, #88994, #186969, #233690, #63621, #22573, #30340, #144904, #18756, #116753, #186250, #236294, #79149, #222503, #119852, #85301, #73010, #70640, #16353, #152295, #195344, #242804, #237845, #38514, #106971, #218210, #131771, #67056, #72281, #25719, #144010, #212266, #172633, #197925, #54814, #186819, #25823, #133667, #57669, #218286, #236616, #147449, #47068, #41717, #227342, #151141, #64007, #66390, #122446, #175180, #339, #80567, #166673, #76529, #114324, #25525, #53560, #173757, #145933, #63458, #84017, #69389, #192058, #81747, #196469, #91341, #150968, #149574, #18539, #26190, #50794, #92326, #232793, #125541, #44672, #214374, #148622, #2114, #143285, #190090, #218395, #126833, #200403, #151770, #196371, #129970, #113263, #56435, #141168, #140562, #99243, #202389, #206494, #73044, #155921, #103825, #249541, #236848, #61180, #132073, #1051, #16155, #138651, #30865, #230690, #139926, #38200, #232754, #255294, #69823, #78321, #17116, #18783, #91340, #143208, #32268, #121435, #211134, #197850, #196817, #212696, #36416, #71238, #97290, #189812, #156181, #21894, #99254, #166061, #40324, #124734, #108633, #92428, #143960, #163225, #162801, #254985, #36532, #193683, #119040, #239316, #120377, #83105, #30239, #44185, #122485, #178403, #35231, #163001, #213091, #59579, #122114, #10267, #22514, #77563, #141583, #225177, #174703, #176625, #60423, #48027, #4080, #144506, #132413, #187231, #116301, #13321, #1346, #12676, #123523, #86947, #218777, #48867, #155553, #225649, #239244 ) ) ;
#74160 = EDGE_CURVE ( 'NONE', #192351, #5146, #74361, .T. ) ;
#74161 = CARTESIAN_POINT ( 'NONE',  ( 21.05000000000000071, 62.86885547537412577, -207.0505773246641752 ) ) ;
#74162 = LINE ( 'NONE', #254030, #59910 ) ;
#74163 = DIRECTION ( 'NONE',  ( -1.000000000000000000, 0.000000000000000000, 0.000000000000000000 ) ) ;
#74164 = CYLINDRICAL_SURFACE ( 'NONE', #14660, 0.09999999999999939493 ) ;
#74165 = CARTESIAN_POINT ( 'NONE',  ( -18.50000000000000000, 61.53642629385834795, -221.5144953033309321 ) ) ;
#74166 = AXIS2_PLACEMENT_3D ( 'NONE', #105042, #144196, #243303 ) ;
#74167 = TOROIDAL_SURFACE ( 'NONE', #194953, 11.89999999999999858, 0.1000000000000000056 ) ;
#74168 = DIRECTION ( 'NONE',  ( 0.000000000000000000, 0.000000000000000000, -1.000000000000000000 ) ) ;
#74169 = ORIENTED_EDGE ( 'NONE', *, *, #226259, .T. ) ;
#74170 = VERTEX_POINT ( 'NONE', #111186 ) ;
#74171 = CARTESIAN_POINT ( 'NONE',  ( 23.24999999999999645, 1.115600667400684642E-11, -134.0000000000000284 ) ) ;
#74172 = VECTOR ( 'NONE', #98070, 999.9999999999998863 ) ;
#74173 = EDGE_CURVE ( 'NONE', #3474, #164498, #12108, .T. ) ;
#74174 = ORIENTED_EDGE ( 'NONE', *, *, #191812, .F. ) ;
#74175 = DIRECTION ( 'NONE',  ( 0.000000000000000000, 0.2617529984165152257, 0.9651348961777124202 ) ) ;
#74177 = ADVANCED_FACE ( 'NONE', ( #231157 ), #227267, .T. ) ;
#74176 = ORIENTED_EDGE ( 'NONE', *, *, #110289, .F. ) ;
#74178 = CARTESIAN_POINT ( 'NONE',  ( 18.46932045258647648, -9.670685200265751291, -40.17386037299664991 ) ) ;
#74179 = AXIS2_PLACEMENT_3D ( 'NONE', #111138, #193253, #9465 ) ;
#74180 = SPHERICAL_SURFACE ( 'NONE', #138404, 0.1000000000000000056 ) ;
#74181 = DIRECTION ( 'NONE',  ( 0.000000000000000000, 0.000000000000000000, 1.000000000000000000 ) ) ;
#74182 = EDGE_CURVE ( 'NONE', #251797, #183226, #253381, .T. ) ;
#74183 = DIRECTION ( 'NONE',  ( 1.000000000000000000, 0.000000000000000000, 0.000000000000000000 ) ) ;
#74184 = CARTESIAN_POINT ( 'NONE',  ( 21.12642695952774119, 75.90109671682336057, -209.8987674065595286 ) ) ;
#74185 = EDGE_LOOP ( 'NONE', ( #175621, #49460, #234039, #219681, #136887, #176495, #51322, #104742, #169265, #53010, #54297, #156561 ) ) ;
#74186 = VECTOR ( 'NONE', #239384, 999.9999999999998863 ) ;
#74187 = LINE ( 'NONE', #115842, #141971 ) ;
#74188 = CYLINDRICAL_SURFACE ( 'NONE', #121569, 4.000000000000006217 ) ;
#74189 = VECTOR ( 'NONE', #228922, 1000.000000000000000 ) ;
#74191 = DIRECTION ( 'NONE',  ( -1.000000000000000000, -0.000000000000000000, 0.000000000000000000 ) ) ;
#74190 = AXIS2_PLACEMENT_3D ( 'NONE', #145181, #146460, #126922 ) ;
#74192 = EDGE_CURVE ( 'NONE', #233652, #32887, #145032, .T. ) ;
#74193 = DIRECTION ( 'NONE',  ( -3.469446951953738513E-14, 0.9770955615653543758, 0.2128009952262553683 ) ) ;
#74194 = CIRCLE ( 'NONE', #103355, 0.5000000000000004441 ) ;
#74195 = CARTESIAN_POINT ( 'NONE',  ( 20.04142135623731136, 11.75000000001116085, -125.2671572875254213 ) ) ;
#74197 = VERTEX_POINT ( 'NONE', #43069 ) ;
#74196 = ADVANCED_FACE ( 'NONE', ( #163031 ), #83439, .F. ) ;
#74199 = DIRECTION ( 'NONE',  ( 0.000000000000000000, -0.1350103645451876666, -0.9908441862701600211 ) ) ;
#74198 = FACE_OUTER_BOUND ( 'NONE', #1217, .T. ) ;
#74200 = ORIENTED_EDGE ( 'NONE', *, *, #22695, .T. ) ;
#74203 = VERTEX_POINT ( 'NONE', #204684 ) ;
#74202 = DIRECTION ( 'NONE',  ( -1.000000000000000000, -0.000000000000000000, -0.000000000000000000 ) ) ;
#74201 = FACE_OUTER_BOUND ( 'NONE', #193229, .T. ) ;
#74204 = AXIS2_PLACEMENT_3D ( 'NONE', #30663, #148021, #47607 ) ;
#74205 = CARTESIAN_POINT ( 'NONE',  ( -22.59999999999999787, 75.90000000001222702, -148.1726782920690937 ) ) ;
#74206 = EDGE_CURVE ( 'NONE', #222707, #23293, #18040, .T. ) ;
#74207 = DIRECTION ( 'NONE',  ( 1.000000000000000000, 8.153259210133938153E-16, 2.158126701439427964E-16 ) ) ;
#74208 = ORIENTED_EDGE ( 'NONE', *, *, #201831, .F. ) ;
#74209 = DIRECTION ( 'NONE',  ( 0.000000000000000000, 0.000000000000000000, -1.000000000000000000 ) ) ;
#74210 = DIRECTION ( 'NONE',  ( 0.000000000000000000, -0.8660254037844377084, -0.5000000000000016653 ) ) ;
#74211 = CARTESIAN_POINT ( 'NONE',  ( -22.48479450179659977, -3.118395934723631413, -228.1902321699264746 ) ) ;
#74212 = ADVANCED_FACE ( 'NONE', ( #44360 ), #47891, .T. ) ;
#74214 = ORIENTED_EDGE ( 'NONE', *, *, #144735, .F. ) ;
#74213 = DIRECTION ( 'NONE',  ( 1.000000000000000000, -0.000000000000000000, -0.000000000000000000 ) ) ;
#74215 = AXIS2_PLACEMENT_3D ( 'NONE', #82085, #177398, #256844 ) ;
#74216 = ORIENTED_EDGE ( 'NONE', *, *, #86219, .F. ) ;
#74217 = FACE_OUTER_BOUND ( 'NONE', #97765, .T. ) ;
#74218 = FACE_OUTER_BOUND ( 'NONE', #55000, .T. ) ;
#74219 = DIRECTION ( 'NONE',  ( 0.000000000000000000, -6.982962677686266711E-15, 1.000000000000000000 ) ) ;
#74220 = CIRCLE ( 'NONE', #219923, 0.1000000000000024342 ) ;
#74221 = CARTESIAN_POINT ( 'NONE',  ( 20.94999999999999929, 61.95000000001194707, -108.5368025552853197 ) ) ;
#74222 = VERTEX_POINT ( 'NONE', #246402 ) ;
#74223 = DIRECTION ( 'NONE',  ( 0.000000000000000000, 0.000000000000000000, 1.000000000000000000 ) ) ;
#74224 = DIRECTION ( 'NONE',  ( 0.000000000000000000, 0.000000000000000000, 1.000000000000000000 ) ) ;
#74225 = CARTESIAN_POINT ( 'NONE',  ( -16.87683809663752399, 9.850000000011144508, -53.59763598180369826 ) ) ;
#74226 = ORIENTED_EDGE ( 'NONE', *, *, #219922, .T. ) ;
#74227 = CARTESIAN_POINT ( 'NONE',  ( 20.86036036209928923, 58.98722522104349508, -225.6759763284424309 ) ) ;
#74228 = CARTESIAN_POINT ( 'NONE',  ( 18.49999999999998934, 6.550000000011156231, -77.01702717044007329 ) ) ;
#74229 = VERTEX_POINT ( 'NONE', #108181 ) ;
#74230 = AXIS2_PLACEMENT_3D ( 'NONE', #116401, #73442, #96793 ) ;
#74231 = AXIS2_PLACEMENT_3D ( 'NONE', #233758, #57655, #74717 ) ;
#74233 = TOROIDAL_SURFACE ( 'NONE', #219943, 0.4000000000000005773, 0.1000000000000000056 ) ;
#74232 = DIRECTION ( 'NONE',  ( 0.000000000000000000, -1.000000000000000000, 0.000000000000000000 ) ) ;
#74234 = LINE ( 'NONE', #153786, #185488 ) ;
#74235 = AXIS2_PLACEMENT_3D ( 'NONE', #77520, #99650, #119260 ) ;
#74236 = ORIENTED_EDGE ( 'NONE', *, *, #170429, .F. ) ;
#74237 = ORIENTED_EDGE ( 'NONE', *, *, #91438, .T. ) ;
#74238 = DIRECTION ( 'NONE',  ( -1.000000000000000000, 0.000000000000000000, 0.000000000000000000 ) ) ;
#74239 = ADVANCED_FACE ( 'NONE', ( #207291 ), #78396, .T. ) ;
#74240 = ORIENTED_EDGE ( 'NONE', *, *, #57814, .F. ) ;
#74242 = EDGE_LOOP ( 'NONE', ( #40290, #90827, #1043, #147618 ) ) ;
#74241 = CARTESIAN_POINT ( 'NONE',  ( 21.05000000000000071, 69.65000000001205649, -126.6792853948412159 ) ) ;
#74245 = EDGE_LOOP ( 'NONE', ( #141423, #213071, #107675, #46974 ) ) ;
#74244 = ORIENTED_EDGE ( 'NONE', *, *, #33820, .T. ) ;
#74243 = LINE ( 'NONE', #172061, #76284 ) ;
#74246 = CIRCLE ( 'NONE', #128379, 0.09999999999998898659 ) ;
#74247 = B_SPLINE_CURVE_WITH_KNOTS ( 'NONE', 3,
 ( #153539, #34852, #131350, #13988, #169237, #111802, #192620, #148353, #72696, #113082 ),
 .UNSPECIFIED., .F., .F.,
 ( 4, 2, 2, 2, 4 ),
 ( 0.000000000000000000, 4.221631689688577077E-05, 8.443263379377154154E-05, 0.0001688652675874691676, 0.0003377305351749402868 ),
 .UNSPECIFIED. ) ;
#74248 = CARTESIAN_POINT ( 'NONE',  ( -23.15000000000000213, 1.115600667400684642E-11, -67.00000000000004263 ) ) ;
#74249 = CIRCLE ( 'NONE', #7771, 0.2000000000000057288 ) ;
#74250 = CARTESIAN_POINT ( 'NONE',  ( -16.85722902420162228, 12.43862204461421150, -211.3557898750716788 ) ) ;
#74252 = EDGE_CURVE ( 'NONE', #225390, #63280, #226830, .T. ) ;
#74251 = CARTESIAN_POINT ( 'NONE',  ( 18.39999999999999503, 28.17589918783267322, -238.5974746063260739 ) ) ;
#74253 = DIRECTION ( 'NONE',  ( -0.000000000000000000, 0.1350103645451835865, 0.9908441862701605762 ) ) ;
#74254 = DIRECTION ( 'NONE',  ( 1.000000000000000000, -2.952720810173289112E-16, -2.061873921506763405E-30 ) ) ;
#74255 = AXIS2_PLACEMENT_3D ( 'NONE', #224012, #24566, #244862 ) ;
#74256 = CARTESIAN_POINT ( 'NONE',  ( -18.59999999999999787, 72.08710075277841156, -91.54128451151336776 ) ) ;
#74257 = EDGE_LOOP ( 'NONE', ( #256941, #105502, #107981, #208555 ) ) ;
#74258 = ORIENTED_EDGE ( 'NONE', *, *, #44922, .T. ) ;
#74259 = ORIENTED_EDGE ( 'NONE', *, *, #180062, .F. ) ;
#74260 = DIRECTION ( 'NONE',  ( 1.000000000000000000, 7.304098846218135653E-16, 5.100424963727256530E-30 ) ) ;
#74262 = ORIENTED_EDGE ( 'NONE', *, *, #115866, .T. ) ;
#74261 = CARTESIAN_POINT ( 'NONE',  ( 21.05000000000000071, 45.02833974712562792, -238.5149546970766892 ) ) ;
#74263 = DIRECTION ( 'NONE',  ( 1.000000000000000000, 0.000000000000000000, 0.000000000000000000 ) ) ;
#74264 = ORIENTED_EDGE ( 'NONE', *, *, #110996, .F. ) ;
#74265 = ORIENTED_EDGE ( 'NONE', *, *, #81700, .F. ) ;
#74266 = FACE_OUTER_BOUND ( 'NONE', #144228, .T. ) ;
#74267 = ORIENTED_EDGE ( 'NONE', *, *, #160748, .F. ) ;
#74268 = DIRECTION ( 'NONE',  ( 0.000000000000000000, -7.487053152578134969E-15, 1.000000000000000000 ) ) ;
#74269 = DIRECTION ( 'NONE',  ( -1.073024830501117725E-15, 0.000000000000000000, 1.000000000000000000 ) ) ;
#74270 = VECTOR ( 'NONE', #44403, 1000.000000000000000 ) ;
#74271 = AXIS2_PLACEMENT_3D ( 'NONE', #181194, #24697, #27273 ) ;
#74273 = ORIENTED_EDGE ( 'NONE', *, *, #169067, .F. ) ;
#74272 = ORIENTED_EDGE ( 'NONE', *, *, #938, .F. ) ;
#74274 = ORIENTED_EDGE ( 'NONE', *, *, #203888, .T. ) ;
#74275 = CARTESIAN_POINT ( 'NONE',  ( 21.05000000000000071, 8.815452279197549146, -8.420392552614265114 ) ) ;
#74276 = ORIENTED_EDGE ( 'NONE', *, *, #243109, .F. ) ;
#74277 = ORIENTED_EDGE ( 'NONE', *, *, #11566, .T. ) ;
#74278 = CARTESIAN_POINT ( 'NONE',  ( -23.25000000000000000, 43.62273694548321146, -253.2814864317374770 ) ) ;
#74280 = ORIENTED_EDGE ( 'NONE', *, *, #196165, .T. ) ;
#74279 = DIRECTION ( 'NONE',  ( -1.836970198721029934E-16, 1.000000000000000000, 0.000000000000000000 ) ) ;
#74281 = LINE ( 'NONE', #192918, #73411 ) ;
#74282 = AXIS2_PLACEMENT_3D ( 'NONE', #210374, #252053, #73450 ) ;
#74284 = CARTESIAN_POINT ( 'NONE',  ( -21.29999999999995808, 1.115650265596050101E-11, -29.45000000000000284 ) ) ;
#74283 = DIRECTION ( 'NONE',  ( 1.000000000000000000, 0.000000000000000000, 0.000000000000000000 ) ) ;
#74285 = DIRECTION ( 'NONE',  ( 1.000000000000000000, 0.000000000000000000, 0.000000000000000000 ) ) ;
#74286 = DIRECTION ( 'NONE',  ( -1.000000000000000000, 2.952720810173289112E-16, 2.061873921506763405E-30 ) ) ;
#74287 = ORIENTED_EDGE ( 'NONE', *, *, #128428, .F. ) ;
#74288 = ORIENTED_EDGE ( 'NONE', *, *, #98920, .T. ) ;
#74289 = CARTESIAN_POINT ( 'NONE',  ( 18.59999996954842771, 85.52320413787082032, -96.14006577260795439 ) ) ;
#74290 = CARTESIAN_POINT ( 'NONE',  ( -22.39999999999999858, -1.560176095955062348, -193.3663837337744837 ) ) ;
#74291 = DIRECTION ( 'NONE',  ( 0.000000000000000000, 1.000000000000000000, 0.000000000000000000 ) ) ;
#74292 = ADVANCED_FACE ( 'NONE', ( #142156, #28684 ), #9069, .F. ) ;
#74293 = VERTEX_POINT ( 'NONE', #5185 ) ;
#74294 = CIRCLE ( 'NONE', #86695, 0.1000000000000124678 ) ;
#74296 = DIRECTION ( 'NONE',  ( 0.000000000000000000, -0.8814952561688430555, 0.4721928772777346239 ) ) ;
#74295 = CIRCLE ( 'NONE', #95106, 0.1000000000000028644 ) ;
#74297 = VECTOR ( 'NONE', #244417, 1000.000000000000000 ) ;
#74298 = DIRECTION ( 'NONE',  ( 0.000000000000000000, -1.000000000000000000, 0.000000000000000000 ) ) ;
#74299 = CARTESIAN_POINT ( 'NONE',  ( 18.69999999999999929, 1.212568896937007645, -7.800000000000000711 ) ) ;
#74300 = AXIS2_PLACEMENT_3D ( 'NONE', #158118, #197188, #255836 ) ;
#74301 = VERTEX_POINT ( 'NONE', #164307 ) ;
#74302 = ORIENTED_EDGE ( 'NONE', *, *, #133771, .T. ) ;
#74303 = EDGE_CURVE ( 'NONE', #232474, #96897, #116032, .T. ) ;
#74304 = DIRECTION ( 'NONE',  ( 0.000000000000000000, -1.000000000000000000, -6.982962677686266711E-15 ) ) ;
#74305 = DIRECTION ( 'NONE',  ( 0.000000000000000000, 1.000000000000000000, 6.982962677686266711E-15 ) ) ;
#74306 = ORIENTED_EDGE ( 'NONE', *, *, #38623, .T. ) ;
#74307 = CARTESIAN_POINT ( 'NONE',  ( -18.50000000000000000, -9.399999999988850163, -174.7972597596632625 ) ) ;
#74308 = VERTEX_POINT ( 'NONE', #168191 ) ;
#74309 = CARTESIAN_POINT ( 'NONE',  ( 18.58725287972279361, -9.566626910681348406, -140.8225048057644244 ) ) ;
#74310 = CARTESIAN_POINT ( 'NONE',  ( 18.49999999999999289, 7.474345188812916874, -187.3467314563696107 ) ) ;
#74312 = DIRECTION ( 'NONE',  ( 7.304098846218135653E-16, 0.9651348961777157509, -0.2617529984165031243 ) ) ;
#74311 = CARTESIAN_POINT ( 'NONE',  ( -18.50000000000000000, 1.835341550235567887, -112.0551512925630249 ) ) ;
#74313 = EDGE_CURVE ( 'NONE', #156398, #151223, #120145, .T. ) ;
#74314 = CIRCLE ( 'NONE', #253333, 0.2000000000000057288 ) ;
#74315 = CARTESIAN_POINT ( 'NONE',  ( -20.54999999999999716, 47.48953316408024961, -242.5895867826444601 ) ) ;
#74316 = CARTESIAN_POINT ( 'NONE',  ( 20.94999999999999929, -11.48912529306489994, -97.60000000000005116 ) ) ;
#74318 = EDGE_CURVE ( 'NONE', #252850, #107953, #165919, .T. ) ;
#74317 = TOROIDAL_SURFACE ( 'NONE', #157715, 0.4000000000000005773, 0.1000000000000000056 ) ;
#74319 = CARTESIAN_POINT ( 'NONE',  ( 20.94999999999999929, 0.000000000000000000, -33.50000000000000000 ) ) ;
#74320 = VECTOR ( 'NONE', #48254, 1000.000000000000000 ) ;
#74323 = ORIENTED_EDGE ( 'NONE', *, *, #185009, .T. ) ;
#74322 = EDGE_LOOP ( 'NONE', ( #212481, #209558, #75993, #196765 ) ) ;
#74321 = VECTOR ( 'NONE', #113720, 1000.000000000000000 ) ;
#74324 = ORIENTED_EDGE ( 'NONE', *, *, #109274, .T. ) ;
#74325 = AXIS2_PLACEMENT_3D ( 'NONE', #210215, #169833, #249342 ) ;
#74326 = VECTOR ( 'NONE', #223074, 1000.000000000000000 ) ;
#74327 = AXIS2_PLACEMENT_3D ( 'NONE', #46560, #123554, #184800 ) ;
#74328 = CARTESIAN_POINT ( 'NONE',  ( -21.05000000000000071, 76.00000000001190870, -103.0231074845243029 ) ) ;
#74329 = CARTESIAN_POINT ( 'NONE',  ( 22.49806830649814060, 0.07746431632550720980, 11.64988965483908068 ) ) ;
#74330 = CARTESIAN_POINT ( 'NONE',  ( -23.25000000000000000, 2.000000000011154189, -154.2753780772379173 ) ) ;
#74331 = CIRCLE ( 'NONE', #32641, 0.1000000000000013933 ) ;
#74332 = ADVANCED_FACE ( 'NONE', ( #49481 ), #162936, .T. ) ;
#74334 = DIRECTION ( 'NONE',  ( -0.000000000000000000, 0.000000000000000000, -1.000000000000000000 ) ) ;
#74333 = PLANE ( 'NONE',  #241076 ) ;
#74335 = CARTESIAN_POINT ( 'NONE',  ( 21.14999999999999858, 11.75000000001116263, -155.7499999999999716 ) ) ;
#74336 = VERTEX_POINT ( 'NONE', #208577 ) ;
#74337 = CARTESIAN_POINT ( 'NONE',  ( 21.93340585971891343, 68.67585297715665149, -69.52310748452435973 ) ) ;
#74338 = ORIENTED_EDGE ( 'NONE', *, *, #177845, .F. ) ;
#74339 = VERTEX_POINT ( 'NONE', #149887 ) ;
#74340 = CARTESIAN_POINT ( 'NONE',  ( 12.25000000000000000, 66.65000000001204228, -119.7731074845243739 ) ) ;
#74341 = CARTESIAN_POINT ( 'NONE',  ( -22.48479450179659977, 0.04699158119804078271, -88.85000155374841313 ) ) ;
#74342 = CARTESIAN_POINT ( 'NONE',  ( 19.58285714285715073, 9.015001489659738354, -175.9206528160816845 ) ) ;
#74343 = VECTOR ( 'NONE', #136702, 1000.000000000000114 ) ;
#74344 = TOROIDAL_SURFACE ( 'NONE', #36928, 0.6000000000000009770, 0.1000000000000000056 ) ;
#74345 = DIRECTION ( 'NONE',  ( 0.000000000000000000, 0.000000000000000000, -1.000000000000000000 ) ) ;
#74346 = CARTESIAN_POINT ( 'NONE',  ( 20.94999999999999929, 39.26973050389061370, -236.6309188891183055 ) ) ;
#74347 = ORIENTED_EDGE ( 'NONE', *, *, #74570, .T. ) ;
#74348 = EDGE_LOOP ( 'NONE', ( #28630, #196534, #22042, #179868 ) ) ;
#74349 = DIRECTION ( 'NONE',  ( 0.000000000000000000, -1.000000000000000000, 0.000000000000000000 ) ) ;
#74350 = DIRECTION ( 'NONE',  ( -3.469446951953635015E-14, -1.000000000000000000, 0.000000000000000000 ) ) ;
#74351 = FACE_OUTER_BOUND ( 'NONE', #3267, .T. ) ;
#74352 = FACE_OUTER_BOUND ( 'NONE', #103068, .T. ) ;
#74353 = FACE_OUTER_BOUND ( 'NONE', #78067, .T. ) ;
#74354 = CARTESIAN_POINT ( 'NONE',  ( 21.72449340488910607, 10.28395627750226815, -87.85000000000003695 ) ) ;
#74356 = EDGE_CURVE ( 'NONE', #178668, #102259, #92442, .T. ) ;
#74355 = LINE ( 'NONE', #209989, #100113 ) ;
#74357 = AXIS2_PLACEMENT_3D ( 'NONE', #112200, #56018, #131738 ) ;
#74359 = DIRECTION ( 'NONE',  ( 1.000000000000000000, 0.000000000000000000, -0.000000000000000000 ) ) ;
#74358 = CARTESIAN_POINT ( 'NONE',  ( -22.49756042579671700, 0.07804633701718154126, 11.64986496110232572 ) ) ;
#74360 = CARTESIAN_POINT ( 'NONE',  ( 22.39999999999999503, 1.115600667400684642E-11, -25.70922040162662370 ) ) ;
#74362 = B_SPLINE_CURVE_WITH_KNOTS ( 'NONE', 3,
 ( #3415, #163804, #82935, #199070, #21723, #243316, #64685, #144207, #20450, #162531 ),
 .UNSPECIFIED., .F., .F.,
 ( 4, 3, 3, 4 ),
 ( 1.891508146150501351E-15, 3.877043166999833362E-05, 7.336897548476496527E-05, 7.659383120240286283E-05 ),
 .UNSPECIFIED. ) ;
#74361 = CIRCLE ( 'NONE', #3563, 0.09999999999999939493 ) ;
#74363 = CYLINDRICAL_SURFACE ( 'NONE', #75049, 0.1000000000000028644 ) ;
#74364 = DIRECTION ( 'NONE',  ( 0.000000000000000000, -0.4721928772777342354, -0.8814952561688431665 ) ) ;
#74366 = DIRECTION ( 'NONE',  ( 1.000000000000000000, -6.938893903907222067E-15, -4.845403715540888588E-29 ) ) ;
#74365 = VECTOR ( 'NONE', #145899, 1000.000000000000114 ) ;
#74368 = ORIENTED_EDGE ( 'NONE', *, *, #111090, .T. ) ;
#74367 = DIRECTION ( 'NONE',  ( -1.000000000000000000, -0.000000000000000000, -0.000000000000000000 ) ) ;
#74369 = AXIS2_PLACEMENT_3D ( 'NONE', #38678, #185877, #128481 ) ;
#74370 = EDGE_CURVE ( 'NONE', #10361, #52922, #7690, .T. ) ;
#74371 = DIRECTION ( 'NONE',  ( 0.000000000000000000, -0.000000000000000000, 1.000000000000000000 ) ) ;
#74372 = CIRCLE ( 'NONE', #15916, 0.1000000000000028644 ) ;
#74373 = ADVANCED_FACE ( 'NONE', ( #54603 ), #173331, .T. ) ;
#74374 = DIRECTION ( 'NONE',  ( -1.000000000000000000, -0.000000000000000000, -0.000000000000000000 ) ) ;
#74375 = AXIS2_PLACEMENT_3D ( 'NONE', #248174, #185632, #145205 ) ;
#74376 = AXIS2_PLACEMENT_3D ( 'NONE', #185303, #6653, #44519 ) ;
#74377 = CARTESIAN_POINT ( 'NONE',  ( 21.00000000000000000, 14.04870287383362992, -219.6884709798077893 ) ) ;
#74378 = AXIS2_PLACEMENT_3D ( 'NONE', #244470, #170127, #71008 ) ;
#74379 = ADVANCED_FACE ( 'NONE', ( #229411 ), #35092, .T. ) ;
#74380 = CARTESIAN_POINT ( 'NONE',  ( 13.22461703343585171, 9.436662931810239741, -85.32303673229492347 ) ) ;
#74381 = CARTESIAN_POINT ( 'NONE',  ( 22.42196299218230493, 0.002441673998456600492, -21.85038829735053056 ) ) ;
#74382 = AXIS2_PLACEMENT_3D ( 'NONE', #20677, #100159, #81874 ) ;
#74383 = DIRECTION ( 'NONE',  ( -1.000000000000000000, 3.265361837132813093E-16, 2.280189983783949500E-30 ) ) ;
#74384 = DIRECTION ( 'NONE',  ( 0.000000000000000000, 0.000000000000000000, 1.000000000000000000 ) ) ;
#74385 = CARTESIAN_POINT ( 'NONE',  ( -20.54999999999999716, 7.150000000011155876, -83.75000000000004263 ) ) ;
#74386 = ORIENTED_EDGE ( 'NONE', *, *, #137929, .F. ) ;
#74387 = DIRECTION ( 'NONE',  ( 0.000000000000000000, 6.982962677686266711E-15, -1.000000000000000000 ) ) ;
#74389 = ORIENTED_EDGE ( 'NONE', *, *, #215703, .T. ) ;
#74388 = CARTESIAN_POINT ( 'NONE',  ( 21.30000000000002558, 3.558777552609279304, -231.8203201594644725 ) ) ;
#74390 = CARTESIAN_POINT ( 'NONE',  ( -22.47071067811865319, 75.90090754530959316, -144.2431822290223522 ) ) ;
#74391 = ADVANCED_FACE ( 'NONE', ( #131582 ), #129028, .F. ) ;
#74392 = CARTESIAN_POINT ( 'NONE',  ( -16.79363873026997922, 9.948850229429586634, -188.3461537814454516 ) ) ;
#74393 = DIRECTION ( 'NONE',  ( -1.000000000000000000, -0.000000000000000000, 0.000000000000000000 ) ) ;
#74394 = ORIENTED_EDGE ( 'NONE', *, *, #218098, .T. ) ;
#74395 = CARTESIAN_POINT ( 'NONE',  ( -16.82542659449972788, 66.06550010858516941, -190.7784718844984013 ) ) ;
#74396 = CIRCLE ( 'NONE', #32885, 0.1000000000000091649 ) ;
#74397 = ADVANCED_FACE ( 'NONE', ( #112034 ), #33813, .T. ) ;
#74398 = APPLICATION_PROTOCOL_DEFINITION ( 'draft international standard', 'automotive_design', 1998, #65706 ) ;
#74399 = EDGE_CURVE ( 'NONE', #159790, #220173, #110732, .T. ) ;
#74400 = CARTESIAN_POINT ( 'NONE',  ( 22.49999999999999289, 11.45898712536580710, -198.4011321578509808 ) ) ;
#74401 = CARTESIAN_POINT ( 'NONE',  ( -18.50000000000000000, 66.85000000001180354, -81.87310748452438247 ) ) ;
#74402 = ORIENTED_EDGE ( 'NONE', *, *, #188861, .T. ) ;
#74403 = CARTESIAN_POINT ( 'NONE',  ( 18.49999999999999289, 63.83083047455526327, -209.3924252461221158 ) ) ;
#74404 = DIRECTION ( 'NONE',  ( 1.186688945009009831E-16, -0.9770955615653313941, -0.2128009952263603677 ) ) ;
#74405 = ADVANCED_FACE ( 'NONE', ( #74217 ), #103330, .F. ) ;
#74406 = LINE ( 'NONE', #58631, #191028 ) ;
#74407 = EDGE_LOOP ( 'NONE', ( #156490, #201017, #116115 ) ) ;
#74408 = ORIENTED_EDGE ( 'NONE', *, *, #136881, .T. ) ;
#74409 = ADVANCED_FACE ( 'NONE', ( #231989 ), #93738, .T. ) ;
#74410 = ADVANCED_FACE ( 'NONE', ( #233279 ), #72930, .T. ) ;
#74411 = CARTESIAN_POINT ( 'NONE',  ( -23.25000000000000000, 65.66751761918619934, -30.42826094061123854 ) ) ;
#74412 = DIRECTION ( 'NONE',  ( 0.000000000000000000, -6.308085367188393199E-16, -1.000000000000000000 ) ) ;
#74413 = DIRECTION ( 'NONE',  ( 1.000000000000000000, -7.510212038922846022E-17, 1.676432719286211941E-16 ) ) ;
#74414 = CARTESIAN_POINT ( 'NONE',  ( -20.15000000000000568, 9.291421356248463326, -45.85000000000000142 ) ) ;
#74416 = DIRECTION ( 'NONE',  ( -6.938893903907222067E-15, -1.000000000000000000, -7.272083257015735086E-15 ) ) ;
#74415 = DIRECTION ( 'NONE',  ( -1.000000000000000000, -2.952720810173289112E-16, 0.000000000000000000 ) ) ;
#74417 = AXIS2_PLACEMENT_3D ( 'NONE', #55758, #91077, #93643 ) ;
#74419 = DIRECTION ( 'NONE',  ( 0.000000000000000000, -0.4999999999999689138, 0.8660254037844565822 ) ) ;
#74418 = CIRCLE ( 'NONE', #70317, 0.09999999999999939493 ) ;
#74420 = CARTESIAN_POINT ( 'NONE',  ( -21.65000000000000213, 7.250000000011139534, -146.6500000000000341 ) ) ;
#74421 = CARTESIAN_POINT ( 'NONE',  ( -20.94999999999999929, 67.84340367245323478, -228.0791829662263410 ) ) ;
#74422 = CIRCLE ( 'NONE', #66183, 14.30833333333335311 ) ;
#74423 = CARTESIAN_POINT ( 'NONE',  ( -18.59999999999999787, 1.115600667400684642E-11, -167.5000000000000284 ) ) ;
#74424 = ORIENTED_EDGE ( 'NONE', *, *, #55927, .F. ) ;
#74425 = ORIENTED_EDGE ( 'NONE', *, *, #11499, .F. ) ;
#74426 = CARTESIAN_POINT ( 'NONE',  ( -21.04999999999994387, 73.58898499266442172, -51.80813886865390572 ) ) ;
#74427 = DIRECTION ( 'NONE',  ( 0.000000000000000000, 0.000000000000000000, -1.000000000000000000 ) ) ;
#74429 = DIRECTION ( 'NONE',  ( -1.000000000000000000, 0.000000000000000000, -0.000000000000000000 ) ) ;
#74428 = LINE ( 'NONE', #16999, #179693 ) ;
#74430 = VECTOR ( 'NONE', #125635, 1000.000000000000000 ) ;
#74431 = EDGE_CURVE ( 'NONE', #83776, #245477, #211882, .T. ) ;
#74432 = CARTESIAN_POINT ( 'NONE',  ( -21.14999999999999858, 55.91711482281189660, -232.6830152854666949 ) ) ;
#74434 = EDGE_CURVE ( 'NONE', #64265, #104499, #120339, .T. ) ;
#74433 = CARTESIAN_POINT ( 'NONE',  ( 20.04142135623731136, 64.25000000001196554, -111.8731074845243825 ) ) ;
#74435 = CARTESIAN_POINT ( 'NONE',  ( 12.42718393586865844, 12.88553809045802723, -216.1303193953968673 ) ) ;
#74436 = ORIENTED_EDGE ( 'NONE', *, *, #179866, .F. ) ;
#74437 = ORIENTED_EDGE ( 'NONE', *, *, #243414, .F. ) ;
#74438 = AXIS2_PLACEMENT_3D ( 'NONE', #96929, #233909, #55237 ) ;
#74439 = AXIS2_PLACEMENT_3D ( 'NONE', #204795, #183965, #26189 ) ;
#74440 = ADVANCED_FACE ( 'NONE', ( #178439 ), #157764, .F. ) ;
#74442 = VECTOR ( 'NONE', #241215, 999.9999999999998863 ) ;
#74441 = LINE ( 'NONE', #234757, #30254 ) ;
#74443 = ORIENTED_EDGE ( 'NONE', *, *, #158407, .F. ) ;
#74444 = DIRECTION ( 'NONE',  ( -6.938893903907221278E-15, -0.9651348961777157509, 0.2617529984165028467 ) ) ;
#74446 = CARTESIAN_POINT ( 'NONE',  ( -20.85000000000000142, 68.97833521811159585, -65.68954208262705663 ) ) ;
#74445 = AXIS2_PLACEMENT_3D ( 'NONE', #155763, #179177, #54055 ) ;
#74447 = DIRECTION ( 'NONE',  ( 0.8049926720990052686, 0.2801448344544982261, 0.5229776951222349091 ) ) ;
#74448 = ORIENTED_EDGE ( 'NONE', *, *, #171220, .T. ) ;
#74449 = CARTESIAN_POINT ( 'NONE',  ( -18.59999999999999787, 30.18746141061095045, -235.4776000216846796 ) ) ;
#74450 = B_SPLINE_CURVE_WITH_KNOTS ( 'NONE', 3,
 ( #134234, #196777, #78113, #234633 ),
 .UNSPECIFIED., .F., .F.,
 ( 4, 4 ),
 ( 0.000000000000000000, 7.713889350928925437E-05 ),
 .UNSPECIFIED. ) ;
#74451 = CYLINDRICAL_SURFACE ( 'NONE', #253644, 0.09999999999999693856 ) ;
#74452 = CARTESIAN_POINT ( 'NONE',  ( 21.05000000000000071, 0.09779029131994770863, -27.24218538952387547 ) ) ;
#74453 = EDGE_CURVE ( 'NONE', #12569, #232481, #136701, .T. ) ;
#74454 = CARTESIAN_POINT ( 'NONE',  ( -21.05000000000000071, 68.35681244624936426, -231.7050464529142459 ) ) ;
#74455 = DIRECTION ( 'NONE',  ( 1.000000000000000000, 0.000000000000000000, 0.000000000000000000 ) ) ;
#74457 = DIRECTION ( 'NONE',  ( 0.000000000000000000, -1.000000000000000000, -8.609265936414504429E-15 ) ) ;
#74456 = DIRECTION ( 'NONE',  ( 1.000000000000000000, 0.000000000000000000, 0.000000000000000000 ) ) ;
#74458 = DIRECTION ( 'NONE',  ( 0.000000000000000000, -6.467318590049456648E-15, 1.000000000000000000 ) ) ;
#74459 = ADVANCED_FACE ( 'NONE', ( #135418 ), #154560, .T. ) ;
#74460 = ORIENTED_EDGE ( 'NONE', *, *, #56787, .T. ) ;
#74462 = CARTESIAN_POINT ( 'NONE',  ( -16.92989143108098560, 9.950000000011138823, -180.3824838747567014 ) ) ;
#74461 = CYLINDRICAL_SURFACE ( 'NONE', #24351, 0.1000000000000028644 ) ;
#74464 = ORIENTED_EDGE ( 'NONE', *, *, #17479, .T. ) ;
#74463 = VECTOR ( 'NONE', #216288, 1000.000000000000000 ) ;
#74466 = ORIENTED_EDGE ( 'NONE', *, *, #240014, .F. ) ;
#74465 = CARTESIAN_POINT ( 'NONE',  ( -23.15000000000000213, 11.65000000000000036, -26.48519422934605672 ) ) ;
#74467 = TOROIDAL_SURFACE ( 'NONE', #90987, 0.2000000000000000111, 0.1000000000000000056 ) ;
#74468 = ORIENTED_EDGE ( 'NONE', *, *, #36730, .F. ) ;
#74469 = CYLINDRICAL_SURFACE ( 'NONE', #149026, 0.09999999999999609201 ) ;
#74470 = CARTESIAN_POINT ( 'NONE',  ( 12.48201962039797408, 66.62334006147874277, -152.3949149363072024 ) ) ;
#74471 = CARTESIAN_POINT ( 'NONE',  ( -21.05000000000000071, 30.90801580390628800, -252.0203440857197279 ) ) ;
#74472 = DIRECTION ( 'NONE',  ( -1.836970198721029934E-16, 0.9770955615653316162, 0.2128009952263604232 ) ) ;
#74473 = VERTEX_POINT ( 'NONE', #235805 ) ;
#74474 = ADVANCED_FACE ( 'NONE', ( #1016 ), #216236, .F. ) ;
#74475 = CIRCLE ( 'NONE', #70369, 0.09999999999999939493 ) ;
#74476 = CARTESIAN_POINT ( 'NONE',  ( -20.94999999999999929, -11.48912529307605901, -3.100000000000000533 ) ) ;
#74477 = EDGE_CURVE ( 'NONE', #60251, #33844, #157607, .T. ) ;
#74478 = EDGE_LOOP ( 'NONE', ( #108828, #80563, #217309, #148134 ) ) ;
#74479 = DIRECTION ( 'NONE',  ( 1.000000000000000000, 0.000000000000000000, 0.000000000000000000 ) ) ;
#74480 = EDGE_CURVE ( 'NONE', #153430, #219970, #119735, .T. ) ;
#74481 = LINE ( 'NONE', #154032, #56066 ) ;
#74482 = AXIS2_PLACEMENT_3D ( 'NONE', #146011, #26089, #222979 ) ;
#74483 = ORIENTED_EDGE ( 'NONE', *, *, #26774, .F. ) ;
#74484 = ORIENTED_EDGE ( 'NONE', *, *, #69115, .F. ) ;
#74485 = AXIS2_PLACEMENT_3D ( 'NONE', #139404, #218954, #40369 ) ;
#74486 = CARTESIAN_POINT ( 'NONE',  ( -20.54999999999999716, 76.00000000001172396, -71.42310748452430857 ) ) ;
#74487 = TOROIDAL_SURFACE ( 'NONE', #124516, 0.2000000000000000111, 0.1000000000000000056 ) ;
#74488 = ADVANCED_FACE ( 'NONE', ( #199265 ), #255322, .T. ) ;
#74489 = VERTEX_POINT ( 'NONE', #76730 ) ;
#74490 = DIRECTION ( 'NONE',  ( 0.000000000000000000, 0.9999176327611370985, -0.01283462868041286391 ) ) ;
#74494 = ADVANCED_FACE ( 'NONE', ( #20637 ), #19336, .T. ) ;
#74493 = EDGE_CURVE ( 'NONE', #240054, #79346, #253541, .T. ) ;
#74492 = ORIENTED_EDGE ( 'NONE', *, *, #235169, .T. ) ;
#74491 = CIRCLE ( 'NONE', #37058, 0.09999999999998898659 ) ;
#74495 = CARTESIAN_POINT ( 'NONE',  ( 21.04999999999999716, 76.01681986839808758, -176.3305327040897055 ) ) ;
#74496 = LINE ( 'NONE', #92718, #14938 ) ;
#74497 = CARTESIAN_POINT ( 'NONE',  ( 23.15000000000000213, -11.48912529306489816, -97.40000000000004832 ) ) ;
#74498 = FACE_OUTER_BOUND ( 'NONE', #240879, .T. ) ;
#74499 = VECTOR ( 'NONE', #500, 1000.000000000000000 ) ;
#74500 = AXIS2_PLACEMENT_3D ( 'NONE', #151046, #170653, #111929 ) ;
#74501 = DIRECTION ( 'NONE',  ( -1.000000000000000000, -0.000000000000000000, -0.000000000000000000 ) ) ;
#74502 = CIRCLE ( 'NONE', #86898, 0.09999999999999939493 ) ;
#74503 = LINE ( 'NONE', #134405, #219572 ) ;
#74504 = LINE ( 'NONE', #131864, #205572 ) ;
#74506 = ORIENTED_EDGE ( 'NONE', *, *, #174275, .T. ) ;
#74505 = EDGE_CURVE ( 'NONE', #5643, #241641, #101383, .T. ) ;
#74509 = ADVANCED_FACE ( 'NONE', ( #239672 ), #121035, .T. ) ;
#74508 = CARTESIAN_POINT ( 'NONE',  ( 11.60000000000000142, -11.65000000000000036, 17.60000000000000497 ) ) ;
#74507 = CARTESIAN_POINT ( 'NONE',  ( 21.06280952165538167, 22.90470512554973581, -230.1276019220326532 ) ) ;
#74510 = ORIENTED_EDGE ( 'NONE', *, *, #113080, .F. ) ;
#74513 = ORIENTED_EDGE ( 'NONE', *, *, #18379, .T. ) ;
#74512 = LINE ( 'NONE', #237397, #96211 ) ;
#74511 = CARTESIAN_POINT ( 'NONE',  ( -23.25000000000000000, 66.21323668544584962, -222.9901119748073484 ) ) ;
#74514 = EDGE_LOOP ( 'NONE', ( #31183, #216888 ) ) ;
#74515 = DIRECTION ( 'NONE',  ( 7.304098846218134667E-16, 1.000000000000000000, -0.000000000000000000 ) ) ;
#74516 = CIRCLE ( 'NONE', #241080, 4.099999999999992539 ) ;
#74517 = CIRCLE ( 'NONE', #53627, 3.999999999999999112 ) ;
#74518 = CARTESIAN_POINT ( 'NONE',  ( 21.05000000000000071, -0.09999999998884512298, -60.45934304829879835 ) ) ;
#74519 = FACE_OUTER_BOUND ( 'NONE', #133851, .T. ) ;
#74520 = EDGE_CURVE ( 'NONE', #44645, #208853, #207796, .T. ) ;
#74522 = EDGE_LOOP ( 'NONE', ( #131029, #6578, #174984, #158939 ) ) ;
#74521 =( BOUNDED_CURVE ( )  B_SPLINE_CURVE ( 3, ( #182075, #67250, #204182, #26873 ),
 .UNSPECIFIED., .F., .F. ) 
 B_SPLINE_CURVE_WITH_KNOTS ( ( 4, 4 ),
 ( 4.712388980384690562, 6.283185307179586232 ),
 .UNSPECIFIED. ) 
 CURVE ( )  GEOMETRIC_REPRESENTATION_ITEM ( )  RATIONAL_B_SPLINE_CURVE ( ( 1.000000000000000000, 0.8047378541243652705, 0.8047378541243652705, 1.000000000000000000 ) ) 
 REPRESENTATION_ITEM ( '' )  );
#74524 = ORIENTED_EDGE ( 'NONE', *, *, #124839, .F. ) ;
#74523 = CARTESIAN_POINT ( 'NONE',  ( -16.86420534634261514, 66.02938455442028953, -115.6047709352869788 ) ) ;
#74525 = VECTOR ( 'NONE', #133569, 1000.000000000000000 ) ;
#74526 = EDGE_CURVE ( 'NONE', #217944, #68201, #182861, .T. ) ;
#74528 = DIRECTION ( 'NONE',  ( -0.000000000000000000, -1.000000000000000000, -7.272083257015735086E-15 ) ) ;
#74527 = FACE_OUTER_BOUND ( 'NONE', #4428, .T. ) ;
#74529 = ADVANCED_FACE ( 'NONE', ( #107154 ), #28762, .F. ) ;
#74531 = VERTEX_POINT ( 'NONE', #83705 ) ;
#74530 = CARTESIAN_POINT ( 'NONE',  ( -16.90128866880176162, 9.953795777214113016, -54.36267618338864338 ) ) ;
#74532 = PRODUCT ( 'Snap Open Cable Crossbars 9', 'Snap Open Cable Crossbars 9', '', ( #160344 ) ) ;
#74533 = VERTEX_POINT ( 'NONE', #122888 ) ;
#74534 = CIRCLE ( 'NONE', #161996, 0.09999999999999939493 ) ;
#74535 = CARTESIAN_POINT ( 'NONE',  ( 20.95575313997065336, 11.99325116692322268, -206.1879418114507985 ) ) ;
#74537 = VECTOR ( 'NONE', #131531, 1000.000000000000114 ) ;
#74536 = PLANE ( 'NONE',  #142809 ) ;
#74538 = EDGE_LOOP ( 'NONE', ( #168811, #34448, #236665, #134508 ) ) ;
#74539 = FACE_OUTER_BOUND ( 'NONE', #226683, .T. ) ;
#74540 = ORIENTED_EDGE ( 'NONE', *, *, #173922, .F. ) ;
#74542 = EDGE_CURVE ( 'NONE', #208877, #7521, #111932, .T. ) ;
#74541 = DIRECTION ( 'NONE',  ( 1.000000000000000000, 5.603460673774840016E-17, 1.046060675573451769E-16 ) ) ;
#74543 = SPHERICAL_SURFACE ( 'NONE', #84859, 0.1000000000000000056 ) ;
#74544 = EDGE_CURVE ( 'NONE', #231430, #234281, #247948, .T. ) ;
#74545 = ORIENTED_EDGE ( 'NONE', *, *, #145090, .T. ) ;
#74546 = CARTESIAN_POINT ( 'NONE',  ( 20.95000000000005258, 65.35000000001120668, -3.023107484524792277 ) ) ;
#74547 = VECTOR ( 'NONE', #82964, 1000.000000000000000 ) ;
#74548 = VECTOR ( 'NONE', #133148, 1000.000000000000000 ) ;
#74549 = ADVANCED_FACE ( 'NONE', ( #88857 ), #31210, .F. ) ;
#74550 = CIRCLE ( 'NONE', #91263, 0.09999999999999939493 ) ;
#74551 = DIRECTION ( 'NONE',  ( 0.000000000000000000, 0.000000000000000000, 1.000000000000000000 ) ) ;
#74552 = VECTOR ( 'NONE', #196151, 1000.000000000000000 ) ;
#74553 = ORIENTED_EDGE ( 'NONE', *, *, #33527, .T. ) ;
#74554 = ORIENTED_EDGE ( 'NONE', *, *, #173962, .F. ) ;
#74555 = CARTESIAN_POINT ( 'NONE',  ( 20.97565083910961192, 18.75479403086622199, -228.0776265554289068 ) ) ;
#74556 = ORIENTED_EDGE ( 'NONE', *, *, #218245, .T. ) ;
#74557 = EDGE_CURVE ( 'NONE', #232336, #24864, #195329, .T. ) ;
#74558 = VERTEX_POINT ( 'NONE', #206267 ) ;
#74560 = VERTEX_POINT ( 'NONE', #184121 ) ;
#74559 = PLANE ( 'NONE',  #42772 ) ;
#74561 = ORIENTED_EDGE ( 'NONE', *, *, #42676, .F. ) ;
#74562 = DIRECTION ( 'NONE',  ( 0.000000000000000000, 0.000000000000000000, -1.000000000000000000 ) ) ;
#74563 = AXIS2_PLACEMENT_3D ( 'NONE', #66349, #140743, #179890 ) ;
#74564 = ORIENTED_EDGE ( 'NONE', *, *, #64079, .T. ) ;
#74567 = ORIENTED_EDGE ( 'NONE', *, *, #400, .T. ) ;
#74566 = ORIENTED_EDGE ( 'NONE', *, *, #58462, .T. ) ;
#74565 = LINE ( 'NONE', #75804, #39560 ) ;
#74568 = AXIS2_PLACEMENT_3D ( 'NONE', #222017, #143781, #78664 ) ;
#74569 = ORIENTED_EDGE ( 'NONE', *, *, #138506, .F. ) ;
#74570 = EDGE_CURVE ( 'NONE', #227863, #166449, #65460, .T. ) ;
#74571 = VERTEX_POINT ( 'NONE', #87578 ) ;
#74572 = CARTESIAN_POINT ( 'NONE',  ( 20.95000000000005258, 64.25000000001119815, -5.923107484524795296 ) ) ;
#74574 = ORIENTED_EDGE ( 'NONE', *, *, #226155, .F. ) ;
#74573 = DIRECTION ( 'NONE',  ( 0.000000000000000000, -4.336808689942494997E-15, -1.000000000000000000 ) ) ;
#74575 = DIRECTION ( 'NONE',  ( 1.000000000000000000, -7.304098846218133681E-16, 4.217023435051677994E-16 ) ) ;
#74576 = ORIENTED_EDGE ( 'NONE', *, *, #228139, .F. ) ;
#74577 =( BOUNDED_SURFACE ( )  B_SPLINE_SURFACE ( 3, 2, ( 
 ( #102339, #59358, #180637 ),
 ( #82769, #161080, #22868 ),
 ( #673, #58088, #1974 ),
 ( #181918, #43689, #137629 ) ),
 .UNSPECIFIED., .F., .F., .F. ) 
 B_SPLINE_SURFACE_WITH_KNOTS ( ( 4, 4 ),
 ( 3, 3 ),
 ( -3.469446951953614189E-18, 0.001979672783031543714 ),
 ( 0.000000000000000000, 1.000000000000000000 ),
 .UNSPECIFIED. ) 
 GEOMETRIC_REPRESENTATION_ITEM ( )  RATIONAL_B_SPLINE_SURFACE ( (
 ( 1.000000000000000000, 0.7103081912007699339, 1.000000000000000000),
 ( 1.000000000000000000, 0.7104998333558610879, 1.000000000000000000),
 ( 1.000000000000000000, 0.7107238315755344260, 1.000000000000000000),
 ( 1.000000000000000000, 0.7110073749539295163, 1.000000000000000000) ) ) 
 REPRESENTATION_ITEM ( '' )  SURFACE ( )  );
#74578 = ORIENTED_EDGE ( 'NONE', *, *, #206068, .F. ) ;
#74579 = DIRECTION ( 'NONE',  ( -0.000000000000000000, -0.9316174814283004757, -0.3634403228828502752 ) ) ;
#74580 = CARTESIAN_POINT ( 'NONE',  ( -21.05000000000000071, -12.41227409413852811, -164.6000000000000227 ) ) ;
#74581 = ORIENTED_EDGE ( 'NONE', *, *, #78318, .T. ) ;
#74583 = ORIENTED_EDGE ( 'NONE', *, *, #225704, .T. ) ;
#74582 = B_SPLINE_CURVE_WITH_KNOTS ( 'NONE', 3,
 ( #210943, #130109, #114410, #32336 ),
 .UNSPECIFIED., .F., .F.,
 ( 4, 4 ),
 ( 3.469446951953614189E-18, 0.0001058379652594699388 ),
 .UNSPECIFIED. ) ;
#74584 = DIRECTION ( 'NONE',  ( -0.5932847527679299127, 0.8049926720990051576, 6.366092712777055223E-16 ) ) ;
#74585 = CARTESIAN_POINT ( 'NONE',  ( -18.50000000000000000, 14.06640494040441247, -210.3712993791105532 ) ) ;
#74587 = VERTEX_POINT ( 'NONE', #27666 ) ;
#74586 = ORIENTED_EDGE ( 'NONE', *, *, #199354, .T. ) ;
#74588 = ORIENTED_EDGE ( 'NONE', *, *, #25286, .F. ) ;
#74589 = CARTESIAN_POINT ( 'NONE',  ( 21.05000000000000071, 65.27628289530409234, -61.85819391543678591 ) ) ;
#74590 = ORIENTED_EDGE ( 'NONE', *, *, #69272, .T. ) ;
#74591 = ORIENTED_EDGE ( 'NONE', *, *, #57533, .F. ) ;
#74592 = DIRECTION ( 'NONE',  ( 0.000000000000000000, -0.000000000000000000, -1.000000000000000000 ) ) ;
#74593 = ORIENTED_EDGE ( 'NONE', *, *, #97123, .T. ) ;
#74594 = DIRECTION ( 'NONE',  ( 0.000000000000000000, -0.1332476588733448597, 0.9910827722268067408 ) ) ;
#74595 = CARTESIAN_POINT ( 'NONE',  ( -21.05000000000000071, 68.20313450767837082, -227.8297066677462794 ) ) ;
#74596 = EDGE_LOOP ( 'NONE', ( #237130, #251550, #19463, #125877 ) ) ;
#74597 = ADVANCED_FACE ( 'NONE', ( #202410 ), #32849, .T. ) ;
#74598 = ORIENTED_EDGE ( 'NONE', *, *, #19975, .F. ) ;
#74599 = CIRCLE ( 'NONE', #16317, 0.1999999999999996503 ) ;
#74600 = CARTESIAN_POINT ( 'NONE',  ( -18.59999999999999787, 76.00000000001195133, -103.0231074845243171 ) ) ;
#74601 = AXIS2_PLACEMENT_3D ( 'NONE', #72021, #151577, #14625 ) ;
#74602 = CIRCLE ( 'NONE', #237059, 0.09999999999999939493 ) ;
#74603 = AXIS2_PLACEMENT_3D ( 'NONE', #131700, #108294, #88692 ) ;
#74604 = ORIENTED_EDGE ( 'NONE', *, *, #100048, .F. ) ;
#74605 =( BOUNDED_SURFACE ( )  B_SPLINE_SURFACE ( 3, 2, ( 
 ( #251532, #169485, #70371 ),
 ( #211132, #89885, #131590 ),
 ( #14238, #95027, #11667 ),
 ( #174629, #33826, #152470 ),
 ( #93747, #189006, #208586 ),
 ( #12956, #110740, #173342 ),
 ( #254090, #109446, #153780 ),
 ( #149897, #250257, #194157 ),
 ( #190301, #130299, #252812 ),
 ( #248992, #75498, #50745 ),
 ( #72941, #91187, #74227 ),
 ( #233288, #15525, #53340 ) ),
 .UNSPECIFIED., .F., .F., .F. ) 
 B_SPLINE_SURFACE_WITH_KNOTS ( ( 4, 2, 2, 2, 2, 4 ),
 ( 3, 3 ),
 ( 3.174653483277205090, 3.943930578431713574, 4.713207673586222057, 5.482484768740730985, 5.867123316317985449, 6.251761863895239912 ),
 ( 0.000000000000000000, 1.000000000000000000 ),
 .UNSPECIFIED. ) 
 GEOMETRIC_REPRESENTATION_ITEM ( )  RATIONAL_B_SPLINE_SURFACE ( (
 ( 1.000000000000000000, 0.8659465255642661008, 1.000000000000000000),
 ( 1.000000000000000000, 0.8648614068561133461, 1.000000000000000000),
 ( 1.000000000000000000, 0.8489031841225879171, 1.000000000000000000),
 ( 1.000000000000000000, 0.7927507630259206239, 1.000000000000000000),
 ( 1.000000000000000000, 0.7523013859064423547, 1.000000000000000000),
 ( 1.000000000000000000, 0.6616226951140901091, 1.000000000000000000),
 ( 1.000000000000000000, 0.6112214368715968016, 1.000000000000000000),
 ( 1.000000000000000000, 0.5507684314502028222, 1.000000000000000000),
 ( 1.000000000000000000, 0.5333267243212502784, 1.000000000000000000),
 ( 1.000000000000000000, 0.5084565446419482271, 1.000000000000000000),
 ( 1.000000000000000000, 0.5010722703496404140, 1.000000000000000000),
 ( 1.000000000000000000, 0.5001234037138357902, 1.000000000000000000) ) ) 
 REPRESENTATION_ITEM ( '' )  SURFACE ( )  );
#74606 = AXIS2_PLACEMENT_3D ( 'NONE', #133349, #79755, #135883 ) ;
#74607 = CARTESIAN_POINT ( 'NONE',  ( -18.39999999999999858, 85.50000000001189449, -95.99103808782457747 ) ) ;
#74608 = ORIENTED_EDGE ( 'NONE', *, *, #110334, .T. ) ;
#74609 = ORIENTED_EDGE ( 'NONE', *, *, #179627, .F. ) ;
#74610 = EDGE_CURVE ( 'NONE', #32909, #252850, #224536, .T. ) ;
#74611 = DIRECTION ( 'NONE',  ( -0.000000000000000000, -0.000000000000000000, 1.000000000000000000 ) ) ;
#74613 = ORIENTED_EDGE ( 'NONE', *, *, #144300, .F. ) ;
#74612 = FACE_OUTER_BOUND ( 'NONE', #178820, .T. ) ;
#74614 = DIRECTION ( 'NONE',  ( 0.000000000000000000, 6.982962677686267499E-15, -1.000000000000000000 ) ) ;
#74615 = FACE_OUTER_BOUND ( 'NONE', #6177, .T. ) ;
#74616 = CARTESIAN_POINT ( 'NONE',  ( -18.59999999999999787, 66.85000000001203091, -114.7731074845243739 ) ) ;
#74617 = DIRECTION ( 'NONE',  ( 0.000000000000000000, 0.2617529984165029577, 0.9651348961777157509 ) ) ;
#74618 = PLANE ( 'NONE',  #190489 ) ;
#74619 = EDGE_CURVE ( 'NONE', #102037, #41600, #48463, .T. ) ;
#74620 = DIRECTION ( 'NONE',  ( 1.000000000000000000, -0.000000000000000000, -0.000000000000000000 ) ) ;
#74622 = LINE ( 'NONE', #78420, #120475 ) ;
#74621 = VECTOR ( 'NONE', #138011, 1000.000000000000000 ) ;
#74624 = CARTESIAN_POINT ( 'NONE',  ( -21.07928932188134041, 0.09889514565439468108, 6.328516656393293083 ) ) ;
#74623 = CIRCLE ( 'NONE', #16342, 4.050000000000002487 ) ;
#74625 = DIRECTION ( 'NONE',  ( 1.000000000000000000, -2.952720810173289112E-16, -2.061873921506763405E-30 ) ) ;
#74626 = CIRCLE ( 'NONE', #253446, 0.1000000000000024342 ) ;
#74627 = DIRECTION ( 'NONE',  ( 2.978066053179067751E-16, -1.000000000000000000, -2.382452842543254201E-15 ) ) ;
#74628 = CARTESIAN_POINT ( 'NONE',  ( -20.85000000000000142, 87.75000000001247713, -172.9231074845242802 ) ) ;
#74629 = ADVANCED_FACE ( 'NONE', ( #204958 ), #64192, .T. ) ;
#74630 = ORIENTED_EDGE ( 'NONE', *, *, #187479, .F. ) ;
#74631 = AXIS2_PLACEMENT_3D ( 'NONE', #21089, #161880, #19793 ) ;
#74632 = EDGE_CURVE ( 'NONE', #215029, #224490, #53653, .T. ) ;
#74634 = ORIENTED_EDGE ( 'NONE', *, *, #252470, .F. ) ;
#74633 = EDGE_LOOP ( 'NONE', ( #82965, #6248, #83778 ) ) ;
#74635 = ORIENTED_EDGE ( 'NONE', *, *, #129149, .T. ) ;
#74636 = EDGE_CURVE ( 'NONE', #72890, #57467, #11982, .T. ) ;
#74637 = CARTESIAN_POINT ( 'NONE',  ( -21.08078803292166725, 0.07918598716886154909, -94.16698703556289729 ) ) ;
#74638 = PLANE ( 'NONE',  #215384 ) ;
#74639 = ADVANCED_FACE ( 'NONE', ( #147575 ), #7881, .F. ) ;
#74641 = CARTESIAN_POINT ( 'NONE',  ( -20.85000000000000142, 7.021664781911246322, -171.2335654018973230 ) ) ;
#74640 = DIRECTION ( 'NONE',  ( 1.000000000000000000, 0.000000000000000000, 0.000000000000000000 ) ) ;
#74642 = ORIENTED_EDGE ( 'NONE', *, *, #254482, .T. ) ;
#74643 = ORIENTED_EDGE ( 'NONE', *, *, #57716, .T. ) ;
#74644 =( LENGTH_UNIT ( ) NAMED_UNIT ( * ) SI_UNIT ( .MILLI., .METRE. ) );
#74645 = DIRECTION ( 'NONE',  ( 0.000000000000000000, -0.9654727137038715545, -0.2605042016806676242 ) ) ;
#74646 = EDGE_CURVE ( 'NONE', #191070, #44201, #232270, .T. ) ;
#74647 = DIRECTION ( 'NONE',  ( 0.000000000000000000, 0.9908441862701605762, -0.1350103645451835310 ) ) ;
#74648 = FACE_OUTER_BOUND ( 'NONE', #250336, .T. ) ;
#74649 = ORIENTED_EDGE ( 'NONE', *, *, #229977, .T. ) ;
#74650 = EDGE_LOOP ( 'NONE', ( #129590, #165452, #87926, #176343 ) ) ;
#74651 = CIRCLE ( 'NONE', #199532, 0.1000000000000017958 ) ;
#74652 = DIRECTION ( 'NONE',  ( -0.000000000000000000, -0.000000000000000000, -1.000000000000000000 ) ) ;
#74653 = SPHERICAL_SURFACE ( 'NONE', #168044, 0.1000000000000000056 ) ;
#74654 = ORIENTED_EDGE ( 'NONE', *, *, #52119, .F. ) ;
#74655 = CARTESIAN_POINT ( 'NONE',  ( 21.00000000000000000, 9.749999999999998224, -12.35000000000000320 ) ) ;
#74657 = ORIENTED_EDGE ( 'NONE', *, *, #168579, .T. ) ;
#74656 = CARTESIAN_POINT ( 'NONE',  ( -22.84999999999999787, 0.000000000000000000, 0.000000000000000000 ) ) ;
#74658 = AXIS2_PLACEMENT_3D ( 'NONE', #208012, #231424, #168913 ) ;
#74659 = SPHERICAL_SURFACE ( 'NONE', #232019, 0.1000000000000000056 ) ;
#74660 = DIRECTION ( 'NONE',  ( 1.000000000000000000, -0.000000000000000000, 0.000000000000000000 ) ) ;
#74661 = DIRECTION ( 'NONE',  ( 2.715809747126116508E-16, -1.000000000000000000, -2.172647797700893206E-15 ) ) ;
#74662 = EDGE_LOOP ( 'NONE', ( #78626, #243738, #149735, #62019 ) ) ;
#74663 = CARTESIAN_POINT ( 'NONE',  ( 18.41356215285960474, 46.96039402156211651, -255.3459641718773128 ) ) ;
#74664 = DIRECTION ( 'NONE',  ( 1.000000000000000000, 0.000000000000000000, 0.000000000000000000 ) ) ;
#74666 = ADVANCED_FACE ( 'NONE', ( #113580 ), #116215, .T. ) ;
#74665 = DIRECTION ( 'NONE',  ( 0.000000000000000000, 0.9126074666063771490, 0.4088369013363281623 ) ) ;
#74667 = LINE ( 'NONE', #177609, #86696 ) ;
#74668 = DIRECTION ( 'NONE',  ( -1.000000000000000000, -0.000000000000000000, -0.000000000000000000 ) ) ;
#74669 = CARTESIAN_POINT ( 'NONE',  ( -16.97683809663752186, 66.05000000001233218, -160.7731074845244166 ) ) ;
#74670 = AXIS2_PLACEMENT_3D ( 'NONE', #89383, #230188, #48981 ) ;
#74671 = CARTESIAN_POINT ( 'NONE',  ( -21.05000000000000071, 4.617781596423511381, -222.2029736859691980 ) ) ;
#74672 = DIRECTION ( 'NONE',  ( -1.000000000000000000, 0.000000000000000000, -0.000000000000000000 ) ) ;
#74673 = CIRCLE ( 'NONE', #82960, 0.1000000000000033362 ) ;
#74674 = EDGE_LOOP ( 'NONE', ( #213041, #147718, #107570, #120824 ) ) ;
#74675 = VECTOR ( 'NONE', #159414, 1000.000000000000000 ) ;
#74676 = VERTEX_POINT ( 'NONE', #169744 ) ;
#74677 = EDGE_CURVE ( 'NONE', #189423, #94999, #62033, .T. ) ;
#74678 = DIRECTION ( 'NONE',  ( 1.000000000000000000, 0.000000000000000000, 0.000000000000000000 ) ) ;
#74679 = ORIENTED_EDGE ( 'NONE', *, *, #257703, .F. ) ;
#74680 = FACE_OUTER_BOUND ( 'NONE', #245735, .T. ) ;
#74681 = AXIS2_PLACEMENT_3D ( 'NONE', #146430, #246827, #132026 ) ;
#74682 = AXIS2_PLACEMENT_3D ( 'NONE', #182839, #175450, #83666 ) ;
#74683 = VERTEX_POINT ( 'NONE', #250516 ) ;
#74684 = ORIENTED_EDGE ( 'NONE', *, *, #100841, .T. ) ;
#74685 = CARTESIAN_POINT ( 'NONE',  ( 22.14074124539698829, 7.390077851054901892, -66.90094710415597490 ) ) ;
#74686 = ORIENTED_EDGE ( 'NONE', *, *, #11538, .T. ) ;
#74687 = ADVANCED_FACE ( 'NONE', ( #11937 ), #171042, .T. ) ;
#74688 = CIRCLE ( 'NONE', #24799, 11.80000000000000426 ) ;
#74689 = PLANE ( 'NONE',  #230384 ) ;
#74690 = AXIS2_PLACEMENT_3D ( 'NONE', #207176, #31134, #48082 ) ;
#74691 = AXIS2_PLACEMENT_3D ( 'NONE', #227269, #31680, #107321 ) ;
#74692 = DIRECTION ( 'NONE',  ( 1.000000000000000000, -7.304098846218134667E-16, -4.217023435051626718E-16 ) ) ;
#74693 = TOROIDAL_SURFACE ( 'NONE', #116359, 0.2000000000000000111, 0.1000000000000000056 ) ;
#74694 = FACE_OUTER_BOUND ( 'NONE', #228907, .T. ) ;
#74695 = DIRECTION ( 'NONE',  ( 0.000000000000000000, 0.000000000000000000, 1.000000000000000000 ) ) ;
#74697 = ORIENTED_EDGE ( 'NONE', *, *, #108625, .F. ) ;
#74696 = CARTESIAN_POINT ( 'NONE',  ( 20.94999999999999929, 71.00000000001199396, -115.4283735034374274 ) ) ;
#74699 = DIRECTION ( 'NONE',  ( 1.000000000000000000, -0.000000000000000000, -0.000000000000000000 ) ) ;
#74698 = DIRECTION ( 'NONE',  ( -1.000000000000000000, 7.304098846218134667E-16, 5.100424963727256530E-30 ) ) ;
#74700 = AXIS2_PLACEMENT_3D ( 'NONE', #118860, #40634, #80980 ) ;
#74701 = DIRECTION ( 'NONE',  ( -1.000000000000000000, 0.000000000000000000, 0.000000000000000000 ) ) ;
#74702 = EDGE_CURVE ( 'NONE', #88400, #190257, #144614, .T. ) ;
#74703 = CARTESIAN_POINT ( 'NONE',  ( -21.05000000000000071, 1.115600667400684642E-11, -100.5000000000000284 ) ) ;
#74704 = DIRECTION ( 'NONE',  ( -1.000000000000000000, 0.000000000000000000, 0.000000000000000000 ) ) ;
#74705 = CARTESIAN_POINT ( 'NONE',  ( -23.25000000000000000, -1.835859311432481045, -212.5044391687984842 ) ) ;
#74706 = EDGE_LOOP ( 'NONE', ( #146409, #253012, #128518 ) ) ;
#74707 = EDGE_CURVE ( 'NONE', #168971, #38731, #16259, .T. ) ;
#74708 = DIRECTION ( 'NONE',  ( 0.000000000000000000, 1.000000000000000000, 1.265107689135680095E-16 ) ) ;
#74709 = EDGE_CURVE ( 'NONE', #26749, #19568, #173610, .T. ) ;
#74710 = VERTEX_POINT ( 'NONE', #112311 ) ;
#74711 = CARTESIAN_POINT ( 'NONE',  ( 18.59999999999999076, 64.35000000001201670, -114.7731074845243882 ) ) ;
#74712 = ADVANCED_FACE ( 'NONE', ( #90144 ), #94003, .F. ) ;
#74714 = ORIENTED_EDGE ( 'NONE', *, *, #195472, .T. ) ;
#74713 = AXIS2_PLACEMENT_3D ( 'NONE', #197079, #181407, #257016 ) ;
#74715 = CARTESIAN_POINT ( 'NONE',  ( 18.52928932304301668, 54.97610475762002835, -230.0816435235718131 ) ) ;
#74716 = EDGE_CURVE ( 'NONE', #137338, #226022, #15798, .T. ) ;
#74717 = DIRECTION ( 'NONE',  ( 1.000000000000000000, 0.000000000000000000, 0.000000000000000000 ) ) ;
#74718 = LINE ( 'NONE', #29172, #28366 ) ;
#74719 = EDGE_LOOP ( 'NONE', ( #49268, #190015, #117900, #238871 ) ) ;
#74720 = VERTEX_POINT ( 'NONE', #229685 ) ;
#74721 = CIRCLE ( 'NONE', #16435, 0.1000000000000002554 ) ;
#74722 = CARTESIAN_POINT ( 'NONE',  ( -21.05000000000000071, 56.06656052939784729, -228.0911609752645290 ) ) ;
#74723 = DIRECTION ( 'NONE',  ( 1.000000000000000000, 0.000000000000000000, 0.000000000000000000 ) ) ;
#74724 = DIRECTION ( 'NONE',  ( 1.000000000000000000, 0.000000000000000000, 0.000000000000000000 ) ) ;
#74725 = CIRCLE ( 'NONE', #20537, 3.899999999999987033 ) ;
#74727 = CARTESIAN_POINT ( 'NONE',  ( 21.05000000000000071, 76.00000000001169553, -67.52310748452430289 ) ) ;
#74726 = CARTESIAN_POINT ( 'NONE',  ( 23.14999999999998437, 76.00000000001210765, -132.4731074845242915 ) ) ;
#74728 = CARTESIAN_POINT ( 'NONE',  ( -23.15000000000000213, 11.65000000001115588, -160.4851942293460638 ) ) ;
#74729 = CARTESIAN_POINT ( 'NONE',  ( 12.42718393586866732, 9.370655051134640701, -51.02582325598088175 ) ) ;
#74730 = CARTESIAN_POINT ( 'NONE',  ( -16.94107738177414291, 30.32481141862675145, -234.7976376674202186 ) ) ;
#74731 = ORIENTED_EDGE ( 'NONE', *, *, #202364, .T. ) ;
#74732 = CARTESIAN_POINT ( 'NONE',  ( -23.15000000000000213, 87.48912529308798014, -106.1231074845242262 ) ) ;
#74733 = AXIS2_PLACEMENT_3D ( 'NONE', #130742, #173782, #189444 ) ;
#74734 = ADVANCED_FACE ( 'NONE', ( #74498 ), #91457, .F. ) ;
#74736 = EDGE_LOOP ( 'NONE', ( #213957, #174284, #121007, #37445 ) ) ;
#74735 = DIRECTION ( 'NONE',  ( 0.000000000000000000, 0.8814952561688476074, -0.4721928772777262417 ) ) ;
#74737 = DIRECTION ( 'NONE',  ( -0.000000000000000000, -0.9770955615653316162, -0.2128009952263604232 ) ) ;
#74739 = CARTESIAN_POINT ( 'NONE',  ( 21.87500000000000355, 66.25000000001179501, -81.87310748452438247 ) ) ;
#74738 = CARTESIAN_POINT ( 'NONE',  ( -18.59999999999999787, 51.24799949642838470, -230.1402408152235637 ) ) ;
#74740 = EDGE_CURVE ( 'NONE', #52116, #68194, #37104, .T. ) ;
#74742 = ORIENTED_EDGE ( 'NONE', *, *, #140601, .T. ) ;
#74741 = DIRECTION ( 'NONE',  ( 0.000000000000000000, 0.000000000000000000, -1.000000000000000000 ) ) ;
#74743 = DIRECTION ( 'NONE',  ( 0.000000000000000000, 0.000000000000000000, -1.000000000000000000 ) ) ;
#74745 = ADVANCED_FACE ( 'NONE', ( #190573 ), #172322, .F. ) ;
#74744 = CARTESIAN_POINT ( 'NONE',  ( 0.000000000000000000, 1.350000000000000089, 16.60000000000000142 ) ) ;
#74746 = CARTESIAN_POINT ( 'NONE',  ( -23.15000000000000213, 1.115600667400684642E-11, -67.00000000000000000 ) ) ;
#74747 = DIRECTION ( 'NONE',  ( 0.000000000000000000, -0.6728971962616792091, 0.7397360091702790408 ) ) ;
#74748 = DIRECTION ( 'NONE',  ( -1.000000000000000000, -0.000000000000000000, -0.000000000000000000 ) ) ;
#74749 = ORIENTED_EDGE ( 'NONE', *, *, #124949, .T. ) ;
#74750 = CYLINDRICAL_SURFACE ( 'NONE', #105536, 0.09999999999999939493 ) ;
#74752 = VERTEX_POINT ( 'NONE', #134401 ) ;
#74751 = AXIS2_PLACEMENT_3D ( 'NONE', #108046, #71505, #151025 ) ;
#74753 = TOROIDAL_SURFACE ( 'NONE', #153872, 0.6000000000000004219, 0.1000000000000000056 ) ;
#74754 = DIRECTION ( 'NONE',  ( -1.000000000000000000, -0.000000000000000000, -0.000000000000000000 ) ) ;
#74755 = VERTEX_POINT ( 'NONE', #130565 ) ;
#74756 = DIRECTION ( 'NONE',  ( -1.000000000000000000, -2.952720810173289112E-16, 0.000000000000000000 ) ) ;
#74757 = B_SPLINE_CURVE_WITH_KNOTS ( 'NONE', 3,
 ( #46174, #103563, #26644, #243094, #205239, #142698, #86563, #83971, #245670, #67034, #47446, #127005, #206542, #27941, #107439, #8355 ),
 .UNSPECIFIED., .F., .F.,
 ( 4, 3, 3, 3, 3, 4 ),
 ( 0.000000000000000000, 3.357088238233600668E-05, 6.714213034886770139E-05, 0.0001007408646120938085, 0.0001343627955914254344, 0.0001573956632896058639 ),
 .UNSPECIFIED. ) ;
#74758 = AXIS2_PLACEMENT_3D ( 'NONE', #21257, #40819, #62918 ) ;
#74759 = ORIENTED_EDGE ( 'NONE', *, *, #189420, .T. ) ;
#74760 = CARTESIAN_POINT ( 'NONE',  ( 23.15000000000000213, 85.00000000001251976, -179.9170766071767389 ) ) ;
#74761 = DIRECTION ( 'NONE',  ( 0.000000000000000000, -1.000000000000000000, 0.000000000000000000 ) ) ;
#74762 = DIRECTION ( 'NONE',  ( 1.000000000000000000, 0.000000000000000000, 0.000000000000000000 ) ) ;
#74763 = VERTEX_POINT ( 'NONE', #213969 ) ;
#74764 = CARTESIAN_POINT ( 'NONE',  ( -16.87683809663752754, 9.865889849332413419, -13.26742680706974831 ) ) ;
#74765 = ADVANCED_FACE ( 'NONE', ( #35372 ), #170225, .T. ) ;
#74766 = CARTESIAN_POINT ( 'NONE',  ( -20.64999999999999858, 71.65000000001259650, -191.2731074845243882 ) ) ;
#74767 = CARTESIAN_POINT ( 'NONE',  ( 23.14999999999999503, 64.25000000001172396, -81.27310748452440237 ) ) ;
#74769 = VECTOR ( 'NONE', #174551, 1000.000000000000000 ) ;
#74768 = DIRECTION ( 'NONE',  ( -1.000000000000000000, 0.000000000000000000, 0.000000000000000000 ) ) ;
#74770 = CARTESIAN_POINT ( 'NONE',  ( -16.89268316805465986, 66.04827818676982076, -115.6673550059788340 ) ) ;
#74771 = EDGE_CURVE ( 'NONE', #38549, #85926, #194930, .T. ) ;
#74772 = EDGE_LOOP ( 'NONE', ( #26892, #192238, #74513, #33026, #152715, #109847, #54922, #92387, #120137, #257846, #35471, #175950, #157568, #176095, #7105, #254893, #68046, #174929 ) ) ;
#74773 = CARTESIAN_POINT ( 'NONE',  ( -18.39999999999999858, 85.50000000001212186, -129.6009576351939074 ) ) ;
#74774 = ORIENTED_EDGE ( 'NONE', *, *, #232288, .T. ) ;
#74776 = ORIENTED_EDGE ( 'NONE', *, *, #32853, .T. ) ;
#74775 = DIRECTION ( 'NONE',  ( 0.000000000000000000, 1.000000000000000000, 0.000000000000000000 ) ) ;
#74777 = EDGE_LOOP ( 'NONE', ( #163079, #90821, #210916, #200036, #124560 ) ) ;
#74778 = CARTESIAN_POINT ( 'NONE',  ( -18.59999999999999787, 68.97833521811203639, -132.6895420826271277 ) ) ;
#74779 = DIRECTION ( 'NONE',  ( -0.4999999999999799050, -6.047423072554995242E-15, 0.8660254037844502539 ) ) ;
#74780 = CARTESIAN_POINT ( 'NONE',  ( 22.59999999999999432, 11.74987124437650721, 0.06542959101367906705 ) ) ;
#74781 = DIRECTION ( 'NONE',  ( 0.000000000000000000, 0.9908441862701596881, 0.1350103645451904977 ) ) ;
#74782 = ORIENTED_EDGE ( 'NONE', *, *, #22685, .F. ) ;
#74783 = EDGE_CURVE ( 'NONE', #62912, #118476, #41772, .T. ) ;
#74784 = CARTESIAN_POINT ( 'NONE',  ( -16.77683809663752257, 9.945835743204145984, -12.66394901910421034 ) ) ;
#74785 = CARTESIAN_POINT ( 'NONE',  ( 23.40000000000005187, 77.16254490893143725, -44.02310748452479316 ) ) ;
#74786 = VERTEX_POINT ( 'NONE', #196955 ) ;
#74787 = EDGE_CURVE ( 'NONE', #65513, #84546, #237000, .T. ) ;
#74789 = ORIENTED_EDGE ( 'NONE', *, *, #213937, .F. ) ;
#74788 = CARTESIAN_POINT ( 'NONE',  ( 18.59999999999999076, 53.41483507351092896, -234.9770603882373337 ) ) ;
#74790 = PLANE ( 'NONE',  #223499 ) ;
#74791 = DIRECTION ( 'NONE',  ( -1.000000000000000000, -2.952720810173289112E-16, 0.000000000000000000 ) ) ;
#74792 = CIRCLE ( 'NONE', #145635, 0.1000000000000006301 ) ;
#74793 = VECTOR ( 'NONE', #11758, 1000.000000000000227 ) ;
#74794 = ADVANCED_FACE ( 'NONE', ( #139544 ), #176147, .F. ) ;
#74795 = CIRCLE ( 'NONE', #91676, 0.2000000000000057288 ) ;
#74797 = AXIS2_PLACEMENT_3D ( 'NONE', #39037, #55986, #135532 ) ;
#74796 = DIRECTION ( 'NONE',  ( -0.000000000000000000, -6.982962677686266711E-15, 1.000000000000000000 ) ) ;
#74798 = ORIENTED_EDGE ( 'NONE', *, *, #49180, .F. ) ;
#74799 = EDGE_LOOP ( 'NONE', ( #101655, #129389, #223077, #233829 ) ) ;
#74800 = ADVANCED_FACE ( 'NONE', ( #39206 ), #232920, .F. ) ;
#74801 = AXIS2_PLACEMENT_3D ( 'NONE', #59893, #45490, #82012 ) ;
#74802 = CARTESIAN_POINT ( 'NONE',  ( -20.94999999999999929, 69.06797323185276127, -247.4100621602722470 ) ) ;
#74804 = EDGE_CURVE ( 'NONE', #24375, #195865, #83014, .T. ) ;
#74803 = ORIENTED_EDGE ( 'NONE', *, *, #85253, .T. ) ;
#74805 = DIRECTION ( 'NONE',  ( -0.000000000000000000, -1.000000000000000000, -6.982962677686266711E-15 ) ) ;
#74806 = CARTESIAN_POINT ( 'NONE',  ( 13.54577453029515510, 66.54939790392303678, -51.07921152142773735 ) ) ;
#74807 = DIRECTION ( 'NONE',  ( 0.7071067811865463515, 0.7071067811865487940, 7.587431340288849180E-16 ) ) ;
#74808 = TOROIDAL_SURFACE ( 'NONE', #29015, 0.2000000000000000111, 0.1000000000000000056 ) ;
#74810 = ADVANCED_FACE ( 'NONE', ( #97834 ), #177441, .F. ) ;
#74809 = CIRCLE ( 'NONE', #74631, 4.099999999999992539 ) ;
#74811 = EDGE_CURVE ( 'NONE', #154736, #127278, #101682, .T. ) ;
#74812 = ORIENTED_EDGE ( 'NONE', *, *, #155310, .F. ) ;
#74813 = CARTESIAN_POINT ( 'NONE',  ( 21.05000000000000071, 1.835341550235569663, -145.5551512925629822 ) ) ;
#74814 = VERTEX_POINT ( 'NONE', #120033 ) ;
#74815 = DIRECTION ( 'NONE',  ( 1.000000000000000000, 0.000000000000000000, 0.000000000000000000 ) ) ;
#74816 = CARTESIAN_POINT ( 'NONE',  ( -16.87036670365549895, 9.989418819312803066, -79.52043988269799968 ) ) ;
#74818 = EDGE_LOOP ( 'NONE', ( #90806, #252641, #197297, #87940 ) ) ;
#74817 = CARTESIAN_POINT ( 'NONE',  ( 18.59999999999999076, 11.65000000001115943, -91.75000000000005684 ) ) ;
#74819 = CARTESIAN_POINT ( 'NONE',  ( -21.05000000000000071, -1.162701749938009677, -8.099999999999999645 ) ) ;
#74820 = CARTESIAN_POINT ( 'NONE',  ( -18.59999999999999787, 76.00000000001244871, -170.0231074845243597 ) ) ;
#74821 = DIRECTION ( 'NONE',  ( 0.000000000000000000, -0.9126074666063844765, -0.4088369013363114535 ) ) ;
#74822 = DIRECTION ( 'NONE',  ( -1.000000000000000000, -1.594516344651357984E-15, 4.324467345337419894E-16 ) ) ;
#74823 = CARTESIAN_POINT ( 'NONE',  ( 21.13422380239050824, 6.493326514816692985, -33.50000000000000000 ) ) ;
#74824 = DIRECTION ( 'NONE',  ( 0.000000000000000000, 0.2128009952263601456, -0.9770955615653316162 ) ) ;
#74826 = EDGE_CURVE ( 'NONE', #197596, #188850, #174691, .T. ) ;
#74825 = CARTESIAN_POINT ( 'NONE',  ( -23.25000000000000355, 70.35000000001187459, -90.37310748452433984 ) ) ;
#74828 = VERTEX_POINT ( 'NONE', #36646 ) ;
#74827 = DIRECTION ( 'NONE',  ( 1.000000000000000000, 7.136802563874199107E-16, 1.554319503706929991E-16 ) ) ;
#74829 = EDGE_CURVE ( 'NONE', #61363, #11718, #74721, .T. ) ;
#74830 = DIRECTION ( 'NONE',  ( 1.000000000000000000, 0.000000000000000000, 0.000000000000000000 ) ) ;
#74831 = AXIS2_PLACEMENT_3D ( 'NONE', #192008, #13354, #129439 ) ;
#74833 = ADVANCED_FACE ( 'NONE', ( #40503 ), #132960, .F. ) ;
#74832 = CARTESIAN_POINT ( 'NONE',  ( -21.05000000000000071, 46.50671693017397246, -243.2369495081682942 ) ) ;
#74834 = DIRECTION ( 'NONE',  ( 1.000000000000000000, 0.000000000000000000, 0.000000000000000000 ) ) ;
#74835 = ORIENTED_EDGE ( 'NONE', *, *, #115990, .F. ) ;
#74836 = CARTESIAN_POINT ( 'NONE',  ( 18.69999999999999929, 4.513204987021264714, 22.10000000000000142 ) ) ;
#74837 = DIRECTION ( 'NONE',  ( 0.7071067811865474617, 0.6909108974501236844, 0.1504730267678055788 ) ) ;
#74838 = EDGE_CURVE ( 'NONE', #102935, #200910, #141312, .T. ) ;
#74839 = ORIENTED_EDGE ( 'NONE', *, *, #205455, .T. ) ;
#74840 = CIRCLE ( 'NONE', #228933, 0.1999999999999987899 ) ;
#74841 = CARTESIAN_POINT ( 'NONE',  ( -23.25000000000000000, -1.851617760457748618, -179.1031897196036766 ) ) ;
#74842 = AXIS2_PLACEMENT_3D ( 'NONE', #144949, #224500, #127981 ) ;
#74843 = FACE_OUTER_BOUND ( 'NONE', #103609, .T. ) ;
#74844 = ORIENTED_EDGE ( 'NONE', *, *, #214250, .F. ) ;
#74845 = DIRECTION ( 'NONE',  ( 0.000000000000000000, -0.9651348961777157509, 0.2617529984165031243 ) ) ;
#74846 = CIRCLE ( 'NONE', #175361, 0.09999999999998898659 ) ;
#74847 = VERTEX_POINT ( 'NONE', #159157 ) ;
#74848 = EDGE_CURVE ( 'NONE', #39830, #237838, #117335, .T. ) ;
#74850 = ORIENTED_EDGE ( 'NONE', *, *, #200035, .T. ) ;
#74849 = CARTESIAN_POINT ( 'NONE',  ( 18.52928932188133970, 65.72071067813013201, -44.77310748452439526 ) ) ;
#74851 = CIRCLE ( 'NONE', #116518, 0.1000000000000028644 ) ;
#74852 = AXIS2_PLACEMENT_3D ( 'NONE', #125415, #210092, #31472 ) ;
#74853 = CARTESIAN_POINT ( 'NONE',  ( 21.14999999999999858, 6.649999999999999467, -12.35000000000000142 ) ) ;
#74854 = ORIENTED_EDGE ( 'NONE', *, *, #129599, .T. ) ;
#74855 = CARTESIAN_POINT ( 'NONE',  ( 23.14999999999999858, 64.35000000001146248, -43.03791325517834565 ) ) ;
#74856 = ORIENTED_EDGE ( 'NONE', *, *, #150368, .F. ) ;
#74858 = ORIENTED_EDGE ( 'NONE', *, *, #161579, .T. ) ;
#74857 = ORIENTED_EDGE ( 'NONE', *, *, #155728, .F. ) ;
#74859 = DIRECTION ( 'NONE',  ( 0.000000000000000000, 0.000000000000000000, 1.000000000000000000 ) ) ;
#74861 = ORIENTED_EDGE ( 'NONE', *, *, #189455, .T. ) ;
#74860 = DIRECTION ( 'NONE',  ( 2.952720810173289112E-16, -1.000000000000000000, 0.000000000000000000 ) ) ;
#74862 = CYLINDRICAL_SURFACE ( 'NONE', #52364, 0.09999999999999939493 ) ;
#74863 = VERTEX_POINT ( 'NONE', #102984 ) ;
#74864 = AXIS2_PLACEMENT_3D ( 'NONE', #86794, #205467, #124669 ) ;
#74865 = VECTOR ( 'NONE', #76628, 1000.000000000000114 ) ;
#74866 = AXIS2_PLACEMENT_3D ( 'NONE', #138422, #194605, #173784 ) ;
#74867 = AXIS2_PLACEMENT_3D ( 'NONE', #256363, #238136, #36119 ) ;
#74868 = TOROIDAL_SURFACE ( 'NONE', #95666, 0.2000000000000000111, 0.1000000000000000056 ) ;
#74869 = VERTEX_POINT ( 'NONE', #85974 ) ;
#74871 = AXIS2_PLACEMENT_3D ( 'NONE', #81607, #7228, #226263 ) ;
#74870 = LINE ( 'NONE', #176518, #41224 ) ;
#74872 = FACE_OUTER_BOUND ( 'NONE', #40400, .T. ) ;
#74873 = DIRECTION ( 'NONE',  ( -0.000000000000000000, -0.9876197685951290106, 0.1568667991644625281 ) ) ;
#74874 = ORIENTED_EDGE ( 'NONE', *, *, #194208, .F. ) ;
#74875 = DIRECTION ( 'NONE',  ( 0.000000000000000000, -1.776356839400188145E-15, 1.000000000000000000 ) ) ;
#74876 = CARTESIAN_POINT ( 'NONE',  ( -18.45037301276668984, -9.490200447530813932, -74.01267413641436121 ) ) ;
#74877 = CARTESIAN_POINT ( 'NONE',  ( 18.59999999999999076, 1.835341550235567887, -112.1551512925630192 ) ) ;
#74878 = VERTEX_POINT ( 'NONE', #48156 ) ;
#74879 = CARTESIAN_POINT ( 'NONE',  ( -22.39999999999999858, 59.71212129423881976, -233.8158665866020272 ) ) ;
#74880 = FACE_OUTER_BOUND ( 'NONE', #175022, .T. ) ;
#74881 = CARTESIAN_POINT ( 'NONE',  ( -18.39999999999999858, 11.47316190336247388, -9.325946066807970780 ) ) ;
#74882 = ORIENTED_EDGE ( 'NONE', *, *, #249290, .T. ) ;
#74883 = DIRECTION ( 'NONE',  ( 0.000000000000000000, -6.467318590049456648E-15, 1.000000000000000000 ) ) ;
#74884 = EDGE_LOOP ( 'NONE', ( #93047, #103600, #129647, #117540 ) ) ;
#74885 = MECHANICAL_DESIGN_GEOMETRIC_PRESENTATION_REPRESENTATION (  '', ( #178941 ), #20700 ) ;
#74886 = VERTEX_POINT ( 'NONE', #46862 ) ;
#74887 = CARTESIAN_POINT ( 'NONE',  ( -14.11697426661281085, 24.81705829073095160, -232.4789712399791028 ) ) ;
#74888 = ORIENTED_EDGE ( 'NONE', *, *, #68529, .T. ) ;
#74889 = ORIENTED_EDGE ( 'NONE', *, *, #114145, .F. ) ;
#74890 = DIRECTION ( 'NONE',  ( -1.000000000000000000, -2.952720810173289112E-16, 0.000000000000000000 ) ) ;
#74891 = DIRECTION ( 'NONE',  ( 0.000000000000000000, 0.000000000000000000, 1.000000000000000000 ) ) ;
#74892 = VERTEX_POINT ( 'NONE', #165558 ) ;
#74893 = EDGE_LOOP ( 'NONE', ( #22245, #23084, #174903, #252406 ) ) ;
#74894 = DIRECTION ( 'NONE',  ( 1.000000000000000000, 0.000000000000000000, 0.000000000000000000 ) ) ;
#74895 = SURFACE_SIDE_STYLE ('',( #248365 ) ) ;
#74896 = TOROIDAL_SURFACE ( 'NONE', #66492, 0.2000000000000000111, 0.1000000000000000056 ) ;
#74897 = VERTEX_POINT ( 'NONE', #123862 ) ;
#74898 = ADVANCED_FACE ( 'NONE', ( #245080 ), #156095, .F. ) ;
#74899 = VECTOR ( 'NONE', #174727, 1000.000000000000000 ) ;
#74900 = VERTEX_POINT ( 'NONE', #5153 ) ;
#74901 = CIRCLE ( 'NONE', #241472, 0.09999999999999939493 ) ;
#74902 = DIRECTION ( 'NONE',  ( 0.000000000000000000, -0.4999999999999949485, 0.8660254037844415942 ) ) ;
#74903 = DIRECTION ( 'NONE',  ( 0.000000000000000000, 0.000000000000000000, -1.000000000000000000 ) ) ;
#74904 = CARTESIAN_POINT ( 'NONE',  ( -20.64999999999999858, 85.50000000001251976, -179.9170766071767389 ) ) ;
#74905 = DIRECTION ( 'NONE',  ( -1.000000000000000000, -0.000000000000000000, -0.000000000000000000 ) ) ;
#74906 = CARTESIAN_POINT ( 'NONE',  ( 18.49999999999999289, 70.37092869010230345, -198.1237041667535550 ) ) ;
#74908 = ADVANCED_FACE ( 'NONE', ( #24783 ), #83406, .F. ) ;
#74907 = AXIS2_PLACEMENT_3D ( 'NONE', #116710, #175431, #155865 ) ;
#74909 = CARTESIAN_POINT ( 'NONE',  ( -18.39999999999999858, -9.499999999988849808, -174.5320693966996259 ) ) ;
#74910 = DIRECTION ( 'NONE',  ( -1.000000000000000000, 0.000000000000000000, 0.000000000000000000 ) ) ;
#74911 = AXIS2_PLACEMENT_3D ( 'NONE', #91228, #131623, #114630 ) ;
#74913 = CARTESIAN_POINT ( 'NONE',  ( 21.05000000000000071, 1.115623935689868526E-11, -199.0999999999999375 ) ) ;
#74912 = CARTESIAN_POINT ( 'NONE',  ( 21.07928932188134397, 75.90110485435707233, -75.85162414092303607 ) ) ;
#74914 = DIRECTION ( 'NONE',  ( -1.000000000000000000, -0.000000000000000000, -0.000000000000000000 ) ) ;
#74915 = CARTESIAN_POINT ( 'NONE',  ( -16.80621392010911208, 23.00928570187805633, -230.9606318461273702 ) ) ;
#74916 = CARTESIAN_POINT ( 'NONE',  ( -21.05000000000000071, 1.835341550235567887, -145.5551512925629822 ) ) ;
#74917 = CARTESIAN_POINT ( 'NONE',  ( -20.94999999999999929, 87.65000000001172964, -72.52310748452423184 ) ) ;
#74918 = AXIS2_PLACEMENT_3D ( 'NONE', #193571, #16238, #137423 ) ;
#74919 =( BOUNDED_CURVE ( )  B_SPLINE_CURVE ( 3, ( #126584, #209983, #206121, #151301 ),
 .UNSPECIFIED., .F., .T. ) 
 B_SPLINE_CURVE_WITH_KNOTS ( ( 4, 4 ),
 ( 1.570796326794899223, 3.141592653589871276 ),
 .UNSPECIFIED. ) 
 CURVE ( )  GEOMETRIC_REPRESENTATION_ITEM ( )  RATIONAL_B_SPLINE_CURVE ( ( 1.000000000000000000, 0.8047378541243471739, 0.8047378541243471739, 1.000000000000000000 ) ) 
 REPRESENTATION_ITEM ( '' )  );
#74920 = ORIENTED_EDGE ( 'NONE', *, *, #20023, .F. ) ;
#74921 = EDGE_CURVE ( 'NONE', #150529, #60954, #249659, .T. ) ;
#74923 = ORIENTED_EDGE ( 'NONE', *, *, #118543, .T. ) ;
#74922 = DIRECTION ( 'NONE',  ( 0.000000000000000000, -0.9126074666063770380, -0.4088369013363281068 ) ) ;
#74924 = EDGE_CURVE ( 'NONE', #255894, #87561, #178778, .T. ) ;
#74925 = FACE_OUTER_BOUND ( 'NONE', #110020, .T. ) ;
#74926 = EDGE_CURVE ( 'NONE', #98560, #222722, #166295, .T. ) ;
#74927 = FACE_OUTER_BOUND ( 'NONE', #55886, .T. ) ;
#74928 = ORIENTED_EDGE ( 'NONE', *, *, #94074, .T. ) ;
#74929 = PRESENTATION_STYLE_ASSIGNMENT (( #73645 ) ) ;
#74931 = FACE_OUTER_BOUND ( 'NONE', #174638, .T. ) ;
#74930 = CIRCLE ( 'NONE', #16663, 6.258578643762696458 ) ;
#74932 = ADVANCED_FACE ( 'NONE', ( #84680 ), #6462, .F. ) ;
#74933 = AXIS2_PLACEMENT_3D ( 'NONE', #188292, #9662, #12256 ) ;
#74934 = DIRECTION ( 'NONE',  ( -1.000000000000000000, 0.000000000000000000, 0.000000000000000000 ) ) ;
#74935 = VERTEX_POINT ( 'NONE', #242510 ) ;
#74936 = DIRECTION ( 'NONE',  ( 0.000000000000000000, 0.000000000000000000, -1.000000000000000000 ) ) ;
#74937 = DIRECTION ( 'NONE',  ( 2.259780016855445309E-14, 0.9875055080513753802, -0.1575844902526748192 ) ) ;
#74938 = EDGE_CURVE ( 'NONE', #138502, #90335, #62211, .T. ) ;
#74939 = CARTESIAN_POINT ( 'NONE',  ( -20.64999999999999858, 74.05981308412474107, -190.6939882734710636 ) ) ;
#74941 = EDGE_LOOP ( 'NONE', ( #164111, #43034, #111740, #29829 ) ) ;
#74940 = CARTESIAN_POINT ( 'NONE',  ( -18.50000000000000000, 66.75000000001253397, -182.3731074845244393 ) ) ;
#74942 = DIRECTION ( 'NONE',  ( -0.000000000000000000, -0.8660254037844420383, 0.4999999999999943379 ) ) ;
#74944 = ORIENTED_EDGE ( 'NONE', *, *, #81872, .F. ) ;
#74943 = CARTESIAN_POINT ( 'NONE',  ( -18.59999994787167310, 85.52363768977360792, -96.14065794975194024 ) ) ;
#74945 = FACE_OUTER_BOUND ( 'NONE', #102831, .T. ) ;
#74946 = CARTESIAN_POINT ( 'NONE',  ( 20.73486653747088582, 7.250000000011182166, -109.7500000000000426 ) ) ;
#74947 = CARTESIAN_POINT ( 'NONE',  ( -21.05000000000000071, -10.58757034444203704, -206.3761839813444396 ) ) ;
#74949 = ADVANCED_FACE ( 'NONE', ( #144681 ), #228812, .F. ) ;
#74948 = CARTESIAN_POINT ( 'NONE',  ( -20.85000000000000142, 0.1610488207298751417, -100.2158101556398293 ) ) ;
#74950 = AXIS2_PLACEMENT_3D ( 'NONE', #142410, #22493, #202393 ) ;
#74953 = DIRECTION ( 'NONE',  ( 0.1538461538461484146, -0.9880948137434723000, 0.000000000000000000 ) ) ;
#74952 = AXIS2_PLACEMENT_3D ( 'NONE', #220837, #81299, #21390 ) ;
#74951 = CARTESIAN_POINT ( 'NONE',  ( -16.96982749440706328, 9.950000000011137047, -154.3752215911892733 ) ) ;
#74954 = DIRECTION ( 'NONE',  ( -1.000000000000000000, 0.000000000000000000, 0.000000000000000000 ) ) ;
#74955 = AXIS2_PLACEMENT_3D ( 'NONE', #48921, #43803, #84145 ) ;
#74956 = AXIS2_PLACEMENT_3D ( 'NONE', #247164, #191083, #209325 ) ;
#74957 = CARTESIAN_POINT ( 'NONE',  ( -21.14999999999999858, 64.25000000001233502, -163.2392418215462726 ) ) ;
#74958 = CARTESIAN_POINT ( 'NONE',  ( -18.31331870001069362, 85.53629471919325056, -163.1545287935392423 ) ) ;
#74959 = DIRECTION ( 'NONE',  ( 1.000000000000000000, 0.000000000000000000, 0.000000000000000000 ) ) ;
#74960 = DIRECTION ( 'NONE',  ( 0.000000000000000000, -0.2617529984164955192, -0.9651348961777178603 ) ) ;
#74961 = VERTEX_POINT ( 'NONE', #28658 ) ;
#74962 = FACE_OUTER_BOUND ( 'NONE', #33495, .T. ) ;
#74963 = TOROIDAL_SURFACE ( 'NONE', #70873, 1.900000000000002576, 0.1000000000000000056 ) ;
#74964 = VERTEX_POINT ( 'NONE', #67729 ) ;
#74965 = ORIENTED_EDGE ( 'NONE', *, *, #92317, .F. ) ;
#74966 = CARTESIAN_POINT ( 'NONE',  ( -20.94999999999999929, 67.65035251205981126, -227.9627438638999877 ) ) ;
#74967 = DIRECTION ( 'NONE',  ( 2.952720810173289112E-16, 1.000000000000000000, 6.982962677686266711E-15 ) ) ;
#74968 = VERTEX_POINT ( 'NONE', #226793 ) ;
#74969 =( BOUNDED_SURFACE ( )  B_SPLINE_SURFACE ( 3, 2, ( 
 ( #161587, #216395, #160307 ),
 ( #141987, #101552, #182427 ),
 ( #221513, #237254, #122445 ),
 ( #57303, #58590, #138126 ) ),
 .UNSPECIFIED., .F., .F., .F. ) 
 B_SPLINE_SURFACE_WITH_KNOTS ( ( 4, 4 ),
 ( 3, 3 ),
 ( 0.0006461284895273765793, 0.0007503702773986197947 ),
 ( 0.000000000000000000, 1.000000000000000000 ),
 .UNSPECIFIED. ) 
 GEOMETRIC_REPRESENTATION_ITEM ( )  RATIONAL_B_SPLINE_SURFACE ( (
 ( 1.000000000000000000, 0.7071067811865475727, 1.000000000000000000),
 ( 1.000000000000000000, 0.7076476444648808206, 1.000000000000000000),
 ( 1.000000000000000000, 0.7075727925191797052, 1.000000000000000000),
 ( 1.000000000000000000, 0.7071067811865581199, 1.000000000000000000) ) ) 
 REPRESENTATION_ITEM ( '' )  SURFACE ( )  );
#74970 = ORIENTED_EDGE ( 'NONE', *, *, #176940, .T. ) ;
#74971 = AXIS2_PLACEMENT_3D ( 'NONE', #224858, #42383, #67085 ) ;
#74972 = CARTESIAN_POINT ( 'NONE',  ( -23.15000000000000213, 7.128833340093095217, -233.7327013124392749 ) ) ;
#74973 = ORIENTED_EDGE ( 'NONE', *, *, #117758, .F. ) ;
#74974 = AXIS2_PLACEMENT_3D ( 'NONE', #112175, #191722, #13075 ) ;
#74975 = ORIENTED_EDGE ( 'NONE', *, *, #50290, .T. ) ;
#74976 = EDGE_CURVE ( 'NONE', #11734, #129370, #116382, .T. ) ;
#74977 = CARTESIAN_POINT ( 'NONE',  ( 21.05000000000005400, 64.35000000001120668, -30.12310748452479103 ) ) ;
#74978 = CARTESIAN_POINT ( 'NONE',  ( -23.25000000000000000, 76.00000000001210765, -132.3731074845242972 ) ) ;
#74979 = DIRECTION ( 'NONE',  ( -1.000000000000000000, -1.646408749285562691E-14, 1.073024830501117725E-15 ) ) ;
#74980 = EDGE_CURVE ( 'NONE', #119332, #204996, #2607, .T. ) ;
#74981 = CARTESIAN_POINT ( 'NONE',  ( 21.05000000000000071, 7.128833340093095217, -233.7327013124392749 ) ) ;
#74982 = CARTESIAN_POINT ( 'NONE',  ( 13.12220780326571834, 9.430633469072795094, -15.23176579482408322 ) ) ;
#74984 = CARTESIAN_POINT ( 'NONE',  ( -20.54999999999999716, -9.399999999988848387, -110.3939691226524786 ) ) ;
#74983 = CARTESIAN_POINT ( 'NONE',  ( 13.99999999999999822, 9.850000000011137402, -117.2500000000000284 ) ) ;
#74985 = DIRECTION ( 'NONE',  ( -1.000000000000000000, 0.000000000000000000, -0.000000000000000000 ) ) ;
#74987 = ORIENTED_EDGE ( 'NONE', *, *, #155446, .F. ) ;
#74986 = DIRECTION ( 'NONE',  ( 0.000000000000000000, 0.000000000000000000, 1.000000000000000000 ) ) ;
#74989 = CARTESIAN_POINT ( 'NONE',  ( 20.94999999999999929, -11.39257802169451317, -197.9260504201680249 ) ) ;
#74988 = CARTESIAN_POINT ( 'NONE',  ( -22.94999999999999929, 6.223900101154157483, 12.09999999999999964 ) ) ;
#74990 = ADVANCED_FACE ( 'NONE', ( #51993, #173301 ), #208541, .T. ) ;
#74991 = DIRECTION ( 'NONE',  ( 1.000000000000000000, 1.541880601228652843E-16, 2.878400969107353907E-16 ) ) ;
#74992 = EDGE_CURVE ( 'NONE', #35062, #68656, #93705, .T. ) ;
#74993 = ORIENTED_EDGE ( 'NONE', *, *, #157964, .T. ) ;
#74994 = CARTESIAN_POINT ( 'NONE',  ( -21.05000000000000071, 1.851028230152016674, -45.15391326942250316 ) ) ;
#74995 = VERTEX_POINT ( 'NONE', #213657 ) ;
#74996 = EDGE_CURVE ( 'NONE', #38707, #214401, #12162, .T. ) ;
#74997 = DIRECTION ( 'NONE',  ( -4.336808689942053235E-15, -0.8660254037844482555, -0.4999999999999836797 ) ) ;
#74998 = CIRCLE ( 'NONE', #45748, 0.09999999999999939493 ) ;
#74999 = EDGE_CURVE ( 'NONE', #52494, #28807, #8059, .T. ) ;
#75000 = CARTESIAN_POINT ( 'NONE',  ( -23.25000000000000000, 2.718532714028242925, -213.4823957989985956 ) ) ;
#75001 = CARTESIAN_POINT ( 'NONE',  ( 14.56326696814971200, 66.55335100938299320, -87.93394418860121675 ) ) ;
#75003 = ADVANCED_FACE ( 'NONE', ( #53302 ), #162184, .F. ) ;
#75002 = EDGE_CURVE ( 'NONE', #207677, #226065, #153844, .T. ) ;
#75004 = ORIENTED_EDGE ( 'NONE', *, *, #123407, .T. ) ;
#75005 = EDGE_LOOP ( 'NONE', ( #188142, #36581, #29742, #255969 ) ) ;
#75006 = CARTESIAN_POINT ( 'NONE',  ( 21.72449340488910607, 65.71604372252112114, -149.1731074845244507 ) ) ;
#75007 = EDGE_CURVE ( 'NONE', #165380, #210276, #54943, .T. ) ;
#75008 = TOROIDAL_SURFACE ( 'NONE', #124865, 11.70000000000000462, 0.1000000000000000056 ) ;
#75009 = DIRECTION ( 'NONE',  ( 0.000000000000000000, 0.1350103645451807832, 0.9908441862701610203 ) ) ;
#75010 = DIRECTION ( 'NONE',  ( 0.000000000000000000, -0.1568667991644355497, 0.9876197685951332295 ) ) ;
#75011 = VERTEX_POINT ( 'NONE', #54573 ) ;
#75012 = CARTESIAN_POINT ( 'NONE',  ( 18.59999999999999076, 6.450000000000001066, -10.01702717044001822 ) ) ;
#75013 = EDGE_CURVE ( 'NONE', #194521, #102331, #92413, .T. ) ;
#75014 = DIRECTION ( 'NONE',  ( 1.000000000000000000, 0.000000000000000000, 0.000000000000000000 ) ) ;
#75015 = CARTESIAN_POINT ( 'NONE',  ( -21.05000000000000071, 67.23127455305841238, -235.8551265064783991 ) ) ;
#75016 = LINE ( 'NONE', #150678, #7558 ) ;
#75017 = EDGE_CURVE ( 'NONE', #141149, #133516, #70331, .T. ) ;
#75018 = ADVANCED_FACE ( 'NONE', ( #134101 ), #149728, .T. ) ;
#75019 = AXIS2_PLACEMENT_3D ( 'NONE', #95237, #17004, #57376 ) ;
#75021 = CARTESIAN_POINT ( 'NONE',  ( -23.15000000000000213, 11.75000000001116263, -146.1500000000000341 ) ) ;
#75020 = CIRCLE ( 'NONE', #104201, 0.1000000000000106914 ) ;
#75022 = EDGE_CURVE ( 'NONE', #235545, #18136, #99585, .T. ) ;
#75024 = VERTEX_POINT ( 'NONE', #32492 ) ;
#75023 = CARTESIAN_POINT ( 'NONE',  ( -16.93860193097148326, 66.00689223268254580, -82.12296911721753645 ) ) ;
#75025 = CYLINDRICAL_SURFACE ( 'NONE', #155950, 0.09999999999999939493 ) ;
#75026 = CARTESIAN_POINT ( 'NONE',  ( -23.15000000000000213, 76.00000000001190870, -103.0231074845243029 ) ) ;
#75027 = DIRECTION ( 'NONE',  ( 1.000000000000000000, 0.000000000000000000, 0.000000000000000000 ) ) ;
#75028 = VECTOR ( 'NONE', #179226, 1000.000000000000114 ) ;
#75029 = LINE ( 'NONE', #237915, #117889 ) ;
#75030 = CARTESIAN_POINT ( 'NONE',  ( -18.59999999999999787, 0.000000000000000000, -41.40000000000000568 ) ) ;
#75031 = EDGE_CURVE ( 'NONE', #78593, #20074, #87143, .T. ) ;
#75033 = ORIENTED_EDGE ( 'NONE', *, *, #234538, .F. ) ;
#75032 = CARTESIAN_POINT ( 'NONE',  ( 18.59999999999999076, 80.78317333349157536, -192.9003134612049166 ) ) ;
#75034 = LINE ( 'NONE', #197504, #17398 ) ;
#75035 = EDGE_CURVE ( 'NONE', #76326, #25605, #224521, .T. ) ;
#75036 = VECTOR ( 'NONE', #145198, 1000.000000000000000 ) ;
#75037 = CARTESIAN_POINT ( 'NONE',  ( 18.49999999999999289, 14.51805813080544638, -219.6885945441820809 ) ) ;
#75038 = CARTESIAN_POINT ( 'NONE',  ( -20.65000000000000568, 42.79061499530347845, -240.6131891775583824 ) ) ;
#75039 = AXIS2_PLACEMENT_3D ( 'NONE', #72856, #170692, #251454 ) ;
#75040 = ORIENTED_EDGE ( 'NONE', *, *, #244501, .F. ) ;
#75041 = DIRECTION ( 'NONE',  ( 0.000000000000000000, -6.982962677686266711E-15, 1.000000000000000000 ) ) ;
#75042 = FACE_OUTER_BOUND ( 'NONE', #93205, .T. ) ;
#75043 = CARTESIAN_POINT ( 'NONE',  ( 20.94999999999999574, -11.64999999998883595, -103.4000000000000341 ) ) ;
#75044 = DIRECTION ( 'NONE',  ( 0.000000000000000000, 0.000000000000000000, 1.000000000000000000 ) ) ;
#75045 = CARTESIAN_POINT ( 'NONE',  ( -23.24999999999999645, -0.8467571797981052750, -242.2246066262668194 ) ) ;
#75047 = DIRECTION ( 'NONE',  ( 1.000000000000000000, 0.000000000000000000, 0.000000000000000000 ) ) ;
#75046 = AXIS2_PLACEMENT_3D ( 'NONE', #219585, #166083, #82619 ) ;
#75048 = AXIS2_PLACEMENT_3D ( 'NONE', #1907, #60600, #83979 ) ;
#75050 = ORIENTED_EDGE ( 'NONE', *, *, #176301, .T. ) ;
#75049 = AXIS2_PLACEMENT_3D ( 'NONE', #195575, #37786, #215115 ) ;
#75051 = VERTEX_POINT ( 'NONE', #229383 ) ;
#75052 = AXIS2_PLACEMENT_3D ( 'NONE', #31669, #80698, #216372 ) ;
#75053 = LINE ( 'NONE', #57998, #151697 ) ;
#75054 = FACE_OUTER_BOUND ( 'NONE', #55666, .T. ) ;
#75055 = AXIS2_PLACEMENT_3D ( 'NONE', #3067, #6936, #185576 ) ;
#75056 = CARTESIAN_POINT ( 'NONE',  ( 21.14999999999999503, 64.25000000001269029, -203.5231074845244166 ) ) ;
#75057 = CARTESIAN_POINT ( 'NONE',  ( 18.49999999999999289, 65.79142135624930177, -115.1731074845243796 ) ) ;
#75058 = CARTESIAN_POINT ( 'NONE',  ( -20.54999999999999716, 1.115600667400684642E-11, -33.50000000000000000 ) ) ;
#75059 = CARTESIAN_POINT ( 'NONE',  ( 18.39999999999999503, 59.20211495293902004, -220.5705723384363921 ) ) ;
#75060 = CARTESIAN_POINT ( 'NONE',  ( -16.93583594267724024, 10.00862343506335783, -113.0593908393207840 ) ) ;
#75061 = CARTESIAN_POINT ( 'NONE',  ( -18.59999999999999787, 68.97833521811131163, -32.18954208262707795 ) ) ;
#75062 = ORIENTED_EDGE ( 'NONE', *, *, #3406, .T. ) ;
#75063 = CARTESIAN_POINT ( 'NONE',  ( -16.27683809663750480, 66.65000000001153069, -48.57310748452439242 ) ) ;
#75064 = VERTEX_POINT ( 'NONE', #251489 ) ;
#75065 = ORIENTED_EDGE ( 'NONE', *, *, #85161, .F. ) ;
#75066 = CARTESIAN_POINT ( 'NONE',  ( -18.79999999999999716, 7.799999999999999822, -15.00000000000000000 ) ) ;
#75067 = DIRECTION ( 'NONE',  ( 1.000000000000000000, 0.000000000000000000, 0.000000000000000000 ) ) ;
#75068 = CARTESIAN_POINT ( 'NONE',  ( 20.94999999999999929, 76.00000000001142553, -36.02310748452432421 ) ) ;
#75070 = EDGE_LOOP ( 'NONE', ( #224321, #179529, #131580, #123651 ) ) ;
#75069 = CARTESIAN_POINT ( 'NONE',  ( -16.83199318825829138, 9.930646127992318384, -87.72758518820923257 ) ) ;
#75071 = CARTESIAN_POINT ( 'NONE',  ( -18.59999999999999787, 74.83729825007431202, -161.9231074845243654 ) ) ;
#75072 = CARTESIAN_POINT ( 'NONE',  ( -21.64999999999999858, 7.250000000011148416, -88.25000000000005684 ) ) ;
#75073 = CARTESIAN_POINT ( 'NONE',  ( 18.47135592147649774, 85.47108861327741636, -62.83951254468078673 ) ) ;
#75075 = ORIENTED_EDGE ( 'NONE', *, *, #35904, .F. ) ;
#75074 = AXIS2_PLACEMENT_3D ( 'NONE', #203735, #27706, #245441 ) ;
#75076 = CARTESIAN_POINT ( 'NONE',  ( -18.50000000000000000, 64.18627039993180006, -224.3513032416919089 ) ) ;
#75077 = EDGE_CURVE ( 'NONE', #20649, #136330, #57902, .T. ) ;
#75078 = LINE ( 'NONE', #33390, #42251 ) ;
#75079 = AXIS2_PLACEMENT_3D ( 'NONE', #157945, #41829, #237436 ) ;
#75080 = CARTESIAN_POINT ( 'NONE',  ( -20.85000000000000142, -1.135018845899022466, -141.7169768834323520 ) ) ;
#75081 = SPHERICAL_SURFACE ( 'NONE', #60427, 0.1000000000000000056 ) ;
#75082 = EDGE_CURVE ( 'NONE', #157057, #14440, #88554, .T. ) ;
#75083 = VECTOR ( 'NONE', #186270, 1000.000000000000000 ) ;
#75084 = EDGE_LOOP ( 'NONE', ( #90513, #133973, #205267, #136001 ) ) ;
#75085 = FACE_OUTER_BOUND ( 'NONE', #248741, .T. ) ;
#75087 = EDGE_CURVE ( 'NONE', #87344, #179596, #170406, .T. ) ;
#75086 = CARTESIAN_POINT ( 'NONE',  ( -16.87683809663752399, 66.15000000001187175, -89.62074346632807931 ) ) ;
#75089 = EDGE_CURVE ( 'NONE', #158190, #178251, #157937, .T. ) ;
#75088 = VERTEX_POINT ( 'NONE', #96258 ) ;
#75090 = CARTESIAN_POINT ( 'NONE',  ( 21.10320863425824811, 6.400277386470322405, -133.9749777487728579 ) ) ;
#75091 = CARTESIAN_POINT ( 'NONE',  ( 22.57320508075688181, 55.89093952297025680, -232.7795287750844864 ) ) ;
#75092 = LINE ( 'NONE', #54201, #89887 ) ;
#75093 = AXIS2_PLACEMENT_3D ( 'NONE', #248224, #145248, #86542 ) ;
#75094 = CIRCLE ( 'NONE', #250037, 4.300000000000032685 ) ;
#75095 = ORIENTED_EDGE ( 'NONE', *, *, #112576, .T. ) ;
#75096 = CARTESIAN_POINT ( 'NONE',  ( 18.31325810956334266, -9.536388475996066205, -174.3684402063047969 ) ) ;
#75097 = CARTESIAN_POINT ( 'NONE',  ( 21.14999999999999858, 64.35000000001258513, -191.3731074845244393 ) ) ;
#75098 = ORIENTED_EDGE ( 'NONE', *, *, #104562, .T. ) ;
#75099 = AXIS2_PLACEMENT_3D ( 'NONE', #124306, #40941, #81285 ) ;
#75100 = ADVANCED_FACE ( 'NONE', ( #177123 ), #254051, .F. ) ;
#75101 = AXIS2_PLACEMENT_3D ( 'NONE', #161447, #18059, #42765 ) ;
#75102 = ADVANCED_FACE ( 'NONE', ( #197927 ), #75460, .T. ) ;
#75103 = ORIENTED_EDGE ( 'NONE', *, *, #251969, .T. ) ;
#75104 = DIRECTION ( 'NONE',  ( -0.8660254037843878594, 0.000000000000000000, -0.5000000000000880407 ) ) ;
#75105 = CARTESIAN_POINT ( 'NONE',  ( -23.25000000000000000, 68.97833521811131163, -32.18954208262707795 ) ) ;
#75107 = ORIENTED_EDGE ( 'NONE', *, *, #98223, .F. ) ;
#75106 = CARTESIAN_POINT ( 'NONE',  ( -18.59999999999999787, 66.65000000001229807, -157.6731074845244223 ) ) ;
#75108 = DIRECTION ( 'NONE',  ( 1.875376730785737719E-16, 1.000000000000000000, 6.982962677686266711E-15 ) ) ;
#75109 = CARTESIAN_POINT ( 'NONE',  ( -22.48660254037843487, 11.65000000001115588, -133.9500000000000455 ) ) ;
#75110 = CARTESIAN_POINT ( 'NONE',  ( 21.72449340488910252, 59.72708471423849375, -224.2357723256170061 ) ) ;
#75111 = FACE_OUTER_BOUND ( 'NONE', #80345, .T. ) ;
#75112 = DIRECTION ( 'NONE',  ( 0.000000000000000000, 0.000000000000000000, -1.000000000000000000 ) ) ;
#75115 = ORIENTED_EDGE ( 'NONE', *, *, #162628, .F. ) ;
#75114 = EDGE_CURVE ( 'NONE', #75851, #194825, #175833, .T. ) ;
#75113 = CARTESIAN_POINT ( 'NONE',  ( -20.54999999999999716, 71.65000000001253966, -182.3731074845244109 ) ) ;
#75116 = EDGE_LOOP ( 'NONE', ( #197928, #196458, #96394, #105342, #120324, #95359, #257627, #126904, #100079, #172947, #169514 ) ) ;
#75119 = CARTESIAN_POINT ( 'NONE',  ( -18.59999999999999787, 9.350000000011156942, -45.75000000000000000 ) ) ;
#75118 = CARTESIAN_POINT ( 'NONE',  ( -23.25000000000000000, 26.22918441313017723, -241.0147027585851731 ) ) ;
#75117 = VECTOR ( 'NONE', #132629, 1000.000000000000000 ) ;
#75121 = ORIENTED_EDGE ( 'NONE', *, *, #185519, .F. ) ;
#75120 = DIRECTION ( 'NONE',  ( -1.000000000000000000, 0.000000000000000000, 0.000000000000000000 ) ) ;
#75122 = ORIENTED_EDGE ( 'NONE', *, *, #187254, .F. ) ;
#75123 = EDGE_CURVE ( 'NONE', #97348, #20836, #78919, .T. ) ;
#75124 = CARTESIAN_POINT ( 'NONE',  ( -18.50596464788227635, 10.30632246271647112, -106.0041836778896283 ) ) ;
#75125 = CARTESIAN_POINT ( 'NONE',  ( 23.14999999999999503, 11.65000000001116298, -60.08519422934606524 ) ) ;
#75126 = B_SPLINE_CURVE_WITH_KNOTS ( 'NONE', 3,
 ( #84918, #25008, #64112, #139771 ),
 .UNSPECIFIED., .F., .F.,
 ( 4, 4 ),
 ( 0.000000000000000000, 0.0001048066582182494762 ),
 .UNSPECIFIED. ) ;
#75127 = CARTESIAN_POINT ( 'NONE',  ( -20.94999999999999929, 14.64166534854604507, -236.4381089660238331 ) ) ;
#75128 = DIRECTION ( 'NONE',  ( 0.000000000000000000, 0.000000000000000000, -1.000000000000000000 ) ) ;
#75129 = CARTESIAN_POINT ( 'NONE',  ( -18.51024323315077424, 67.49344847133114911, -195.4961807846321733 ) ) ;
#75131 = EDGE_CURVE ( 'NONE', #207350, #245627, #37468, .T. ) ;
#75130 = DIRECTION ( 'NONE',  ( 0.000000000000000000, 0.000000000000000000, -1.000000000000000000 ) ) ;
#75132 = EDGE_CURVE ( 'NONE', #30882, #100578, #18015, .T. ) ;
#75133 = CARTESIAN_POINT ( 'NONE',  ( -23.15000000000000213, 78.08573236070779444, -228.9307947190811774 ) ) ;
#75134 = AXIS2_PLACEMENT_3D ( 'NONE', #10616, #133127, #212671 ) ;
#75135 = ORIENTED_EDGE ( 'NONE', *, *, #229019, .T. ) ;
#75136 = ORIENTED_EDGE ( 'NONE', *, *, #233616, .F. ) ;
#75137 = AXIS2_PLACEMENT_3D ( 'NONE', #197120, #257052, #253240 ) ;
#75138 = CIRCLE ( 'NONE', #95936, 4.149999999999987033 ) ;
#75139 = EDGE_CURVE ( 'NONE', #220244, #170581, #145580, .T. ) ;
#75140 = ORIENTED_EDGE ( 'NONE', *, *, #211235, .T. ) ;
#75141 = FACE_OUTER_BOUND ( 'NONE', #16508, .T. ) ;
#75142 = FACE_OUTER_BOUND ( 'NONE', #252628, .T. ) ;
#75143 = AXIS2_PLACEMENT_3D ( 'NONE', #154568, #153288, #112839 ) ;
#75144 = DIRECTION ( 'NONE',  ( 1.000000000000000000, 7.304098846218135653E-16, 5.311601492717085047E-30 ) ) ;
#75145 = ORIENTED_EDGE ( 'NONE', *, *, #88142, .T. ) ;
#75146 = CARTESIAN_POINT ( 'NONE',  ( -14.11361717019515893, 66.54257354752313347, -118.0230656161243274 ) ) ;
#75147 = ORIENTED_EDGE ( 'NONE', *, *, #219693, .F. ) ;
#75148 = EDGE_CURVE ( 'NONE', #217909, #106580, #95697, .T. ) ;
#75149 = DIRECTION ( 'NONE',  ( 7.589415207398576792E-15, 0.9651348961777157509, -0.2617529984165031243 ) ) ;
#75150 = EDGE_LOOP ( 'NONE', ( #166325, #177653, #107852, #105176, #248787 ) ) ;
#75151 = AXIS2_PLACEMENT_3D ( 'NONE', #247863, #208754, #167079 ) ;
#75152 = CARTESIAN_POINT ( 'NONE',  ( -20.64999999999999858, 75.47649400317826007, -205.4533772768803317 ) ) ;
#75154 = TOROIDAL_SURFACE ( 'NONE', #208235, 7.800000000000000711, 0.1000000000000000056 ) ;
#75153 = DIRECTION ( 'NONE',  ( -0.7071067811865475727, -0.7071067811865475727, 0.000000000000000000 ) ) ;
#75155 = EDGE_CURVE ( 'NONE', #66273, #129641, #158111, .T. ) ;
#75156 = ORIENTED_EDGE ( 'NONE', *, *, #128319, .T. ) ;
#75157 = FACE_OUTER_BOUND ( 'NONE', #233808, .T. ) ;
#75158 = ORIENTED_EDGE ( 'NONE', *, *, #92102, .T. ) ;
#75161 = EDGE_LOOP ( 'NONE', ( #107650, #152575, #197270 ) ) ;
#75160 = DIRECTION ( 'NONE',  ( -7.304098846218134667E-16, -1.000000000000000000, 0.000000000000000000 ) ) ;
#75159 = CARTESIAN_POINT ( 'NONE',  ( 22.49806830649814060, 55.96728299348496449, -232.8804964729971232 ) ) ;
#75162 = CARTESIAN_POINT ( 'NONE',  ( -20.94560253601877164, 64.25000000001148237, -43.01302397200913674 ) ) ;
#75163 = VERTEX_POINT ( 'NONE', #57121 ) ;
#75164 = ORIENTED_EDGE ( 'NONE', *, *, #159776, .F. ) ;
#75165 = CARTESIAN_POINT ( 'NONE',  ( -2.995603634470891112E-16, 87.75000000001223555, -148.7731074845242745 ) ) ;
#75166 = ORIENTED_EDGE ( 'NONE', *, *, #165020, .F. ) ;
#75167 = DIRECTION ( 'NONE',  ( 0.000000000000000000, 0.8660254037844482555, 0.4999999999999837907 ) ) ;
#75168 = FACE_OUTER_BOUND ( 'NONE', #235537, .T. ) ;
#75169 = CARTESIAN_POINT ( 'NONE',  ( 20.95512820512820440, 8.876151316288115822, -21.25000000000000000 ) ) ;
#75170 = CARTESIAN_POINT ( 'NONE',  ( -21.08078803292166725, 0.07918598716886154909, -60.66698703556290440 ) ) ;
#75171 = VERTEX_POINT ( 'NONE', #15477 ) ;
#75172 = DIRECTION ( 'NONE',  ( 0.000000000000000000, 0.000000000000000000, 1.000000000000000000 ) ) ;
#75173 = DIRECTION ( 'NONE',  ( -0.000000000000000000, 0.000000000000000000, 1.000000000000000000 ) ) ;
#75174 = CARTESIAN_POINT ( 'NONE',  ( -23.25000000000000000, 11.75000000000000000, 0.000000000000000000 ) ) ;
#75175 = VECTOR ( 'NONE', #136298, 1000.000000000000000 ) ;
#75176 = ORIENTED_EDGE ( 'NONE', *, *, #26412, .T. ) ;
#75177 = DIRECTION ( 'NONE',  ( 1.000000000000000000, 0.000000000000000000, 0.000000000000000000 ) ) ;
#75178 = ORIENTED_EDGE ( 'NONE', *, *, #237302, .F. ) ;
#75179 = CARTESIAN_POINT ( 'NONE',  ( -21.78635804494510708, 33.69213361928919426, -243.1708424215785271 ) ) ;
#75180 = ORIENTED_EDGE ( 'NONE', *, *, #163044, .F. ) ;
#75181 = CARTESIAN_POINT ( 'NONE',  ( 23.14999999999999503, 17.04051908253854108, -224.4971436904607174 ) ) ;
#75182 = CYLINDRICAL_SURFACE ( 'NONE', #222802, 12.87499999999999822 ) ;
#75183 = AXIS2_PLACEMENT_3D ( 'NONE', #248793, #207097, #229231 ) ;
#75185 = ORIENTED_EDGE ( 'NONE', *, *, #42629, .T. ) ;
#75184 = CARTESIAN_POINT ( 'NONE',  ( -20.54999999999999716, 36.65892442174935439, -249.5511627012433848 ) ) ;
#75186 = CARTESIAN_POINT ( 'NONE',  ( -18.49999999999997868, 9.105964803472803126, -245.3658845043482302 ) ) ;
#75187 = ORIENTED_EDGE ( 'NONE', *, *, #83754, .T. ) ;
#75188 = CARTESIAN_POINT ( 'NONE',  ( -20.99551997958407057, 36.17041074700907899, -235.9598556649060015 ) ) ;
#75189 = CARTESIAN_POINT ( 'NONE',  ( -16.77308656112214180, 9.950000000011135270, -113.1501931917023427 ) ) ;
#75190 = ORIENTED_EDGE ( 'NONE', *, *, #236922, .F. ) ;
#75191 = DIRECTION ( 'NONE',  ( -0.000000000000000000, -0.000000000000000000, -1.000000000000000000 ) ) ;
#75192 = CARTESIAN_POINT ( 'NONE',  ( -21.05000000000000071, 1.835341550235567887, -179.1551512925629197 ) ) ;
#75193 = ORIENTED_EDGE ( 'NONE', *, *, #232606, .F. ) ;
#75194 = FACE_OUTER_BOUND ( 'NONE', #140250, .T. ) ;
#75195 = CIRCLE ( 'NONE', #220897, 12.77500000000000924 ) ;
#75196 = AXIS2_PLACEMENT_3D ( 'NONE', #169087, #170383, #71252 ) ;
#75197 = VERTEX_POINT ( 'NONE', #217483 ) ;
#75198 = CARTESIAN_POINT ( 'NONE',  ( -23.25000000000000000, 1.910280373831780176, -12.63136785519894012 ) ) ;
#75199 = DIRECTION ( 'NONE',  ( 0.000000000000000000, -0.9994937237965558774, -0.03181660087586650476 ) ) ;
#75200 = VECTOR ( 'NONE', #206163, 1000.000000000000000 ) ;
#75201 = EDGE_CURVE ( 'NONE', #61667, #251571, #218768, .T. ) ;
#75202 = CIRCLE ( 'NONE', #220911, 0.1000000000000089151 ) ;
#75203 = CIRCLE ( 'NONE', #133453, 0.1000000000000013933 ) ;
#75205 = VERTEX_POINT ( 'NONE', #19304 ) ;
#75204 = CARTESIAN_POINT ( 'NONE',  ( -0.8999999999999438449, 67.75000000001118394, -5.981686128287480919 ) ) ;
#75206 = EDGE_CURVE ( 'NONE', #173295, #198415, #64654, .T. ) ;
#75207 = PLANE ( 'NONE',  #215821 ) ;
#75208 = EDGE_CURVE ( 'NONE', #96187, #190057, #129037, .T. ) ;
#75209 = CARTESIAN_POINT ( 'NONE',  ( -22.39999999999999858, 1.115600667400684642E-11, -155.8504291924551808 ) ) ;
#75210 = DIRECTION ( 'NONE',  ( 0.000000000000000000, 0.000000000000000000, 1.000000000000000000 ) ) ;
#75212 = CARTESIAN_POINT ( 'NONE',  ( 20.94999999999999929, 79.34051597037932879, -196.3602670448451875 ) ) ;
#75211 = DIRECTION ( 'NONE',  ( 0.000000000000000000, 0.9889818879709272315, 0.1480365673253073999 ) ) ;
#75213 = CYLINDRICAL_SURFACE ( 'NONE', #207054, 0.09999999999999939493 ) ;
#75214 = DIRECTION ( 'NONE',  ( 1.000000000000000000, 0.000000000000000000, 0.000000000000000000 ) ) ;
#75215 = DIRECTION ( 'NONE',  ( 0.000000000000000000, 0.9915357197604982575, -0.1298341882519033486 ) ) ;
#75216 = AXIS2_PLACEMENT_3D ( 'NONE', #190133, #171882, #54454 ) ;
#75217 = CARTESIAN_POINT ( 'NONE',  ( 20.94999999999999929, 65.27628289530457550, -128.8581939154367717 ) ) ;
#75218 = AXIS2_PLACEMENT_3D ( 'NONE', #221601, #43003, #202073 ) ;
#75219 = AXIS2_PLACEMENT_3D ( 'NONE', #127573, #252633, #136529 ) ;
#75220 = ORIENTED_EDGE ( 'NONE', *, *, #246677, .T. ) ;
#75221 = CIRCLE ( 'NONE', #54528, 11.75000000000000355 ) ;
#75223 = VERTEX_POINT ( 'NONE', #55830 ) ;
#75222 = CIRCLE ( 'NONE', #50231, 2.600000000000000089 ) ;
#75224 = CARTESIAN_POINT ( 'NONE',  ( 21.07928932188134397, 33.98134083355422774, -243.8161431329846778 ) ) ;
#75226 = ORIENTED_EDGE ( 'NONE', *, *, #135548, .F. ) ;
#75225 = CARTESIAN_POINT ( 'NONE',  ( -18.50000000000000000, 76.00000000001165290, -69.52310748452431710 ) ) ;
#75227 = ORIENTED_EDGE ( 'NONE', *, *, #125298, .F. ) ;
#75228 = ADVANCED_FACE ( 'NONE', ( #98802 ), #74896, .T. ) ;
#75229 = LINE ( 'NONE', #36087, #155960 ) ;
#75230 = ORIENTED_EDGE ( 'NONE', *, *, #213526, .T. ) ;
#75231 = CARTESIAN_POINT ( 'NONE',  ( 22.47071067811866740, 33.41224047107335338, -242.5462774987836667 ) ) ;
#75232 = AXIS2_PLACEMENT_3D ( 'NONE', #20039, #96947, #177836 ) ;
#75233 = EDGE_LOOP ( 'NONE', ( #168213, #38119, #213500, #203730 ) ) ;
#75234 = DIRECTION ( 'NONE',  ( -1.000000000000000000, -0.000000000000000000, -0.000000000000000000 ) ) ;
#75236 = EDGE_LOOP ( 'NONE', ( #221483, #84994, #151118, #87077 ) ) ;
#75235 = ORIENTED_EDGE ( 'NONE', *, *, #228398, .T. ) ;
#75237 = ORIENTED_EDGE ( 'NONE', *, *, #239772, .F. ) ;
#75238 = VERTEX_POINT ( 'NONE', #257861 ) ;
#75239 = ORIENTED_EDGE ( 'NONE', *, *, #49334, .F. ) ;
#75240 = CARTESIAN_POINT ( 'NONE',  ( 21.07189867249812210, 43.41933109301616156, -234.7705648221715933 ) ) ;
#75241 = CARTESIAN_POINT ( 'NONE',  ( -18.54118089899632693, -9.463537631848099707, -7.048577597868117550 ) ) ;
#75243 = ORIENTED_EDGE ( 'NONE', *, *, #57716, .F. ) ;
#75242 = CARTESIAN_POINT ( 'NONE',  ( -18.79999999999999716, 6.644425182197214674, 9.641788261573355001 ) ) ;
#75244 = ADVANCED_FACE ( 'NONE', ( #59687 ), #4119, .T. ) ;
#75245 = EDGE_CURVE ( 'NONE', #128128, #16470, #241459, .T. ) ;
#75246 = CARTESIAN_POINT ( 'NONE',  ( 20.97107704358301916, 40.84128431181879648, -237.9521109762849846 ) ) ;
#75247 = DIRECTION ( 'NONE',  ( 0.000000000000000000, -0.8814952561688428334, 0.4721928772777348460 ) ) ;
#75249 = VERTEX_POINT ( 'NONE', #225178 ) ;
#75248 = DIRECTION ( 'NONE',  ( 1.000000000000000000, 0.000000000000000000, 0.000000000000000000 ) ) ;
#75250 = CARTESIAN_POINT ( 'NONE',  ( -23.15000000000000213, 87.48912529308779540, -72.62310748452422615 ) ) ;
#75251 = ORIENTED_EDGE ( 'NONE', *, *, #254095, .T. ) ;
#75252 = DIRECTION ( 'NONE',  ( -5.603264701231743991E-32, 1.897661533703519897E-16, -1.000000000000000000 ) ) ;
#75253 = CIRCLE ( 'NONE', #108548, 0.09999999999998898659 ) ;
#75255 = ORIENTED_EDGE ( 'NONE', *, *, #147676, .F. ) ;
#75254 = CARTESIAN_POINT ( 'NONE',  ( 23.14999999999999503, 11.75000000001116263, -122.2500000000000284 ) ) ;
#75256 = CARTESIAN_POINT ( 'NONE',  ( -18.50000000000000000, 68.97833521811203639, -132.8895420826271163 ) ) ;
#75257 = DIRECTION ( 'NONE',  ( 0.000000000000000000, -1.000000000000000000, -6.982962677686266711E-15 ) ) ;
#75258 = AXIS2_PLACEMENT_3D ( 'NONE', #179731, #38938, #21939 ) ;
#75259 = EDGE_CURVE ( 'NONE', #35508, #54116, #70796, .T. ) ;
#75260 = ORIENTED_EDGE ( 'NONE', *, *, #150428, .T. ) ;
#75262 = DIRECTION ( 'NONE',  ( 0.000000000000000000, -0.8660254037844377084, -0.5000000000000016653 ) ) ;
#75261 = FACE_OUTER_BOUND ( 'NONE', #128310, .T. ) ;
#75263 = DIRECTION ( 'NONE',  ( 0.000000000000000000, 0.2128009952263485993, -0.9770955615653341697 ) ) ;
#75264 = VECTOR ( 'NONE', #30602, 1000.000000000000114 ) ;
#75265 = CARTESIAN_POINT ( 'NONE',  ( 23.14999999999998792, 11.65000000001115588, -134.0000000000000000 ) ) ;
#75266 = CARTESIAN_POINT ( 'NONE',  ( -21.37071067811865532, 8.070710678129811910, -121.6500000000000341 ) ) ;
#75267 = ORIENTED_EDGE ( 'NONE', *, *, #7197, .T. ) ;
#75268 = ORIENTED_EDGE ( 'NONE', *, *, #97825, .F. ) ;
#75270 = TOROIDAL_SURFACE ( 'NONE', #12730, 11.70000000000000462, 0.1000000000000000056 ) ;
#75269 = DIRECTION ( 'NONE',  ( -0.000000000000000000, -6.982962677686266711E-15, 1.000000000000000000 ) ) ;
#75271 = B_SPLINE_CURVE_WITH_KNOTS ( 'NONE', 3,
 ( #69318, #151425, #148855, #31492 ),
 .UNSPECIFIED., .F., .F.,
 ( 4, 4 ),
 ( 0.000000000000000000, 0.001767853679387121216 ),
 .UNSPECIFIED. ) ;
#75272 = CARTESIAN_POINT ( 'NONE',  ( -26.01805557925458956, 8.624264858734566275, -347.0000000000001137 ) ) ;
#75273 = ORIENTED_EDGE ( 'NONE', *, *, #105249, .F. ) ;
#75274 = DIRECTION ( 'NONE',  ( 1.000000000000000000, 0.000000000000000000, 0.000000000000000000 ) ) ;
#75275 = ORIENTED_EDGE ( 'NONE', *, *, #131545, .F. ) ;
#75276 = FACE_OUTER_BOUND ( 'NONE', #126520, .T. ) ;
#75277 = DIRECTION ( 'NONE',  ( 0.000000000000000000, 0.000000000000000000, -1.000000000000000000 ) ) ;
#75278 = EDGE_CURVE ( 'NONE', #102720, #119208, #224686, .T. ) ;
#75279 = TOROIDAL_SURFACE ( 'NONE', #196058, 4.099999999999999645, 0.1000000000000000056 ) ;
#75280 = ORIENTED_EDGE ( 'NONE', *, *, #150665, .F. ) ;
#75281 = DIRECTION ( 'NONE',  ( 0.000000000000000000, 0.9876197685951252359, -0.1568667991644863424 ) ) ;
#75282 = AXIS2_PLACEMENT_3D ( 'NONE', #122741, #81001, #26198 ) ;
#75284 = VERTEX_POINT ( 'NONE', #43995 ) ;
#75283 = CIRCLE ( 'NONE', #12936, 0.1000000000000028644 ) ;
#75285 = ORIENTED_EDGE ( 'NONE', *, *, #157663, .F. ) ;
#75286 = VERTEX_POINT ( 'NONE', #24465 ) ;
#75287 = TOROIDAL_SURFACE ( 'NONE', #8631, 0.4000000000000010214, 0.1000000000000000056 ) ;
#75288 = EDGE_CURVE ( 'NONE', #10849, #177234, #126566, .T. ) ;
#75289 = DIRECTION ( 'NONE',  ( -0.000000000000000000, 0.1332476588733589318, 0.9910827722268049644 ) ) ;
#75290 = DIRECTION ( 'NONE',  ( 0.000000000000000000, 0.2128009952263485993, -0.9770955615653341697 ) ) ;
#75291 = EDGE_CURVE ( 'NONE', #174920, #65240, #154029, .T. ) ;
#75292 = CARTESIAN_POINT ( 'NONE',  ( -20.54999999999999716, 7.128833340094563376, -233.7327013124401276 ) ) ;
#75293 = CARTESIAN_POINT ( 'NONE',  ( 20.85000000000000142, -1.149570369564537842, -208.8159124845019221 ) ) ;
#75294 =( BOUNDED_SURFACE ( )  B_SPLINE_SURFACE ( 3, 2, ( 
 ( #215747, #77507, #239180 ),
 ( #60526, #38414, #56651 ),
 ( #140056, #159652, #157094 ),
 ( #155816, #41008, #120543 ) ),
 .UNSPECIFIED., .F., .F., .F. ) 
 B_SPLINE_SURFACE_WITH_KNOTS ( ( 4, 4 ),
 ( 3, 3 ),
 ( 0.0006461284895273917582, 0.0007503702773985875939 ),
 ( 0.000000000000000000, 1.000000000000000000 ),
 .UNSPECIFIED. ) 
 GEOMETRIC_REPRESENTATION_ITEM ( )  RATIONAL_B_SPLINE_SURFACE ( (
 ( 1.000000000000000000, 0.7071067811865475727, 1.000000000000000000),
 ( 1.000000000000000000, 0.7076476444648721609, 1.000000000000000000),
 ( 1.000000000000000000, 0.7075727925191875878, 1.000000000000000000),
 ( 1.000000000000000000, 0.7071067811865475727, 1.000000000000000000) ) ) 
 REPRESENTATION_ITEM ( '' )  SURFACE ( )  );
#75296 = LINE ( 'NONE', #176965, #215673 ) ;
#75295 = CARTESIAN_POINT ( 'NONE',  ( 21.11825140030092740, 0.007203620643933773479, -161.0545924345799165 ) ) ;
#75298 = ORIENTED_EDGE ( 'NONE', *, *, #82243, .F. ) ;
#75297 = CARTESIAN_POINT ( 'NONE',  ( 23.15000000000000213, 62.08591502004790641, -248.5699171172615820 ) ) ;
#75299 = EDGE_LOOP ( 'NONE', ( #237226, #92742, #89264, #4403 ) ) ;
#75300 = EDGE_CURVE ( 'NONE', #144444, #214790, #246059, .T. ) ;
#75301 = CARTESIAN_POINT ( 'NONE',  ( -16.86379686415369861, 22.91646731419714200, -230.8734579643043219 ) ) ;
#75302 = ADVANCED_FACE ( 'NONE', ( #203066 ), #183514, .F. ) ;
#75303 = ORIENTED_EDGE ( 'NONE', *, *, #47565, .F. ) ;
#75304 = ORIENTED_EDGE ( 'NONE', *, *, #141329, .F. ) ;
#75305 = CARTESIAN_POINT ( 'NONE',  ( 23.14999999999999503, 61.90000000001194280, -108.6234050956637560 ) ) ;
#75306 = CARTESIAN_POINT ( 'NONE',  ( -21.05000000000000071, 6.413662734880722027, -134.0855928633627911 ) ) ;
#75307 = DIRECTION ( 'NONE',  ( 0.000000000000000000, -7.086529944415894657E-15, 1.000000000000000000 ) ) ;
#75308 = DIRECTION ( 'NONE',  ( 0.000000000000000000, -0.9893560106964500722, 0.1455152366551550613 ) ) ;
#75309 = AXIS2_PLACEMENT_3D ( 'NONE', #76716, #220094, #163979 ) ;
#75310 = EDGE_CURVE ( 'NONE', #211037, #18932, #27037, .T. ) ;
#75311 = CARTESIAN_POINT ( 'NONE',  ( 21.14999999999999503, 76.10000000001174669, -81.17267829206912211 ) ) ;
#75312 = EDGE_CURVE ( 'NONE', #229783, #133438, #105206, .T. ) ;
#75313 = ORIENTED_EDGE ( 'NONE', *, *, #155034, .T. ) ;
#75314 = ORIENTED_EDGE ( 'NONE', *, *, #17876, .F. ) ;
#75315 = PLANE ( 'NONE',  #161664 ) ;
#75316 = ORIENTED_EDGE ( 'NONE', *, *, #14819, .T. ) ;
#75317 = DIRECTION ( 'NONE',  ( 1.000000000000000000, 0.000000000000000000, 0.000000000000000000 ) ) ;
#75318 = DIRECTION ( 'NONE',  ( -1.000000000000000000, 2.952720810173289112E-16, 2.061873921506763405E-30 ) ) ;
#75319 = ORIENTED_EDGE ( 'NONE', *, *, #138324, .T. ) ;
#75320 = CARTESIAN_POINT ( 'NONE',  ( 20.90000000000000213, 7.973296578895943121, 1.410778198689825347 ) ) ;
#75321 = ADVANCED_FACE ( 'NONE', ( #244751 ), #21282, .T. ) ;
#75322 = CARTESIAN_POINT ( 'NONE',  ( -22.49806830649814060, 64.35011034517256689, -69.60057180084992012 ) ) ;
#75323 = CARTESIAN_POINT ( 'NONE',  ( -20.54999999999999716, 71.65000000001180069, -81.87310748452433984 ) ) ;
#75324 = ORIENTED_EDGE ( 'NONE', *, *, #50887, .T. ) ;
#75325 = DIRECTION ( 'NONE',  ( 0.7071067811865487940, -0.7071067811865462405, -4.216150419019403701E-15 ) ) ;
#75326 = AXIS2_PLACEMENT_3D ( 'NONE', #99744, #21533, #155918 ) ;
#75327 = EDGE_CURVE ( 'NONE', #9830, #109222, #182238, .T. ) ;
#75328 = AXIS2_PLACEMENT_3D ( 'NONE', #216384, #37779, #195568 ) ;
#75329 = DIRECTION ( 'NONE',  ( 0.000000000000000000, 0.4999999999999478195, -0.8660254037844686836 ) ) ;
#75330 = CIRCLE ( 'NONE', #162798, 0.1000000000000124678 ) ;
#75331 = CARTESIAN_POINT ( 'NONE',  ( 23.15000000000000213, -8.596261682231833845, -76.45012751715033517 ) ) ;
#75332 = EDGE_CURVE ( 'NONE', #129819, #16537, #33213, .T. ) ;
#75333 = EDGE_CURVE ( 'NONE', #230954, #224326, #196038, .T. ) ;
#75334 = ORIENTED_EDGE ( 'NONE', *, *, #26394, .F. ) ;
#75335 = AXIS2_PLACEMENT_3D ( 'NONE', #98071, #35602, #197203 ) ;
#75336 = EDGE_CURVE ( 'NONE', #115457, #89961, #141488, .T. ) ;
#75337 = CARTESIAN_POINT ( 'NONE',  ( 18.59999999999999432, 77.86671491006937629, -124.7704322382422788 ) ) ;
#75338 = VERTEX_POINT ( 'NONE', #136024 ) ;
#75339 = DIRECTION ( 'NONE',  ( -0.000000000000000000, 1.000000000000000000, 6.982962677686266711E-15 ) ) ;
#75340 = CARTESIAN_POINT ( 'NONE',  ( -16.93211319090181632, 14.22327269246674852, -219.3152801208867118 ) ) ;
#75341 = DIRECTION ( 'NONE',  ( 0.000000000000000000, 0.9651348961777157509, -0.2617529984165031243 ) ) ;
#75342 = EDGE_CURVE ( 'NONE', #136435, #87098, #134745, .T. ) ;
#75343 = LINE ( 'NONE', #19186, #94089 ) ;
#75344 = PLANE ( 'NONE',  #154868 ) ;
#75345 = DIRECTION ( 'NONE',  ( 0.000000000000000000, 1.000000000000000000, 6.982962677686266711E-15 ) ) ;
#75346 = VECTOR ( 'NONE', #1219, 1000.000000000000000 ) ;
#75347 = ORIENTED_EDGE ( 'NONE', *, *, #74783, .F. ) ;
#75348 = CARTESIAN_POINT ( 'NONE',  ( -23.25000000000000000, 74.83412143252222393, -233.7087995678629966 ) ) ;
#75349 = DIRECTION ( 'NONE',  ( 0.000000000000000000, 0.000000000000000000, -1.000000000000000000 ) ) ;
#75351 = EDGE_CURVE ( 'NONE', #255544, #170158, #54011, .T. ) ;
#75350 = CARTESIAN_POINT ( 'NONE',  ( -18.59999999999999787, 11.65000000001115232, -79.25000000000004263 ) ) ;
#75352 = DIRECTION ( 'NONE',  ( 0.000000000000000000, -0.1298341882520022694, -0.9915357197604852679 ) ) ;
#75353 = DIRECTION ( 'NONE',  ( 1.000000000000000000, -0.000000000000000000, -0.000000000000000000 ) ) ;
#75354 = ORIENTED_EDGE ( 'NONE', *, *, #79129, .F. ) ;
#75355 = VERTEX_POINT ( 'NONE', #107820 ) ;
#75356 = CARTESIAN_POINT ( 'NONE',  ( 18.59999999999999076, 7.120270961708750512, -171.1595630418393625 ) ) ;
#75357 = DIRECTION ( 'NONE',  ( 1.000000000000000000, 0.000000000000000000, 0.000000000000000000 ) ) ;
#75358 = CARTESIAN_POINT ( 'NONE',  ( 21.05000000000000071, 11.65000000001115943, -33.60000000000000142 ) ) ;
#75359 = ADVANCED_FACE ( 'NONE', ( #213019 ), #199783, .F. ) ;
#75360 = VECTOR ( 'NONE', #99676, 1000.000000000000000 ) ;
#75361 = ORIENTED_EDGE ( 'NONE', *, *, #146778, .F. ) ;
#75362 = DIRECTION ( 'NONE',  ( 1.000000000000000000, 0.000000000000000000, 0.000000000000000000 ) ) ;
#75363 = DIRECTION ( 'NONE',  ( -1.000000000000000000, -0.000000000000000000, -0.000000000000000000 ) ) ;
#75364 = TOROIDAL_SURFACE ( 'NONE', #309, 0.2000000000000000111, 0.1000000000000000056 ) ;
#75365 = ORIENTED_EDGE ( 'NONE', *, *, #48407, .F. ) ;
#75366 = DIRECTION ( 'NONE',  ( -1.000000000000000000, 2.952720810173289112E-16, 2.061873921506763405E-30 ) ) ;
#75367 = CARTESIAN_POINT ( 'NONE',  ( 21.13507111622890022, 13.07883613358315245, -210.6878745673258493 ) ) ;
#75368 = CIRCLE ( 'NONE', #104525, 0.1000000000000045158 ) ;
#75369 = ORIENTED_EDGE ( 'NONE', *, *, #14671, .F. ) ;
#75370 = CARTESIAN_POINT ( 'NONE',  ( -21.00250684356853270, 12.97363049731598039, -205.3537238879905544 ) ) ;
#75371 = CIRCLE ( 'NONE', #208640, 0.09999999999999939493 ) ;
#75372 = VERTEX_POINT ( 'NONE', #127390 ) ;
#75373 = CYLINDRICAL_SURFACE ( 'NONE', #243346, 0.5000000000000004441 ) ;
#75374 = CYLINDRICAL_SURFACE ( 'NONE', #121468, 0.1000000000000028644 ) ;
#75375 = LINE ( 'NONE', #157487, #174240 ) ;
#75376 = CARTESIAN_POINT ( 'NONE',  ( 21.59780538579342490, 75.90102133041445143, -176.8701980144676043 ) ) ;
#75377 = DIRECTION ( 'NONE',  ( 0.000000000000000000, 0.2617529984165027912, 0.9651348961777157509 ) ) ;
#75378 = LINE ( 'NONE', #227041, #205438 ) ;
#75379 = CARTESIAN_POINT ( 'NONE',  ( 20.94999999999999574, 0.3813505302108621264, -209.0906591966561336 ) ) ;
#75380 = CARTESIAN_POINT ( 'NONE',  ( 23.14999999999999503, 64.35000000001146248, -42.93791325517834423 ) ) ;
#75382 = LINE ( 'NONE', #74107, #62364 ) ;
#75381 = CARTESIAN_POINT ( 'NONE',  ( -20.99142135623731065, 16.98881331171929787, -224.4946931418895701 ) ) ;
#75383 = EDGE_CURVE ( 'NONE', #160000, #241513, #87318, .T. ) ;
#75384 = DIRECTION ( 'NONE',  ( 1.000000000000000000, -2.952720810173289112E-16, -2.061873921506763405E-30 ) ) ;
#75385 = DIRECTION ( 'NONE',  ( -1.836970198721029934E-16, -1.000000000000000000, -6.982962677686266711E-15 ) ) ;
#75386 = FACE_OUTER_BOUND ( 'NONE', #181271, .T. ) ;
#75387 = CARTESIAN_POINT ( 'NONE',  ( 20.95568717954149562, 18.83659447889446170, -227.9769441489441704 ) ) ;
#75388 = AXIS2_PLACEMENT_3D ( 'NONE', #95886, #218394, #254912 ) ;
#75389 = EDGE_LOOP ( 'NONE', ( #172305, #246213, #118565, #53152 ) ) ;
#75390 = EDGE_CURVE ( 'NONE', #97822, #196712, #83201, .T. ) ;
#75391 = CIRCLE ( 'NONE', #171272, 0.5000000000000004441 ) ;
#75392 = FACE_OUTER_BOUND ( 'NONE', #200192, .T. ) ;
#75393 = LINE ( 'NONE', #16690, #7749 ) ;
#75394 = CIRCLE ( 'NONE', #46127, 0.1000000000000001860 ) ;
#75395 = VERTEX_POINT ( 'NONE', #16134 ) ;
#75397 =( BOUNDED_CURVE ( )  B_SPLINE_CURVE ( 3, ( #31676, #168642, #227265, #47330 ),
 .UNSPECIFIED., .F., .T. ) 
 B_SPLINE_CURVE_WITH_KNOTS ( ( 4, 4 ),
 ( 4.712388980384690562, 5.672655318024762749 ),
 .UNSPECIFIED. ) 
 CURVE ( )  GEOMETRIC_REPRESENTATION_ITEM ( )  RATIONAL_B_SPLINE_CURVE ( ( 1.000000000000000000, 0.9246222802177245237, 0.9246222802177245237, 1.000000000000000000 ) ) 
 REPRESENTATION_ITEM ( '' )  );
#75396 = AXIS2_PLACEMENT_3D ( 'NONE', #121223, #142023, #239857 ) ;
#75398 = CARTESIAN_POINT ( 'NONE',  ( -21.05000000000000071, 76.00000000001170974, -69.52310748452431710 ) ) ;
#75400 = ADVANCED_FACE ( 'NONE', ( #155656 ), #215579, .F. ) ;
#75399 = DIRECTION ( 'NONE',  ( 0.000000000000000000, 0.000000000000000000, 1.000000000000000000 ) ) ;
#75401 = DIRECTION ( 'NONE',  ( 0.000000000000000000, 0.2617529984164506107, 0.9651348961777299618 ) ) ;
#75402 = EDGE_CURVE ( 'NONE', #148418, #19570, #153094, .T. ) ;
#75403 = VECTOR ( 'NONE', #240887, 1000.000000000000114 ) ;
#75404 = VERTEX_POINT ( 'NONE', #94345 ) ;
#75405 = DIRECTION ( 'NONE',  ( 0.000000000000000000, -0.7397360091702823714, 0.6728971962616756564 ) ) ;
#75406 = ORIENTED_EDGE ( 'NONE', *, *, #51725, .T. ) ;
#75407 = DIRECTION ( 'NONE',  ( 0.000000000000000000, 6.982962677686266711E-15, -1.000000000000000000 ) ) ;
#75408 = DIRECTION ( 'NONE',  ( -1.000000000000000000, 0.000000000000000000, 0.000000000000000000 ) ) ;
#75409 = CIRCLE ( 'NONE', #67002, 0.1000000000000028644 ) ;
#75410 = AXIS2_PLACEMENT_3D ( 'NONE', #217803, #56167, #135706 ) ;
#75411 = AXIS2_PLACEMENT_3D ( 'NONE', #217331, #197784, #199078 ) ;
#75412 = AXIS2_PLACEMENT_3D ( 'NONE', #63271, #24171, #121973 ) ;
#75413 = VERTEX_POINT ( 'NONE', #116499 ) ;
#75414 = CARTESIAN_POINT ( 'NONE',  ( 18.59999999999997655, 77.16412189325258453, -28.10825939895270764 ) ) ;
#75415 = ORIENTED_EDGE ( 'NONE', *, *, #157341, .T. ) ;
#75416 = FACE_OUTER_BOUND ( 'NONE', #3382, .T. ) ;
#75417 = CARTESIAN_POINT ( 'NONE',  ( 21.08804582317324261, 67.12183383292016003, -124.1731076551190114 ) ) ;
#75418 = DIRECTION ( 'NONE',  ( 0.000000000000000000, 0.000000000000000000, 1.000000000000000000 ) ) ;
#75419 = DIRECTION ( 'NONE',  ( 4.026293107431335996E-15, -0.8700118002898359348, 0.4930308989875165082 ) ) ;
#75420 = CARTESIAN_POINT ( 'NONE',  ( -20.54999999999999716, 1.115600667400684642E-11, -67.00000000000000000 ) ) ;
#75421 = AXIS2_PLACEMENT_3D ( 'NONE', #179761, #117211, #139312 ) ;
#75422 = CARTESIAN_POINT ( 'NONE',  ( -23.15000000000000213, 4.150000000011156764, -54.64999999999999858 ) ) ;
#75423 = DIRECTION ( 'NONE',  ( 0.000000000000000000, 0.000000000000000000, 1.000000000000000000 ) ) ;
#75424 = DIRECTION ( 'NONE',  ( 0.000000000000000000, -1.000000000000000000, 0.000000000000000000 ) ) ;
#75426 = ORIENTED_EDGE ( 'NONE', *, *, #242302, .F. ) ;
#75425 = CARTESIAN_POINT ( 'NONE',  ( 21.05000000000041993, 69.65564095796835886, -103.0379631194186345 ) ) ;
#75427 = ORIENTED_EDGE ( 'NONE', *, *, #224895, .F. ) ;
#75429 = CARTESIAN_POINT ( 'NONE',  ( 22.19999999999999929, -1.467286812112899463, 28.00000000000000000 ) ) ;
#75428 = CARTESIAN_POINT ( 'NONE',  ( -18.69999999999999929, -8.250000000000005329, 16.39999999999999858 ) ) ;
#75430 = ORIENTED_EDGE ( 'NONE', *, *, #223660, .F. ) ;
#75432 = ORIENTED_EDGE ( 'NONE', *, *, #78505, .F. ) ;
#75431 = PRESENTATION_STYLE_ASSIGNMENT (( #94950 ) ) ;
#75433 = EDGE_LOOP ( 'NONE', ( #92386, #153761, #2985, #156093 ) ) ;
#75434 = ADVANCED_FACE ( 'NONE', ( #175230 ), #133132, .T. ) ;
#75435 = CARTESIAN_POINT ( 'NONE',  ( 20.95000000000005258, 66.25000000001119815, -4.523107484524794053 ) ) ;
#75436 = DIRECTION ( 'NONE',  ( 1.000000000000000000, 0.000000000000000000, 0.000000000000000000 ) ) ;
#75437 = DIRECTION ( 'NONE',  ( -1.000000000000000000, 0.000000000000000000, 0.000000000000000000 ) ) ;
#75438 = DIRECTION ( 'NONE',  ( 1.000000000000000000, 0.000000000000000000, 0.000000000000000000 ) ) ;
#75439 = DIRECTION ( 'NONE',  ( 0.000000000000000000, 0.9893560106964510714, -0.1455152366551481502 ) ) ;
#75440 = CYLINDRICAL_SURFACE ( 'NONE', #118709, 0.1000000000000013933 ) ;
#75442 = ADVANCED_FACE ( 'NONE', ( #112646 ), #13550, .T. ) ;
#75441 = DIRECTION ( 'NONE',  ( -1.000000000000000000, 0.000000000000000000, 0.000000000000000000 ) ) ;
#75443 = AXIS2_PLACEMENT_3D ( 'NONE', #165271, #244799, #201832 ) ;
#75444 = ADVANCED_FACE ( 'NONE', ( #28327 ), #20716, .F. ) ;
#75445 = CARTESIAN_POINT ( 'NONE',  ( 21.14999999999999858, 76.10000000001214460, -136.5231074845242745 ) ) ;
#75446 = VERTEX_POINT ( 'NONE', #193479 ) ;
#75447 = ORIENTED_EDGE ( 'NONE', *, *, #965, .F. ) ;
#75448 = DIRECTION ( 'NONE',  ( 0.000000000000000000, 0.9126074666063660468, 0.4088369013363524762 ) ) ;
#75449 = ORIENTED_EDGE ( 'NONE', *, *, #169768, .F. ) ;
#75450 = LINE ( 'NONE', #237062, #92764 ) ;
#75451 = VERTEX_POINT ( 'NONE', #74836 ) ;
#75452 = CARTESIAN_POINT ( 'NONE',  ( 18.36493879433275822, -9.500000806189802915, -40.42214866035106269 ) ) ;
#75453 = ADVANCED_FACE ( 'NONE', ( #154377 ), #233871, .T. ) ;
#75454 = AXIS2_PLACEMENT_3D ( 'NONE', #238166, #218596, #159954 ) ;
#75455 = LINE ( 'NONE', #154987, #17785 ) ;
#75456 = CARTESIAN_POINT ( 'NONE',  ( -23.15000000000000213, -7.176961358819843539, -212.6889627706600834 ) ) ;
#75458 = ORIENTED_EDGE ( 'NONE', *, *, #108463, .F. ) ;
#75457 = CARTESIAN_POINT ( 'NONE',  ( 18.58719872626880942, -9.566644397587477755, -207.8224781963969860 ) ) ;
#75459 = EDGE_CURVE ( 'NONE', #134685, #43942, #203846, .T. ) ;
#75460 = CYLINDRICAL_SURFACE ( 'NONE', #41571, 0.09999999999999811817 ) ;
#75461 = ORIENTED_EDGE ( 'NONE', *, *, #182618, .T. ) ;
#75462 = EDGE_CURVE ( 'NONE', #25217, #34176, #237185, .T. ) ;
#75463 = CARTESIAN_POINT ( 'NONE',  ( -18.47130263965431496, -9.471155585952907074, -207.6834047654772348 ) ) ;
#75464 = DIRECTION ( 'NONE',  ( 0.000000000000000000, -0.5378121776619205763, 0.8430646840892713767 ) ) ;
#75465 = CARTESIAN_POINT ( 'NONE',  ( -20.94999999999999929, 0.000000000000000000, -29.40000000000000213 ) ) ;
#75466 = DIRECTION ( 'NONE',  ( 0.000000000000000000, 0.1332476588733589318, 0.9910827722268050755 ) ) ;
#75467 = EDGE_CURVE ( 'NONE', #233607, #23909, #160787, .T. ) ;
#75468 = CARTESIAN_POINT ( 'NONE',  ( 19.75857864376268935, 11.75000000001115907, -125.3500000000000512 ) ) ;
#75469 = ORIENTED_EDGE ( 'NONE', *, *, #38397, .F. ) ;
#75471 = CARTESIAN_POINT ( 'NONE',  ( -18.41817142474035762, 85.49870306661347286, -29.41914199688725162 ) ) ;
#75470 = CIRCLE ( 'NONE', #171167, 0.09999999999998898659 ) ;
#75472 = VERTEX_POINT ( 'NONE', #38247 ) ;
#75474 = VERTEX_POINT ( 'NONE', #219422 ) ;
#75473 = CYLINDRICAL_SURFACE ( 'NONE', #54714, 0.09999999999999939493 ) ;
#75475 = VECTOR ( 'NONE', #11086, 1000.000000000000000 ) ;
#75476 = CARTESIAN_POINT ( 'NONE',  ( -19.89999999999999858, 1.350000000000000089, 21.90000000000000213 ) ) ;
#75477 = AXIS2_PLACEMENT_3D ( 'NONE', #228077, #246351, #67709 ) ;
#75478 = CARTESIAN_POINT ( 'NONE',  ( -22.57848426163148048, -2.504590758878124213, -189.5199776337204867 ) ) ;
#75479 = VERTEX_POINT ( 'NONE', #142463 ) ;
#75480 = DIRECTION ( 'NONE',  ( 2.952720810173289112E-16, -1.000000000000000000, 0.000000000000000000 ) ) ;
#75481 = ADVANCED_FACE ( 'NONE', ( #79895 ), #240301, .T. ) ;
#75482 = CYLINDRICAL_SURFACE ( 'NONE', #40652, 0.1000000000000013933 ) ;
#75483 = FACE_OUTER_BOUND ( 'NONE', #7191, .T. ) ;
#75485 = ORIENTED_EDGE ( 'NONE', *, *, #58772, .T. ) ;
#75484 = DIRECTION ( 'NONE',  ( -1.000000000000000000, 0.000000000000000000, -0.000000000000000000 ) ) ;
#75486 = FACE_OUTER_BOUND ( 'NONE', #246917, .T. ) ;
#75487 = AXIS2_PLACEMENT_3D ( 'NONE', #229729, #71951, #151506 ) ;
#75488 = ORIENTED_EDGE ( 'NONE', *, *, #173922, .T. ) ;
#75489 = DIRECTION ( 'NONE',  ( -1.000000000000000000, -3.265361837132813093E-16, 0.000000000000000000 ) ) ;
#75490 = DIRECTION ( 'NONE',  ( 0.000000000000000000, 0.9875102702516471709, 0.1575546449569757979 ) ) ;
#75491 = CARTESIAN_POINT ( 'NONE',  ( -18.59999999999999787, -1.866714910046153308, -112.2526752462820525 ) ) ;
#75492 = DIRECTION ( 'NONE',  ( -0.7071067811865462405, 0.3338907855510739875, 0.6233112732207629625 ) ) ;
#75493 = ORIENTED_EDGE ( 'NONE', *, *, #27347, .F. ) ;
#75494 = DIRECTION ( 'NONE',  ( 0.000000000000000000, -0.9915357197604892647, 0.1298341882519715440 ) ) ;
#75495 = CARTESIAN_POINT ( 'NONE',  ( -21.05000000000000071, 0.2428138352382497867, -200.9114032742886309 ) ) ;
#75496 = CARTESIAN_POINT ( 'NONE',  ( -16.95709691156394427, 9.950000000011280932, -46.16005756250920911 ) ) ;
#75497 = ORIENTED_EDGE ( 'NONE', *, *, #179678, .F. ) ;
#75498 = CARTESIAN_POINT ( 'NONE',  ( 20.72390388899077607, 58.97664953679249322, -225.8337075495444992 ) ) ;
#75499 = CARTESIAN_POINT ( 'NONE',  ( 20.94999999999999929, 2.388061258337340615E-16, -31.59999999999999787 ) ) ;
#75500 = AXIS2_PLACEMENT_3D ( 'NONE', #69717, #30596, #125810 ) ;
#75501 = AXIS2_PLACEMENT_3D ( 'NONE', #55769, #96208, #214879 ) ;
#75502 = ORIENTED_EDGE ( 'NONE', *, *, #177803, .T. ) ;
#75503 = CARTESIAN_POINT ( 'NONE',  ( -16.97683809663752186, 66.15000000001261071, -190.1207434663279514 ) ) ;
#75504 = DIRECTION ( 'NONE',  ( 0.000000000000000000, 0.000000000000000000, 1.000000000000000000 ) ) ;
#75505 = CARTESIAN_POINT ( 'NONE',  ( 23.04999999999999716, 61.13752757784637026, -224.6182967272386009 ) ) ;
#75506 = ADVANCED_FACE ( 'NONE', ( #177775 ), #199900, .F. ) ;
#75507 = ORIENTED_EDGE ( 'NONE', *, *, #95977, .T. ) ;
#75508 = ORIENTED_EDGE ( 'NONE', *, *, #88720, .F. ) ;
#75509 = CARTESIAN_POINT ( 'NONE',  ( -18.39999999999999858, 85.40000000001174385, -81.27310748452426026 ) ) ;
#75510 = ORIENTED_EDGE ( 'NONE', *, *, #129265, .F. ) ;
#75512 = ORIENTED_EDGE ( 'NONE', *, *, #194657, .T. ) ;
#75511 = DIRECTION ( 'NONE',  ( 1.186688945009009831E-16, -1.000000000000000000, 0.000000000000000000 ) ) ;
#75513 = EDGE_CURVE ( 'NONE', #102386, #102873, #187494, .T. ) ;
#75516 = VERTEX_POINT ( 'NONE', #239011 ) ;
#75515 = VERTEX_POINT ( 'NONE', #159483 ) ;
#75514 = DIRECTION ( 'NONE',  ( 1.000000000000000000, 0.000000000000000000, 0.000000000000000000 ) ) ;
#75517 = EDGE_CURVE ( 'NONE', #42156, #117767, #162553, .T. ) ;
#75518 = EDGE_CURVE ( 'NONE', #54887, #72537, #87494, .T. ) ;
#75519 = DIRECTION ( 'NONE',  ( 0.000000000000000000, -0.9998779222360104635, -0.01562499999996343723 ) ) ;
#75520 = CARTESIAN_POINT ( 'NONE',  ( -16.87998658237730965, 12.45949613983442994, -211.4516352247128168 ) ) ;
#75521 = CARTESIAN_POINT ( 'NONE',  ( -18.50000000000000000, -1.637172712970379918, -11.58215336547201701 ) ) ;
#75522 = CARTESIAN_POINT ( 'NONE',  ( 21.04999999999914806, 65.49746832288764153, -195.9642776674505456 ) ) ;
#75523 = CARTESIAN_POINT ( 'NONE',  ( -20.94999999999999929, 76.00000000001170974, -69.52310748452431710 ) ) ;
#75524 = ORIENTED_EDGE ( 'NONE', *, *, #250129, .T. ) ;
#75525 = ORIENTED_EDGE ( 'NONE', *, *, #57623, .T. ) ;
#75526 = EDGE_LOOP ( 'NONE', ( #66702, #128592 ) ) ;
#75527 = FACE_OUTER_BOUND ( 'NONE', #158268, .T. ) ;
#75529 = VERTEX_POINT ( 'NONE', #201160 ) ;
#75528 = LINE ( 'NONE', #190336, #45372 ) ;
#75530 = CARTESIAN_POINT ( 'NONE',  ( -20.64999999999999858, 85.00000000001197975, -112.9170766071766820 ) ) ;
#75531 = ORIENTED_EDGE ( 'NONE', *, *, #224822, .F. ) ;
#75532 = EDGE_CURVE ( 'NONE', #138363, #247713, #20911, .T. ) ;
#75534 = CARTESIAN_POINT ( 'NONE',  ( -18.40000000000000213, 61.34848953995435039, -212.6564661897791098 ) ) ;
#75533 = VECTOR ( 'NONE', #155239, 999.9999999999998863 ) ;
#75535 = ORIENTED_EDGE ( 'NONE', *, *, #46532, .T. ) ;
#75536 = LINE ( 'NONE', #31294, #204198 ) ;
#75537 = EDGE_CURVE ( 'NONE', #156856, #86816, #145761, .T. ) ;
#75538 = AXIS2_PLACEMENT_3D ( 'NONE', #130806, #210361, #192090 ) ;
#75540 = ORIENTED_EDGE ( 'NONE', *, *, #62317, .F. ) ;
#75539 = PRODUCT_DEFINITION ( 'UNKNOWN', '', #44678, #180909 ) ;
#75541 = CARTESIAN_POINT ( 'NONE',  ( -23.25000000000000000, 76.00000000001270450, -207.6731074845243370 ) ) ;
#75542 = DIRECTION ( 'NONE',  ( 1.000000000000000000, 0.000000000000000000, 0.000000000000000000 ) ) ;
#75544 = EDGE_LOOP ( 'NONE', ( #222201, #75723, #76386, #191385, #49814 ) ) ;
#75543 = ORIENTED_EDGE ( 'NONE', *, *, #133988, .F. ) ;
#75545 = EDGE_LOOP ( 'NONE', ( #116498, #76618, #133524, #20824 ) ) ;
#75547 = DIRECTION ( 'NONE',  ( 0.000000000000000000, -1.000000000000000000, 0.000000000000000000 ) ) ;
#75546 = AXIS2_PLACEMENT_3D ( 'NONE', #194926, #18829, #16298 ) ;
#75548 = ORIENTED_EDGE ( 'NONE', *, *, #180110, .T. ) ;
#75549 = VERTEX_POINT ( 'NONE', #120382 ) ;
#75550 = ADVANCED_FACE ( 'NONE', ( #100735 ), #26, .F. ) ;
#75551 = DIRECTION ( 'NONE',  ( 0.000000000000000000, 0.2128009952263403282, -0.9770955615653358350 ) ) ;
#75552 = VECTOR ( 'NONE', #183722, 1000.000000000000000 ) ;
#75554 = ORIENTED_EDGE ( 'NONE', *, *, #234032, .T. ) ;
#75553 = CARTESIAN_POINT ( 'NONE',  ( 18.46932045258644450, -9.670685200254593994, -107.1738603729966997 ) ) ;
#75555 = EDGE_CURVE ( 'NONE', #34114, #103572, #61653, .T. ) ;
#75556 = DIRECTION ( 'NONE',  ( 0.000000000000000000, -0.000000000000000000, -1.000000000000000000 ) ) ;
#75557 = EDGE_CURVE ( 'NONE', #80255, #257282, #254092, .T. ) ;
#75559 = FACE_OUTER_BOUND ( 'NONE', #31489, .T. ) ;
#75558 = DIRECTION ( 'NONE',  ( -1.000000000000000000, -3.265361837132813093E-16, 0.000000000000000000 ) ) ;
#75560 = DIRECTION ( 'NONE',  ( 0.000000000000000000, 2.891205793294679805E-16, -1.000000000000000000 ) ) ;
#75561 = CYLINDRICAL_SURFACE ( 'NONE', #98504, 0.1000000000000090400 ) ;
#75562 = DIRECTION ( 'NONE',  ( -0.000000000000000000, -0.000000000000000000, 1.000000000000000000 ) ) ;
#75563 = VERTEX_POINT ( 'NONE', #42113 ) ;
#75564 = AXIS2_PLACEMENT_3D ( 'NONE', #77445, #114019, #76175 ) ;
#75565 = EDGE_LOOP ( 'NONE', ( #192912, #241981, #228467, #175000 ) ) ;
#75566 = CYLINDRICAL_SURFACE ( 'NONE', #53871, 0.1000000000000024342 ) ;
#75567 = DIRECTION ( 'NONE',  ( 0.000000000000000000, 0.000000000000000000, 1.000000000000000000 ) ) ;
#75568 = DIRECTION ( 'NONE',  ( 0.000000000000000000, 0.8814952561688438326, -0.4721928772777334582 ) ) ;
#75569 = ADVANCED_FACE ( 'NONE', ( #39563 ), #83389, .T. ) ;
#75571 = ORIENTED_EDGE ( 'NONE', *, *, #138421, .F. ) ;
#75570 = VECTOR ( 'NONE', #41749, 1000.000000000000000 ) ;
#75572 = CARTESIAN_POINT ( 'NONE',  ( -21.05000000000000071, -11.48912529306489994, -131.0000000000000284 ) ) ;
#75573 = AXIS2_PLACEMENT_3D ( 'NONE', #27368, #224228, #28663 ) ;
#75574 = DIRECTION ( 'NONE',  ( -1.000000000000000000, 0.000000000000000000, 0.000000000000000000 ) ) ;
#75575 = LINE ( 'NONE', #192935, #250822 ) ;
#75576 = VERTEX_POINT ( 'NONE', #241574 ) ;
#75577 = EDGE_LOOP ( 'NONE', ( #204099, #223180, #257708, #218708 ) ) ;
#75578 = VECTOR ( 'NONE', #217060, 1000.000000000000114 ) ;
#75579 = FACE_OUTER_BOUND ( 'NONE', #179384, .T. ) ;
#75580 = CARTESIAN_POINT ( 'NONE',  ( -20.54999999999999716, 7.250000000011155521, -121.6500000000000341 ) ) ;
#75581 = VERTEX_POINT ( 'NONE', #156930 ) ;
#75582 = CARTESIAN_POINT ( 'NONE',  ( -23.25000000000000000, -1.149570369575693807, -41.31591248450196474 ) ) ;
#75583 = ORIENTED_EDGE ( 'NONE', *, *, #184521, .F. ) ;
#75584 = CARTESIAN_POINT ( 'NONE',  ( 20.99999999999999645, 30.11188998467138234, -234.9833440560338147 ) ) ;
#75586 = CIRCLE ( 'NONE', #221274, 0.1000000000000016431 ) ;
#75585 = DIRECTION ( 'NONE',  ( 0.000000000000000000, -1.000000000000000000, -7.109473446599835262E-15 ) ) ;
#75588 = CARTESIAN_POINT ( 'NONE',  ( 23.14999999999999858, 78.00000000001170974, -69.52310748452430289 ) ) ;
#75587 = CARTESIAN_POINT ( 'NONE',  ( 21.14999999999999503, -11.64999999998883595, -36.39999999999999858 ) ) ;
#75589 = CARTESIAN_POINT ( 'NONE',  ( 18.51024323315077069, 65.68895814178291914, -164.5026557862138645 ) ) ;
#75590 = EDGE_CURVE ( 'NONE', #53354, #213752, #4295, .T. ) ;
#75591 = CARTESIAN_POINT ( 'NONE',  ( 18.49999999999998934, 69.35000000001186038, -90.67310748452435121 ) ) ;
#75592 = LINE ( 'NONE', #135516, #94118 ) ;
#75593 = CIRCLE ( 'NONE', #204721, 0.1000000000000000472 ) ;
#75594 = AXIS2_PLACEMENT_3D ( 'NONE', #155897, #133726, #73791 ) ;
#75596 = ORIENTED_EDGE ( 'NONE', *, *, #203419, .F. ) ;
#75595 = VERTEX_POINT ( 'NONE', #216865 ) ;
#75597 = ORIENTED_EDGE ( 'NONE', *, *, #172474, .T. ) ;
#75598 = ADVANCED_FACE ( 'NONE', ( #26397 ), #70978, .T. ) ;
#75599 = DIRECTION ( 'NONE',  ( 0.000000000000000000, 0.000000000000000000, 1.000000000000000000 ) ) ;
#75600 = CARTESIAN_POINT ( 'NONE',  ( 22.43288208788031568, 0.004899854885382672054, 11.64965184371907192 ) ) ;
#75601 = DIRECTION ( 'NONE',  ( 1.000000000000000000, 0.000000000000000000, 0.000000000000000000 ) ) ;
#75602 = DIRECTION ( 'NONE',  ( 0.000000000000000000, 0.2617529984165152257, 0.9651348961777124202 ) ) ;
#75604 = DIRECTION ( 'NONE',  ( -1.000000000000000000, -0.000000000000000000, -0.000000000000000000 ) ) ;
#75603 = DIRECTION ( 'NONE',  ( -0.000000000000000000, -0.4721928772777346239, -0.8814952561688430555 ) ) ;
#75605 = DIRECTION ( 'NONE',  ( 0.000000000000000000, 0.000000000000000000, -1.000000000000000000 ) ) ;
#75606 = ORIENTED_EDGE ( 'NONE', *, *, #58330, .T. ) ;
#75607 = EDGE_CURVE ( 'NONE', #248699, #89072, #112477, .T. ) ;
#75608 = DIRECTION ( 'NONE',  ( 1.000000000000000000, -1.335000415235278971E-16, 2.979993593738921214E-16 ) ) ;
#75609 = ORIENTED_EDGE ( 'NONE', *, *, #28797, .F. ) ;
#75610 = EDGE_LOOP ( 'NONE', ( #24572, #115232, #139383, #165844 ) ) ;
#75611 = DIRECTION ( 'NONE',  ( -1.000000000000000000, 0.000000000000000000, 0.000000000000000000 ) ) ;
#75612 = DIRECTION ( 'NONE',  ( 0.000000000000000000, -6.982962677686266711E-15, 1.000000000000000000 ) ) ;
#75613 = CARTESIAN_POINT ( 'NONE',  ( 21.00023020733504708, 76.00000000001273293, -209.9139767297927222 ) ) ;
#75614 = DIRECTION ( 'NONE',  ( 0.000000000000000000, 0.000000000000000000, -1.000000000000000000 ) ) ;
#75615 = EDGE_CURVE ( 'NONE', #135478, #168421, #33387, .T. ) ;
#75616 = CARTESIAN_POINT ( 'NONE',  ( -23.15000000000000213, 2.000000000011154189, -121.2753780772379315 ) ) ;
#75617 = ADVANCED_FACE ( 'NONE', ( #223280 ), #6815, .T. ) ;
#75618 = VERTEX_POINT ( 'NONE', #247989 ) ;
#75619 = ORIENTED_EDGE ( 'NONE', *, *, #50577, .T. ) ;
#75620 = DIRECTION ( 'NONE',  ( 1.000000000000000000, 0.000000000000000000, 0.000000000000000000 ) ) ;
#75621 = DIRECTION ( 'NONE',  ( 1.000000000000000000, 3.265361837132813093E-16, -0.000000000000000000 ) ) ;
#75622 = PLANE ( 'NONE',  #173060 ) ;
#75623 = DIRECTION ( 'NONE',  ( 0.000000000000000000, 0.000000000000000000, 1.000000000000000000 ) ) ;
#75624 = DIRECTION ( 'NONE',  ( 0.000000000000000000, -7.056502275159890043E-15, 1.000000000000000000 ) ) ;
#75625 = DIRECTION ( 'NONE',  ( 0.000000000000000000, 6.982962677686266711E-15, -1.000000000000000000 ) ) ;
#75626 = VECTOR ( 'NONE', #151854, 1000.000000000000000 ) ;
#75627 = DIRECTION ( 'NONE',  ( 0.000000000000000000, -1.000000000000000000, 0.000000000000000000 ) ) ;
#75629 = CYLINDRICAL_SURFACE ( 'NONE', #112259, 1.749999999999999778 ) ;
#75628 = DIRECTION ( 'NONE',  ( -1.000000000000000000, -0.000000000000000000, -0.000000000000000000 ) ) ;
#75630 = CARTESIAN_POINT ( 'NONE',  ( 20.12500000000000000, 9.750000000011153745, -41.61177128211428311 ) ) ;
#75631 = DIRECTION ( 'NONE',  ( 1.000000000000000000, 0.000000000000000000, 0.000000000000000000 ) ) ;
#75632 = DIRECTION ( 'NONE',  ( -3.265361837132813093E-16, 1.000000000000000000, 0.000000000000000000 ) ) ;
#75633 = DIRECTION ( 'NONE',  ( -2.952720810173289605E-16, -1.000000000000000000, -7.086529944415894657E-15 ) ) ;
#75635 = EDGE_LOOP ( 'NONE', ( #127178, #125542, #46258 ) ) ;
#75634 = CARTESIAN_POINT ( 'NONE',  ( 18.59999999999999076, 69.35000000001254250, -182.2731074845244166 ) ) ;
#75636 = EDGE_CURVE ( 'NONE', #245973, #50347, #12524, .T. ) ;
#75637 = VECTOR ( 'NONE', #43537, 1000.000000000000000 ) ;
#75638 = ADVANCED_FACE ( 'NONE', ( #188033 ), #154208, .T. ) ;
#75639 = CARTESIAN_POINT ( 'NONE',  ( -20.64999999999999858, 7.150000000011155876, -121.6500000000000341 ) ) ;
#75640 = VERTEX_POINT ( 'NONE', #208871 ) ;
#75641 = CARTESIAN_POINT ( 'NONE',  ( -20.64999999999999858, 6.759468328187065111, -212.0650163994647812 ) ) ;
#75642 = EDGE_CURVE ( 'NONE', #77215, #76792, #143750, .T. ) ;
#75643 = VERTEX_POINT ( 'NONE', #47204 ) ;
#75644 = DIRECTION ( 'NONE',  ( -1.000000000000000000, 0.000000000000000000, 0.000000000000000000 ) ) ;
#75646 = ADVANCED_FACE ( 'NONE', ( #145029 ), #146315, .F. ) ;
#75645 = CARTESIAN_POINT ( 'NONE',  ( 12.68104795156993880, 9.396533993965071829, -84.90593977917332325 ) ) ;
#75647 = CARTESIAN_POINT ( 'NONE',  ( 20.94999999999999929, 65.27628289530507288, -191.3731074845244393 ) ) ;
#75648 = AXIS2_PLACEMENT_3D ( 'NONE', #46398, #188487, #127240 ) ;
#75649 = TOROIDAL_SURFACE ( 'NONE', #221344, 4.099999999999999645, 0.1000000000000000056 ) ;
#75650 = DIRECTION ( 'NONE',  ( 1.000000000000000000, -0.000000000000000000, -0.000000000000000000 ) ) ;
#75651 = CARTESIAN_POINT ( 'NONE',  ( 18.50000000000046541, 10.44006789214481579, -24.76711774888623196 ) ) ;
#75653 = CARTESIAN_POINT ( 'NONE',  ( -23.25000000000000000, 64.25000000001142553, -36.02310748452440237 ) ) ;
#75652 = AXIS2_PLACEMENT_3D ( 'NONE', #19561, #93945, #253016 ) ;
#75654 = ORIENTED_EDGE ( 'NONE', *, *, #71412, .T. ) ;
#75655 = DIRECTION ( 'NONE',  ( 0.000000000000000000, 0.9770955615653316162, 0.2128009952263604232 ) ) ;
#75657 = ORIENTED_EDGE ( 'NONE', *, *, #10294, .F. ) ;
#75656 = CARTESIAN_POINT ( 'NONE',  ( 21.05000000000000071, 70.15000000001178648, -79.65560470880227228 ) ) ;
#75658 = DIRECTION ( 'NONE',  ( 0.7071067811865475727, -0.7071067811865475727, -5.142139384388981164E-15 ) ) ;
#75659 = DIRECTION ( 'NONE',  ( -1.000000000000000000, -0.000000000000000000, -0.000000000000000000 ) ) ;
#75660 = ADVANCED_FACE ( 'NONE', ( #87617 ), #158292, .F. ) ;
#75661 = DIRECTION ( 'NONE',  ( 0.7071067811865127117, 0.7071067811865821007, 0.000000000000000000 ) ) ;
#75662 = ORIENTED_EDGE ( 'NONE', *, *, #212952, .T. ) ;
#75663 = CARTESIAN_POINT ( 'NONE',  ( -16.84793658983408449, 66.05000000001261640, -190.7894608067139472 ) ) ;
#75664 = ADVANCED_FACE ( 'NONE', ( #69379 ), #164618, .F. ) ;
#75665 = APPLICATION_PROTOCOL_DEFINITION ( 'draft international standard', 'automotive_design', 1998, #25723 ) ;
#75666 = FACE_OUTER_BOUND ( 'NONE', #84820, .T. ) ;
#75667 = CARTESIAN_POINT ( 'NONE',  ( -18.49719636458544869, 85.44636535923997656, -95.95149361464065407 ) ) ;
#75668 = AXIS2_PLACEMENT_3D ( 'NONE', #74098, #149774, #213561 ) ;
#75669 = VERTEX_POINT ( 'NONE', #244129 ) ;
#75670 = CARTESIAN_POINT ( 'NONE',  ( -18.59999999999999787, 11.65000000001115232, -40.51480577065400013 ) ) ;
#75671 = CARTESIAN_POINT ( 'NONE',  ( 22.39999999999999503, 55.86476422312859569, -232.8760422647022494 ) ) ;
#75672 = ORIENTED_EDGE ( 'NONE', *, *, #147739, .T. ) ;
#75673 = ORIENTED_EDGE ( 'NONE', *, *, #68146, .T. ) ;
#75674 = DIRECTION ( 'NONE',  ( 0.000000000000000000, 0.000000000000000000, -1.000000000000000000 ) ) ;
#75675 = FACE_OUTER_BOUND ( 'NONE', #7126, .T. ) ;
#75677 = CARTESIAN_POINT ( 'NONE',  ( -16.91049119928362998, 30.23428993624846584, -234.8220231485292118 ) ) ;
#75676 = AXIS2_PLACEMENT_3D ( 'NONE', #238977, #77309, #257188 ) ;
#75678 = CIRCLE ( 'NONE', #83983, 0.4000000000000114575 ) ;
#75681 = DIRECTION ( 'NONE',  ( -1.000000000000000000, 0.000000000000000000, 0.000000000000000000 ) ) ;
#75680 = CIRCLE ( 'NONE', #75845, 0.1000000000000022676 ) ;
#75679 = CARTESIAN_POINT ( 'NONE',  ( 20.27550659511088682, 22.63149853307782422, -231.5820423879664247 ) ) ;
#75682 = CARTESIAN_POINT ( 'NONE',  ( 20.91682497891422798, 65.67736539654895012, -30.46251168765720152 ) ) ;
#75683 = DIRECTION ( 'NONE',  ( -1.000000000000000000, -0.000000000000000000, -0.000000000000000000 ) ) ;
#75684 = LINE ( 'NONE', #119961, #200411 ) ;
#75685 = CARTESIAN_POINT ( 'NONE',  ( -18.60000000000000142, 47.07326788871597500, -255.0992659944397758 ) ) ;
#75686 = ORIENTED_EDGE ( 'NONE', *, *, #136196, .F. ) ;
#75687 = EDGE_CURVE ( 'NONE', #83024, #200313, #166661, .T. ) ;
#75688 = VERTEX_POINT ( 'NONE', #186756 ) ;
#75689 = DIRECTION ( 'NONE',  ( 0.000000000000000000, -0.7106264324241464703, 0.7035695228903324772 ) ) ;
#75690 = CARTESIAN_POINT ( 'NONE',  ( -21.14999999999999858, 7.128833340093095217, -233.7327013124392749 ) ) ;
#75692 = LINE ( 'NONE', #213898, #228512 ) ;
#75691 = DIRECTION ( 'NONE',  ( -1.000000000000000000, 3.265361837132813093E-16, 2.280189983783949500E-30 ) ) ;
#75693 = CARTESIAN_POINT ( 'NONE',  ( -21.64999999999999858, 9.350000000011133849, -113.1500000000000341 ) ) ;
#75694 = CARTESIAN_POINT ( 'NONE',  ( -20.94999999999999929, 12.97363049771892207, -205.3537238898406940 ) ) ;
#75695 = DIRECTION ( 'NONE',  ( 1.186688945009010077E-16, 1.000000000000000000, 6.982962677686266711E-15 ) ) ;
#75696 = VERTEX_POINT ( 'NONE', #44667 ) ;
#75698 = ORIENTED_EDGE ( 'NONE', *, *, #30563, .F. ) ;
#75697 = AXIS2_PLACEMENT_3D ( 'NONE', #218363, #180554, #99691 ) ;
#75699 = DIRECTION ( 'NONE',  ( 0.000000000000000000, 1.000000000000000000, 6.938893903907222067E-15 ) ) ;
#75700 = ORIENTED_EDGE ( 'NONE', *, *, #218992, .T. ) ;
#75701 = ADVANCED_FACE ( 'NONE', ( #207605 ), #148911, .T. ) ;
#75702 = DIRECTION ( 'NONE',  ( 0.000000000000000000, 0.9090645160163607352, 0.4166553800443956734 ) ) ;
#75703 = DIRECTION ( 'NONE',  ( 0.000000000000000000, -0.2128009952263603954, 0.9770955615653315052 ) ) ;
#75704 = DIRECTION ( 'NONE',  ( -0.5932847527679296906, 0.3801118060259212061, 0.7095972217059539622 ) ) ;
#75705 = EDGE_LOOP ( 'NONE', ( #207923, #160529, #151467, #24540 ) ) ;
#75706 = CARTESIAN_POINT ( 'NONE',  ( 20.85000000000000142, 6.933893972126341509, -37.28564583437357527 ) ) ;
#75707 = ORIENTED_EDGE ( 'NONE', *, *, #57878, .T. ) ;
#75708 = DIRECTION ( 'NONE',  ( 0.000000000000000000, -0.2558827019434133376, 0.9667078373770113808 ) ) ;
#75709 = CARTESIAN_POINT ( 'NONE',  ( -23.15000000000000213, -11.64999999998884483, -131.0000000000000284 ) ) ;
#75711 = AXIS2_PLACEMENT_3D ( 'NONE', #101861, #242673, #241411 ) ;
#75710 = DIRECTION ( 'NONE',  ( 0.000000000000000000, -6.938893903907222067E-15, 1.000000000000000000 ) ) ;
#75712 = DIRECTION ( 'NONE',  ( -1.000000000000000000, 0.000000000000000000, 0.000000000000000000 ) ) ;
#75713 = CARTESIAN_POINT ( 'NONE',  ( 21.14999999999999858, 65.51923798433685420, -242.1677427744926092 ) ) ;
#75715 = CYLINDRICAL_SURFACE ( 'NONE', #54154, 0.8750000000000007772 ) ;
#75714 = DIRECTION ( 'NONE',  ( -1.000000000000000000, 0.000000000000000000, -0.000000000000000000 ) ) ;
#75717 = DIRECTION ( 'NONE',  ( 0.000000000000000000, 0.8660254037844411501, 0.4999999999999956701 ) ) ;
#75716 = CIRCLE ( 'NONE', #38297, 0.1999999999999987899 ) ;
#75718 = ORIENTED_EDGE ( 'NONE', *, *, #66151, .F. ) ;
#75720 = LINE ( 'NONE', #17035, #193314 ) ;
#75719 = CYLINDRICAL_SURFACE ( 'NONE', #86846, 0.09999999999999939493 ) ;
#75721 = VERTEX_POINT ( 'NONE', #168508 ) ;
#75723 = ORIENTED_EDGE ( 'NONE', *, *, #144072, .T. ) ;
#75722 = LINE ( 'NONE', #135663, #123081 ) ;
#75724 = ORIENTED_EDGE ( 'NONE', *, *, #29266, .F. ) ;
#75725 = CARTESIAN_POINT ( 'NONE',  ( -16.91256925476571382, 9.985731158139332209, -146.5323575109947569 ) ) ;
#75726 = AXIS2_PLACEMENT_3D ( 'NONE', #117631, #237586, #199762 ) ;
#75727 = DIRECTION ( 'NONE',  ( -0.000000000000000000, 1.000000000000000000, -0.000000000000000000 ) ) ;
#75728 = DIRECTION ( 'NONE',  ( -1.000000000000000000, 0.000000000000000000, 0.000000000000000000 ) ) ;
#75729 = CARTESIAN_POINT ( 'NONE',  ( -17.73285935860374352, 21.28367419047321718, -228.9973760273217920 ) ) ;
#75730 = AXIS2_PLACEMENT_3D ( 'NONE', #234379, #192705, #37491 ) ;
#75731 = ORIENTED_EDGE ( 'NONE', *, *, #35619, .F. ) ;
#75732 = CARTESIAN_POINT ( 'NONE',  ( 22.57320508075688537, 64.25000000001267608, -203.5231074845244450 ) ) ;
#75733 = ORIENTED_EDGE ( 'NONE', *, *, #198383, .T. ) ;
#75734 = CIRCLE ( 'NONE', #38313, 0.1000000000000002554 ) ;
#75735 = DIRECTION ( 'NONE',  ( 1.000000000000000000, 0.000000000000000000, 0.000000000000000000 ) ) ;
#75736 = EDGE_CURVE ( 'NONE', #54663, #20774, #204029, .T. ) ;
#75737 = DIRECTION ( 'NONE',  ( 0.000000000000000000, 1.000000000000000000, 0.000000000000000000 ) ) ;
#75738 = AXIS2_PLACEMENT_3D ( 'NONE', #231618, #50369, #30867 ) ;
#75739 = ORIENTED_EDGE ( 'NONE', *, *, #61847, .F. ) ;
#75740 = EDGE_LOOP ( 'NONE', ( #71225, #158898, #241448 ) ) ;
#75741 = CARTESIAN_POINT ( 'NONE',  ( -21.05000000000000071, -11.64999999998884483, -36.39999999999999858 ) ) ;
#75742 = VERTEX_POINT ( 'NONE', #30251 ) ;
#75743 = DIRECTION ( 'NONE',  ( -0.000000000000000000, 0.000000000000000000, 1.000000000000000000 ) ) ;
#75744 = VERTEX_POINT ( 'NONE', #4229 ) ;
#75745 = DIRECTION ( 'NONE',  ( 1.000000000000000000, 0.000000000000000000, 0.000000000000000000 ) ) ;
#75746 = CIRCLE ( 'NONE', #46672, 11.80000000000000249 ) ;
#75747 = EDGE_CURVE ( 'NONE', #38899, #2960, #83742, .T. ) ;
#75748 = DIRECTION ( 'NONE',  ( 0.000000000000000000, 0.6728971962616697722, -0.7397360091702875895 ) ) ;
#75749 = DIRECTION ( 'NONE',  ( -1.000000000000000000, 0.000000000000000000, 0.000000000000000000 ) ) ;
#75750 = VECTOR ( 'NONE', #139225, 1000.000000000000000 ) ;
#75751 = EDGE_CURVE ( 'NONE', #160204, #88769, #29295, .T. ) ;
#75752 = DIRECTION ( 'NONE',  ( 1.000000000000000000, 0.000000000000000000, 0.000000000000000000 ) ) ;
#75753 = DIRECTION ( 'NONE',  ( 0.000000000000000000, 0.000000000000000000, 1.000000000000000000 ) ) ;
#75754 = ADVANCED_FACE ( 'NONE', ( #210167 ), #130614, .T. ) ;
#75755 = CARTESIAN_POINT ( 'NONE',  ( 18.52326479938714954, -9.642364444904220733, -73.71475741340583454 ) ) ;
#75756 = CIRCLE ( 'NONE', #79989, 0.4000000000000114575 ) ;
#75757 = VERTEX_POINT ( 'NONE', #90183 ) ;
#75759 = CARTESIAN_POINT ( 'NONE',  ( 22.49806830649814060, 64.35011034517307849, -136.6005718008498775 ) ) ;
#75758 = FACE_OUTER_BOUND ( 'NONE', #80267, .T. ) ;
#75760 = ORIENTED_EDGE ( 'NONE', *, *, #86508, .T. ) ;
#75763 = ORIENTED_EDGE ( 'NONE', *, *, #38294, .F. ) ;
#75762 = DIRECTION ( 'NONE',  ( 0.000000000000000000, 0.2128009952263601179, -0.9770955615653315052 ) ) ;
#75761 = DIRECTION ( 'NONE',  ( 0.000000000000000000, 0.9126074666063765939, 0.4088369013363289950 ) ) ;
#75764 = VECTOR ( 'NONE', #72196, 1000.000000000000000 ) ;
#75765 = ORIENTED_EDGE ( 'NONE', *, *, #192449, .F. ) ;
#75766 = CARTESIAN_POINT ( 'NONE',  ( 23.14999999999999503, 43.07541598710462694, -233.9110336739111347 ) ) ;
#75767 = VECTOR ( 'NONE', #225643, 1000.000000000000000 ) ;
#75768 = CARTESIAN_POINT ( 'NONE',  ( 21.11825140030084569, 0.007203620643888101679, -60.55459243458003016 ) ) ;
#75769 = LINE ( 'NONE', #155329, #158506 ) ;
#75770 = EDGE_LOOP ( 'NONE', ( #182570, #144609, #29977, #209892 ) ) ;
#75772 = ORIENTED_EDGE ( 'NONE', *, *, #90031, .F. ) ;
#75771 = CARTESIAN_POINT ( 'NONE',  ( -23.15000000000000213, 48.40874555430183079, -244.2873875965402704 ) ) ;
#75773 = EDGE_CURVE ( 'NONE', #96108, #19722, #111052, .T. ) ;
#75775 = CARTESIAN_POINT ( 'NONE',  ( 20.95520789717937404, 10.57693059938495672, -7.580232973874853286 ) ) ;
#75774 = DIRECTION ( 'NONE',  ( 1.000000000000000000, 0.000000000000000000, 0.000000000000000000 ) ) ;
#75777 = ORIENTED_EDGE ( 'NONE', *, *, #248648, .T. ) ;
#75776 = DIRECTION ( 'NONE',  ( -1.000000000000000000, -0.000000000000000000, 0.000000000000000000 ) ) ;
#75778 = ORIENTED_EDGE ( 'NONE', *, *, #235520, .T. ) ;
#75779 = AXIS2_PLACEMENT_3D ( 'NONE', #243937, #178878, #41922 ) ;
#75780 = CARTESIAN_POINT ( 'NONE',  ( 20.95566103547454517, 11.99910583982818224, -206.1974635114572720 ) ) ;
#75781 = CARTESIAN_POINT ( 'NONE',  ( 18.39999999999999858, 85.50000000001240608, -163.1084491415546154 ) ) ;
#75782 = ORIENTED_EDGE ( 'NONE', *, *, #8061, .T. ) ;
#75783 = CARTESIAN_POINT ( 'NONE',  ( -23.15000000000000213, 17.95002310328549200, -228.2032933776778520 ) ) ;
#75784 = ORIENTED_EDGE ( 'NONE', *, *, #75013, .F. ) ;
#75785 = CARTESIAN_POINT ( 'NONE',  ( 18.59999999999999787, 36.65892442174472876, -249.5511627012454596 ) ) ;
#75786 = DIRECTION ( 'NONE',  ( -1.000000000000000000, 0.000000000000000000, 0.000000000000000000 ) ) ;
#75787 = VERTEX_POINT ( 'NONE', #173657 ) ;
#75788 = CARTESIAN_POINT ( 'NONE',  ( 18.59999999999999432, 0.8650195716890449749, -212.6652626294507229 ) ) ;
#75789 = CARTESIAN_POINT ( 'NONE',  ( -16.81453563122427397, 9.939100205448108127, -54.28825866064529748 ) ) ;
#75790 = B_SPLINE_CURVE_WITH_KNOTS ( 'NONE', 3,
 ( #92302, #192703, #55706, #153623, #231840, #177016, #154882, #51877, #193997, #171888 ),
 .UNSPECIFIED., .F., .F.,
 ( 4, 3, 3, 4 ),
 ( 0.000000000000000000, 1.004626015991719593E-05, 1.831183478183680716E-05, 2.062343583996558100E-05 ),
 .UNSPECIFIED. ) ;
#75791 = ADVANCED_FACE ( 'NONE', ( #190611 ), #133190, .F. ) ;
#75793 = EDGE_LOOP ( 'NONE', ( #34426, #205792, #47485, #217182, #256544, #59535 ) ) ;
#75792 = CIRCLE ( 'NONE', #250562, 0.2000000000000057288 ) ;
#75794 = ORIENTED_EDGE ( 'NONE', *, *, #2752, .F. ) ;
#75795 = CARTESIAN_POINT ( 'NONE',  ( 20.30466543256790501, 18.79779222453387533, -229.4283813036538788 ) ) ;
#75796 = ORIENTED_EDGE ( 'NONE', *, *, #156072, .T. ) ;
#75797 = EDGE_LOOP ( 'NONE', ( #38978, #70044 ) ) ;
#75799 = ORIENTED_EDGE ( 'NONE', *, *, #79816, .F. ) ;
#75798 = FACE_OUTER_BOUND ( 'NONE', #201355, .T. ) ;
#75800 = EDGE_CURVE ( 'NONE', #126029, #192766, #79121, .T. ) ;
#75801 = EDGE_LOOP ( 'NONE', ( #5319, #140102, #197650, #193972 ) ) ;
#75802 = DIRECTION ( 'NONE',  ( 0.000000000000000000, 6.938893903907222067E-15, -1.000000000000000000 ) ) ;
#75803 = ORIENTED_EDGE ( 'NONE', *, *, #10574, .F. ) ;
#75806 = ORIENTED_EDGE ( 'NONE', *, *, #164273, .F. ) ;
#75805 = ORIENTED_EDGE ( 'NONE', *, *, #45902, .T. ) ;
#75804 = CARTESIAN_POINT ( 'NONE',  ( 22.50000000000000000, 7.750000000000007105, 0.09999999999999939493 ) ) ;
#75807 = EDGE_CURVE ( 'NONE', #183282, #132561, #62585, .T. ) ;
#75808 = TOROIDAL_SURFACE ( 'NONE', #196597, 0.4000000000000012990, 0.1000000000000000056 ) ;
#75809 = VERTEX_POINT ( 'NONE', #114912 ) ;
#75810 = DIRECTION ( 'NONE',  ( 0.000000000000000000, 0.2617529984165030688, 0.9651348961777158619 ) ) ;
#75811 = AXIS2_PLACEMENT_3D ( 'NONE', #185701, #244370, #124449 ) ;
#75812 = DIRECTION ( 'NONE',  ( 1.000000000000000000, 0.000000000000000000, 0.000000000000000000 ) ) ;
#75813 = ORIENTED_EDGE ( 'NONE', *, *, #27157, .F. ) ;
#75814 = CARTESIAN_POINT ( 'NONE',  ( -16.93658211146644987, 9.994108662352344297, -154.9042950699557082 ) ) ;
#75815 = ADVANCED_FACE ( 'NONE', ( #152784 ), #249296, .T. ) ;
#75817 = ORIENTED_EDGE ( 'NONE', *, *, #84433, .F. ) ;
#75816 = DIRECTION ( 'NONE',  ( 1.000000000000000000, 0.000000000000000000, 1.073024830501117725E-15 ) ) ;
#75818 = CARTESIAN_POINT ( 'NONE',  ( -21.05000000000000071, 1.115600667400684642E-11, -33.50000000000000000 ) ) ;
#75819 = ORIENTED_EDGE ( 'NONE', *, *, #44679, .T. ) ;
#75820 = ORIENTED_EDGE ( 'NONE', *, *, #190099, .F. ) ;
#75821 = EDGE_CURVE ( 'NONE', #37010, #187076, #54915, .T. ) ;
#75822 = FACE_OUTER_BOUND ( 'NONE', #124973, .T. ) ;
#75823 = FILL_AREA_STYLE_COLOUR ( '', #99198 ) ;
#75824 = VECTOR ( 'NONE', #153500, 1000.000000000000000 ) ;
#75825 = ORIENTED_EDGE ( 'NONE', *, *, #43180, .T. ) ;
#75826 = ORIENTED_EDGE ( 'NONE', *, *, #85609, .F. ) ;
#75827 = CARTESIAN_POINT ( 'NONE',  ( 21.15000000000005542, 74.16448838626247664, -47.52760213295649550 ) ) ;
#75828 = DIRECTION ( 'NONE',  ( 0.000000000000000000, 0.9770955615653313941, 0.2128009952263606730 ) ) ;
#75829 = EDGE_CURVE ( 'NONE', #115218, #243446, #232312, .T. ) ;
#75831 = ORIENTED_EDGE ( 'NONE', *, *, #105806, .T. ) ;
#75830 = EDGE_LOOP ( 'NONE', ( #189290, #73594, #246992, #84380 ) ) ;
#75832 = ORIENTED_EDGE ( 'NONE', *, *, #106192, .F. ) ;
#75833 = DIRECTION ( 'NONE',  ( 1.000000000000000000, 0.000000000000000000, 0.000000000000000000 ) ) ;
#75834 = VERTEX_POINT ( 'NONE', #51041 ) ;
#75835 = EDGE_LOOP ( 'NONE', ( #138773, #240008, #9273 ) ) ;
#75836 = CARTESIAN_POINT ( 'NONE',  ( -23.25000000000000355, 11.75000000001113953, -191.7499999999999716 ) ) ;
#75837 = EDGE_LOOP ( 'NONE', ( #114434, #85662, #15426, #185144 ) ) ;
#75838 = EDGE_CURVE ( 'NONE', #159923, #249034, #193179, .T. ) ;
#75839 = CARTESIAN_POINT ( 'NONE',  ( 21.05000000000005400, 64.25000000001119815, -5.923107484524795296 ) ) ;
#75840 = EDGE_CURVE ( 'NONE', #158987, #89853, #91970, .T. ) ;
#75841 = CARTESIAN_POINT ( 'NONE',  ( -20.94999999999999929, 76.00000000001170974, -69.52310748452431710 ) ) ;
#75842 = VERTEX_POINT ( 'NONE', #212738 ) ;
#75843 = AXIS2_PLACEMENT_3D ( 'NONE', #57993, #78840, #134951 ) ;
#75844 = ORIENTED_EDGE ( 'NONE', *, *, #90028, .F. ) ;
#75845 = AXIS2_PLACEMENT_3D ( 'NONE', #149120, #126969, #26606 ) ;
#75846 = DIRECTION ( 'NONE',  ( 1.186688945009009831E-16, 1.000000000000000000, 6.982962677686266711E-15 ) ) ;
#75847 = ORIENTED_EDGE ( 'NONE', *, *, #120416, .T. ) ;
#75848 = DIRECTION ( 'NONE',  ( -1.000000000000000000, 0.000000000000000000, 0.000000000000000000 ) ) ;
#75849 = ORIENTED_EDGE ( 'NONE', *, *, #138555, .F. ) ;
#75850 = EDGE_CURVE ( 'NONE', #142529, #183742, #233469, .T. ) ;
#75851 = VERTEX_POINT ( 'NONE', #52344 ) ;
#75852 = ADVANCED_FACE ( 'NONE', ( #253116 ), #155354, .T. ) ;
#75853 = CARTESIAN_POINT ( 'NONE',  ( -21.05000000000000071, 67.23127455305835554, -235.8551265064784559 ) ) ;
#75854 = VERTEX_POINT ( 'NONE', #74546 ) ;
#75855 = CARTESIAN_POINT ( 'NONE',  ( 18.79999999999999716, 7.900000000000000355, 1.212568896937007867 ) ) ;
#75856 = CARTESIAN_POINT ( 'NONE',  ( -18.50000000000000711, 64.35000000001208775, -129.5083017138703667 ) ) ;
#75857 = ORIENTED_EDGE ( 'NONE', *, *, #253669, .F. ) ;
#75858 = CARTESIAN_POINT ( 'NONE',  ( 20.95512820512820440, 65.37615131630019505, -128.8581939154367717 ) ) ;
#75859 = CARTESIAN_POINT ( 'NONE',  ( 18.49999999999999289, 33.95290177507398255, -236.2840123990883114 ) ) ;
#75860 = AXIS2_PLACEMENT_3D ( 'NONE', #83959, #207848, #43608 ) ;
#75861 = DIRECTION ( 'NONE',  ( 1.000000000000000000, 0.000000000000000000, 0.000000000000000000 ) ) ;
#75862 = CARTESIAN_POINT ( 'NONE',  ( 23.14999999999999858, 65.17014820068582992, -222.4427298839669618 ) ) ;
#75863 = CARTESIAN_POINT ( 'NONE',  ( 21.05000000000000071, 6.450000000000001066, -10.01702717044001822 ) ) ;
#75864 = DIRECTION ( 'NONE',  ( 0.000000000000000000, 0.000000000000000000, 1.000000000000000000 ) ) ;
#75865 = DIRECTION ( 'NONE',  ( -0.000000000000000000, 1.000000000000000000, -0.000000000000000000 ) ) ;
#75866 = EDGE_CURVE ( 'NONE', #102067, #60014, #75253, .T. ) ;
#75867 = CARTESIAN_POINT ( 'NONE',  ( -25.10847955711010115, 9.068702471349579852, 33.00000000000000000 ) ) ;
#75868 = DIRECTION ( 'NONE',  ( -0.000000000000000000, -0.3427706569149635007, 0.9394191166662961834 ) ) ;
#75869 = VERTEX_POINT ( 'NONE', #70673 ) ;
#75870 = CIRCLE ( 'NONE', #242446, 0.8750000000000007772 ) ;
#75872 = VERTEX_POINT ( 'NONE', #35410 ) ;
#75871 = VERTEX_POINT ( 'NONE', #214015 ) ;
#75873 = EDGE_LOOP ( 'NONE', ( #178723, #152473, #44167, #132592, #79264 ) ) ;
#75874 = CARTESIAN_POINT ( 'NONE',  ( 20.94999999999999574, 13.53186623653377119, -238.6930807526024694 ) ) ;
#75875 = CIRCLE ( 'NONE', #167480, 0.09999999999998898659 ) ;
#75876 = DIRECTION ( 'NONE',  ( -0.000000000000000000, 0.000000000000000000, 1.000000000000000000 ) ) ;
#75878 = DIRECTION ( 'NONE',  ( 0.7070776581708964059, -0.6233369439636241571, 0.3339045366652730884 ) ) ;
#75877 = DIRECTION ( 'NONE',  ( -0.8660254037844352659, 0.000000000000000000, 0.5000000000000059952 ) ) ;
#75879 = VERTEX_POINT ( 'NONE', #215288 ) ;
#75880 = AXIS2_PLACEMENT_3D ( 'NONE', #109268, #89705, #70187 ) ;
#75881 = ADVANCED_FACE ( 'NONE', ( #10679 ), #254270, .T. ) ;
#75882 = CARTESIAN_POINT ( 'NONE',  ( -23.15000000000000213, 2.571758278209444422E-16, -31.39999999999999858 ) ) ;
#75883 = CARTESIAN_POINT ( 'NONE',  ( 13.99999999999999822, 66.15000000001155911, -52.77310748452440237 ) ) ;
#75884 = AXIS2_PLACEMENT_3D ( 'NONE', #89871, #32519, #208571 ) ;
#75885 = CARTESIAN_POINT ( 'NONE',  ( -20.64999999999999858, 7.128833340094563376, -233.7327013124401276 ) ) ;
#75886 = AXIS2_PLACEMENT_3D ( 'NONE', #214041, #194497, #56223 ) ;
#75887 = EDGE_CURVE ( 'NONE', #137538, #119326, #12714, .T. ) ;
#75888 = CIRCLE ( 'NONE', #221605, 0.1000000000000028644 ) ;
#75889 = CARTESIAN_POINT ( 'NONE',  ( -23.15000000000000213, 76.00000000001192291, -105.1231074845242972 ) ) ;
#75890 = ORIENTED_EDGE ( 'NONE', *, *, #76213, .F. ) ;
#75891 = ORIENTED_EDGE ( 'NONE', *, *, #42817, .T. ) ;
#75892 = CARTESIAN_POINT ( 'NONE',  ( 20.84999999999998721, -11.75000000000000000, -33.50000000000000000 ) ) ;
#75893 = VECTOR ( 'NONE', #199455, 1000.000000000000000 ) ;
#75894 = CARTESIAN_POINT ( 'NONE',  ( 18.46921299892753865, 8.797208686344667683, -245.4141857684114427 ) ) ;
#75895 = EDGE_CURVE ( 'NONE', #250282, #138432, #180032, .T. ) ;
#75896 = ADVANCED_FACE ( 'NONE', ( #238705 ), #39251, .F. ) ;
#75897 = ORIENTED_EDGE ( 'NONE', *, *, #93725, .F. ) ;
#75898 = CARTESIAN_POINT ( 'NONE',  ( 23.24999999999999289, 69.35000000001205933, -124.1731074845243370 ) ) ;
#75899 = DIRECTION ( 'NONE',  ( 0.000000000000000000, -0.9998779222360097974, 0.01562500000000363945 ) ) ;
#75900 = DIRECTION ( 'NONE',  ( -0.000000000000000000, -0.000000000000000000, -1.000000000000000000 ) ) ;
#75901 = CARTESIAN_POINT ( 'NONE',  ( -20.94999999999999929, 87.75000000001192291, -100.1231074845242262 ) ) ;
#75902 = EDGE_CURVE ( 'NONE', #92448, #101761, #137743, .T. ) ;
#75904 = CIRCLE ( 'NONE', #230015, 0.1999999999999996503 ) ;
#75903 = DIRECTION ( 'NONE',  ( 0.000000000000000000, 1.000000000000000000, 6.982962677686266711E-15 ) ) ;
#75905 = ORIENTED_EDGE ( 'NONE', *, *, #26096, .T. ) ;
#75906 = CARTESIAN_POINT ( 'NONE',  ( -23.25000000000000000, 85.60000000001150511, -45.91707660717669626 ) ) ;
#75907 = CYLINDRICAL_SURFACE ( 'NONE', #201672, 0.1000000000000013933 ) ;
#75908 = CARTESIAN_POINT ( 'NONE',  ( 21.14999999999999858, 52.64219947837469959, -255.2660483925003803 ) ) ;
#75909 = AXIS2_PLACEMENT_3D ( 'NONE', #199760, #197154, #18534 ) ;
#75911 = DIRECTION ( 'NONE',  ( 0.000000000000000000, -1.000000000000000000, -0.000000000000000000 ) ) ;
#75910 = CARTESIAN_POINT ( 'NONE',  ( -16.83199030136657370, 66.06935196689859424, -123.7507064618668977 ) ) ;
#75912 = DIRECTION ( 'NONE',  ( 1.000000000000000000, 0.000000000000000000, 0.000000000000000000 ) ) ;
#75914 = DIRECTION ( 'NONE',  ( -0.000000000000000000, -0.2617529984165028467, -0.9651348961777159730 ) ) ;
#75913 = AXIS2_PLACEMENT_3D ( 'NONE', #221009, #106191, #183195 ) ;
#75915 = AXIS2_PLACEMENT_3D ( 'NONE', #140650, #39007, #22007 ) ;
#75916 = CARTESIAN_POINT ( 'NONE',  ( -20.94999999999999929, 36.65892442174472876, -249.5511627012454596 ) ) ;
#75917 = DIRECTION ( 'NONE',  ( 0.000000000000000000, -6.982962677686266711E-15, 1.000000000000000000 ) ) ;
#75918 = AXIS2_PLACEMENT_3D ( 'NONE', #103788, #256742, #178577 ) ;
#75919 = VERTEX_POINT ( 'NONE', #217833 ) ;
#75920 = EDGE_CURVE ( 'NONE', #240894, #85481, #37963, .T. ) ;
#75921 = ADVANCED_FACE ( 'NONE', ( #1359 ), #179306, .T. ) ;
#75922 = AXIS2_PLACEMENT_3D ( 'NONE', #185964, #166435, #4732 ) ;
#75923 = ORIENTED_EDGE ( 'NONE', *, *, #64050, .T. ) ;
#75924 = CARTESIAN_POINT ( 'NONE',  ( 21.14999999999999503, 1.115600667400684642E-11, -100.5000000000000284 ) ) ;
#75925 = ORIENTED_EDGE ( 'NONE', *, *, #125809, .F. ) ;
#75926 = EDGE_CURVE ( 'NONE', #8049, #63952, #216866, .T. ) ;
#75927 = CIRCLE ( 'NONE', #50762, 7.799999999999997158 ) ;
#75928 = CARTESIAN_POINT ( 'NONE',  ( -21.14999999999999858, 18.65704504850842582, -226.5784250989226507 ) ) ;
#75929 = ORIENTED_EDGE ( 'NONE', *, *, #99325, .F. ) ;
#75930 = SURFACE_STYLE_FILL_AREA ( #115054 ) ;
#75931 = ADVANCED_FACE ( 'NONE', ( #159197 ), #177488, .F. ) ;
#75932 = DIRECTION ( 'NONE',  ( 0.000000000000000000, 0.6728971962616697722, -0.7397360091702875895 ) ) ;
#75933 = VECTOR ( 'NONE', #196247, 1000.000000000000000 ) ;
#75934 = ORIENTED_EDGE ( 'NONE', *, *, #14131, .T. ) ;
#75936 = CARTESIAN_POINT ( 'NONE',  ( 21.08479644141222664, 0.05855444257529676677, -161.1549613422680522 ) ) ;
#75935 = AXIS2_PLACEMENT_3D ( 'NONE', #139390, #3753, #200681 ) ;
#75937 = CARTESIAN_POINT ( 'NONE',  ( -13.11924609551135035, 9.431689550535260480, -51.77929003223608362 ) ) ;
#75938 = DIRECTION ( 'NONE',  ( 0.000000000000000000, -0.8814952561688476074, 0.4721928772777262417 ) ) ;
#75939 = EDGE_CURVE ( 'NONE', #151382, #221285, #256932, .T. ) ;
#75940 = CARTESIAN_POINT ( 'NONE',  ( 18.49999999999999289, 10.20857864377385127, -192.1499999999999488 ) ) ;
#75942 = ORIENTED_EDGE ( 'NONE', *, *, #157563, .F. ) ;
#75941 = CARTESIAN_POINT ( 'NONE',  ( 18.39999999999999503, 64.52683809664949877, -112.2731074845243739 ) ) ;
#75944 = CARTESIAN_POINT ( 'NONE',  ( -20.85000000000000142, 11.75000000001115552, -167.5000000000000284 ) ) ;
#75943 = CARTESIAN_POINT ( 'NONE',  ( 21.05000000000000071, 6.134002965564945065, -199.5633345488327848 ) ) ;
#75945 = LINE ( 'NONE', #155514, #190231 ) ;
#75946 = EDGE_CURVE ( 'NONE', #167063, #91225, #66855, .T. ) ;
#75947 = DIRECTION ( 'NONE',  ( 0.000000000000000000, -1.000000000000000000, -2.891205793294679805E-16 ) ) ;
#75948 = CARTESIAN_POINT ( 'NONE',  ( 0.000000000000000000, 0.000000000000000000, 33.00000000000000000 ) ) ;
#75949 = DIRECTION ( 'NONE',  ( 0.000000000000000000, 0.000000000000000000, -1.000000000000000000 ) ) ;
#75950 = ORIENTED_EDGE ( 'NONE', *, *, #218090, .T. ) ;
#75951 = EDGE_CURVE ( 'NONE', #42521, #110495, #154378, .T. ) ;
#75952 =( NAMED_UNIT ( * ) SI_UNIT ( $, .STERADIAN. ) SOLID_ANGLE_UNIT ( ) );
#75953 = CARTESIAN_POINT ( 'NONE',  ( -20.64999999999999858, 2.400000000011155432, -147.2246219227621111 ) ) ;
#75954 = EDGE_LOOP ( 'NONE', ( #240681, #188339, #14584, #205576 ) ) ;
#75955 = CYLINDRICAL_SURFACE ( 'NONE', #2911, 0.1000000000000028644 ) ;
#75956 = CIRCLE ( 'NONE', #242539, 0.09999999999999939493 ) ;
#75957 = ORIENTED_EDGE ( 'NONE', *, *, #204163, .F. ) ;
#75958 = CARTESIAN_POINT ( 'NONE',  ( 21.05000000000000071, 7.128833340094563376, -233.7327013124401276 ) ) ;
#75959 = CARTESIAN_POINT ( 'NONE',  ( -16.92563707711778420, 9.968990694396778096, -20.88075829952397555 ) ) ;
#75960 = DIRECTION ( 'NONE',  ( 0.000000000000000000, -7.086529944415886769E-15, 1.000000000000000000 ) ) ;
#75961 = EDGE_CURVE ( 'NONE', #104626, #111385, #241295, .T. ) ;
#75962 = ORIENTED_EDGE ( 'NONE', *, *, #52119, .T. ) ;
#75963 = ORIENTED_EDGE ( 'NONE', *, *, #32683, .F. ) ;
#75965 = ADVANCED_FACE ( 'NONE', ( #120078 ), #199606, .F. ) ;
#75964 = CARTESIAN_POINT ( 'NONE',  ( -21.55000000000000426, 7.708578643762696636, -21.25000000000000000 ) ) ;
#75966 = CARTESIAN_POINT ( 'NONE',  ( 20.85000000000000142, 77.83585931145546510, -91.51866831572576189 ) ) ;
#75967 = CARTESIAN_POINT ( 'NONE',  ( -16.97683809663752186, 62.88879881541066652, -213.8537543555185607 ) ) ;
#75968 = CARTESIAN_POINT ( 'NONE',  ( -23.25000000000000000, 48.79765034352288922, -253.5326144460178170 ) ) ;
#75970 = CARTESIAN_POINT ( 'NONE',  ( -20.85000000000000142, -11.64999999998884483, -131.1000000000000227 ) ) ;
#75969 = FACE_OUTER_BOUND ( 'NONE', #118554, .T. ) ;
#75971 = CARTESIAN_POINT ( 'NONE',  ( 23.14999999999999503, 11.65000000001116298, -155.3500000000000227 ) ) ;
#75972 = CARTESIAN_POINT ( 'NONE',  ( 12.26145404764308289, 9.351413679112543065, -50.48034356754896379 ) ) ;
#75973 = ORIENTED_EDGE ( 'NONE', *, *, #47248, .F. ) ;
#75974 = CARTESIAN_POINT ( 'NONE',  ( 20.94999999999999929, 56.45527679911575802, -225.2871936083021467 ) ) ;
#75975 = AXIS2_PLACEMENT_3D ( 'NONE', #108989, #129838, #208127 ) ;
#75977 = ORIENTED_EDGE ( 'NONE', *, *, #210232, .T. ) ;
#75976 = DIRECTION ( 'NONE',  ( 1.000000000000000000, 0.000000000000000000, 0.000000000000000000 ) ) ;
#75978 = CARTESIAN_POINT ( 'NONE',  ( 22.49999999999999645, 11.74956712348939014, 0.1008583690987083642 ) ) ;
#75979 = FACE_OUTER_BOUND ( 'NONE', #146030, .T. ) ;
#75981 = CARTESIAN_POINT ( 'NONE',  ( -18.59999999999999787, 67.65998959290219261, -227.8609496483021530 ) ) ;
#75980 = CARTESIAN_POINT ( 'NONE',  ( -20.64999999999999858, 7.554435330547284444, -235.6868924355707691 ) ) ;
#75982 = ADVANCED_FACE ( 'NONE', ( #200864 ), #54371, .T. ) ;
#75984 = EDGE_LOOP ( 'NONE', ( #151802, #240276 ) ) ;
#75983 = CARTESIAN_POINT ( 'NONE',  ( 21.53699400380725137, 69.21228820682151195, -136.5231074845243597 ) ) ;
#75986 = FACE_BOUND ( 'NONE', #245485, .T. ) ;
#75985 = DIRECTION ( 'NONE',  ( 0.000000000000000000, -0.4088369013363276072, 0.9126074666063773710 ) ) ;
#75987 = DIRECTION ( 'NONE',  ( 1.000000000000000000, -2.952720810173289112E-16, -2.061873921506763405E-30 ) ) ;
#75988 = CARTESIAN_POINT ( 'NONE',  ( 18.60000000000000142, 85.40000000001226965, -162.7258477248609836 ) ) ;
#75989 = CARTESIAN_POINT ( 'NONE',  ( 20.95000000000000284, 11.60000000001116227, -194.0717967697244717 ) ) ;
#75990 = CARTESIAN_POINT ( 'NONE',  ( -18.59999999999999787, 74.83729825007408465, -128.4231074845243086 ) ) ;
#75991 = ORIENTED_EDGE ( 'NONE', *, *, #240963, .F. ) ;
#75992 = CARTESIAN_POINT ( 'NONE',  ( 18.43473516226064746, -7.778091709709652690, -209.9050494981294435 ) ) ;
#75993 = ORIENTED_EDGE ( 'NONE', *, *, #129772, .F. ) ;
#75995 = TOROIDAL_SURFACE ( 'NONE', #21826, 0.2000000000000000111, 0.1000000000000000056 ) ;
#75994 = CARTESIAN_POINT ( 'NONE',  ( -23.15000000000000213, 27.77927773649450316, -239.9732258281457860 ) ) ;
#75996 = ORIENTED_EDGE ( 'NONE', *, *, #119405, .F. ) ;
#75997 = ADVANCED_FACE ( 'NONE', ( #181321 ), #161764, .F. ) ;
#75998 = CARTESIAN_POINT ( 'NONE',  ( 23.14999999999999858, 74.00000000001141132, -36.02310748452433842 ) ) ;
#75999 = ORIENTED_EDGE ( 'NONE', *, *, #72842, .F. ) ;
#76000 = CIRCLE ( 'NONE', #51011, 0.09999999999999963085 ) ;
#76001 = CARTESIAN_POINT ( 'NONE',  ( -22.47071067811865319, 7.720074744509219933, -167.4009075452973434 ) ) ;
#76002 = DIRECTION ( 'NONE',  ( 1.000000000000000000, 0.000000000000000000, 0.000000000000000000 ) ) ;
#76003 = AXIS2_PLACEMENT_3D ( 'NONE', #105363, #241088, #162834 ) ;
#76004 =( BOUNDED_SURFACE ( )  B_SPLINE_SURFACE ( 3, 2, ( 
 ( #246479, #46975, #189082 ),
 ( #169564, #130378, #67841 ),
 ( #204772, #185230, #146088 ),
 ( #225603, #27483, #228215 ),
 ( #127831, #6579, #149978 ),
 ( #147384, #226918, #187815 ) ),
 .UNSPECIFIED., .F., .F., .F. ) 
 B_SPLINE_SURFACE_WITH_KNOTS ( ( 4, 2, 4 ),
 ( 3, 3 ),
 ( 1.570796326794895448, 2.356194490192343505, 3.141592653589791784 ),
 ( 0.000000000000000000, 1.000000000000000000 ),
 .UNSPECIFIED. ) 
 GEOMETRIC_REPRESENTATION_ITEM ( )  RATIONAL_B_SPLINE_SURFACE ( (
 ( 1.000000000000000000, 0.7071067811865475727, 1.000000000000000000),
 ( 1.000000000000000000, 0.6611148371779083099, 1.000000000000000000),
 ( 1.000000000000000000, 0.6092287576696373552, 1.000000000000000000),
 ( 1.000000000000000000, 0.5278258667057376119, 1.000000000000000000),
 ( 1.000000000000000000, 0.4993418825332260891, 1.000000000000000000),
 ( 1.000000000000000000, 0.5000000000000456302, 1.000000000000000000) ) ) 
 REPRESENTATION_ITEM ( '' )  SURFACE ( )  );
#76005 = DIRECTION ( 'NONE',  ( 0.000000000000000000, -0.8660254037844459241, -0.4999999999999873990 ) ) ;
#76006 = VERTEX_POINT ( 'NONE', #176187 ) ;
#76007 = CARTESIAN_POINT ( 'NONE',  ( -20.64999999999999858, 85.40000000001231228, -160.1291383618718385 ) ) ;
#76008 = AXIS2_PLACEMENT_3D ( 'NONE', #223671, #205387, #244525 ) ;
#76009 = DIRECTION ( 'NONE',  ( 0.000000000000000000, 0.8814952561688430555, -0.4721928772777346239 ) ) ;
#76010 = AXIS2_PLACEMENT_3D ( 'NONE', #156320, #158875, #1020 ) ;
#76011 = CARTESIAN_POINT ( 'NONE',  ( -21.14999999999999858, -11.74999999998884448, -33.50000000000000000 ) ) ;
#76012 = ORIENTED_EDGE ( 'NONE', *, *, #216199, .F. ) ;
#76013 = CARTESIAN_POINT ( 'NONE',  ( -18.46154800491001069, 85.48020627425415796, -129.8656566461428099 ) ) ;
#76014 = ORIENTED_EDGE ( 'NONE', *, *, #55544, .F. ) ;
#76016 = ORIENTED_EDGE ( 'NONE', *, *, #3443, .F. ) ;
#76015 = CARTESIAN_POINT ( 'NONE',  ( 21.05095171578076574, 67.22382012124081996, -90.85723420788649207 ) ) ;
#76017 = ORIENTED_EDGE ( 'NONE', *, *, #116423, .F. ) ;
#76018 = DIRECTION ( 'NONE',  ( 0.000000000000000000, -0.9126074666063769270, -0.4088369013363280513 ) ) ;
#76019 = FACE_OUTER_BOUND ( 'NONE', #254956, .T. ) ;
#76020 = CARTESIAN_POINT ( 'NONE',  ( -21.14999999999994174, 65.15000000001120384, -3.123107484524795474 ) ) ;
#76021 = ORIENTED_EDGE ( 'NONE', *, *, #246861, .F. ) ;
#76022 = CARTESIAN_POINT ( 'NONE',  ( 20.85000000000000142, 7.783179459866048866, -245.3643104511423303 ) ) ;
#76023 = DIRECTION ( 'NONE',  ( 1.000000000000000000, 0.000000000000000000, 0.000000000000000000 ) ) ;
#76024 = ORIENTED_EDGE ( 'NONE', *, *, #23802, .F. ) ;
#76025 = AXIS2_PLACEMENT_3D ( 'NONE', #73730, #155831, #112833 ) ;
#76027 = ORIENTED_EDGE ( 'NONE', *, *, #82800, .F. ) ;
#76026 = CARTESIAN_POINT ( 'NONE',  ( -22.50000000000000000, 0.1000000000111554016, -59.20922040162664501 ) ) ;
#76028 = AXIS2_PLACEMENT_3D ( 'NONE', #83074, #204333, #239635 ) ;
#76030 = ADVANCED_FACE ( 'NONE', ( #255655 ), #87317, .T. ) ;
#76029 = TOROIDAL_SURFACE ( 'NONE', #159437, 7.800000000000000711, 0.1000000000000000056 ) ;
#76031 = DIRECTION ( 'NONE',  ( 0.000000000000000000, 0.2617529984165152257, 0.9651348961777124202 ) ) ;
#76032 = AXIS2_PLACEMENT_3D ( 'NONE', #7015, #86525, #27903 ) ;
#76033 = B_SPLINE_CURVE_WITH_KNOTS ( 'NONE', 3,
 ( #39874, #37302, #157256, #56806, #119392, #136343, #198914, #20301, #99789, #686 ),
 .UNSPECIFIED., .F., .F.,
 ( 4, 3, 3, 4 ),
 ( 0.000000000000000000, 4.874959354401679605E-05, 9.785140065120178569E-05, 0.0001360444631935974781 ),
 .UNSPECIFIED. ) ;
#76034 = CARTESIAN_POINT ( 'NONE',  ( -16.88705144915408951, 9.950000000011138823, -79.93097859471261302 ) ) ;
#76035 = ORIENTED_EDGE ( 'NONE', *, *, #138548, .F. ) ;
#76036 = CARTESIAN_POINT ( 'NONE',  ( 20.94999999999999929, 64.25000000001195133, -109.8069731475024753 ) ) ;
#76037 = ORIENTED_EDGE ( 'NONE', *, *, #23272, .T. ) ;
#76038 = CARTESIAN_POINT ( 'NONE',  ( 21.97500000000000497, 66.25000000001260503, -191.2731074845244166 ) ) ;
#76039 = EDGE_CURVE ( 'NONE', #202540, #217215, #37839, .T. ) ;
#76040 = CARTESIAN_POINT ( 'NONE',  ( 20.94560253601876809, 64.25000000001249134, -177.0130239720093925 ) ) ;
#76041 = ADVANCED_FACE ( 'NONE', ( #46903 ), #246413, .T. ) ;
#76042 = CARTESIAN_POINT ( 'NONE',  ( 16.87683809663750267, 12.41403342719998371, -211.2428889513006993 ) ) ;
#76043 = AXIS2_PLACEMENT_3D ( 'NONE', #130876, #135996, #229985 ) ;
#76044 = EDGE_CURVE ( 'NONE', #184791, #152584, #125132, .T. ) ;
#76045 = AXIS2_PLACEMENT_3D ( 'NONE', #153855, #15607, #95109 ) ;
#76046 = ORIENTED_EDGE ( 'NONE', *, *, #3437, .F. ) ;
#76047 = DIRECTION ( 'NONE',  ( 0.000000000000000000, -0.9654727137038715545, 0.2605042016806676242 ) ) ;
#76048 = ADVANCED_FACE ( 'NONE', ( #222982 ), #41938, .F. ) ;
#76049 = ORIENTED_EDGE ( 'NONE', *, *, #181014, .F. ) ;
#76050 = ADVANCED_FACE ( 'NONE', ( #226841 ), #185152, .T. ) ;
#76051 = DIRECTION ( 'NONE',  ( 2.342056488767301376E-15, 0.1350103645451835865, 0.9908441862701605762 ) ) ;
#76052 = CARTESIAN_POINT ( 'NONE',  ( -16.89318236219975589, 9.951535257886289898, -79.64487036789418539 ) ) ;
#76053 = AXIS2_PLACEMENT_3D ( 'NONE', #236505, #35772, #154450 ) ;
#76055 = ORIENTED_EDGE ( 'NONE', *, *, #5726, .T. ) ;
#76054 = DIRECTION ( 'NONE',  ( 1.441126678808781001E-14, -0.9876197685951241256, -0.1568667991644932258 ) ) ;
#76056 = CARTESIAN_POINT ( 'NONE',  ( 18.59999999999999076, 10.20857864376269575, -24.65000000000000213 ) ) ;
#76057 = DIRECTION ( 'NONE',  ( 1.000000000000000000, -0.000000000000000000, -0.000000000000000000 ) ) ;
#76058 = EDGE_CURVE ( 'NONE', #258015, #78383, #187680, .T. ) ;
#76059 = DIRECTION ( 'NONE',  ( 0.000000000000000000, 0.8814952561688431665, -0.4721928772777344019 ) ) ;
#76060 = CYLINDRICAL_SURFACE ( 'NONE', #225546, 0.09999999999999817368 ) ;
#76061 = CARTESIAN_POINT ( 'NONE',  ( 21.07928932188134397, 6.328516656404468144, -33.40110485434561127 ) ) ;
#76062 = CIRCLE ( 'NONE', #163549, 4.000000000000003553 ) ;
#76063 = CARTESIAN_POINT ( 'NONE',  ( 21.08198257630413508, 6.336596734026219480, -66.92735667621543882 ) ) ;
#76065 = ORIENTED_EDGE ( 'NONE', *, *, #168274, .F. ) ;
#76064 = DIRECTION ( 'NONE',  ( 0.000000000000000000, 1.000000000000000000, 6.982962677686266711E-15 ) ) ;
#76066 = EDGE_CURVE ( 'NONE', #186207, #245477, #208, .T. ) ;
#76067 = VECTOR ( 'NONE', #173197, 1000.000000000000000 ) ;
#76068 = AXIS2_PLACEMENT_3D ( 'NONE', #160119, #199232, #156279 ) ;
#76069 = DIRECTION ( 'NONE',  ( 1.000000000000000000, 0.000000000000000000, 0.000000000000000000 ) ) ;
#76070 = CARTESIAN_POINT ( 'NONE',  ( 20.94999999999999574, 62.00000000001190870, -97.59601495414186445 ) ) ;
#76071 = CARTESIAN_POINT ( 'NONE',  ( 21.05000000000000071, 67.12338541492479749, -94.63802700567968884 ) ) ;
#76072 = VECTOR ( 'NONE', #159628, 1000.000000000000000 ) ;
#76073 = VERTEX_POINT ( 'NONE', #207302 ) ;
#76074 = DIRECTION ( 'NONE',  ( 3.265361837132812600E-16, -0.9770955615653313941, -0.2128009952263603677 ) ) ;
#76075 = EDGE_CURVE ( 'NONE', #224095, #170589, #241816, .T. ) ;
#76076 = AXIS2_PLACEMENT_3D ( 'NONE', #56039, #16960, #135587 ) ;
#76077 = FACE_OUTER_BOUND ( 'NONE', #66074, .T. ) ;
#76078 = CARTESIAN_POINT ( 'NONE',  ( -18.39999999999999858, 85.50000000001161027, -62.49103808782459168 ) ) ;
#76079 = CIRCLE ( 'NONE', #47034, 0.09999999999999939493 ) ;
#76080 = VERTEX_POINT ( 'NONE', #108191 ) ;
#76081 = CARTESIAN_POINT ( 'NONE',  ( -23.25000000000000000, 70.29876110920605470, -198.0544810472949564 ) ) ;
#76082 = AXIS2_PLACEMENT_3D ( 'NONE', #95, #242561, #160497 ) ;
#76084 =( BOUNDED_SURFACE ( )  B_SPLINE_SURFACE ( 3, 2, ( 
 ( #93640, #74112, #68967 ),
 ( #190190, #171937, #92349 ),
 ( #251430, #153676, #233181 ),
 ( #148489, #128927, #208478 ),
 ( #54506, #29847, #109332 ),
 ( #102260, #78860, #59274 ) ),
 .UNSPECIFIED., .F., .F., .F. ) 
 B_SPLINE_SURFACE_WITH_KNOTS ( ( 4, 2, 4 ),
 ( 3, 3 ),
 ( 1.570796326794897668, 2.356194490192346169, 3.141592653589794448 ),
 ( 0.000000000000000000, 1.000000000000000000 ),
 .UNSPECIFIED. ) 
 GEOMETRIC_REPRESENTATION_ITEM ( )  RATIONAL_B_SPLINE_SURFACE ( (
 ( 1.000000000000000000, 0.7071067811865475727, 1.000000000000000000),
 ( 1.000000000000000000, 0.6611148371772178622, 1.000000000000000000),
 ( 1.000000000000000000, 0.6092287576704737972, 1.000000000000000000),
 ( 1.000000000000000000, 0.5278258667049164909, 1.000000000000000000),
 ( 1.000000000000000000, 0.4993418825341195411, 1.000000000000000000),
 ( 1.000000000000000000, 0.4999999999999960587, 1.000000000000000000) ) ) 
 REPRESENTATION_ITEM ( '' )  SURFACE ( )  );
#76083 = AXIS2_PLACEMENT_3D ( 'NONE', #74746, #14760, #235070 ) ;
#76085 = DIRECTION ( 'NONE',  ( 0.000000000000000000, 0.000000000000000000, 1.000000000000000000 ) ) ;
#76086 = EDGE_CURVE ( 'NONE', #206261, #144388, #123907, .T. ) ;
#76087 = ORIENTED_EDGE ( 'NONE', *, *, #170281, .F. ) ;
#76088 = CARTESIAN_POINT ( 'NONE',  ( -20.85000000000000142, 77.16412189325305349, -95.10825939895268277 ) ) ;
#76089 = ORIENTED_EDGE ( 'NONE', *, *, #6717, .T. ) ;
#76090 = CARTESIAN_POINT ( 'NONE',  ( 22.39999999999999858, 7.790779598384538929, -100.4000000000000341 ) ) ;
#76092 = ORIENTED_EDGE ( 'NONE', *, *, #159776, .T. ) ;
#76091 = DIRECTION ( 'NONE',  ( 0.000000000000000000, 0.000000000000000000, 1.000000000000000000 ) ) ;
#76093 = DIRECTION ( 'NONE',  ( 0.000000000000000000, -0.1455152366551522025, -0.9893560106964505163 ) ) ;
#76094 = ORIENTED_EDGE ( 'NONE', *, *, #124465, .T. ) ;
#76095 = PLANE ( 'NONE',  #214021 ) ;
#76096 = ORIENTED_EDGE ( 'NONE', *, *, #34327, .F. ) ;
#76098 = EDGE_LOOP ( 'NONE', ( #242276, #192070, #246214, #108990 ) ) ;
#76097 = ORIENTED_EDGE ( 'NONE', *, *, #116831, .T. ) ;
#76099 = DIRECTION ( 'NONE',  ( 1.000000000000000000, 0.000000000000000000, 0.000000000000000000 ) ) ;
#76100 = VERTEX_POINT ( 'NONE', #163046 ) ;
#76101 = ADVANCED_FACE ( 'NONE', ( #165607 ), #203440, .T. ) ;
#76102 = CARTESIAN_POINT ( 'NONE',  ( -18.79999999999999716, 0.000000000000000000, 32.89999999999999858 ) ) ;
#76104 = VERTEX_POINT ( 'NONE', #182603 ) ;
#76103 = CIRCLE ( 'NONE', #5346, 12.87499999999999822 ) ;
#76105 = VECTOR ( 'NONE', #114521, 1000.000000000000000 ) ;
#76106 = EDGE_CURVE ( 'NONE', #108295, #228170, #63924, .T. ) ;
#76107 = AXIS2_PLACEMENT_3D ( 'NONE', #225034, #25588, #86812 ) ;
#76108 = EDGE_LOOP ( 'NONE', ( #40709, #22862, #237395, #195258 ) ) ;
#76109 = DIRECTION ( 'NONE',  ( -1.000000000000000000, -0.000000000000000000, -0.000000000000000000 ) ) ;
#76110 = CARTESIAN_POINT ( 'NONE',  ( 22.47071067811865319, 75.90090754530910999, -77.24318222902238062 ) ) ;
#76111 = EDGE_CURVE ( 'NONE', #237933, #225653, #171138, .T. ) ;
#76112 = LINE ( 'NONE', #77383, #178125 ) ;
#76113 = EDGE_LOOP ( 'NONE', ( #251736, #133258, #250038, #29229 ) ) ;
#76114 = DIRECTION ( 'NONE',  ( 1.000000000000000000, 0.000000000000000000, 0.000000000000000000 ) ) ;
#76115 = CARTESIAN_POINT ( 'NONE',  ( 18.59999999999999432, 1.162701749949165642, -175.5999999999999659 ) ) ;
#76116 = CARTESIAN_POINT ( 'NONE',  ( 21.13736287352038445, 8.046642376395153562, -188.3499999999999659 ) ) ;
#76118 = EDGE_LOOP ( 'NONE', ( #179707, #249565 ) ) ;
#76117 = EDGE_CURVE ( 'NONE', #49587, #157237, #116919, .T. ) ;
#76120 = ADVANCED_FACE ( 'NONE', ( #242550 ), #243833, .T. ) ;
#76119 = FACE_OUTER_BOUND ( 'NONE', #188553, .T. ) ;
#76121 = CARTESIAN_POINT ( 'NONE',  ( -18.36527282682001427, 38.27493327899719588, -261.1939576002376953 ) ) ;
#76122 = CARTESIAN_POINT ( 'NONE',  ( 20.12500000000000000, 63.38346053167636995, -212.7939182281409956 ) ) ;
#76123 = ORIENTED_EDGE ( 'NONE', *, *, #150856, .F. ) ;
#76125 = CARTESIAN_POINT ( 'NONE',  ( -21.44999999999999929, 65.69978428250288971, -213.4221254243406065 ) ) ;
#76124 = AXIS2_PLACEMENT_3D ( 'NONE', #72380, #52782, #34542 ) ;
#76126 = ORIENTED_EDGE ( 'NONE', *, *, #134751, .T. ) ;
#76127 = ORIENTED_EDGE ( 'NONE', *, *, #222519, .T. ) ;
#76128 = CARTESIAN_POINT ( 'NONE',  ( -22.50000000000000000, 30.95512775545487472, -252.1063933345974988 ) ) ;
#76129 = EDGE_CURVE ( 'NONE', #212015, #22978, #66490, .T. ) ;
#76130 = ORIENTED_EDGE ( 'NONE', *, *, #40277, .F. ) ;
#76131 = AXIS2_PLACEMENT_3D ( 'NONE', #135633, #134341, #193067 ) ;
#76132 = ORIENTED_EDGE ( 'NONE', *, *, #209439, .F. ) ;
#76133 = DIRECTION ( 'NONE',  ( -1.000000000000000000, 0.000000000000000000, -0.000000000000000000 ) ) ;
#76134 = FACE_OUTER_BOUND ( 'NONE', #154106, .T. ) ;
#76135 = EDGE_LOOP ( 'NONE', ( #107296, #253708, #80384, #96120 ) ) ;
#76136 = VERTEX_POINT ( 'NONE', #213693 ) ;
#76137 = DIRECTION ( 'NONE',  ( 0.000000000000000000, 0.1350103645451876666, -0.9908441862701600211 ) ) ;
#76138 = CYLINDRICAL_SURFACE ( 'NONE', #185753, 0.09999999999999939493 ) ;
#76139 = EDGE_LOOP ( 'NONE', ( #246300, #164853 ) ) ;
#76140 = VERTEX_POINT ( 'NONE', #132891 ) ;
#76141 = CIRCLE ( 'NONE', #242734, 0.09999999999999939493 ) ;
#76142 = DIRECTION ( 'NONE',  ( 1.000000000000000000, -0.000000000000000000, -0.000000000000000000 ) ) ;
#76143 = DIRECTION ( 'NONE',  ( 1.000000000000000000, 0.000000000000000000, 0.000000000000000000 ) ) ;
#76144 = EDGE_CURVE ( 'NONE', #254106, #136435, #137933, .T. ) ;
#76145 = ADVANCED_FACE ( 'NONE', ( #92455 ), #74605, .T. ) ;
#76146 = CARTESIAN_POINT ( 'NONE',  ( -16.87435696428308063, 9.950002462943377424, -46.14999176516656831 ) ) ;
#76147 = CARTESIAN_POINT ( 'NONE',  ( 22.39999999999999503, 11.75000000001116263, -33.40000000000000568 ) ) ;
#76148 = CARTESIAN_POINT ( 'NONE',  ( 18.59999999999999076, 6.400000000011158541, -143.9304246300615944 ) ) ;
#76149 = FACE_OUTER_BOUND ( 'NONE', #213550, .T. ) ;
#76150 = LINE ( 'NONE', #166004, #227180 ) ;
#76152 = DIRECTION ( 'NONE',  ( -1.000000000000000000, -0.000000000000000000, -0.000000000000000000 ) ) ;
#76151 = CARTESIAN_POINT ( 'NONE',  ( 21.05000000000000071, 76.09999993531877749, -76.00118570561897968 ) ) ;
#76153 = CARTESIAN_POINT ( 'NONE',  ( 18.59999999999999076, 1.749999999999999778, -11.66951155790164485 ) ) ;
#76154 = CARTESIAN_POINT ( 'NONE',  ( -16.87683809663748846, 23.64127277249475156, -231.2903243416350563 ) ) ;
#76155 = EDGE_CURVE ( 'NONE', #191840, #255281, #54614, .T. ) ;
#76156 = AXIS2_PLACEMENT_3D ( 'NONE', #257430, #217058, #201368 ) ;
#76157 = CARTESIAN_POINT ( 'NONE',  ( 22.50000000000000000, 33.38250548509083870, -242.4821227592188961 ) ) ;
#76158 = CYLINDRICAL_SURFACE ( 'NONE', #234201, 0.09999999999999939493 ) ;
#76159 = VECTOR ( 'NONE', #77954, 1000.000000000000000 ) ;
#76160 = ORIENTED_EDGE ( 'NONE', *, *, #200336, .F. ) ;
#76161 = CIRCLE ( 'NONE', #96975, 2.000000000000002665 ) ;
#76163 = ORIENTED_EDGE ( 'NONE', *, *, #120580, .F. ) ;
#76162 = FACE_OUTER_BOUND ( 'NONE', #181156, .T. ) ;
#76164 = CARTESIAN_POINT ( 'NONE',  ( -20.64999999999999858, 7.150000000011155876, -112.7500000000000284 ) ) ;
#76165 = LINE ( 'NONE', #158323, #119675 ) ;
#76166 = ORIENTED_EDGE ( 'NONE', *, *, #16749, .F. ) ;
#76167 = VECTOR ( 'NONE', #41581, 1000.000000000000000 ) ;
#76168 = AXIS2_PLACEMENT_3D ( 'NONE', #150834, #230369, #118128 ) ;
#76169 = DIRECTION ( 'NONE',  ( 0.000000000000000000, 0.000000000000000000, 1.000000000000000000 ) ) ;
#76170 = ADVANCED_BREP_SHAPE_REPRESENTATION ( '', ( #25658, #2425 ), #32042 ) ;
#76171 = EDGE_CURVE ( 'NONE', #170879, #185463, #134147, .T. ) ;
#76172 = B_SPLINE_CURVE_WITH_KNOTS ( 'NONE', 3,
 ( #223464, #126950, #104780, #89098, #166115, #248186 ),
 .UNSPECIFIED., .F., .F.,
 ( 4, 2, 4 ),
 ( 0.000000000000000000, 0.0002113392456165982716, 0.0004226784912331965432 ),
 .UNSPECIFIED. ) ;
#76173 = ORIENTED_EDGE ( 'NONE', *, *, #40204, .T. ) ;
#76174 = DIRECTION ( 'NONE',  ( 1.000000000000000000, 0.000000000000000000, 0.000000000000000000 ) ) ;
#76175 = DIRECTION ( 'NONE',  ( 0.000000000000000000, -7.116814260417660624E-15, 1.000000000000000000 ) ) ;
#76176 = AXIS2_PLACEMENT_3D ( 'NONE', #231762, #130067, #150931 ) ;
#76177 = EDGE_CURVE ( 'NONE', #217530, #61798, #12900, .T. ) ;
#76178 = DIRECTION ( 'NONE',  ( 0.000000000000000000, -0.1495327102803283015, 0.9887567792719397231 ) ) ;
#76180 = ORIENTED_EDGE ( 'NONE', *, *, #185438, .T. ) ;
#76179 = CARTESIAN_POINT ( 'NONE',  ( 16.87683809663749557, 9.950000000011131718, -87.85000000000005116 ) ) ;
#76182 = EDGE_LOOP ( 'NONE', ( #83380, #67746, #244500, #128228 ) ) ;
#76181 = CARTESIAN_POINT ( 'NONE',  ( -18.33682934331560688, 85.51118559110531692, -96.11745271585121486 ) ) ;
#76183 = CIRCLE ( 'NONE', #130361, 0.1000000000000028644 ) ;
#76185 = ADVANCED_FACE ( 'NONE', ( #129036 ), #229419, .T. ) ;
#76184 = CARTESIAN_POINT ( 'NONE',  ( -18.59999999999999787, 38.29773864426885410, -236.0513742605307925 ) ) ;
#76186 = CARTESIAN_POINT ( 'NONE',  ( 20.95512820512820440, 40.84069494668059264, -237.9516373772122222 ) ) ;
#76187 = VECTOR ( 'NONE', #171948, 1000.000000000000000 ) ;
#76188 = CARTESIAN_POINT ( 'NONE',  ( 21.97500000000000497, 9.750000000011153745, -146.3500000000000227 ) ) ;
#76189 = DIRECTION ( 'NONE',  ( 1.000000000000000000, 0.000000000000000000, 0.000000000000000000 ) ) ;
#76191 = CARTESIAN_POINT ( 'NONE',  ( -20.90000000000000213, 6.841561409100513025, 9.675512259591560138 ) ) ;
#76190 = CARTESIAN_POINT ( 'NONE',  ( 18.49505832270841310, 9.017683668627247684, -245.4513460378304899 ) ) ;
#76193 = ADVANCED_FACE ( 'NONE', ( #52036 ), #32534, .F. ) ;
#76192 = DIRECTION ( 'NONE',  ( 0.000000000000000000, 0.5407049257165758016, -0.8412123295017925884 ) ) ;
#76194 = CARTESIAN_POINT ( 'NONE',  ( -15.55912972643740488, 8.490870273573721150, -87.85000000000003695 ) ) ;
#76195 = DIRECTION ( 'NONE',  ( 0.000000000000000000, 7.086529944415894657E-15, -1.000000000000000000 ) ) ;
#76196 = DIRECTION ( 'NONE',  ( 0.000000000000000000, 1.776356839400254803E-15, -1.000000000000000000 ) ) ;
#76197 = ORIENTED_EDGE ( 'NONE', *, *, #139490, .T. ) ;
#76198 = ADVANCED_FACE ( 'NONE', ( #172045 ), #135432, .T. ) ;
#76199 = FACE_OUTER_BOUND ( 'NONE', #185695, .T. ) ;
#76201 = EDGE_CURVE ( 'NONE', #232936, #191282, #129589, .T. ) ;
#76200 = ADVANCED_FACE ( 'NONE', ( #256613 ), #118464, .F. ) ;
#76202 = ORIENTED_EDGE ( 'NONE', *, *, #123122, .T. ) ;
#76203 = ORIENTED_EDGE ( 'NONE', *, *, #68258, .F. ) ;
#76204 = FACE_OUTER_BOUND ( 'NONE', #114760, .T. ) ;
#76205 = LINE ( 'NONE', #99602, #231616 ) ;
#76206 = ORIENTED_EDGE ( 'NONE', *, *, #163708, .T. ) ;
#76207 = ORIENTED_EDGE ( 'NONE', *, *, #197311, .T. ) ;
#76208 = FACE_OUTER_BOUND ( 'NONE', #229924, .T. ) ;
#76209 = SURFACE_STYLE_FILL_AREA ( #154517 ) ;
#76210 = AXIS2_PLACEMENT_3D ( 'NONE', #175047, #130723, #254498 ) ;
#76211 = ORIENTED_EDGE ( 'NONE', *, *, #54991, .T. ) ;
#76212 = EDGE_CURVE ( 'NONE', #123298, #93557, #200898, .T. ) ;
#76213 = EDGE_CURVE ( 'NONE', #30110, #59493, #235818, .T. ) ;
#76214 = ORIENTED_EDGE ( 'NONE', *, *, #63348, .T. ) ;
#76215 = DIRECTION ( 'NONE',  ( 0.000000000000000000, -1.000000000000000000, -6.352154140967427193E-15 ) ) ;
#76216 = DIRECTION ( 'NONE',  ( -1.000000000000000000, 3.265361837132813093E-16, 2.280189983783949500E-30 ) ) ;
#76217 = CARTESIAN_POINT ( 'NONE',  ( 20.73486653747088226, 7.250000000011182166, -146.6500000000000341 ) ) ;
#76218 = LINE ( 'NONE', #20127, #115664 ) ;
#76219 = CARTESIAN_POINT ( 'NONE',  ( 13.43443725621852458, 9.446557523072529605, -15.08994195434588370 ) ) ;
#76220 = CIRCLE ( 'NONE', #80886, 0.09999999999999939493 ) ;
#76221 = ADVANCED_FACE ( 'NONE', ( #37649 ), #80571, .F. ) ;
#76222 = VECTOR ( 'NONE', #21348, 1000.000000000000000 ) ;
#76223 = CARTESIAN_POINT ( 'NONE',  ( 20.94999999999999574, 74.15091558138529138, -158.3670969630772447 ) ) ;
#76224 = FACE_OUTER_BOUND ( 'NONE', #235719, .T. ) ;
#76226 = ORIENTED_EDGE ( 'NONE', *, *, #29701, .T. ) ;
#76225 = FACE_OUTER_BOUND ( 'NONE', #70062, .T. ) ;
#76228 = CARTESIAN_POINT ( 'NONE',  ( -18.59999999999999787, 1.162701749949165642, -142.1000000000000227 ) ) ;
#76227 = CARTESIAN_POINT ( 'NONE',  ( 20.94999999999999574, 87.65000000001211333, -133.4231074845242233 ) ) ;
#76229 = LINE ( 'NONE', #145191, #6873 ) ;
#76230 = ORIENTED_EDGE ( 'NONE', *, *, #95931, .F. ) ;
#76231 = CIRCLE ( 'NONE', #105432, 0.1000000000000028644 ) ;
#76232 = CARTESIAN_POINT ( 'NONE',  ( -16.89268316805465986, 63.08557629953710943, -213.1216189793661329 ) ) ;
#76233 = DIRECTION ( 'NONE',  ( -1.000000000000000000, 0.000000000000000000, 0.000000000000000000 ) ) ;
#76234 = EDGE_LOOP ( 'NONE', ( #74782, #100184, #189401, #68991 ) ) ;
#76235 = EDGE_CURVE ( 'NONE', #79346, #215387, #142038, .T. ) ;
#76236 = CIRCLE ( 'NONE', #209516, 0.1000000000000070832 ) ;
#76238 = DIRECTION ( 'NONE',  ( -1.000000000000000000, 0.000000000000000000, -0.000000000000000000 ) ) ;
#76237 = VECTOR ( 'NONE', #87689, 1000.000000000000000 ) ;
#76239 = CIRCLE ( 'NONE', #63784, 7.900000000000003908 ) ;
#76240 = ADVANCED_FACE ( 'NONE', ( #61027 ), #117172, .F. ) ;
#76241 = CARTESIAN_POINT ( 'NONE',  ( 18.59999999999999076, 76.00000000001190870, -103.0231074845243029 ) ) ;
#76242 = DIRECTION ( 'NONE',  ( 1.000000000000000000, -0.000000000000000000, -0.000000000000000000 ) ) ;
#76243 = ORIENTED_EDGE ( 'NONE', *, *, #197737, .F. ) ;
#76244 = ORIENTED_EDGE ( 'NONE', *, *, #155788, .T. ) ;
#76245 = AXIS2_PLACEMENT_3D ( 'NONE', #155962, #95943, #20292 ) ;
#76246 = DIRECTION ( 'NONE',  ( 1.000000000000000000, 0.000000000000000000, 0.000000000000000000 ) ) ;
#76247 = CARTESIAN_POINT ( 'NONE',  ( 18.39999999999999503, 5.650000000011139001, -121.3500000000000369 ) ) ;
#76248 = LINE ( 'NONE', #39733, #207230 ) ;
#76250 = EDGE_CURVE ( 'NONE', #3673, #67428, #160170, .T. ) ;
#76249 = DIRECTION ( 'NONE',  ( 0.000000000000000000, 1.734723475976757554E-14, -1.000000000000000000 ) ) ;
#76251 = ORIENTED_EDGE ( 'NONE', *, *, #92751, .F. ) ;
#76252 = CIRCLE ( 'NONE', #226254, 0.1000000000000028644 ) ;
#76254 = CIRCLE ( 'NONE', #221980, 11.80000000000000249 ) ;
#76253 = CARTESIAN_POINT ( 'NONE',  ( 14.77516762759922209, 46.65138127958493897, -234.7343221152024739 ) ) ;
#76256 = ADVANCED_FACE ( 'NONE', ( #214975 ), #29650, .T. ) ;
#76255 = DIRECTION ( 'NONE',  ( 1.000000000000000000, 0.000000000000000000, 0.000000000000000000 ) ) ;
#76257 = VECTOR ( 'NONE', #176211, 1000.000000000000114 ) ;
#76258 = CARTESIAN_POINT ( 'NONE',  ( -20.94999999999999929, 1.115600667400684642E-11, -100.5000000000000426 ) ) ;
#76259 = VECTOR ( 'NONE', #55573, 1000.000000000000000 ) ;
#76260 = AXIS2_PLACEMENT_3D ( 'NONE', #197627, #190285, #11651 ) ;
#76262 = EDGE_LOOP ( 'NONE', ( #131250, #199929, #145514, #71117, #164598, #214831 ) ) ;
#76261 = FACE_OUTER_BOUND ( 'NONE', #41558, .T. ) ;
#76263 = VECTOR ( 'NONE', #201339, 1000.000000000000000 ) ;
#76264 = CARTESIAN_POINT ( 'NONE',  ( 20.94999999999999574, 1.835341550235569663, -145.5551512925629822 ) ) ;
#76265 = CARTESIAN_POINT ( 'NONE',  ( -16.97683810757273193, 66.05000000001187743, -89.75953077206389707 ) ) ;
#76266 = CARTESIAN_POINT ( 'NONE',  ( -18.40000000000000213, 11.33174054713633261, -154.8500000000000227 ) ) ;
#76267 = EDGE_CURVE ( 'NONE', #48052, #88042, #181001, .T. ) ;
#76268 = DIRECTION ( 'NONE',  ( -0.000000000000000000, 0.000000000000000000, -1.000000000000000000 ) ) ;
#76270 = VERTEX_POINT ( 'NONE', #139265 ) ;
#76269 = FACE_OUTER_BOUND ( 'NONE', #24373, .T. ) ;
#76271 = DIRECTION ( 'NONE',  ( 0.000000000000000000, 0.000000000000000000, -1.000000000000000000 ) ) ;
#76272 = CARTESIAN_POINT ( 'NONE',  ( -22.39999999999999858, 75.90000000001273861, -211.3138870828977645 ) ) ;
#76273 = CARTESIAN_POINT ( 'NONE',  ( 20.94999999999999929, -11.29603075032412640, -63.95210084033612929 ) ) ;
#76274 = ORIENTED_EDGE ( 'NONE', *, *, #63862, .F. ) ;
#76275 = CARTESIAN_POINT ( 'NONE',  ( -20.64999999999999858, -9.499999999988846255, -57.10603087734755690 ) ) ;
#76276 = DIRECTION ( 'NONE',  ( -0.000000000000000000, 0.000000000000000000, 1.000000000000000000 ) ) ;
#76277 = CARTESIAN_POINT ( 'NONE',  ( 23.14999999999999503, 11.65000000001116298, -59.98519422934606382 ) ) ;
#76278 = DIRECTION ( 'NONE',  ( 1.000000000000000000, 0.000000000000000000, 0.000000000000000000 ) ) ;
#76279 = CARTESIAN_POINT ( 'NONE',  ( -18.59999999999999787, 77.16412189325258453, -28.10825939895270764 ) ) ;
#76280 = AXIS2_PLACEMENT_3D ( 'NONE', #172344, #73223, #154065 ) ;
#76281 = CIRCLE ( 'NONE', #138616, 0.1000000000000028644 ) ;
#76282 = DIRECTION ( 'NONE',  ( 0.000000000000000000, 0.000000000000000000, 1.000000000000000000 ) ) ;
#76283 = CIRCLE ( 'NONE', #109604, 0.09999999999999080458 ) ;
#76284 = VECTOR ( 'NONE', #134168, 999.9999999999998863 ) ;
#76285 = EDGE_LOOP ( 'NONE', ( #89590, #203962, #148670, #159261 ) ) ;
#76286 = ORIENTED_EDGE ( 'NONE', *, *, #40622, .T. ) ;
#76287 = CARTESIAN_POINT ( 'NONE',  ( 22.47071067811864964, -1.546016791165053306, -193.4356622592197255 ) ) ;
#76288 = CARTESIAN_POINT ( 'NONE',  ( -17.01764560440361862, 66.05000000001201954, -115.7731074837375616 ) ) ;
#76289 = CARTESIAN_POINT ( 'NONE',  ( 18.41416235934318735, -0.7490476236415684053, -242.2033265267442061 ) ) ;
#76290 = CARTESIAN_POINT ( 'NONE',  ( -22.24259225415828567, 7.491937870576586889, -133.9009341165471483 ) ) ;
#76291 = DIRECTION ( 'NONE',  ( 0.000000000000000000, -0.2818822000686205809, 0.9594490217226104845 ) ) ;
#76292 = CARTESIAN_POINT ( 'NONE',  ( 20.11144452913633884, 11.38514937259154713, -206.5956884379970688 ) ) ;
#76293 = CARTESIAN_POINT ( 'NONE',  ( -16.77977881697927032, 9.946601933532905448, -12.66137857311505499 ) ) ;
#76294 = DIRECTION ( 'NONE',  ( 0.000000000000000000, -0.9651348961777157509, 0.2617529984165031243 ) ) ;
#76295 = ORIENTED_EDGE ( 'NONE', *, *, #33638, .F. ) ;
#76296 = DIRECTION ( 'NONE',  ( 0.000000000000000000, -0.4088369013363281623, 0.9126074666063771490 ) ) ;
#76297 = ORIENTED_EDGE ( 'NONE', *, *, #149191, .T. ) ;
#76298 = AXIS2_PLACEMENT_3D ( 'NONE', #198835, #119310, #137560 ) ;
#76299 = VERTEX_POINT ( 'NONE', #58446 ) ;
#76300 = CARTESIAN_POINT ( 'NONE',  ( 21.07946286933444568, 75.92331615675604439, -176.3521448035320986 ) ) ;
#76301 = DIRECTION ( 'NONE',  ( 0.000000000000000000, 0.9915357197604982575, -0.1298341882519033486 ) ) ;
#76302 = DIRECTION ( 'NONE',  ( 0.000000000000000000, -6.982962677686266711E-15, 1.000000000000000000 ) ) ;
#76303 = ORIENTED_EDGE ( 'NONE', *, *, #201594, .F. ) ;
#76304 = DIRECTION ( 'NONE',  ( 0.000000000000000000, -1.000000000000000000, -6.982962677686265922E-15 ) ) ;
#76305 = DIRECTION ( 'NONE',  ( 1.000000000000000000, -0.000000000000000000, -0.000000000000000000 ) ) ;
#76306 = DIRECTION ( 'NONE',  ( -0.7071067811865474617, 0.7071067811865474617, 5.142139384388980375E-15 ) ) ;
#76307 = VERTEX_POINT ( 'NONE', #178451 ) ;
#76308 = DIRECTION ( 'NONE',  ( 0.7071067811865474617, -0.7071067811865474617, -4.937700262164531476E-15 ) ) ;
#76309 = CARTESIAN_POINT ( 'NONE',  ( -23.25000000000000355, 31.05627573922685514, -233.2203535436961488 ) ) ;
#76310 = EDGE_CURVE ( 'NONE', #122621, #55457, #50435, .T. ) ;
#76311 = FACE_OUTER_BOUND ( 'NONE', #221856, .T. ) ;
#76312 = CIRCLE ( 'NONE', #35245, 0.1000000000000065004 ) ;
#76313 = CIRCLE ( 'NONE', #192872, 0.09999999999999913125 ) ;
#76314 = VERTEX_POINT ( 'NONE', #238389 ) ;
#76315 = CARTESIAN_POINT ( 'NONE',  ( 21.05000000000000071, -11.48912529307605546, -30.59999999999999432 ) ) ;
#76316 = DIRECTION ( 'NONE',  ( 1.000000000000000000, -0.000000000000000000, -0.000000000000000000 ) ) ;
#76317 = ORIENTED_EDGE ( 'NONE', *, *, #16502, .T. ) ;
#76318 = CARTESIAN_POINT ( 'NONE',  ( -23.49999999999994316, 83.97335046823651794, -37.38386894789040582 ) ) ;
#76319 = EDGE_CURVE ( 'NONE', #200940, #60702, #212796, .T. ) ;
#76320 = DIRECTION ( 'NONE',  ( 0.000000000000000000, 1.776356839400155604E-15, 1.000000000000000000 ) ) ;
#76321 = CARTESIAN_POINT ( 'NONE',  ( 23.14999999999999858, 35.66731937946610742, -251.4023027391979497 ) ) ;
#76322 = ADVANCED_FACE ( 'NONE', ( #83127 ), #208714, .T. ) ;
#76323 = EDGE_LOOP ( 'NONE', ( #202930, #74798, #174971 ) ) ;
#76324 = DIRECTION ( 'NONE',  ( 0.000000000000000000, -1.000000000000000000, 0.000000000000000000 ) ) ;
#76325 = AXIS2_PLACEMENT_3D ( 'NONE', #8329, #164823, #64437 ) ;
#76326 = VERTEX_POINT ( 'NONE', #143122 ) ;
#76327 = CIRCLE ( 'NONE', #59754, 0.09999999999999999167 ) ;
#76328 = AXIS2_PLACEMENT_3D ( 'NONE', #93749, #12957, #233290 ) ;
#76329 = EDGE_CURVE ( 'NONE', #160190, #245420, #146153, .T. ) ;
#76330 = ORIENTED_EDGE ( 'NONE', *, *, #161371, .T. ) ;
#76331 = ADVANCED_FACE ( 'NONE', ( #25765 ), #246106, .F. ) ;
#76332 = CARTESIAN_POINT ( 'NONE',  ( 18.59999999999999432, -9.480686695267811714, -107.4411151687579036 ) ) ;
#76333 = FACE_OUTER_BOUND ( 'NONE', #215750, .T. ) ;
#76335 = EDGE_LOOP ( 'NONE', ( #251719, #114353, #216743, #154760 ) ) ;
#76334 = CARTESIAN_POINT ( 'NONE',  ( -18.59999999999999787, -9.749999999999996447, 31.39999999999999858 ) ) ;
#76336 = CARTESIAN_POINT ( 'NONE',  ( -21.05000000000000071, -4.756823075239758225, -233.1486023682345490 ) ) ;
#76337 = CARTESIAN_POINT ( 'NONE',  ( -20.94999999999999929, 77.07318729351892728, -199.5660544101962728 ) ) ;
#76338 = ADVANCED_FACE ( 'NONE', ( #27080 ), #4884, .T. ) ;
#76339 = FACE_OUTER_BOUND ( 'NONE', #70049, .T. ) ;
#76340 = FACE_OUTER_BOUND ( 'NONE', #143050, .T. ) ;
#76341 = DIRECTION ( 'NONE',  ( 0.000000000000000000, 0.000000000000000000, -1.000000000000000000 ) ) ;
#76342 = AXIS2_PLACEMENT_3D ( 'NONE', #229187, #208352, #90942 ) ;
#76343 = CARTESIAN_POINT ( 'NONE',  ( 23.14999999999999503, 11.75000000001116263, -93.48519422934610645 ) ) ;
#76345 = CARTESIAN_POINT ( 'NONE',  ( -18.40000000000000213, 64.25000000001224976, -149.1731074845244507 ) ) ;
#76344 = AXIS2_PLACEMENT_3D ( 'NONE', #107541, #87958, #245784 ) ;
#76347 = EDGE_LOOP ( 'NONE', ( #44097, #163749, #68332, #35156 ) ) ;
#76346 = DIRECTION ( 'NONE',  ( 1.000000000000000000, -2.986185139342066440E-16, 6.665775143889693760E-16 ) ) ;
#76349 = ORIENTED_EDGE ( 'NONE', *, *, #63486, .T. ) ;
#76348 = DIRECTION ( 'NONE',  ( 0.000000000000000000, -6.938893903907222067E-15, 1.000000000000000000 ) ) ;
#76352 = LINE ( 'NONE', #178061, #31395 ) ;
#76351 = CARTESIAN_POINT ( 'NONE',  ( 23.15000000000000213, 85.50000000001159606, -59.62913836187181715 ) ) ;
#76350 = AXIS2_PLACEMENT_3D ( 'NONE', #14797, #53893, #215525 ) ;
#76353 = EDGE_CURVE ( 'NONE', #198469, #56261, #187868, .T. ) ;
#76355 = ORIENTED_EDGE ( 'NONE', *, *, #51216, .F. ) ;
#76354 = CARTESIAN_POINT ( 'NONE',  ( 21.05000000000000071, -11.48912529306489994, -64.00000000000000000 ) ) ;
#76356 = ORIENTED_EDGE ( 'NONE', *, *, #252204, .T. ) ;
#76357 = LINE ( 'NONE', #155943, #201478 ) ;
#76358 = DIRECTION ( 'NONE',  ( -0.000000000000000000, 6.982962677686266711E-15, -1.000000000000000000 ) ) ;
#76359 = ADVANCED_FACE ( 'NONE', ( #203113 ), #42760, .F. ) ;
#76360 = CARTESIAN_POINT ( 'NONE',  ( 18.49999999999999289, 6.450000000011156587, -21.75000000000000355 ) ) ;
#76361 = CIRCLE ( 'NONE', #222089, 11.90000000000000746 ) ;
#76362 = SPHERICAL_SURFACE ( 'NONE', #240160, 0.1000000000000000056 ) ;
#76363 = LINE ( 'NONE', #214598, #130435 ) ;
#76364 = DIRECTION ( 'NONE',  ( 1.000000000000000000, 0.000000000000000000, 0.000000000000000000 ) ) ;
#76365 = VECTOR ( 'NONE', #35299, 1000.000000000000000 ) ;
#76366 = CIRCLE ( 'NONE', #1542, 0.1000000000000031558 ) ;
#76367 = EDGE_CURVE ( 'NONE', #254207, #178561, #225219, .T. ) ;
#76369 = CIRCLE ( 'NONE', #222104, 0.2000000000000000944 ) ;
#76368 = CARTESIAN_POINT ( 'NONE',  ( -16.90138253750127006, 66.05000000001201954, -115.8115447766197974 ) ) ;
#76370 = ORIENTED_EDGE ( 'NONE', *, *, #24683, .T. ) ;
#76371 = ORIENTED_EDGE ( 'NONE', *, *, #245561, .F. ) ;
#76372 = CARTESIAN_POINT ( 'NONE',  ( 21.05000000000000071, 30.78786553159818951, -252.2909008153935133 ) ) ;
#76373 = ORIENTED_EDGE ( 'NONE', *, *, #216243, .T. ) ;
#76374 = DIRECTION ( 'NONE',  ( -1.000000000000000000, -0.000000000000000000, 0.000000000000000000 ) ) ;
#76375 = DIRECTION ( 'NONE',  ( 0.000000000000000000, 0.000000000000000000, -1.000000000000000000 ) ) ;
#76376 = LINE ( 'NONE', #1976, #134495 ) ;
#76377 = ORIENTED_EDGE ( 'NONE', *, *, #33799, .F. ) ;
#76378 = CARTESIAN_POINT ( 'NONE',  ( -13.54036565897075484, 66.54845833862648874, -118.0692319856938184 ) ) ;
#76379 = VERTEX_POINT ( 'NONE', #206970 ) ;
#76380 = CARTESIAN_POINT ( 'NONE',  ( -20.85000000000000142, -1.835859311432481045, -145.6044391687985637 ) ) ;
#76381 = ORIENTED_EDGE ( 'NONE', *, *, #112441, .T. ) ;
#76382 = CARTESIAN_POINT ( 'NONE',  ( -20.85000000000000142, 7.675662554762638479, -241.7139905447625381 ) ) ;
#76383 = CARTESIAN_POINT ( 'NONE',  ( 18.40000000000000213, 8.780520186313284015, -245.4165333277510115 ) ) ;
#76384 = VECTOR ( 'NONE', #52254, 1000.000000000000000 ) ;
#76385 = DIRECTION ( 'NONE',  ( -0.7071067811865388020, 0.7071067811865561215, 0.000000000000000000 ) ) ;
#76386 = ORIENTED_EDGE ( 'NONE', *, *, #213360, .F. ) ;
#76387 = CIRCLE ( 'NONE', #184727, 0.09999999999999939493 ) ;
#76388 = CARTESIAN_POINT ( 'NONE',  ( -21.05000000000000071, 44.58277672189309015, -247.4925639031954745 ) ) ;
#76390 = EDGE_LOOP ( 'NONE', ( #79355, #102353, #87680, #249241 ) ) ;
#76389 = DIRECTION ( 'NONE',  ( 0.000000000000000000, 0.000000000000000000, -1.000000000000000000 ) ) ;
#76391 = AXIS2_PLACEMENT_3D ( 'NONE', #22477, #44593, #225766 ) ;
#76392 = FACE_OUTER_BOUND ( 'NONE', #155497, .T. ) ;
#76393 = VERTEX_POINT ( 'NONE', #240966 ) ;
#76394 =( BOUNDED_SURFACE ( )  B_SPLINE_SURFACE ( 3, 2, ( 
 ( #62505, #142025, #6361 ),
 ( #165461, #128897, #89746 ),
 ( #227991, #187600, #109304 ),
 ( #8944, #208448, #66352 ) ),
 .UNSPECIFIED., .F., .F., .T. ) 
 B_SPLINE_SURFACE_WITH_KNOTS ( ( 4, 4 ),
 ( 3, 3 ),
 ( 0.0006461284895273985886, 0.0007503702773985944244 ),
 ( 0.000000000000000000, 1.000000000000000000 ),
 .UNSPECIFIED. ) 
 GEOMETRIC_REPRESENTATION_ITEM ( )  RATIONAL_B_SPLINE_SURFACE ( (
 ( 1.000000000000000000, 0.7071067811865475727, 1.000000000000000000),
 ( 1.000000000000000000, 0.7076476444648753805, 1.000000000000000000),
 ( 1.000000000000000000, 0.7075727925191906964, 1.000000000000000000),
 ( 1.000000000000000000, 0.7071067811865475727, 1.000000000000000000) ) ) 
 REPRESENTATION_ITEM ( '' )  SURFACE ( )  );
#76395 = EDGE_CURVE ( 'NONE', #174683, #237270, #171341, .T. ) ;
#76396 = ORIENTED_EDGE ( 'NONE', *, *, #93795, .F. ) ;
#76397 = AXIS2_PLACEMENT_3D ( 'NONE', #76128, #17441, #176540 ) ;
#76398 = CIRCLE ( 'NONE', #51443, 0.09999999999999939493 ) ;
#76399 = DIRECTION ( 'NONE',  ( -0.000000000000000000, 0.000000000000000000, -1.000000000000000000 ) ) ;
#76400 = ORIENTED_EDGE ( 'NONE', *, *, #95880, .T. ) ;
#76401 = LINE ( 'NONE', #153442, #201645 ) ;
#76402 = EDGE_CURVE ( 'NONE', #92927, #249092, #45326, .T. ) ;
#76403 = CARTESIAN_POINT ( 'NONE',  ( 21.05000000000000071, 69.58602111852277972, -69.43730836824991570 ) ) ;
#76404 = EDGE_CURVE ( 'NONE', #45390, #33354, #204577, .T. ) ;
#76405 = DIRECTION ( 'NONE',  ( 1.000000000000000000, 0.000000000000000000, 0.000000000000000000 ) ) ;
#76406 = PLANE ( 'NONE',  #64286 ) ;
#76407 = AXIS2_PLACEMENT_3D ( 'NONE', #122166, #77882, #99992 ) ;
#76408 = CARTESIAN_POINT ( 'NONE',  ( -21.14250536705909411, 1.115600667400684642E-11, -60.48182782311928918 ) ) ;
#76409 = CIRCLE ( 'NONE', #226228, 0.5000000000000004441 ) ;
#76411 = ORIENTED_EDGE ( 'NONE', *, *, #249926, .T. ) ;
#76410 = EDGE_CURVE ( 'NONE', #18420, #2705, #38026, .T. ) ;
#76412 = VECTOR ( 'NONE', #245509, 1000.000000000000000 ) ;
#76413 = EDGE_CURVE ( 'NONE', #43432, #101652, #87858, .T. ) ;
#76414 = VECTOR ( 'NONE', #113344, 1000.000000000000114 ) ;
#76415 = CARTESIAN_POINT ( 'NONE',  ( 20.94999999999999574, 1.162701749938009677, -8.000000000000000000 ) ) ;
#76416 = CARTESIAN_POINT ( 'NONE',  ( -20.96428641294177808, 64.25000000001195133, -109.8482143065830456 ) ) ;
#76417 = CARTESIAN_POINT ( 'NONE',  ( -21.02374657821563630, 11.60000000083177696, -160.5717967701983184 ) ) ;
#76418 = EDGE_CURVE ( 'NONE', #25096, #106161, #183747, .T. ) ;
#76419 = ORIENTED_EDGE ( 'NONE', *, *, #18943, .T. ) ;
#76420 = CARTESIAN_POINT ( 'NONE',  ( -23.15000000000000213, 4.350000000011156054, -79.15000000000004832 ) ) ;
#76422 = EDGE_CURVE ( 'NONE', #172262, #60290, #104596, .T. ) ;
#76421 = ORIENTED_EDGE ( 'NONE', *, *, #255373, .F. ) ;
#76423 = DIRECTION ( 'NONE',  ( 0.000000000000000000, 1.000000000000000000, 6.982962677686266711E-15 ) ) ;
#76425 = ORIENTED_EDGE ( 'NONE', *, *, #185104, .F. ) ;
#76424 = AXIS2_PLACEMENT_3D ( 'NONE', #248308, #207921, #30568 ) ;
#76426 = DIRECTION ( 'NONE',  ( 0.000000000000000000, 0.000000000000000000, 1.000000000000000000 ) ) ;
#76427 = FACE_OUTER_BOUND ( 'NONE', #170666, .T. ) ;
#76428 = EDGE_CURVE ( 'NONE', #246321, #4110, #221135, .T. ) ;
#76430 = VERTEX_POINT ( 'NONE', #81844 ) ;
#76429 = DIRECTION ( 'NONE',  ( 1.000000000000000000, 0.000000000000000000, 0.000000000000000000 ) ) ;
#76431 = CARTESIAN_POINT ( 'NONE',  ( -18.39999999999999858, 8.841736820195468027, -245.4273993276875956 ) ) ;
#76432 = VERTEX_POINT ( 'NONE', #161445 ) ;
#76433 = VECTOR ( 'NONE', #210013, 1000.000000000000000 ) ;
#76434 = DIRECTION ( 'NONE',  ( 1.000000000000000000, 0.000000000000000000, 0.000000000000000000 ) ) ;
#76435 = DIRECTION ( 'NONE',  ( 0.000000000000000000, 0.4721928772777351790, 0.8814952561688427224 ) ) ;
#76436 = ORIENTED_EDGE ( 'NONE', *, *, #255338, .F. ) ;
#76437 = CIRCLE ( 'NONE', #226445, 3.970710678118656300 ) ;
#76438 = CARTESIAN_POINT ( 'NONE',  ( -23.25000000000000000, 6.857177884343597540, -212.0437362999421680 ) ) ;
#76439 = FACE_OUTER_BOUND ( 'NONE', #134592, .T. ) ;
#76440 = ORIENTED_EDGE ( 'NONE', *, *, #32646, .F. ) ;
#76441 = CARTESIAN_POINT ( 'NONE',  ( 21.05000000000000071, 10.05622153401856522, -228.2005611962535454 ) ) ;
#76442 = VECTOR ( 'NONE', #39928, 1000.000000000000000 ) ;
#76443 = ORIENTED_EDGE ( 'NONE', *, *, #61425, .F. ) ;
#76444 = AXIS2_PLACEMENT_3D ( 'NONE', #176503, #153116, #253441 ) ;
#76445 = ADVANCED_FACE ( 'NONE', ( #110429 ), #108734, .T. ) ;
#76446 = CARTESIAN_POINT ( 'NONE',  ( -18.40000000000000213, 31.05627573922685514, -233.2203535436961488 ) ) ;
#76447 = TOROIDAL_SURFACE ( 'NONE', #230600, 11.65000000000000036, 0.1000000000000000056 ) ;
#76448 = CARTESIAN_POINT ( 'NONE',  ( 21.30000000000002558, 76.00000000001168132, -73.57310748452432847 ) ) ;
#76449 = EDGE_CURVE ( 'NONE', #233233, #101698, #233643, .T. ) ;
#76450 = EDGE_CURVE ( 'NONE', #75919, #223695, #114283, .T. ) ;
#76452 = ORIENTED_EDGE ( 'NONE', *, *, #14978, .T. ) ;
#76451 = DIRECTION ( 'NONE',  ( -0.000000000000000000, 0.8660254037844377084, 0.5000000000000016653 ) ) ;
#76453 = LINE ( 'NONE', #173045, #128366 ) ;
#76454 = CARTESIAN_POINT ( 'NONE',  ( 18.50000000000000000, -9.499999999999998224, 11.75000000000000000 ) ) ;
#76455 = CARTESIAN_POINT ( 'NONE',  ( -20.94999999999999929, 86.10439672154322466, -209.4215112426525138 ) ) ;
#76457 = PLANE ( 'NONE',  #71941 ) ;
#76456 = CARTESIAN_POINT ( 'NONE',  ( -21.55000000000000426, 68.29142135624910281, -81.77310748452435973 ) ) ;
#76458 = DIRECTION ( 'NONE',  ( -1.000000000000000000, 0.000000000000000000, -0.000000000000000000 ) ) ;
#76459 = SPHERICAL_SURFACE ( 'NONE', #77648, 0.1000000000000000056 ) ;
#76460 = CARTESIAN_POINT ( 'NONE',  ( -18.59999999999999787, 31.49702336731128582, -233.4564499823349877 ) ) ;
#76461 = CIRCLE ( 'NONE', #226289, 12.87500000000000711 ) ;
#76462 = CARTESIAN_POINT ( 'NONE',  ( -21.51976009735018991, 69.08954155835293420, -136.5231074845243313 ) ) ;
#76463 = CIRCLE ( 'NONE', #255493, 11.79999999999999893 ) ;
#76464 = VECTOR ( 'NONE', #82838, 1000.000000000000000 ) ;
#76465 = ORIENTED_EDGE ( 'NONE', *, *, #76066, .T. ) ;
#76466 = VERTEX_POINT ( 'NONE', #132573 ) ;
#76467 = DIRECTION ( 'NONE',  ( 0.000000000000000000, -0.9770955615652943127, -0.2128009952265311755 ) ) ;
#76469 = ORIENTED_EDGE ( 'NONE', *, *, #238486, .T. ) ;
#76468 = CARTESIAN_POINT ( 'NONE',  ( -18.40000000000000213, 33.92901942162173157, -235.0579290632217067 ) ) ;
#76470 = ORIENTED_EDGE ( 'NONE', *, *, #88654, .F. ) ;
#76471 = DIRECTION ( 'NONE',  ( -0.000000000000000000, -6.982962677686266711E-15, 1.000000000000000000 ) ) ;
#76472 = ORIENTED_EDGE ( 'NONE', *, *, #216710, .T. ) ;
#76473 = LINE ( 'NONE', #158616, #146743 ) ;
#76474 = B_SPLINE_CURVE_WITH_KNOTS ( 'NONE', 3,
 ( #102107, #157331, #164685, #244196 ),
 .UNSPECIFIED., .F., .F.,
 ( 4, 4 ),
 ( 0.000000000000000000, 0.001767853679387121216 ),
 .UNSPECIFIED. ) ;
#76475 = VERTEX_POINT ( 'NONE', #148281 ) ;
#76476 = CARTESIAN_POINT ( 'NONE',  ( 23.14999999999999147, 76.00000000001195133, -103.0231074845243171 ) ) ;
#76478 = ORIENTED_EDGE ( 'NONE', *, *, #88215, .F. ) ;
#76477 = ORIENTED_EDGE ( 'NONE', *, *, #35173, .T. ) ;
#76479 = ORIENTED_EDGE ( 'NONE', *, *, #196603, .T. ) ;
#76480 = VERTEX_POINT ( 'NONE', #131278 ) ;
#76481 = ORIENTED_EDGE ( 'NONE', *, *, #179163, .F. ) ;
#76482 = DIRECTION ( 'NONE',  ( 6.938893903907222067E-15, -1.000000000000000000, -0.000000000000000000 ) ) ;
#76483 = CIRCLE ( 'NONE', #51523, 0.09999999999999939493 ) ;
#76484 = CARTESIAN_POINT ( 'NONE',  ( -18.59999999999999787, 76.00000000001244871, -170.0231074845243597 ) ) ;
#76486 = ORIENTED_EDGE ( 'NONE', *, *, #210708, .F. ) ;
#76485 = DIRECTION ( 'NONE',  ( -1.000000000000000000, 0.000000000000000000, 0.000000000000000000 ) ) ;
#76487 = CARTESIAN_POINT ( 'NONE',  ( -21.07094088545304800, 33.98475570745946328, -243.8237622992367051 ) ) ;
#76488 = DIRECTION ( 'NONE',  ( 0.000000000000000000, 0.000000000000000000, -1.000000000000000000 ) ) ;
#76490 = ORIENTED_EDGE ( 'NONE', *, *, #119877, .T. ) ;
#76489 = DIRECTION ( 'NONE',  ( 1.000000000000000000, -0.000000000000000000, -0.000000000000000000 ) ) ;
#76491 = CARTESIAN_POINT ( 'NONE',  ( -18.50000000000000000, 11.64999999999999680, -12.15000000000000036 ) ) ;
#76492 = ORIENTED_EDGE ( 'NONE', *, *, #25986, .T. ) ;
#76493 = DIRECTION ( 'NONE',  ( 9.044546369203337730E-15, 0.7397360091702647189, 0.6728971962616949742 ) ) ;
#76495 = ORIENTED_EDGE ( 'NONE', *, *, #64538, .T. ) ;
#76494 = FACE_OUTER_BOUND ( 'NONE', #31165, .T. ) ;
#76496 = DIRECTION ( 'NONE',  ( 1.000000000000000000, 2.952720810173289112E-16, -0.000000000000000000 ) ) ;
#76498 = EDGE_CURVE ( 'NONE', #214842, #109178, #53017, .T. ) ;
#76497 = FACE_OUTER_BOUND ( 'NONE', #29004, .T. ) ;
#76499 = LINE ( 'NONE', #88675, #77331 ) ;
#76500 = ORIENTED_EDGE ( 'NONE', *, *, #64882, .F. ) ;
#76502 = DIRECTION ( 'NONE',  ( 0.000000000000000000, 0.000000000000000000, 1.000000000000000000 ) ) ;
#76501 = DIRECTION ( 'NONE',  ( -1.000000000000000000, -3.265361837132813093E-16, 0.000000000000000000 ) ) ;
#76503 = EDGE_CURVE ( 'NONE', #148589, #204523, #133669, .T. ) ;
#76504 = VECTOR ( 'NONE', #206601, 1000.000000000000000 ) ;
#76505 = DIRECTION ( 'NONE',  ( -1.000000000000000000, -0.000000000000000000, 0.000000000000000000 ) ) ;
#76506 = AXIS2_PLACEMENT_3D ( 'NONE', #252712, #94923, #177069 ) ;
#76507 = DIRECTION ( 'NONE',  ( -0.000000000000000000, -0.9875055080513799322, 0.1575844902526464253 ) ) ;
#76508 = CARTESIAN_POINT ( 'NONE',  ( 20.94999999999999929, 5.850000000011156942, -90.36750277572211587 ) ) ;
#76509 = ORIENTED_EDGE ( 'NONE', *, *, #69585, .F. ) ;
#76511 = ORIENTED_EDGE ( 'NONE', *, *, #25094, .T. ) ;
#76510 = AXIS2_PLACEMENT_3D ( 'NONE', #122060, #97316, #118205 ) ;
#76512 = EDGE_CURVE ( 'NONE', #169064, #146292, #167035, .T. ) ;
#76513 = CARTESIAN_POINT ( 'NONE',  ( -21.14999999999999503, 1.115524773248610657E-11, -127.4593430482987912 ) ) ;
#76515 = ADVANCED_FACE ( 'NONE', ( #210820 ), #29648, .T. ) ;
#76514 = CARTESIAN_POINT ( 'NONE',  ( -20.64999999999999858, 1.940186915899004161, -121.1708807889467039 ) ) ;
#76516 = EDGE_LOOP ( 'NONE', ( #3144, #113466, #113388, #408 ) ) ;
#76517 = DIRECTION ( 'NONE',  ( 1.000000000000000000, 0.000000000000000000, 0.000000000000000000 ) ) ;
#76518 = ORIENTED_EDGE ( 'NONE', *, *, #166501, .T. ) ;
#76519 = FACE_OUTER_BOUND ( 'NONE', #237945, .T. ) ;
#76520 = DIRECTION ( 'NONE',  ( 1.000000000000000000, 0.000000000000000000, 0.000000000000000000 ) ) ;
#76521 = ORIENTED_EDGE ( 'NONE', *, *, #178313, .T. ) ;
#76522 = AXIS2_PLACEMENT_3D ( 'NONE', #64493, #223540, #184428 ) ;
#76523 = LINE ( 'NONE', #115667, #31977 ) ;
#76524 = FILL_AREA_STYLE_COLOUR ( '', #6516 ) ;
#76525 = TOROIDAL_SURFACE ( 'NONE', #97345, 0.2000000000000000111, 0.1000000000000000056 ) ;
#76526 = ORIENTED_EDGE ( 'NONE', *, *, #32228, .F. ) ;
#76527 = EDGE_CURVE ( 'NONE', #218429, #13339, #90863, .T. ) ;
#76528 = ORIENTED_EDGE ( 'NONE', *, *, #112042, .T. ) ;
#76529 = ADVANCED_FACE ( 'NONE', ( #50433 ), #230380, .T. ) ;
#76530 = VECTOR ( 'NONE', #77972, 1000.000000000000000 ) ;
#76531 = VERTEX_POINT ( 'NONE', #191288 ) ;
#76532 = VECTOR ( 'NONE', #69078, 1000.000000000000000 ) ;
#76533 = FACE_OUTER_BOUND ( 'NONE', #32418, .T. ) ;
#76534 = CARTESIAN_POINT ( 'NONE',  ( 20.94999999999999929, -1.835341550213257733, -112.0551512925630249 ) ) ;
#76535 = CARTESIAN_POINT ( 'NONE',  ( 21.14999999999999858, 11.65000000001116298, -112.6500000000000341 ) ) ;
#76536 = DIRECTION ( 'NONE',  ( 0.000000000000000000, -0.4721928772777346239, -0.8814952561688430555 ) ) ;
#76537 = CARTESIAN_POINT ( 'NONE',  ( 12.93279065517212345, 66.58230930894892197, -118.3815067877597897 ) ) ;
#76539 = FACE_OUTER_BOUND ( 'NONE', #84793, .T. ) ;
#76538 = CARTESIAN_POINT ( 'NONE',  ( 21.05000000000000071, 0.09779029132037916905, -161.2421853895184540 ) ) ;
#76541 = VERTEX_POINT ( 'NONE', #251210 ) ;
#76540 = FACE_OUTER_BOUND ( 'NONE', #186309, .T. ) ;
#76542 = DIRECTION ( 'NONE',  ( 0.000000000000000000, 0.000000000000000000, 1.000000000000000000 ) ) ;
#76543 = ORIENTED_EDGE ( 'NONE', *, *, #164813, .F. ) ;
#76544 = CARTESIAN_POINT ( 'NONE',  ( -16.86578989773641979, 22.89342784614964543, -230.8502347937079264 ) ) ;
#76545 = ORIENTED_EDGE ( 'NONE', *, *, #215128, .T. ) ;
#76546 = ORIENTED_EDGE ( 'NONE', *, *, #168294, .T. ) ;
#76547 = LINE ( 'NONE', #176974, #104448 ) ;
#76549 = VECTOR ( 'NONE', #74959, 1000.000000000000000 ) ;
#76548 = CARTESIAN_POINT ( 'NONE',  ( -21.07928932188134041, 6.328516656409861163, -133.9011048543453910 ) ) ;
#76550 = CYLINDRICAL_SURFACE ( 'NONE', #129362, 0.09999999999999939493 ) ;
#76551 = AXIS2_PLACEMENT_3D ( 'NONE', #221402, #162759, #42796 ) ;
#76552 = VERTEX_POINT ( 'NONE', #32206 ) ;
#76553 = EDGE_CURVE ( 'NONE', #55598, #10735, #179660, .T. ) ;
#76554 = FACE_OUTER_BOUND ( 'NONE', #58336, .T. ) ;
#76555 = VECTOR ( 'NONE', #142099, 1000.000000000000000 ) ;
#76556 = EDGE_CURVE ( 'NONE', #175607, #226006, #206316, .T. ) ;
#76557 = CARTESIAN_POINT ( 'NONE',  ( -20.64999999999999858, 66.26558728512915764, -222.7970849955717938 ) ) ;
#76558 = ORIENTED_EDGE ( 'NONE', *, *, #66424, .T. ) ;
#76559 = ORIENTED_EDGE ( 'NONE', *, *, #231985, .F. ) ;
#76560 = AXIS2_PLACEMENT_3D ( 'NONE', #63059, #26531, #22689 ) ;
#76561 = DIRECTION ( 'NONE',  ( -1.000000000000000000, 0.000000000000000000, 0.000000000000000000 ) ) ;
#76562 = ORIENTED_EDGE ( 'NONE', *, *, #117024, .T. ) ;
#76563 = CARTESIAN_POINT ( 'NONE',  ( -16.93230518875208546, 60.87094908132711168, -221.1000775826128972 ) ) ;
#76564 = DIRECTION ( 'NONE',  ( 0.000000000000000000, 0.000000000000000000, -1.000000000000000000 ) ) ;
#76565 = ORIENTED_EDGE ( 'NONE', *, *, #66186, .F. ) ;
#76566 = DIRECTION ( 'NONE',  ( -1.000000000000000000, 3.265361837132813093E-16, 2.280189983783949500E-30 ) ) ;
#76568 = EDGE_CURVE ( 'NONE', #229103, #164631, #30933, .T. ) ;
#76567 = CARTESIAN_POINT ( 'NONE',  ( 21.11344571971268280, 65.38212097649376631, -157.7770865921222594 ) ) ;
#76569 = EDGE_LOOP ( 'NONE', ( #34674, #166519, #225584, #215400 ) ) ;
#76570 = VECTOR ( 'NONE', #110729, 1000.000000000000000 ) ;
#76571 = CIRCLE ( 'NONE', #80835, 0.09999999999999939493 ) ;
#76572 = EDGE_CURVE ( 'NONE', #53762, #53755, #71522, .T. ) ;
#76573 = AXIS2_PLACEMENT_3D ( 'NONE', #242415, #63792, #122496 ) ;
#76574 = CARTESIAN_POINT ( 'NONE',  ( -21.64999999999999858, 66.65000000001255387, -182.6731074845244223 ) ) ;
#76575 = CARTESIAN_POINT ( 'NONE',  ( 18.59999999999999076, 6.650000000011155876, -155.1500000000000057 ) ) ;
#76576 = EDGE_CURVE ( 'NONE', #71110, #99076, #12642, .T. ) ;
#76577 = DIRECTION ( 'NONE',  ( 0.000000000000000000, 0.9126074666063660468, 0.4088369013363524762 ) ) ;
#76578 = VERTEX_POINT ( 'NONE', #153464 ) ;
#76579 = DIRECTION ( 'NONE',  ( 0.000000000000000000, 0.008583690987128059571, -0.9999631594459056361 ) ) ;
#76580 = EDGE_LOOP ( 'NONE', ( #36659, #108095, #117643, #96824 ) ) ;
#76581 = CARTESIAN_POINT ( 'NONE',  ( 20.94999999999999574, 4.287142817744433287, -211.9955491415249469 ) ) ;
#76582 = EDGE_CURVE ( 'NONE', #234345, #729, #217216, .T. ) ;
#76583 = CARTESIAN_POINT ( 'NONE',  ( 18.39999999999999858, 85.68240343348806221, -62.86626410711144786 ) ) ;
#76584 = DIRECTION ( 'NONE',  ( 0.000000000000000000, -0.3488585713686311318, -0.9371753822965249725 ) ) ;
#76585 = DIRECTION ( 'NONE',  ( -4.801466763864314121E-15, 0.2605042016806606298, 0.9654727137038736640 ) ) ;
#76586 = LINE ( 'NONE', #160005, #109028 ) ;
#76587 = DIRECTION ( 'NONE',  ( 0.000000000000000000, 0.000000000000000000, -1.000000000000000000 ) ) ;
#76588 = ORIENTED_EDGE ( 'NONE', *, *, #105237, .T. ) ;
#76589 = CARTESIAN_POINT ( 'NONE',  ( -18.40000000000000213, 43.42149616655404287, -233.9497663708821165 ) ) ;
#76590 = EDGE_CURVE ( 'NONE', #108024, #47116, #29659, .T. ) ;
#76591 = LINE ( 'NONE', #156164, #127322 ) ;
#76592 = DIRECTION ( 'NONE',  ( -1.000000000000000000, 0.000000000000000000, -0.000000000000000000 ) ) ;
#76594 = AXIS2_PLACEMENT_3D ( 'NONE', #98457, #195063, #178065 ) ;
#76593 = CARTESIAN_POINT ( 'NONE',  ( -21.04999999999994387, 67.65000000001118963, -25.49719488170504533 ) ) ;
#76595 = AXIS2_PLACEMENT_3D ( 'NONE', #204616, #125113, #122544 ) ;
#76596 = CARTESIAN_POINT ( 'NONE',  ( -23.15000000000000213, 55.49311008795314137, -234.6486875357297492 ) ) ;
#76597 = ORIENTED_EDGE ( 'NONE', *, *, #104904, .F. ) ;
#76598 = ORIENTED_EDGE ( 'NONE', *, *, #89630, .F. ) ;
#76599 = CARTESIAN_POINT ( 'NONE',  ( 23.15000000000000213, 85.00000000001222134, -145.9170766071767389 ) ) ;
#76600 = VECTOR ( 'NONE', #56103, 1000.000000000000000 ) ;
#76601 = CARTESIAN_POINT ( 'NONE',  ( -18.59999999999999787, -1.851617760457748618, -179.1031897196036766 ) ) ;
#76602 = DIRECTION ( 'NONE',  ( 0.000000000000000000, 6.982962677686266711E-15, -1.000000000000000000 ) ) ;
#76603 = CARTESIAN_POINT ( 'NONE',  ( -21.05000000000000071, 69.58624026620243797, -203.4374944237204943 ) ) ;
#76604 = AXIS2_PLACEMENT_3D ( 'NONE', #138076, #217603, #40315 ) ;
#76605 = CARTESIAN_POINT ( 'NONE',  ( -20.15000000000000568, 13.60062771638445511, -219.7860569715900567 ) ) ;
#76606 = ORIENTED_EDGE ( 'NONE', *, *, #198986, .T. ) ;
#76607 = DIRECTION ( 'NONE',  ( -1.000000000000000000, -0.000000000000000000, -0.000000000000000000 ) ) ;
#76608 = AXIS2_PLACEMENT_3D ( 'NONE', #9905, #108997, #125998 ) ;
#76610 = TOROIDAL_SURFACE ( 'NONE', #209907, 11.65000000000000036, 0.1000000000000000056 ) ;
#76609 = CARTESIAN_POINT ( 'NONE',  ( 21.05000000000000071, 4.999999999999997335, -21.09473398108690390 ) ) ;
#76611 = ORIENTED_EDGE ( 'NONE', *, *, #115605, .T. ) ;
#76612 = DIRECTION ( 'NONE',  ( 0.000000000000000000, 1.000000000000000000, -5.551115123125777653E-14 ) ) ;
#76613 = CIRCLE ( 'NONE', #164124, 0.1999999999999987899 ) ;
#76614 = CARTESIAN_POINT ( 'NONE',  ( -23.15000000000000213, 62.92003201576280702, -207.2439188921395896 ) ) ;
#76615 = VECTOR ( 'NONE', #203110, 1000.000000000000000 ) ;
#76616 = VERTEX_POINT ( 'NONE', #88271 ) ;
#76617 = DIRECTION ( 'NONE',  ( 1.000000000000000000, 2.952720810173289112E-16, -0.000000000000000000 ) ) ;
#76618 = ORIENTED_EDGE ( 'NONE', *, *, #192110, .T. ) ;
#76619 = CARTESIAN_POINT ( 'NONE',  ( 20.94999999999999929, 5.400000000011154988, -121.5947339810869465 ) ) ;
#76620 = DIRECTION ( 'NONE',  ( 0.000000000000000000, 0.000000000000000000, 1.000000000000000000 ) ) ;
#76622 = TOROIDAL_SURFACE ( 'NONE', #84977, 0.2000000000000000111, 0.1000000000000000056 ) ;
#76621 = DIRECTION ( 'NONE',  ( 0.000000000000000000, 0.2617529984164856383, 0.9651348961777204138 ) ) ;
#76623 = DIRECTION ( 'NONE',  ( -0.000000000000000000, 0.000000000000000000, 1.000000000000000000 ) ) ;
#76624 = CARTESIAN_POINT ( 'NONE',  ( 20.94999999999999929, 56.27731819600170837, -227.9967441372480437 ) ) ;
#76625 = CARTESIAN_POINT ( 'NONE',  ( 21.05000000000000071, 18.65264105882984680, -228.0115894607347968 ) ) ;
#76626 = LINE ( 'NONE', #132779, #203638 ) ;
#76627 = FACE_OUTER_BOUND ( 'NONE', #53380, .T. ) ;
#76628 = DIRECTION ( 'NONE',  ( 0.000000000000000000, 0.8700118002898356018, -0.4930308989875170078 ) ) ;
#76629 = AXIS2_PLACEMENT_3D ( 'NONE', #66210, #145724, #27111 ) ;
#76630 = ADVANCED_FACE ( 'NONE', ( #59404 ), #137677, .T. ) ;
#76631 = CARTESIAN_POINT ( 'NONE',  ( 21.08804582317339893, 22.20750643078865139, -231.7382219064953404 ) ) ;
#76632 = DIRECTION ( 'NONE',  ( -1.000000000000000000, 0.000000000000000000, -0.000000000000000000 ) ) ;
#76633 = CARTESIAN_POINT ( 'NONE',  ( 18.50211644919734866, 10.30207779525984968, -206.4895520716782187 ) ) ;
#76634 = CIRCLE ( 'NONE', #101733, 0.1999999999999987899 ) ;
#76635 = DIRECTION ( 'NONE',  ( 0.1538461538461510236, 0.9880948137434718559, 0.000000000000000000 ) ) ;
#76636 = DIRECTION ( 'NONE',  ( -1.000000000000000000, -3.265361837132813093E-16, 0.000000000000000000 ) ) ;
#76637 = AXIS2_PLACEMENT_3D ( 'NONE', #113640, #54926, #92781 ) ;
#76638 = AXIS2_PLACEMENT_3D ( 'NONE', #193690, #149444, #131134 ) ;
#76639 = ORIENTED_EDGE ( 'NONE', *, *, #85825, .T. ) ;
#76640 = CARTESIAN_POINT ( 'NONE',  ( 18.49999999999999289, 11.75000000001115552, -91.85000000000003695 ) ) ;
#76642 = EDGE_CURVE ( 'NONE', #180800, #98196, #212971, .T. ) ;
#76641 = CARTESIAN_POINT ( 'NONE',  ( 20.94999999999999929, 23.68770167995059239, -252.8127582590406348 ) ) ;
#76643 = ORIENTED_EDGE ( 'NONE', *, *, #17750, .T. ) ;
#76644 = DIRECTION ( 'NONE',  ( 0.000000000000000000, 0.000000000000000000, -1.000000000000000000 ) ) ;
#76645 = EDGE_CURVE ( 'NONE', #2008, #210270, #234220, .T. ) ;
#76646 = EDGE_CURVE ( 'NONE', #83134, #99760, #25707, .T. ) ;
#76647 = CARTESIAN_POINT ( 'NONE',  ( -23.25000000000000000, 76.00000000001142553, -36.02310748452432421 ) ) ;
#76648 = ORIENTED_EDGE ( 'NONE', *, *, #188234, .T. ) ;
#76649 = CARTESIAN_POINT ( 'NONE',  ( 21.05000000000000071, 6.349993537836307489, -199.7193832479148625 ) ) ;
#76650 = CARTESIAN_POINT ( 'NONE',  ( 21.05000000000000071, 87.29603075034721371, -99.97520832486037534 ) ) ;
#76651 = AXIS2_PLACEMENT_3D ( 'NONE', #57772, #197292, #52640 ) ;
#76652 = TOROIDAL_SURFACE ( 'NONE', #39276, 11.65000000000000036, 0.1000000000000000056 ) ;
#76653 = AXIS2_PLACEMENT_3D ( 'NONE', #176562, #39636, #136097 ) ;
#76654 = ORIENTED_EDGE ( 'NONE', *, *, #22146, .F. ) ;
#76655 = CARTESIAN_POINT ( 'NONE',  ( -20.85000000000000142, 7.120270961708750512, -204.6595630418393057 ) ) ;
#76656 = ADVANCED_FACE ( 'NONE', ( #214659 ), #197922, .T. ) ;
#76657 = ORIENTED_EDGE ( 'NONE', *, *, #50005, .F. ) ;
#76658 = DIRECTION ( 'NONE',  ( 1.441126678808781001E-14, 0.9876197685951252359, 0.1568667991644863424 ) ) ;
#76660 = DIRECTION ( 'NONE',  ( 1.000000000000000000, 0.000000000000000000, 0.000000000000000000 ) ) ;
#76659 = UNCERTAINTY_MEASURE_WITH_UNIT (LENGTH_MEASURE( 1.000000000000000082E-05 ), #152956, 'distance_accuracy_value', 'NONE');
#76661 = CARTESIAN_POINT ( 'NONE',  ( -20.85000000000000142, 7.070967871809997973, -70.74656422186831151 ) ) ;
#76662 = CARTESIAN_POINT ( 'NONE',  ( -20.94999999999999929, 1.360870587203197646, -142.0729979270909951 ) ) ;
#76663 = CARTESIAN_POINT ( 'NONE',  ( -13.54795643572458097, 46.53494637834451453, -234.7711487335851643 ) ) ;
#76664 = CARTESIAN_POINT ( 'NONE',  ( 20.27550659511088682, 41.33268472976309482, -237.3587910501520071 ) ) ;
#76665 = DIRECTION ( 'NONE',  ( -1.000000000000000000, 8.673617379884087537E-15, 0.000000000000000000 ) ) ;
#76667 = EDGE_LOOP ( 'NONE', ( #2062, #58437, #145290, #88150, #122117 ) ) ;
#76666 = DIRECTION ( 'NONE',  ( -1.000000000000000000, 1.836970198721029934E-16, 1.282749433769087582E-30 ) ) ;
#76668 = ORIENTED_EDGE ( 'NONE', *, *, #209794, .T. ) ;
#76670 = CARTESIAN_POINT ( 'NONE',  ( -21.00448002041608575, 64.25000000001159606, -62.67476662221319117 ) ) ;
#76669 = DIRECTION ( 'NONE',  ( 0.000000000000000000, -0.2617529984165031243, -0.9651348961777157509 ) ) ;
#76672 = ORIENTED_EDGE ( 'NONE', *, *, #250111, .F. ) ;
#76671 = DIRECTION ( 'NONE',  ( -0.000000000000000000, 0.000000000000000000, -1.000000000000000000 ) ) ;
#76673 = ORIENTED_EDGE ( 'NONE', *, *, #29484, .T. ) ;
#76674 = CARTESIAN_POINT ( 'NONE',  ( -16.92563707711778775, 66.03100930561545567, -149.1423491850004552 ) ) ;
#76675 = DIRECTION ( 'NONE',  ( -1.000000000000000000, 0.000000000000000000, 0.000000000000000000 ) ) ;
#76676 = CIRCLE ( 'NONE', #1655, 0.09999999999999939493 ) ;
#76677 = EDGE_CURVE ( 'NONE', #45881, #250378, #118137, .T. ) ;
#76678 = DIRECTION ( 'NONE',  ( 3.469446951953498700E-14, -0.7899159663865300551, -0.6132151058540831201 ) ) ;
#76679 = LINE ( 'NONE', #96240, #27621 ) ;
#76680 = DIRECTION ( 'NONE',  ( 0.000000000000000000, -6.308085367188367561E-15, 1.000000000000000000 ) ) ;
#76681 = DIRECTION ( 'NONE',  ( 0.000000000000000000, 0.8814952561688416122, -0.4721928772777371219 ) ) ;
#76682 = EDGE_CURVE ( 'NONE', #232467, #222218, #198948, .T. ) ;
#76683 = DIRECTION ( 'NONE',  ( -0.000000000000000000, 0.2617529984165031243, 0.9651348961777157509 ) ) ;
#76684 = ORIENTED_EDGE ( 'NONE', *, *, #12823, .F. ) ;
#76685 = EDGE_LOOP ( 'NONE', ( #198577, #78908, #103993, #2088 ) ) ;
#76686 = DIRECTION ( 'NONE',  ( -1.000000000000000000, 0.000000000000000000, 0.000000000000000000 ) ) ;
#76687 = VECTOR ( 'NONE', #26980, 1000.000000000000000 ) ;
#76688 = ORIENTED_EDGE ( 'NONE', *, *, #175363, .F. ) ;
#76689 = CARTESIAN_POINT ( 'NONE',  ( 20.95443524775735256, 8.878554263883964737, -142.5337222756001552 ) ) ;
#76690 = ORIENTED_EDGE ( 'NONE', *, *, #93137, .F. ) ;
#76691 = CARTESIAN_POINT ( 'NONE',  ( -23.25000000000000000, 76.00000000001237765, -170.0231074845243597 ) ) ;
#76692 = CIRCLE ( 'NONE', #172426, 0.1000000000000024342 ) ;
#76693 = AXIS2_PLACEMENT_3D ( 'NONE', #75266, #234299, #251292 ) ;
#76694 = CARTESIAN_POINT ( 'NONE',  ( 22.39999999999999503, 7.790779598384535376, -134.0000000000000000 ) ) ;
#76695 = CARTESIAN_POINT ( 'NONE',  ( 21.05000000000000071, 69.55000000001159322, -59.50608031408435039 ) ) ;
#76697 = ORIENTED_EDGE ( 'NONE', *, *, #175897, .T. ) ;
#76696 = CARTESIAN_POINT ( 'NONE',  ( 23.14999999999999503, 69.45000000001149942, -48.27310748452436684 ) ) ;
#76698 = DIRECTION ( 'NONE',  ( 1.000000000000000000, 0.000000000000000000, 3.523657060577910710E-15 ) ) ;
#76699 = ORIENTED_EDGE ( 'NONE', *, *, #188174, .F. ) ;
#76700 = DIRECTION ( 'NONE',  ( -0.000000000000000000, -6.982962677686266711E-15, 1.000000000000000000 ) ) ;
#76701 = DIRECTION ( 'NONE',  ( 0.000000000000000000, -6.982962677686266711E-15, 1.000000000000000000 ) ) ;
#76702 = DIRECTION ( 'NONE',  ( 1.186688945009010077E-16, 1.000000000000000000, 6.982962677686266711E-15 ) ) ;
#76704 = TOROIDAL_SURFACE ( 'NONE', #1690, 0.2000000000000000111, 0.1000000000000000056 ) ;
#76703 = CARTESIAN_POINT ( 'NONE',  ( -16.87331047859649757, 66.05000000001255955, -182.6731074845244223 ) ) ;
#76705 = CARTESIAN_POINT ( 'NONE',  ( -16.27683809663750480, 66.65000000001201386, -115.5731074845243711 ) ) ;
#76706 = ORIENTED_EDGE ( 'NONE', *, *, #72673, .T. ) ;
#76707 = DIRECTION ( 'NONE',  ( 4.239556034732056743E-17, 0.3848449534832867891, 0.9229812358755983270 ) ) ;
#76709 = ORIENTED_EDGE ( 'NONE', *, *, #39455, .F. ) ;
#76708 = CIRCLE ( 'NONE', #14210, 0.5000000000000004441 ) ;
#76712 = ORIENTED_EDGE ( 'NONE', *, *, #113718, .T. ) ;
#76711 = FACE_OUTER_BOUND ( 'NONE', #173383, .T. ) ;
#76710 = LINE ( 'NONE', #53316, #207398 ) ;
#76713 = CARTESIAN_POINT ( 'NONE',  ( 21.05000000000000071, 56.01362831242965967, -232.7091905853083347 ) ) ;
#76714 = VECTOR ( 'NONE', #188690, 1000.000000000000000 ) ;
#76715 = EDGE_CURVE ( 'NONE', #75669, #43158, #39915, .T. ) ;
#76716 = CARTESIAN_POINT ( 'NONE',  ( 23.14999999999999858, 71.00000000001180922, -81.92837350343744163 ) ) ;
#76717 = ORIENTED_EDGE ( 'NONE', *, *, #136879, .T. ) ;
#76720 = ADVANCED_FACE ( 'NONE', ( #116854 ), #136377, .F. ) ;
#76719 = DIRECTION ( 'NONE',  ( 1.000000000000000000, 0.000000000000000000, 0.000000000000000000 ) ) ;
#76718 = VECTOR ( 'NONE', #223181, 999.9999999999998863 ) ;
#76721 = DIRECTION ( 'NONE',  ( 1.000000000000000000, 0.000000000000000000, 0.000000000000000000 ) ) ;
#76722 = ADVANCED_FACE ( 'NONE', ( #219793 ), #41195, .T. ) ;
#76723 = DIRECTION ( 'NONE',  ( 0.000000000000000000, 0.000000000000000000, 1.000000000000000000 ) ) ;
#76724 = EDGE_CURVE ( 'NONE', #56702, #196380, #246289, .T. ) ;
#76725 = EDGE_LOOP ( 'NONE', ( #3927, #205234, #70491, #125196 ) ) ;
#76726 = VECTOR ( 'NONE', #74672, 1000.000000000000000 ) ;
#76727 = DIRECTION ( 'NONE',  ( 1.000000000000000000, 0.000000000000000000, 0.000000000000000000 ) ) ;
#76729 = VERTEX_POINT ( 'NONE', #180688 ) ;
#76728 = ADVANCED_FACE ( 'NONE', ( #62028 ), #221075, .F. ) ;
#76730 = CARTESIAN_POINT ( 'NONE',  ( -20.54999999999999716, 65.86663596189677605, -213.5709895136416776 ) ) ;
#76731 = CARTESIAN_POINT ( 'NONE',  ( -23.15000000000000213, 74.00000000001199396, -116.2477294072864140 ) ) ;
#76732 = CIRCLE ( 'NONE', #47503, 0.09999999999998898659 ) ;
#76733 = CARTESIAN_POINT ( 'NONE',  ( -22.59999999999999787, 11.64957080755595520, -66.90000000000004832 ) ) ;
#76734 = EDGE_CURVE ( 'NONE', #205600, #143381, #108897, .T. ) ;
#76735 = EDGE_LOOP ( 'NONE', ( #130727, #235649, #111843, #252393 ) ) ;
#76736 = CARTESIAN_POINT ( 'NONE',  ( 21.05000000000000071, -11.64999999998883595, -198.0999999999999659 ) ) ;
#76739 = ADVANCED_FACE ( 'NONE', ( #3301 ), #142806, .T. ) ;
#76738 = EDGE_CURVE ( 'NONE', #126698, #127664, #38205, .T. ) ;
#76737 = ORIENTED_EDGE ( 'NONE', *, *, #30754, .T. ) ;
#76740 = DIRECTION ( 'NONE',  ( 6.484947573744953299E-15, 0.7674881895858254310, 0.6410630849193176273 ) ) ;
#76741 = VECTOR ( 'NONE', #66485, 1000.000000000000000 ) ;
#76742 = LINE ( 'NONE', #156323, #188869 ) ;
#76743 = DIRECTION ( 'NONE',  ( -1.000000000000000000, 0.000000000000000000, 0.000000000000000000 ) ) ;
#76744 = VERTEX_POINT ( 'NONE', #184517 ) ;
#76745 = CARTESIAN_POINT ( 'NONE',  ( 21.09696443733127325, 22.97753277350960488, -230.0567122760072039 ) ) ;
#76746 = VECTOR ( 'NONE', #2312, 1000.000000000000227 ) ;
#76747 = CIRCLE ( 'NONE', #114355, 0.09999999999999938105 ) ;
#76749 = TOROIDAL_SURFACE ( 'NONE', #151620, 0.2000000000000000111, 0.1000000000000000056 ) ;
#76748 = LINE ( 'NONE', #250259, #217983 ) ;
#76750 = ADVANCED_FACE ( 'NONE', ( #7161 ), #83915, .F. ) ;
#76751 = ORIENTED_EDGE ( 'NONE', *, *, #255895, .T. ) ;
#76752 = DIRECTION ( 'NONE',  ( 0.000000000000000000, 1.181088324069314461E-14, -1.000000000000000000 ) ) ;
#76753 = EDGE_CURVE ( 'NONE', #194487, #195803, #167211, .T. ) ;
#76755 = EDGE_CURVE ( 'NONE', #143163, #225625, #201518, .T. ) ;
#76754 = DIRECTION ( 'NONE',  ( 0.000000000000000000, -0.9770955615653317272, -0.2128009952263598126 ) ) ;
#76756 = VERTEX_POINT ( 'NONE', #223636 ) ;
#76757 = ADVANCED_FACE ( 'NONE', ( #181970 ), #243207, .T. ) ;
#76758 = DIRECTION ( 'NONE',  ( 0.000000000000000000, 6.982962677686266711E-15, -1.000000000000000000 ) ) ;
#76759 = VERTEX_POINT ( 'NONE', #245794 ) ;
#76761 = ORIENTED_EDGE ( 'NONE', *, *, #205370, .T. ) ;
#76760 = FACE_OUTER_BOUND ( 'NONE', #115403, .T. ) ;
#76762 = EDGE_CURVE ( 'NONE', #10328, #7257, #172757, .T. ) ;
#76765 = ORIENTED_EDGE ( 'NONE', *, *, #2026, .T. ) ;
#76764 = ORIENTED_EDGE ( 'NONE', *, *, #222134, .F. ) ;
#76763 = LINE ( 'NONE', #158902, #255310 ) ;
#76766 = DIRECTION ( 'NONE',  ( 1.000000000000000000, 0.000000000000000000, 0.000000000000000000 ) ) ;
#76767 = CARTESIAN_POINT ( 'NONE',  ( -21.08198257630413508, 0.07264332379574613141, -161.1634032659849254 ) ) ;
#76768 = EDGE_CURVE ( 'NONE', #196290, #136430, #63289, .T. ) ;
#76769 = AXIS2_PLACEMENT_3D ( 'NONE', #20947, #100423, #137007 ) ;
#76770 = DIRECTION ( 'NONE',  ( 1.000000000000000000, 0.000000000000000000, -0.000000000000000000 ) ) ;
#76771 = CARTESIAN_POINT ( 'NONE',  ( -21.05000000000000071, 6.257814610476114758, 0.09779029130879343668 ) ) ;
#76772 = CARTESIAN_POINT ( 'NONE',  ( 21.06490991615909181, 10.72489134759826790, -112.7037113535331656 ) ) ;
#76773 = AXIS2_PLACEMENT_3D ( 'NONE', #129904, #30847, #46511 ) ;
#76774 = DIRECTION ( 'NONE',  ( 0.000000000000000000, 0.8814952561688431665, -0.4721928772777346794 ) ) ;
#76775 = DIRECTION ( 'NONE',  ( -1.000000000000000000, 0.000000000000000000, -0.000000000000000000 ) ) ;
#76776 = CARTESIAN_POINT ( 'NONE',  ( 23.14999999999998437, 1.115600667400684642E-11, -37.54999999999999716 ) ) ;
#76777 = EDGE_LOOP ( 'NONE', ( #46930, #67108, #217572, #7207 ) ) ;
#76778 = ORIENTED_EDGE ( 'NONE', *, *, #118481, .F. ) ;
#76780 = ORIENTED_EDGE ( 'NONE', *, *, #202746, .T. ) ;
#76779 = AXIS2_PLACEMENT_3D ( 'NONE', #246376, #16446, #76375 ) ;
#76781 = CYLINDRICAL_SURFACE ( 'NONE', #62424, 4.049999999999998046 ) ;
#76782 = CIRCLE ( 'NONE', #147528, 3.999999999999999112 ) ;
#76784 = ORIENTED_EDGE ( 'NONE', *, *, #163953, .F. ) ;
#76783 = DIRECTION ( 'NONE',  ( 0.000000000000000000, 1.000000000000000000, 0.000000000000000000 ) ) ;
#76785 = DIRECTION ( 'NONE',  ( 1.000000000000000000, 0.000000000000000000, 0.000000000000000000 ) ) ;
#76786 = ORIENTED_EDGE ( 'NONE', *, *, #101478, .F. ) ;
#76787 =( BOUNDED_CURVE ( )  B_SPLINE_CURVE ( 3, ( #37761, #14353, #155155, #173458 ),
 .UNSPECIFIED., .F., .F. ) 
 B_SPLINE_CURVE_WITH_KNOTS ( ( 4, 4 ),
 ( 4.712388980384689674, 6.231880751915386263 ),
 .UNSPECIFIED. ) 
 CURVE ( )  GEOMETRIC_REPRESENTATION_ITEM ( )  RATIONAL_B_SPLINE_CURVE ( ( 1.000000000000000000, 0.8166740347213228279, 0.8166740347213228279, 1.000000000000000000 ) ) 
 REPRESENTATION_ITEM ( '' )  );
#76788 = ORIENTED_EDGE ( 'NONE', *, *, #218231, .T. ) ;
#76789 = FACE_OUTER_BOUND ( 'NONE', #100093, .T. ) ;
#76790 = AXIS2_PLACEMENT_3D ( 'NONE', #61883, #82686, #100946 ) ;
#76791 = AXIS2_PLACEMENT_3D ( 'NONE', #42498, #182025, #202856 ) ;
#76792 = VERTEX_POINT ( 'NONE', #43738 ) ;
#76793 = AXIS2_PLACEMENT_3D ( 'NONE', #230147, #210586, #48933 ) ;
#76794 = CARTESIAN_POINT ( 'NONE',  ( 11.60000000000006182, 64.35000000001120668, -18.42310748452479530 ) ) ;
#76795 = DIRECTION ( 'NONE',  ( 1.000000000000000000, 0.000000000000000000, 0.000000000000000000 ) ) ;
#76797 = ORIENTED_EDGE ( 'NONE', *, *, #45122, .F. ) ;
#76796 = ORIENTED_EDGE ( 'NONE', *, *, #168829, .F. ) ;
#76798 = ORIENTED_EDGE ( 'NONE', *, *, #23246, .F. ) ;
#76799 = DIRECTION ( 'NONE',  ( 0.000000000000000000, 0.9126074666063769270, 0.4088369013363283844 ) ) ;
#76800 = ORIENTED_EDGE ( 'NONE', *, *, #121162, .T. ) ;
#76801 = EDGE_LOOP ( 'NONE', ( #240319, #217805, #133834, #182150, #55460, #188949, #176213, #29943, #61715, #8851, #215222, #15273 ) ) ;
#76802 = CARTESIAN_POINT ( 'NONE',  ( 20.94999999999999574, 65.52661458509973613, -195.9444530202758870 ) ) ;
#76804 = ORIENTED_EDGE ( 'NONE', *, *, #234843, .F. ) ;
#76803 = CARTESIAN_POINT ( 'NONE',  ( -20.94999999999999929, -11.65000000000000036, -2.900000000000003464 ) ) ;
#76805 = AXIS2_PLACEMENT_3D ( 'NONE', #244963, #211953, #87163 ) ;
#76807 = CARTESIAN_POINT ( 'NONE',  ( -22.59999999999999787, 64.25043287652329127, -203.6239658536231332 ) ) ;
#76806 = DIRECTION ( 'NONE',  ( -1.000000000000000000, 0.000000000000000000, -0.000000000000000000 ) ) ;
#76808 = CYLINDRICAL_SURFACE ( 'NONE', #232460, 0.1000000000000028644 ) ;
#76809 = CARTESIAN_POINT ( 'NONE',  ( -18.59999999999999787, 11.60000000001115872, -174.4282032302755283 ) ) ;
#76810 = CARTESIAN_POINT ( 'NONE',  ( 23.15000000000000213, 78.47509609352879068, -238.9045489380306435 ) ) ;
#76811 = ORIENTED_EDGE ( 'NONE', *, *, #183439, .F. ) ;
#76812 = VERTEX_POINT ( 'NONE', #21617 ) ;
#76813 = DIRECTION ( 'NONE',  ( 1.000000000000000000, 0.000000000000000000, 0.000000000000000000 ) ) ;
#76814 = CIRCLE ( 'NONE', #35170, 4.049999999999998934 ) ;
#76815 = CARTESIAN_POINT ( 'NONE',  ( -21.05000000000000071, 76.10000000001218723, -143.0637644362255401 ) ) ;
#76817 = EDGE_CURVE ( 'NONE', #85530, #242990, #123277, .T. ) ;
#76816 = LINE ( 'NONE', #38999, #107972 ) ;
#76818 = EDGE_LOOP ( 'NONE', ( #244797, #185271, #134796, #81605 ) ) ;
#76819 = DIRECTION ( 'NONE',  ( 1.000000000000000000, 0.000000000000000000, 0.000000000000000000 ) ) ;
#76820 = EDGE_CURVE ( 'NONE', #245055, #142813, #233826, .T. ) ;
#76821 = AXIS2_PLACEMENT_3D ( 'NONE', #112109, #96351, #58506 ) ;
#76822 = DIRECTION ( 'NONE',  ( 1.000000000000000000, 0.000000000000000000, 0.000000000000000000 ) ) ;
#76823 = CIRCLE ( 'NONE', #31084, 0.09999999999998898659 ) ;
#76824 = CARTESIAN_POINT ( 'NONE',  ( -14.56556274378147542, 12.44134409367007521, -213.7340784654984986 ) ) ;
#76825 = VERTEX_POINT ( 'NONE', #120733 ) ;
#76826 = ORIENTED_EDGE ( 'NONE', *, *, #101820, .F. ) ;
#76827 = ADVANCED_FACE ( 'NONE', ( #65863 ), #200244, .F. ) ;
#76828 = CARTESIAN_POINT ( 'NONE',  ( -21.05000000000000426, 64.40000000001188596, -96.09490425424884563 ) ) ;
#76829 = EDGE_CURVE ( 'NONE', #176651, #206737, #142227, .T. ) ;
#76830 = ORIENTED_EDGE ( 'NONE', *, *, #250758, .T. ) ;
#76831 = DIRECTION ( 'NONE',  ( 0.000000000000000000, 6.982962677686266711E-15, -1.000000000000000000 ) ) ;
#76832 = ORIENTED_EDGE ( 'NONE', *, *, #100825, .T. ) ;
#76833 = DIRECTION ( 'NONE',  ( 7.304098846218134667E-16, -1.000000000000000000, 0.000000000000000000 ) ) ;
#76834 = DIRECTION ( 'NONE',  ( -0.7071067811865475727, -0.7071067811865475727, 0.000000000000000000 ) ) ;
#76836 = CARTESIAN_POINT ( 'NONE',  ( -20.94788355080264353, 68.02921119886117651, -224.2090419302654141 ) ) ;
#76835 = CARTESIAN_POINT ( 'NONE',  ( -18.59999999999999787, 9.350000000011156942, -155.1500000000000057 ) ) ;
#76837 = CARTESIAN_POINT ( 'NONE',  ( 23.14999999999999858, 1.115600667400684642E-11, -100.5000000000000426 ) ) ;
#76838 = CARTESIAN_POINT ( 'NONE',  ( 20.94999999999999929, 7.120270961708750512, -137.6595630418393625 ) ) ;
#76839 = DIRECTION ( 'NONE',  ( 0.000000000000000000, -6.982962677686267499E-15, 1.000000000000000000 ) ) ;
#76840 = AXIS2_PLACEMENT_3D ( 'NONE', #224645, #139959, #186831 ) ;
#76841 = ADVANCED_FACE ( 'NONE', ( #146661 ), #96425, .T. ) ;
#76843 = ORIENTED_EDGE ( 'NONE', *, *, #116918, .T. ) ;
#76842 = VERTEX_POINT ( 'NONE', #153153 ) ;
#76844 = ORIENTED_EDGE ( 'NONE', *, *, #138665, .T. ) ;
#76845 = DIRECTION ( 'NONE',  ( 0.000000000000000000, 1.000000000000000000, 6.688090509790097607E-15 ) ) ;
#76846 = CARTESIAN_POINT ( 'NONE',  ( -22.48660254037843487, 55.97436536266719997, -232.8539608197349651 ) ) ;
#76847 = VECTOR ( 'NONE', #248833, 1000.000000000000000 ) ;
#76848 = CARTESIAN_POINT ( 'NONE',  ( -21.44999999999999929, 21.43869811404188752, -233.1734427395952025 ) ) ;
#76850 = PLANE ( 'NONE',  #78137 ) ;
#76849 = CARTESIAN_POINT ( 'NONE',  ( 20.22894356738451194, 9.278498222838468479, -8.268522906243765291 ) ) ;
#76851 = CARTESIAN_POINT ( 'NONE',  ( -16.87683809663752399, 66.13508655273133741, -49.29882593322043505 ) ) ;
#76852 = EDGE_LOOP ( 'NONE', ( #208307, #140348, #168278, #130345, #75275 ) ) ;
#76853 = CARTESIAN_POINT ( 'NONE',  ( 22.39999999999999147, 68.20922040163827660, -69.52310748452435973 ) ) ;
#76854 = VERTEX_POINT ( 'NONE', #168868 ) ;
#76855 = ORIENTED_EDGE ( 'NONE', *, *, #145025, .T. ) ;
#76856 = DIRECTION ( 'NONE',  ( 1.000000000000000000, -3.265361837132813093E-16, -2.280189983783949500E-30 ) ) ;
#76857 = CARTESIAN_POINT ( 'NONE',  ( -20.94999999999994600, 65.35000000001120668, -3.123107484524795474 ) ) ;
#76858 = CARTESIAN_POINT ( 'NONE',  ( -21.05000000000000071, 74.83729825007431202, -161.9231074845243654 ) ) ;
#76859 = CARTESIAN_POINT ( 'NONE',  ( 22.47071067811864964, 75.90090754531013317, -211.2431822290224090 ) ) ;
#76860 = ADVANCED_FACE ( 'NONE', ( #172725 ), #9738, .F. ) ;
#76861 = AXIS2_PLACEMENT_3D ( 'NONE', #229998, #50075, #173931 ) ;
#76862 = DIRECTION ( 'NONE',  ( 1.000000000000000000, -0.000000000000000000, -0.000000000000000000 ) ) ;
#76863 = ORIENTED_EDGE ( 'NONE', *, *, #149917, .T. ) ;
#76864 = ORIENTED_EDGE ( 'NONE', *, *, #34800, .T. ) ;
#76865 = DIRECTION ( 'NONE',  ( 1.000000000000000000, 0.000000000000000000, 0.000000000000000000 ) ) ;
#76866 = CARTESIAN_POINT ( 'NONE',  ( -18.50000000000000000, 11.56851667937982775, -211.1200010790121553 ) ) ;
#76867 = ORIENTED_EDGE ( 'NONE', *, *, #253669, .T. ) ;
#76868 = LINE ( 'NONE', #58579, #73101 ) ;
#76869 = CARTESIAN_POINT ( 'NONE',  ( -18.59999999999999787, -9.849999999999994316, 30.00000000000000000 ) ) ;
#76870 = DIRECTION ( 'NONE',  ( 0.000000000000000000, 0.000000000000000000, -1.000000000000000000 ) ) ;
#76872 = EDGE_CURVE ( 'NONE', #14704, #194376, #162539, .T. ) ;
#76871 = CARTESIAN_POINT ( 'NONE',  ( -20.65000000000000568, 68.75000000001263345, -194.2731074845244166 ) ) ;
#76873 = DIRECTION ( 'NONE',  ( -4.336808689942017736E-16, 0.000000000000000000, -1.000000000000000000 ) ) ;
#76875 = DIRECTION ( 'NONE',  ( -0.000000000000000000, 6.982962677686266711E-15, -1.000000000000000000 ) ) ;
#76874 = CARTESIAN_POINT ( 'NONE',  ( -22.47886152344871036, 0.03750093886169331148, 11.64998864304793003 ) ) ;
#76876 = DIRECTION ( 'NONE',  ( 0.000000000000000000, -0.1455152366551522025, -0.9893560106964505163 ) ) ;
#76877 = ADVANCED_FACE ( 'NONE', ( #187126 ), #47570, .F. ) ;
#76878 = CARTESIAN_POINT ( 'NONE',  ( -18.59999999999999787, 11.65000000001115232, -141.0148057706539930 ) ) ;
#76879 = CARTESIAN_POINT ( 'NONE',  ( 23.04999999999999716, 32.67104411594546320, -237.4063322638886859 ) ) ;
#76880 = CARTESIAN_POINT ( 'NONE',  ( -18.50000000000000000, 74.83729825007388570, -94.92310748452432279 ) ) ;
#76882 = ORIENTED_EDGE ( 'NONE', *, *, #88255, .F. ) ;
#76881 = DIRECTION ( 'NONE',  ( 0.000000000000000000, -6.352154140967427193E-15, 1.000000000000000000 ) ) ;
#76883 = AXIS2_PLACEMENT_3D ( 'NONE', #51610, #132472, #210723 ) ;
#76884 = AXIS2_PLACEMENT_3D ( 'NONE', #242354, #79413, #256736 ) ;
#76885 = AXIS2_PLACEMENT_3D ( 'NONE', #227401, #64488, #246960 ) ;
#76886 = EDGE_CURVE ( 'NONE', #195525, #41986, #46348, .T. ) ;
#76887 = DIRECTION ( 'NONE',  ( -1.000000000000000000, -0.000000000000000000, -0.000000000000000000 ) ) ;
#76888 = VERTEX_POINT ( 'NONE', #129695 ) ;
#76889 = EDGE_CURVE ( 'NONE', #203961, #65541, #90555, .T. ) ;
#76890 = EDGE_CURVE ( 'NONE', #62919, #212664, #192148, .T. ) ;
#76891 = CARTESIAN_POINT ( 'NONE',  ( -22.37643362114956957, 0.09908137369253962323, -92.87421000604163623 ) ) ;
#76892 = DIRECTION ( 'NONE',  ( -1.000000000000000000, 7.304098846218134667E-16, 5.100424963727256530E-30 ) ) ;
#76893 = EDGE_LOOP ( 'NONE', ( #112055, #44521, #152469, #220782 ) ) ;
#76894 = VECTOR ( 'NONE', #14197, 1000.000000000000000 ) ;
#76895 = EDGE_CURVE ( 'NONE', #146024, #70177, #113008, .T. ) ;
#76896 = CARTESIAN_POINT ( 'NONE',  ( -20.85000000000000142, 77.16412189325286874, -61.60825939895269698 ) ) ;
#76897 = DIRECTION ( 'NONE',  ( 0.000000000000000000, -7.189901751995743170E-15, 1.000000000000000000 ) ) ;
#76898 = AXIS2_PLACEMENT_3D ( 'NONE', #181077, #58518, #81914 ) ;
#76899 = FACE_OUTER_BOUND ( 'NONE', #218985, .T. ) ;
#76900 = VECTOR ( 'NONE', #213688, 1000.000000000000000 ) ;
#76901 = DIRECTION ( 'NONE',  ( 1.000000000000000000, -7.304098846218134667E-16, -5.100424963727256530E-30 ) ) ;
#76902 = CIRCLE ( 'NONE', #255918, 0.09999999999999799327 ) ;
#76903 = AXIS2_PLACEMENT_3D ( 'NONE', #199497, #58652, #159088 ) ;
#76904 = VERTEX_POINT ( 'NONE', #209225 ) ;
#76905 = DIRECTION ( 'NONE',  ( 1.000000000000000000, 0.000000000000000000, 0.000000000000000000 ) ) ;
#76907 = ORIENTED_EDGE ( 'NONE', *, *, #23809, .F. ) ;
#76906 = DIRECTION ( 'NONE',  ( 0.000000000000000000, -0.1455152366551522025, -0.9893560106964505163 ) ) ;
#76908 = DIRECTION ( 'NONE',  ( 0.000000000000000000, 0.000000000000000000, -1.000000000000000000 ) ) ;
#76909 = EDGE_CURVE ( 'NONE', #2368, #102509, #221313, .T. ) ;
#76910 = CARTESIAN_POINT ( 'NONE',  ( -18.39999999999999858, 85.68240343348826116, -96.36626410711143365 ) ) ;
#76911 = DIRECTION ( 'NONE',  ( 0.000000000000000000, 0.000000000000000000, -1.000000000000000000 ) ) ;
#76912 = ORIENTED_EDGE ( 'NONE', *, *, #123892, .F. ) ;
#76913 = DIRECTION ( 'NONE',  ( 0.000000000000000000, 0.9868171638914230437, 0.1618390714546045217 ) ) ;
#76914 = AXIS2_PLACEMENT_3D ( 'NONE', #191497, #233189, #33723 ) ;
#76915 = SHAPE_DEFINITION_REPRESENTATION ( #128458, #206680 ) ;
#76916 = AXIS2_PLACEMENT_3D ( 'NONE', #226746, #145922, #105487 ) ;
#76918 = CIRCLE ( 'NONE', #89558, 0.1000000000000033362 ) ;
#76917 = CARTESIAN_POINT ( 'NONE',  ( 22.49544290803765634, 11.46684760846049578, -198.4357998940971868 ) ) ;
#76919 = CARTESIAN_POINT ( 'NONE',  ( -20.64999999999999858, 71.65000000001228386, -157.7731074845243882 ) ) ;
#76920 = ORIENTED_EDGE ( 'NONE', *, *, #239684, .T. ) ;
#76921 = LINE ( 'NONE', #151354, #12799 ) ;
#76922 = FACE_OUTER_BOUND ( 'NONE', #112750, .T. ) ;
#76923 = AXIS2_PLACEMENT_3D ( 'NONE', #251833, #155343, #152774 ) ;
#76924 = AXIS2_PLACEMENT_3D ( 'NONE', #53001, #92135, #132556 ) ;
#76925 = SURFACE_STYLE_USAGE ( .BOTH. , #16979 ) ;
#76926 = VERTEX_POINT ( 'NONE', #13608 ) ;
#76927 = VERTEX_POINT ( 'NONE', #249656 ) ;
#76928 = DIRECTION ( 'NONE',  ( 0.000000000000000000, -6.688090509790097607E-15, 1.000000000000000000 ) ) ;
#76929 = AXIS2_PLACEMENT_3D ( 'NONE', #90203, #69399, #229739 ) ;
#76930 = DIRECTION ( 'NONE',  ( 1.000000000000000000, 0.000000000000000000, -0.000000000000000000 ) ) ;
#76932 = B_SPLINE_CURVE_WITH_KNOTS ( 'NONE', 3,
 ( #149865, #71614, #87283, #110719, #151144, #67743, #147275, #169453, #207273, #108158, #226809, #48169, #187710, #127726 ),
 .UNSPECIFIED., .F., .F.,
 ( 4, 2, 2, 2, 2, 2, 4 ),
 ( 6.938893903907227607E-18, 0.0003823333598417784991, 0.0005735000397626514044, 0.0006690833797230878299, 0.0007168750497033175894, 0.0007407708846934301381, 0.0007646667196835427952 ),
 .UNSPECIFIED. ) ;
#76931 = CIRCLE ( 'NONE', #151982, 0.1000000000000028783 ) ;
#76933 = CARTESIAN_POINT ( 'NONE',  ( 21.30000000000002558, 76.00000000001240608, -174.0731074845243711 ) ) ;
#76934 = CARTESIAN_POINT ( 'NONE',  ( -20.54999999999999716, 19.73066058418984170, -238.2142830767208466 ) ) ;
#76935 = DIRECTION ( 'NONE',  ( 0.000000000000000000, 0.000000000000000000, -1.000000000000000000 ) ) ;
#76937 = CARTESIAN_POINT ( 'NONE',  ( 21.14999999999999858, 13.07482039728799528, -210.6896000549707537 ) ) ;
#76936 = CARTESIAN_POINT ( 'NONE',  ( -16.94445028196807002, 9.992063609708893068, -154.8926698215815634 ) ) ;
#76938 = CARTESIAN_POINT ( 'NONE',  ( -18.59999999999999787, 1.115600667400684642E-11, -100.5000000000000426 ) ) ;
#76939 = CARTESIAN_POINT ( 'NONE',  ( -23.15000000000000213, -4.831324760622930370, -16.96969694219874825 ) ) ;
#76940 = PLANE ( 'NONE',  #12997 ) ;
#76941 = DIRECTION ( 'NONE',  ( 2.840903330521631775E-16, -0.8700118002898321601, 0.4930308989875230585 ) ) ;
#76942 = VERTEX_POINT ( 'NONE', #71030 ) ;
#76943 = EDGE_CURVE ( 'NONE', #7645, #178157, #189672, .T. ) ;
#76944 = ORIENTED_EDGE ( 'NONE', *, *, #123322, .F. ) ;
#76945 = CARTESIAN_POINT ( 'NONE',  ( 21.14999999999999503, 64.35000000001194564, -102.9231074845243938 ) ) ;
#76946 = DIRECTION ( 'NONE',  ( 0.000000000000000000, 0.3738317757009942399, -0.9274965247785252886 ) ) ;
#76948 = DIRECTION ( 'NONE',  ( 1.000000000000000000, 0.000000000000000000, 0.000000000000000000 ) ) ;
#76947 = DIRECTION ( 'NONE',  ( -0.7071067811865475727, -0.7071067811865475727, -0.000000000000000000 ) ) ;
#76949 = DIRECTION ( 'NONE',  ( 0.000000000000000000, 0.000000000000000000, -1.000000000000000000 ) ) ;
#76950 = DIRECTION ( 'NONE',  ( -3.265361837132813586E-16, 0.4721928772777346239, 0.8814952561688430555 ) ) ;
#76952 = EDGE_CURVE ( 'NONE', #17335, #75581, #175222, .T. ) ;
#76951 = DIRECTION ( 'NONE',  ( 0.000000000000000000, 0.000000000000000000, -1.000000000000000000 ) ) ;
#76953 = ORIENTED_EDGE ( 'NONE', *, *, #125698, .F. ) ;
#76954 = VERTEX_POINT ( 'NONE', #247056 ) ;
#76955 = VECTOR ( 'NONE', #222907, 1000.000000000000000 ) ;
#76956 = EDGE_CURVE ( 'NONE', #119208, #124485, #68446, .T. ) ;
#76957 = ADVANCED_FACE ( 'NONE', ( #107552 ), #41923, .T. ) ;
#76958 = AXIS2_PLACEMENT_3D ( 'NONE', #225194, #127410, #7447 ) ;
#76959 = CARTESIAN_POINT ( 'NONE',  ( -21.14999999999994174, 74.83745509109094485, -44.02310748452479316 ) ) ;
#76960 = VERTEX_POINT ( 'NONE', #128414 ) ;
#76961 = DIRECTION ( 'NONE',  ( -1.000000000000000000, -0.000000000000000000, 0.000000000000000000 ) ) ;
#76962 = CIRCLE ( 'NONE', #226803, 7.800000000000001599 ) ;
#76963 = CARTESIAN_POINT ( 'NONE',  ( 18.41815437325351823, 85.49870985315280336, -29.41916164572225156 ) ) ;
#76964 = TOROIDAL_SURFACE ( 'NONE', #181039, 3.899999999999999467, 0.1000000000000000056 ) ;
#76965 = AXIS2_PLACEMENT_3D ( 'NONE', #1486, #178893, #160604 ) ;
#76966 = ORIENTED_EDGE ( 'NONE', *, *, #135985, .F. ) ;
#76967 = DIRECTION ( 'NONE',  ( -1.000000000000000000, 0.000000000000000000, 0.000000000000000000 ) ) ;
#76968 = EDGE_CURVE ( 'NONE', #119503, #156593, #162706, .T. ) ;
#76969 = VERTEX_POINT ( 'NONE', #108839 ) ;
#76970 = DIRECTION ( 'NONE',  ( 1.000000000000000000, 7.304098846218134667E-16, 5.100424963727256530E-30 ) ) ;
#76972 = CIRCLE ( 'NONE', #110292, 0.1000000000000024342 ) ;
#76971 = DIRECTION ( 'NONE',  ( 0.000000000000000000, -3.208737065390626061E-15, 1.000000000000000000 ) ) ;
#76973 = DIRECTION ( 'NONE',  ( 0.000000000000000000, -6.982962677686266711E-15, 1.000000000000000000 ) ) ;
#76974 = DIRECTION ( 'NONE',  ( 0.000000000000000000, 0.000000000000000000, 1.000000000000000000 ) ) ;
#76976 = AXIS2_PLACEMENT_3D ( 'NONE', #112278, #109678, #9306 ) ;
#76975 = CARTESIAN_POINT ( 'NONE',  ( 21.07928932188134041, 65.47931918658339612, -241.9371126717067568 ) ) ;
#76978 = DIRECTION ( 'NONE',  ( 0.000000000000000000, -0.9908441862701420355, -0.1350103645453197554 ) ) ;
#76977 = LINE ( 'NONE', #118699, #41696 ) ;
#76979 = VECTOR ( 'NONE', #188160, 1000.000000000000000 ) ;
#76980 = CARTESIAN_POINT ( 'NONE',  ( -18.40000000000000213, 11.75000000001113953, -54.35000000000000142 ) ) ;
#76981 = ORIENTED_EDGE ( 'NONE', *, *, #250682, .T. ) ;
#76983 = CARTESIAN_POINT ( 'NONE',  ( 20.94999999999999929, 0.000000000000000000, -41.30000000000000426 ) ) ;
#76982 = FACE_OUTER_BOUND ( 'NONE', #27027, .T. ) ;
#76984 = ORIENTED_EDGE ( 'NONE', *, *, #211034, .T. ) ;
#76986 = ORIENTED_EDGE ( 'NONE', *, *, #79460, .F. ) ;
#76985 = FACE_OUTER_BOUND ( 'NONE', #118608, .T. ) ;
#76987 = EDGE_LOOP ( 'NONE', ( #121346, #209226, #14787, #194490 ) ) ;
#76988 = CARTESIAN_POINT ( 'NONE',  ( 20.85000000000000142, 11.65000000001115943, -67.00000000000000000 ) ) ;
#76989 = DIRECTION ( 'NONE',  ( 1.000000000000000000, 0.000000000000000000, 0.000000000000000000 ) ) ;
#76990 = CARTESIAN_POINT ( 'NONE',  ( 21.05000000000000071, 70.60000000001157616, -57.11784146561126363 ) ) ;
#76991 = CARTESIAN_POINT ( 'NONE',  ( 23.24999999999999645, 1.115600667400684642E-11, -67.00000000000000000 ) ) ;
#76992 = EDGE_LOOP ( 'NONE', ( #225842, #53711, #252737, #227648 ) ) ;
#76993 = EDGE_CURVE ( 'NONE', #13008, #85372, #130980, .T. ) ;
#76995 = EDGE_CURVE ( 'NONE', #236521, #63340, #191773, .T. ) ;
#76994 = CARTESIAN_POINT ( 'NONE',  ( 20.90000000000000213, 0.000000000000000000, 0.000000000000000000 ) ) ;
#76996 = CARTESIAN_POINT ( 'NONE',  ( -20.64999999999999858, 85.00000000001179501, -79.41707660717668205 ) ) ;
#76998 = CARTESIAN_POINT ( 'NONE',  ( 18.79999999999999716, 11.49641995933507843, -1.885425182446135661 ) ) ;
#76997 = TOROIDAL_SURFACE ( 'NONE', #156143, 0.2000000000000000111, 0.1000000000000000056 ) ;
#76999 = ORIENTED_EDGE ( 'NONE', *, *, #85878, .T. ) ;
#77000 = DIRECTION ( 'NONE',  ( -1.000000000000000000, 0.000000000000000000, 0.000000000000000000 ) ) ;
#77001 = ADVANCED_FACE ( 'NONE', ( #235218 ), #12691, .F. ) ;
#77002 = LINE ( 'NONE', #255592, #110063 ) ;
#77003 = ORIENTED_EDGE ( 'NONE', *, *, #124441, .F. ) ;
#77004 = ORIENTED_EDGE ( 'NONE', *, *, #153159, .F. ) ;
#77005 = CARTESIAN_POINT ( 'NONE',  ( -16.92570016628985030, 9.958788957751021798, -188.3793493299609452 ) ) ;
#77006 = AXIS2_PLACEMENT_3D ( 'NONE', #40629, #57559, #219209 ) ;
#77007 = ORIENTED_EDGE ( 'NONE', *, *, #59677, .T. ) ;
#77008 = CARTESIAN_POINT ( 'NONE',  ( -17.27223548803747377, 10.34539739140543269, -11.36639382080207028 ) ) ;
#77009 = ORIENTED_EDGE ( 'NONE', *, *, #256879, .T. ) ;
#77010 = DIRECTION ( 'NONE',  ( 0.000000000000000000, 0.9126074666063770380, 0.4088369013363281068 ) ) ;
#77011 = DIRECTION ( 'NONE',  ( -1.000000000000000000, 0.000000000000000000, 0.000000000000000000 ) ) ;
#77012 = CARTESIAN_POINT ( 'NONE',  ( -23.25000000000000000, 1.115650265596050101E-11, -129.9500000000000171 ) ) ;
#77013 = CARTESIAN_POINT ( 'NONE',  ( -16.86337532320260735, 63.08270373490941552, -213.0243021242677628 ) ) ;
#77014 = ADVANCED_FACE ( 'NONE', ( #76134 ), #253480, .F. ) ;
#77015 = DIRECTION ( 'NONE',  ( 1.000000000000000000, 0.000000000000000000, 0.000000000000000000 ) ) ;
#77016 = DIRECTION ( 'NONE',  ( 1.000000000000000000, 0.000000000000000000, 0.000000000000000000 ) ) ;
#77017 = CARTESIAN_POINT ( 'NONE',  ( -21.37071067811865532, 29.58339010484111498, -236.6052874901905625 ) ) ;
#77018 = VERTEX_POINT ( 'NONE', #198652 ) ;
#77019 = AXIS2_PLACEMENT_3D ( 'NONE', #67844, #88668, #192610 ) ;
#77021 = CYLINDRICAL_SURFACE ( 'NONE', #152370, 1.749999999999999778 ) ;
#77020 = CARTESIAN_POINT ( 'NONE',  ( 20.95512820512820440, 22.85550638026972692, -230.1049725544161220 ) ) ;
#77022 = ORIENTED_EDGE ( 'NONE', *, *, #38448, .F. ) ;
#77025 = ORIENTED_EDGE ( 'NONE', *, *, #146427, .T. ) ;
#77024 = LINE ( 'NONE', #236103, #191937 ) ;
#77023 = FACE_OUTER_BOUND ( 'NONE', #84441, .T. ) ;
#77026 = EDGE_LOOP ( 'NONE', ( #152505, #155338, #173461, #11195 ) ) ;
#77027 = CARTESIAN_POINT ( 'NONE',  ( -18.59999999999999787, 1.835341550235567887, -45.05515129256298223 ) ) ;
#77028 = CARTESIAN_POINT ( 'NONE',  ( 13.76927104934457624, 66.54401276639956109, -155.0115763176266341 ) ) ;
#77029 = CARTESIAN_POINT ( 'NONE',  ( 20.94999999999999929, 76.00000000001126921, -203.5231074845248997 ) ) ;
#77030 = EDGE_CURVE ( 'NONE', #242592, #180754, #121033, .T. ) ;
#77031 = CARTESIAN_POINT ( 'NONE',  ( -18.34374000495059676, 64.52683809664972614, -145.7731074845244450 ) ) ;
#77032 = VECTOR ( 'NONE', #224457, 1000.000000000000000 ) ;
#77033 = ORIENTED_EDGE ( 'NONE', *, *, #171027, .F. ) ;
#77034 = CARTESIAN_POINT ( 'NONE',  ( 20.94999999999999574, 67.07338541492552508, -195.0514244653012952 ) ) ;
#77035 = DIRECTION ( 'NONE',  ( 0.000000000000000000, -6.982962677686266711E-15, 1.000000000000000000 ) ) ;
#77036 = EDGE_CURVE ( 'NONE', #297, #239496, #213075, .T. ) ;
#77038 = CARTESIAN_POINT ( 'NONE',  ( 20.95132126680579887, 10.48994987014678770, -7.570324538434519468 ) ) ;
#77037 = DIRECTION ( 'NONE',  ( -1.462545276649423285E-15, 0.1686199900910279881, -0.9856811345164833149 ) ) ;
#77039 = EDGE_CURVE ( 'NONE', #88959, #4968, #166828, .T. ) ;
#77041 = ORIENTED_EDGE ( 'NONE', *, *, #230058, .F. ) ;
#77040 = DIRECTION ( 'NONE',  ( -0.000000000000000000, -0.000000000000000000, -1.000000000000000000 ) ) ;
#77042 = EDGE_LOOP ( 'NONE', ( #120295, #137001, #145023, #206947 ) ) ;
#77044 = EDGE_CURVE ( 'NONE', #242842, #157610, #70970, .T. ) ;
#77043 = CARTESIAN_POINT ( 'NONE',  ( 22.59066674512285999, 11.75000000001115552, -167.4694958763696206 ) ) ;
#77045 = AXIS2_PLACEMENT_3D ( 'NONE', #164003, #166592, #243528 ) ;
#77046 = VECTOR ( 'NONE', #164599, 1000.000000000000000 ) ;
#77047 = CARTESIAN_POINT ( 'NONE',  ( -21.64999999999999858, 9.350000000011133849, -176.7499999999999716 ) ) ;
#77049 = EDGE_CURVE ( 'NONE', #81086, #256073, #28128, .T. ) ;
#77048 = ORIENTED_EDGE ( 'NONE', *, *, #192352, .F. ) ;
#77050 = CARTESIAN_POINT ( 'NONE',  ( -23.25000000000000000, 11.75000000001115552, -155.7499999999999716 ) ) ;
#77051 = ORIENTED_EDGE ( 'NONE', *, *, #138812, .F. ) ;
#77052 = DIRECTION ( 'NONE',  ( -0.000000000000000000, 0.000000000000000000, -1.000000000000000000 ) ) ;
#77053 = CYLINDRICAL_SURFACE ( 'NONE', #91010, 2.000000000000003109 ) ;
#77054 = CARTESIAN_POINT ( 'NONE',  ( 18.59999999999999432, 1.162701749949165642, -142.1000000000000227 ) ) ;
#77055 = ADVANCED_FACE ( 'NONE', ( #236490 ), #233459, .T. ) ;
#77056 = ORIENTED_EDGE ( 'NONE', *, *, #5513, .T. ) ;
#77057 = DIRECTION ( 'NONE',  ( 1.000000000000000000, 0.000000000000000000, 0.000000000000000000 ) ) ;
#77058 = EDGE_CURVE ( 'NONE', #68117, #245768, #249994, .T. ) ;
#77059 = CARTESIAN_POINT ( 'NONE',  ( -21.00857864376268935, 11.60000000001115161, -73.92820323027561358 ) ) ;
#77060 = AXIS2_PLACEMENT_3D ( 'NONE', #212378, #195390, #76686 ) ;
#77061 = EDGE_CURVE ( 'NONE', #207338, #56486, #59105, .T. ) ;
#77062 = EDGE_CURVE ( 'NONE', #27420, #59785, #218192, .T. ) ;
#77063 = AXIS2_PLACEMENT_3D ( 'NONE', #17540, #97046, #159642 ) ;
#77064 = CIRCLE ( 'NONE', #139585, 0.6000000000000033085 ) ;
#77065 = EDGE_LOOP ( 'NONE', ( #257068, #205945, #151663, #18811 ) ) ;
#77066 = ORIENTED_EDGE ( 'NONE', *, *, #78522, .F. ) ;
#77067 = ORIENTED_EDGE ( 'NONE', *, *, #11813, .F. ) ;
#77068 =( GEOMETRIC_REPRESENTATION_CONTEXT ( 3 ) GLOBAL_UNCERTAINTY_ASSIGNED_CONTEXT ( ( #32124 ) ) GLOBAL_UNIT_ASSIGNED_CONTEXT ( ( #107297, #143845, #184266 ) ) REPRESENTATION_CONTEXT ( 'NONE', 'WORKASPACE' ) );
#77069 = EDGE_CURVE ( 'NONE', #244261, #243110, #166065, .T. ) ;
#77070 = ORIENTED_EDGE ( 'NONE', *, *, #238577, .F. ) ;
#77072 = EDGE_LOOP ( 'NONE', ( #160841, #34824, #221701, #157418 ) ) ;
#77071 = DIRECTION ( 'NONE',  ( 0.000000000000000000, -0.8777080977375715243, 0.4791956752370512551 ) ) ;
#77074 = ADVANCED_FACE ( 'NONE', ( #133545 ), #193534, .F. ) ;
#77073 = VERTEX_POINT ( 'NONE', #194832 ) ;
#77075 = DIRECTION ( 'NONE',  ( -1.000000000000000000, 0.000000000000000000, 0.000000000000000000 ) ) ;
#77076 = ADVANCED_FACE ( 'NONE', ( #106924 ), #10417, .F. ) ;
#77079 = ORIENTED_EDGE ( 'NONE', *, *, #249252, .F. ) ;
#77078 = ORIENTED_EDGE ( 'NONE', *, *, #154185, .F. ) ;
#77077 = FACE_OUTER_BOUND ( 'NONE', #102464, .T. ) ;
#77080 = EDGE_CURVE ( 'NONE', #145161, #72156, #116717, .T. ) ;
#77081 = ORIENTED_EDGE ( 'NONE', *, *, #230704, .T. ) ;
#77082 = CARTESIAN_POINT ( 'NONE',  ( 21.05000000000000071, -9.400000000000000355, -23.60603087734755690 ) ) ;
#77083 = AXIS2_PLACEMENT_3D ( 'NONE', #14234, #212426, #235813 ) ;
#77084 = CARTESIAN_POINT ( 'NONE',  ( 20.99142135623731065, 64.40000000001175806, -76.45131071479988805 ) ) ;
#77085 = VECTOR ( 'NONE', #57210, 1000.000000000000000 ) ;
#77086 = CARTESIAN_POINT ( 'NONE',  ( 21.05000000000000071, 71.00000000001253397, -181.9283735034374843 ) ) ;
#77087 = CIRCLE ( 'NONE', #193805, 0.09999999999999939493 ) ;
#77088 = VERTEX_POINT ( 'NONE', #168240 ) ;
#77089 = FACE_OUTER_BOUND ( 'NONE', #113145, .T. ) ;
#77091 = EDGE_LOOP ( 'NONE', ( #186607, #91085, #58791, #65275 ) ) ;
#77090 = CARTESIAN_POINT ( 'NONE',  ( 18.39999999999999503, 5.650000000011139001, -154.8500000000000227 ) ) ;
#77092 = CYLINDRICAL_SURFACE ( 'NONE', #71620, 12.87499999999999822 ) ;
#77094 = EDGE_LOOP ( 'NONE', ( #244740, #247311, #184479, #218628 ) ) ;
#77093 = DIRECTION ( 'NONE',  ( 1.000000000000000000, 0.000000000000000000, 0.000000000000000000 ) ) ;
#77095 = ADVANCED_FACE ( 'NONE', ( #147344 ), #8582, .F. ) ;
#77096 = ORIENTED_EDGE ( 'NONE', *, *, #221011, .T. ) ;
#77097 = EDGE_CURVE ( 'NONE', #39261, #197319, #48244, .T. ) ;
#77098 = AXIS2_PLACEMENT_3D ( 'NONE', #245383, #147555, #108432 ) ;
#77099 = CIRCLE ( 'NONE', #27261, 0.09999999999999939493 ) ;
#77100 = CIRCLE ( 'NONE', #227122, 0.1999999999999987899 ) ;
#77101 = CARTESIAN_POINT ( 'NONE',  ( 18.59999999999999787, 4.324939842317335525, -212.0862480289983409 ) ) ;
#77102 = CARTESIAN_POINT ( 'NONE',  ( -20.54999999999999716, -9.499999999988846255, -90.60603087734760663 ) ) ;
#77103 = VERTEX_POINT ( 'NONE', #84764 ) ;
#77104 = ORIENTED_EDGE ( 'NONE', *, *, #156545, .T. ) ;
#77105 = DIRECTION ( 'NONE',  ( -0.000000000000000000, 1.000000000000000000, 6.982962677686266711E-15 ) ) ;
#77106 = DIRECTION ( 'NONE',  ( 0.000000000000000000, -3.552713678800483969E-15, 1.000000000000000000 ) ) ;
#77109 = EDGE_LOOP ( 'NONE', ( #124215, #129076, #162968, #202820 ) ) ;
#77108 = ORIENTED_EDGE ( 'NONE', *, *, #30580, .T. ) ;
#77107 = CIRCLE ( 'NONE', #247978, 0.1000000000000021427 ) ;
#77110 = ORIENTED_EDGE ( 'NONE', *, *, #227664, .F. ) ;
#77111 = FACE_OUTER_BOUND ( 'NONE', #188871, .T. ) ;
#77112 = ORIENTED_EDGE ( 'NONE', *, *, #5812, .T. ) ;
#77113 = ORIENTED_EDGE ( 'NONE', *, *, #87984, .T. ) ;
#77114 = CARTESIAN_POINT ( 'NONE',  ( 21.14999999999999858, -11.74999999998884448, -146.2500000000000284 ) ) ;
#77115 = EDGE_LOOP ( 'NONE', ( #17486, #166770, #168255, #177714 ) ) ;
#77116 = CARTESIAN_POINT ( 'NONE',  ( -16.93262454970420094, 12.44846049787371278, -211.1565081053942663 ) ) ;
#77117 = AXIS2_PLACEMENT_3D ( 'NONE', #168531, #70696, #130635 ) ;
#77118 = AXIS2_PLACEMENT_3D ( 'NONE', #200190, #101027, #202749 ) ;
#77120 = CARTESIAN_POINT ( 'NONE',  ( -22.50000000000000000, 64.35042919246788529, -203.6231074845244393 ) ) ;
#77119 = FACE_OUTER_BOUND ( 'NONE', #208311, .T. ) ;
#77121 = ORIENTED_EDGE ( 'NONE', *, *, #178101, .F. ) ;
#77122 = ORIENTED_EDGE ( 'NONE', *, *, #100045, .T. ) ;
#77124 = ADVANCED_FACE ( 'NONE', ( #246449 ), #86053, .T. ) ;
#77123 = FACE_OUTER_BOUND ( 'NONE', #248609, .T. ) ;
#77125 = EDGE_LOOP ( 'NONE', ( #23852, #70271, #65491, #105217 ) ) ;
#77126 = EDGE_CURVE ( 'NONE', #44645, #177357, #245913, .T. ) ;
#77127 = CARTESIAN_POINT ( 'NONE',  ( -23.15000000000000213, 28.50120599808395028, -258.2149742250584268 ) ) ;
#77128 = VERTEX_POINT ( 'NONE', #46940 ) ;
#77129 = ORIENTED_EDGE ( 'NONE', *, *, #103318, .F. ) ;
#77130 = CARTESIAN_POINT ( 'NONE',  ( 18.59999999999999076, 62.96704557978079464, -212.5773704035085814 ) ) ;
#77132 = VERTEX_POINT ( 'NONE', #199957 ) ;
#77131 = CARTESIAN_POINT ( 'NONE',  ( 18.42595409746874680, 85.49999981257727200, -163.0237451327774068 ) ) ;
#77133 = DIRECTION ( 'NONE',  ( 1.000000000000000000, 0.000000000000000000, 0.000000000000000000 ) ) ;
#77134 = DIRECTION ( 'NONE',  ( 0.000000000000000000, 0.1350103645451974088, -0.9908441862701587999 ) ) ;
#77135 = VERTEX_POINT ( 'NONE', #108227 ) ;
#77136 = DIRECTION ( 'NONE',  ( -1.000000000000000000, -0.000000000000000000, -0.000000000000000000 ) ) ;
#77137 = CARTESIAN_POINT ( 'NONE',  ( 18.59999999999999787, 1.851028230152016674, -145.6539132694225032 ) ) ;
#77138 = DIRECTION ( 'NONE',  ( 0.000000000000000000, 0.000000000000000000, -1.000000000000000000 ) ) ;
#77139 = CIRCLE ( 'NONE', #93709, 0.09999999999998898659 ) ;
#77140 = DIRECTION ( 'NONE',  ( 0.000000000000000000, -1.000000000000000000, -6.982962677686265922E-15 ) ) ;
#77141 = CARTESIAN_POINT ( 'NONE',  ( -16.84419801905645997, 63.08063082738696181, -213.1464319176388642 ) ) ;
#77142 = CARTESIAN_POINT ( 'NONE',  ( -16.81931177881022066, 66.06300394050835223, -149.2498896059072422 ) ) ;
#77143 = CIRCLE ( 'NONE', #152183, 0.1000000000000072220 ) ;
#77144 = CARTESIAN_POINT ( 'NONE',  ( 22.45301702632625762, 75.98478912030203958, -148.1728997087846835 ) ) ;
#77145 = FACE_OUTER_BOUND ( 'NONE', #58780, .T. ) ;
#77146 = EDGE_CURVE ( 'NONE', #106243, #231649, #54346, .T. ) ;
#77147 = VECTOR ( 'NONE', #74191, 1000.000000000000000 ) ;
#77148 = VERTEX_POINT ( 'NONE', #164356 ) ;
#77149 = CIRCLE ( 'NONE', #235361, 12.87499999999999822 ) ;
#77151 = EDGE_LOOP ( 'NONE', ( #197700, #143779, #227479 ) ) ;
#77150 = ORIENTED_EDGE ( 'NONE', *, *, #206192, .T. ) ;
#77152 = CIRCLE ( 'NONE', #18887, 7.899999999999995914 ) ;
#77153 = ORIENTED_EDGE ( 'NONE', *, *, #17203, .F. ) ;
#77154 = CARTESIAN_POINT ( 'NONE',  ( -21.07928932188134041, 0.09889514566555068775, -94.17148334360673800 ) ) ;
#77155 = CARTESIAN_POINT ( 'NONE',  ( -20.94999999999999929, -1.164121893230052995, -141.9148480855716343 ) ) ;
#77157 = CARTESIAN_POINT ( 'NONE',  ( -20.94999999999999929, 79.23417978893665747, -236.1056577391152587 ) ) ;
#77156 = CARTESIAN_POINT ( 'NONE',  ( 23.14999999999999858, 76.00000000001267608, -203.5231074845243597 ) ) ;
#77159 = ORIENTED_EDGE ( 'NONE', *, *, #5328, .T. ) ;
#77158 = CIRCLE ( 'NONE', #256159, 0.8750000000000007772 ) ;
#77160 = CARTESIAN_POINT ( 'NONE',  ( -20.64999999999999858, -9.499999999988848032, -143.8939691226524644 ) ) ;
#77161 = CARTESIAN_POINT ( 'NONE',  ( -23.25000000000000000, 77.14957036958777792, -128.7071950000224092 ) ) ;
#77162 = VECTOR ( 'NONE', #89725, 1000.000000000000000 ) ;
#77163 = DIRECTION ( 'NONE',  ( 0.000000000000000000, 0.4999999999999956701, -0.8660254037844411501 ) ) ;
#77164 = DIRECTION ( 'NONE',  ( 0.000000000000000000, 0.000000000000000000, -1.000000000000000000 ) ) ;
#77165 = EDGE_LOOP ( 'NONE', ( #257639, #196502, #165707, #140681 ) ) ;
#77166 = AXIS2_PLACEMENT_3D ( 'NONE', #100075, #84333, #3559 ) ;
#77167 = DIRECTION ( 'NONE',  ( -1.040834085586054343E-13, 0.9999176327611370985, 0.01283462868040226822 ) ) ;
#77168 = EDGE_LOOP ( 'NONE', ( #147106, #78717, #150909, #239661 ) ) ;
#77169 = DIRECTION ( 'NONE',  ( 0.000000000000000000, 1.734723475976805517E-14, -1.000000000000000000 ) ) ;
#77170 = DIRECTION ( 'NONE',  ( 0.000000000000000000, 0.4999999999999994449, 0.8660254037844390407 ) ) ;
#77171 = CIRCLE ( 'NONE', #222918, 0.2000000000000005107 ) ;
#77172 = CARTESIAN_POINT ( 'NONE',  ( -21.05000000000000071, 68.58368164137472434, -224.2353459317783120 ) ) ;
#77173 = FACE_OUTER_BOUND ( 'NONE', #79835, .T. ) ;
#77174 = CARTESIAN_POINT ( 'NONE',  ( 23.14999999999999858, 33.13294339707397285, -247.6623911921324463 ) ) ;
#77175 = CARTESIAN_POINT ( 'NONE',  ( 23.14999999999999503, 6.450000000011156587, -54.65000000000000568 ) ) ;
#77176 = EDGE_LOOP ( 'NONE', ( #5965, #67015, #137179, #48417 ) ) ;
#77177 = CARTESIAN_POINT ( 'NONE',  ( -19.89999999999999858, 11.61130914238355771, 21.90000000000000213 ) ) ;
#77179 = ADVANCED_FACE ( 'NONE', ( #204737 ), #145929, .T. ) ;
#77178 = CARTESIAN_POINT ( 'NONE',  ( -18.59999999999999787, 67.23127455305835554, -235.8551265064784559 ) ) ;
#77180 = CARTESIAN_POINT ( 'NONE',  ( 21.14999999999999858, 76.10000000001170406, -76.06376443622556849 ) ) ;
#77182 = LINE ( 'NONE', #34246, #249437 ) ;
#77181 = CARTESIAN_POINT ( 'NONE',  ( -18.59999999999999787, -1.835341550213255957, -45.05515129256298223 ) ) ;
#77183 = CARTESIAN_POINT ( 'NONE',  ( 21.05000000000000071, 84.66355140188093742, -79.04720860259155302 ) ) ;
#77184 = EDGE_CURVE ( 'NONE', #169096, #113211, #254257, .T. ) ;
#77185 = CARTESIAN_POINT ( 'NONE',  ( 21.14999999999999858, 1.115600667400684642E-11, -26.95934304829875927 ) ) ;
#77186 = CARTESIAN_POINT ( 'NONE',  ( -20.90000000000000213, -11.75000000000000178, 0.000000000000000000 ) ) ;
#77187 = DIRECTION ( 'NONE',  ( 2.952720810173289112E-16, -1.000000000000000000, 0.000000000000000000 ) ) ;
#77189 = EDGE_LOOP ( 'NONE', ( #218405, #187459, #256069, #40031 ) ) ;
#77188 = AXIS2_PLACEMENT_3D ( 'NONE', #57250, #135509, #118557 ) ;
#77190 = AXIS2_PLACEMENT_3D ( 'NONE', #59292, #116740, #176737 ) ;
#77191 = ORIENTED_EDGE ( 'NONE', *, *, #66758, .T. ) ;
#77192 = EDGE_CURVE ( 'NONE', #113369, #79663, #208507, .T. ) ;
#77193 = DIRECTION ( 'NONE',  ( -0.000000000000000000, -0.2617529984165031243, -0.9651348961777157509 ) ) ;
#77194 = VERTEX_POINT ( 'NONE', #224313 ) ;
#77195 = EDGE_CURVE ( 'NONE', #200910, #143844, #189, .T. ) ;
#77196 = FACE_OUTER_BOUND ( 'NONE', #186858, .T. ) ;
#77197 = EDGE_CURVE ( 'NONE', #218463, #31922, #141836, .T. ) ;
#77198 = CYLINDRICAL_SURFACE ( 'NONE', #204514, 0.1000000000000028644 ) ;
#77199 = AXIS2_PLACEMENT_3D ( 'NONE', #13656, #248419, #131032 ) ;
#77200 = VERTEX_POINT ( 'NONE', #109489 ) ;
#77201 = CARTESIAN_POINT ( 'NONE',  ( -20.54999999999999716, 1.115600667400684642E-11, -134.0000000000000284 ) ) ;
#77202 = DIRECTION ( 'NONE',  ( -1.000000000000000000, 0.000000000000000000, 0.000000000000000000 ) ) ;
#77203 = DIRECTION ( 'NONE',  ( -1.000000000000000000, 0.000000000000000000, 0.000000000000000000 ) ) ;
#77204 = VECTOR ( 'NONE', #36254, 1000.000000000000000 ) ;
#77205 = CARTESIAN_POINT ( 'NONE',  ( 20.94999999999999929, 1.115600667400684642E-11, -138.0000000000000284 ) ) ;
#77207 = ORIENTED_EDGE ( 'NONE', *, *, #83085, .F. ) ;
#77206 = CARTESIAN_POINT ( 'NONE',  ( -16.87683809663752399, 9.865889849343231432, -187.7325731929304879 ) ) ;
#77209 = DIRECTION ( 'NONE',  ( 0.000000000000000000, -0.2128009952257606530, 0.9770955615654620674 ) ) ;
#77208 = FACE_OUTER_BOUND ( 'NONE', #42250, .T. ) ;
#77210 = EDGE_CURVE ( 'NONE', #88201, #104499, #148649, .T. ) ;
#77211 = CARTESIAN_POINT ( 'NONE',  ( 20.85000000000000142, -1.835859311432481045, -179.1044391687985353 ) ) ;
#77212 = CARTESIAN_POINT ( 'NONE',  ( 23.15000000000000213, -11.64999999998884483, -33.50000000000000000 ) ) ;
#77213 = DIRECTION ( 'NONE',  ( 0.000000000000000000, -0.000000000000000000, 1.000000000000000000 ) ) ;
#77214 = DIRECTION ( 'NONE',  ( 0.000000000000000000, -0.9987946567507778317, 0.04908394489133698774 ) ) ;
#77215 = VERTEX_POINT ( 'NONE', #186483 ) ;
#77216 = DIRECTION ( 'NONE',  ( 0.000000000000000000, 0.000000000000000000, 1.000000000000000000 ) ) ;
#77217 = CARTESIAN_POINT ( 'NONE',  ( -22.39999999999999858, 75.90000000001214175, -136.5231074845242745 ) ) ;
#77218 = ORIENTED_EDGE ( 'NONE', *, *, #210132, .F. ) ;
#77219 = DIRECTION ( 'NONE',  ( -1.000000000000000000, -0.000000000000000000, 0.000000000000000000 ) ) ;
#77220 = ORIENTED_EDGE ( 'NONE', *, *, #39146, .F. ) ;
#77221 = CIRCLE ( 'NONE', #198021, 0.1000000000000108025 ) ;
#77223 = DIRECTION ( 'NONE',  ( -1.000000000000000000, 0.000000000000000000, 0.000000000000000000 ) ) ;
#77222 = AXIS2_PLACEMENT_3D ( 'NONE', #80734, #42919, #118622 ) ;
#77224 = CYLINDRICAL_SURFACE ( 'NONE', #149226, 0.09999999999999939493 ) ;
#77225 = FACE_OUTER_BOUND ( 'NONE', #181591, .T. ) ;
#77226 = VERTEX_POINT ( 'NONE', #228178 ) ;
#77227 = EDGE_LOOP ( 'NONE', ( #232355, #176915, #152889, #120099 ) ) ;
#77228 = CARTESIAN_POINT ( 'NONE',  ( -20.64999999999999858, 4.349999999999999645, -12.25000000000000000 ) ) ;
#77229 = CARTESIAN_POINT ( 'NONE',  ( 23.14999999999999503, 11.75000000001116263, -155.7499999999999716 ) ) ;
#77230 = FACE_OUTER_BOUND ( 'NONE', #152213, .T. ) ;
#77231 = CARTESIAN_POINT ( 'NONE',  ( -16.90202395485798093, 66.03405545546124245, -90.42612120578500878 ) ) ;
#77234 = DIRECTION ( 'NONE',  ( 0.000000000000000000, -1.000000000000000000, -6.982962677686265922E-15 ) ) ;
#77233 = AXIS2_PLACEMENT_3D ( 'NONE', #104338, #82198, #161799 ) ;
#77232 = LINE ( 'NONE', #215466, #57488 ) ;
#77235 = CARTESIAN_POINT ( 'NONE',  ( -18.58735405345342784, -9.566478620336599903, -40.32271464626595758 ) ) ;
#77236 = VECTOR ( 'NONE', #146919, 1000.000000000000000 ) ;
#77237 = CARTESIAN_POINT ( 'NONE',  ( 20.95512820512820440, 65.37615131629999610, -90.87310748452438247 ) ) ;
#77238 = LINE ( 'NONE', #201051, #172304 ) ;
#77240 = EDGE_LOOP ( 'NONE', ( #15339, #217903, #192812, #36426 ) ) ;
#77239 = CIRCLE ( 'NONE', #164745, 0.09999999999998898659 ) ;
#77241 = DIRECTION ( 'NONE',  ( 0.000000000000000000, 0.8814952561688430555, -0.4721928772777346239 ) ) ;
#77242 = CIRCLE ( 'NONE', #64774, 0.1000000000000028644 ) ;
#77243 = EDGE_CURVE ( 'NONE', #4043, #17513, #25167, .T. ) ;
#77245 = ORIENTED_EDGE ( 'NONE', *, *, #212202, .T. ) ;
#77244 = DIRECTION ( 'NONE',  ( -1.000000000000000000, 2.952720810173289112E-16, 2.061873921506763405E-30 ) ) ;
#77246 = FACE_OUTER_BOUND ( 'NONE', #199573, .T. ) ;
#77247 = CYLINDRICAL_SURFACE ( 'NONE', #215763, 0.1000000000000028644 ) ;
#77249 = CYLINDRICAL_SURFACE ( 'NONE', #211391, 0.1000000000000024342 ) ;
#77248 = FACE_OUTER_BOUND ( 'NONE', #215557, .T. ) ;
#77250 = ORIENTED_EDGE ( 'NONE', *, *, #108656, .F. ) ;
#77252 = DIRECTION ( 'NONE',  ( -1.000000000000000000, -0.000000000000000000, 0.000000000000000000 ) ) ;
#77251 = FACE_OUTER_BOUND ( 'NONE', #58133, .T. ) ;
#77253 = CARTESIAN_POINT ( 'NONE',  ( 19.75857864376268935, 54.53338637621133955, -228.6684279704127789 ) ) ;
#77254 = DIRECTION ( 'NONE',  ( 1.020425574104004196E-15, -6.982962677686266711E-15, 1.000000000000000000 ) ) ;
#77255 = CARTESIAN_POINT ( 'NONE',  ( 20.85000000000000142, 7.070967871809997973, -70.74656422186831151 ) ) ;
#77257 = EDGE_CURVE ( 'NONE', #62762, #70815, #83370, .T. ) ;
#77256 = CARTESIAN_POINT ( 'NONE',  ( -18.58735405345342429, 85.56647862034844820, -96.20039283825825294 ) ) ;
#77258 = VERTEX_POINT ( 'NONE', #139943 ) ;
#77259 = FACE_OUTER_BOUND ( 'NONE', #130625, .T. ) ;
#77260 = ORIENTED_EDGE ( 'NONE', *, *, #178726, .T. ) ;
#77261 = EDGE_CURVE ( 'NONE', #3690, #212292, #219489, .T. ) ;
#77262 = ADVANCED_FACE ( 'NONE', ( #74266 ), #91238, .F. ) ;
#77263 = CARTESIAN_POINT ( 'NONE',  ( 22.45380639571440895, 75.99999985733725794, -215.2735403756365429 ) ) ;
#77264 = ORIENTED_EDGE ( 'NONE', *, *, #116110, .F. ) ;
#77265 = CARTESIAN_POINT ( 'NONE',  ( -20.93975676684922504, 46.39397692848788068, -243.0687461883537424 ) ) ;
#77266 = AXIS2_PLACEMENT_3D ( 'NONE', #231678, #70042, #34775 ) ;
#77267 = ORIENTED_EDGE ( 'NONE', *, *, #205563, .F. ) ;
#77268 = LINE ( 'NONE', #236357, #160059 ) ;
#77269 = CIRCLE ( 'NONE', #64790, 0.09999999999999939493 ) ;
#77270 = DIRECTION ( 'NONE',  ( 0.000000000000000000, -6.982962677686266711E-15, 1.000000000000000000 ) ) ;
#77272 = ORIENTED_EDGE ( 'NONE', *, *, #120941, .F. ) ;
#77271 = AXIS2_PLACEMENT_3D ( 'NONE', #36930, #116438, #151733 ) ;
#77273 = EDGE_CURVE ( 'NONE', #33512, #223504, #134190, .T. ) ;
#77274 = AXIS2_PLACEMENT_3D ( 'NONE', #128975, #226774, #170714 ) ;
#77275 = EDGE_CURVE ( 'NONE', #227551, #150544, #237640, .T. ) ;
#77276 = AXIS2_PLACEMENT_3D ( 'NONE', #190570, #182558, #43036 ) ;
#77278 = CARTESIAN_POINT ( 'NONE',  ( -18.39999999999999858, -9.499999999988849808, -174.1001893912220737 ) ) ;
#77277 = AXIS2_PLACEMENT_3D ( 'NONE', #171135, #208928, #10736 ) ;
#77279 = DIRECTION ( 'NONE',  ( 1.000000000000000000, 0.000000000000000000, 0.000000000000000000 ) ) ;
#77280 = CARTESIAN_POINT ( 'NONE',  ( 23.15000000000000213, 11.31726856452598362, -246.8669175193824969 ) ) ;
#77281 = FACE_OUTER_BOUND ( 'NONE', #158896, .T. ) ;
#77282 = CARTESIAN_POINT ( 'NONE',  ( 19.94784844284945180, 62.39243729835731500, -208.9482361014044329 ) ) ;
#77283 = VERTEX_POINT ( 'NONE', #70419 ) ;
#77284 = DIRECTION ( 'NONE',  ( 0.000000000000000000, -0.2128009952263603677, 0.9770955615653313941 ) ) ;
#77285 = ORIENTED_EDGE ( 'NONE', *, *, #250390, .T. ) ;
#77287 = ORIENTED_EDGE ( 'NONE', *, *, #63896, .T. ) ;
#77286 = CARTESIAN_POINT ( 'NONE',  ( 23.15000000000000213, 85.50000000001222134, -146.4170766071767389 ) ) ;
#77288 = CIRCLE ( 'NONE', #156633, 0.5000000000000004441 ) ;
#77289 = ORIENTED_EDGE ( 'NONE', *, *, #180201, .F. ) ;
#77290 = CARTESIAN_POINT ( 'NONE',  ( 21.07094088545368749, 0.09889370256337753906, -60.67983277808289699 ) ) ;
#77291 = CARTESIAN_POINT ( 'NONE',  ( 18.39999999999999503, 59.20211495293902004, -220.5705723384363921 ) ) ;
#77292 = AXIS2_PLACEMENT_3D ( 'NONE', #228487, #103364, #102434 ) ;
#77293 = CARTESIAN_POINT ( 'NONE',  ( 20.94999999999999929, 78.08573236070779444, -228.9307947190811774 ) ) ;
#77294 = EDGE_CURVE ( 'NONE', #101453, #97478, #112092, .T. ) ;
#77295 = DIRECTION ( 'NONE',  ( 0.000000000000000000, -0.1350103645451557199, -0.9908441862701644620 ) ) ;
#77296 = ORIENTED_EDGE ( 'NONE', *, *, #14663, .T. ) ;
#77297 = EDGE_CURVE ( 'NONE', #204733, #110754, #75536, .T. ) ;
#77298 = EDGE_CURVE ( 'NONE', #81857, #103692, #228410, .T. ) ;
#77299 = VECTOR ( 'NONE', #40116, 999.9999999999998863 ) ;
#77300 = DIRECTION ( 'NONE',  ( 0.000000000000000000, -0.1350103645451876666, -0.9908441862701600211 ) ) ;
#77301 = DIRECTION ( 'NONE',  ( 0.000000000000000000, 0.9770955615653551529, 0.2128009952262517601 ) ) ;
#77302 = VECTOR ( 'NONE', #45807, 999.9999999999998863 ) ;
#77303 = VERTEX_POINT ( 'NONE', #15567 ) ;
#77305 = ORIENTED_EDGE ( 'NONE', *, *, #56336, .T. ) ;
#77304 = DIRECTION ( 'NONE',  ( 0.000000000000000000, 0.000000000000000000, 1.000000000000000000 ) ) ;
#77306 = LINE ( 'NONE', #155610, #152421 ) ;
#77307 = CARTESIAN_POINT ( 'NONE',  ( -16.87683809663750978, 9.950000000011137047, -80.40236401819653622 ) ) ;
#77308 = ORIENTED_EDGE ( 'NONE', *, *, #10063, .F. ) ;
#77309 = DIRECTION ( 'NONE',  ( 0.000000000000000000, -6.982962677686267499E-15, 1.000000000000000000 ) ) ;
#77310 = ORIENTED_EDGE ( 'NONE', *, *, #99495, .T. ) ;
#77311 = CARTESIAN_POINT ( 'NONE',  ( 20.94999999999999574, 74.83729825007360148, -61.62310748452433273 ) ) ;
#77312 = EDGE_CURVE ( 'NONE', #245302, #109034, #91783, .T. ) ;
#77313 = PLANE ( 'NONE',  #6364 ) ;
#77314 = CARTESIAN_POINT ( 'NONE',  ( 15.31784899511109899, 66.60336962369380842, -51.61605009170609293 ) ) ;
#77315 = CARTESIAN_POINT ( 'NONE',  ( -18.50000000000000000, 5.341242990002803559, -124.1933497935119988 ) ) ;
#77316 = VECTOR ( 'NONE', #1324, 1000.000000000000000 ) ;
#77317 = VECTOR ( 'NONE', #141224, 1000.000000000000000 ) ;
#77318 = EDGE_CURVE ( 'NONE', #212023, #19725, #21264, .T. ) ;
#77319 = B_SPLINE_CURVE_WITH_KNOTS ( 'NONE', 3,
 ( #249055, #89952, #232058, #53402, #67825, #147369 ),
 .UNSPECIFIED., .F., .F.,
 ( 4, 2, 4 ),
 ( 0.000000000000000000, 0.0001496588209255951573, 0.0002993176418511903146 ),
 .UNSPECIFIED. ) ;
#77320 = ORIENTED_EDGE ( 'NONE', *, *, #249884, .T. ) ;
#77321 = FACE_OUTER_BOUND ( 'NONE', #124264, .T. ) ;
#77322 = CIRCLE ( 'NONE', #73100, 0.09999999999999939493 ) ;
#77323 = ORIENTED_EDGE ( 'NONE', *, *, #108625, .T. ) ;
#77324 = EDGE_CURVE ( 'NONE', #225466, #286, #216853, .T. ) ;
#77325 = CARTESIAN_POINT ( 'NONE',  ( -23.24999999999999645, -9.599999999988845900, -140.6001893912220737 ) ) ;
#77327 = ORIENTED_EDGE ( 'NONE', *, *, #142924, .F. ) ;
#77326 = LINE ( 'NONE', #154362, #145874 ) ;
#77328 = DIRECTION ( 'NONE',  ( -1.000000000000000000, -0.000000000000000000, -0.000000000000000000 ) ) ;
#77329 = CARTESIAN_POINT ( 'NONE',  ( 21.72449340488910607, 10.28395627750227703, -143.2500000000000284 ) ) ;
#77330 = CARTESIAN_POINT ( 'NONE',  ( 22.49436431346199683, 64.35004905235850003, -103.0900110142466417 ) ) ;
#77332 = DIRECTION ( 'NONE',  ( 0.000000000000000000, -1.000000000000000000, -6.982962677686266711E-15 ) ) ;
#77331 = VECTOR ( 'NONE', #127842, 1000.000000000000227 ) ;
#77333 = DIRECTION ( 'NONE',  ( -0.7071067811865463515, -0.7071067811865487940, 7.587431340288849180E-16 ) ) ;
#77334 = VECTOR ( 'NONE', #149387, 1000.000000000000000 ) ;
#77335 = ADVANCED_FACE ( 'NONE', ( #52079 ), #36414, .F. ) ;
#77336 = DIRECTION ( 'NONE',  ( 1.000000000000000000, 2.952720810173289112E-16, -0.000000000000000000 ) ) ;
#77337 = CARTESIAN_POINT ( 'NONE',  ( -18.42609945526433535, 85.49999971050304737, -129.5237449942748640 ) ) ;
#77339 = ORIENTED_EDGE ( 'NONE', *, *, #142418, .F. ) ;
#77338 = DIRECTION ( 'NONE',  ( 0.000000000000000000, 0.9126074666063660468, 0.4088369013363524762 ) ) ;
#77340 = AXIS2_PLACEMENT_3D ( 'NONE', #90377, #168696, #246886 ) ;
#77341 = EDGE_CURVE ( 'NONE', #212737, #12445, #11706, .T. ) ;
#77343 = ADVANCED_FACE ( 'NONE', ( #53383 ), #115931, .T. ) ;
#77342 = FACE_OUTER_BOUND ( 'NONE', #154941, .T. ) ;
#77344 = EDGE_CURVE ( 'NONE', #249092, #41516, #121229, .T. ) ;
#77345 = AXIS2_PLACEMENT_3D ( 'NONE', #16822, #213714, #71662 ) ;
#77346 = CARTESIAN_POINT ( 'NONE',  ( 21.46681500593529535, 69.14248884062985212, -103.0231074845243597 ) ) ;
#77347 = ORIENTED_EDGE ( 'NONE', *, *, #149901, .T. ) ;
#77348 = DIRECTION ( 'NONE',  ( -1.000000000000000000, -0.000000000000000000, -0.000000000000000000 ) ) ;
#77349 = DIRECTION ( 'NONE',  ( -0.000000000000000000, -0.000000000000000000, 1.000000000000000000 ) ) ;
#77350 = ORIENTED_EDGE ( 'NONE', *, *, #238339, .T. ) ;
#77351 = AXIS2_PLACEMENT_3D ( 'NONE', #69841, #67247, #206764 ) ;
#77352 = AXIS2_PLACEMENT_3D ( 'NONE', #36140, #116942, #238156 ) ;
#77354 = ADVANCED_FACE ( 'NONE', ( #229459 ), #152516, .F. ) ;
#77353 = DIRECTION ( 'NONE',  ( 0.000000000000000000, 0.2617529984165152257, 0.9651348961777124202 ) ) ;
#77355 = CIRCLE ( 'NONE', #10746, 0.09999999999999939493 ) ;
#77356 = EDGE_CURVE ( 'NONE', #136008, #202789, #158618, .T. ) ;
#77357 = CARTESIAN_POINT ( 'NONE',  ( -16.93440969289730802, 66.00481482419864676, -190.9318732995136259 ) ) ;
#77358 = VERTEX_POINT ( 'NONE', #100177 ) ;
#77359 = DIRECTION ( 'NONE',  ( 0.000000000000000000, 7.086529944415886769E-15, -1.000000000000000000 ) ) ;
#77360 = ORIENTED_EDGE ( 'NONE', *, *, #171600, .F. ) ;
#77361 = EDGE_CURVE ( 'NONE', #224786, #96826, #16841, .T. ) ;
#77362 = PLANE ( 'NONE',  #4703 ) ;
#77364 = ORIENTED_EDGE ( 'NONE', *, *, #2175, .F. ) ;
#77363 = CARTESIAN_POINT ( 'NONE',  ( -18.59999999999999787, -1.835341550224411922, -11.55515129256297868 ) ) ;
#77365 = DIRECTION ( 'NONE',  ( 0.000000000000000000, 0.000000000000000000, -1.000000000000000000 ) ) ;
#77366 = ORIENTED_EDGE ( 'NONE', *, *, #178, .F. ) ;
#77367 = CARTESIAN_POINT ( 'NONE',  ( -23.15000000000000213, 11.75000000001115907, -93.65839931010299324 ) ) ;
#77369 = VERTEX_POINT ( 'NONE', #217566 ) ;
#77368 = EDGE_CURVE ( 'NONE', #106325, #59419, #104408, .T. ) ;
#77371 = ORIENTED_EDGE ( 'NONE', *, *, #57814, .T. ) ;
#77370 = ORIENTED_EDGE ( 'NONE', *, *, #204028, .F. ) ;
#77372 = CARTESIAN_POINT ( 'NONE',  ( 18.39999999999999858, 85.50000000001209344, -129.4910380878245633 ) ) ;
#77373 = ORIENTED_EDGE ( 'NONE', *, *, #142407, .F. ) ;
#77374 = ADVANCED_FACE ( 'NONE', ( #198014 ), #372, .F. ) ;
#77375 = CYLINDRICAL_SURFACE ( 'NONE', #6595, 1.500000000000001332 ) ;
#77376 = VECTOR ( 'NONE', #55026, 1000.000000000000000 ) ;
#77377 = EDGE_LOOP ( 'NONE', ( #45230, #22770, #197729, #183300 ) ) ;
#77378 = ADVANCED_FACE ( 'NONE', ( #79343 ), #216295, .F. ) ;
#77379 = AXIS2_PLACEMENT_3D ( 'NONE', #102583, #182165, #162606 ) ;
#77380 = ORIENTED_EDGE ( 'NONE', *, *, #217623, .F. ) ;
#77381 = DIRECTION ( 'NONE',  ( -1.000000000000000000, 0.000000000000000000, 0.000000000000000000 ) ) ;
#77382 = DIRECTION ( 'NONE',  ( -0.000000000000000000, 1.000000000000000000, 6.982962677686266711E-15 ) ) ;
#77383 = CARTESIAN_POINT ( 'NONE',  ( 23.25000000000000000, 81.75190851390706825, -227.2043352493130612 ) ) ;
#77384 = DIRECTION ( 'NONE',  ( -0.000000000000000000, 0.8660254037844411501, 0.4999999999999956146 ) ) ;
#77385 = ORIENTED_EDGE ( 'NONE', *, *, #132796, .T. ) ;
#77386 = CARTESIAN_POINT ( 'NONE',  ( -22.39999999999999858, 64.25000000001165290, -69.62310748452439668 ) ) ;
#77387 = CARTESIAN_POINT ( 'NONE',  ( 21.08489247129321598, 67.12232480914222776, -157.6731074845244223 ) ) ;
#77388 = EDGE_CURVE ( 'NONE', #60388, #137538, #167018, .T. ) ;
#77389 = CARTESIAN_POINT ( 'NONE',  ( -22.84999999999999787, 0.000000000000000000, -4.000000000000000000 ) ) ;
#77390 = VERTEX_POINT ( 'NONE', #221412 ) ;
#77391 = DIRECTION ( 'NONE',  ( 1.020425574104004196E-15, 1.210927747993693964E-31, 1.000000000000000000 ) ) ;
#77392 = FACE_OUTER_BOUND ( 'NONE', #118528, .T. ) ;
#77393 = CYLINDRICAL_SURFACE ( 'NONE', #94927, 12.87500000000000178 ) ;
#77394 = ORIENTED_EDGE ( 'NONE', *, *, #245685, .T. ) ;
#77395 = DIRECTION ( 'NONE',  ( 2.952720810173289112E-16, -0.9770955615653302839, -0.2128009952263658355 ) ) ;
#77396 = ORIENTED_EDGE ( 'NONE', *, *, #244498, .T. ) ;
#77397 = VERTEX_POINT ( 'NONE', #196736 ) ;
#77398 = CARTESIAN_POINT ( 'NONE',  ( 22.50000000000000000, 0.1000000000111554016, -122.3504291924552234 ) ) ;
#77399 = VERTEX_POINT ( 'NONE', #58491 ) ;
#77400 = VERTEX_POINT ( 'NONE', #1079 ) ;
#77401 = CARTESIAN_POINT ( 'NONE',  ( -21.05000000000000071, -11.48912529306489994, -197.8999999999999773 ) ) ;
#77402 = CARTESIAN_POINT ( 'NONE',  ( -17.71734398241073194, 10.84235722847571459, -157.2251382530056674 ) ) ;
#77403 = ORIENTED_EDGE ( 'NONE', *, *, #34401, .F. ) ;
#77404 = EDGE_LOOP ( 'NONE', ( #179512, #56735, #181079, #148471 ) ) ;
#77405 = CARTESIAN_POINT ( 'NONE',  ( 20.85000000000000142, 62.88396779178381735, -206.9948552354529170 ) ) ;
#77406 = CARTESIAN_POINT ( 'NONE',  ( -21.05000000000000071, 76.00000000001195133, -103.0231074845243171 ) ) ;
#77407 = ORIENTED_EDGE ( 'NONE', *, *, #125890, .F. ) ;
#77408 = VERTEX_POINT ( 'NONE', #157662 ) ;
#77409 = AXIS2_PLACEMENT_3D ( 'NONE', #225121, #127332, #223842 ) ;
#77410 = AXIS2_PLACEMENT_3D ( 'NONE', #212066, #133789, #37284 ) ;
#77411 = ORIENTED_EDGE ( 'NONE', *, *, #253038, .F. ) ;
#77412 = VECTOR ( 'NONE', #24347, 1000.000000000000000 ) ;
#77413 = TOROIDAL_SURFACE ( 'NONE', #110749, 6.258578643762712446, 0.1000000000000000056 ) ;
#77414 = DIRECTION ( 'NONE',  ( 0.000000000000000000, 0.000000000000000000, -1.000000000000000000 ) ) ;
#77415 = EDGE_CURVE ( 'NONE', #95768, #154701, #250183, .T. ) ;
#77416 = DIRECTION ( 'NONE',  ( 2.489438768765008884E-17, 0.1686199900910312910, -0.9856811345164826488 ) ) ;
#77417 = DIRECTION ( 'NONE',  ( 1.000000000000000000, 2.952720810173289112E-16, -0.000000000000000000 ) ) ;
#77418 = CARTESIAN_POINT ( 'NONE',  ( -20.64999999999999858, 1.115600667400684642E-11, -33.50000000000000000 ) ) ;
#77419 = CARTESIAN_POINT ( 'NONE',  ( -18.40000000000000213, 11.33174054713631662, -46.15000000000000568 ) ) ;
#77420 = CYLINDRICAL_SURFACE ( 'NONE', #256667, 12.87499999999999822 ) ;
#77421 = CYLINDRICAL_SURFACE ( 'NONE', #52205, 0.09999999999999939493 ) ;
#77423 = CARTESIAN_POINT ( 'NONE',  ( 20.94999999999999574, 87.41227409416205774, -167.0231074845242745 ) ) ;
#77422 = CARTESIAN_POINT ( 'NONE',  ( 21.05000000000000071, 75.90156250001138005, -75.82233839461660807 ) ) ;
#77424 = LINE ( 'NONE', #61739, #115653 ) ;
#77425 = CARTESIAN_POINT ( 'NONE',  ( -16.89155683853296352, 23.53109276876853428, -231.2313039298783508 ) ) ;
#77426 = DIRECTION ( 'NONE',  ( -1.000000000000000000, -0.000000000000000000, -0.000000000000000000 ) ) ;
#77427 = ADVANCED_FACE ( 'NONE', ( #257948 ), #18101, .T. ) ;
#77428 = CARTESIAN_POINT ( 'NONE',  ( 21.05995757104869526, 44.20038294471087426, -236.5569497315613035 ) ) ;
#77429 = AXIS2_PLACEMENT_3D ( 'NONE', #120551, #15028, #56664 ) ;
#77430 = VERTEX_POINT ( 'NONE', #97609 ) ;
#77431 = CIRCLE ( 'NONE', #185786, 3.970710678118657189 ) ;
#77433 = ORIENTED_EDGE ( 'NONE', *, *, #221326, .F. ) ;
#77432 = CARTESIAN_POINT ( 'NONE',  ( -21.05000000000000071, 76.00000000001165290, -69.52310748452431710 ) ) ;
#77434 = AXIS2_PLACEMENT_3D ( 'NONE', #120004, #198216, #221611 ) ;
#77435 = DIRECTION ( 'NONE',  ( 0.000000000000000000, 0.000000000000000000, -1.000000000000000000 ) ) ;
#77436 = AXIS2_PLACEMENT_3D ( 'NONE', #137928, #40163, #179657 ) ;
#77437 = VECTOR ( 'NONE', #53398, 1000.000000000000000 ) ;
#77438 = CARTESIAN_POINT ( 'NONE',  ( -22.50000000000000000, 64.09252369393823301, -247.0744076673471170 ) ) ;
#77439 = ORIENTED_EDGE ( 'NONE', *, *, #50517, .T. ) ;
#77440 = CARTESIAN_POINT ( 'NONE',  ( 20.94999999999999929, 10.29270135741298731, -206.4573618871519045 ) ) ;
#77441 = DIRECTION ( 'NONE',  ( 0.000000000000000000, 0.000000000000000000, 1.000000000000000000 ) ) ;
#77442 = ORIENTED_EDGE ( 'NONE', *, *, #233362, .T. ) ;
#77444 = CARTESIAN_POINT ( 'NONE',  ( -18.55807992284871943, 10.32898536001801126, -206.5826683222764188 ) ) ;
#77443 = AXIS2_PLACEMENT_3D ( 'NONE', #149304, #31926, #9760 ) ;
#77445 = CARTESIAN_POINT ( 'NONE',  ( 21.05000000000000071, 76.00000000001237765, -170.0231074845243597 ) ) ;
#77446 = AXIS2_PLACEMENT_3D ( 'NONE', #127943, #104490, #5387 ) ;
#77447 = DIRECTION ( 'NONE',  ( 0.000000000000000000, -0.4721928772777346239, -0.8814952561688430555 ) ) ;
#77449 = ORIENTED_EDGE ( 'NONE', *, *, #176193, .F. ) ;
#77448 = CARTESIAN_POINT ( 'NONE',  ( 21.05000000000000071, 74.65091558138531980, -162.0366085209788878 ) ) ;
#77450 = AXIS2_PLACEMENT_3D ( 'NONE', #59406, #239375, #179415 ) ;
#77452 = VERTEX_POINT ( 'NONE', #98890 ) ;
#77451 = FACE_OUTER_BOUND ( 'NONE', #175579, .T. ) ;
#77453 = CARTESIAN_POINT ( 'NONE',  ( -18.59999999999999787, 76.00000000001142553, -36.02310748452432421 ) ) ;
#77454 = LINE ( 'NONE', #236546, #170848 ) ;
#77455 = EDGE_CURVE ( 'NONE', #183594, #13712, #221117, .T. ) ;
#77456 = DIRECTION ( 'NONE',  ( -0.000000000000000000, 1.000000000000000000, 0.000000000000000000 ) ) ;
#77457 = DIRECTION ( 'NONE',  ( 0.000000000000000000, -0.1022405907414164900, -0.9947597004326451664 ) ) ;
#77459 = LINE ( 'NONE', #218261, #49512 ) ;
#77458 = CARTESIAN_POINT ( 'NONE',  ( -18.59999999999999787, 9.350000000011156942, -54.85000000000000142 ) ) ;
#77460 = LINE ( 'NONE', #236551, #137046 ) ;
#77461 = DIRECTION ( 'NONE',  ( 0.000000000000000000, -1.000000000000000000, -6.982962677686265922E-15 ) ) ;
#77462 = AXIS2_PLACEMENT_3D ( 'NONE', #246741, #128098, #87664 ) ;
#77463 = CARTESIAN_POINT ( 'NONE',  ( 20.94999999999999929, 76.00000000001126921, -203.5231074845248997 ) ) ;
#77464 = CARTESIAN_POINT ( 'NONE',  ( -20.94999999999999929, -11.41227409413852811, -64.10000000000000853 ) ) ;
#77465 = CARTESIAN_POINT ( 'NONE',  ( 21.08134388332232234, 10.05319037393296355, -228.1129092785580781 ) ) ;
#77466 = ORIENTED_EDGE ( 'NONE', *, *, #126321, .T. ) ;
#77467 = CYLINDRICAL_SURFACE ( 'NONE', #151421, 11.80000000000000782 ) ;
#77468 = ORIENTED_EDGE ( 'NONE', *, *, #63535, .F. ) ;
#77469 = ORIENTED_EDGE ( 'NONE', *, *, #180549, .T. ) ;
#77470 = EDGE_CURVE ( 'NONE', #170896, #207616, #171121, .T. ) ;
#77471 = FACE_OUTER_BOUND ( 'NONE', #91511, .T. ) ;
#77472 = ORIENTED_EDGE ( 'NONE', *, *, #122385, .F. ) ;
#77473 = APPLICATION_CONTEXT ( 'automotive_design' ) ;
#77474 = EDGE_CURVE ( 'NONE', #118431, #219246, #177214, .T. ) ;
#77475 = VECTOR ( 'NONE', #239653, 999.9999999999998863 ) ;
#77476 = CIRCLE ( 'NONE', #48465, 11.80000000000000249 ) ;
#77477 = VERTEX_POINT ( 'NONE', #119798 ) ;
#77478 = CIRCLE ( 'NONE', #227527, 11.89999999999999858 ) ;
#77479 = AXIS2_PLACEMENT_3D ( 'NONE', #153114, #93084, #115223 ) ;
#77480 = ADVANCED_FACE ( 'NONE', ( #76789 ), #122345, .F. ) ;
#77481 = VERTEX_POINT ( 'NONE', #20697 ) ;
#77482 = ORIENTED_EDGE ( 'NONE', *, *, #236912, .F. ) ;
#77483 = AXIS2_PLACEMENT_3D ( 'NONE', #136720, #175884, #59733 ) ;
#77484 = DIRECTION ( 'NONE',  ( -1.000000000000000000, 0.000000000000000000, -0.000000000000000000 ) ) ;
#77485 = CARTESIAN_POINT ( 'NONE',  ( -21.46681500597532022, -5.827586677109586333E-16, 6.857511159431289194 ) ) ;
#77486 = DIRECTION ( 'NONE',  ( 0.000000000000000000, 0.000000000000000000, 1.000000000000000000 ) ) ;
#77487 = DIRECTION ( 'NONE',  ( -1.000000000000000000, -0.000000000000000000, -0.000000000000000000 ) ) ;
#77488 = DIRECTION ( 'NONE',  ( 0.000000000000000000, 0.000000000000000000, -1.000000000000000000 ) ) ;
#77489 =( BOUNDED_SURFACE ( )  B_SPLINE_SURFACE ( 3, 2, ( 
 ( #158455, #120606, #17610 ),
 ( #39796, #38482, #136261 ),
 ( #201396, #178007, #176721 ),
 ( #159719, #237951, #257462 ),
 ( #60592, #239253, #215805 ),
 ( #256169, #219671, #118010 ) ),
 .UNSPECIFIED., .F., .F., .F. ) 
 B_SPLINE_SURFACE_WITH_KNOTS ( ( 4, 2, 4 ),
 ( 3, 3 ),
 ( 0.0001792624049599548033, 0.0003686986002124707481, 0.0005581347954649866928 ),
 ( 0.000000000000000000, 1.000000000000000000 ),
 .UNSPECIFIED. ) 
 GEOMETRIC_REPRESENTATION_ITEM ( )  RATIONAL_B_SPLINE_SURFACE ( (
 ( 1.000000000000000000, 0.9238795325112840739, 1.000000000000000000),
 ( 1.000000000000000000, 0.9229318695237281878, 1.000000000000000000),
 ( 1.000000000000000000, 0.8926288119232251850, 1.000000000000000000),
 ( 1.000000000000000000, 0.8123777807269819684, 1.000000000000000000),
 ( 1.000000000000000000, 0.7629087100932636645, 1.000000000000000000),
 ( 1.000000000000000000, 0.7071067811865475727, 1.000000000000000000) ) ) 
 REPRESENTATION_ITEM ( '' )  SURFACE ( )  );
#77490 = CARTESIAN_POINT ( 'NONE',  ( -18.39999999999999858, 77.26488334054519669, -241.9697969554615611 ) ) ;
#77491 = DIRECTION ( 'NONE',  ( 0.000000000000000000, 0.9908441862701600211, -0.1350103645451876666 ) ) ;
#77493 = VERTEX_POINT ( 'NONE', #220165 ) ;
#77492 = CARTESIAN_POINT ( 'NONE',  ( -23.25000000000000000, 11.65000000001115588, -188.8499999999999659 ) ) ;
#77495 = CARTESIAN_POINT ( 'NONE',  ( -21.76363531954647357, 65.30006722027489729, -242.5976422560627270 ) ) ;
#77494 = CARTESIAN_POINT ( 'NONE',  ( -21.14999999999999858, 11.65000000001115588, -167.4999999999999716 ) ) ;
#77496 = ADVANCED_FACE ( 'NONE', ( #256659 ), #161488, .F. ) ;
#77497 = DIRECTION ( 'NONE',  ( 1.000000000000000000, 7.304098846218133681E-16, 4.639676173203992654E-30 ) ) ;
#77498 = ORIENTED_EDGE ( 'NONE', *, *, #216083, .T. ) ;
#77499 = CARTESIAN_POINT ( 'NONE',  ( 20.94999999999999929, 70.50000000001158185, -57.11784146561126363 ) ) ;
#77500 = DIRECTION ( 'NONE',  ( -1.000000000000000000, -0.000000000000000000, -0.000000000000000000 ) ) ;
#77502 = VERTEX_POINT ( 'NONE', #2372 ) ;
#77501 = CIRCLE ( 'NONE', #11072, 0.1000000000000079159 ) ;
#77503 = VECTOR ( 'NONE', #234732, 1000.000000000000000 ) ;
#77505 = CARTESIAN_POINT ( 'NONE',  ( -20.64999999999999858, 1.925233644870972816, -113.2302435331261563 ) ) ;
#77504 = DIRECTION ( 'NONE',  ( 0.000000000000000000, 0.000000000000000000, 1.000000000000000000 ) ) ;
#77506 = DIRECTION ( 'NONE',  ( 0.000000000000000000, 1.000000000000000000, -6.308085367188393199E-16 ) ) ;
#77507 = CARTESIAN_POINT ( 'NONE',  ( 22.49999999999999645, 64.25043287652226809, -69.62396585362311896 ) ) ;
#77508 = VERTEX_POINT ( 'NONE', #235858 ) ;
#77509 = VERTEX_POINT ( 'NONE', #57205 ) ;
#77510 = CARTESIAN_POINT ( 'NONE',  ( 22.59999954896768770, 64.16406410971224261, -247.1982632919209379 ) ) ;
#77511 = DIRECTION ( 'NONE',  ( -0.000000000000000000, 0.2128009952263604232, -0.9770955615653316162 ) ) ;
#77512 = CIRCLE ( 'NONE', #256551, 0.1000000000000002554 ) ;
#77513 = LINE ( 'NONE', #179240, #119747 ) ;
#77514 = CARTESIAN_POINT ( 'NONE',  ( 12.25000000000000000, 26.54497872210689735, -232.9592037335782209 ) ) ;
#77515 = EDGE_LOOP ( 'NONE', ( #163082, #181637, #122961, #219798 ) ) ;
#77516 = EDGE_CURVE ( 'NONE', #205304, #11636, #112815, .T. ) ;
#77517 = DIRECTION ( 'NONE',  ( -2.840903330521631775E-16, 0.8700118002898321601, -0.4930308989875230030 ) ) ;
#77518 = B_SPLINE_CURVE_WITH_KNOTS ( 'NONE', 3,
 ( #221182, #244602, #159965, #140363, #123388, #25578, #41309, #120849, #103789, #183367, #201629, #23027, #84190, #182080, #223747, #165075, #5982, #101202, #161236 ),
 .UNSPECIFIED., .F., .F.,
 ( 4, 3, 3, 3, 3, 3, 4 ),
 ( 0.000000000000000000, 7.110282409890569127E-05, 0.0001508797727291477891, 0.0002027344179858564716, 0.0002343294522349123317, 0.0002454816334821249683, 0.0002619873080085630829 ),
 .UNSPECIFIED. ) ;
#77519 = CARTESIAN_POINT ( 'NONE',  ( 21.70464131381650219, 7.095358018979006864, -167.4999999999999716 ) ) ;
#77520 = CARTESIAN_POINT ( 'NONE',  ( 20.94999999999999574, 6.350000000011161383, -43.34382208968312966 ) ) ;
#77521 = AXIS2_PLACEMENT_3D ( 'NONE', #33300, #256089, #213171 ) ;
#77522 = VECTOR ( 'NONE', #72709, 1000.000000000000000 ) ;
#77523 = LINE ( 'NONE', #157113, #244895 ) ;
#77524 = CIRCLE ( 'NONE', #231696, 0.1000000000000000472 ) ;
#77525 = CIRCLE ( 'NONE', #73315, 3.999999999999994671 ) ;
#77526 = DIRECTION ( 'NONE',  ( 1.000000000000000000, 0.000000000000000000, 0.000000000000000000 ) ) ;
#77527 = EDGE_CURVE ( 'NONE', #199924, #46048, #42104, .T. ) ;
#77529 = ORIENTED_EDGE ( 'NONE', *, *, #231013, .T. ) ;
#77528 = DIRECTION ( 'NONE',  ( 0.000000000000000000, 0.6603344063872684799, -0.7509716850462297977 ) ) ;
#77530 = CARTESIAN_POINT ( 'NONE',  ( -21.14999999999999858, -11.64999999998884483, -33.50000000000000000 ) ) ;
#77531 = CARTESIAN_POINT ( 'NONE',  ( 18.59999999999999076, 65.79142135624952914, -148.7731074845244450 ) ) ;
#77532 = DIRECTION ( 'NONE',  ( -1.000000000000000000, 0.000000000000000000, 0.000000000000000000 ) ) ;
#77533 = DIRECTION ( 'NONE',  ( -1.000000000000000000, -0.000000000000000000, -0.000000000000000000 ) ) ;
#77534 = CARTESIAN_POINT ( 'NONE',  ( -0.8999999999999994671, -8.350000000000004974, 30.04142135623731136 ) ) ;
#77536 = ORIENTED_EDGE ( 'NONE', *, *, #91200, .T. ) ;
#77535 = CARTESIAN_POINT ( 'NONE',  ( -21.44999999999999929, 29.24307565605548120, -237.2405905340223455 ) ) ;
#77537 = DIRECTION ( 'NONE',  ( 1.000000000000000000, -0.000000000000000000, -0.000000000000000000 ) ) ;
#77538 = CARTESIAN_POINT ( 'NONE',  ( -20.64999999999999858, 1.999999999999998224, -20.27537807723789953 ) ) ;
#77539 = CARTESIAN_POINT ( 'NONE',  ( 20.90851465518105812, 67.49261718274587452, -195.4446851895584416 ) ) ;
#77540 = EDGE_CURVE ( 'NONE', #150108, #239317, #96225, .T. ) ;
#77541 = ORIENTED_EDGE ( 'NONE', *, *, #104544, .F. ) ;
#77542 = CARTESIAN_POINT ( 'NONE',  ( -20.64999999999999858, 11.60596396992030144, -220.2204734678737168 ) ) ;
#77543 = CARTESIAN_POINT ( 'NONE',  ( 21.05000000000000071, 75.90220970870319661, -176.2809220950059057 ) ) ;
#77544 = CARTESIAN_POINT ( 'NONE',  ( 18.49999999999998934, 65.75000000001251976, -178.7731074845244450 ) ) ;
#77545 = DIRECTION ( 'NONE',  ( 0.000000000000000000, -0.4999999999999689138, -0.8660254037844565822 ) ) ;
#77546 = CIRCLE ( 'NONE', #139910, 11.75000000000000000 ) ;
#77547 = ADVANCED_FACE ( 'NONE', ( #201876 ), #172858, .T. ) ;
#77548 = AXIS2_PLACEMENT_3D ( 'NONE', #219250, #83568, #61477 ) ;
#77549 = LINE ( 'NONE', #198800, #204993 ) ;
#77550 = DIRECTION ( 'NONE',  ( -1.000000000000000000, 0.000000000000000000, 0.000000000000000000 ) ) ;
#77551 = ORIENTED_EDGE ( 'NONE', *, *, #25433, .T. ) ;
#77552 = ORIENTED_EDGE ( 'NONE', *, *, #148924, .F. ) ;
#77554 = CARTESIAN_POINT ( 'NONE',  ( 6.100000000000000533, -11.75000000000000000, 13.90000000000000213 ) ) ;
#77553 = CIRCLE ( 'NONE', #19134, 0.1000000000000028644 ) ;
#77555 = CYLINDRICAL_SURFACE ( 'NONE', #158144, 4.049999999999998046 ) ;
#77556 = EDGE_CURVE ( 'NONE', #81484, #69698, #142027, .T. ) ;
#77557 = CARTESIAN_POINT ( 'NONE',  ( -20.64999999999999858, 1.115600667400684642E-11, -134.0000000000000284 ) ) ;
#77558 = DIRECTION ( 'NONE',  ( 0.000000000000000000, 1.000000000000000000, 0.000000000000000000 ) ) ;
#77559 = EDGE_LOOP ( 'NONE', ( #249473, #42818, #200377, #183988 ) ) ;
#77560 = CARTESIAN_POINT ( 'NONE',  ( -20.64999999999999858, 76.00000000001190870, -103.0231074845243029 ) ) ;
#77561 = ADVANCED_FACE ( 'NONE', ( #243568 ), #4923, .T. ) ;
#77563 = ADVANCED_FACE ( 'NONE', ( #145740 ), #62925, .T. ) ;
#77562 = DIRECTION ( 'NONE',  ( -1.000000000000000000, -5.641646265808601873E-14, 4.044497296483820071E-14 ) ) ;
#77564 = DIRECTION ( 'NONE',  ( 0.000000000000000000, 0.4088369013363281068, -0.9126074666063770380 ) ) ;
#77565 = DIRECTION ( 'NONE',  ( 0.000000000000000000, 0.000000000000000000, -1.000000000000000000 ) ) ;
#77566 = VECTOR ( 'NONE', #9441, 1000.000000000000000 ) ;
#77567 = ORIENTED_EDGE ( 'NONE', *, *, #98679, .F. ) ;
#77568 = CARTESIAN_POINT ( 'NONE',  ( 20.05000000000002913, 68.75000000001155342, -56.87310748452436826 ) ) ;
#77569 = ADVANCED_FACE ( 'NONE', ( #107905 ), #187467, .F. ) ;
#77570 = ORIENTED_EDGE ( 'NONE', *, *, #195398, .T. ) ;
#77571 = ORIENTED_EDGE ( 'NONE', *, *, #119420, .T. ) ;
#77572 = CARTESIAN_POINT ( 'NONE',  ( 20.94999999999999574, 1.835341550235567887, -145.5551512925629822 ) ) ;
#77573 = CARTESIAN_POINT ( 'NONE',  ( -20.54999999999999716, 44.91518204311810081, -238.0177672736398620 ) ) ;
#77574 = DIRECTION ( 'NONE',  ( 1.875376730785737719E-16, 1.000000000000000000, 6.982962677686266711E-15 ) ) ;
#77575 = ORIENTED_EDGE ( 'NONE', *, *, #202867, .F. ) ;
#77576 = EDGE_CURVE ( 'NONE', #50999, #13347, #242273, .T. ) ;
#77577 = EDGE_CURVE ( 'NONE', #43171, #258063, #143167, .T. ) ;
#77578 = CARTESIAN_POINT ( 'NONE',  ( -22.39999999999999858, 11.75000000001115552, -33.50000000000000000 ) ) ;
#77579 = CARTESIAN_POINT ( 'NONE',  ( -18.59999999999999787, 66.75000000001158185, -57.17310748452438673 ) ) ;
#77580 = FACE_OUTER_BOUND ( 'NONE', #159364, .T. ) ;
#77581 = VERTEX_POINT ( 'NONE', #85739 ) ;
#77582 = CARTESIAN_POINT ( 'NONE',  ( -23.15000000000000213, 76.00000000001192291, -98.97310748452431994 ) ) ;
#77584 = VERTEX_POINT ( 'NONE', #225265 ) ;
#77583 = LINE ( 'NONE', #212004, #175731 ) ;
#77585 = DIRECTION ( 'NONE',  ( 2.840903330521633255E-16, -0.09425075112713275638, -0.9955484899852801162 ) ) ;
#77586 = CARTESIAN_POINT ( 'NONE',  ( -18.46946985241236661, 85.50931722872408614, -163.0364449190248877 ) ) ;
#77587 = AXIS2_PLACEMENT_3D ( 'NONE', #61234, #179918, #195634 ) ;
#77588 = VECTOR ( 'NONE', #239214, 1000.000000000000000 ) ;
#77589 = VERTEX_POINT ( 'NONE', #46629 ) ;
#77590 =( BOUNDED_CURVE ( )  B_SPLINE_CURVE ( 3, ( #191985, #53726, #111136, #31633 ),
 .UNSPECIFIED., .F., .F. ) 
 B_SPLINE_CURVE_WITH_KNOTS ( ( 4, 4 ),
 ( 0.000000000000000000, 1.570796326794916320 ),
 .UNSPECIFIED. ) 
 CURVE ( )  GEOMETRIC_REPRESENTATION_ITEM ( )  RATIONAL_B_SPLINE_CURVE ( ( 1.000000000000000000, 0.8047378541243603856, 0.8047378541243603856, 1.000000000000000000 ) ) 
 REPRESENTATION_ITEM ( '' )  );
#77592 = DIRECTION ( 'NONE',  ( 1.000000000000000000, -0.000000000000000000, 0.000000000000000000 ) ) ;
#77591 =( GEOMETRIC_REPRESENTATION_CONTEXT ( 3 ) GLOBAL_UNCERTAINTY_ASSIGNED_CONTEXT ( ( #175790 ) ) GLOBAL_UNIT_ASSIGNED_CONTEXT ( ( #56340, #94189, #116351 ) ) REPRESENTATION_CONTEXT ( 'NONE', 'WORKASPACE' ) );
#77593 = CARTESIAN_POINT ( 'NONE',  ( -16.85312841634287295, 66.08639382269167584, -90.12593435123184804 ) ) ;
#77594 = CARTESIAN_POINT ( 'NONE',  ( 21.05000000000000071, -1.835341550213257733, -145.5551512925629822 ) ) ;
#77595 = ORIENTED_EDGE ( 'NONE', *, *, #23186, .F. ) ;
#77596 = DIRECTION ( 'NONE',  ( 1.000000000000000000, 0.000000000000000000, 0.000000000000000000 ) ) ;
#77597 = EDGE_CURVE ( 'NONE', #12394, #201923, #83730, .T. ) ;
#77598 = EDGE_CURVE ( 'NONE', #181206, #102067, #47922, .T. ) ;
#77599 = CYLINDRICAL_SURFACE ( 'NONE', #255605, 0.1000000000000028644 ) ;
#77600 = CYLINDRICAL_SURFACE ( 'NONE', #113759, 0.1000000000000028644 ) ;
#77601 = ORIENTED_EDGE ( 'NONE', *, *, #38713, .F. ) ;
#77602 = ADVANCED_FACE ( 'NONE', ( #247409 ), #83175, .F. ) ;
#77603 = EDGE_LOOP ( 'NONE', ( #126513, #143157, #100374, #204002 ) ) ;
#77604 = AXIS2_PLACEMENT_3D ( 'NONE', #244046, #146228, #186670 ) ;
#77605 = AXIS2_PLACEMENT_3D ( 'NONE', #5824, #68395, #7116 ) ;
#77606 = VERTEX_POINT ( 'NONE', #234261 ) ;
#77607 = AXIS2_PLACEMENT_3D ( 'NONE', #209783, #46207, #25391 ) ;
#77608 = DIRECTION ( 'NONE',  ( 0.000000000000000000, 0.000000000000000000, 1.000000000000000000 ) ) ;
#77609 = CARTESIAN_POINT ( 'NONE',  ( 21.11345278033270034, 8.882122073382243244, -45.74602217075484134 ) ) ;
#77611 = ORIENTED_EDGE ( 'NONE', *, *, #118274, .F. ) ;
#77610 = PLANE ( 'NONE',  #175161 ) ;
#77612 = DIRECTION ( 'NONE',  ( 0.000000000000000000, 0.9229812358756199764, -0.3848449534832346086 ) ) ;
#77614 = AXIS2_PLACEMENT_3D ( 'NONE', #179353, #141485, #223573 ) ;
#77613 = DIRECTION ( 'NONE',  ( 2.952720810173289112E-16, 1.000000000000000000, 6.982962677686266711E-15 ) ) ;
#77615 = CARTESIAN_POINT ( 'NONE',  ( -22.49533356619861735, 11.36930514850286222, -198.4572374200818672 ) ) ;
#77616 = VECTOR ( 'NONE', #48903, 1000.000000000000114 ) ;
#77617 = CARTESIAN_POINT ( 'NONE',  ( -18.50000000000000000, 85.40000000001167280, -62.64106563635157698 ) ) ;
#77618 = CARTESIAN_POINT ( 'NONE',  ( -18.50000000000000000, 44.14788529697245423, -236.0604079036328073 ) ) ;
#77619 = ADVANCED_FACE ( 'NONE', ( #92188 ), #126349, .F. ) ;
#77620 = DIRECTION ( 'NONE',  ( -1.000000000000000000, 0.000000000000000000, 0.000000000000000000 ) ) ;
#77622 = EDGE_LOOP ( 'NONE', ( #234273, #104034 ) ) ;
#77621 = FACE_OUTER_BOUND ( 'NONE', #20380, .T. ) ;
#77624 = ORIENTED_EDGE ( 'NONE', *, *, #198474, .T. ) ;
#77623 = CYLINDRICAL_SURFACE ( 'NONE', #186074, 0.09999999999999939493 ) ;
#77626 = CARTESIAN_POINT ( 'NONE',  ( -16.87998658237754412, 51.42389386751093383, -232.0338127545263944 ) ) ;
#77625 = CARTESIAN_POINT ( 'NONE',  ( 23.14999999999999503, 11.65000000001116298, -155.2500000000000284 ) ) ;
#77628 = ORIENTED_EDGE ( 'NONE', *, *, #189300, .F. ) ;
#77627 = CARTESIAN_POINT ( 'NONE',  ( 18.59999999999996945, 70.22659352830977753, -197.9852579278363578 ) ) ;
#77629 = EDGE_CURVE ( 'NONE', #99108, #158859, #183547, .T. ) ;
#77630 = ORIENTED_EDGE ( 'NONE', *, *, #137200, .F. ) ;
#77631 = DIRECTION ( 'NONE',  ( 0.000000000000000000, 0.000000000000000000, -1.000000000000000000 ) ) ;
#77632 = CARTESIAN_POINT ( 'NONE',  ( -21.05000000000000071, 87.29603075034741266, -133.4752083248603469 ) ) ;
#77633 = TOROIDAL_SURFACE ( 'NONE', #144263, 0.9750000000000019762, 0.1000000000000000056 ) ;
#77634 = AXIS2_PLACEMENT_3D ( 'NONE', #131055, #50220, #129771 ) ;
#77635 = AXIS2_PLACEMENT_3D ( 'NONE', #80429, #122177, #184697 ) ;
#77636 = CARTESIAN_POINT ( 'NONE',  ( -21.05000000000000071, 68.49522935589659767, -224.1230159437372436 ) ) ;
#77637 = CARTESIAN_POINT ( 'NONE',  ( -18.50000000000000000, 77.16412189325305349, -95.30825939895268561 ) ) ;
#77638 = EDGE_CURVE ( 'NONE', #159944, #41810, #54343, .T. ) ;
#77639 = CARTESIAN_POINT ( 'NONE',  ( 21.05000000000000071, 1.115600667400684642E-11, -131.1000000000000227 ) ) ;
#77640 = AXIS2_PLACEMENT_3D ( 'NONE', #51717, #33515, #173031 ) ;
#77641 = CARTESIAN_POINT ( 'NONE',  ( 23.14999999999999858, 21.15538238767524604, -233.7023398932965108 ) ) ;
#77642 = ADVANCED_FACE ( 'NONE', ( #133887 ), #191333, .T. ) ;
#77643 = CARTESIAN_POINT ( 'NONE',  ( -16.97683809663755028, 66.05000000001204796, -116.2946366524138142 ) ) ;
#77644 = EDGE_LOOP ( 'NONE', ( #114086, #51050, #244969, #129450 ) ) ;
#77645 = ORIENTED_EDGE ( 'NONE', *, *, #227411, .T. ) ;
#77646 = ADVANCED_FACE ( 'NONE', ( #132617 ), #150885, .F. ) ;
#77647 = DIRECTION ( 'NONE',  ( 0.000000000000000000, -1.000000000000000000, -6.982962677686265922E-15 ) ) ;
#77648 = AXIS2_PLACEMENT_3D ( 'NONE', #41228, #256320, #198982 ) ;
#77649 = EDGE_LOOP ( 'NONE', ( #162799, #243729, #70476, #123716, #166917 ) ) ;
#77650 = DIRECTION ( 'NONE',  ( 1.000000000000000000, 3.265361837132813093E-16, -0.000000000000000000 ) ) ;
#77651 = CARTESIAN_POINT ( 'NONE',  ( -16.97092634996615956, 51.61617950461997850, -231.8919089950969692 ) ) ;
#77653 = ADVANCED_FACE ( 'NONE', ( #12689 ), #191114, .F. ) ;
#77652 = DIRECTION ( 'NONE',  ( -0.000000000000000000, 1.000000000000000000, 6.982962677686266711E-15 ) ) ;
#77655 = ADVANCED_FACE ( 'NONE', ( #113048 ), #117739, .F. ) ;
#77654 = ADVANCED_FACE ( 'NONE', ( #33559 ), #13959, .F. ) ;
#77656 = CARTESIAN_POINT ( 'NONE',  ( 22.48660254037844197, 11.65000000001116298, -66.95000000000004547 ) ) ;
#77657 = ORIENTED_EDGE ( 'NONE', *, *, #184256, .F. ) ;
#77658 = CARTESIAN_POINT ( 'NONE',  ( -15.39126916658603150, 66.61042836546560864, -118.7054667721551766 ) ) ;
#77659 = ORIENTED_EDGE ( 'NONE', *, *, #64251, .F. ) ;
#77660 = FACE_OUTER_BOUND ( 'NONE', #151465, .T. ) ;
#77661 = ORIENTED_EDGE ( 'NONE', *, *, #150498, .T. ) ;
#77662 = VECTOR ( 'NONE', #115529, 1000.000000000000000 ) ;
#77663 = DIRECTION ( 'NONE',  ( 0.000000000000000000, -0.2617529984164955192, -0.9651348961777178603 ) ) ;
#77664 = CIRCLE ( 'NONE', #173612, 0.09999999999998898659 ) ;
#77665 = DIRECTION ( 'NONE',  ( 0.000000000000000000, 0.000000000000000000, -1.000000000000000000 ) ) ;
#77666 = AXIS2_PLACEMENT_3D ( 'NONE', #245554, #123036, #162177 ) ;
#77667 = VECTOR ( 'NONE', #29010, 1000.000000000000000 ) ;
#77668 = ORIENTED_EDGE ( 'NONE', *, *, #128338, .F. ) ;
#77669 = DIRECTION ( 'NONE',  ( 0.000000000000000000, 0.000000000000000000, 1.000000000000000000 ) ) ;
#77671 = ORIENTED_EDGE ( 'NONE', *, *, #224251, .F. ) ;
#77670 = SPHERICAL_SURFACE ( 'NONE', #142902, 0.1000000000000000056 ) ;
#77672 = EDGE_CURVE ( 'NONE', #86874, #141666, #10095, .T. ) ;
#77673 = DIRECTION ( 'NONE',  ( 0.000000000000000000, 1.000000000000000000, 1.387778780781444413E-14 ) ) ;
#77674 = EDGE_CURVE ( 'NONE', #79203, #242569, #76473, .T. ) ;
#77675 = ORIENTED_EDGE ( 'NONE', *, *, #62639, .T. ) ;
#77676 = VECTOR ( 'NONE', #197670, 1000.000000000000000 ) ;
#77677 = EDGE_CURVE ( 'NONE', #132438, #88936, #215975, .T. ) ;
#77678 = CARTESIAN_POINT ( 'NONE',  ( -18.69999999999999929, -10.84999999999999076, 31.59999999999999787 ) ) ;
#77679 = VERTEX_POINT ( 'NONE', #176894 ) ;
#77680 = CARTESIAN_POINT ( 'NONE',  ( -18.50000000000000000, 7.120270961697591439, -37.15956304183932701 ) ) ;
#77681 = PLANE ( 'NONE',  #197034 ) ;
#77682 = AXIS2_PLACEMENT_3D ( 'NONE', #175058, #69506, #149040 ) ;
#77684 = EDGE_CURVE ( 'NONE', #166580, #177411, #206208, .T. ) ;
#77683 = CARTESIAN_POINT ( 'NONE',  ( -20.94999999999999929, 65.70729864260954400, -30.56574559737245877 ) ) ;
#77685 = CARTESIAN_POINT ( 'NONE',  ( -16.87304349924914604, 9.961745077968330975, -121.3890666750452851 ) ) ;
#77686 = AXIS2_PLACEMENT_3D ( 'NONE', #248204, #189522, #254589 ) ;
#77687 = CARTESIAN_POINT ( 'NONE',  ( 23.14999999999999858, 71.00000000001260503, -191.1178414656112921 ) ) ;
#77688 = EDGE_CURVE ( 'NONE', #143019, #63983, #46807, .T. ) ;
#77689 = AXIS2_PLACEMENT_3D ( 'NONE', #152659, #232184, #14429 ) ;
#77690 = ORIENTED_EDGE ( 'NONE', *, *, #203192, .F. ) ;
#77691 = CARTESIAN_POINT ( 'NONE',  ( -20.85000000000000142, 7.021664781911246322, -171.3335654018973173 ) ) ;
#77692 = DIRECTION ( 'NONE',  ( -7.304098846218201720E-16, 1.000000000000000000, 0.000000000000000000 ) ) ;
#77693 = DIRECTION ( 'NONE',  ( 0.000000000000000000, -1.000000000000000000, 0.000000000000000000 ) ) ;
#77694 = ORIENTED_EDGE ( 'NONE', *, *, #20771, .T. ) ;
#77695 = CARTESIAN_POINT ( 'NONE',  ( -21.05000000000000071, 69.28189128378591022, -247.5258150475912089 ) ) ;
#77696 = ORIENTED_EDGE ( 'NONE', *, *, #236887, .T. ) ;
#77697 = LINE ( 'NONE', #161119, #177264 ) ;
#77698 = ORIENTED_EDGE ( 'NONE', *, *, #189081, .T. ) ;
#77699 = LINE ( 'NONE', #121986, #88685 ) ;
#77700 = DIRECTION ( 'NONE',  ( 0.000000000000000000, -0.2617529984164506107, -0.9651348961777299618 ) ) ;
#77701 = AXIS2_PLACEMENT_3D ( 'NONE', #120759, #256316, #136404 ) ;
#77703 = ORIENTED_EDGE ( 'NONE', *, *, #144210, .T. ) ;
#77702 = DIRECTION ( 'NONE',  ( 0.000000000000000000, 0.000000000000000000, -1.000000000000000000 ) ) ;
#77704 = ADVANCED_FACE ( 'NONE', ( #98568 ), #142663, .T. ) ;
#77705 = CARTESIAN_POINT ( 'NONE',  ( -18.41799967126726756, 8.841737187388694963, -245.4273995243829347 ) ) ;
#77706 = ORIENTED_EDGE ( 'NONE', *, *, #211308, .F. ) ;
#77707 = CARTESIAN_POINT ( 'NONE',  ( 20.94999999999999929, -8.730841121484166578, -157.9019252810156786 ) ) ;
#77708 = CARTESIAN_POINT ( 'NONE',  ( -20.94999999999999929, 77.85102823015347440, -191.8691942151018566 ) ) ;
#77709 = ORIENTED_EDGE ( 'NONE', *, *, #229436, .T. ) ;
#77711 = ORIENTED_EDGE ( 'NONE', *, *, #237052, .F. ) ;
#77710 = EDGE_CURVE ( 'NONE', #245973, #63115, #198999, .T. ) ;
#77712 = CARTESIAN_POINT ( 'NONE',  ( 20.94999999999999929, 10.39655183198267707, -207.4949966697317620 ) ) ;
#77713 = CARTESIAN_POINT ( 'NONE',  ( -13.39999999999994529, 64.35000000001120668, -21.02310748452479316 ) ) ;
#77714 = ORIENTED_EDGE ( 'NONE', *, *, #252726, .T. ) ;
#77715 = LINE ( 'NONE', #99834, #74186 ) ;
#77716 = AXIS2_PLACEMENT_3D ( 'NONE', #148760, #208739, #5352 ) ;
#77717 = AXIS2_PLACEMENT_3D ( 'NONE', #128494, #31984, #51489 ) ;
#77718 = VERTEX_POINT ( 'NONE', #196424 ) ;
#77719 = VERTEX_POINT ( 'NONE', #38647 ) ;
#77720 = DIRECTION ( 'NONE',  ( 0.000000000000000000, 0.000000000000000000, 1.000000000000000000 ) ) ;
#77721 = LINE ( 'NONE', #81558, #88909 ) ;
#77722 = EDGE_CURVE ( 'NONE', #226018, #83103, #176036, .T. ) ;
#77724 = EDGE_LOOP ( 'NONE', ( #137250, #44738, #192469 ) ) ;
#77723 = CARTESIAN_POINT ( 'NONE',  ( 18.49505832270841310, 85.43802806279482809, -95.82463430963039741 ) ) ;
#77725 = FACE_OUTER_BOUND ( 'NONE', #54701, .T. ) ;
#77726 = DIRECTION ( 'NONE',  ( 0.000000000000000000, 1.000000000000000000, 6.982962677686266711E-15 ) ) ;
#77727 = DIRECTION ( 'NONE',  ( -1.000000000000000000, 1.186688945009010077E-16, 8.286604613020808509E-31 ) ) ;
#77728 = CIRCLE ( 'NONE', #52794, 0.1000000000000043493 ) ;
#77730 = FACE_OUTER_BOUND ( 'NONE', #136338, .T. ) ;
#77729 = DIRECTION ( 'NONE',  ( -1.073024830501117725E-15, 6.982962677686266711E-15, -1.000000000000000000 ) ) ;
#77731 = DIRECTION ( 'NONE',  ( 0.000000000000000000, -0.6728971962617102953, -0.7397360091702507301 ) ) ;
#77732 = CARTESIAN_POINT ( 'NONE',  ( -20.94999999999999929, 1.115649653272650466E-11, -204.9999999999999716 ) ) ;
#77733 = AXIS2_PLACEMENT_3D ( 'NONE', #100268, #84530, #164132 ) ;
#77734 = TOROIDAL_SURFACE ( 'NONE', #40193, 0.9750000000000019762, 0.1000000000000000056 ) ;
#77735 = CARTESIAN_POINT ( 'NONE',  ( 20.04142135623730070, 11.65000000001115943, -91.65000000000004832 ) ) ;
#77736 = ADVANCED_FACE ( 'NONE', ( #77747 ), #200950, .T. ) ;
#77737 = CARTESIAN_POINT ( 'NONE',  ( 22.59999999999999432, 11.74987124438766273, -133.9345704089863318 ) ) ;
#77738 = ORIENTED_EDGE ( 'NONE', *, *, #235317, .T. ) ;
#77739 = ORIENTED_EDGE ( 'NONE', *, *, #133370, .F. ) ;
#77740 = CARTESIAN_POINT ( 'NONE',  ( 18.39999999999999858, 85.50000000001233502, -162.9910380878246201 ) ) ;
#77741 = VECTOR ( 'NONE', #173898, 1000.000000000000000 ) ;
#77743 = ORIENTED_EDGE ( 'NONE', *, *, #36139, .F. ) ;
#77742 = CARTESIAN_POINT ( 'NONE',  ( -23.15000000000000213, 78.98983215084128062, -228.7927651294584450 ) ) ;
#77744 = ORIENTED_EDGE ( 'NONE', *, *, #55442, .F. ) ;
#77745 = CYLINDRICAL_SURFACE ( 'NONE', #239324, 0.09999999999998898659 ) ;
#77746 = ORIENTED_EDGE ( 'NONE', *, *, #68173, .F. ) ;
#77747 = FACE_OUTER_BOUND ( 'NONE', #240138, .T. ) ;
#77748 = VERTEX_POINT ( 'NONE', #179455 ) ;
#77749 =( NAMED_UNIT ( * ) PLANE_ANGLE_UNIT ( ) SI_UNIT ( $, .RADIAN. ) );
#77750 = DIRECTION ( 'NONE',  ( 0.000000000000000000, 0.2617529984165034018, 0.9651348961777157509 ) ) ;
#77753 = ORIENTED_EDGE ( 'NONE', *, *, #28259, .T. ) ;
#77752 = ORIENTED_EDGE ( 'NONE', *, *, #98158, .T. ) ;
#77751 = CIRCLE ( 'NONE', #169412, 0.09999999999999939493 ) ;
#77754 = ORIENTED_EDGE ( 'NONE', *, *, #97075, .T. ) ;
#77755 = ORIENTED_EDGE ( 'NONE', *, *, #198498, .T. ) ;
#77756 = ORIENTED_EDGE ( 'NONE', *, *, #130486, .T. ) ;
#77757 = LINE ( 'NONE', #142856, #142066 ) ;
#77758 = CARTESIAN_POINT ( 'NONE',  ( -18.59999999999999787, -9.321008403361290107, -7.235938249077882745 ) ) ;
#77760 = VERTEX_POINT ( 'NONE', #19072 ) ;
#77759 = CARTESIAN_POINT ( 'NONE',  ( 18.59999999999999432, -1.162701749926853712, -142.1000000000000227 ) ) ;
#77761 = FACE_OUTER_BOUND ( 'NONE', #113116, .T. ) ;
#77762 = CARTESIAN_POINT ( 'NONE',  ( 15.75000000000000000, 12.65101141449787292, -215.1505311063240526 ) ) ;
#77764 = ORIENTED_EDGE ( 'NONE', *, *, #75926, .T. ) ;
#77763 = SPHERICAL_SURFACE ( 'NONE', #81055, 0.1000000000000000056 ) ;
#77765 = DIRECTION ( 'NONE',  ( 1.000000000000000000, -7.304098846218133681E-16, -2.111765289898285610E-31 ) ) ;
#77766 = ORIENTED_EDGE ( 'NONE', *, *, #63000, .F. ) ;
#77768 = CARTESIAN_POINT ( 'NONE',  ( -16.97683809663752186, 66.15000000001231228, -156.6207434663279230 ) ) ;
#77767 = VECTOR ( 'NONE', #226673, 1000.000000000000227 ) ;
#77770 = ORIENTED_EDGE ( 'NONE', *, *, #184829, .F. ) ;
#77769 = DIRECTION ( 'NONE',  ( 0.000000000000000000, -1.000000000000000000, -6.982962677686265922E-15 ) ) ;
#77771 = LINE ( 'NONE', #119498, #106102 ) ;
#77772 = CARTESIAN_POINT ( 'NONE',  ( 20.94999999999999929, 8.776282895303632259, -88.25000000000005684 ) ) ;
#77773 = EDGE_CURVE ( 'NONE', #8640, #147707, #760, .T. ) ;
#77774 = CARTESIAN_POINT ( 'NONE',  ( 21.05000000000000071, 11.75000000001116085, -60.15839931010296482 ) ) ;
#77775 = AXIS2_PLACEMENT_3D ( 'NONE', #232840, #235375, #77565 ) ;
#77776 = ORIENTED_EDGE ( 'NONE', *, *, #197140, .F. ) ;
#77778 = DIRECTION ( 'NONE',  ( 1.000000000000000000, -3.265361837132813093E-16, -2.280189983783949500E-30 ) ) ;
#77777 = CARTESIAN_POINT ( 'NONE',  ( -16.83558968593870375, 9.950000000011137047, -46.16230518761685175 ) ) ;
#77779 = SPHERICAL_SURFACE ( 'NONE', #24462, 0.1000000000000000056 ) ;
#77780 = DIRECTION ( 'NONE',  ( 1.000000000000000000, -7.304098846218135653E-16, 0.000000000000000000 ) ) ;
#77781 = CIRCLE ( 'NONE', #169427, 0.1000000000000096922 ) ;
#77782 = AXIS2_PLACEMENT_3D ( 'NONE', #155115, #138065, #61109 ) ;
#77783 = DIRECTION ( 'NONE',  ( 0.000000000000000000, 1.000000000000000000, 0.000000000000000000 ) ) ;
#77784 = CARTESIAN_POINT ( 'NONE',  ( -18.59999999999999787, -7.567701079425722455, -210.0537230116848662 ) ) ;
#77785 = ORIENTED_EDGE ( 'NONE', *, *, #5534, .F. ) ;
#77786 = ORIENTED_EDGE ( 'NONE', *, *, #171438, .T. ) ;
#77787 = VERTEX_POINT ( 'NONE', #239416 ) ;
#77788 =( GEOMETRIC_REPRESENTATION_CONTEXT ( 3 ) GLOBAL_UNCERTAINTY_ASSIGNED_CONTEXT ( ( #19261 ) ) GLOBAL_UNIT_ASSIGNED_CONTEXT ( ( #43242, #23709, #83606 ) ) REPRESENTATION_CONTEXT ( 'NONE', 'WORKASPACE' ) );
#77789 = LINE ( 'NONE', #157383, #38790 ) ;
#77790 = PLANE ( 'NONE',  #219146 ) ;
#77791 = VERTEX_POINT ( 'NONE', #60752 ) ;
#77792 = LINE ( 'NONE', #116940, #43471 ) ;
#77793 = VERTEX_POINT ( 'NONE', #135154 ) ;
#77794 = EDGE_CURVE ( 'NONE', #167344, #183460, #153053, .T. ) ;
#77795 = CARTESIAN_POINT ( 'NONE',  ( -22.50000000000000000, 36.65892442174472876, -249.5511627012454596 ) ) ;
#77796 = CARTESIAN_POINT ( 'NONE',  ( -18.59999999999999787, -1.835859311432481045, -145.5044391687985694 ) ) ;
#77797 = EDGE_CURVE ( 'NONE', #202163, #253241, #34385, .T. ) ;
#77798 = ORIENTED_EDGE ( 'NONE', *, *, #184198, .F. ) ;
#77799 = CARTESIAN_POINT ( 'NONE',  ( -21.00000000000000000, 6.238071963501339745, 11.95857864376269575 ) ) ;
#77801 = EDGE_CURVE ( 'NONE', #42984, #209120, #13682, .T. ) ;
#77800 = VECTOR ( 'NONE', #182781, 1000.000000000000114 ) ;
#77802 = VERTEX_POINT ( 'NONE', #52624 ) ;
#77803 = ORIENTED_EDGE ( 'NONE', *, *, #5849, .F. ) ;
#77804 = ORIENTED_EDGE ( 'NONE', *, *, #254807, .F. ) ;
#77805 = ADVANCED_FACE ( 'NONE', ( #171349 ), #95606, .T. ) ;
#77807 = LINE ( 'NONE', #192650, #216874 ) ;
#77806 = AXIS2_PLACEMENT_3D ( 'NONE', #49911, #190747, #231150 ) ;
#77808 = CARTESIAN_POINT ( 'NONE',  ( -21.05000000000000071, 6.540656951712397138, -134.1000000000000227 ) ) ;
#77809 = CARTESIAN_POINT ( 'NONE',  ( -21.14250536705909411, 1.115548662937858831E-11, -127.4818278231192608 ) ) ;
#77811 = ADVANCED_FACE ( 'NONE', ( #154352 ), #175198, .T. ) ;
#77810 = DIRECTION ( 'NONE',  ( 0.000000000000000000, 1.265107689135680095E-16, -1.000000000000000000 ) ) ;
#77812 = AXIS2_PLACEMENT_3D ( 'NONE', #30217, #210140, #126734 ) ;
#77813 = CARTESIAN_POINT ( 'NONE',  ( 13.43663047529820709, 66.55335465531679517, -118.1123010284241985 ) ) ;
#77815 = DIRECTION ( 'NONE',  ( 0.000000000000000000, 0.1350103645451945777, -0.9908441862701591329 ) ) ;
#77814 = CARTESIAN_POINT ( 'NONE',  ( -23.15000000000000213, 61.88149656937975607, -248.1136133839584090 ) ) ;
#77816 = DIRECTION ( 'NONE',  ( 0.000000000000000000, 0.000000000000000000, -1.000000000000000000 ) ) ;
#77818 = ORIENTED_EDGE ( 'NONE', *, *, #112714, .F. ) ;
#77817 = DIRECTION ( 'NONE',  ( 0.000000000000000000, 0.000000000000000000, 1.000000000000000000 ) ) ;
#77819 = CARTESIAN_POINT ( 'NONE',  ( -16.87845715379269507, 9.957858113908168107, -79.62380065105894289 ) ) ;
#77820 = ORIENTED_EDGE ( 'NONE', *, *, #80395, .T. ) ;
#77821 = EDGE_CURVE ( 'NONE', #147420, #142551, #151071, .T. ) ;
#77822 = CARTESIAN_POINT ( 'NONE',  ( -21.59142135623730852, 7.850000000011158718, -121.6500000000000341 ) ) ;
#77823 = AXIS2_PLACEMENT_3D ( 'NONE', #220819, #77435, #42199 ) ;
#77824 = EDGE_LOOP ( 'NONE', ( #30469, #110810, #77110, #117977 ) ) ;
#77825 = ORIENTED_EDGE ( 'NONE', *, *, #134465, .T. ) ;
#77826 = LINE ( 'NONE', #42555, #237750 ) ;
#77827 = CYLINDRICAL_SURFACE ( 'NONE', #68700, 12.87499999999999467 ) ;
#77828 = CARTESIAN_POINT ( 'NONE',  ( 18.39999999999999503, 14.17280543801757986, -210.8598471598932349 ) ) ;
#77829 = ORIENTED_EDGE ( 'NONE', *, *, #237762, .F. ) ;
#77830 = EDGE_CURVE ( 'NONE', #86874, #165955, #211726, .T. ) ;
#77831 = VECTOR ( 'NONE', #169874, 1000.000000000000000 ) ;
#77832 = LINE ( 'NONE', #40038, #255119 ) ;
#77834 = VERTEX_POINT ( 'NONE', #252107 ) ;
#77833 = VECTOR ( 'NONE', #132039, 1000.000000000000000 ) ;
#77835 = VERTEX_POINT ( 'NONE', #253396 ) ;
#77836 = TOROIDAL_SURFACE ( 'NONE', #69494, 0.6000000000000013101, 0.1000000000000000056 ) ;
#77837 = CARTESIAN_POINT ( 'NONE',  ( 23.14999999999999503, 6.650000000011155876, -88.15000000000004832 ) ) ;
#77838 = EDGE_LOOP ( 'NONE', ( #212345, #139945, #221126, #195340 ) ) ;
#77839 = CARTESIAN_POINT ( 'NONE',  ( -20.64999999999999858, -8.999999999988846255, -177.3939691226524076 ) ) ;
#77840 = CARTESIAN_POINT ( 'NONE',  ( -18.59999999999999787, 9.350000000011156942, -88.15000000000004832 ) ) ;
#77841 = VERTEX_POINT ( 'NONE', #51313 ) ;
#77842 = EDGE_CURVE ( 'NONE', #208794, #156714, #150466, .T. ) ;
#77843 = LINE ( 'NONE', #154853, #65450 ) ;
#77844 = CARTESIAN_POINT ( 'NONE',  ( -16.85312964099708211, 9.913604682078867469, -121.1028157064304622 ) ) ;
#77845 = PLANE ( 'NONE',  #5299 ) ;
#77846 = ORIENTED_EDGE ( 'NONE', *, *, #58529, .T. ) ;
#77847 = ADVANCED_FACE ( 'NONE', ( #254648 ), #55161, .F. ) ;
#77848 = CARTESIAN_POINT ( 'NONE',  ( 23.14999999999999503, 28.86532135423329493, -237.9457867389574517 ) ) ;
#77849 = FACE_OUTER_BOUND ( 'NONE', #35838, .T. ) ;
#77850 = AXIS2_PLACEMENT_3D ( 'NONE', #14927, #94439, #174030 ) ;
#77851 = CARTESIAN_POINT ( 'NONE',  ( -20.94999999999999929, 57.72708596674832648, -226.0092949359174952 ) ) ;
#77852 = ORIENTED_EDGE ( 'NONE', *, *, #229143, .F. ) ;
#77853 = EDGE_CURVE ( 'NONE', #150964, #78372, #192768, .T. ) ;
#77854 = LINE ( 'NONE', #81678, #4405 ) ;
#77855 = ORIENTED_EDGE ( 'NONE', *, *, #234159, .T. ) ;
#77856 = DIRECTION ( 'NONE',  ( 1.000000000000000000, 0.000000000000000000, 0.000000000000000000 ) ) ;
#77857 = CARTESIAN_POINT ( 'NONE',  ( 18.59999999999999432, 77.26178616857662007, -61.43660852097883662 ) ) ;
#77859 = CIRCLE ( 'NONE', #119590, 0.1000000000000028644 ) ;
#77858 = FACE_OUTER_BOUND ( 'NONE', #185712, .T. ) ;
#77860 = CARTESIAN_POINT ( 'NONE',  ( -20.54999999999999716, 61.88149656937975607, -248.1136133839584090 ) ) ;
#77861 = DIRECTION ( 'NONE',  ( 1.224646799147353207E-16, 1.000000000000000000, 0.000000000000000000 ) ) ;
#77863 = ORIENTED_EDGE ( 'NONE', *, *, #110570, .T. ) ;
#77862 = AXIS2_PLACEMENT_3D ( 'NONE', #249341, #9417, #29037 ) ;
#77864 = LINE ( 'NONE', #75348, #930 ) ;
#77865 = CARTESIAN_POINT ( 'NONE',  ( 21.05281448260627641, 67.22398984147443457, -124.3495495727129310 ) ) ;
#77866 = AXIS2_PLACEMENT_3D ( 'NONE', #183984, #202270, #160603 ) ;
#77867 = AXIS2_PLACEMENT_3D ( 'NONE', #226618, #224053, #8874 ) ;
#77868 = CARTESIAN_POINT ( 'NONE',  ( -22.59999970745345976, -0.009356377326984025716, 11.75051320766921314 ) ) ;
#77869 = CARTESIAN_POINT ( 'NONE',  ( -18.79999999999999716, 11.61130914238355771, 22.00000000000000355 ) ) ;
#77870 = DIRECTION ( 'NONE',  ( -0.000000000000000000, 1.000000000000000000, 6.982962677686266711E-15 ) ) ;
#77871 = AXIS2_PLACEMENT_3D ( 'NONE', #121097, #215024, #80626 ) ;
#77872 = EDGE_CURVE ( 'NONE', #154991, #67305, #213400, .T. ) ;
#77873 = ORIENTED_EDGE ( 'NONE', *, *, #19103, .T. ) ;
#77874 = ORIENTED_EDGE ( 'NONE', *, *, #150998, .F. ) ;
#77875 = DIRECTION ( 'NONE',  ( -1.000000000000000000, 0.000000000000000000, 0.000000000000000000 ) ) ;
#77876 = DIRECTION ( 'NONE',  ( 0.000000000000000000, -0.8814952561688430555, 0.4721928772777346239 ) ) ;
#77877 = LINE ( 'NONE', #177025, #147665 ) ;
#77878 = FACE_OUTER_BOUND ( 'NONE', #85668, .T. ) ;
#77879 = CARTESIAN_POINT ( 'NONE',  ( -20.64999999999999858, 67.23127455305841238, -235.8551265064783991 ) ) ;
#77880 = EDGE_CURVE ( 'NONE', #182621, #146084, #192573, .T. ) ;
#77881 = ORIENTED_EDGE ( 'NONE', *, *, #240250, .F. ) ;
#77882 = DIRECTION ( 'NONE',  ( 1.000000000000000000, -2.849773892568378313E-16, 7.728835255496647986E-17 ) ) ;
#77883 = AXIS2_PLACEMENT_3D ( 'NONE', #4944, #122368, #158949 ) ;
#77884 = CARTESIAN_POINT ( 'NONE',  ( 21.00000000000000000, -1.212568896937008089, -7.800000000000000711 ) ) ;
#77885 = CIRCLE ( 'NONE', #82153, 0.1999999999999987899 ) ;
#77886 = EDGE_CURVE ( 'NONE', #97681, #126765, #33117, .T. ) ;
#77887 = ORIENTED_EDGE ( 'NONE', *, *, #7434, .T. ) ;
#77889 = EDGE_CURVE ( 'NONE', #247436, #139556, #38632, .T. ) ;
#77888 = DIRECTION ( 'NONE',  ( 1.000000000000000000, 0.000000000000000000, 0.000000000000000000 ) ) ;
#77890 = DIRECTION ( 'NONE',  ( 1.000000000000000000, 0.000000000000000000, 0.000000000000000000 ) ) ;
#77891 = EDGE_CURVE ( 'NONE', #222832, #230693, #246726, .T. ) ;
#77892 = AXIS2_PLACEMENT_3D ( 'NONE', #158453, #1894, #64469 ) ;
#77893 = ORIENTED_EDGE ( 'NONE', *, *, #69771, .F. ) ;
#77894 = FACE_OUTER_BOUND ( 'NONE', #174702, .T. ) ;
#77895 = EDGE_CURVE ( 'NONE', #28626, #19454, #193444, .T. ) ;
#77896 = ORIENTED_EDGE ( 'NONE', *, *, #206162, .T. ) ;
#77897 = CARTESIAN_POINT ( 'NONE',  ( -21.07928932188134397, 75.90110485435729970, -75.85162414091763594 ) ) ;
#77898 = DIRECTION ( 'NONE',  ( -0.000000000000000000, 1.000000000000000000, -0.000000000000000000 ) ) ;
#77899 = CARTESIAN_POINT ( 'NONE',  ( -21.05000000000000071, 87.29603075034795268, -200.4752083248604038 ) ) ;
#77900 = CARTESIAN_POINT ( 'NONE',  ( 23.14999999999999503, 6.650000000011155876, -121.8500000000000369 ) ) ;
#77901 = DIRECTION ( 'NONE',  ( 1.000000000000000000, 0.000000000000000000, 0.000000000000000000 ) ) ;
#77902 = CARTESIAN_POINT ( 'NONE',  ( -20.64999999999999858, 4.350000000011156054, -88.25000000000005684 ) ) ;
#77903 = DIRECTION ( 'NONE',  ( 1.000000000000000000, 0.000000000000000000, 0.000000000000000000 ) ) ;
#77904 = CARTESIAN_POINT ( 'NONE',  ( 23.15000000000000213, 85.60000000001177511, -79.41707660717668205 ) ) ;
#77905 = DIRECTION ( 'NONE',  ( -0.000000000000000000, -6.982962677686266711E-15, 1.000000000000000000 ) ) ;
#77906 = CARTESIAN_POINT ( 'NONE',  ( -20.94999999999999929, -1.835341550213255957, -45.05515129256298223 ) ) ;
#77907 = CARTESIAN_POINT ( 'NONE',  ( -23.25000000000000000, 76.00000000001213607, -138.6231074845243256 ) ) ;
#77908 = DIRECTION ( 'NONE',  ( 1.000000000000000000, 0.000000000000000000, 0.000000000000000000 ) ) ;
#77909 = CARTESIAN_POINT ( 'NONE',  ( 18.57399277249656322, 10.33112638556969820, -206.5901228926974227 ) ) ;
#77910 = TOROIDAL_SURFACE ( 'NONE', #77716, 11.65000000000000036, 0.1000000000000000056 ) ;
#77911 = AXIS2_PLACEMENT_3D ( 'NONE', #78471, #253257, #237568 ) ;
#77912 = TOROIDAL_SURFACE ( 'NONE', #186276, 0.4000000000000010214, 0.1000000000000000056 ) ;
#77913 = AXIS2_PLACEMENT_3D ( 'NONE', #175354, #101870, #181454 ) ;
#77914 = CARTESIAN_POINT ( 'NONE',  ( -21.55000000000000071, 7.250000000011155521, -146.3500000000000227 ) ) ;
#77915 = FACE_OUTER_BOUND ( 'NONE', #220858, .T. ) ;
#77916 = EDGE_CURVE ( 'NONE', #186334, #151382, #225853, .T. ) ;
#77917 = ORIENTED_EDGE ( 'NONE', *, *, #21529, .F. ) ;
#77918 = DIRECTION ( 'NONE',  ( 1.000000000000000000, -0.000000000000000000, -0.000000000000000000 ) ) ;
#77919 = CARTESIAN_POINT ( 'NONE',  ( -21.65000000000000213, 7.708578643773852157, -79.35000000000005116 ) ) ;
#77920 = DIRECTION ( 'NONE',  ( 1.000000000000000000, 0.000000000000000000, 0.000000000000000000 ) ) ;
#77921 = EDGE_CURVE ( 'NONE', #147057, #150331, #194737, .T. ) ;
#77922 = EDGE_CURVE ( 'NONE', #196436, #14418, #250990, .T. ) ;
#77923 = ORIENTED_EDGE ( 'NONE', *, *, #112149, .F. ) ;
#77924 = DIRECTION ( 'NONE',  ( 0.000000000000000000, 0.000000000000000000, 1.000000000000000000 ) ) ;
#77925 = CARTESIAN_POINT ( 'NONE',  ( -18.59999999999999787, 68.75000000001151079, -48.17310748452437252 ) ) ;
#77926 = ORIENTED_EDGE ( 'NONE', *, *, #114824, .F. ) ;
#77927 = AXIS2_PLACEMENT_3D ( 'NONE', #129301, #128025, #45908 ) ;
#77928 = DIRECTION ( 'NONE',  ( 0.000000000000000000, -6.517943393102682774E-15, 1.000000000000000000 ) ) ;
#77929 = LINE ( 'NONE', #135331, #118407 ) ;
#77930 = CIRCLE ( 'NONE', #56500, 0.3999999999999975797 ) ;
#77931 = AXIS2_PLACEMENT_3D ( 'NONE', #91675, #9564, #70861 ) ;
#77932 = ORIENTED_EDGE ( 'NONE', *, *, #237723, .F. ) ;
#77933 = B_SPLINE_CURVE_WITH_KNOTS ( 'NONE', 3,
 ( #224512, #84972, #164558, #66736, #146251, #47136, #126703, #206242, #107130, #186693, #8051, #127994, #30191, #232244, #173588, #48439, #112289, #251781, #53587 ),
 .UNSPECIFIED., .F., .F.,
 ( 4, 3, 3, 3, 3, 3, 4 ),
 ( -2.000416914663624153E-06, 0.000000000000000000, 4.714008503746000344E-05, 9.979203887777331108E-05, 0.0001372215519229483770, 0.0001635031576220943145, 0.0001900083748504093127 ),
 .UNSPECIFIED. ) ;
#77934 = VERTEX_POINT ( 'NONE', #121621 ) ;
#77935 = CARTESIAN_POINT ( 'NONE',  ( -18.59999999999999787, 67.85125148167622910, -227.9794913823769491 ) ) ;
#77936 = ORIENTED_EDGE ( 'NONE', *, *, #256977, .T. ) ;
#77937 = CARTESIAN_POINT ( 'NONE',  ( 21.05000000000000071, -0.1000000000000011297, 6.540656951701244282 ) ) ;
#77938 = CARTESIAN_POINT ( 'NONE',  ( 20.09999999999999787, 9.750000000011137757, -176.7499999999999716 ) ) ;
#77939 = DIRECTION ( 'NONE',  ( 1.000000000000000000, 0.000000000000000000, 0.000000000000000000 ) ) ;
#77940 = DIRECTION ( 'NONE',  ( 2.259780016855445309E-14, -0.9118278131605127568, 0.4105728183244933271 ) ) ;
#77941 = EDGE_CURVE ( 'NONE', #96681, #37986, #71964, .T. ) ;
#77942 = DIRECTION ( 'NONE',  ( -0.000000000000000000, -6.982962677686266711E-15, 1.000000000000000000 ) ) ;
#77943 = DIRECTION ( 'NONE',  ( 1.000000000000000000, 0.000000000000000000, 0.000000000000000000 ) ) ;
#77944 = LINE ( 'NONE', #115806, #83053 ) ;
#77946 = ORIENTED_EDGE ( 'NONE', *, *, #202893, .F. ) ;
#77945 = CARTESIAN_POINT ( 'NONE',  ( 20.94999999999999574, 77.85102823015273543, -91.36919421510179973 ) ) ;
#77947 = VERTEX_POINT ( 'NONE', #158199 ) ;
#77948 = CARTESIAN_POINT ( 'NONE',  ( -20.64999999999999858, 2.500000000011156409, -113.7246219227621395 ) ) ;
#77950 = ORIENTED_EDGE ( 'NONE', *, *, #91517, .T. ) ;
#77949 = DIRECTION ( 'NONE',  ( 0.000000000000000000, 0.000000000000000000, -1.000000000000000000 ) ) ;
#77951 = PRESENTATION_LAYER_ASSIGNMENT (  '', '', ( #232112 ) ) ;
#77952 = ORIENTED_EDGE ( 'NONE', *, *, #99074, .F. ) ;
#77953 = CARTESIAN_POINT ( 'NONE',  ( -16.93301857435208291, 66.02369064527677267, -149.1373319133629423 ) ) ;
#77954 = DIRECTION ( 'NONE',  ( -0.000000000000000000, -0.000000000000000000, 1.000000000000000000 ) ) ;
#77955 = DIRECTION ( 'NONE',  ( -1.000000000000000000, 0.000000000000000000, 0.000000000000000000 ) ) ;
#77956 = CARTESIAN_POINT ( 'NONE',  ( 18.49999999999998579, -9.321008403361311423, -7.235938249077851658 ) ) ;
#77957 = CARTESIAN_POINT ( 'NONE',  ( -23.25000000000000000, 15.92646454033039660, -219.3818586450342423 ) ) ;
#77959 = DIRECTION ( 'NONE',  ( 0.000000000000000000, 0.9994937237965558774, 0.03181660087586650476 ) ) ;
#77958 = CIRCLE ( 'NONE', #219611, 0.1000000000000024342 ) ;
#77960 = DIRECTION ( 'NONE',  ( -0.000000000000000000, 1.000000000000000000, 6.982962677686266711E-15 ) ) ;
#77961 = EDGE_CURVE ( 'NONE', #132923, #88201, #113461, .T. ) ;
#77962 = DIRECTION ( 'NONE',  ( 0.000000000000000000, -6.982962677686266711E-15, 1.000000000000000000 ) ) ;
#77963 = ORIENTED_EDGE ( 'NONE', *, *, #160054, .T. ) ;
#77964 = EDGE_LOOP ( 'NONE', ( #233215, #198143, #43546, #133794 ) ) ;
#77965 = EDGE_CURVE ( 'NONE', #74054, #20388, #163536, .T. ) ;
#77966 = LINE ( 'NONE', #115827, #156209 ) ;
#77967 = VECTOR ( 'NONE', #27019, 1000.000000000000114 ) ;
#77968 = AXIS2_PLACEMENT_3D ( 'NONE', #255094, #154799, #55627 ) ;
#77969 = ORIENTED_EDGE ( 'NONE', *, *, #74544, .F. ) ;
#77970 = CARTESIAN_POINT ( 'NONE',  ( -20.54999999999999716, 74.00000000001199396, -116.2477294072864140 ) ) ;
#77971 = ORIENTED_EDGE ( 'NONE', *, *, #207808, .T. ) ;
#77972 = DIRECTION ( 'NONE',  ( -1.000000000000000000, -0.000000000000000000, -0.000000000000000000 ) ) ;
#77973 = CARTESIAN_POINT ( 'NONE',  ( -20.05000000000000426, 66.75000000001253397, -182.2731074845244166 ) ) ;
#77974 = ADVANCED_FACE ( 'NONE', ( #197275 ), #199867, .T. ) ;
#77976 = EDGE_CURVE ( 'NONE', #72158, #256994, #126095, .T. ) ;
#77975 = AXIS2_PLACEMENT_3D ( 'NONE', #246151, #162777, #226559 ) ;
#77977 = CARTESIAN_POINT ( 'NONE',  ( -15.31895204843005942, 49.15836891943285281, -233.6552066833103538 ) ) ;
#77978 = CARTESIAN_POINT ( 'NONE',  ( -18.40000000000000213, 43.39957528361355799, -233.6562381667159798 ) ) ;
#77979 = TOROIDAL_SURFACE ( 'NONE', #111328, 11.70000000000000107, 0.1000000000000000056 ) ;
#77981 = ORIENTED_EDGE ( 'NONE', *, *, #250232, .T. ) ;
#77980 = LINE ( 'NONE', #57119, #185608 ) ;
#77982 = DIRECTION ( 'NONE',  ( 0.000000000000000000, 0.000000000000000000, 1.000000000000000000 ) ) ;
#77983 = ORIENTED_EDGE ( 'NONE', *, *, #39573, .F. ) ;
#77984 = DIRECTION ( 'NONE',  ( 0.000000000000000000, 0.000000000000000000, 1.000000000000000000 ) ) ;
#77985 = CARTESIAN_POINT ( 'NONE',  ( -18.52328366898032996, 85.64232108905262919, -29.30828814695420803 ) ) ;
#77986 = DIRECTION ( 'NONE',  ( 0.000000000000000000, 0.000000000000000000, 1.000000000000000000 ) ) ;
#77987 = CARTESIAN_POINT ( 'NONE',  ( 23.15000000000000213, 11.60058429089262333, -246.3380203656811887 ) ) ;
#77988 = DIRECTION ( 'NONE',  ( -2.840903330521632269E-16, -0.8700118002898356018, 0.4930308989875170078 ) ) ;
#77989 = VERTEX_POINT ( 'NONE', #237693 ) ;
#77990 = CARTESIAN_POINT ( 'NONE',  ( -18.40904629823849348, 85.50000000001138289, -29.42291792204254364 ) ) ;
#77991 = AXIS2_PLACEMENT_3D ( 'NONE', #230902, #130483, #67950 ) ;
#77992 = EDGE_LOOP ( 'NONE', ( #57827, #99566, #127818, #24814 ) ) ;
#77995 = ORIENTED_EDGE ( 'NONE', *, *, #121036, .T. ) ;
#77994 = CARTESIAN_POINT ( 'NONE',  ( 21.14999999999999503, -0.09999999998884338825, -88.85042919245522341 ) ) ;
#77993 = DIRECTION ( 'NONE',  ( 1.000000000000000000, -0.000000000000000000, -0.000000000000000000 ) ) ;
#77996 = ADVANCED_FACE ( 'NONE', ( #236402 ), #57752, .F. ) ;
#77997 = CARTESIAN_POINT ( 'NONE',  ( 18.59999999999999076, 14.05000000000000959, -5.513695070760984862 ) ) ;
#77999 = EDGE_CURVE ( 'NONE', #22816, #120125, #19943, .T. ) ;
#77998 = AXIS2_PLACEMENT_3D ( 'NONE', #161124, #198945, #81540 ) ;
#78000 = AXIS2_PLACEMENT_3D ( 'NONE', #26150, #108248, #226898 ) ;
#78001 = CARTESIAN_POINT ( 'NONE',  ( -21.10000000000000142, 0.000000000000000000, 0.000000000000000000 ) ) ;
#78002 = EDGE_LOOP ( 'NONE', ( #142090, #162282, #81557 ) ) ;
#78003 = CARTESIAN_POINT ( 'NONE',  ( 18.44206774312965180, 85.49102735755222682, -129.8968799798263092 ) ) ;
#78004 = CIRCLE ( 'NONE', #161424, 0.5000000000000004441 ) ;
#78005 = DIRECTION ( 'NONE',  ( 1.000000000000000000, 0.000000000000000000, 0.000000000000000000 ) ) ;
#78006 = AXIS2_PLACEMENT_3D ( 'NONE', #243502, #119725, #203091 ) ;
#78007 = DIRECTION ( 'NONE',  ( 0.000000000000000000, -1.756682000989170847E-15, 1.000000000000000000 ) ) ;
#78009 = VERTEX_POINT ( 'NONE', #138556 ) ;
#78008 = DIRECTION ( 'NONE',  ( 0.000000000000000000, 1.953992523340277404E-14, 1.000000000000000000 ) ) ;
#78010 = CARTESIAN_POINT ( 'NONE',  ( -21.59142135623730852, 7.850000000011158718, -146.2500000000000284 ) ) ;
#78011 = EDGE_CURVE ( 'NONE', #229125, #124002, #992, .T. ) ;
#78012 = VERTEX_POINT ( 'NONE', #160752 ) ;
#78014 = EDGE_CURVE ( 'NONE', #23243, #202405, #117738, .T. ) ;
#78013 = DIRECTION ( 'NONE',  ( -3.265361837132813093E-16, 1.000000000000000000, 0.000000000000000000 ) ) ;
#78015 = CARTESIAN_POINT ( 'NONE',  ( 18.54147908293611735, -9.463261657916946845, -74.04894889675584579 ) ) ;
#78016 = PLANE ( 'NONE',  #42142 ) ;
#78017 = VECTOR ( 'NONE', #31335, 1000.000000000000000 ) ;
#78018 = ORIENTED_EDGE ( 'NONE', *, *, #188128, .T. ) ;
#78019 = DIRECTION ( 'NONE',  ( 1.000000000000000000, -0.000000000000000000, 0.000000000000000000 ) ) ;
#78021 = ORIENTED_EDGE ( 'NONE', *, *, #18501, .T. ) ;
#78020 = CIRCLE ( 'NONE', #44722, 0.09999999999999609201 ) ;
#78023 = AXIS2_PLACEMENT_3D ( 'NONE', #182421, #19488, #121183 ) ;
#78022 = CARTESIAN_POINT ( 'NONE',  ( 18.59999999999999076, 10.20857864377385127, -188.8499999999999659 ) ) ;
#78024 = ORIENTED_EDGE ( 'NONE', *, *, #203262, .F. ) ;
#78025 = ADVANCED_FACE ( 'NONE', ( #255912 ), #18642, .T. ) ;
#78026 = DIRECTION ( 'NONE',  ( 0.000000000000000000, 7.116814260417668513E-15, -1.000000000000000000 ) ) ;
#78027 = FACE_OUTER_BOUND ( 'NONE', #213251, .T. ) ;
#78028 = VECTOR ( 'NONE', #152883, 1000.000000000000114 ) ;
#78029 = DIRECTION ( 'NONE',  ( -0.000000000000000000, 1.000000000000000000, 1.734723475976807292E-15 ) ) ;
#78030 = CIRCLE ( 'NONE', #19808, 0.5000000000000008882 ) ;
#78031 = EDGE_LOOP ( 'NONE', ( #22282, #103853, #124402, #244717 ) ) ;
#78032 = EDGE_CURVE ( 'NONE', #11174, #41773, #240270, .T. ) ;
#78033 = DIRECTION ( 'NONE',  ( 0.000000000000000000, 0.000000000000000000, 1.000000000000000000 ) ) ;
#78034 = DIRECTION ( 'NONE',  ( 0.000000000000000000, 0.000000000000000000, -1.000000000000000000 ) ) ;
#78035 = CARTESIAN_POINT ( 'NONE',  ( 23.15000000000000213, 85.60000000001188880, -93.12913836187179584 ) ) ;
#78036 = ORIENTED_EDGE ( 'NONE', *, *, #164378, .T. ) ;
#78037 = DIRECTION ( 'NONE',  ( 1.000000000000000000, -0.000000000000000000, -0.000000000000000000 ) ) ;
#78038 = EDGE_LOOP ( 'NONE', ( #142468, #241221, #95005, #67271 ) ) ;
#78040 = ORIENTED_EDGE ( 'NONE', *, *, #195890, .T. ) ;
#78039 = DIRECTION ( 'NONE',  ( 1.000000000000000000, 0.000000000000000000, 0.000000000000000000 ) ) ;
#78041 = ADVANCED_FACE ( 'NONE', ( #201125 ), #177745, .T. ) ;
#78042 = CIRCLE ( 'NONE', #219696, 11.70000000000001528 ) ;
#78045 = ORIENTED_EDGE ( 'NONE', *, *, #140638, .T. ) ;
#78044 = ORIENTED_EDGE ( 'NONE', *, *, #249589, .T. ) ;
#78043 = CARTESIAN_POINT ( 'NONE',  ( -21.07933241753356413, 0.09337959041926464920, 6.328645948379739039 ) ) ;
#78046 = CARTESIAN_POINT ( 'NONE',  ( 21.05000000000036309, 65.39167043205783614, -95.43142247122897004 ) ) ;
#78047 = AXIS2_PLACEMENT_3D ( 'NONE', #139394, #1167, #218944 ) ;
#78048 = DIRECTION ( 'NONE',  ( 1.000000000000000000, 0.000000000000000000, 0.000000000000000000 ) ) ;
#78049 = CIRCLE ( 'NONE', #211350, 0.09999999999999939493 ) ;
#78050 = DIRECTION ( 'NONE',  ( 1.000000000000000000, -1.186688945009010077E-16, -8.286604613020808509E-31 ) ) ;
#78051 = DIRECTION ( 'NONE',  ( 1.000000000000000000, -0.000000000000000000, -0.000000000000000000 ) ) ;
#78052 = SPHERICAL_SURFACE ( 'NONE', #61687, 0.1000000000000000056 ) ;
#78053 = CARTESIAN_POINT ( 'NONE',  ( 21.05000000000000071, 65.27628318601635726, -195.9287082486404756 ) ) ;
#78054 = CIRCLE ( 'NONE', #198862, 0.1000000000000028644 ) ;
#78055 = CARTESIAN_POINT ( 'NONE',  ( -20.94999999999999929, -11.48912529306490349, -36.60000000000000142 ) ) ;
#78057 = DIRECTION ( 'NONE',  ( 0.000000000000000000, -1.000000000000000000, -6.982962677686267499E-15 ) ) ;
#78056 = DIRECTION ( 'NONE',  ( -1.836970198721029934E-16, 1.000000000000000000, 0.000000000000000000 ) ) ;
#78058 = VERTEX_POINT ( 'NONE', #78602 ) ;
#78059 = ORIENTED_EDGE ( 'NONE', *, *, #7, .T. ) ;
#78060 = ORIENTED_EDGE ( 'NONE', *, *, #204960, .F. ) ;
#78061 = DIRECTION ( 'NONE',  ( 1.000000000000000000, -0.000000000000000000, 0.000000000000000000 ) ) ;
#78063 = ORIENTED_EDGE ( 'NONE', *, *, #46487, .F. ) ;
#78062 = DIRECTION ( 'NONE',  ( -1.000000000000000000, 1.836970198721029934E-16, 1.282749433769087757E-30 ) ) ;
#78064 = CARTESIAN_POINT ( 'NONE',  ( 18.39999999999999503, 5.650000000011139001, -154.8500000000000227 ) ) ;
#78065 = VERTEX_POINT ( 'NONE', #196011 ) ;
#78066 = DIRECTION ( 'NONE',  ( 1.000000000000000000, 0.000000000000000000, -0.000000000000000000 ) ) ;
#78067 = EDGE_LOOP ( 'NONE', ( #21166, #186241, #1721 ) ) ;
#78068 = DIRECTION ( 'NONE',  ( 1.000000000000000000, 0.000000000000000000, 0.000000000000000000 ) ) ;
#78069 = ORIENTED_EDGE ( 'NONE', *, *, #43363, .F. ) ;
#78070 = B_SPLINE_CURVE_WITH_KNOTS ( 'NONE', 3,
 ( #82850, #97275, #77737, #99854 ),
 .UNSPECIFIED., .F., .F.,
 ( 4, 4 ),
 ( 3.469446951953614189E-18, 0.0001058379652594581074 ),
 .UNSPECIFIED. ) ;
#78071 = DIRECTION ( 'NONE',  ( 0.000000000000000000, 0.000000000000000000, 1.000000000000000000 ) ) ;
#78072 = CARTESIAN_POINT ( 'NONE',  ( 18.57071067811864040, 30.75534497283957691, -234.8410239939103406 ) ) ;
#78073 = AXIS2_PLACEMENT_3D ( 'NONE', #30189, #126702, #9317 ) ;
#78075 = ORIENTED_EDGE ( 'NONE', *, *, #130394, .F. ) ;
#78074 = ORIENTED_EDGE ( 'NONE', *, *, #3426, .T. ) ;
#78076 = ORIENTED_EDGE ( 'NONE', *, *, #204702, .T. ) ;
#78077 = DIRECTION ( 'NONE',  ( -0.000000000000000000, 0.9770955615653313941, 0.2128009952263603954 ) ) ;
#78078 = VERTEX_POINT ( 'NONE', #42078 ) ;
#78079 = EDGE_LOOP ( 'NONE', ( #4174, #197991, #162462, #77468 ) ) ;
#78080 = DIRECTION ( 'NONE',  ( 1.000000000000000000, -0.000000000000000000, -0.000000000000000000 ) ) ;
#78082 = ORIENTED_EDGE ( 'NONE', *, *, #172499, .T. ) ;
#78081 = FACE_OUTER_BOUND ( 'NONE', #253091, .T. ) ;
#78083 = CARTESIAN_POINT ( 'NONE',  ( -16.97683809663752186, 66.15000000001201386, -116.4254715027206828 ) ) ;
#78084 = LINE ( 'NONE', #158948, #224046 ) ;
#78085 = CARTESIAN_POINT ( 'NONE',  ( 23.24999999999999289, 64.35000000001218723, -143.5379132551783812 ) ) ;
#78086 = CARTESIAN_POINT ( 'NONE',  ( 21.05000000000000071, -8.999999999988842703, -90.60603087734760663 ) ) ;
#78087 = ORIENTED_EDGE ( 'NONE', *, *, #237819, .F. ) ;
#78088 = ORIENTED_EDGE ( 'NONE', *, *, #121032, .F. ) ;
#78089 = CARTESIAN_POINT ( 'NONE',  ( 21.05000000000000071, -11.48912529306489994, -198.0999999999999659 ) ) ;
#78090 = DIRECTION ( 'NONE',  ( 0.000000000000000000, -0.2128009952263603677, 0.9770955615653313941 ) ) ;
#78091 = CARTESIAN_POINT ( 'NONE',  ( -20.94999999999999929, 88.41227409416161720, -106.0231074845242176 ) ) ;
#78092 = ADVANCED_FACE ( 'NONE', ( #241538 ), #38829, .T. ) ;
#78093 = ORIENTED_EDGE ( 'NONE', *, *, #130000, .T. ) ;
#78094 = CIRCLE ( 'NONE', #19674, 0.6000000000000033085 ) ;
#78095 = AXIS2_PLACEMENT_3D ( 'NONE', #216070, #119571, #180816 ) ;
#78096 = DIRECTION ( 'NONE',  ( -0.000000000000000000, -1.897661533703519897E-16, 1.000000000000000000 ) ) ;
#78097 = CIRCLE ( 'NONE', #223831, 0.1000000000000021844 ) ;
#78098 = CARTESIAN_POINT ( 'NONE',  ( -23.15000000000000213, 1.115648428625851357E-11, -96.60000000000005116 ) ) ;
#78099 = DIRECTION ( 'NONE',  ( 0.000000000000000000, -0.1568667991644355497, -0.9876197685951332295 ) ) ;
#78100 = ORIENTED_EDGE ( 'NONE', *, *, #173248, .T. ) ;
#78101 = ORIENTED_EDGE ( 'NONE', *, *, #229810, .F. ) ;
#78102 = DIRECTION ( 'NONE',  ( 0.000000000000000000, 0.000000000000000000, 1.000000000000000000 ) ) ;
#78103 = EDGE_CURVE ( 'NONE', #232311, #52763, #134471, .T. ) ;
#78104 = DIRECTION ( 'NONE',  ( 1.000000000000000000, -0.000000000000000000, -0.000000000000000000 ) ) ;
#78105 = EDGE_LOOP ( 'NONE', ( #184570, #11517, #180377, #12254 ) ) ;
#78106 = DIRECTION ( 'NONE',  ( -0.000000000000000000, -0.000000000000000000, 1.000000000000000000 ) ) ;
#78107 = VERTEX_POINT ( 'NONE', #17365 ) ;
#78108 = LINE ( 'NONE', #98936, #231330 ) ;
#78109 = DIRECTION ( 'NONE',  ( 0.000000000000000000, 1.000000000000000000, 6.982962677686267499E-15 ) ) ;
#78111 = CARTESIAN_POINT ( 'NONE',  ( 23.14999999999999858, 5.600000000011153389, -188.5947339810868755 ) ) ;
#78110 = CARTESIAN_POINT ( 'NONE',  ( 23.14999999999999858, 68.08983204586465376, -237.7716021863518563 ) ) ;
#78112 = EDGE_CURVE ( 'NONE', #24864, #190429, #5467, .T. ) ;
#78113 = CARTESIAN_POINT ( 'NONE',  ( -18.39999999999999858, 13.18942546263217785, -207.6195883042091737 ) ) ;
#78114 = CARTESIAN_POINT ( 'NONE',  ( -18.59999999999999787, 9.250000000000001776, -12.25000000000000000 ) ) ;
#78115 = AXIS2_PLACEMENT_3D ( 'NONE', #144988, #109716, #246664 ) ;
#78116 = CARTESIAN_POINT ( 'NONE',  ( -18.54270223418607699, 85.62410550289459366, -62.78217243411680926 ) ) ;
#78118 = ORIENTED_EDGE ( 'NONE', *, *, #55702, .T. ) ;
#78117 = EDGE_LOOP ( 'NONE', ( #115224, #110717, #201823 ) ) ;
#78119 = ORIENTED_EDGE ( 'NONE', *, *, #20749, .T. ) ;
#78120 = EDGE_CURVE ( 'NONE', #74117, #205048, #226212, .T. ) ;
#78121 = CARTESIAN_POINT ( 'NONE',  ( -18.79999999999999716, 5.488301202077012775, 16.40000000000000213 ) ) ;
#78122 = CARTESIAN_POINT ( 'NONE',  ( 21.14999999999999503, -10.76604040606816959, -206.3127087229280789 ) ) ;
#78124 = EDGE_CURVE ( 'NONE', #41986, #9191, #241685, .T. ) ;
#78123 = CARTESIAN_POINT ( 'NONE',  ( 18.59999999999999787, 70.10000000001267040, -193.3040077198679967 ) ) ;
#78125 = DIRECTION ( 'NONE',  ( 0.000000000000000000, -0.008583690987162452199, -0.9999631594459053030 ) ) ;
#78127 = FACE_OUTER_BOUND ( 'NONE', #55622, .T. ) ;
#78126 = CARTESIAN_POINT ( 'NONE',  ( 20.21567752745019320, 10.19811410123150353, -7.882620347651839943 ) ) ;
#78128 = FACE_OUTER_BOUND ( 'NONE', #117791, .T. ) ;
#78129 = ORIENTED_EDGE ( 'NONE', *, *, #101447, .T. ) ;
#78130 = EDGE_CURVE ( 'NONE', #94336, #105678, #189578, .T. ) ;
#78131 = ORIENTED_EDGE ( 'NONE', *, *, #1005, .F. ) ;
#78132 = EDGE_LOOP ( 'NONE', ( #171382, #173697, #193887, #181007 ) ) ;
#78133 = PLANE ( 'NONE',  #137585 ) ;
#78134 = CARTESIAN_POINT ( 'NONE',  ( -20.94999999999999929, 87.39257802171833589, -200.4491579046923277 ) ) ;
#78135 = FACE_OUTER_BOUND ( 'NONE', #243924, .T. ) ;
#78136 = LINE ( 'NONE', #175998, #199895 ) ;
#78137 = AXIS2_PLACEMENT_3D ( 'NONE', #118574, #74334, #234650 ) ;
#78138 = AXIS2_PLACEMENT_3D ( 'NONE', #213052, #74873, #37019 ) ;
#78139 = LINE ( 'NONE', #220253, #225561 ) ;
#78140 = ORIENTED_EDGE ( 'NONE', *, *, #159460, .T. ) ;
#78142 = ORIENTED_EDGE ( 'NONE', *, *, #38179, .F. ) ;
#78141 = EDGE_CURVE ( 'NONE', #13111, #162125, #252760, .T. ) ;
#78143 = CARTESIAN_POINT ( 'NONE',  ( -21.05000000000000071, 11.65000000001115232, -40.28386566297815108 ) ) ;
#78144 = CARTESIAN_POINT ( 'NONE',  ( 18.59999999999999787, 1.115600667400684642E-11, -33.50000000000000000 ) ) ;
#78145 = ORIENTED_EDGE ( 'NONE', *, *, #245430, .T. ) ;
#78146 = CARTESIAN_POINT ( 'NONE',  ( -17.11825945287482753, 22.97806745954241592, -230.9350634111226270 ) ) ;
#78147 = DIRECTION ( 'NONE',  ( 0.000000000000000000, 0.000000000000000000, -1.000000000000000000 ) ) ;
#78148 = DIRECTION ( 'NONE',  ( 1.224646799147353207E-16, -1.000000000000000000, -6.982962677686266711E-15 ) ) ;
#78149 = CYLINDRICAL_SURFACE ( 'NONE', #257046, 11.80000000000000426 ) ;
#78150 = CARTESIAN_POINT ( 'NONE',  ( -16.81744102076749314, 66.05000000001187743, -90.37310748452438247 ) ) ;
#78151 = CARTESIAN_POINT ( 'NONE',  ( -21.05000000000000426, -0.09999999999999968636, 6.477067021124752522 ) ) ;
#78153 = DIRECTION ( 'NONE',  ( 1.000000000000000000, 0.000000000000000000, 0.000000000000000000 ) ) ;
#78152 = PLANE ( 'NONE',  #199356 ) ;
#78154 = CARTESIAN_POINT ( 'NONE',  ( 20.12500000000000355, 9.258049272928479567, -41.86333883714243598 ) ) ;
#78155 = ADVANCED_FACE ( 'NONE', ( #201266 ), #181717, .F. ) ;
#78156 = AXIS2_PLACEMENT_3D ( 'NONE', #217754, #176113, #58682 ) ;
#78157 = CARTESIAN_POINT ( 'NONE',  ( -18.39999999999999858, 85.50000000001210765, -129.9229180933022576 ) ) ;
#78158 = DIRECTION ( 'NONE',  ( 1.000000000000000000, 0.000000000000000000, -0.000000000000000000 ) ) ;
#78159 = CARTESIAN_POINT ( 'NONE',  ( 21.07933241753356768, 69.67135405163293171, -203.6164870749437057 ) ) ;
#78161 = EDGE_LOOP ( 'NONE', ( #130970, #144367, #146591, #138041, #159747 ) ) ;
#78160 = CARTESIAN_POINT ( 'NONE',  ( 23.14999999999999858, 0.000000000000000000, -33.50000000000000000 ) ) ;
#78162 = AXIS2_PLACEMENT_3D ( 'NONE', #4655, #221143, #60785 ) ;
#78163 = AXIS2_PLACEMENT_3D ( 'NONE', #186039, #127347, #208186 ) ;
#78164 = AXIS2_PLACEMENT_3D ( 'NONE', #56575, #138676, #236520 ) ;
#78165 = CARTESIAN_POINT ( 'NONE',  ( -21.05000000000000071, 76.00000000001270450, -207.8231074845243143 ) ) ;
#78166 = AXIS2_PLACEMENT_3D ( 'NONE', #544, #121806, #219591 ) ;
#78167 = VERTEX_POINT ( 'NONE', #18775 ) ;
#78168 = CARTESIAN_POINT ( 'NONE',  ( -18.39418127959864790, 54.09461110551220742, -229.1565698459269811 ) ) ;
#78169 = PLANE ( 'NONE',  #210515 ) ;
#78170 = VERTEX_POINT ( 'NONE', #218246 ) ;
#78171 = CARTESIAN_POINT ( 'NONE',  ( -21.64999999999999858, 9.350000000011133849, -154.8500000000000227 ) ) ;
#78172 = CARTESIAN_POINT ( 'NONE',  ( 20.94999999999999574, 70.10000000001213039, -126.3040077198679398 ) ) ;
#78173 = LINE ( 'NONE', #252963, #46463 ) ;
#78174 = AXIS2_PLACEMENT_3D ( 'NONE', #243716, #5068, #24698 ) ;
#78175 = CARTESIAN_POINT ( 'NONE',  ( -18.50000000000000000, 9.150000000011157653, -155.1500000000000057 ) ) ;
#78176 = CIRCLE ( 'NONE', #223915, 0.1000000000000055705 ) ;
#78177 = DIRECTION ( 'NONE',  ( 0.000000000000000000, 6.982962677686266711E-15, -1.000000000000000000 ) ) ;
#78178 = DIRECTION ( 'NONE',  ( 0.000000000000000000, -6.308085367188393199E-16, -1.000000000000000000 ) ) ;
#78179 = ADVANCED_FACE ( 'NONE', ( #216966 ), #43493, .T. ) ;
#78180 = AXIS2_PLACEMENT_3D ( 'NONE', #101458, #244861, #63659 ) ;
#78182 = EDGE_CURVE ( 'NONE', #23701, #183417, #67856, .T. ) ;
#78181 = AXIS2_PLACEMENT_3D ( 'NONE', #231365, #189658, #16180 ) ;
#78183 = ORIENTED_EDGE ( 'NONE', *, *, #102262, .T. ) ;
#78186 = ORIENTED_EDGE ( 'NONE', *, *, #175307, .T. ) ;
#78185 = DIRECTION ( 'NONE',  ( 0.000000000000000000, 0.9126074666063850316, 0.4088369013363101212 ) ) ;
#78184 = AXIS2_PLACEMENT_3D ( 'NONE', #177450, #82138, #39218 ) ;
#78187 = DIRECTION ( 'NONE',  ( 1.000000000000000000, 0.000000000000000000, 0.000000000000000000 ) ) ;
#78188 = DIRECTION ( 'NONE',  ( 0.000000000000000000, -7.272083257015735086E-15, 1.000000000000000000 ) ) ;
#78189 = AXIS2_PLACEMENT_3D ( 'NONE', #114262, #176820, #63262 ) ;
#78191 = EDGE_CURVE ( 'NONE', #177586, #204227, #63759, .T. ) ;
#78190 = FACE_OUTER_BOUND ( 'NONE', #170500, .T. ) ;
#78192 = EDGE_CURVE ( 'NONE', #106794, #211140, #97028, .T. ) ;
#78193 = EDGE_LOOP ( 'NONE', ( #116902, #202116, #25312, #114722 ) ) ;
#78194 = LINE ( 'NONE', #114769, #63777 ) ;
#78195 = APPLICATION_PROTOCOL_DEFINITION ( 'draft international standard', 'automotive_design', 1998, #922 ) ;
#78196 = DIRECTION ( 'NONE',  ( 1.000000000000000000, 0.000000000000000000, 0.000000000000000000 ) ) ;
#78197 = ADVANCED_FACE ( 'NONE', ( #78738 ), #117875, .T. ) ;
#78198 = ORIENTED_EDGE ( 'NONE', *, *, #170316, .T. ) ;
#78199 = CYLINDRICAL_SURFACE ( 'NONE', #208602, 0.1000000000000028644 ) ;
#78200 = DIRECTION ( 'NONE',  ( -1.000000000000000000, 0.000000000000000000, 0.000000000000000000 ) ) ;
#78201 = EDGE_CURVE ( 'NONE', #4469, #20618, #26355, .T. ) ;
#78202 = AXIS2_PLACEMENT_3D ( 'NONE', #39015, #95121, #57252 ) ;
#78205 = ADVANCED_FACE ( 'NONE', ( #4341 ), #120487, .T. ) ;
#78204 = ADVANCED_FACE ( 'NONE', ( #222087 ), #17957, .T. ) ;
#78203 = CIRCLE ( 'NONE', #165723, 0.09999999999999939493 ) ;
#78206 = AXIS2_PLACEMENT_3D ( 'NONE', #249767, #188505, #51526 ) ;
#78207 = CARTESIAN_POINT ( 'NONE',  ( -16.78805706634180339, 9.948252493082335945, -121.3441532080318979 ) ) ;
#78208 = ORIENTED_EDGE ( 'NONE', *, *, #225642, .T. ) ;
#78209 = ORIENTED_EDGE ( 'NONE', *, *, #41553, .T. ) ;
#78210 = CARTESIAN_POINT ( 'NONE',  ( -23.15000000000000213, 85.00000000001261924, -194.1291383618718385 ) ) ;
#78211 = CARTESIAN_POINT ( 'NONE',  ( 5.899999999999996803, -11.34999999999999964, 13.90000000000000213 ) ) ;
#78212 = CARTESIAN_POINT ( 'NONE',  ( 23.24999999999999289, 11.75000000001116263, -21.75000000000000355 ) ) ;
#78213 = DIRECTION ( 'NONE',  ( 2.952720810173289112E-16, 0.4088369013363281068, -0.9126074666063770380 ) ) ;
#78214 = EDGE_CURVE ( 'NONE', #75742, #198610, #1774, .T. ) ;
#78215 = CARTESIAN_POINT ( 'NONE',  ( -21.00000000000000000, 7.800000000000000711, 1.212568896937007867 ) ) ;
#78216 = TOROIDAL_SURFACE ( 'NONE', #57357, 0.2000000000000000111, 0.1000000000000000056 ) ;
#78218 = DIRECTION ( 'NONE',  ( 0.000000000000000000, 6.982962677686266711E-15, -1.000000000000000000 ) ) ;
#78217 = CARTESIAN_POINT ( 'NONE',  ( -16.77683809663752257, 66.05000000001182059, -82.17310748452439384 ) ) ;
#78220 = ADVANCED_FACE ( 'NONE', ( #197414 ), #98279, .T. ) ;
#78219 = DIRECTION ( 'NONE',  ( -1.186688945009010077E-16, -1.000000000000000000, -6.982962677686266711E-15 ) ) ;
#78221 = CARTESIAN_POINT ( 'NONE',  ( 23.14999999999999503, 29.00069016757795026, -237.9048565010683376 ) ) ;
#78223 = EDGE_CURVE ( 'NONE', #254810, #205457, #217853, .T. ) ;
#78222 = CARTESIAN_POINT ( 'NONE',  ( -20.94999999999999929, -5.011722593499800205, -233.2041167654973322 ) ) ;
#78224 = ORIENTED_EDGE ( 'NONE', *, *, #127764, .F. ) ;
#78225 = ORIENTED_EDGE ( 'NONE', *, *, #230430, .T. ) ;
#78226 = DIRECTION ( 'NONE',  ( 0.000000000000000000, -7.272083257015735086E-15, 1.000000000000000000 ) ) ;
#78228 = CARTESIAN_POINT ( 'NONE',  ( -21.14999999999994174, 77.16254490893143725, -44.02310748452479316 ) ) ;
#78227 = CYLINDRICAL_SURFACE ( 'NONE', #42312, 0.1000000000000124678 ) ;
#78229 = AXIS2_PLACEMENT_3D ( 'NONE', #59131, #158310, #138668 ) ;
#78230 = ADVANCED_FACE ( 'NONE', ( #223387 ), #224676, .T. ) ;
#78231 = CARTESIAN_POINT ( 'NONE',  ( 20.02499999999999858, 30.46448808713892831, -235.1722212069449256 ) ) ;
#78232 = DIRECTION ( 'NONE',  ( 0.000000000000000000, 0.000000000000000000, -1.000000000000000000 ) ) ;
#78233 = CARTESIAN_POINT ( 'NONE',  ( 21.05000000000000071, 1.115600667400684642E-11, -64.10000000000000853 ) ) ;
#78234 = ORIENTED_EDGE ( 'NONE', *, *, #45155, .T. ) ;
#78235 = ADVANCED_FACE ( 'NONE', ( #206413 ), #65610, .F. ) ;
#78236 = ORIENTED_EDGE ( 'NONE', *, *, #113065, .T. ) ;
#78237 = TOROIDAL_SURFACE ( 'NONE', #248949, 11.65000000000000036, 0.1000000000000000056 ) ;
#78238 = TOROIDAL_SURFACE ( 'NONE', #257253, 0.6000000000000004219, 0.1000000000000000056 ) ;
#78239 = CARTESIAN_POINT ( 'NONE',  ( 21.14999999999999858, 55.91711482281188950, -232.6830152854666949 ) ) ;
#78240 = TOROIDAL_SURFACE ( 'NONE', #53309, 0.4000000000000003553, 0.1000000000000000056 ) ;
#78241 = ORIENTED_EDGE ( 'NONE', *, *, #28793, .T. ) ;
#78242 = DIRECTION ( 'NONE',  ( 1.000000000000000000, 0.000000000000000000, 0.000000000000000000 ) ) ;
#78243 = CIRCLE ( 'NONE', #119985, 0.1000000000000028644 ) ;
#78244 = DIRECTION ( 'NONE',  ( -1.000000000000000000, 0.000000000000000000, -0.000000000000000000 ) ) ;
#78245 = EDGE_LOOP ( 'NONE', ( #164753, #105910, #26670, #93602, #16851 ) ) ;
#78246 = CARTESIAN_POINT ( 'NONE',  ( 23.14999999999999858, 70.40000000001180069, -81.92837350343744163 ) ) ;
#78247 = ORIENTED_EDGE ( 'NONE', *, *, #169395, .F. ) ;
#78248 = DIRECTION ( 'NONE',  ( 1.000000000000000000, -1.186688945009010077E-16, -8.286604613020808509E-31 ) ) ;
#78249 = CARTESIAN_POINT ( 'NONE',  ( 20.94999999999999574, 56.21213088740040575, -228.0580413555848338 ) ) ;
#78251 = CIRCLE ( 'NONE', #70098, 0.2000000000000057288 ) ;
#78250 = CARTESIAN_POINT ( 'NONE',  ( 18.50000000000000000, 85.40000000001239755, -163.1410656363516125 ) ) ;
#78252 = DIRECTION ( 'NONE',  ( 0.000000000000000000, 0.000000000000000000, -1.000000000000000000 ) ) ;
#78253 = CARTESIAN_POINT ( 'NONE',  ( -16.97683809663752896, 9.949999999999986855, -13.27152476866994490 ) ) ;
#78254 = CARTESIAN_POINT ( 'NONE',  ( 18.56579813702274961, 65.66974365629688748, -130.9360145562605169 ) ) ;
#78255 = DIRECTION ( 'NONE',  ( 0.000000000000000000, -0.000000000000000000, 1.000000000000000000 ) ) ;
#78256 = ORIENTED_EDGE ( 'NONE', *, *, #84087, .F. ) ;
#78258 = CARTESIAN_POINT ( 'NONE',  ( -16.87372397896796983, 66.11940046337028321, -116.1723829744886558 ) ) ;
#78257 = CARTESIAN_POINT ( 'NONE',  ( -16.89208623190940628, 9.951577948986638944, -188.3552722032182487 ) ) ;
#78259 = VERTEX_POINT ( 'NONE', #248102 ) ;
#78261 = ORIENTED_EDGE ( 'NONE', *, *, #160854, .F. ) ;
#78260 = CARTESIAN_POINT ( 'NONE',  ( 12.25000000000000000, 26.54497872210689735, -232.9592037335782209 ) ) ;
#78262 = VECTOR ( 'NONE', #226769, 1000.000000000000000 ) ;
#78263 = ORIENTED_EDGE ( 'NONE', *, *, #205981, .T. ) ;
#78264 = PLANE ( 'NONE',  #120006 ) ;
#78265 = CARTESIAN_POINT ( 'NONE',  ( -22.47007471830798409, 1.115783626517291733E-11, -25.77928934807352945 ) ) ;
#78266 = DIRECTION ( 'NONE',  ( 1.000000000000000000, 0.000000000000000000, 0.000000000000000000 ) ) ;
#78267 = DIRECTION ( 'NONE',  ( 0.000000000000000000, -1.000000000000000000, 0.000000000000000000 ) ) ;
#78268 = ORIENTED_EDGE ( 'NONE', *, *, #150711, .T. ) ;
#78269 = CARTESIAN_POINT ( 'NONE',  ( 20.95000000000005258, 65.35000000001120668, -4.423107484524790856 ) ) ;
#78270 = CARTESIAN_POINT ( 'NONE',  ( 22.59999999999999432, 64.25043287652329127, -203.6239658536231616 ) ) ;
#78271 = ORIENTED_EDGE ( 'NONE', *, *, #122979, .F. ) ;
#78272 = DIRECTION ( 'NONE',  ( -1.000000000000000000, -0.000000000000000000, -0.000000000000000000 ) ) ;
#78273 = ADVANCED_FACE ( 'NONE', ( #245550 ), #138725, .T. ) ;
#78274 = SPHERICAL_SURFACE ( 'NONE', #155717, 0.1000000000000000056 ) ;
#78275 = VECTOR ( 'NONE', #174476, 1000.000000000000227 ) ;
#78276 = EDGE_LOOP ( 'NONE', ( #104213, #102471, #103557, #170702 ) ) ;
#78278 = ORIENTED_EDGE ( 'NONE', *, *, #109540, .T. ) ;
#78277 = VECTOR ( 'NONE', #119251, 1000.000000000000000 ) ;
#78279 = EDGE_CURVE ( 'NONE', #215522, #12719, #155375, .T. ) ;
#78280 = CARTESIAN_POINT ( 'NONE',  ( -20.54999999999999716, 4.250000000011156409, -179.7499999999999716 ) ) ;
#78281 = AXIS2_PLACEMENT_3D ( 'NONE', #47707, #167699, #166420 ) ;
#78282 = ORIENTED_EDGE ( 'NONE', *, *, #213467, .T. ) ;
#78283 = CARTESIAN_POINT ( 'NONE',  ( -18.37013991200266005, 11.49974761621196961, -9.206976989482884122 ) ) ;
#78284 = ORIENTED_EDGE ( 'NONE', *, *, #111501, .F. ) ;
#78285 = DIRECTION ( 'NONE',  ( 0.000000000000000000, 0.000000000000000000, 1.000000000000000000 ) ) ;
#78286 = EDGE_CURVE ( 'NONE', #245440, #65298, #205103, .T. ) ;
#78287 = ADVANCED_FACE ( 'NONE', ( #86429 ), #251223, .F. ) ;
#78288 = DIRECTION ( 'NONE',  ( 1.000000000000000000, 0.000000000000000000, 0.000000000000000000 ) ) ;
#78289 = CARTESIAN_POINT ( 'NONE',  ( -23.15000000000000213, 54.92280082623103965, -239.2759596675668092 ) ) ;
#78290 = CARTESIAN_POINT ( 'NONE',  ( -16.88460203013674388, 63.08529900177730099, -213.1110381636136424 ) ) ;
#78292 = AXIS2_PLACEMENT_3D ( 'NONE', #181553, #240240, #4169 ) ;
#78291 = CARTESIAN_POINT ( 'NONE',  ( -23.15000000000000213, 76.00000000001190870, -103.0231074845243029 ) ) ;
#78293 = CARTESIAN_POINT ( 'NONE',  ( -22.60000000000094289, 0.1008583691096561347, -88.75043287651061519 ) ) ;
#78294 = DIRECTION ( 'NONE',  ( 1.000000000000000000, 0.000000000000000000, 0.000000000000000000 ) ) ;
#78295 = ORIENTED_EDGE ( 'NONE', *, *, #31383, .F. ) ;
#78297 = DIRECTION ( 'NONE',  ( 0.000000000000000000, -0.4088369013363783999, 0.9126074666063545004 ) ) ;
#78296 = DIRECTION ( 'NONE',  ( 0.000000000000000000, 7.162729191130023213E-15, -1.000000000000000000 ) ) ;
#78298 = ORIENTED_EDGE ( 'NONE', *, *, #157075, .T. ) ;
#78301 = ORIENTED_EDGE ( 'NONE', *, *, #112233, .T. ) ;
#78300 = CARTESIAN_POINT ( 'NONE',  ( 23.24999999999999645, 5.650000000011139001, -154.8500000000000227 ) ) ;
#78299 = SURFACE_SIDE_STYLE ('',( #123877 ) ) ;
#78302 = ADVANCED_FACE ( 'NONE', ( #68189 ), #105418, .T. ) ;
#78303 = VERTEX_POINT ( 'NONE', #188138 ) ;
#78304 = VECTOR ( 'NONE', #198035, 1000.000000000000000 ) ;
#78305 = CARTESIAN_POINT ( 'NONE',  ( -18.79999999999999716, -11.75000000000000178, 0.000000000000000000 ) ) ;
#78306 = EDGE_CURVE ( 'NONE', #165183, #177806, #251171, .T. ) ;
#78307 = CARTESIAN_POINT ( 'NONE',  ( 21.05000000000080362, 0.05148288189288811878, -60.69982018208269636 ) ) ;
#78308 = DIRECTION ( 'NONE',  ( 0.000000000000000000, -6.982962677686266711E-15, 1.000000000000000000 ) ) ;
#78309 = DIRECTION ( 'NONE',  ( -0.000000000000000000, -0.000000000000000000, 1.000000000000000000 ) ) ;
#78310 = ORIENTED_EDGE ( 'NONE', *, *, #106205, .T. ) ;
#78311 = CARTESIAN_POINT ( 'NONE',  ( -16.86379686415369150, 66.02478224075885294, -115.5897175954340810 ) ) ;
#78313 = CARTESIAN_POINT ( 'NONE',  ( -23.25000000000000000, 74.86109765932731364, -233.8067614591677454 ) ) ;
#78312 =( BOUNDED_SURFACE ( )  B_SPLINE_SURFACE ( 3, 2, ( 
 ( #240453, #158384, #80051 ),
 ( #159637, #102186, #140042 ),
 ( #121804, #40999, #237882 ),
 ( #241734, #120533, #181768 ) ),
 .UNSPECIFIED., .F., .F., .F. ) 
 B_SPLINE_SURFACE_WITH_KNOTS ( ( 4, 4 ),
 ( 3, 3 ),
 ( 0.3000847527772385059, 0.5552748953338751958 ),
 ( 0.000000000000000000, 1.000000000000000000 ),
 .UNSPECIFIED. ) 
 GEOMETRIC_REPRESENTATION_ITEM ( )  RATIONAL_B_SPLINE_SURFACE ( (
 ( 1.000000000000000000, 0.9152888060719372998, 1.000000000000000000),
 ( 1.000000000000000000, 0.9104333467450547168, 1.000000000000000000),
 ( 1.000000000000000000, 0.9035312726220219304, 1.000000000000000000),
 ( 1.000000000000000000, 0.8946697475932521293, 1.000000000000000000) ) ) 
 REPRESENTATION_ITEM ( '' )  SURFACE ( )  );
#78315 = CARTESIAN_POINT ( 'NONE',  ( 18.59999999999999787, 80.69087520990402140, -192.8618289658565743 ) ) ;
#78314 = DIRECTION ( 'NONE',  ( 1.186688945009009831E-16, 1.000000000000000000, 6.982962677686266711E-15 ) ) ;
#78317 = ORIENTED_EDGE ( 'NONE', *, *, #248168, .T. ) ;
#78316 = CARTESIAN_POINT ( 'NONE',  ( 23.24999999999999645, 8.822561741677553471, -109.7500000000000426 ) ) ;
#78318 = EDGE_CURVE ( 'NONE', #198298, #215317, #163719, .T. ) ;
#78319 = ORIENTED_EDGE ( 'NONE', *, *, #21735, .T. ) ;
#78320 = CIRCLE ( 'NONE', #224068, 0.3999999999999975797 ) ;
#78321 = ADVANCED_FACE ( 'NONE', ( #129447 ), #30362, .T. ) ;
#78322 = VECTOR ( 'NONE', #60394, 1000.000000000000000 ) ;
#78323 = AXIS2_PLACEMENT_3D ( 'NONE', #164190, #83320, #207168 ) ;
#78324 = CARTESIAN_POINT ( 'NONE',  ( -23.15000000000000213, 67.23127455305835554, -235.8551265064784559 ) ) ;
#78325 = ORIENTED_EDGE ( 'NONE', *, *, #209506, .F. ) ;
#78326 = DIRECTION ( 'NONE',  ( 0.000000000000000000, 0.000000000000000000, 1.000000000000000000 ) ) ;
#78327 = ORIENTED_EDGE ( 'NONE', *, *, #189791, .F. ) ;
#78328 =( BOUNDED_SURFACE ( )  B_SPLINE_SURFACE ( 3, 2, ( 
 ( #102536, #238228, #240811 ),
 ( #200399, #41350, #183407 ),
 ( #62176, #122148, #59559 ),
 ( #21772, #199112, #101238 ) ),
 .UNSPECIFIED., .F., .F., .F. ) 
 B_SPLINE_SURFACE_WITH_KNOTS ( ( 4, 4 ),
 ( 3, 3 ),
 ( 0.0008258556059633668459, 0.0009616864997632829570 ),
 ( 0.000000000000000000, 1.000000000000000000 ),
 .UNSPECIFIED. ) 
 GEOMETRIC_REPRESENTATION_ITEM ( )  RATIONAL_B_SPLINE_SURFACE ( (
 ( 1.000000000000000000, 0.9152888060719409635, 1.000000000000000000),
 ( 1.000000000000000000, 0.9327727094138329456, 1.000000000000000000),
 ( 1.000000000000000000, 0.9369023509258374016, 1.000000000000000000),
 ( 1.000000000000000000, 0.9246339933864329286, 1.000000000000000000) ) ) 
 REPRESENTATION_ITEM ( '' )  SURFACE ( )  );
#78329 = DIRECTION ( 'NONE',  ( 1.000000000000000000, 0.000000000000000000, 0.000000000000000000 ) ) ;
#78330 = DIRECTION ( 'NONE',  ( 0.000000000000000000, 0.000000000000000000, 1.000000000000000000 ) ) ;
#78331 = CARTESIAN_POINT ( 'NONE',  ( -18.50000000000000000, 11.64999999999999680, -12.25000000000000000 ) ) ;
#78332 = AXIS2_PLACEMENT_3D ( 'NONE', #70884, #130821, #228663 ) ;
#78333 = ORIENTED_EDGE ( 'NONE', *, *, #4786, .T. ) ;
#78334 = EDGE_CURVE ( 'NONE', #11462, #62456, #143855, .T. ) ;
#78335 = CARTESIAN_POINT ( 'NONE',  ( -1.739115166359751801E-14, 64.35000000001157616, -57.27310748452440237 ) ) ;
#78336 = EDGE_CURVE ( 'NONE', #216063, #71479, #42921, .T. ) ;
#78337 = EDGE_CURVE ( 'NONE', #200852, #140838, #15953, .T. ) ;
#78338 = CIRCLE ( 'NONE', #165859, 0.5000000000000014433 ) ;
#78339 = AXIS2_PLACEMENT_3D ( 'NONE', #161889, #160612, #100568 ) ;
#78340 = DIRECTION ( 'NONE',  ( 0.000000000000000000, 0.000000000000000000, -1.000000000000000000 ) ) ;
#78341 = AXIS2_PLACEMENT_3D ( 'NONE', #31832, #111342, #250830 ) ;
#78342 =( BOUNDED_CURVE ( )  B_SPLINE_CURVE ( 3, ( #245457, #163348, #242872, #184172 ),
 .UNSPECIFIED., .F., .F. ) 
 B_SPLINE_CURVE_WITH_KNOTS ( ( 4, 4 ),
 ( 2.589852378279005940, 2.850972632318390598 ),
 .UNSPECIFIED. ) 
 CURVE ( )  GEOMETRIC_REPRESENTATION_ITEM ( )  RATIONAL_B_SPLINE_CURVE ( ( 1.000000000000000000, 0.9943260843901261525, 0.9943260843901261525, 1.000000000000000000 ) ) 
 REPRESENTATION_ITEM ( '' )  );
#78343 = ORIENTED_EDGE ( 'NONE', *, *, #175157, .F. ) ;
#78344 = EDGE_LOOP ( 'NONE', ( #92050, #209259, #83001, #62380 ) ) ;
#78345 = AXIS2_PLACEMENT_3D ( 'NONE', #109637, #190500, #50931 ) ;
#78346 = ORIENTED_EDGE ( 'NONE', *, *, #204267, .F. ) ;
#78347 = DIRECTION ( 'NONE',  ( 0.000000000000000000, 0.000000000000000000, 1.000000000000000000 ) ) ;
#78348 = ORIENTED_EDGE ( 'NONE', *, *, #52722, .F. ) ;
#78350 = ORIENTED_EDGE ( 'NONE', *, *, #39479, .T. ) ;
#78349 = CARTESIAN_POINT ( 'NONE',  ( 21.14999999999999503, -13.88357498613435048, -191.9982587459959689 ) ) ;
#78351 = EDGE_CURVE ( 'NONE', #223496, #137741, #55338, .T. ) ;
#78352 = ORIENTED_EDGE ( 'NONE', *, *, #188332, .F. ) ;
#78355 = ORIENTED_EDGE ( 'NONE', *, *, #215515, .T. ) ;
#78354 = ORIENTED_EDGE ( 'NONE', *, *, #221700, .F. ) ;
#78353 = LINE ( 'NONE', #79627, #72879 ) ;
#78356 = EDGE_CURVE ( 'NONE', #31598, #126171, #176208, .T. ) ;
#78358 = ORIENTED_EDGE ( 'NONE', *, *, #65061, .F. ) ;
#78357 = AXIS2_PLACEMENT_3D ( 'NONE', #21803, #240846, #180874 ) ;
#78359 = DIRECTION ( 'NONE',  ( 0.000000000000000000, 0.2617529984165031243, 0.9651348961777157509 ) ) ;
#78360 = CIRCLE ( 'NONE', #198598, 0.1000000000000028644 ) ;
#78361 = CARTESIAN_POINT ( 'NONE',  ( -20.54999999999999716, 7.150000000000000355, -16.75000000000000000 ) ) ;
#78362 = AXIS2_PLACEMENT_3D ( 'NONE', #188123, #167302, #48604 ) ;
#78363 = DIRECTION ( 'NONE',  ( -0.000000000000000000, 0.1480365673253065117, -0.9889818879709273425 ) ) ;
#78364 = AXIS2_PLACEMENT_3D ( 'NONE', #21011, #234907, #177531 ) ;
#78365 = ORIENTED_EDGE ( 'NONE', *, *, #28139, .T. ) ;
#78366 = AXIS2_PLACEMENT_3D ( 'NONE', #89859, #183835, #65162 ) ;
#78367 = DIRECTION ( 'NONE',  ( 0.000000000000000000, -6.982962677686266711E-15, 1.000000000000000000 ) ) ;
#78369 = ORIENTED_EDGE ( 'NONE', *, *, #242563, .T. ) ;
#78368 = CARTESIAN_POINT ( 'NONE',  ( 21.05000000000000071, 4.260086453440762533, -245.2296700999207246 ) ) ;
#78370 = CARTESIAN_POINT ( 'NONE',  ( 21.14999999999999503, -0.09999999999999939493, 11.64957080754479968 ) ) ;
#78372 = VERTEX_POINT ( 'NONE', #233695 ) ;
#78371 = FACE_OUTER_BOUND ( 'NONE', #225007, .T. ) ;
#78373 = VECTOR ( 'NONE', #46314, 1000.000000000000000 ) ;
#78374 = ORIENTED_EDGE ( 'NONE', *, *, #38371, .T. ) ;
#78375 = FACE_OUTER_BOUND ( 'NONE', #77649, .T. ) ;
#78376 = PRESENTATION_STYLE_ASSIGNMENT (( #135778 ) ) ;
#78377 = ORIENTED_EDGE ( 'NONE', *, *, #217989, .F. ) ;
#78378 = ORIENTED_EDGE ( 'NONE', *, *, #106959, .T. ) ;
#78379 = CARTESIAN_POINT ( 'NONE',  ( -16.93906926870270624, 10.01214687095770906, -180.0534523072267916 ) ) ;
#78380 = CARTESIAN_POINT ( 'NONE',  ( -18.50000000000000000, 11.65000000001115232, -146.1500000000000341 ) ) ;
#78381 = AXIS2_PLACEMENT_3D ( 'NONE', #53330, #33814, #18047 ) ;
#78382 = CIRCLE ( 'NONE', #90856, 0.1999999999999987899 ) ;
#78384 = ORIENTED_EDGE ( 'NONE', *, *, #245366, .F. ) ;
#78383 = VERTEX_POINT ( 'NONE', #134557 ) ;
#78385 = EDGE_LOOP ( 'NONE', ( #2155, #58390, #150549, #183213, #247661, #54919 ) ) ;
#78386 = CARTESIAN_POINT ( 'NONE',  ( 21.05543885634738288, 61.95077084394885247, -221.7984674804167184 ) ) ;
#78387 = VERTEX_POINT ( 'NONE', #169908 ) ;
#78388 = EDGE_LOOP ( 'NONE', ( #184092, #133425, #5257, #79640, #101871 ) ) ;
#78389 = CARTESIAN_POINT ( 'NONE',  ( -21.55000000000000426, 7.750000000000003553, -21.25000000000000000 ) ) ;
#78390 = ORIENTED_EDGE ( 'NONE', *, *, #225914, .T. ) ;
#78391 = DIRECTION ( 'NONE',  ( 0.000000000000000000, 0.000000000000000000, -1.000000000000000000 ) ) ;
#78393 = DIRECTION ( 'NONE',  ( 1.000000000000000000, 0.000000000000000000, 0.000000000000000000 ) ) ;
#78392 = CARTESIAN_POINT ( 'NONE',  ( -20.85000000000000142, 64.35000000001245724, -170.0231074845244166 ) ) ;
#78394 = VERTEX_POINT ( 'NONE', #234976 ) ;
#78395 = AXIS2_PLACEMENT_3D ( 'NONE', #222437, #123376, #84178 ) ;
#78396 = TOROIDAL_SURFACE ( 'NONE', #211713, 0.2000000000000000111, 0.1000000000000000056 ) ;
#78398 = ORIENTED_EDGE ( 'NONE', *, *, #242800, .T. ) ;
#78397 = EDGE_LOOP ( 'NONE', ( #16076, #23283, #59410, #170703 ) ) ;
#78399 = CARTESIAN_POINT ( 'NONE',  ( -23.25000000000000000, 77.83585931145600512, -158.5186683157258187 ) ) ;
#78400 = CARTESIAN_POINT ( 'NONE',  ( -23.15000000000000213, 1.115650265596050101E-11, -96.45000000000003126 ) ) ;
#78401 = CIRCLE ( 'NONE', #194956, 12.97499999999999964 ) ;
#78402 = ORIENTED_EDGE ( 'NONE', *, *, #67913, .T. ) ;
#78403 = CIRCLE ( 'NONE', #32684, 0.1000000000000091649 ) ;
#78404 = CARTESIAN_POINT ( 'NONE',  ( -18.47653818581420992, 85.46528038777485392, -95.89714666838439427 ) ) ;
#78405 = ORIENTED_EDGE ( 'NONE', *, *, #240963, .T. ) ;
#78406 = ORIENTED_EDGE ( 'NONE', *, *, #12626, .T. ) ;
#78407 = CARTESIAN_POINT ( 'NONE',  ( 18.59999999999998366, 76.00000000001170974, -69.52310748452431710 ) ) ;
#78408 = EDGE_CURVE ( 'NONE', #2075, #237152, #109656, .T. ) ;
#78409 = ORIENTED_EDGE ( 'NONE', *, *, #199743, .T. ) ;
#78410 = CARTESIAN_POINT ( 'NONE',  ( -21.44999999999999929, 68.65000000001187175, -90.67310748452436542 ) ) ;
#78411 = DIRECTION ( 'NONE',  ( 0.000000000000000000, 0.1455152366551500653, 0.9893560106964507384 ) ) ;
#78412 = ORIENTED_EDGE ( 'NONE', *, *, #221212, .T. ) ;
#78413 = VECTOR ( 'NONE', #248086, 1000.000000000000000 ) ;
#78414 = DIRECTION ( 'NONE',  ( 1.000000000000000000, -0.000000000000000000, -0.000000000000000000 ) ) ;
#78415 = DIRECTION ( 'NONE',  ( 0.000000000000000000, 0.2128009952263603954, -0.9770955615653315052 ) ) ;
#78417 = LINE ( 'NONE', #82245, #124740 ) ;
#78416 = DIRECTION ( 'NONE',  ( -1.000000000000000000, 0.000000000000000000, 0.000000000000000000 ) ) ;
#78418 = FACE_OUTER_BOUND ( 'NONE', #193586, .T. ) ;
#78419 = EDGE_CURVE ( 'NONE', #46719, #183460, #12093, .T. ) ;
#78420 = CARTESIAN_POINT ( 'NONE',  ( -22.39999999999999858, 76.00000000001217870, -142.7731074845243029 ) ) ;
#78423 = EDGE_CURVE ( 'NONE', #144728, #196043, #197016, .T. ) ;
#78422 = CIRCLE ( 'NONE', #207626, 0.5999999999999894307 ) ;
#78421 = CARTESIAN_POINT ( 'NONE',  ( 21.07888907270776002, 65.27493078649706604, -157.8019138976912359 ) ) ;
#78424 = AXIS2_PLACEMENT_3D ( 'NONE', #191759, #10528, #208737 ) ;
#78425 = CARTESIAN_POINT ( 'NONE',  ( -16.81453563122428108, 66.06089979457530603, -149.2348488238791901 ) ) ;
#78426 = CARTESIAN_POINT ( 'NONE',  ( 22.40736611211992368, 76.00000000001222134, -148.1726782920690937 ) ) ;
#78428 = CARTESIAN_POINT ( 'NONE',  ( -20.94999999999999929, 1.115600667400684642E-11, -134.0000000000000000 ) ) ;
#78427 = AXIS2_PLACEMENT_3D ( 'NONE', #224897, #248330, #145370 ) ;
#78430 = EDGE_LOOP ( 'NONE', ( #228515, #121843, #60371, #10040 ) ) ;
#78429 = VECTOR ( 'NONE', #121076, 1000.000000000000000 ) ;
#78432 = ORIENTED_EDGE ( 'NONE', *, *, #154159, .F. ) ;
#78431 = ORIENTED_EDGE ( 'NONE', *, *, #188020, .F. ) ;
#78433 = EDGE_LOOP ( 'NONE', ( #246448, #83335, #213644, #124507 ) ) ;
#78434 = ORIENTED_EDGE ( 'NONE', *, *, #112404, .T. ) ;
#78435 = EDGE_CURVE ( 'NONE', #212797, #155749, #226039, .T. ) ;
#78436 = DIRECTION ( 'NONE',  ( -0.000000000000000000, 0.1686199900910312910, -0.9856811345164826488 ) ) ;
#78437 = DIRECTION ( 'NONE',  ( 1.000000000000000000, 0.000000000000000000, 0.000000000000000000 ) ) ;
#78439 = DIRECTION ( 'NONE',  ( -1.836970198721029934E-16, -0.9651348961777157509, 0.2617529984165031243 ) ) ;
#78438 = FACE_OUTER_BOUND ( 'NONE', #144674, .T. ) ;
#78440 = ORIENTED_EDGE ( 'NONE', *, *, #75866, .T. ) ;
#78441 = CIRCLE ( 'NONE', #32522, 0.09999999999999992228 ) ;
#78442 = DIRECTION ( 'NONE',  ( 0.000000000000000000, -0.9126074666063773710, -0.4088369013363271631 ) ) ;
#78443 = LINE ( 'NONE', #198402, #237392 ) ;
#78444 = CARTESIAN_POINT ( 'NONE',  ( -16.88815647973234135, 9.950832619326892114, -180.1472170633259680 ) ) ;
#78445 = CARTESIAN_POINT ( 'NONE',  ( 18.50000000000000000, -9.419078080838366063, -73.82992535020829905 ) ) ;
#78446 = ORIENTED_EDGE ( 'NONE', *, *, #193143, .T. ) ;
#78447 = DIRECTION ( 'NONE',  ( -0.000000000000000000, 0.000000000000000000, 1.000000000000000000 ) ) ;
#78448 = ORIENTED_EDGE ( 'NONE', *, *, #132687, .F. ) ;
#78449 = ADVANCED_FACE ( 'NONE', ( #192012 ), #159623, .T. ) ;
#78450 = CYLINDRICAL_SURFACE ( 'NONE', #103772, 0.1000000000000076522 ) ;
#78451 = EDGE_CURVE ( 'NONE', #140899, #154073, #113645, .T. ) ;
#78452 = DIRECTION ( 'NONE',  ( 0.000000000000000000, 0.000000000000000000, -1.000000000000000000 ) ) ;
#78453 = DIRECTION ( 'NONE',  ( 0.000000000000000000, 6.982962677686266711E-15, -1.000000000000000000 ) ) ;
#78454 = CARTESIAN_POINT ( 'NONE',  ( -20.85000000000000142, 77.16412189325360771, -162.1082593989527254 ) ) ;
#78455 = VERTEX_POINT ( 'NONE', #92873 ) ;
#78456 = CARTESIAN_POINT ( 'NONE',  ( -21.05000000000000071, 1.851028230152016674, -78.65391326942254580 ) ) ;
#78457 = CARTESIAN_POINT ( 'NONE',  ( -21.05000000000000071, 76.00000000001139711, -31.92310748452432279 ) ) ;
#78458 = CARTESIAN_POINT ( 'NONE',  ( 21.05000000000000071, 82.57900542960499024, -215.5587758314583766 ) ) ;
#78460 = DIRECTION ( 'NONE',  ( 2.952720810173289112E-16, -1.000000000000000000, 0.000000000000000000 ) ) ;
#78459 = CARTESIAN_POINT ( 'NONE',  ( 21.00000000000000000, 9.750000000011153745, -121.6500000000000341 ) ) ;
#78461 = CARTESIAN_POINT ( 'NONE',  ( 20.97224591636398472, 10.62515341617478271, -45.74992590466358422 ) ) ;
#78462 = ADVANCED_FACE ( 'NONE', ( #193281 ), #74653, .F. ) ;
#78463 = CARTESIAN_POINT ( 'NONE',  ( -20.00857864376270001, 9.250000000000001776, -12.34999999999999964 ) ) ;
#78464 = CIRCLE ( 'NONE', #49244, 0.09999999999998898659 ) ;
#78465 = AXIS2_PLACEMENT_3D ( 'NONE', #252215, #73624, #116573 ) ;
#78466 = CARTESIAN_POINT ( 'NONE',  ( 22.39999999999999858, 10.71943444926881561, -226.8179467668883547 ) ) ;
#78467 = DIRECTION ( 'NONE',  ( -1.000000000000000000, 0.000000000000000000, 0.000000000000000000 ) ) ;
#78468 = VECTOR ( 'NONE', #35879, 1000.000000000000000 ) ;
#78469 = EDGE_LOOP ( 'NONE', ( #51719, #75510, #173395, #256906 ) ) ;
#78470 = EDGE_LOOP ( 'NONE', ( #189407, #198023, #227564, #213622 ) ) ;
#78471 = CARTESIAN_POINT ( 'NONE',  ( 21.05000000000000071, 85.00000000001251976, -179.5170766071767332 ) ) ;
#78472 = ORIENTED_EDGE ( 'NONE', *, *, #149518, .T. ) ;
#78473 = CARTESIAN_POINT ( 'NONE',  ( 18.59999999999999076, 43.63140573099096287, -239.9077968784524444 ) ) ;
#78474 = ADVANCED_FACE ( 'NONE', ( #17222 ), #113830, .T. ) ;
#78476 = VECTOR ( 'NONE', #36615, 1000.000000000000000 ) ;
#78475 = CARTESIAN_POINT ( 'NONE',  ( 21.05000000000000071, 11.75000000001116263, -160.4851942293460638 ) ) ;
#78477 = DIRECTION ( 'NONE',  ( -1.000000000000000000, 0.000000000000000000, -0.000000000000000000 ) ) ;
#78478 = ORIENTED_EDGE ( 'NONE', *, *, #121053, .F. ) ;
#78479 = CIRCLE ( 'NONE', #178480, 0.5000000000000004441 ) ;
#78480 = DIRECTION ( 'NONE',  ( 0.000000000000000000, 1.000000000000000000, 6.982962677686266711E-15 ) ) ;
#78481 = CARTESIAN_POINT ( 'NONE',  ( -15.06720934482787833, 9.417690691074259490, -51.64160069676458420 ) ) ;
#78482 = CARTESIAN_POINT ( 'NONE',  ( -18.58222699835055280, 65.66799936921530900, -97.42993998886007034 ) ) ;
#78483 = EDGE_CURVE ( 'NONE', #69752, #32613, #238923, .T. ) ;
#78484 = DIRECTION ( 'NONE',  ( 1.000000000000000000, 0.000000000000000000, 0.000000000000000000 ) ) ;
#78486 = ORIENTED_EDGE ( 'NONE', *, *, #194309, .T. ) ;
#78485 = CARTESIAN_POINT ( 'NONE',  ( -16.97683810757273193, 9.950000000011137047, -187.7364232875387984 ) ) ;
#78488 = DIRECTION ( 'NONE',  ( -1.000000000000000000, 0.000000000000000000, 0.000000000000000000 ) ) ;
#78487 = DIRECTION ( 'NONE',  ( -1.000000000000000000, 0.000000000000000000, -0.000000000000000000 ) ) ;
#78489 = PLANE ( 'NONE',  #56905 ) ;
#78490 = DIRECTION ( 'NONE',  ( -7.304098846218134667E-16, -1.000000000000000000, -6.982962677686267499E-15 ) ) ;
#78491 = CARTESIAN_POINT ( 'NONE',  ( 18.60000000000000142, 86.99328439831825222, -199.3739436137589678 ) ) ;
#78493 = EDGE_CURVE ( 'NONE', #199047, #131339, #111171, .T. ) ;
#78492 = DIRECTION ( 'NONE',  ( 0.000000000000000000, 1.000000000000000000, -0.000000000000000000 ) ) ;
#78494 = ADVANCED_FACE ( 'NONE', ( #151607 ), #251382, .T. ) ;
#78495 = EDGE_LOOP ( 'NONE', ( #158572, #252460, #15266, #208167 ) ) ;
#78496 = CARTESIAN_POINT ( 'NONE',  ( 0.000000000000000000, 0.000000000000000000, 0.000000000000000000 ) ) ;
#78497 = DIRECTION ( 'NONE',  ( 0.000000000000000000, -6.467318590049456648E-15, 1.000000000000000000 ) ) ;
#78498 = ORIENTED_EDGE ( 'NONE', *, *, #147127, .T. ) ;
#78499 = VECTOR ( 'NONE', #171522, 1000.000000000000000 ) ;
#78500 = CARTESIAN_POINT ( 'NONE',  ( -23.25000000000000000, 11.75000000001115552, -100.5000000000000426 ) ) ;
#78501 = ORIENTED_EDGE ( 'NONE', *, *, #94090, .F. ) ;
#78502 = AXIS2_PLACEMENT_3D ( 'NONE', #61383, #183901, #5230 ) ;
#78503 = EDGE_CURVE ( 'NONE', #179524, #56891, #126478, .T. ) ;
#78504 = DIRECTION ( 'NONE',  ( 0.000000000000000000, 0.9126074666063770380, 0.4088369013363281068 ) ) ;
#78505 = EDGE_CURVE ( 'NONE', #182894, #221888, #222123, .T. ) ;
#78506 = CARTESIAN_POINT ( 'NONE',  ( -16.93935632781549572, 9.984730499725088748, -20.88966074871030187 ) ) ;
#78507 = CARTESIAN_POINT ( 'NONE',  ( -23.25000000000000000, 76.00000000001244871, -170.0231074845243597 ) ) ;
#78508 = ORIENTED_EDGE ( 'NONE', *, *, #114447, .T. ) ;
#78509 = AXIS2_PLACEMENT_3D ( 'NONE', #84931, #43285, #182812 ) ;
#78510 = EDGE_CURVE ( 'NONE', #213491, #177211, #19790, .T. ) ;
#78511 = ORIENTED_EDGE ( 'NONE', *, *, #166415, .F. ) ;
#78512 = CARTESIAN_POINT ( 'NONE',  ( 21.05000000000000071, 8.575267064043504917, -199.1323982654951976 ) ) ;
#78513 = DIRECTION ( 'NONE',  ( 0.000000000000000000, 0.9126074666063769270, 0.4088369013363280513 ) ) ;
#78514 = EDGE_CURVE ( 'NONE', #97476, #80255, #38073, .T. ) ;
#78515 = CARTESIAN_POINT ( 'NONE',  ( -16.80070461188017816, 63.08652707989409691, -213.1246912725079881 ) ) ;
#78516 = DIRECTION ( 'NONE',  ( -6.938893903907222856E-15, 0.9770955615653315052, 0.2128009952263607008 ) ) ;
#78517 = DIRECTION ( 'NONE',  ( 0.000000000000000000, 0.000000000000000000, 1.000000000000000000 ) ) ;
#78518 = AXIS2_PLACEMENT_3D ( 'NONE', #241290, #1356, #140894 ) ;
#78520 = CARTESIAN_POINT ( 'NONE',  ( 20.94999999999999929, 69.55000000001230376, -160.0060803140843859 ) ) ;
#78519 = AXIS2_PLACEMENT_3D ( 'NONE', #13373, #152909, #17236 ) ;
#78522 = EDGE_CURVE ( 'NONE', #152450, #67428, #172325, .T. ) ;
#78521 = DIRECTION ( 'NONE',  ( 1.000000000000000000, -0.000000000000000000, -0.000000000000000000 ) ) ;
#78524 = EDGE_CURVE ( 'NONE', #71510, #217161, #39365, .T. ) ;
#78523 = DIRECTION ( 'NONE',  ( -1.000000000000000000, -0.000000000000000000, -0.000000000000000000 ) ) ;
#78525 = CIRCLE ( 'NONE', #91197, 0.09999999999998898659 ) ;
#78526 = EDGE_LOOP ( 'NONE', ( #232791, #126836 ) ) ;
#78527 = CARTESIAN_POINT ( 'NONE',  ( 18.59999999999999787, 80.78317333349157536, -192.9003134612049166 ) ) ;
#78529 = ORIENTED_EDGE ( 'NONE', *, *, #52296, .T. ) ;
#78528 = FACE_OUTER_BOUND ( 'NONE', #244075, .T. ) ;
#78530 = CARTESIAN_POINT ( 'NONE',  ( 22.49544290803761015, 11.74987023785715756, 0.06531195925763526311 ) ) ;
#78531 = AXIS2_PLACEMENT_3D ( 'NONE', #88469, #7691, #71528 ) ;
#78532 = DIRECTION ( 'NONE',  ( 0.000000000000000000, 1.000000000000000000, 0.000000000000000000 ) ) ;
#78534 = CARTESIAN_POINT ( 'NONE',  ( -18.50000000000000000, -1.866714910046153308, -112.2526752462820525 ) ) ;
#78533 = DIRECTION ( 'NONE',  ( 1.000000000000000000, 0.000000000000000000, 0.000000000000000000 ) ) ;
#78535 = EDGE_CURVE ( 'NONE', #226308, #199740, #143022, .T. ) ;
#78536 = ORIENTED_EDGE ( 'NONE', *, *, #16654, .T. ) ;
#78538 = CARTESIAN_POINT ( 'NONE',  ( 21.05000000000005400, 65.35000000001120668, -3.023107484524792277 ) ) ;
#78537 = LINE ( 'NONE', #158136, #92630 ) ;
#78539 = CARTESIAN_POINT ( 'NONE',  ( -18.50000000000000000, 77.13501884592184865, -61.80613060109197932 ) ) ;
#78540 = CARTESIAN_POINT ( 'NONE',  ( 12.25000000000000000, 9.350000000011140955, -117.2500000000000284 ) ) ;
#78541 = CARTESIAN_POINT ( 'NONE',  ( -18.51024323315077424, 10.31104185824062469, -139.5204516983106089 ) ) ;
#78542 = ORIENTED_EDGE ( 'NONE', *, *, #176439, .F. ) ;
#78543 = DIRECTION ( 'NONE',  ( 0.000000000000000000, 0.000000000000000000, 1.000000000000000000 ) ) ;
#78544 = EDGE_CURVE ( 'NONE', #173746, #182849, #1574, .T. ) ;
#78545 = AXIS2_PLACEMENT_3D ( 'NONE', #74414, #35293, #56069 ) ;
#78546 = ORIENTED_EDGE ( 'NONE', *, *, #204635, .F. ) ;
#78547 = EDGE_CURVE ( 'NONE', #17884, #64483, #159812, .T. ) ;
#78548 = EDGE_CURVE ( 'NONE', #245009, #70573, #237541, .T. ) ;
#78549 = DIRECTION ( 'NONE',  ( 0.000000000000000000, -1.000000000000000000, -6.352154140967427193E-15 ) ) ;
#78550 = CIRCLE ( 'NONE', #95126, 0.1000000000000028644 ) ;
#78551 = VERTEX_POINT ( 'NONE', #238822 ) ;
#78552 = CARTESIAN_POINT ( 'NONE',  ( -23.15000000000000213, -4.735542975717121905, -233.2463119243910796 ) ) ;
#78553 = ORIENTED_EDGE ( 'NONE', *, *, #76952, .T. ) ;
#78554 = VECTOR ( 'NONE', #50847, 1000.000000000000114 ) ;
#78555 = DIRECTION ( 'NONE',  ( -0.000000000000000000, -0.9910827722268049644, -0.1332476588733589318 ) ) ;
#78556 = CIRCLE ( 'NONE', #157722, 0.1000000000000028644 ) ;
#78557 = VECTOR ( 'NONE', #245227, 1000.000000000000000 ) ;
#78558 = CIRCLE ( 'NONE', #170192, 0.09999999999999939493 ) ;
#78559 = DIRECTION ( 'NONE',  ( 1.000000000000000000, -7.136802563874199107E-16, -1.554319503706929991E-16 ) ) ;
#78560 = VERTEX_POINT ( 'NONE', #160598 ) ;
#78561 = ADVANCED_FACE ( 'NONE', ( #18491 ), #120196, .T. ) ;
#78562 = VECTOR ( 'NONE', #27782, 1000.000000000000000 ) ;
#78563 = CARTESIAN_POINT ( 'NONE',  ( -22.45305610364635385, 76.10085836911078161, -114.7726746080137019 ) ) ;
#78564 = CARTESIAN_POINT ( 'NONE',  ( -23.15000000000000213, -8.999999999988844479, -124.1060308773475924 ) ) ;
#78565 = FACE_OUTER_BOUND ( 'NONE', #43788, .T. ) ;
#78566 = CYLINDRICAL_SURFACE ( 'NONE', #47551, 12.87500000000000533 ) ;
#78567 = CARTESIAN_POINT ( 'NONE',  ( -21.05000000000000071, -1.162701749926853712, -74.90000000000004832 ) ) ;
#78568 = DIRECTION ( 'NONE',  ( 1.000000000000000000, 0.000000000000000000, 0.000000000000000000 ) ) ;
#78569 = VERTEX_POINT ( 'NONE', #21085 ) ;
#78571 = CIRCLE ( 'NONE', #173921, 4.049999999999998046 ) ;
#78570 = DIRECTION ( 'NONE',  ( -1.000000000000000000, 0.000000000000000000, 0.000000000000000000 ) ) ;
#78572 = AXIS2_PLACEMENT_3D ( 'NONE', #58925, #258, #156810 ) ;
#78573 = VERTEX_POINT ( 'NONE', #58868 ) ;
#78575 = EDGE_LOOP ( 'NONE', ( #211923, #1935, #104532, #102647 ) ) ;
#78574 = DIRECTION ( 'NONE',  ( -1.000000000000000000, 0.000000000000000000, -0.000000000000000000 ) ) ;
#78576 = EDGE_LOOP ( 'NONE', ( #105955, #169772, #155908, #257469 ) ) ;
#78577 = CARTESIAN_POINT ( 'NONE',  ( -18.40000000000000213, 33.85569253519368260, -235.0339796035492554 ) ) ;
#78578 = CARTESIAN_POINT ( 'NONE',  ( -16.27683809663750480, 51.95542581965366935, -232.4531498054797680 ) ) ;
#78579 = CARTESIAN_POINT ( 'NONE',  ( 13.12220780326570768, 66.56936653093980283, -188.2913416897004026 ) ) ;
#78580 = CARTESIAN_POINT ( 'NONE',  ( 20.05000000000002913, 68.75000000001222134, -149.1731074845244223 ) ) ;
#78581 = FACE_OUTER_BOUND ( 'NONE', #215075, .T. ) ;
#78582 = ORIENTED_EDGE ( 'NONE', *, *, #126822, .F. ) ;
#78583 = CARTESIAN_POINT ( 'NONE',  ( 23.15000000000000213, -8.895340756380869962, -215.3721227669300049 ) ) ;
#78584 = CARTESIAN_POINT ( 'NONE',  ( 21.00000000000000000, 9.750000000011153745, -188.6499999999999488 ) ) ;
#78585 = EDGE_LOOP ( 'NONE', ( #195060, #45851, #45870, #106946, #187508 ) ) ;
#78587 = VERTEX_POINT ( 'NONE', #82279 ) ;
#78586 = CYLINDRICAL_SURFACE ( 'NONE', #163422, 0.09999999999999939493 ) ;
#78588 = AXIS2_PLACEMENT_3D ( 'NONE', #41486, #75489, #155027 ) ;
#78589 = DIRECTION ( 'NONE',  ( -1.836970198721029934E-16, -1.000000000000000000, -6.982962677686266711E-15 ) ) ;
#78590 = EDGE_CURVE ( 'NONE', #203482, #152525, #101168, .T. ) ;
#78591 = CIRCLE ( 'NONE', #253383, 4.000000000000003553 ) ;
#78592 = CARTESIAN_POINT ( 'NONE',  ( -16.93710578446423654, 9.950000000011137047, -79.91880398379943529 ) ) ;
#78593 = VERTEX_POINT ( 'NONE', #100555 ) ;
#78594 = EDGE_CURVE ( 'NONE', #44321, #121991, #161875, .T. ) ;
#78595 = AXIS2_PLACEMENT_3D ( 'NONE', #159926, #63354, #140321 ) ;
#78596 = LINE ( 'NONE', #81154, #50684 ) ;
#78597 = VERTEX_POINT ( 'NONE', #221792 ) ;
#78598 = FACE_OUTER_BOUND ( 'NONE', #74941, .T. ) ;
#78599 = ADVANCED_FACE ( 'NONE', ( #138403 ), #205569, .F. ) ;
#78600 = DIRECTION ( 'NONE',  ( -1.000000000000000000, -0.000000000000000000, -0.000000000000000000 ) ) ;
#78601 = CARTESIAN_POINT ( 'NONE',  ( 12.42718393586865844, 66.62934494888806114, -51.99728422854352772 ) ) ;
#78602 = CARTESIAN_POINT ( 'NONE',  ( -21.05000000000000071, -11.39257802169451139, -97.42605042016811012 ) ) ;
#78603 = AXIS2_PLACEMENT_3D ( 'NONE', #221535, #122480, #83305 ) ;
#78604 = AXIS2_PLACEMENT_3D ( 'NONE', #133049, #215139, #177333 ) ;
#78605 = VECTOR ( 'NONE', #21309, 1000.000000000000114 ) ;
#78606 = EDGE_CURVE ( 'NONE', #241009, #87006, #197217, .T. ) ;
#78607 = ORIENTED_EDGE ( 'NONE', *, *, #96709, .T. ) ;
#78608 = CARTESIAN_POINT ( 'NONE',  ( -21.45000000000000284, 68.29142135624881860, -48.37310748452437537 ) ) ;
#78609 = ORIENTED_EDGE ( 'NONE', *, *, #113244, .T. ) ;
#78610 = CYLINDRICAL_SURFACE ( 'NONE', #143559, 0.5000000000000004441 ) ;
#78611 = CARTESIAN_POINT ( 'NONE',  ( 20.94999999999999574, 6.350000000011161383, -177.3438220896831012 ) ) ;
#78613 = ORIENTED_EDGE ( 'NONE', *, *, #5494, .F. ) ;
#78612 = CARTESIAN_POINT ( 'NONE',  ( 18.39999999999999858, -9.599999999988845900, -73.60018939122203108 ) ) ;
#78614 = FACE_OUTER_BOUND ( 'NONE', #205888, .T. ) ;
#78615 = DIRECTION ( 'NONE',  ( 1.000000000000000000, -0.000000000000000000, -0.000000000000000000 ) ) ;
#78616 = DIRECTION ( 'NONE',  ( 1.000000000000000000, 0.000000000000000000, -0.000000000000000000 ) ) ;
#78617 = FACE_OUTER_BOUND ( 'NONE', #14479, .T. ) ;
#78618 = AXIS2_PLACEMENT_3D ( 'NONE', #31169, #153703, #110664 ) ;
#78619 = CARTESIAN_POINT ( 'NONE',  ( -18.59999999999999787, 7.783179459866048866, -245.3643104511423303 ) ) ;
#78620 = LINE ( 'NONE', #159464, #257147 ) ;
#78622 = ORIENTED_EDGE ( 'NONE', *, *, #236403, .T. ) ;
#78621 = DIRECTION ( 'NONE',  ( 0.000000000000000000, -0.9770955615652966442, -0.2128009952265203508 ) ) ;
#78623 = EDGE_CURVE ( 'NONE', #172615, #170111, #72335, .T. ) ;
#78624 = FACE_OUTER_BOUND ( 'NONE', #14730, .T. ) ;
#78625 = ORIENTED_EDGE ( 'NONE', *, *, #245447, .F. ) ;
#78626 = ORIENTED_EDGE ( 'NONE', *, *, #110116, .F. ) ;
#78627 = CYLINDRICAL_SURFACE ( 'NONE', #65874, 0.1000000000000028644 ) ;
#78628 = CARTESIAN_POINT ( 'NONE',  ( -18.45037301276614272, 85.49020044755479830, -196.5104333481092453 ) ) ;
#78629 = ORIENTED_EDGE ( 'NONE', *, *, #60875, .F. ) ;
#78630 = ADVANCED_FACE ( 'NONE', ( #148721 ), #151446, .F. ) ;
#78631 = DIRECTION ( 'NONE',  ( 0.000000000000000000, -0.9908441862701596881, 0.1350103645451904977 ) ) ;
#78632 = EDGE_CURVE ( 'NONE', #7235, #249899, #164427, .T. ) ;
#78633 = DIRECTION ( 'NONE',  ( -1.000000000000000000, 0.000000000000000000, 0.000000000000000000 ) ) ;
#78634 = CIRCLE ( 'NONE', #187020, 0.09999999999999939493 ) ;
#78635 = ORIENTED_EDGE ( 'NONE', *, *, #202166, .T. ) ;
#78636 = AXIS2_PLACEMENT_3D ( 'NONE', #202629, #64413, #86503 ) ;
#78637 = CARTESIAN_POINT ( 'NONE',  ( -18.50000000000000000, 11.75000000001115552, -45.65000000000000568 ) ) ;
#78638 = CARTESIAN_POINT ( 'NONE',  ( -16.94309007106720699, 66.00777380744260370, -190.9173162019689300 ) ) ;
#78639 = EDGE_CURVE ( 'NONE', #86831, #137609, #52827, .T. ) ;
#78640 = EDGE_LOOP ( 'NONE', ( #23590, #253824, #85168 ) ) ;
#78641 = AXIS2_PLACEMENT_3D ( 'NONE', #176645, #35849, #140039 ) ;
#78642 = CARTESIAN_POINT ( 'NONE',  ( 20.94999999999999574, -1.162701749926853712, -142.1000000000000227 ) ) ;
#78643 = ORIENTED_EDGE ( 'NONE', *, *, #24997, .T. ) ;
#78644 = CARTESIAN_POINT ( 'NONE',  ( -16.94225986326250677, 9.950000000011138823, -46.44671937560789132 ) ) ;
#78646 = VERTEX_POINT ( 'NONE', #87433 ) ;
#78645 = DIRECTION ( 'NONE',  ( 1.000000000000000000, 0.000000000000000000, 0.000000000000000000 ) ) ;
#78647 = ADVANCED_FACE ( 'NONE', ( #245249 ), #147421, .F. ) ;
#78648 = ADVANCED_FACE ( 'NONE', ( #167023 ), #242994, .T. ) ;
#78649 = LINE ( 'NONE', #82485, #23576 ) ;
#78650 = ORIENTED_EDGE ( 'NONE', *, *, #128636, .F. ) ;
#78651 = DIRECTION ( 'NONE',  ( -1.000000000000000000, -0.000000000000000000, 0.000000000000000000 ) ) ;
#78652 = AXIS2_PLACEMENT_3D ( 'NONE', #20021, #99506, #57820 ) ;
#78653 = AXIS2_PLACEMENT_3D ( 'NONE', #22351, #226943, #101830 ) ;
#78654 = ORIENTED_EDGE ( 'NONE', *, *, #65047, .T. ) ;
#78656 = EDGE_LOOP ( 'NONE', ( #225888, #254833, #227196, #169943 ) ) ;
#78655 = ORIENTED_EDGE ( 'NONE', *, *, #38809, .T. ) ;
#78658 = LINE ( 'NONE', #215606, #248555 ) ;
#78657 = CIRCLE ( 'NONE', #107712, 1.749999999999998002 ) ;
#78659 = ADVANCED_FACE ( 'NONE', ( #65311 ), #14078, .F. ) ;
#78660 = ORIENTED_EDGE ( 'NONE', *, *, #70581, .T. ) ;
#78661 = FACE_OUTER_BOUND ( 'NONE', #114009, .T. ) ;
#78662 = ORIENTED_EDGE ( 'NONE', *, *, #52501, .T. ) ;
#78663 = ORIENTED_EDGE ( 'NONE', *, *, #133033, .F. ) ;
#78664 = DIRECTION ( 'NONE',  ( 1.000000000000000000, 0.000000000000000000, 0.000000000000000000 ) ) ;
#78665 = EDGE_CURVE ( 'NONE', #77589, #102370, #34740, .T. ) ;
#78666 = CARTESIAN_POINT ( 'NONE',  ( -20.94999999999999929, 46.45388641681647357, -243.1520440498138385 ) ) ;
#78668 = EDGE_LOOP ( 'NONE', ( #232420, #141154, #146718 ) ) ;
#78667 = CARTESIAN_POINT ( 'NONE',  ( -18.50000000000000000, 11.65000000001115232, -167.5999999999999659 ) ) ;
#78669 = CARTESIAN_POINT ( 'NONE',  ( 21.14999999999999858, 6.540656951712400691, -167.4999999999999716 ) ) ;
#78670 = ORIENTED_EDGE ( 'NONE', *, *, #175416, .F. ) ;
#78671 = CARTESIAN_POINT ( 'NONE',  ( 18.39999999999999858, 38.03205796367814173, -261.1772988674111957 ) ) ;
#78672 = CARTESIAN_POINT ( 'NONE',  ( 22.39999999999999503, -1.560176095955058129, -193.3663837337745122 ) ) ;
#78673 = ORIENTED_EDGE ( 'NONE', *, *, #181449, .F. ) ;
#78674 = DIRECTION ( 'NONE',  ( 0.000000000000000000, 0.000000000000000000, -1.000000000000000000 ) ) ;
#78675 = DIRECTION ( 'NONE',  ( 1.000000000000000000, 0.000000000000000000, 0.000000000000000000 ) ) ;
#78676 = ORIENTED_EDGE ( 'NONE', *, *, #125494, .T. ) ;
#78677 = DIRECTION ( 'NONE',  ( 0.000000000000000000, 0.9274965247785529332, -0.3738317757009255171 ) ) ;
#78678 = ORIENTED_EDGE ( 'NONE', *, *, #14285, .F. ) ;
#78679 = CIRCLE ( 'NONE', #249401, 7.800000000000001599 ) ;
#78680 = ORIENTED_EDGE ( 'NONE', *, *, #224172, .F. ) ;
#78681 = AXIS2_PLACEMENT_3D ( 'NONE', #129256, #125410, #9300 ) ;
#78682 = CARTESIAN_POINT ( 'NONE',  ( 23.14999999999999858, 6.650000000011155876, -79.35000000000005116 ) ) ;
#78683 = ORIENTED_EDGE ( 'NONE', *, *, #153621, .T. ) ;
#78684 = ORIENTED_EDGE ( 'NONE', *, *, #155743, .F. ) ;
#78685 = CARTESIAN_POINT ( 'NONE',  ( -21.04999999999999716, -0.08574093702224233615, -127.5861737111870440 ) ) ;
#78686 = DIRECTION ( 'NONE',  ( 1.000000000000000000, 0.000000000000000000, 0.000000000000000000 ) ) ;
#78687 = ORIENTED_EDGE ( 'NONE', *, *, #206140, .T. ) ;
#78688 = AXIS2_PLACEMENT_3D ( 'NONE', #224671, #184268, #66895 ) ;
#78689 = ORIENTED_EDGE ( 'NONE', *, *, #125498, .F. ) ;
#78690 = CARTESIAN_POINT ( 'NONE',  ( 21.05000000000000071, 64.35000000001146248, -43.03791325517834565 ) ) ;
#78691 = CARTESIAN_POINT ( 'NONE',  ( 21.14999999999999858, 69.74218538953583391, -103.1208977758331571 ) ) ;
#78692 = ORIENTED_EDGE ( 'NONE', *, *, #57577, .F. ) ;
#78693 = EDGE_LOOP ( 'NONE', ( #148559, #40314, #147828, #218413 ) ) ;
#78694 = AXIS2_PLACEMENT_3D ( 'NONE', #110879, #186581, #185285 ) ;
#78696 = ORIENTED_EDGE ( 'NONE', *, *, #115041, .T. ) ;
#78695 = AXIS2_PLACEMENT_3D ( 'NONE', #228931, #30751, #93254 ) ;
#78697 = EDGE_CURVE ( 'NONE', #128006, #56398, #217700, .T. ) ;
#78698 = CIRCLE ( 'NONE', #3897, 0.1000000000000032391 ) ;
#78699 = CARTESIAN_POINT ( 'NONE',  ( 21.05000000000000071, 69.69548367074820305, -203.5020041764652774 ) ) ;
#78700 = EDGE_CURVE ( 'NONE', #20887, #109, #105603, .T. ) ;
#78701 = CARTESIAN_POINT ( 'NONE',  ( -16.77779411440718249, 14.15241369799481674, -219.2431438278712221 ) ) ;
#78702 = DIRECTION ( 'NONE',  ( 1.000000000000000000, -0.000000000000000000, -0.000000000000000000 ) ) ;
#78703 = AXIS2_PLACEMENT_3D ( 'NONE', #100570, #183994, #64048 ) ;
#78705 = CIRCLE ( 'NONE', #12125, 0.5000000000000007772 ) ;
#78704 = CARTESIAN_POINT ( 'NONE',  ( 20.94999999999999929, 65.52661458509942349, -162.4444530202758870 ) ) ;
#78706 = FACE_OUTER_BOUND ( 'NONE', #128027, .T. ) ;
#78707 = DIRECTION ( 'NONE',  ( 1.000000000000000000, -0.000000000000000000, -0.000000000000000000 ) ) ;
#78708 = ADVANCED_FACE ( 'NONE', ( #127867 ), #9768, .T. ) ;
#78710 = DIRECTION ( 'NONE',  ( 0.000000000000000000, 0.000000000000000000, -1.000000000000000000 ) ) ;
#78709 = CARTESIAN_POINT ( 'NONE',  ( -16.81744102076748959, 66.05000000001224691, -149.1731074845244223 ) ) ;
#78712 = ADVANCED_FACE ( 'NONE', ( #64031 ), #247803, .T. ) ;
#78711 = FACE_OUTER_BOUND ( 'NONE', #130310, .T. ) ;
#78713 = CARTESIAN_POINT ( 'NONE',  ( -16.82542659449979894, 23.05416925116509930, -230.9934129395686568 ) ) ;
#78714 = AXIS2_PLACEMENT_3D ( 'NONE', #41415, #40141, #257815 ) ;
#78715 = DIRECTION ( 'NONE',  ( -0.000000000000000000, -0.000000000000000000, 1.000000000000000000 ) ) ;
#78716 = DIRECTION ( 'NONE',  ( 0.000000000000000000, -0.9594490217226103734, -0.2818822000686205254 ) ) ;
#78717 = ORIENTED_EDGE ( 'NONE', *, *, #140223, .F. ) ;
#78718 = AXIS2_PLACEMENT_3D ( 'NONE', #12751, #113109, #251320 ) ;
#78719 = VECTOR ( 'NONE', #127630, 1000.000000000000114 ) ;
#78720 = AXIS2_PLACEMENT_3D ( 'NONE', #66588, #109537, #146105 ) ;
#78721 = AXIS2_PLACEMENT_3D ( 'NONE', #89958, #70447, #91261 ) ;
#78723 = VERTEX_POINT ( 'NONE', #49604 ) ;
#78722 = DIRECTION ( 'NONE',  ( 1.000000000000000000, 0.000000000000000000, -0.000000000000000000 ) ) ;
#78724 = ADVANCED_FACE ( 'NONE', ( #129150 ), #103141, .T. ) ;
#78725 = CIRCLE ( 'NONE', #178558, 0.1000000000000013933 ) ;
#78726 = DIRECTION ( 'NONE',  ( -3.265361837132813093E-16, -1.000000000000000000, -1.156482317317891801E-14 ) ) ;
#78727 = EDGE_CURVE ( 'NONE', #23626, #224235, #76387, .T. ) ;
#78728 = ORIENTED_EDGE ( 'NONE', *, *, #59514, .F. ) ;
#78729 =( NAMED_UNIT ( * ) PLANE_ANGLE_UNIT ( ) SI_UNIT ( $, .RADIAN. ) );
#78730 = PRODUCT_RELATED_PRODUCT_CATEGORY ( 'part', '', ( #86733 ) ) ;
#78731 = DIRECTION ( 'NONE',  ( 0.000000000000000000, -7.086529944415894657E-15, 1.000000000000000000 ) ) ;
#78732 = PRODUCT_DEFINITION_SHAPE ( 'NONE', 'NONE',  #258134 ) ;
#78733 = FACE_OUTER_BOUND ( 'NONE', #213536, .T. ) ;
#78734 = AXIS2_PLACEMENT_3D ( 'NONE', #236650, #20194, #160989 ) ;
#78735 = ORIENTED_EDGE ( 'NONE', *, *, #30628, .T. ) ;
#78736 = CARTESIAN_POINT ( 'NONE',  ( -18.50000000000000000, 10.29288807859935950, -206.4580020160121592 ) ) ;
#78737 = DIRECTION ( 'NONE',  ( -0.000000000000000000, -6.982962677686266711E-15, 1.000000000000000000 ) ) ;
#78738 = FACE_OUTER_BOUND ( 'NONE', #53350, .T. ) ;
#78739 = EDGE_CURVE ( 'NONE', #236886, #238413, #122209, .T. ) ;
#78740 = EDGE_CURVE ( 'NONE', #148485, #181336, #152593, .T. ) ;
#78741 = LINE ( 'NONE', #158336, #186845 ) ;
#78743 = EDGE_LOOP ( 'NONE', ( #12453, #212063, #14666, #69619 ) ) ;
#78742 = CARTESIAN_POINT ( 'NONE',  ( 23.24999999999999289, 69.35000000001186038, -90.67310748452435121 ) ) ;
#78744 = EDGE_CURVE ( 'NONE', #32909, #68228, #151294, .T. ) ;
#78746 = ORIENTED_EDGE ( 'NONE', *, *, #161785, .T. ) ;
#78745 = CARTESIAN_POINT ( 'NONE',  ( -18.50000000000000000, 9.350000000000001421, -12.34999999999999964 ) ) ;
#78747 = AXIS2_PLACEMENT_3D ( 'NONE', #191746, #193007, #92594 ) ;
#78748 = DIRECTION ( 'NONE',  ( -0.000000000000000000, 1.000000000000000000, 6.352154140967427193E-15 ) ) ;
#78749 = CARTESIAN_POINT ( 'NONE',  ( 21.07888907270776002, 10.72506921351522102, -12.22119358683319135 ) ) ;
#78750 = CARTESIAN_POINT ( 'NONE',  ( -20.54999999999999716, 73.60000000001197407, -112.9170766071767531 ) ) ;
#78751 = AXIS2_PLACEMENT_3D ( 'NONE', #151128, #69032, #187697 ) ;
#78752 = CARTESIAN_POINT ( 'NONE',  ( -15.70407651835960650, 9.355806591641286474, -183.7911025315461018 ) ) ;
#78754 = CARTESIAN_POINT ( 'NONE',  ( -21.05000000000000071, -2.576749817950531707, -189.6385361693310756 ) ) ;
#78753 = CARTESIAN_POINT ( 'NONE',  ( -16.82542659449977762, 9.934499891438612451, -154.7553643999740416 ) ) ;
#78755 = CARTESIAN_POINT ( 'NONE',  ( -21.05000000000000426, 34.11487388478676053, -243.6629159006578504 ) ) ;
#78756 = CARTESIAN_POINT ( 'NONE',  ( -21.05000000000000071, 11.62071067812980907, -40.36841665234103260 ) ) ;
#78757 = LINE ( 'NONE', #158354, #112269 ) ;
#78758 = DIRECTION ( 'NONE',  ( -1.000000000000000000, 0.000000000000000000, -0.000000000000000000 ) ) ;
#78759 = DIRECTION ( 'NONE',  ( 1.000000000000000000, 0.000000000000000000, 0.000000000000000000 ) ) ;
#78761 = ORIENTED_EDGE ( 'NONE', *, *, #255373, .T. ) ;
#78760 = AXIS2_PLACEMENT_3D ( 'NONE', #244252, #66913, #203851 ) ;
#78762 = CARTESIAN_POINT ( 'NONE',  ( 21.04999999999999716, -0.01759718699739741543, -94.05922910633762513 ) ) ;
#78763 = EDGE_LOOP ( 'NONE', ( #77936, #233626, #151297 ) ) ;
#78764 = ORIENTED_EDGE ( 'NONE', *, *, #181141, .F. ) ;
#78765 = DIRECTION ( 'NONE',  ( 0.000000000000000000, -0.000000000000000000, 1.000000000000000000 ) ) ;
#78766 = ORIENTED_EDGE ( 'NONE', *, *, #62827, .F. ) ;
#78767 = CIRCLE ( 'NONE', #103890, 0.5000000000000004441 ) ;
#78769 = EDGE_CURVE ( 'NONE', #149519, #140456, #250374, .T. ) ;
#78768 = ORIENTED_EDGE ( 'NONE', *, *, #216551, .F. ) ;
#78770 = CIRCLE ( 'NONE', #220464, 4.300000000000025580 ) ;
#78771 =( NAMED_UNIT ( * ) PLANE_ANGLE_UNIT ( ) SI_UNIT ( $, .RADIAN. ) );
#78772 = VERTEX_POINT ( 'NONE', #252929 ) ;
#78773 = AXIS2_PLACEMENT_3D ( 'NONE', #105868, #70657, #48483 ) ;
#78774 = VERTEX_POINT ( 'NONE', #13071 ) ;
#78775 = DIRECTION ( 'NONE',  ( 0.000000000000000000, -0.5626415523514111117, 0.8267009638119422466 ) ) ;
#78776 = CARTESIAN_POINT ( 'NONE',  ( -23.25000000000000000, 10.78703865319380206, -235.6923017531418623 ) ) ;
#78777 = FACE_OUTER_BOUND ( 'NONE', #43102, .T. ) ;
#78778 = CARTESIAN_POINT ( 'NONE',  ( -20.54999999999999716, 68.85000000001254250, -182.3731074845244109 ) ) ;
#78779 = DIRECTION ( 'NONE',  ( 0.000000000000000000, 0.000000000000000000, -1.000000000000000000 ) ) ;
#78780 = EDGE_CURVE ( 'NONE', #153266, #231082, #180468, .T. ) ;
#78781 = CARTESIAN_POINT ( 'NONE',  ( 21.07946286933444213, 65.50061980461839539, -241.9434290563612535 ) ) ;
#78782 = CARTESIAN_POINT ( 'NONE',  ( 21.09107601085585770, 75.96069283529517691, -142.8869854598850111 ) ) ;
#78784 = ORIENTED_EDGE ( 'NONE', *, *, #149566, .T. ) ;
#78783 = FACE_OUTER_BOUND ( 'NONE', #81451, .T. ) ;
#78786 = CARTESIAN_POINT ( 'NONE',  ( 21.15000000000005542, 74.83745509109094485, -43.82310748452479743 ) ) ;
#78785 = DIRECTION ( 'NONE',  ( 0.000000000000000000, 0.000000000000000000, -1.000000000000000000 ) ) ;
#78787 = LINE ( 'NONE', #20137, #244185 ) ;
#78788 = VERTEX_POINT ( 'NONE', #192980 ) ;
#78789 = CARTESIAN_POINT ( 'NONE',  ( -16.90128866880176872, 63.08538694504799338, -213.1143938039259069 ) ) ;
#78791 = EDGE_CURVE ( 'NONE', #109963, #242049, #247083, .T. ) ;
#78790 = DIRECTION ( 'NONE',  ( 0.000000000000000000, 0.000000000000000000, 1.000000000000000000 ) ) ;
#78792 = ORIENTED_EDGE ( 'NONE', *, *, #31028, .F. ) ;
#78793 = DIRECTION ( 'NONE',  ( -0.7071067811865474617, 0.6824534298470372740, -0.1850873201762208153 ) ) ;
#78794 = EDGE_CURVE ( 'NONE', #73683, #35302, #22266, .T. ) ;
#78795 = CARTESIAN_POINT ( 'NONE',  ( -16.87683809663752399, 66.15000000001182912, -82.92547150272069700 ) ) ;
#78796 = CARTESIAN_POINT ( 'NONE',  ( -21.14999999999999858, 76.00000000001237765, -170.0231074845243597 ) ) ;
#78797 = ORIENTED_EDGE ( 'NONE', *, *, #5328, .F. ) ;
#78798 = EDGE_CURVE ( 'NONE', #253024, #159614, #198176, .T. ) ;
#78800 = EDGE_CURVE ( 'NONE', #165216, #120023, #114971, .T. ) ;
#78799 = DIRECTION ( 'NONE',  ( -1.000000000000000000, -3.265361837132813093E-16, 0.000000000000000000 ) ) ;
#78801 = CARTESIAN_POINT ( 'NONE',  ( -18.59999999999999787, -0.6576273345615599730, -242.5323337003318898 ) ) ;
#78802 = DIRECTION ( 'NONE',  ( 1.000000000000000000, 0.000000000000000000, 0.000000000000000000 ) ) ;
#78803 = FACE_OUTER_BOUND ( 'NONE', #97567, .T. ) ;
#78804 = EDGE_LOOP ( 'NONE', ( #190422, #222376, #149565, #198231 ) ) ;
#78805 = CARTESIAN_POINT ( 'NONE',  ( -23.25000000000000000, 87.75000000001267608, -203.5231074845243029 ) ) ;
#78806 = CYLINDRICAL_SURFACE ( 'NONE', #77429, 0.1000000000000028644 ) ;
#78807 = CIRCLE ( 'NONE', #33103, 0.1000000000000072220 ) ;
#78808 = CARTESIAN_POINT ( 'NONE',  ( -20.94999999999999929, 11.64999999999999680, -33.50000000000000000 ) ) ;
#78809 = CIRCLE ( 'NONE', #12233, 0.1000000000000013933 ) ;
#78810 = CIRCLE ( 'NONE', #70513, 11.90000000000001101 ) ;
#78811 = AXIS2_PLACEMENT_3D ( 'NONE', #106987, #224372, #7918 ) ;
#78812 = CYLINDRICAL_SURFACE ( 'NONE', #178095, 0.09999999999999939493 ) ;
#78813 = ADVANCED_FACE ( 'NONE', ( #109563 ), #249111, .T. ) ;
#78815 = EDGE_CURVE ( 'NONE', #57917, #115133, #6640, .T. ) ;
#78814 = DIRECTION ( 'NONE',  ( 0.000000000000000000, -0.4088369013363281068, 0.9126074666063770380 ) ) ;
#78817 = EDGE_LOOP ( 'NONE', ( #2058, #166241, #124849, #1891, #69504, #113165, #179404, #205889, #134391, #195478 ) ) ;
#78816 = PLANE ( 'NONE',  #179396 ) ;
#78818 = CIRCLE ( 'NONE', #87004, 0.5000000000000004441 ) ;
#78819 = DIRECTION ( 'NONE',  ( 1.836970198721029934E-16, -1.000000000000000000, -0.000000000000000000 ) ) ;
#78820 = CARTESIAN_POINT ( 'NONE',  ( -16.87401514999235275, 66.05000000001187743, -90.30312547705619863 ) ) ;
#78821 = FACE_OUTER_BOUND ( 'NONE', #254681, .T. ) ;
#78822 = DIRECTION ( 'NONE',  ( -1.000000000000000000, 0.000000000000000000, -0.000000000000000000 ) ) ;
#78823 = ADVANCED_FACE ( 'NONE', ( #50860 ), #174740, .F. ) ;
#78824 = CARTESIAN_POINT ( 'NONE',  ( 21.05000000000000071, 10.42338541492404680, -174.9920519238700649 ) ) ;
#78826 = ORIENTED_EDGE ( 'NONE', *, *, #92104, .F. ) ;
#78825 = CARTESIAN_POINT ( 'NONE',  ( -20.85000000000000142, 68.92903212821327941, -132.7765432626560766 ) ) ;
#78827 = DIRECTION ( 'NONE',  ( 0.000000000000000000, 0.9126074666063772600, 0.4088369013363274407 ) ) ;
#78828 = DIRECTION ( 'NONE',  ( 0.000000000000000000, 0.000000000000000000, -1.000000000000000000 ) ) ;
#78829 = CARTESIAN_POINT ( 'NONE',  ( -23.39999999999994529, 77.85126707825561709, -47.62635315998165453 ) ) ;
#78830 = ORIENTED_EDGE ( 'NONE', *, *, #49497, .T. ) ;
#78831 = CARTESIAN_POINT ( 'NONE',  ( 23.14999999999999858, -3.899999999999999467, -33.50000000000000000 ) ) ;
#78832 = DIRECTION ( 'NONE',  ( -1.000000000000000000, 1.646408749285563322E-14, -1.073024830501002749E-15 ) ) ;
#78833 = CARTESIAN_POINT ( 'NONE',  ( 20.12500000000000000, 52.06567329910104291, -231.9654557484363409 ) ) ;
#78834 = AXIS2_PLACEMENT_3D ( 'NONE', #105283, #162748, #6207 ) ;
#78835 = CIRCLE ( 'NONE', #24727, 0.1000000000000028644 ) ;
#78836 = EDGE_CURVE ( 'NONE', #229356, #104833, #10743, .T. ) ;
#78837 = LINE ( 'NONE', #179272, #250119 ) ;
#78838 = TOROIDAL_SURFACE ( 'NONE', #20616, 11.65000000000000036, 0.1000000000000000056 ) ;
#78839 = EDGE_CURVE ( 'NONE', #91470, #176502, #106570, .T. ) ;
#78840 = DIRECTION ( 'NONE',  ( 1.000000000000000000, 0.000000000000000000, 0.000000000000000000 ) ) ;
#78841 = DIRECTION ( 'NONE',  ( 0.000000000000000000, 0.000000000000000000, 1.000000000000000000 ) ) ;
#78842 = AXIS2_PLACEMENT_3D ( 'NONE', #58871, #135848, #115023 ) ;
#78843 = EDGE_LOOP ( 'NONE', ( #93838, #51407, #147754, #169825 ) ) ;
#78844 = ORIENTED_EDGE ( 'NONE', *, *, #202030, .T. ) ;
#78845 = CARTESIAN_POINT ( 'NONE',  ( -18.37160782347004329, 64.52438358520993233, -160.7731074845244450 ) ) ;
#78846 = LINE ( 'NONE', #243073, #178985 ) ;
#78847 = CARTESIAN_POINT ( 'NONE',  ( 18.39999999999999503, 70.35000000001201670, -115.6731074845243370 ) ) ;
#78848 = CARTESIAN_POINT ( 'NONE',  ( -18.50000000000000000, 11.65000000001115232, -33.60000000000000142 ) ) ;
#78849 = EDGE_LOOP ( 'NONE', ( #103945, #146080, #220368, #243241, #158072 ) ) ;
#78850 = ADVANCED_FACE ( 'NONE', ( #113432 ), #14362, .T. ) ;
#78851 = EDGE_CURVE ( 'NONE', #32455, #212713, #252322, .T. ) ;
#78852 = CARTESIAN_POINT ( 'NONE',  ( -21.14999999999999858, 76.00000000001200817, -109.5637644362255543 ) ) ;
#78853 = FACE_OUTER_BOUND ( 'NONE', #57622, .T. ) ;
#78854 = DIRECTION ( 'NONE',  ( 0.000000000000000000, 0.000000000000000000, 1.000000000000000000 ) ) ;
#78856 = CARTESIAN_POINT ( 'NONE',  ( -18.59999999999999787, 64.35000000001222986, -148.2731074845243882 ) ) ;
#78855 = CIRCLE ( 'NONE', #8161, 3.900000000000000799 ) ;
#78857 = VERTEX_POINT ( 'NONE', #189119 ) ;
#78858 = LINE ( 'NONE', #256166, #48616 ) ;
#78859 = EDGE_LOOP ( 'NONE', ( #54865, #96950, #61068, #235088 ) ) ;
#78860 = CARTESIAN_POINT ( 'NONE',  ( -21.05000000000000071, 11.75000000001115552, -93.65839931010299324 ) ) ;
#78861 = EDGE_LOOP ( 'NONE', ( #9325, #79011, #12351, #230121 ) ) ;
#78862 = CARTESIAN_POINT ( 'NONE',  ( 18.79999999999999716, -1.885425182446133885, -11.49641995933507843 ) ) ;
#78863 = DIRECTION ( 'NONE',  ( 0.000000000000000000, -2.775557561562888827E-14, 1.000000000000000000 ) ) ;
#78864 = LINE ( 'NONE', #119307, #58142 ) ;
#78865 = AXIS2_PLACEMENT_3D ( 'NONE', #156743, #236241, #39361 ) ;
#78866 = ORIENTED_EDGE ( 'NONE', *, *, #153507, .F. ) ;
#78867 = CARTESIAN_POINT ( 'NONE',  ( -20.54999999999999716, 62.24653955602229871, -247.9500786234238490 ) ) ;
#78868 = CARTESIAN_POINT ( 'NONE',  ( -18.50000000000000000, 0.7653315920341953182, -212.6731560895497353 ) ) ;
#78869 = ORIENTED_EDGE ( 'NONE', *, *, #222209, .F. ) ;
#78870 = CARTESIAN_POINT ( 'NONE',  ( -12.25000000000000533, 9.350000000011133849, -150.8657431672739335 ) ) ;
#78872 = ORIENTED_EDGE ( 'NONE', *, *, #134930, .F. ) ;
#78871 = DIRECTION ( 'NONE',  ( 0.000000000000000000, 1.224646799147353207E-16, 1.000000000000000000 ) ) ;
#78873 = CARTESIAN_POINT ( 'NONE',  ( -18.59999999999999787, 12.80863705670246411, -205.3010250813005655 ) ) ;
#78874 = DIRECTION ( 'NONE',  ( -0.000000000000000000, 1.000000000000000000, -0.000000000000000000 ) ) ;
#78875 = AXIS2_PLACEMENT_3D ( 'NONE', #233490, #92665, #109652 ) ;
#78876 = EDGE_CURVE ( 'NONE', #94985, #111525, #10488, .T. ) ;
#78877 = AXIS2_PLACEMENT_3D ( 'NONE', #25050, #8040, #147538 ) ;
#78878 = EDGE_LOOP ( 'NONE', ( #238639, #250538, #226544, #75147 ) ) ;
#78879 = CARTESIAN_POINT ( 'NONE',  ( 20.95512820512820440, 65.37615131630072085, -191.3731074845244393 ) ) ;
#78880 = CARTESIAN_POINT ( 'NONE',  ( 20.85000000000000142, 11.65000000001115943, -67.00000000000000000 ) ) ;
#78881 = ORIENTED_EDGE ( 'NONE', *, *, #172998, .F. ) ;
#78882 = FACE_OUTER_BOUND ( 'NONE', #35998, .T. ) ;
#78883 = CARTESIAN_POINT ( 'NONE',  ( 13.54577453029515688, 49.62720671425051933, -233.3859273903070459 ) ) ;
#78884 = DIRECTION ( 'NONE',  ( 0.000000000000000000, 0.8814952561688431665, -0.4721928772777346794 ) ) ;
#78885 = AXIS2_PLACEMENT_3D ( 'NONE', #246530, #190440, #11809 ) ;
#78886 = CIRCLE ( 'NONE', #124713, 0.1000000000000008799 ) ;
#78887 = ORIENTED_EDGE ( 'NONE', *, *, #239545, .F. ) ;
#78888 = EDGE_CURVE ( 'NONE', #196430, #245420, #240765, .T. ) ;
#78889 = VERTEX_POINT ( 'NONE', #239480 ) ;
#78890 = CIRCLE ( 'NONE', #212216, 0.1000000000000028644 ) ;
#78891 = AXIS2_PLACEMENT_3D ( 'NONE', #217410, #19228, #233170 ) ;
#78892 = AXIS2_PLACEMENT_3D ( 'NONE', #136146, #16265, #39681 ) ;
#78893 = AXIS2_PLACEMENT_3D ( 'NONE', #7551, #51793, #171799 ) ;
#78894 = ORIENTED_EDGE ( 'NONE', *, *, #70054, .F. ) ;
#78895 = CARTESIAN_POINT ( 'NONE',  ( -18.59999999999999787, 77.83585931145570669, -125.0186683157258045 ) ) ;
#78896 = CARTESIAN_POINT ( 'NONE',  ( -16.87036670365548474, 66.01058118071090064, -182.5435473672224020 ) ) ;
#78898 = ORIENTED_EDGE ( 'NONE', *, *, #115659, .T. ) ;
#78897 = CARTESIAN_POINT ( 'NONE',  ( 18.49999999999999289, 6.846123162352588665, -37.23772626684986164 ) ) ;
#78899 = DIRECTION ( 'NONE',  ( 0.7071067811865475727, 0.7071067811865475727, -0.000000000000000000 ) ) ;
#78900 = CARTESIAN_POINT ( 'NONE',  ( -18.50000000000000000, 61.43991280424057777, -221.4883200034892923 ) ) ;
#78901 = PLANE ( 'NONE',  #33917 ) ;
#78902 = DIRECTION ( 'NONE',  ( 1.000000000000000000, 0.000000000000000000, 0.000000000000000000 ) ) ;
#78903 = DIRECTION ( 'NONE',  ( 1.000000000000000000, 0.000000000000000000, 0.000000000000000000 ) ) ;
#78904 = DIRECTION ( 'NONE',  ( 0.000000000000000000, 0.2617529984164506107, 0.9651348961777299618 ) ) ;
#78906 = ORIENTED_EDGE ( 'NONE', *, *, #115777, .F. ) ;
#78905 = FACE_OUTER_BOUND ( 'NONE', #175556, .T. ) ;
#78908 = ORIENTED_EDGE ( 'NONE', *, *, #237705, .F. ) ;
#78907 = CARTESIAN_POINT ( 'NONE',  ( 21.14999999999999858, 76.10000000001166143, -69.52310748452431710 ) ) ;
#78909 = CYLINDRICAL_SURFACE ( 'NONE', #162085, 0.09999999999999939493 ) ;
#78910 = VERTEX_POINT ( 'NONE', #221175 ) ;
#78911 = EDGE_LOOP ( 'NONE', ( #195311, #211025, #66629, #135549 ) ) ;
#78912 = LINE ( 'NONE', #80187, #101495 ) ;
#78913 = CIRCLE ( 'NONE', #199774, 0.09999999999999939493 ) ;
#78914 = DIRECTION ( 'NONE',  ( -1.000000000000000000, 6.239415780002328221E-16, 5.674754385112861898E-16 ) ) ;
#78915 = DIRECTION ( 'NONE',  ( 0.000000000000000000, 0.8814952561688437216, -0.4721928772777334582 ) ) ;
#78916 = CARTESIAN_POINT ( 'NONE',  ( -20.65000000000000568, 42.79061499530347845, -240.6131891775583824 ) ) ;
#78917 = CARTESIAN_POINT ( 'NONE',  ( -20.64999999999999858, 1.940186915899009490, -146.8291192110533530 ) ) ;
#78918 = LINE ( 'NONE', #179355, #111486 ) ;
#78919 = CIRCLE ( 'NONE', #233113, 0.4000000000000010214 ) ;
#78920 = CARTESIAN_POINT ( 'NONE',  ( 20.95512820512820085, 10.49413282287805949, -207.4737445703522383 ) ) ;
#78921 = EDGE_LOOP ( 'NONE', ( #164095, #55675, #15631, #26336 ) ) ;
#78922 = ORIENTED_EDGE ( 'NONE', *, *, #133471, .F. ) ;
#78923 = VECTOR ( 'NONE', #68640, 1000.000000000000000 ) ;
#78924 = EDGE_CURVE ( 'NONE', #73566, #69974, #34411, .T. ) ;
#78925 = B_SPLINE_CURVE_WITH_KNOTS ( 'NONE', 3,
 ( #157028, #236530, #57883, #216961, #38353, #117870, #197408, #59150, #5607, #86423 ),
 .UNSPECIFIED., .F., .F.,
 ( 4, 3, 3, 4 ),
 ( 0.000000000000000000, 1.004626015991467516E-05, 1.831183478183015626E-05, 2.062343583996046153E-05 ),
 .UNSPECIFIED. ) ;
#78926 = VERTEX_POINT ( 'NONE', #5974 ) ;
#78927 = DIRECTION ( 'NONE',  ( -0.000000000000000000, 1.265107689135680095E-16, -1.000000000000000000 ) ) ;
#78928 = DIRECTION ( 'NONE',  ( -1.000000000000000000, 2.952720810173289112E-16, 2.061873921506763405E-30 ) ) ;
#78929 = CIRCLE ( 'NONE', #220447, 0.3999999999999975797 ) ;
#78930 = CARTESIAN_POINT ( 'NONE',  ( -13.22483237240078857, 66.56332574816870817, -54.34624555352518627 ) ) ;
#78931 = DIRECTION ( 'NONE',  ( -4.239556034732056743E-17, -0.1298341882519953583, -0.9915357197604862671 ) ) ;
#78932 = EDGE_CURVE ( 'NONE', #209575, #8977, #235762, .T. ) ;
#78933 = ORIENTED_EDGE ( 'NONE', *, *, #185717, .F. ) ;
#78934 = CARTESIAN_POINT ( 'NONE',  ( 20.94999999999999574, -10.56629024491939894, -206.4738935375009703 ) ) ;
#78935 = ORIENTED_EDGE ( 'NONE', *, *, #199048, .T. ) ;
#78936 = FACE_OUTER_BOUND ( 'NONE', #213450, .T. ) ;
#78937 = ORIENTED_EDGE ( 'NONE', *, *, #51230, .F. ) ;
#78938 = EDGE_CURVE ( 'NONE', #53673, #98456, #202458, .T. ) ;
#78939 = VECTOR ( 'NONE', #39777, 1000.000000000000000 ) ;
#78940 = DIRECTION ( 'NONE',  ( -0.000000000000000000, -6.982962677686266711E-15, 1.000000000000000000 ) ) ;
#78941 = DIRECTION ( 'NONE',  ( 1.000000000000000000, 0.000000000000000000, 0.000000000000000000 ) ) ;
#78942 = AXIS2_PLACEMENT_3D ( 'NONE', #191640, #54644, #36406 ) ;
#78943 = DIRECTION ( 'NONE',  ( -1.000000000000000000, 0.000000000000000000, 0.000000000000000000 ) ) ;
#78944 = VERTEX_POINT ( 'NONE', #81640 ) ;
#78945 = DIRECTION ( 'NONE',  ( 0.000000000000000000, 0.000000000000000000, -1.000000000000000000 ) ) ;
#78946 = ADVANCED_FACE ( 'NONE', ( #60816 ), #84181, .T. ) ;
#78948 = VERTEX_POINT ( 'NONE', #123380 ) ;
#78947 = DIRECTION ( 'NONE',  ( 1.713247197920696616E-14, -0.9121259477928120862, 0.4099100576505341209 ) ) ;
#78949 = CARTESIAN_POINT ( 'NONE',  ( 23.14999999999999503, 64.35000000001249987, -177.0379132551783812 ) ) ;
#78950 = VECTOR ( 'NONE', #95729, 1000.000000000000000 ) ;
#78951 = ORIENTED_EDGE ( 'NONE', *, *, #11315, .T. ) ;
#78952 = DIRECTION ( 'NONE',  ( 1.000000000000000000, -1.186688945009010077E-16, -8.286604613020808509E-31 ) ) ;
#78953 = ORIENTED_EDGE ( 'NONE', *, *, #1009, .T. ) ;
#78954 = DIRECTION ( 'NONE',  ( -2.840903330521631775E-16, 0.8700118002898321601, -0.4930308989875230030 ) ) ;
#78955 = EDGE_CURVE ( 'NONE', #12339, #6622, #248254, .T. ) ;
#78956 = LINE ( 'NONE', #158551, #88698 ) ;
#78957 = DIRECTION ( 'NONE',  ( 0.000000000000000000, 0.000000000000000000, -1.000000000000000000 ) ) ;
#78958 = DIRECTION ( 'NONE',  ( -1.000000000000000000, 0.000000000000000000, 0.000000000000000000 ) ) ;
#78959 = CARTESIAN_POINT ( 'NONE',  ( 21.05000000000000071, 86.10439672154322466, -209.4215112426525138 ) ) ;
#78960 = ORIENTED_EDGE ( 'NONE', *, *, #202258, .T. ) ;
#78961 = DIRECTION ( 'NONE',  ( 0.000000000000000000, 0.000000000000000000, -1.000000000000000000 ) ) ;
#78962 = CARTESIAN_POINT ( 'NONE',  ( 21.14999999999999858, 6.540656951712399803, -100.5000000000000426 ) ) ;
#78963 = AXIS2_PLACEMENT_3D ( 'NONE', #115484, #82432, #136306 ) ;
#78964 = CARTESIAN_POINT ( 'NONE',  ( 18.59999999999996945, 10.33248238083634440, -139.5948465439131780 ) ) ;
#78965 = ORIENTED_EDGE ( 'NONE', *, *, #179148, .F. ) ;
#78966 = DIRECTION ( 'NONE',  ( 0.000000000000000000, 0.000000000000000000, -1.000000000000000000 ) ) ;
#78967 = VERTEX_POINT ( 'NONE', #163798 ) ;
#78968 = CARTESIAN_POINT ( 'NONE',  ( -23.15000000000000213, 24.26958830762006869, -252.6664436919618879 ) ) ;
#78969 = ORIENTED_EDGE ( 'NONE', *, *, #131929, .F. ) ;
#78970 = LINE ( 'NONE', #137672, #42930 ) ;
#78971 = CARTESIAN_POINT ( 'NONE',  ( -21.05000000000000071, 1.115600667400684642E-11, -108.4000000000000341 ) ) ;
#78973 = ORIENTED_EDGE ( 'NONE', *, *, #151761, .T. ) ;
#78972 = DIRECTION ( 'NONE',  ( 0.7071067811865127117, 0.7071067811865821007, 0.000000000000000000 ) ) ;
#78974 = CARTESIAN_POINT ( 'NONE',  ( -18.48550754432023169, 8.873758098311299136, -245.4030316389878124 ) ) ;
#78975 = EDGE_LOOP ( 'NONE', ( #174356, #117507, #20455, #174374, #92229 ) ) ;
#78976 = EDGE_CURVE ( 'NONE', #249646, #239047, #31618, .T. ) ;
#78977 = CARTESIAN_POINT ( 'NONE',  ( -23.25000000000000000, -11.64999999998884483, -100.5000000000000284 ) ) ;
#78978 = DIRECTION ( 'NONE',  ( -1.000000000000000000, -2.952720810173289112E-16, 0.000000000000000000 ) ) ;
#78979 = ORIENTED_EDGE ( 'NONE', *, *, #154194, .T. ) ;
#78980 = ORIENTED_EDGE ( 'NONE', *, *, #69943, .T. ) ;
#78981 = VECTOR ( 'NONE', #230250, 1000.000000000000000 ) ;
#78983 = AXIS2_PLACEMENT_3D ( 'NONE', #126889, #248110, #72063 ) ;
#78982 = FACE_OUTER_BOUND ( 'NONE', #50967, .T. ) ;
#78984 = DIRECTION ( 'NONE',  ( -2.915501640297153790E-16, 1.000000000000000000, 0.000000000000000000 ) ) ;
#78985 = ORIENTED_EDGE ( 'NONE', *, *, #186901, .T. ) ;
#78986 = AXIS2_PLACEMENT_3D ( 'NONE', #217080, #219659, #98392 ) ;
#78988 = DIRECTION ( 'NONE',  ( 0.000000000000000000, -0.8814952561688429444, 0.4721928772777345684 ) ) ;
#78987 = AXIS2_PLACEMENT_3D ( 'NONE', #122414, #42873, #85806 ) ;
#78989 = ORIENTED_EDGE ( 'NONE', *, *, #246951, .F. ) ;
#78990 = ORIENTED_EDGE ( 'NONE', *, *, #27637, .T. ) ;
#78991 = EDGE_CURVE ( 'NONE', #245391, #111271, #122099, .T. ) ;
#78992 = AXIS2_PLACEMENT_3D ( 'NONE', #170937, #71799, #109612 ) ;
#78993 = CARTESIAN_POINT ( 'NONE',  ( -23.30000000000000426, -11.79999999999999893, -347.0000000000001137 ) ) ;
#78994 = APPLICATION_CONTEXT ( 'automotive_design' ) ;
#78995 = ADVANCED_FACE ( 'NONE', ( #64677 ), #24296, .F. ) ;
#78997 = ORIENTED_EDGE ( 'NONE', *, *, #27254, .T. ) ;
#78996 = CYLINDRICAL_SURFACE ( 'NONE', #205456, 0.09999999999999939493 ) ;
#78998 = CARTESIAN_POINT ( 'NONE',  ( -1.820710678118657944, 85.92928932189384739, -178.7731074845243029 ) ) ;
#78999 = CIRCLE ( 'NONE', #133040, 0.09999999999999939493 ) ;
#79000 = SPHERICAL_SURFACE ( 'NONE', #123452, 0.1000000000000000056 ) ;
#79001 = DIRECTION ( 'NONE',  ( -0.000000000000000000, 1.000000000000000000, 6.982962677686266711E-15 ) ) ;
#79002 = CIRCLE ( 'NONE', #120760, 0.09999999999999939493 ) ;
#79004 = SPHERICAL_SURFACE ( 'NONE', #196821, 0.1000000000000000056 ) ;
#79003 = DIRECTION ( 'NONE',  ( -3.265361837132813093E-16, 1.000000000000000000, 0.000000000000000000 ) ) ;
#79006 = ADVANCED_FACE ( 'NONE', ( #4687 ), #202905, .T. ) ;
#79005 = CARTESIAN_POINT ( 'NONE',  ( -21.05000000000000071, 75.96824164695662773, -142.7819546076043764 ) ) ;
#79007 = CARTESIAN_POINT ( 'NONE',  ( -23.25000000000000000, 11.65000000001115588, -160.4851942293460638 ) ) ;
#79008 = CARTESIAN_POINT ( 'NONE',  ( 18.45139536634708577, 85.48608172029256025, -29.38259586671361134 ) ) ;
#79009 = CARTESIAN_POINT ( 'NONE',  ( 20.94999999999999929, 10.38178547073510316, -139.5078453638842291 ) ) ;
#79010 = AXIS2_PLACEMENT_3D ( 'NONE', #216045, #200352, #161233 ) ;
#79011 = ORIENTED_EDGE ( 'NONE', *, *, #131424, .F. ) ;
#79013 = ORIENTED_EDGE ( 'NONE', *, *, #182, .T. ) ;
#79012 = CARTESIAN_POINT ( 'NONE',  ( 23.25000000000000000, 84.59626168225457832, -60.07297996737398194 ) ) ;
#79014 = VERTEX_POINT ( 'NONE', #124666 ) ;
#79015 = CARTESIAN_POINT ( 'NONE',  ( -23.25000000000000355, 65.95000000001230944, -157.2731074845244166 ) ) ;
#79017 = EDGE_CURVE ( 'NONE', #141295, #200852, #222441, .T. ) ;
#79016 =( BOUNDED_CURVE ( )  B_SPLINE_CURVE ( 3, ( #64681, #28160, #184630, #124671 ),
 .UNSPECIFIED., .F., .F. ) 
 B_SPLINE_CURVE_WITH_KNOTS ( ( 4, 4 ),
 ( 3.141592653589791784, 4.712388980384688786 ),
 .UNSPECIFIED. ) 
 CURVE ( )  GEOMETRIC_REPRESENTATION_ITEM ( )  RATIONAL_B_SPLINE_CURVE ( ( 1.000000000000000000, 0.8047378541243649375, 0.8047378541243649375, 1.000000000000000000 ) ) 
 REPRESENTATION_ITEM ( '' )  );
#79018 = VERTEX_POINT ( 'NONE', #42543 ) ;
#79019 = CARTESIAN_POINT ( 'NONE',  ( 13.40000000000005898, 63.75000000001119815, -21.02310748452479316 ) ) ;
#79020 = ADVANCED_FACE ( 'NONE', ( #183359 ), #62126, .F. ) ;
#79021 = EDGE_CURVE ( 'NONE', #250431, #25855, #180791, .T. ) ;
#79022 = ORIENTED_EDGE ( 'NONE', *, *, #160734, .F. ) ;
#79023 = LINE ( 'NONE', #253826, #124057 ) ;
#79024 = VECTOR ( 'NONE', #236697, 1000.000000000000000 ) ;
#79026 = ORIENTED_EDGE ( 'NONE', *, *, #23764, .T. ) ;
#79025 = ORIENTED_EDGE ( 'NONE', *, *, #230278, .F. ) ;
#79027 = ORIENTED_EDGE ( 'NONE', *, *, #251473, .F. ) ;
#79028 = ORIENTED_EDGE ( 'NONE', *, *, #200889, .T. ) ;
#79029 = EDGE_CURVE ( 'NONE', #238847, #146731, #44056, .T. ) ;
#79030 = CARTESIAN_POINT ( 'NONE',  ( -20.90000000000000213, 7.973296578895943121, -1.410778198689825347 ) ) ;
#79031 = CARTESIAN_POINT ( 'NONE',  ( 23.24999999999999289, 69.55000000001223270, -148.2731074845243597 ) ) ;
#79033 = ORIENTED_EDGE ( 'NONE', *, *, #74707, .T. ) ;
#79032 = DIRECTION ( 'NONE',  ( 0.000000000000000000, -7.086529944415886769E-15, 1.000000000000000000 ) ) ;
#79034 = AXIS2_PLACEMENT_3D ( 'NONE', #14359, #252927, #233403 ) ;
#79035 = CARTESIAN_POINT ( 'NONE',  ( 20.75572585718203911, 40.78216703416070033, -237.9711013405598692 ) ) ;
#79036 = ADVANCED_FACE ( 'NONE', ( #50235 ), #26871, .F. ) ;
#79037 = DIRECTION ( 'NONE',  ( 1.000000000000000000, 0.000000000000000000, 0.000000000000000000 ) ) ;
#79039 = ORIENTED_EDGE ( 'NONE', *, *, #165458, .T. ) ;
#79038 = CARTESIAN_POINT ( 'NONE',  ( 18.50000000000000000, -4.317402351199911337, -229.8357552817742260 ) ) ;
#79040 = LINE ( 'NONE', #781, #58345 ) ;
#79042 = EDGE_CURVE ( 'NONE', #188126, #116664, #206557, .T. ) ;
#79041 = ORIENTED_EDGE ( 'NONE', *, *, #95765, .F. ) ;
#79043 = DIRECTION ( 'NONE',  ( 0.000000000000000000, 0.000000000000000000, 1.000000000000000000 ) ) ;
#79045 = ORIENTED_EDGE ( 'NONE', *, *, #48278, .F. ) ;
#79044 = CARTESIAN_POINT ( 'NONE',  ( 23.15000000000000213, 85.00000000001197975, -112.4170766071766678 ) ) ;
#79046 = DIRECTION ( 'NONE',  ( 0.000000000000000000, -0.3343365196859449662, 0.9424537609900497381 ) ) ;
#79047 = DIRECTION ( 'NONE',  ( 0.000000000000000000, 0.000000000000000000, -1.000000000000000000 ) ) ;
#79048 = CARTESIAN_POINT ( 'NONE',  ( 21.05000000000000071, 6.450000000011156587, -77.01702717044007329 ) ) ;
#79049 = ORIENTED_EDGE ( 'NONE', *, *, #21163, .T. ) ;
#79051 = DIRECTION ( 'NONE',  ( -0.000000000000000000, 1.000000000000000000, -0.000000000000000000 ) ) ;
#79050 = CARTESIAN_POINT ( 'NONE',  ( -16.77180007708461318, 9.950000000011137047, -46.13561411895483388 ) ) ;
#79052 = CARTESIAN_POINT ( 'NONE',  ( -13.11924609551135568, 66.56831044948773979, -84.74381745228834006 ) ) ;
#79053 = CIRCLE ( 'NONE', #112243, 0.1000000000000013933 ) ;
#79054 = DIRECTION ( 'NONE',  ( -0.7071067811865389130, 8.659560562355038861E-17, -0.7071067811865561215 ) ) ;
#79055 = FACE_OUTER_BOUND ( 'NONE', #184589, .T. ) ;
#79056 = DIRECTION ( 'NONE',  ( -0.000000000000000000, 0.2617529984165031243, 0.9651348961777157509 ) ) ;
#79057 = AXIS2_PLACEMENT_3D ( 'NONE', #138216, #39168, #20893 ) ;
#79058 = VERTEX_POINT ( 'NONE', #208066 ) ;
#79059 = ORIENTED_EDGE ( 'NONE', *, *, #45494, .T. ) ;
#79060 = ORIENTED_EDGE ( 'NONE', *, *, #67890, .F. ) ;
#79061 = CARTESIAN_POINT ( 'NONE',  ( 23.14999999999999858, 76.00000000001244871, -170.0231074845243597 ) ) ;
#79063 = ORIENTED_EDGE ( 'NONE', *, *, #85169, .F. ) ;
#79062 = ADVANCED_FACE ( 'NONE', ( #48964 ), #2530, .F. ) ;
#79065 = CARTESIAN_POINT ( 'NONE',  ( 23.14999999999999858, -11.74999999998883560, -21.75000000000000355 ) ) ;
#79064 = CIRCLE ( 'NONE', #87457, 0.09999999999999063804 ) ;
#79066 = ORIENTED_EDGE ( 'NONE', *, *, #185409, .F. ) ;
#79067 = EDGE_CURVE ( 'NONE', #173321, #64202, #148292, .T. ) ;
#79068 = CARTESIAN_POINT ( 'NONE',  ( 20.94999999999999574, 1.250000000011155299, -108.4000000000000341 ) ) ;
#79069 = CYLINDRICAL_SURFACE ( 'NONE', #19215, 0.09999999999999939493 ) ;
#79070 = AXIS2_PLACEMENT_3D ( 'NONE', #44830, #25284, #124378 ) ;
#79071 = AXIS2_PLACEMENT_3D ( 'NONE', #13168, #112277, #176109 ) ;
#79073 = EDGE_CURVE ( 'NONE', #32089, #142573, #185715, .T. ) ;
#79072 = ORIENTED_EDGE ( 'NONE', *, *, #75467, .T. ) ;
#79074 = LINE ( 'NONE', #16582, #52614 ) ;
#79075 = PRESENTATION_STYLE_ASSIGNMENT (( #195232 ) ) ;
#79077 = ORIENTED_EDGE ( 'NONE', *, *, #254583, .T. ) ;
#79076 = VECTOR ( 'NONE', #186923, 1000.000000000000000 ) ;
#79078 = VERTEX_POINT ( 'NONE', #191075 ) ;
#79079 = AXIS2_PLACEMENT_3D ( 'NONE', #34047, #205247, #73168 ) ;
#79080 = CIRCLE ( 'NONE', #199755, 0.09999999999999939493 ) ;
#79081 = EDGE_LOOP ( 'NONE', ( #128986, #210330, #131356, #45809, #249954, #84407, #228503 ) ) ;
#79082 = AXIS2_PLACEMENT_3D ( 'NONE', #42507, #200311, #65935 ) ;
#79083 = CIRCLE ( 'NONE', #66647, 0.09999999999999971412 ) ;
#79084 = PLANE ( 'NONE',  #75454 ) ;
#79085 = CARTESIAN_POINT ( 'NONE',  ( -18.40000000000000213, 64.66825945288736932, -182.6731074845244507 ) ) ;
#79086 = CARTESIAN_POINT ( 'NONE',  ( -20.94999999999999929, 28.60154115857408641, -258.4512230915049713 ) ) ;
#79087 = DIRECTION ( 'NONE',  ( 0.000000000000000000, 0.000000000000000000, 1.000000000000000000 ) ) ;
#79088 = DIRECTION ( 'NONE',  ( 0.000000000000000000, 0.000000000000000000, 1.000000000000000000 ) ) ;
#79089 = VECTOR ( 'NONE', #97322, 1000.000000000000000 ) ;
#79091 = FACE_OUTER_BOUND ( 'NONE', #157262, .T. ) ;
#79090 = LINE ( 'NONE', #238172, #37428 ) ;
#79092 = DIRECTION ( 'NONE',  ( -1.000000000000000000, 0.000000000000000000, 0.000000000000000000 ) ) ;
#79094 = EDGE_LOOP ( 'NONE', ( #38178, #46581, #1415, #233774 ) ) ;
#79093 = CARTESIAN_POINT ( 'NONE',  ( -18.59999999999999787, 64.35000000001259934, -191.2731074845244450 ) ) ;
#79095 = DIRECTION ( 'NONE',  ( 0.000000000000000000, -1.000000000000000000, -6.352154140967427193E-15 ) ) ;
#79096 = VERTEX_POINT ( 'NONE', #86792 ) ;
#79097 = CARTESIAN_POINT ( 'NONE',  ( -18.51991288638514277, -9.392436789662243157, -141.1432664039592169 ) ) ;
#79098 = ORIENTED_EDGE ( 'NONE', *, *, #6908, .F. ) ;
#79099 = VERTEX_POINT ( 'NONE', #107655 ) ;
#79100 = DIRECTION ( 'NONE',  ( -1.000000000000000000, 0.000000000000000000, 0.000000000000000000 ) ) ;
#79101 = CARTESIAN_POINT ( 'NONE',  ( 20.94999999999999929, 5.000000000011153745, -112.9052660189131245 ) ) ;
#79103 = ADVANCED_FACE ( 'NONE', ( #46385 ), #231507, .F. ) ;
#79102 = DIRECTION ( 'NONE',  ( -1.000000000000000000, -0.000000000000000000, -0.000000000000000000 ) ) ;
#79104 = ORIENTED_EDGE ( 'NONE', *, *, #28311, .F. ) ;
#79105 = EDGE_CURVE ( 'NONE', #51816, #60637, #181621, .T. ) ;
#79106 = DIRECTION ( 'NONE',  ( 0.000000000000000000, -0.8814952561688430555, 0.4721928772777346239 ) ) ;
#79107 = ORIENTED_EDGE ( 'NONE', *, *, #257661, .T. ) ;
#79108 = ORIENTED_EDGE ( 'NONE', *, *, #100171, .T. ) ;
#79109 = EDGE_CURVE ( 'NONE', #80663, #196636, #69218, .T. ) ;
#79111 = ADVANCED_FACE ( 'NONE', ( #30723 ), #11134, .T. ) ;
#79110 = CARTESIAN_POINT ( 'NONE',  ( 20.94999999999999929, 67.23127455305835554, -235.8551265064784559 ) ) ;
#79112 = ORIENTED_EDGE ( 'NONE', *, *, #115188, .T. ) ;
#79113 = CARTESIAN_POINT ( 'NONE',  ( 20.00000000000000355, 5.454087299794354138, 16.60000000000000142 ) ) ;
#79114 = LINE ( 'NONE', #6974, #169581 ) ;
#79115 = ORIENTED_EDGE ( 'NONE', *, *, #115989, .F. ) ;
#79116 = CARTESIAN_POINT ( 'NONE',  ( -20.54999999999999716, 85.00000000001261924, -193.6291383618718385 ) ) ;
#79117 = CARTESIAN_POINT ( 'NONE',  ( -20.94999999999999929, 7.031312794766356511, -137.6091509382273443 ) ) ;
#79118 = DIRECTION ( 'NONE',  ( -0.7071067811865562325, -0.7071067811865388020, 0.000000000000000000 ) ) ;
#79119 = VERTEX_POINT ( 'NONE', #9842 ) ;
#79120 = EDGE_CURVE ( 'NONE', #102738, #137157, #71124, .T. ) ;
#79121 = CIRCLE ( 'NONE', #175057, 0.1000000000000028644 ) ;
#79122 = DIRECTION ( 'NONE',  ( 0.000000000000000000, 0.000000000000000000, -1.000000000000000000 ) ) ;
#79123 = DIRECTION ( 'NONE',  ( -1.000000000000000000, 0.000000000000000000, 0.000000000000000000 ) ) ;
#79124 = AXIS2_PLACEMENT_3D ( 'NONE', #211142, #170787, #191616 ) ;
#79125 = CARTESIAN_POINT ( 'NONE',  ( -20.64999999999999858, 68.75000000001151079, -48.37310748452436826 ) ) ;
#79126 = CIRCLE ( 'NONE', #34, 0.09999999999999810429 ) ;
#79127 = EDGE_CURVE ( 'NONE', #56338, #164531, #89364, .T. ) ;
#79128 = VERTEX_POINT ( 'NONE', #210610 ) ;
#79129 = EDGE_CURVE ( 'NONE', #230388, #236302, #245897, .T. ) ;
#79130 =( BOUNDED_SURFACE ( )  B_SPLINE_SURFACE ( 3, 2, ( 
 ( #64594, #166315, #128435 ),
 ( #25493, #204105, #247078 ),
 ( #146681, #124592, #144119 ),
 ( #104972, #167584, #48889 ) ),
 .UNSPECIFIED., .F., .F., .F. ) 
 B_SPLINE_SURFACE_WITH_KNOTS ( ( 4, 4 ),
 ( 3, 3 ),
 ( 0.0008258556059633754111, 0.0009616864997632845833 ),
 ( 0.000000000000000000, 1.000000000000000000 ),
 .UNSPECIFIED. ) 
 GEOMETRIC_REPRESENTATION_ITEM ( )  RATIONAL_B_SPLINE_SURFACE ( (
 ( 1.000000000000000000, 0.9152888060719386321, 1.000000000000000000),
 ( 1.000000000000000000, 0.9327727094138064112, 1.000000000000000000),
 ( 1.000000000000000000, 0.9369023509258621596, 1.000000000000000000),
 ( 1.000000000000000000, 0.9246339933864486937, 1.000000000000000000) ) ) 
 REPRESENTATION_ITEM ( '' )  SURFACE ( )  );
#79132 = ORIENTED_EDGE ( 'NONE', *, *, #156253, .T. ) ;
#79131 = DIRECTION ( 'NONE',  ( 1.000000000000000000, 0.000000000000000000, 0.000000000000000000 ) ) ;
#79133 = EDGE_LOOP ( 'NONE', ( #125553, #6083, #20897, #109770 ) ) ;
#79134 = DIRECTION ( 'NONE',  ( -1.000000000000000000, -0.000000000000000000, -0.000000000000000000 ) ) ;
#79135 = EDGE_CURVE ( 'NONE', #168895, #57327, #111515, .T. ) ;
#79136 = LINE ( 'NONE', #255165, #137707 ) ;
#79137 = CYLINDRICAL_SURFACE ( 'NONE', #158890, 0.1000000000000028644 ) ;
#79138 = CARTESIAN_POINT ( 'NONE',  ( -17.11825945287482753, 9.950000000011138823, -46.25000000000000711 ) ) ;
#79139 = DIRECTION ( 'NONE',  ( -0.000000000000000000, -1.000000000000000000, -0.000000000000000000 ) ) ;
#79140 = FACE_OUTER_BOUND ( 'NONE', #36942, .T. ) ;
#79141 = AXIS2_PLACEMENT_3D ( 'NONE', #69599, #228675, #149138 ) ;
#79142 = ORIENTED_EDGE ( 'NONE', *, *, #24410, .T. ) ;
#79143 = CIRCLE ( 'NONE', #220804, 0.1000000000000124678 ) ;
#79144 = CARTESIAN_POINT ( 'NONE',  ( -16.77683809663752257, 9.945835743215301505, -146.6639490191042228 ) ) ;
#79145 = LINE ( 'NONE', #38764, #114837 ) ;
#79146 = DIRECTION ( 'NONE',  ( 0.000000000000000000, 0.000000000000000000, 1.000000000000000000 ) ) ;
#79147 = EDGE_CURVE ( 'NONE', #80372, #25370, #225015, .T. ) ;
#79149 = ADVANCED_FACE ( 'NONE', ( #205464 ), #102460, .T. ) ;
#79148 = AXIS2_PLACEMENT_3D ( 'NONE', #152891, #233687, #53751 ) ;
#79150 = CARTESIAN_POINT ( 'NONE',  ( 20.97438252431638972, 67.07457649393559507, -61.05073679551357202 ) ) ;
#79151 = TOROIDAL_SURFACE ( 'NONE', #170989, 0.6000000000000009770, 0.1000000000000000056 ) ;
#79152 = ORIENTED_EDGE ( 'NONE', *, *, #30098, .F. ) ;
#79153 = VERTEX_POINT ( 'NONE', #146754 ) ;
#79154 = DIRECTION ( 'NONE',  ( 1.000000000000000000, 0.000000000000000000, 0.000000000000000000 ) ) ;
#79155 = DIRECTION ( 'NONE',  ( 1.000000000000000000, 0.000000000000000000, 0.000000000000000000 ) ) ;
#79157 = EDGE_CURVE ( 'NONE', #30344, #72156, #127228, .T. ) ;
#79156 = CARTESIAN_POINT ( 'NONE',  ( -18.39999999999999858, 11.41458325959979625, -20.85000000000000142 ) ) ;
#79158 = CARTESIAN_POINT ( 'NONE',  ( 21.05000000000000071, 59.06422320270096549, -225.9139711108258552 ) ) ;
#79159 = DIRECTION ( 'NONE',  ( 0.000000000000000000, 0.000000000000000000, 1.000000000000000000 ) ) ;
#79160 = ORIENTED_EDGE ( 'NONE', *, *, #40311, .T. ) ;
#79162 = EDGE_CURVE ( 'NONE', #154736, #159251, #119262, .T. ) ;
#79161 = CARTESIAN_POINT ( 'NONE',  ( -18.50000000000000000, 47.16152503674118890, -255.1462838189583806 ) ) ;
#79163 = EDGE_CURVE ( 'NONE', #24047, #227863, #235300, .T. ) ;
#79164 = DIRECTION ( 'NONE',  ( 0.000000000000000000, -0.008583690987162452199, 0.9999631594459053030 ) ) ;
#79165 = CARTESIAN_POINT ( 'NONE',  ( -20.64999999999999858, 4.350000000011156054, -121.6500000000000341 ) ) ;
#79166 = AXIS2_PLACEMENT_3D ( 'NONE', #54362, #71388, #76485 ) ;
#79167 = CIRCLE ( 'NONE', #62633, 0.1999999999999987899 ) ;
#79168 = DIRECTION ( 'NONE',  ( -1.000000000000000000, 2.849773892568378313E-16, -7.728835255496647986E-17 ) ) ;
#79169 = VERTEX_POINT ( 'NONE', #112802 ) ;
#79170 = CARTESIAN_POINT ( 'NONE',  ( 20.99999999999997868, 36.65892442174472876, -249.5511627012454596 ) ) ;
#79171 = ORIENTED_EDGE ( 'NONE', *, *, #114968, .T. ) ;
#79172 = ADVANCED_FACE ( 'NONE', ( #157074 ), #37134, .T. ) ;
#79173 = CARTESIAN_POINT ( 'NONE',  ( 20.94999999999999574, -1.162701749926853712, -175.5999999999999659 ) ) ;
#79174 = CARTESIAN_POINT ( 'NONE',  ( 21.11833042828143547, 69.55435530615680761, -170.0302079935837014 ) ) ;
#79175 = DIRECTION ( 'NONE',  ( 1.000000000000000000, 0.000000000000000000, 0.000000000000000000 ) ) ;
#79176 = CARTESIAN_POINT ( 'NONE',  ( 18.58222699835054570, 65.66799936921511005, -63.92993998886009877 ) ) ;
#79177 = CARTESIAN_POINT ( 'NONE',  ( -20.85000000000000142, 76.00000000001244871, -170.0231074845243597 ) ) ;
#79178 = LINE ( 'NONE', #179603, #226272 ) ;
#79179 = LINE ( 'NONE', #256488, #8195 ) ;
#79180 = CARTESIAN_POINT ( 'NONE',  ( -20.94999999999999929, 1.115600667400684642E-11, -134.0000000000000000 ) ) ;
#79181 = DIRECTION ( 'NONE',  ( -1.000000000000000000, 0.000000000000000000, -0.000000000000000000 ) ) ;
#79182 = EDGE_CURVE ( 'NONE', #27184, #163802, #102645, .T. ) ;
#79183 = VECTOR ( 'NONE', #238962, 1000.000000000000000 ) ;
#79184 = CARTESIAN_POINT ( 'NONE',  ( -18.59999999999999787, 11.65000000001115232, -121.8500000000000369 ) ) ;
#79185 = CIRCLE ( 'NONE', #33455, 0.09999999999998898659 ) ;
#79186 = FACE_OUTER_BOUND ( 'NONE', #114695, .T. ) ;
#79188 = CARTESIAN_POINT ( 'NONE',  ( -23.15000000000000213, 48.89266972451527948, -253.5637804087949121 ) ) ;
#79187 = CIRCLE ( 'NONE', #66748, 0.09999999999999939493 ) ;
#79189 = AXIS2_PLACEMENT_3D ( 'NONE', #85495, #150650, #86800 ) ;
#79190 = CARTESIAN_POINT ( 'NONE',  ( 20.95512820512820440, 10.62384868372303259, -79.15000000000003411 ) ) ;
#79191 = PLANE ( 'NONE',  #170467 ) ;
#79192 = CIRCLE ( 'NONE', #224936, 0.09999999999999939493 ) ;
#79193 = ORIENTED_EDGE ( 'NONE', *, *, #115097, .F. ) ;
#79194 = CARTESIAN_POINT ( 'NONE',  ( 21.05000000000000071, 6.413978881488429984, -0.08579911627414654740 ) ) ;
#79195 = DIRECTION ( 'NONE',  ( 2.952720810173289112E-16, 1.000000000000000000, 6.982962677686266711E-15 ) ) ;
#79196 = EDGE_CURVE ( 'NONE', #162352, #135449, #232986, .T. ) ;
#79197 = CARTESIAN_POINT ( 'NONE',  ( 20.75572585718222385, 8.882316728409756834, -41.99725839870686883 ) ) ;
#79198 = VERTEX_POINT ( 'NONE', #55345 ) ;
#79199 = DIRECTION ( 'NONE',  ( 1.000000000000000000, -0.000000000000000000, 0.000000000000000000 ) ) ;
#79200 = AXIS2_PLACEMENT_3D ( 'NONE', #243348, #64713, #223773 ) ;
#79202 = CIRCLE ( 'NONE', #224945, 0.1999999999999987899 ) ;
#79201 = DIRECTION ( 'NONE',  ( -1.000000000000000000, 0.000000000000000000, -0.000000000000000000 ) ) ;
#79203 = VERTEX_POINT ( 'NONE', #94504 ) ;
#79204 = CARTESIAN_POINT ( 'NONE',  ( -23.15000000000000213, -11.64999999998884483, -197.8999999999999773 ) ) ;
#79205 = DIRECTION ( 'NONE',  ( 0.000000000000000000, 0.000000000000000000, 1.000000000000000000 ) ) ;
#79206 = ADVANCED_FACE ( 'NONE', ( #35845 ), #16290, .T. ) ;
#79207 = VERTEX_POINT ( 'NONE', #95777 ) ;
#79208 = ORIENTED_EDGE ( 'NONE', *, *, #245089, .T. ) ;
#79209 = CYLINDRICAL_SURFACE ( 'NONE', #81180, 1.749999999999998002 ) ;
#79210 = ORIENTED_EDGE ( 'NONE', *, *, #212137, .F. ) ;
#79211 = CARTESIAN_POINT ( 'NONE',  ( 21.05000000000000071, -0.01454569056957751363, 6.497017786431992015 ) ) ;
#79212 = CYLINDRICAL_SURFACE ( 'NONE', #241074, 0.1000000000000028644 ) ;
#79214 = CARTESIAN_POINT ( 'NONE',  ( 21.14250536705908345, 33.99405510657214791, -243.6026301039981945 ) ) ;
#79213 = UNCERTAINTY_MEASURE_WITH_UNIT (LENGTH_MEASURE( 1.000000000000000082E-05 ), #209015, 'distance_accuracy_value', 'NONE');
#79215 = CARTESIAN_POINT ( 'NONE',  ( -20.00857864376270001, 66.65000000001180069, -81.87310748452438247 ) ) ;
#79216 = CARTESIAN_POINT ( 'NONE',  ( -12.29659703204452015, 47.69902910524212558, -234.3535107520373799 ) ) ;
#79217 = CARTESIAN_POINT ( 'NONE',  ( 5.551115123125782702E-14, 65.35000000001120668, -3.123107484524795474 ) ) ;
#79218 = FACE_OUTER_BOUND ( 'NONE', #121161, .T. ) ;
#79220 = ORIENTED_EDGE ( 'NONE', *, *, #13690, .F. ) ;
#79219 = FACE_OUTER_BOUND ( 'NONE', #229979, .T. ) ;
#79221 = ORIENTED_EDGE ( 'NONE', *, *, #72276, .T. ) ;
#79223 = CARTESIAN_POINT ( 'NONE',  ( -20.54999999999999716, 74.07476635515169505, -48.75335101765046630 ) ) ;
#79222 = CARTESIAN_POINT ( 'NONE',  ( 18.47149038651510722, 37.97416073834201455, -261.2273484851261856 ) ) ;
#79226 = ORIENTED_EDGE ( 'NONE', *, *, #193921, .T. ) ;
#79225 = DIRECTION ( 'NONE',  ( 1.000000000000000000, 0.000000000000000000, 0.000000000000000000 ) ) ;
#79224 = FACE_OUTER_BOUND ( 'NONE', #53640, .T. ) ;
#79227 = CIRCLE ( 'NONE', #91723, 11.74999999999999645 ) ;
#79228 = EDGE_LOOP ( 'NONE', ( #93204, #188963, #121333 ) ) ;
#79229 = CARTESIAN_POINT ( 'NONE',  ( 18.39999999999999503, 50.88295650978584206, -230.3037755757580953 ) ) ;
#79230 = CARTESIAN_POINT ( 'NONE',  ( 20.52683494730037239, 8.980530818312608687, -176.0052527225371648 ) ) ;
#79231 = CARTESIAN_POINT ( 'NONE',  ( 20.85000000000000142, 62.88396779178383156, -206.9948552354529170 ) ) ;
#79232 = CIRCLE ( 'NONE', #75183, 0.09999999999999939493 ) ;
#79233 = DIRECTION ( 'NONE',  ( -4.408576920032447972E-17, 0.1290532225515392262, 0.9916376685811522096 ) ) ;
#79234 = DIRECTION ( 'NONE',  ( 1.000000000000000000, 0.000000000000000000, 0.000000000000000000 ) ) ;
#79235 = DIRECTION ( 'NONE',  ( 0.000000000000000000, 6.982962677686266711E-15, -1.000000000000000000 ) ) ;
#79236 = EDGE_CURVE ( 'NONE', #232528, #87393, #123529, .T. ) ;
#79237 = CARTESIAN_POINT ( 'NONE',  ( 20.94999999999999929, 64.35000000001146248, -42.86470817442145886 ) ) ;
#79238 = ORIENTED_EDGE ( 'NONE', *, *, #63824, .F. ) ;
#79239 = VERTEX_POINT ( 'NONE', #136172 ) ;
#79240 = DIRECTION ( 'NONE',  ( -0.000000000000000000, 7.172728831056617961E-15, -1.000000000000000000 ) ) ;
#79241 = ORIENTED_EDGE ( 'NONE', *, *, #110636, .F. ) ;
#79242 = DIRECTION ( 'NONE',  ( 1.000000000000000000, -0.000000000000000000, -0.000000000000000000 ) ) ;
#79244 = ORIENTED_EDGE ( 'NONE', *, *, #32155, .F. ) ;
#79243 = AXIS2_PLACEMENT_3D ( 'NONE', #97159, #94633, #76341 ) ;
#79245 = CYLINDRICAL_SURFACE ( 'NONE', #35079, 0.5000000000000004441 ) ;
#79246 = COLOUR_RGB ( '', 0.40784314, 0.44705882, 0.49803922) ;
#79247 = CARTESIAN_POINT ( 'NONE',  ( -15.06720934482788543, 49.36478519392533570, -233.5395520442457382 ) ) ;
#79248 = SPHERICAL_SURFACE ( 'NONE', #18063, 0.1000000000000000056 ) ;
#79249 = EDGE_CURVE ( 'NONE', #140980, #219433, #46336, .T. ) ;
#79250 = DIRECTION ( 'NONE',  ( 0.000000000000000000, -1.000000000000000000, 0.000000000000000000 ) ) ;
#79251 = DIRECTION ( 'NONE',  ( 1.000000000000000000, 3.265361837132813093E-16, -0.000000000000000000 ) ) ;
#79252 = ORIENTED_EDGE ( 'NONE', *, *, #120330, .T. ) ;
#79253 = VECTOR ( 'NONE', #5364, 1000.000000000000114 ) ;
#79255 = VECTOR ( 'NONE', #135343, 1000.000000000000000 ) ;
#79254 = CARTESIAN_POINT ( 'NONE',  ( -23.15000000000000213, 73.40000000001201386, -116.2477294072864140 ) ) ;
#79256 = ADVANCED_FACE ( 'NONE', ( #114065 ), #72407, .F. ) ;
#79257 = CARTESIAN_POINT ( 'NONE',  ( -33.72168855820451938, 66.05000000001152216, -48.67310748452433700 ) ) ;
#79258 = CARTESIAN_POINT ( 'NONE',  ( -20.64999999999999858, 4.350000000011156054, -179.8499999999999943 ) ) ;
#79259 = CARTESIAN_POINT ( 'NONE',  ( -21.30740335185486245, 75.90106547423687289, -210.0797654065523545 ) ) ;
#79260 = CARTESIAN_POINT ( 'NONE',  ( 20.94999999999999929, 76.00000000001170974, -69.52310748452431710 ) ) ;
#79261 = EDGE_LOOP ( 'NONE', ( #190665, #23412, #218831, #66700 ) ) ;
#79262 = CARTESIAN_POINT ( 'NONE',  ( -18.36527282682062534, 85.50000060000994040, -29.10095852002216077 ) ) ;
#79263 = EDGE_CURVE ( 'NONE', #120323, #180338, #11352, .T. ) ;
#79264 = ORIENTED_EDGE ( 'NONE', *, *, #237083, .F. ) ;
#79267 = ORIENTED_EDGE ( 'NONE', *, *, #67890, .T. ) ;
#79266 = FACE_OUTER_BOUND ( 'NONE', #156006, .T. ) ;
#79265 = DIRECTION ( 'NONE',  ( 1.000000000000000000, 0.000000000000000000, 0.000000000000000000 ) ) ;
#79268 = AXIS2_PLACEMENT_3D ( 'NONE', #238537, #241132, #133348 ) ;
#79269 = CARTESIAN_POINT ( 'NONE',  ( -23.15000000000000213, 87.65000000001172964, -72.62310748452422615 ) ) ;
#79270 = CIRCLE ( 'NONE', #116886, 0.1000000000000028644 ) ;
#79271 = AXIS2_PLACEMENT_3D ( 'NONE', #208719, #189136, #168337 ) ;
#79272 = TOROIDAL_SURFACE ( 'NONE', #220761, 0.2000000000000000111, 0.1000000000000000056 ) ;
#79273 = EDGE_CURVE ( 'NONE', #207248, #40059, #19293, .T. ) ;
#79274 = CARTESIAN_POINT ( 'NONE',  ( -22.49544290803788371, 64.25012976215435856, -69.58841944378173139 ) ) ;
#79275 = EDGE_LOOP ( 'NONE', ( #225271, #254945, #62983, #103045 ) ) ;
#79276 = CARTESIAN_POINT ( 'NONE',  ( 18.33996824403561376, 85.56963985944319973, -129.7040418470071472 ) ) ;
#79277 = ADVANCED_FACE ( 'NONE', ( #21427 ), #162220, .T. ) ;
#79278 = CYLINDRICAL_SURFACE ( 'NONE', #194755, 1.749999999999999778 ) ;
#79279 = ADVANCED_FACE ( 'NONE', ( #3095 ), #240064, .T. ) ;
#79280 = FACE_OUTER_BOUND ( 'NONE', #111875, .T. ) ;
#79282 = ORIENTED_EDGE ( 'NONE', *, *, #114435, .F. ) ;
#79281 = DIRECTION ( 'NONE',  ( -0.000000000000000000, -6.982962677686266711E-15, 1.000000000000000000 ) ) ;
#79283 = CARTESIAN_POINT ( 'NONE',  ( 20.84999999999999432, 7.021664781911246322, -204.8335654018972605 ) ) ;
#79284 = VECTOR ( 'NONE', #137382, 1000.000000000000000 ) ;
#79285 = EDGE_CURVE ( 'NONE', #98428, #54594, #248431, .T. ) ;
#79286 = VERTEX_POINT ( 'NONE', #81334 ) ;
#79287 = DIRECTION ( 'NONE',  ( 1.000000000000000000, 3.265361837132813093E-16, -0.000000000000000000 ) ) ;
#79288 = LINE ( 'NONE', #240954, #244985 ) ;
#79289 = DIRECTION ( 'NONE',  ( 0.000000000000000000, 0.000000000000000000, 1.000000000000000000 ) ) ;
#79290 = ORIENTED_EDGE ( 'NONE', *, *, #231786, .F. ) ;
#79291 = CARTESIAN_POINT ( 'NONE',  ( -16.88495309932524080, 66.04537294153944060, -157.3885588107125386 ) ) ;
#79292 = ORIENTED_EDGE ( 'NONE', *, *, #201471, .T. ) ;
#79293 = CARTESIAN_POINT ( 'NONE',  ( -18.50000000000000000, 9.250000000011157297, -155.3500000000000227 ) ) ;
#79294 = LINE ( 'NONE', #121043, #59848 ) ;
#79295 = CARTESIAN_POINT ( 'NONE',  ( 22.57320508075687115, 11.48087284840413425, -198.4995883060917663 ) ) ;
#79296 = VERTEX_POINT ( 'NONE', #201315 ) ;
#79297 = DIRECTION ( 'NONE',  ( 4.377807931758639578E-15, -0.2605042016806606298, -0.9654727137038736640 ) ) ;
#79298 = AXIS2_PLACEMENT_3D ( 'NONE', #43080, #147303, #144724 ) ;
#79299 = EDGE_CURVE ( 'NONE', #222338, #31357, #194302, .T. ) ;
#79300 = DIRECTION ( 'NONE',  ( 1.000000000000000000, 0.000000000000000000, 0.000000000000000000 ) ) ;
#79301 = CARTESIAN_POINT ( 'NONE',  ( -20.96077737575351918, 64.37609936600773608, -176.8823155274181147 ) ) ;
#79302 = CIRCLE ( 'NONE', #225049, 0.2000000000000057288 ) ;
#79303 = ORIENTED_EDGE ( 'NONE', *, *, #76512, .T. ) ;
#79304 = CARTESIAN_POINT ( 'NONE',  ( 21.08489247129321242, 8.877675190870073507, -12.35000000000000142 ) ) ;
#79305 = DIRECTION ( 'NONE',  ( 0.000000000000000000, 0.1298341882519953583, 0.9915357197604862671 ) ) ;
#79306 = DIRECTION ( 'NONE',  ( 0.000000000000000000, -0.000000000000000000, -1.000000000000000000 ) ) ;
#79307 = VECTOR ( 'NONE', #121187, 999.9999999999998863 ) ;
#79308 = ORIENTED_EDGE ( 'NONE', *, *, #249001, .T. ) ;
#79309 = EDGE_CURVE ( 'NONE', #108480, #220499, #227573, .T. ) ;
#79311 = CARTESIAN_POINT ( 'NONE',  ( 21.05000000000000071, 1.115600667400684642E-11, -167.4999999999999716 ) ) ;
#79310 = AXIS2_PLACEMENT_3D ( 'NONE', #196476, #33618, #54408 ) ;
#79312 = ORIENTED_EDGE ( 'NONE', *, *, #174552, .F. ) ;
#79314 = ORIENTED_EDGE ( 'NONE', *, *, #222519, .F. ) ;
#79313 = DIRECTION ( 'NONE',  ( 0.000000000000000000, 6.982962677686266711E-15, -1.000000000000000000 ) ) ;
#79317 = ORIENTED_EDGE ( 'NONE', *, *, #243765, .T. ) ;
#79316 = EDGE_LOOP ( 'NONE', ( #248420, #98528, #107873, #802, #243806, #165060, #70995, #129712, #83970, #177240, #181090 ) ) ;
#79315 = CARTESIAN_POINT ( 'NONE',  ( -21.08376601933334271, 0.06377601092987864040, 6.341947271275729214 ) ) ;
#79318 = CIRCLE ( 'NONE', #237742, 4.300000000000029132 ) ;
#79319 = DIRECTION ( 'NONE',  ( 0.000000000000000000, 0.000000000000000000, -1.000000000000000000 ) ) ;
#79320 = CARTESIAN_POINT ( 'NONE',  ( -21.08078803292166725, 0.07918598716886542099, -161.1669870355628120 ) ) ;
#79321 = CARTESIAN_POINT ( 'NONE',  ( -21.14999999999999858, 76.00000000001195133, -103.0231074845243171 ) ) ;
#79322 = CARTESIAN_POINT ( 'NONE',  ( 20.85882249326303040, 46.46967969402478360, -243.0849751855955674 ) ) ;
#79324 = EDGE_CURVE ( 'NONE', #82580, #161077, #102180, .T. ) ;
#79323 = DIRECTION ( 'NONE',  ( 0.000000000000000000, 0.000000000000000000, 1.000000000000000000 ) ) ;
#79325 = VECTOR ( 'NONE', #33943, 1000.000000000000000 ) ;
#79326 = CARTESIAN_POINT ( 'NONE',  ( 18.39999999999999503, 64.25000000001202238, -115.6731074845243938 ) ) ;
#79327 = ADVANCED_FACE ( 'NONE', ( #243003 ), #181761, .T. ) ;
#79328 = AXIS2_PLACEMENT_3D ( 'NONE', #204474, #47972, #107957 ) ;
#79329 = CARTESIAN_POINT ( 'NONE',  ( -23.25000000000000000, 70.05000000001197691, -113.3288097895591591 ) ) ;
#79331 = LINE ( 'NONE', #59757, #247229 ) ;
#79330 = CARTESIAN_POINT ( 'NONE',  ( 18.59999999999999787, 77.83585931145546510, -91.51866831572576189 ) ) ;
#79333 = ORIENTED_EDGE ( 'NONE', *, *, #108857, .F. ) ;
#79332 = AXIS2_PLACEMENT_3D ( 'NONE', #59437, #5577, #96028 ) ;
#79334 = VERTEX_POINT ( 'NONE', #222132 ) ;
#79335 = CARTESIAN_POINT ( 'NONE',  ( 21.14999999999999503, 1.115600667400684642E-11, -33.50000000000000000 ) ) ;
#79337 = ORIENTED_EDGE ( 'NONE', *, *, #232448, .T. ) ;
#79336 = DIRECTION ( 'NONE',  ( 0.000000000000000000, 6.982962677686266711E-15, -1.000000000000000000 ) ) ;
#79338 = DIRECTION ( 'NONE',  ( -0.000000000000000000, 0.9770955615653312831, 0.2128009952263620053 ) ) ;
#79339 = ORIENTED_EDGE ( 'NONE', *, *, #224630, .F. ) ;
#79340 = DIRECTION ( 'NONE',  ( 1.000000000000000000, -0.000000000000000000, 0.000000000000000000 ) ) ;
#79341 = ADVANCED_FACE ( 'NONE', ( #123078 ), #43541, .F. ) ;
#79342 = ORIENTED_EDGE ( 'NONE', *, *, #159032, .F. ) ;
#79343 = FACE_OUTER_BOUND ( 'NONE', #96937, .T. ) ;
#79344 = EDGE_CURVE ( 'NONE', #31293, #52970, #99617, .T. ) ;
#79345 = EDGE_CURVE ( 'NONE', #68680, #118232, #177921, .T. ) ;
#79346 = VERTEX_POINT ( 'NONE', #183055 ) ;
#79347 = TOROIDAL_SURFACE ( 'NONE', #141898, 12.97499999999999787, 0.1000000000000000056 ) ;
#79348 = CARTESIAN_POINT ( 'NONE',  ( 21.00000000000000000, 9.750000000011153745, -54.65000000000000568 ) ) ;
#79349 = CARTESIAN_POINT ( 'NONE',  ( -23.39999999999994529, 79.88763423575340994, -7.282924647898262549 ) ) ;
#79351 = EDGE_LOOP ( 'NONE', ( #191932, #65993, #55079, #33986 ) ) ;
#79350 = ORIENTED_EDGE ( 'NONE', *, *, #186164, .F. ) ;
#79352 = ORIENTED_EDGE ( 'NONE', *, *, #48101, .F. ) ;
#79353 = CARTESIAN_POINT ( 'NONE',  ( 18.39999999999999503, 70.35000000001230092, -157.3731074845244109 ) ) ;
#79354 = ORIENTED_EDGE ( 'NONE', *, *, #38311, .T. ) ;
#79355 = ORIENTED_EDGE ( 'NONE', *, *, #63368, .F. ) ;
#79356 = EDGE_CURVE ( 'NONE', #137609, #3992, #163479, .T. ) ;
#79357 = CARTESIAN_POINT ( 'NONE',  ( -21.14999999999999858, 11.65000000001115588, -167.5999999999999659 ) ) ;
#79359 = ORIENTED_EDGE ( 'NONE', *, *, #48316, .T. ) ;
#79358 = CARTESIAN_POINT ( 'NONE',  ( -18.59999999999999787, 4.252251777740764460, -211.8999245327126744 ) ) ;
#79361 = LINE ( 'NONE', #178511, #56889 ) ;
#79360 = CARTESIAN_POINT ( 'NONE',  ( -18.34374000495060386, 11.47316190337362585, -176.7499999999999716 ) ) ;
#79362 = DIRECTION ( 'NONE',  ( 0.000000000000000000, 0.000000000000000000, -1.000000000000000000 ) ) ;
#79363 = CARTESIAN_POINT ( 'NONE',  ( 20.94999999999999929, -1.135018845899022466, -208.7169768834322952 ) ) ;
#79364 = CARTESIAN_POINT ( 'NONE',  ( -18.79999999999999716, -1.885425182446133885, -11.49641995933507843 ) ) ;
#79365 = EDGE_LOOP ( 'NONE', ( #220676, #14154, #104325, #220547 ) ) ;
#79366 = VERTEX_POINT ( 'NONE', #143904 ) ;
#79367 = LINE ( 'NONE', #98916, #195542 ) ;
#79369 = VECTOR ( 'NONE', #162004, 1000.000000000000114 ) ;
#79368 = CARTESIAN_POINT ( 'NONE',  ( 20.94999999999999929, 67.22371710471982453, -157.8731074845244109 ) ) ;
#79370 = CARTESIAN_POINT ( 'NONE',  ( 20.94999999999999929, 5.400000000011154988, -191.1060308773475072 ) ) ;
#79371 = TOROIDAL_SURFACE ( 'NONE', #266, 6.258578643762712446, 0.1000000000000000056 ) ;
#79372 = VECTOR ( 'NONE', #129499, 1000.000000000000114 ) ;
#79373 = VERTEX_POINT ( 'NONE', #257374 ) ;
#79374 = DIRECTION ( 'NONE',  ( -0.000000000000000000, -0.2617529984165031243, -0.9651348961777157509 ) ) ;
#79375 = CARTESIAN_POINT ( 'NONE',  ( -20.94999999999999929, 43.16050967218924939, -245.0573091940785844 ) ) ;
#79376 = AXIS2_PLACEMENT_3D ( 'NONE', #169007, #151996, #29491 ) ;
#79377 = DIRECTION ( 'NONE',  ( -0.7071067811865487940, -0.2890913453342118800, 0.6453109281988440582 ) ) ;
#79378 = ORIENTED_EDGE ( 'NONE', *, *, #76890, .T. ) ;
#79379 = EDGE_LOOP ( 'NONE', ( #143755, #80929, #213516, #253451 ) ) ;
#79380 = CARTESIAN_POINT ( 'NONE',  ( 18.39999999999997371, 11.75000000001113953, -143.2500000000000284 ) ) ;
#79381 = CARTESIAN_POINT ( 'NONE',  ( 18.49999999999999289, 69.55000000001223270, -148.8731074845244109 ) ) ;
#79383 = EDGE_CURVE ( 'NONE', #5568, #63710, #252506, .T. ) ;
#79382 = VERTEX_POINT ( 'NONE', #198744 ) ;
#79384 = DIRECTION ( 'NONE',  ( 1.000000000000000000, 7.304098846218133681E-16, -4.607487905232622991E-31 ) ) ;
#79385 = EDGE_LOOP ( 'NONE', ( #57086, #98691, #100468, #241586 ) ) ;
#79386 = EDGE_CURVE ( 'NONE', #20026, #83116, #179216, .T. ) ;
#79387 = DIRECTION ( 'NONE',  ( 0.000000000000000000, -2.220446049250311819E-14, -1.000000000000000000 ) ) ;
#79388 = DIRECTION ( 'NONE',  ( 0.000000000000000000, -0.8814952561688430555, 0.4721928772777346239 ) ) ;
#79390 = SURFACE_SIDE_STYLE ('',( #257991 ) ) ;
#79389 = DIRECTION ( 'NONE',  ( -0.000000000000000000, -1.000000000000000000, 0.000000000000000000 ) ) ;
#79391 = AXIS2_PLACEMENT_3D ( 'NONE', #159356, #62806, #121525 ) ;
#79392 = CARTESIAN_POINT ( 'NONE',  ( -20.54999999999999716, 4.349999999999999645, -21.15000000000000213 ) ) ;
#79393 = DIRECTION ( 'NONE',  ( -0.000000000000000000, -0.1686199900910312910, 0.9856811345164826488 ) ) ;
#79395 = EDGE_CURVE ( 'NONE', #183742, #29761, #94302, .T. ) ;
#79394 = ORIENTED_EDGE ( 'NONE', *, *, #237579, .T. ) ;
#79396 = DIRECTION ( 'NONE',  ( 0.000000000000000000, -0.7397360091702744889, 0.6728971962616842051 ) ) ;
#79398 = VERTEX_POINT ( 'NONE', #205148 ) ;
#79397 = ORIENTED_EDGE ( 'NONE', *, *, #112760, .T. ) ;
#79399 = ORIENTED_EDGE ( 'NONE', *, *, #117742, .F. ) ;
#79400 = FACE_OUTER_BOUND ( 'NONE', #142094, .T. ) ;
#79401 = CARTESIAN_POINT ( 'NONE',  ( -21.65000000000000213, 21.56708615768143034, -232.7219885528102736 ) ) ;
#79402 = DIRECTION ( 'NONE',  ( -1.000000000000000000, 0.000000000000000000, 0.000000000000000000 ) ) ;
#79403 = DIRECTION ( 'NONE',  ( -0.000000000000000000, -0.000000000000000000, -1.000000000000000000 ) ) ;
#79404 = AXIS2_PLACEMENT_3D ( 'NONE', #159692, #20183, #218345 ) ;
#79405 = CARTESIAN_POINT ( 'NONE',  ( -15.15766958671844300, 66.58946139148297050, -87.59041948738348538 ) ) ;
#79406 = ORIENTED_EDGE ( 'NONE', *, *, #235385, .T. ) ;
#79407 = CARTESIAN_POINT ( 'NONE',  ( -16.94445028196808778, 66.00793639031486748, -190.9157773061059800 ) ) ;
#79408 = ORIENTED_EDGE ( 'NONE', *, *, #76058, .F. ) ;
#79409 = DIRECTION ( 'NONE',  ( 0.000000000000000000, 0.000000000000000000, -1.000000000000000000 ) ) ;
#79410 = ORIENTED_EDGE ( 'NONE', *, *, #54275, .F. ) ;
#79411 = VERTEX_POINT ( 'NONE', #6964 ) ;
#79412 = CARTESIAN_POINT ( 'NONE',  ( 20.94999999999999574, 1.162701749949165642, -141.9000000000000341 ) ) ;
#79413 = DIRECTION ( 'NONE',  ( 1.000000000000000000, 3.469446951953704435E-14, -2.003086131649669752E-14 ) ) ;
#79414 = LINE ( 'NONE', #239808, #50065 ) ;
#79415 = CARTESIAN_POINT ( 'NONE',  ( -17.22361732159831504, 10.34515565861358866, -89.12921547413290568 ) ) ;
#79416 = TOROIDAL_SURFACE ( 'NONE', #33695, 11.70000000000000107, 0.1000000000000000056 ) ;
#79417 = EDGE_CURVE ( 'NONE', #182938, #92704, #114717, .T. ) ;
#79418 = CARTESIAN_POINT ( 'NONE',  ( -20.85000000000000142, 56.23643450586806836, -227.9054833905874204 ) ) ;
#79419 = ORIENTED_EDGE ( 'NONE', *, *, #110202, .F. ) ;
#79420 = EDGE_LOOP ( 'NONE', ( #132335, #212730, #24085, #155457 ) ) ;
#79421 = CARTESIAN_POINT ( 'NONE',  ( -18.59999999999999787, 77.16412189325305349, -95.10825939895268277 ) ) ;
#79422 = AXIS2_PLACEMENT_3D ( 'NONE', #31697, #190773, #171227 ) ;
#79424 = EDGE_CURVE ( 'NONE', #136260, #165708, #127635, .T. ) ;
#79423 = CARTESIAN_POINT ( 'NONE',  ( -18.54118089899633048, -9.463537631836944186, -40.54857759786813176 ) ) ;
#79425 = EDGE_LOOP ( 'NONE', ( #48444, #51536, #104006, #5945 ) ) ;
#79426 = CARTESIAN_POINT ( 'NONE',  ( -20.85000000000000142, 67.23127455305835554, -235.8551265064784559 ) ) ;
#79427 = DIRECTION ( 'NONE',  ( 0.000000000000000000, 6.982962677686266711E-15, -1.000000000000000000 ) ) ;
#79428 = DIRECTION ( 'NONE',  ( -1.000000000000000000, 2.849773892568378313E-16, -7.728835255496647986E-17 ) ) ;
#79429 = DIRECTION ( 'NONE',  ( 1.000000000000000000, 0.000000000000000000, 0.000000000000000000 ) ) ;
#79430 = LINE ( 'NONE', #1175, #230001 ) ;
#79431 = DIRECTION ( 'NONE',  ( 2.840903330521632762E-16, -0.8454177738465994407, -0.5341055959866553016 ) ) ;
#79432 = EDGE_CURVE ( 'NONE', #73243, #59416, #140071, .T. ) ;
#79434 = DIRECTION ( 'NONE',  ( 0.000000000000000000, 0.9274965247785529332, -0.3738317757009255171 ) ) ;
#79433 = CARTESIAN_POINT ( 'NONE',  ( -16.94389599337536012, 30.26311786373704038, -234.7907289951723158 ) ) ;
#79435 = DIRECTION ( 'NONE',  ( 0.000000000000000000, -0.9893560106964500722, 0.1455152366551550613 ) ) ;
#79436 = ADVANCED_FACE ( 'NONE', ( #225979 ), #126923, .T. ) ;
#79437 = AXIS2_PLACEMENT_3D ( 'NONE', #4780, #84284, #45218 ) ;
#79438 = CARTESIAN_POINT ( 'NONE',  ( -18.41431012584569160, 11.48747202921933130, -57.77323601310166623 ) ) ;
#79439 = EDGE_CURVE ( 'NONE', #157942, #73178, #109906, .T. ) ;
#79441 = ORIENTED_EDGE ( 'NONE', *, *, #209888, .F. ) ;
#79440 = TOROIDAL_SURFACE ( 'NONE', #204338, 11.70000000000000107, 0.1000000000000000056 ) ;
#79443 = EDGE_CURVE ( 'NONE', #202540, #158504, #98349, .T. ) ;
#79442 = ADVANCED_FACE ( 'NONE', ( #150346 ), #219196, .T. ) ;
#79444 = AXIS2_PLACEMENT_3D ( 'NONE', #237287, #20821, #217685 ) ;
#79445 = CARTESIAN_POINT ( 'NONE',  ( 20.94999999999999929, 76.00000000001126921, -203.5231074845248997 ) ) ;
#79446 = ORIENTED_EDGE ( 'NONE', *, *, #186062, .T. ) ;
#79447 = CIRCLE ( 'NONE', #212751, 0.5999999999999894307 ) ;
#79448 = VECTOR ( 'NONE', #140478, 1000.000000000000000 ) ;
#79449 = DIRECTION ( 'NONE',  ( 0.000000000000000000, 0.000000000000000000, 1.000000000000000000 ) ) ;
#79450 = CARTESIAN_POINT ( 'NONE',  ( -21.76363531954647357, 0.09900187431060442078, -93.48706345212828239 ) ) ;
#79451 = DIRECTION ( 'NONE',  ( -1.073024830501118120E-15, -0.8814952561688430555, 0.4721928772777346239 ) ) ;
#79452 = ORIENTED_EDGE ( 'NONE', *, *, #18595, .F. ) ;
#79453 = CARTESIAN_POINT ( 'NONE',  ( 21.05000000000000071, 71.00000000001223555, -148.9283735034374843 ) ) ;
#79454 = CARTESIAN_POINT ( 'NONE',  ( 23.24999999999999289, 64.35000000001275566, -215.2731074845244450 ) ) ;
#79455 = CARTESIAN_POINT ( 'NONE',  ( -21.55000000000000071, 68.75000000001260503, -191.1731074845243938 ) ) ;
#79456 = AXIS2_PLACEMENT_3D ( 'NONE', #137827, #256438, #77856 ) ;
#79457 = EDGE_CURVE ( 'NONE', #147882, #101473, #165038, .T. ) ;
#79458 = FACE_OUTER_BOUND ( 'NONE', #218072, .T. ) ;
#79460 = EDGE_CURVE ( 'NONE', #185078, #102497, #15212, .T. ) ;
#79459 = AXIS2_PLACEMENT_3D ( 'NONE', #23519, #104278, #63892 ) ;
#79461 = CIRCLE ( 'NONE', #137710, 11.80000000000000071 ) ;
#79462 = CARTESIAN_POINT ( 'NONE',  ( 20.94999999999999929, 88.41227409416161720, -106.0231074845242176 ) ) ;
#79463 = DIRECTION ( 'NONE',  ( 1.000000000000000000, 0.000000000000000000, 0.000000000000000000 ) ) ;
#79464 = VECTOR ( 'NONE', #122423, 1000.000000000000000 ) ;
#79465 = ORIENTED_EDGE ( 'NONE', *, *, #41835, .T. ) ;
#79466 = CARTESIAN_POINT ( 'NONE',  ( 21.70464131381650219, 68.90464198104429272, -136.5231074845243313 ) ) ;
#79468 = EDGE_LOOP ( 'NONE', ( #158588, #92654, #132428, #110690 ) ) ;
#79467 = CARTESIAN_POINT ( 'NONE',  ( 21.05000000000000071, 36.65892442174472876, -249.5511627012454596 ) ) ;
#79469 = FACE_OUTER_BOUND ( 'NONE', #104160, .T. ) ;
#79470 = EDGE_CURVE ( 'NONE', #4036, #6721, #85900, .T. ) ;
#79471 = CYLINDRICAL_SURFACE ( 'NONE', #46302, 0.1000000000000028644 ) ;
#79472 = ORIENTED_EDGE ( 'NONE', *, *, #10415, .T. ) ;
#79473 = CARTESIAN_POINT ( 'NONE',  ( -18.50000000000000000, 9.350000000011156942, -188.6499999999999488 ) ) ;
#79474 = APPLICATION_PROTOCOL_DEFINITION ( 'draft international standard', 'automotive_design', 1998, #165871 ) ;
#79475 = EDGE_CURVE ( 'NONE', #94336, #16688, #48509, .T. ) ;
#79476 = AXIS2_PLACEMENT_3D ( 'NONE', #211174, #232040, #200592 ) ;
#79477 = EDGE_LOOP ( 'NONE', ( #9947, #153463, #78872, #160623 ) ) ;
#79478 = DIRECTION ( 'NONE',  ( 0.000000000000000000, 0.9126074666063660468, 0.4088369013363524762 ) ) ;
#79479 = DIRECTION ( 'NONE',  ( -1.000000000000000000, 0.000000000000000000, 0.000000000000000000 ) ) ;
#79480 = EDGE_CURVE ( 'NONE', #109372, #100102, #148484, .T. ) ;
#79481 = CARTESIAN_POINT ( 'NONE',  ( 21.00000000000000000, 66.25000000001158185, -57.27310748452438816 ) ) ;
#79482 = ORIENTED_EDGE ( 'NONE', *, *, #206023, .T. ) ;
#79483 = ORIENTED_EDGE ( 'NONE', *, *, #230771, .F. ) ;
#79484 = EDGE_CURVE ( 'NONE', #250869, #46074, #181792, .T. ) ;
#79485 = CARTESIAN_POINT ( 'NONE',  ( 20.99999999999999645, 22.88362888408687468, -231.1113624623564249 ) ) ;
#79486 = CARTESIAN_POINT ( 'NONE',  ( 23.14999999999999858, 76.00000000001213607, -136.5231074845243313 ) ) ;
#79487 = AXIS2_PLACEMENT_3D ( 'NONE', #97568, #239683, #16801 ) ;
#79488 = DIRECTION ( 'NONE',  ( 0.000000000000000000, 0.000000000000000000, -1.000000000000000000 ) ) ;
#79489 = DIRECTION ( 'NONE',  ( -1.000000000000000000, -0.000000000000000000, 0.000000000000000000 ) ) ;
#79490 = DIRECTION ( 'NONE',  ( 0.000000000000000000, 0.000000000000000000, 1.000000000000000000 ) ) ;
#79491 = DIRECTION ( 'NONE',  ( 0.000000000000000000, 0.000000000000000000, -1.000000000000000000 ) ) ;
#79493 = DIRECTION ( 'NONE',  ( 1.000000000000000000, 0.000000000000000000, 0.000000000000000000 ) ) ;
#79492 = LINE ( 'NONE', #159076, #145160 ) ;
#79494 = EDGE_CURVE ( 'NONE', #18766, #180038, #23617, .T. ) ;
#79495 = CARTESIAN_POINT ( 'NONE',  ( 20.94999999999999574, 1.115600667400684642E-11, -100.5000000000000284 ) ) ;
#79496 = DIRECTION ( 'NONE',  ( 0.000000000000000000, 0.000000000000000000, -1.000000000000000000 ) ) ;
#79497 = DIRECTION ( 'NONE',  ( 1.000000000000000000, 0.000000000000000000, 0.000000000000000000 ) ) ;
#79498 = CARTESIAN_POINT ( 'NONE',  ( -21.05000000000000071, 1.835341550235567887, -145.5551512925629822 ) ) ;
#79499 = ORIENTED_EDGE ( 'NONE', *, *, #40110, .T. ) ;
#79500 = ORIENTED_EDGE ( 'NONE', *, *, #42233, .T. ) ;
#79501 = B_SPLINE_CURVE_WITH_KNOTS ( 'NONE', 3,
 ( #233688, #176295, #78444, #57589, #135840, #73350, #234970, #55013, #155468, #193276 ),
 .UNSPECIFIED., .F., .F.,
 ( 4, 3, 3, 4 ),
 ( 1.950915401637565782E-15, 8.145022132839031210E-06, 1.905645951092651034E-05, 2.061107371226032482E-05 ),
 .UNSPECIFIED. ) ;
#79502 = CARTESIAN_POINT ( 'NONE',  ( 23.14999999999999858, 71.22429906543214884, -57.67433938047838637 ) ) ;
#79504 = CARTESIAN_POINT ( 'NONE',  ( -22.39999999999999858, 7.790779598373403836, 0.000000000000000000 ) ) ;
#79503 = CARTESIAN_POINT ( 'NONE',  ( 21.11101077988997332, 69.57631526528561494, -69.53839275343867143 ) ) ;
#79505 = AXIS2_PLACEMENT_3D ( 'NONE', #50232, #124662, #129782 ) ;
#79506 = LINE ( 'NONE', #198186, #120621 ) ;
#79507 = EDGE_CURVE ( 'NONE', #187000, #236168, #172520, .T. ) ;
#79508 = CARTESIAN_POINT ( 'NONE',  ( 18.59999999999999432, -1.162701749926853712, -108.6000000000000227 ) ) ;
#79509 = ORIENTED_EDGE ( 'NONE', *, *, #146724, .F. ) ;
#79510 = CARTESIAN_POINT ( 'NONE',  ( 21.05000000000000071, 77.36087058720436005, -161.9501095574333931 ) ) ;
#79511 = VERTEX_POINT ( 'NONE', #33006 ) ;
#79512 = DIRECTION ( 'NONE',  ( -1.000000000000000000, 0.000000000000000000, 0.000000000000000000 ) ) ;
#79513 = EDGE_LOOP ( 'NONE', ( #117420, #116678, #89193, #56504 ) ) ;
#79514 = DIRECTION ( 'NONE',  ( 0.000000000000000000, -1.000000000000000000, -6.982962677686266711E-15 ) ) ;
#79515 = CIRCLE ( 'NONE', #33789, 7.900000000000000355 ) ;
#79516 = AXIS2_PLACEMENT_3D ( 'NONE', #85439, #88019, #244543 ) ;
#79517 = CARTESIAN_POINT ( 'NONE',  ( 18.40000000000000568, 85.50000000001136868, -29.10095763519384704 ) ) ;
#79518 = VECTOR ( 'NONE', #170716, 1000.000000000000000 ) ;
#79519 = ORIENTED_EDGE ( 'NONE', *, *, #183603, .F. ) ;
#79520 = DIRECTION ( 'NONE',  ( 0.000000000000000000, 0.8814952561688430555, -0.4721928772777346239 ) ) ;
#79521 = ORIENTED_EDGE ( 'NONE', *, *, #14390, .T. ) ;
#79522 = DIRECTION ( 'NONE',  ( 1.000000000000000000, 0.000000000000000000, 0.000000000000000000 ) ) ;
#79523 = CARTESIAN_POINT ( 'NONE',  ( 23.15000000000000213, 82.57900542960499024, -215.5587758314583766 ) ) ;
#79524 = DIRECTION ( 'NONE',  ( -1.000000000000000000, 1.836970198721029934E-16, 1.601412966608202925E-30 ) ) ;
#79525 = CARTESIAN_POINT ( 'NONE',  ( -18.42637059832563295, 77.14546960815955856, -241.8200751569217459 ) ) ;
#79526 = FACE_OUTER_BOUND ( 'NONE', #254827, .T. ) ;
#79527 = B_SPLINE_CURVE_WITH_KNOTS ( 'NONE', 3,
 ( #253845, #45716, #125261, #204775, #66576, #59469, #19093, #139005 ),
 .UNSPECIFIED., .F., .F.,
 ( 4, 2, 2, 4 ),
 ( 0.000000000000000000, 6.534141206311429892E-05, 0.0001306828241262285978, 0.0002613656482524603399 ),
 .UNSPECIFIED. ) ;
#79529 = CARTESIAN_POINT ( 'NONE',  ( 20.85000000000000142, 0.1610488207298751417, -100.2158101556398293 ) ) ;
#79528 = SPHERICAL_SURFACE ( 'NONE', #41510, 0.1000000000000000056 ) ;
#79530 = TOROIDAL_SURFACE ( 'NONE', #133534, 7.800000000000000711, 0.1000000000000000056 ) ;
#79531 = DIRECTION ( 'NONE',  ( 0.000000000000000000, 1.000000000000000000, -1.224646799147353207E-16 ) ) ;
#79533 = ORIENTED_EDGE ( 'NONE', *, *, #120961, .F. ) ;
#79532 = CARTESIAN_POINT ( 'NONE',  ( 20.19326291201646129, 65.84393901210815159, -128.7612456769174685 ) ) ;
#79535 = CYLINDRICAL_SURFACE ( 'NONE', #197383, 7.900000000000003908 ) ;
#79534 = CARTESIAN_POINT ( 'NONE',  ( 20.95000000000005258, 66.15000000001120384, -5.923107484524795296 ) ) ;
#79536 = ORIENTED_EDGE ( 'NONE', *, *, #227729, .T. ) ;
#79538 = ORIENTED_EDGE ( 'NONE', *, *, #220741, .F. ) ;
#79537 = DIRECTION ( 'NONE',  ( 0.000000000000000000, -0.2617529984165152257, -0.9651348961777124202 ) ) ;
#79539 = VERTEX_POINT ( 'NONE', #155507 ) ;
#79540 = DIRECTION ( 'NONE',  ( 1.000000000000000000, 0.000000000000000000, 0.000000000000000000 ) ) ;
#79541 = CARTESIAN_POINT ( 'NONE',  ( 23.15000000000000213, -11.64999999998884483, -167.4999999999999432 ) ) ;
#79542 = CARTESIAN_POINT ( 'NONE',  ( -23.15000000000000213, 55.98745301258801987, -232.8057040749261262 ) ) ;
#79543 = CARTESIAN_POINT ( 'NONE',  ( -17.80356949363709163, 21.33262576353195072, -229.0023278304047949 ) ) ;
#79544 = ORIENTED_EDGE ( 'NONE', *, *, #97066, .T. ) ;
#79545 = CARTESIAN_POINT ( 'NONE',  ( 21.05000000000000071, 1.115600667400684642E-11, -146.8750000000000000 ) ) ;
#79546 = FACE_OUTER_BOUND ( 'NONE', #87520, .T. ) ;
#79547 = DIRECTION ( 'NONE',  ( 1.000000000000000000, 1.186688945009010077E-16, 0.000000000000000000 ) ) ;
#79548 = ORIENTED_EDGE ( 'NONE', *, *, #6908, .T. ) ;
#79549 = CARTESIAN_POINT ( 'NONE',  ( -21.05000000000000071, 1.115649653272650466E-11, -71.00000000000001421 ) ) ;
#79550 = AXIS2_PLACEMENT_3D ( 'NONE', #141462, #137591, #59320 ) ;
#79551 = CIRCLE ( 'NONE', #154617, 0.5000000000000004441 ) ;
#79553 = EDGE_CURVE ( 'NONE', #255448, #253555, #202631, .T. ) ;
#79552 = AXIS2_PLACEMENT_3D ( 'NONE', #189549, #211686, #129567 ) ;
#79555 = CIRCLE ( 'NONE', #150325, 2.100000000000004530 ) ;
#79554 = CARTESIAN_POINT ( 'NONE',  ( 21.10320863425824811, 6.400277386459165996, 0.02502225122713586103 ) ) ;
#79556 = VERTEX_POINT ( 'NONE', #175084 ) ;
#79557 = ORIENTED_EDGE ( 'NONE', *, *, #241972, .T. ) ;
#79558 = FACE_OUTER_BOUND ( 'NONE', #178516, .T. ) ;
#79559 = ORIENTED_EDGE ( 'NONE', *, *, #168274, .T. ) ;
#79560 = VECTOR ( 'NONE', #217048, 1000.000000000000000 ) ;
#79561 = DIRECTION ( 'NONE',  ( -1.000000000000000000, 0.000000000000000000, 0.000000000000000000 ) ) ;
#79562 = ORIENTED_EDGE ( 'NONE', *, *, #48420, .F. ) ;
#79563 = CARTESIAN_POINT ( 'NONE',  ( 20.94999675878240808, 10.29307482169070731, -172.9586421466940465 ) ) ;
#79564 = LINE ( 'NONE', #3901, #106469 ) ;
#79565 = CARTESIAN_POINT ( 'NONE',  ( 21.05000000000000071, -8.999999999988842703, -57.10603087734755690 ) ) ;
#79567 = EDGE_CURVE ( 'NONE', #189058, #153937, #154236, .T. ) ;
#79566 = AXIS2_PLACEMENT_3D ( 'NONE', #23409, #220306, #2509 ) ;
#79568 = EDGE_CURVE ( 'NONE', #231047, #128423, #156782, .T. ) ;
#79569 = CARTESIAN_POINT ( 'NONE',  ( 21.05000000000000071, -1.162701749926853712, -41.40000000000000568 ) ) ;
#79570 = CARTESIAN_POINT ( 'NONE',  ( -22.50875500270928953, -0.1008579137641491541, -88.75043287260213276 ) ) ;
#79571 = DIRECTION ( 'NONE',  ( -0.7071067811865708874, 0.3338907855511046296, 0.6233112732207185536 ) ) ;
#79572 = VERTEX_POINT ( 'NONE', #250709 ) ;
#79574 = CARTESIAN_POINT ( 'NONE',  ( 18.59999999999999787, -10.74999999999999289, 31.59999999999999787 ) ) ;
#79573 = CYLINDRICAL_SURFACE ( 'NONE', #154107, 0.09999999999999939493 ) ;
#79575 = ORIENTED_EDGE ( 'NONE', *, *, #8106, .T. ) ;
#79578 = ORIENTED_EDGE ( 'NONE', *, *, #247778, .F. ) ;
#79577 = DIRECTION ( 'NONE',  ( -0.000000000000000000, -0.9770955615653316162, -0.2128009952263604232 ) ) ;
#79576 = DIRECTION ( 'NONE',  ( -0.000000000000000000, -0.000000000000000000, 1.000000000000000000 ) ) ;
#79579 = EDGE_LOOP ( 'NONE', ( #190941, #94657, #145872, #84165 ) ) ;
#79580 = DIRECTION ( 'NONE',  ( -0.000000000000000000, 0.8814952561688430555, -0.4721928772777346239 ) ) ;
#79581 = FACE_OUTER_BOUND ( 'NONE', #254067, .T. ) ;
#79582 = DIRECTION ( 'NONE',  ( -0.000000000000000000, 0.4721928772777345684, 0.8814952561688429444 ) ) ;
#79583 = EDGE_CURVE ( 'NONE', #71736, #24624, #214162, .T. ) ;
#79584 = CARTESIAN_POINT ( 'NONE',  ( -18.40000000000000213, 64.58541674041221370, -115.6731074845243938 ) ) ;
#79585 = ORIENTED_EDGE ( 'NONE', *, *, #153694, .T. ) ;
#79586 = DIRECTION ( 'NONE',  ( 0.000000000000000000, 0.9126074666063771490, 0.4088369013363276627 ) ) ;
#79587 = EDGE_CURVE ( 'NONE', #58261, #245971, #254536, .T. ) ;
#79588 = TOROIDAL_SURFACE ( 'NONE', #225328, 0.2000000000000000111, 0.1000000000000000056 ) ;
#79589 = CARTESIAN_POINT ( 'NONE',  ( 23.40000000000005542, 77.16254490893143725, -43.92310748452479885 ) ) ;
#79590 = EDGE_CURVE ( 'NONE', #15098, #171125, #244316, .T. ) ;
#79592 = DIRECTION ( 'NONE',  ( -0.000000000000000000, -0.1290532225515392817, -0.9916376685811522096 ) ) ;
#79591 = DIRECTION ( 'NONE',  ( 1.000000000000000000, 0.000000000000000000, 0.000000000000000000 ) ) ;
#79594 = ORIENTED_EDGE ( 'NONE', *, *, #236214, .F. ) ;
#79593 = DIRECTION ( 'NONE',  ( -1.020425574104004196E-15, 0.000000000000000000, 1.000000000000000000 ) ) ;
#79595 = AXIS2_PLACEMENT_3D ( 'NONE', #226021, #163517, #146499 ) ;
#79596 = EDGE_CURVE ( 'NONE', #249596, #130308, #235014, .T. ) ;
#79597 = ORIENTED_EDGE ( 'NONE', *, *, #7762, .F. ) ;
#79598 = CIRCLE ( 'NONE', #229646, 0.1000000000000017958 ) ;
#79599 = B_SPLINE_CURVE_WITH_KNOTS ( 'NONE', 3,
 ( #161506, #141913, #221431, #83197, #44109, #242296, #63661, #123654 ),
 .UNSPECIFIED., .F., .F.,
 ( 4, 2, 2, 4 ),
 ( 0.000000000000000000, 0.0001306511400391352018, 0.0001959767100587012307, 0.0002613022800782672595 ),
 .UNSPECIFIED. ) ;
#79600 = DIRECTION ( 'NONE',  ( 0.000000000000000000, 0.000000000000000000, -1.000000000000000000 ) ) ;
#79602 = ORIENTED_EDGE ( 'NONE', *, *, #42869, .F. ) ;
#79601 = CIRCLE ( 'NONE', #175503, 0.1000000000000012546 ) ;
#79603 = CARTESIAN_POINT ( 'NONE',  ( -23.15000000000000213, 1.115600667400684642E-11, -167.5000000000000284 ) ) ;
#79604 = EDGE_CURVE ( 'NONE', #200654, #212362, #57044, .T. ) ;
#79605 = ORIENTED_EDGE ( 'NONE', *, *, #210825, .F. ) ;
#79606 = CARTESIAN_POINT ( 'NONE',  ( -21.05000000000000071, 1.162701749938009677, -8.099999999999999645 ) ) ;
#79607 = TOROIDAL_SURFACE ( 'NONE', #196318, 11.65000000000000036, 0.1000000000000000056 ) ;
#79608 = CYLINDRICAL_SURFACE ( 'NONE', #232674, 0.5000000000000004441 ) ;
#79609 = DIRECTION ( 'NONE',  ( -1.000000000000000000, 7.304098846218135653E-16, 0.000000000000000000 ) ) ;
#79610 = EDGE_LOOP ( 'NONE', ( #215204, #223227, #39617, #217756, #159901 ) ) ;
#79611 = CARTESIAN_POINT ( 'NONE',  ( -22.59999999999999787, 36.65892442174472876, -249.5511627012454596 ) ) ;
#79612 = AXIS2_PLACEMENT_3D ( 'NONE', #171478, #206713, #33250 ) ;
#79613 = EDGE_CURVE ( 'NONE', #24834, #105325, #193321, .T. ) ;
#79614 = CIRCLE ( 'NONE', #225369, 0.09999999999999939493 ) ;
#79615 = CARTESIAN_POINT ( 'NONE',  ( -21.29999999999995808, 36.65892442174472876, -249.5511627012454596 ) ) ;
#79616 = CIRCLE ( 'NONE', #63057, 0.5000000000000048850 ) ;
#79617 = ORIENTED_EDGE ( 'NONE', *, *, #80881, .T. ) ;
#79618 = ORIENTED_EDGE ( 'NONE', *, *, #208437, .T. ) ;
#79619 = AXIS2_PLACEMENT_3D ( 'NONE', #252983, #172222, #116063 ) ;
#79620 = ORIENTED_EDGE ( 'NONE', *, *, #33315, .T. ) ;
#79621 = DIRECTION ( 'NONE',  ( 0.000000000000000000, -0.4088369013363783999, 0.9126074666063545004 ) ) ;
#79622 = ORIENTED_EDGE ( 'NONE', *, *, #135713, .T. ) ;
#79624 = ORIENTED_EDGE ( 'NONE', *, *, #66209, .T. ) ;
#79623 = DIRECTION ( 'NONE',  ( -1.000000000000000000, -0.000000000000000000, 0.000000000000000000 ) ) ;
#79625 = CIRCLE ( 'NONE', #225376, 0.09999999999999939493 ) ;
#79626 = VERTEX_POINT ( 'NONE', #137186 ) ;
#79629 = VERTEX_POINT ( 'NONE', #57635 ) ;
#79628 = ORIENTED_EDGE ( 'NONE', *, *, #187651, .T. ) ;
#79627 = CARTESIAN_POINT ( 'NONE',  ( 23.14999999999999503, 11.75000000001116263, -21.75000000000000355 ) ) ;
#79630 = EDGE_LOOP ( 'NONE', ( #22961, #226811, #143922, #120680 ) ) ;
#79631 = LINE ( 'NONE', #159216, #39863 ) ;
#79632 = VECTOR ( 'NONE', #155841, 1000.000000000000000 ) ;
#79633 = AXIS2_PLACEMENT_3D ( 'NONE', #178422, #58414, #137962 ) ;
#79634 = AXIS2_PLACEMENT_3D ( 'NONE', #65995, #28190, #69870 ) ;
#79635 = DIRECTION ( 'NONE',  ( 0.000000000000000000, 6.982962677686266711E-15, -1.000000000000000000 ) ) ;
#79636 = CIRCLE ( 'NONE', #530, 0.09999999999998898659 ) ;
#79637 = EDGE_CURVE ( 'NONE', #205457, #137667, #36257, .T. ) ;
#79638 = CARTESIAN_POINT ( 'NONE',  ( -16.77308656112213470, 14.15896047666961977, -219.2548837893815801 ) ) ;
#79639 = EDGE_CURVE ( 'NONE', #130077, #77719, #90382, .T. ) ;
#79640 = ORIENTED_EDGE ( 'NONE', *, *, #38386, .F. ) ;
#79641 = CARTESIAN_POINT ( 'NONE',  ( -20.94999999999999929, 69.25047167775285573, -247.4556800696333596 ) ) ;
#79643 = ORIENTED_EDGE ( 'NONE', *, *, #42962, .T. ) ;
#79642 = CARTESIAN_POINT ( 'NONE',  ( -18.59999999999999787, 70.22659352830977753, -197.9852579278363578 ) ) ;
#79644 = CARTESIAN_POINT ( 'NONE',  ( 23.15000000000000213, 85.00000000001197975, -112.9170766071766820 ) ) ;
#79646 = VERTEX_POINT ( 'NONE', #56347 ) ;
#79645 = CARTESIAN_POINT ( 'NONE',  ( -23.15000000000000213, -11.48912529306489994, -63.89999999999999858 ) ) ;
#79647 = EDGE_CURVE ( 'NONE', #102088, #171936, #61176, .T. ) ;
#79648 = EDGE_CURVE ( 'NONE', #91629, #166025, #81988, .T. ) ;
#79649 = ORIENTED_EDGE ( 'NONE', *, *, #88526, .F. ) ;
#79650 = DIRECTION ( 'NONE',  ( -1.000000000000000000, 0.000000000000000000, 0.000000000000000000 ) ) ;
#79651 = EDGE_CURVE ( 'NONE', #182491, #94835, #206916, .T. ) ;
#79652 = VERTEX_POINT ( 'NONE', #176338 ) ;
#79653 = EDGE_LOOP ( 'NONE', ( #223930, #183627, #221631, #90500 ) ) ;
#79654 = CARTESIAN_POINT ( 'NONE',  ( -16.93909480342659890, 9.993078364812696179, -180.1003470166722877 ) ) ;
#79656 = ADVANCED_FACE ( 'NONE', ( #255804 ), #236140, .T. ) ;
#79655 = DIRECTION ( 'NONE',  ( 1.000000000000000000, -7.304098846218133681E-16, -2.111765289898285610E-31 ) ) ;
#79657 = EDGE_CURVE ( 'NONE', #44689, #156098, #215290, .T. ) ;
#79659 = ORIENTED_EDGE ( 'NONE', *, *, #205832, .T. ) ;
#79658 = ORIENTED_EDGE ( 'NONE', *, *, #216098, .F. ) ;
#79660 = EDGE_LOOP ( 'NONE', ( #181628, #50011, #74265, #170520 ) ) ;
#79661 = DIRECTION ( 'NONE',  ( 1.000000000000000000, -0.000000000000000000, 0.000000000000000000 ) ) ;
#79662 = ORIENTED_EDGE ( 'NONE', *, *, #158622, .T. ) ;
#79663 = VERTEX_POINT ( 'NONE', #52498 ) ;
#79664 = EDGE_CURVE ( 'NONE', #126429, #48124, #73673, .T. ) ;
#79665 = CYLINDRICAL_SURFACE ( 'NONE', #146777, 0.09999999999999939493 ) ;
#79666 = ORIENTED_EDGE ( 'NONE', *, *, #194064, .T. ) ;
#79668 = CARTESIAN_POINT ( 'NONE',  ( 23.25000000000000000, -9.599999999988842347, -191.1060308773475072 ) ) ;
#79667 = DIRECTION ( 'NONE',  ( 0.000000000000000000, -1.000000000000000000, -6.982962677686266711E-15 ) ) ;
#79669 = AXIS2_PLACEMENT_3D ( 'NONE', #25473, #81542, #125831 ) ;
#79670 = ORIENTED_EDGE ( 'NONE', *, *, #237261, .F. ) ;
#79671 = EDGE_CURVE ( 'NONE', #153892, #156274, #190184, .T. ) ;
#79673 = ORIENTED_EDGE ( 'NONE', *, *, #250234, .F. ) ;
#79672 = ORIENTED_EDGE ( 'NONE', *, *, #249001, .F. ) ;
#79674 = DIRECTION ( 'NONE',  ( 1.000000000000000000, 0.000000000000000000, 0.000000000000000000 ) ) ;
#79675 = CARTESIAN_POINT ( 'NONE',  ( 18.49999999999999289, 64.35000000001141984, -36.02310748452440237 ) ) ;
#79676 = ADVANCED_FACE ( 'NONE', ( #138442 ), #121506, .T. ) ;
#79677 = VERTEX_POINT ( 'NONE', #100591 ) ;
#79678 = EDGE_CURVE ( 'NONE', #132976, #106155, #81042, .T. ) ;
#79679 = AXIS2_PLACEMENT_3D ( 'NONE', #196180, #73694, #153238 ) ;
#79680 = DIRECTION ( 'NONE',  ( 0.000000000000000000, -0.000000000000000000, 1.000000000000000000 ) ) ;
#79681 = ORIENTED_EDGE ( 'NONE', *, *, #158371, .F. ) ;
#79682 = VERTEX_POINT ( 'NONE', #238 ) ;
#79683 = CARTESIAN_POINT ( 'NONE',  ( 18.39999999999999503, 43.51275691321468031, -233.9088826807484622 ) ) ;
#79685 = ADVANCED_FACE ( 'NONE', ( #199757 ), #1432, .F. ) ;
#79684 = ORIENTED_EDGE ( 'NONE', *, *, #108378, .T. ) ;
#79686 = DIRECTION ( 'NONE',  ( -1.000000000000000000, 0.000000000000000000, 0.000000000000000000 ) ) ;
#79687 = FACE_OUTER_BOUND ( 'NONE', #123514, .T. ) ;
#79688 = ORIENTED_EDGE ( 'NONE', *, *, #210687, .F. ) ;
#79689 = EDGE_CURVE ( 'NONE', #136568, #119565, #86083, .T. ) ;
#79690 = DIRECTION ( 'NONE',  ( 0.000000000000000000, 0.8777080977375655291, -0.4791956752370622463 ) ) ;
#79691 = DIRECTION ( 'NONE',  ( 1.000000000000000000, -0.000000000000000000, 0.000000000000000000 ) ) ;
#79693 = CARTESIAN_POINT ( 'NONE',  ( -16.87683809663752399, 9.850000000011139178, -120.5976359818037196 ) ) ;
#79692 = CARTESIAN_POINT ( 'NONE',  ( 23.14999999999998437, 36.65892442174472876, -249.5511627012454596 ) ) ;
#79694 = CARTESIAN_POINT ( 'NONE',  ( -16.77683809663752257, 12.41293291551535916, -211.2574046339461233 ) ) ;
#79695 = LINE ( 'NONE', #219214, #33015 ) ;
#79696 = DIRECTION ( 'NONE',  ( -1.000000000000000000, -0.000000000000000000, -0.000000000000000000 ) ) ;
#79697 = CARTESIAN_POINT ( 'NONE',  ( -20.00857864376270001, 9.350000000011156942, -146.2500000000000284 ) ) ;
#79698 = CARTESIAN_POINT ( 'NONE',  ( -23.15000000000000213, 11.75000000001115552, -21.75000000000000355 ) ) ;
#79699 = AXIS2_PLACEMENT_3D ( 'NONE', #103794, #182085, #102501 ) ;
#79700 = EDGE_LOOP ( 'NONE', ( #114026, #179268, #79594 ) ) ;
#79701 = VECTOR ( 'NONE', #9794, 1000.000000000000114 ) ;
#79702 = AXIS2_PLACEMENT_3D ( 'NONE', #77572, #21503, #138820 ) ;
#79704 = EDGE_LOOP ( 'NONE', ( #78358, #97462, #68913, #242905 ) ) ;
#79703 = EDGE_LOOP ( 'NONE', ( #252486, #180374, #149363, #231534 ) ) ;
#79705 = ORIENTED_EDGE ( 'NONE', *, *, #192386, .F. ) ;
#79706 = EDGE_LOOP ( 'NONE', ( #99219, #132146, #54256, #5140 ) ) ;
#79707 = DIRECTION ( 'NONE',  ( -0.000000000000000000, 0.1298341882520054891, 0.9915357197604850459 ) ) ;
#79708 = CARTESIAN_POINT ( 'NONE',  ( 20.94999999999999929, 67.84340367245323478, -228.0791829662263410 ) ) ;
#79710 = CARTESIAN_POINT ( 'NONE',  ( 22.39999999999999503, 0.3085173699977246109, -229.9658011520297975 ) ) ;
#79709 = LINE ( 'NONE', #159288, #53623 ) ;
#79711 = DIRECTION ( 'NONE',  ( 0.000000000000000000, 0.9998779222360096863, -0.01562500000001061998 ) ) ;
#79712 = EDGE_LOOP ( 'NONE', ( #162989, #193100 ) ) ;
#79713 = CARTESIAN_POINT ( 'NONE',  ( 20.00000000000000355, 4.547418889303922462, 21.90000000000000213 ) ) ;
#79714 = DIRECTION ( 'NONE',  ( 0.000000000000000000, -0.1350103645451807555, -0.9908441862701610203 ) ) ;
#79716 = VECTOR ( 'NONE', #167846, 1000.000000000000000 ) ;
#79715 = DIRECTION ( 'NONE',  ( 0.000000000000000000, -0.2558827019433787542, 0.9667078373770204847 ) ) ;
#79717 = ORIENTED_EDGE ( 'NONE', *, *, #67450, .F. ) ;
#79718 = DIRECTION ( 'NONE',  ( -1.000000000000000000, -0.000000000000000000, 0.000000000000000000 ) ) ;
#79719 = CARTESIAN_POINT ( 'NONE',  ( -21.05000000000000071, 87.48912529308769592, -66.42310748452423752 ) ) ;
#79720 = VERTEX_POINT ( 'NONE', #122784 ) ;
#79721 = PLANE ( 'NONE',  #107896 ) ;
#79722 = CARTESIAN_POINT ( 'NONE',  ( 18.59999999999999076, 43.30036367478129478, -245.0872390055602352 ) ) ;
#79723 = CARTESIAN_POINT ( 'NONE',  ( -16.98495255085916966, 10.00556436600592214, -121.3653827937795313 ) ) ;
#79724 = CARTESIAN_POINT ( 'NONE',  ( 20.04142135623730070, 64.35000000001275566, -215.2731074845244450 ) ) ;
#79725 = CARTESIAN_POINT ( 'NONE',  ( 20.85000000000000142, 0.000000000000000000, -33.50000000000000000 ) ) ;
#79726 = VERTEX_POINT ( 'NONE', #58902 ) ;
#79727 = CARTESIAN_POINT ( 'NONE',  ( 18.45068634130096896, 46.98837814534854829, -255.3186415057529075 ) ) ;
#79728 = DIRECTION ( 'NONE',  ( 0.000000000000000000, 0.000000000000000000, -1.000000000000000000 ) ) ;
#79729 = CARTESIAN_POINT ( 'NONE',  ( -20.94999999999999929, 68.97833521811159585, -65.68954208262705663 ) ) ;
#79730 = EDGE_CURVE ( 'NONE', #41537, #28425, #216198, .T. ) ;
#79733 = DIRECTION ( 'NONE',  ( 1.000000000000000000, 0.000000000000000000, 0.000000000000000000 ) ) ;
#79732 = AXIS2_PLACEMENT_3D ( 'NONE', #50566, #72759, #210957 ) ;
#79731 = DIRECTION ( 'NONE',  ( -0.000000000000000000, 1.000000000000000000, 6.982962677686266711E-15 ) ) ;
#79735 = DIRECTION ( 'NONE',  ( 0.000000000000000000, -1.156482317317873105E-15, -1.000000000000000000 ) ) ;
#79734 = AXIS2_PLACEMENT_3D ( 'NONE', #115465, #174209, #32109 ) ;
#79736 = LINE ( 'NONE', #74669, #12495 ) ;
#79738 = EDGE_CURVE ( 'NONE', #119168, #64013, #6997, .T. ) ;
#79737 = DIRECTION ( 'NONE',  ( 1.000000000000000000, 0.000000000000000000, 0.000000000000000000 ) ) ;
#79739 = CARTESIAN_POINT ( 'NONE',  ( -22.39999999999999858, 75.90000000001194280, -103.0231074845243171 ) ) ;
#79740 = ORIENTED_EDGE ( 'NONE', *, *, #39156, .F. ) ;
#79741 = EDGE_LOOP ( 'NONE', ( #192516, #131953, #41367 ) ) ;
#79742 = EDGE_CURVE ( 'NONE', #199626, #169837, #217982, .T. ) ;
#79743 = EDGE_CURVE ( 'NONE', #246153, #242065, #105441, .T. ) ;
#79744 = ORIENTED_EDGE ( 'NONE', *, *, #35478, .T. ) ;
#79745 = CARTESIAN_POINT ( 'NONE',  ( 21.05000000000000071, -9.000000000000000000, -23.60603087734755690 ) ) ;
#79746 = AXIS2_PLACEMENT_3D ( 'NONE', #238250, #58312, #162590 ) ;
#79747 = CARTESIAN_POINT ( 'NONE',  ( 18.54999999999999716, 52.10946721379481517, -233.0415979755771900 ) ) ;
#79748 = FACE_OUTER_BOUND ( 'NONE', #104354, .T. ) ;
#79749 = CARTESIAN_POINT ( 'NONE',  ( 22.47071067811864964, 65.11488425470513164, -243.2801022963548689 ) ) ;
#79750 = ORIENTED_EDGE ( 'NONE', *, *, #221889, .T. ) ;
#79751 = CYLINDRICAL_SURFACE ( 'NONE', #38864, 0.1000000000000028644 ) ;
#79752 = ADVANCED_FACE ( 'NONE', ( #67923 ), #28852, .F. ) ;
#79753 = DIRECTION ( 'NONE',  ( -0.000000000000000000, 1.000000000000000000, 6.982962677686267499E-15 ) ) ;
#79754 = CARTESIAN_POINT ( 'NONE',  ( -18.50000324121759121, 65.70692517833234092, -97.56446533783034170 ) ) ;
#79755 = DIRECTION ( 'NONE',  ( 1.000000000000000000, 0.000000000000000000, 0.000000000000000000 ) ) ;
#79757 = ORIENTED_EDGE ( 'NONE', *, *, #112376, .F. ) ;
#79756 = CARTESIAN_POINT ( 'NONE',  ( -16.87998658237754768, 9.950000000011263168, -188.1363604322614833 ) ) ;
#79759 = CARTESIAN_POINT ( 'NONE',  ( -16.87036670365548474, 9.989418819312804843, -154.9795601173020714 ) ) ;
#79758 = FACE_OUTER_BOUND ( 'NONE', #200587, .T. ) ;
#79761 = CARTESIAN_POINT ( 'NONE',  ( -23.15000000000000213, 62.12679871018154643, -248.6611778639222337 ) ) ;
#79760 = VECTOR ( 'NONE', #107601, 1000.000000000000000 ) ;
#79762 =( NAMED_UNIT ( * ) PLANE_ANGLE_UNIT ( ) SI_UNIT ( $, .RADIAN. ) );
#79763 = ORIENTED_EDGE ( 'NONE', *, *, #143489, .F. ) ;
#79764 = AXIS2_PLACEMENT_3D ( 'NONE', #122759, #223108, #245261 ) ;
#79765 = CARTESIAN_POINT ( 'NONE',  ( 0.000000000000000000, 0.000000000000000000, 0.000000000000000000 ) ) ;
#79766 = DIRECTION ( 'NONE',  ( -1.000000000000000000, -7.166229603267618227E-16, -4.447280054184918885E-16 ) ) ;
#79767 = EDGE_CURVE ( 'NONE', #118980, #7608, #143605, .T. ) ;
#79768 = CARTESIAN_POINT ( 'NONE',  ( -23.25000000000000000, 70.22889768795992893, -198.1282601183952750 ) ) ;
#79769 = ORIENTED_EDGE ( 'NONE', *, *, #246193, .T. ) ;
#79770 = VECTOR ( 'NONE', #190494, 1000.000000000000000 ) ;
#79771 = CYLINDRICAL_SURFACE ( 'NONE', #79391, 0.09999999999999939493 ) ;
#79772 = CARTESIAN_POINT ( 'NONE',  ( -21.05000000000000071, -11.48912529306490349, -69.90000000000004832 ) ) ;
#79773 = ADVANCED_FACE ( 'NONE', ( #243983 ), #186606, .T. ) ;
#79774 = EDGE_LOOP ( 'NONE', ( #221142, #212136, #161806, #212068 ) ) ;
#79775 = DIRECTION ( 'NONE',  ( 1.000000000000000000, 0.000000000000000000, 0.000000000000000000 ) ) ;
#79776 = AXIS2_PLACEMENT_3D ( 'NONE', #224426, #203587, #168364 ) ;
#79778 = DIRECTION ( 'NONE',  ( -0.000000000000000000, 0.8660254037844411501, 0.4999999999999956701 ) ) ;
#79777 = VECTOR ( 'NONE', #71178, 1000.000000000000000 ) ;
#79779 = LINE ( 'NONE', #38131, #95152 ) ;
#79780 = ORIENTED_EDGE ( 'NONE', *, *, #209234, .F. ) ;
#79781 = ORIENTED_EDGE ( 'NONE', *, *, #69886, .F. ) ;
#79782 = EDGE_CURVE ( 'NONE', #139626, #250872, #2896, .T. ) ;
#79783 = AXIS2_PLACEMENT_3D ( 'NONE', #249403, #186867, #147728 ) ;
#79784 = EDGE_CURVE ( 'NONE', #198561, #192673, #161135, .T. ) ;
#79785 = CARTESIAN_POINT ( 'NONE',  ( 20.95512820512820440, 8.876151316299271343, -112.6500000000000341 ) ) ;
#79786 = CARTESIAN_POINT ( 'NONE',  ( -22.39999999999999858, 1.115600667400684642E-11, -92.70922040162662370 ) ) ;
#79787 = CARTESIAN_POINT ( 'NONE',  ( 23.15000000000000213, 85.60000000001208775, -126.6291383618717816 ) ) ;
#79789 = DIRECTION ( 'NONE',  ( -0.000000000000000000, -0.000000000000000000, -1.000000000000000000 ) ) ;
#79788 = CARTESIAN_POINT ( 'NONE',  ( 18.79999999999999716, 0.000000000000000000, 32.89999999999999858 ) ) ;
#79791 = ADVANCED_FACE ( 'NONE', ( #228295 ), #26246, .F. ) ;
#79790 = AXIS2_PLACEMENT_3D ( 'NONE', #78269, #178706, #59983 ) ;
#79792 = CARTESIAN_POINT ( 'NONE',  ( -18.38639463286148867, 58.57254856461742065, -223.9226520559630558 ) ) ;
#79793 = CARTESIAN_POINT ( 'NONE',  ( 23.14999999999999858, 11.60000000001116227, -194.0717967697244717 ) ) ;
#79794 = AXIS2_PLACEMENT_3D ( 'NONE', #24473, #4844, #85657 ) ;
#79795 = VERTEX_POINT ( 'NONE', #84876 ) ;
#79796 = DIRECTION ( 'NONE',  ( -1.000000000000000000, -0.000000000000000000, -0.000000000000000000 ) ) ;
#79798 = ORIENTED_EDGE ( 'NONE', *, *, #147617, .F. ) ;
#79797 = CYLINDRICAL_SURFACE ( 'NONE', #219663, 0.09999999999999939493 ) ;
#79799 = CARTESIAN_POINT ( 'NONE',  ( 22.49999999999999645, 11.64957080754479968, 0.09999999999999595324 ) ) ;
#79800 = DIRECTION ( 'NONE',  ( 1.000000000000000000, 0.000000000000000000, 0.000000000000000000 ) ) ;
#79802 = CARTESIAN_POINT ( 'NONE',  ( 23.24999999999999645, 70.35000000001224407, -149.1731074845243938 ) ) ;
#79801 = DIRECTION ( 'NONE',  ( 1.186688945009010077E-16, 1.000000000000000000, 6.982962677686266711E-15 ) ) ;
#79803 = VECTOR ( 'NONE', #215780, 1000.000000000000000 ) ;
#79804 = EDGE_LOOP ( 'NONE', ( #178189, #12974, #231192, #105354, #110969, #141010, #46623, #56626, #198944, #21722, #89067 ) ) ;
#79806 = CARTESIAN_POINT ( 'NONE',  ( 21.05000000000000071, 5.900000000011162093, -56.78090023534362984 ) ) ;
#79805 = FACE_OUTER_BOUND ( 'NONE', #245598, .T. ) ;
#79807 = DIRECTION ( 'NONE',  ( 1.000000000000000000, 0.000000000000000000, 0.000000000000000000 ) ) ;
#79808 = EDGE_CURVE ( 'NONE', #228403, #175328, #10529, .T. ) ;
#79809 = DIRECTION ( 'NONE',  ( 0.000000000000000000, 0.2617529984165025692, 0.9651348961777157509 ) ) ;
#79810 = CARTESIAN_POINT ( 'NONE',  ( -23.15000000000000213, 76.00000000001126921, -203.5231074845248997 ) ) ;
#79812 = CARTESIAN_POINT ( 'NONE',  ( -12.33960340485503870, 66.63925083009745265, -186.2085373439171008 ) ) ;
#79811 = CIRCLE ( 'NONE', #204711, 0.09999999999999646672 ) ;
#79813 = ORIENTED_EDGE ( 'NONE', *, *, #79457, .T. ) ;
#79814 = PLANE ( 'NONE',  #188774 ) ;
#79815 = ORIENTED_EDGE ( 'NONE', *, *, #161247, .T. ) ;
#79816 = EDGE_CURVE ( 'NONE', #100189, #196305, #136148, .T. ) ;
#79817 = CARTESIAN_POINT ( 'NONE',  ( -22.19999999999999929, -11.75000000000000000, 32.89999999999999858 ) ) ;
#79818 = ORIENTED_EDGE ( 'NONE', *, *, #251041, .T. ) ;
#79820 = DIRECTION ( 'NONE',  ( 0.000000000000000000, -1.000000000000000000, 0.000000000000000000 ) ) ;
#79819 = CIRCLE ( 'NONE', #4791, 11.75000000000000000 ) ;
#79821 = AXIS2_PLACEMENT_3D ( 'NONE', #228309, #246565, #28865 ) ;
#79822 = ORIENTED_EDGE ( 'NONE', *, *, #103394, .F. ) ;
#79823 = CIRCLE ( 'NONE', #242142, 0.1000000000000024342 ) ;
#79824 = CARTESIAN_POINT ( 'NONE',  ( -21.40925344232282512, 6.658518859401606704, -167.4010498113803180 ) ) ;
#79825 = TOROIDAL_SURFACE ( 'NONE', #192853, 11.65000000000000036, 0.1000000000000000056 ) ;
#79826 = DIRECTION ( 'NONE',  ( 0.000000000000000000, -0.5000000000000016653, 0.8660254037844377084 ) ) ;
#79827 = EDGE_LOOP ( 'NONE', ( #165735, #206839, #155024, #139003 ) ) ;
#79828 =( BOUNDED_SURFACE ( )  B_SPLINE_SURFACE ( 3, 2, ( 
 ( #252728, #188924, #131510 ),
 ( #148519, #127672, #247611 ),
 ( #110667, #171967, #231918 ),
 ( #32451, #168124, #111969 ) ),
 .UNSPECIFIED., .F., .F., .T. ) 
 B_SPLINE_SURFACE_WITH_KNOTS ( ( 4, 4 ),
 ( 3, 3 ),
 ( 0.000000000000000000, 0.001979672783031562362 ),
 ( 0.000000000000000000, 1.000000000000000000 ),
 .UNSPECIFIED. ) 
 GEOMETRIC_REPRESENTATION_ITEM ( )  RATIONAL_B_SPLINE_SURFACE ( (
 ( 1.000000000000000000, 0.7103081912008026855, 1.000000000000000000),
 ( 1.000000000000000000, 0.7104998333558677492, 1.000000000000000000),
 ( 1.000000000000000000, 0.7107238315755500802, 1.000000000000000000),
 ( 1.000000000000000000, 0.7110073749539205235, 1.000000000000000000) ) ) 
 REPRESENTATION_ITEM ( '' )  SURFACE ( )  );
#79829 = FACE_OUTER_BOUND ( 'NONE', #126300, .T. ) ;
#79830 = DIRECTION ( 'NONE',  ( 1.000000000000000000, -2.952720810173289112E-16, -2.061873921506763405E-30 ) ) ;
#79831 = FACE_OUTER_BOUND ( 'NONE', #97506, .T. ) ;
#79832 = DIRECTION ( 'NONE',  ( 1.000000000000000000, -2.952720810173289112E-16, -2.061873921506763405E-30 ) ) ;
#79833 = DIRECTION ( 'NONE',  ( -1.000000000000000000, -2.885090398161910739E-16, -6.283419270304611573E-17 ) ) ;
#79834 = CARTESIAN_POINT ( 'NONE',  ( 19.83283456528360489, 62.39550153346884542, -208.7959266056268461 ) ) ;
#79835 = EDGE_LOOP ( 'NONE', ( #77786, #58265 ) ) ;
#79836 = VECTOR ( 'NONE', #104407, 1000.000000000000000 ) ;
#79837 = CARTESIAN_POINT ( 'NONE',  ( -18.59999999999999787, 69.01799029515495931, -32.32695536626808774 ) ) ;
#79838 = ORIENTED_EDGE ( 'NONE', *, *, #52501, .F. ) ;
#79840 = EDGE_LOOP ( 'NONE', ( #218374, #5870, #59438, #157980 ) ) ;
#79839 = CARTESIAN_POINT ( 'NONE',  ( -16.27683809663751191, 9.350000000011132073, -79.55000000000005400 ) ) ;
#79841 = ORIENTED_EDGE ( 'NONE', *, *, #253248, .F. ) ;
#79842 = CARTESIAN_POINT ( 'NONE',  ( 21.13736287352038445, 67.95335762362863363, -194.2731074845244166 ) ) ;
#79843 = FACE_OUTER_BOUND ( 'NONE', #143758, .T. ) ;
#79844 = CARTESIAN_POINT ( 'NONE',  ( 13.54556439290363024, 66.54940788787888550, -188.4669191657160638 ) ) ;
#79845 =( BOUNDED_CURVE ( )  B_SPLINE_CURVE ( 3, ( #116127, #17031, #159119, #157853 ),
 .UNSPECIFIED., .F., .F. ) 
 B_SPLINE_CURVE_WITH_KNOTS ( ( 4, 4 ),
 ( 3.432212674861197854, 3.693332928900581180 ),
 .UNSPECIFIED. ) 
 CURVE ( )  GEOMETRIC_REPRESENTATION_ITEM ( )  RATIONAL_B_SPLINE_CURVE ( ( 1.000000000000000000, 0.9943260843901262636, 0.9943260843901262636, 1.000000000000000000 ) ) 
 REPRESENTATION_ITEM ( '' )  );
#79846 = CARTESIAN_POINT ( 'NONE',  ( 21.05000000000000071, 60.15342460706035865, -221.3466381063981032 ) ) ;
#79847 = LINE ( 'NONE', #159429, #79183 ) ;
#79848 = ORIENTED_EDGE ( 'NONE', *, *, #255374, .T. ) ;
#79849 = CARTESIAN_POINT ( 'NONE',  ( 23.24999999999999645, 7.128833340094563376, -233.7327013124401276 ) ) ;
#79850 = DIRECTION ( 'NONE',  ( 0.000000000000000000, -0.000000000000000000, 1.000000000000000000 ) ) ;
#79852 = ORIENTED_EDGE ( 'NONE', *, *, #228413, .T. ) ;
#79851 = PLANE ( 'NONE',  #59313 ) ;
#79853 = CARTESIAN_POINT ( 'NONE',  ( -20.94999999999999929, 10.29270135740183179, -38.95736188715193293 ) ) ;
#79854 = B_SPLINE_CURVE_WITH_KNOTS ( 'NONE', 3,
 ( #72796, #89741, #49346, #207149 ),
 .UNSPECIFIED., .F., .F.,
 ( 4, 4 ),
 ( 7.757919228897728493E-18, 0.0001058379652594581074 ),
 .UNSPECIFIED. ) ;
#79855 = ADVANCED_FACE ( 'NONE', ( #207450 ), #88748, .F. ) ;
#79856 = DIRECTION ( 'NONE',  ( 0.000000000000000000, 0.000000000000000000, -1.000000000000000000 ) ) ;
#79857 = ORIENTED_EDGE ( 'NONE', *, *, #35809, .F. ) ;
#79858 =( BOUNDED_CURVE ( )  B_SPLINE_CURVE ( 3, ( #21986, #101454, #40288, #138047 ),
 .UNSPECIFIED., .F., .F. ) 
 B_SPLINE_CURVE_WITH_KNOTS ( ( 4, 4 ),
 ( 4.712388980384689674, 5.672655318024873772 ),
 .UNSPECIFIED. ) 
 CURVE ( )  GEOMETRIC_REPRESENTATION_ITEM ( )  RATIONAL_B_SPLINE_CURVE ( ( 1.000000000000000000, 0.9246222802177073152, 0.9246222802177073152, 1.000000000000000000 ) ) 
 REPRESENTATION_ITEM ( '' )  );
#79859 = CIRCLE ( 'NONE', #225599, 0.09999999999999939493 ) ;
#79860 = DIRECTION ( 'NONE',  ( 0.7071359030027593029, -0.7070776581709197206, 0.000000000000000000 ) ) ;
#79861 = ORIENTED_EDGE ( 'NONE', *, *, #209427, .T. ) ;
#79862 = DIRECTION ( 'NONE',  ( -1.000000000000000000, 7.304098846218164250E-16, -4.217023435051628197E-16 ) ) ;
#79863 = EDGE_CURVE ( 'NONE', #35438, #121064, #31973, .T. ) ;
#79864 = CARTESIAN_POINT ( 'NONE',  ( -23.25000000000000000, 84.59626168225457832, -60.07297996737398194 ) ) ;
#79865 = CARTESIAN_POINT ( 'NONE',  ( 18.54999999999999716, 8.750000000000024869, -20.85000000000000142 ) ) ;
#79866 = DIRECTION ( 'NONE',  ( 0.000000000000000000, -0.6728971962617102953, -0.7397360091702507301 ) ) ;
#79867 = ADVANCED_FACE ( 'NONE', ( #225677 ), #7965, .F. ) ;
#79868 = EDGE_CURVE ( 'NONE', #135120, #246187, #104454, .T. ) ;
#79869 = AXIS2_PLACEMENT_3D ( 'NONE', #252961, #57319, #232143 ) ;
#79870 = AXIS2_PLACEMENT_3D ( 'NONE', #129443, #196788, #194265 ) ;
#79872 = ORIENTED_EDGE ( 'NONE', *, *, #160593, .T. ) ;
#79871 = CIRCLE ( 'NONE', #179882, 4.150000000000000355 ) ;
#79873 =( NAMED_UNIT ( * ) SI_UNIT ( $, .STERADIAN. ) SOLID_ANGLE_UNIT ( ) );
#79874 = ORIENTED_EDGE ( 'NONE', *, *, #202378, .F. ) ;
#79875 = LINE ( 'NONE', #98147, #22962 ) ;
#79876 = EDGE_CURVE ( 'NONE', #221149, #18233, #190375, .T. ) ;
#79877 = FACE_OUTER_BOUND ( 'NONE', #131235, .T. ) ;
#79879 = VERTEX_POINT ( 'NONE', #66645 ) ;
#79878 = DIRECTION ( 'NONE',  ( 0.000000000000000000, 0.000000000000000000, -1.000000000000000000 ) ) ;
#79880 = CARTESIAN_POINT ( 'NONE',  ( 18.49999999999999289, 69.55000000001187743, -93.00608031408432907 ) ) ;
#79881 = CARTESIAN_POINT ( 'NONE',  ( 20.94999999999999574, 39.29335463311362275, -236.8946393634874994 ) ) ;
#79882 = DIRECTION ( 'NONE',  ( -1.000000000000000000, -7.304098846218135653E-16, -4.639676173203994055E-30 ) ) ;
#79883 = CARTESIAN_POINT ( 'NONE',  ( -21.05000000000000071, 77.16270174994961906, -61.52310748452431710 ) ) ;
#79884 = CARTESIAN_POINT ( 'NONE',  ( -18.41799967126736348, 85.50000000001209344, -129.4910376712676907 ) ) ;
#79886 = ORIENTED_EDGE ( 'NONE', *, *, #221765, .T. ) ;
#79885 = DIRECTION ( 'NONE',  ( 1.000000000000000000, 0.000000000000000000, 0.000000000000000000 ) ) ;
#79887 = AXIS2_PLACEMENT_3D ( 'NONE', #108061, #183744, #67640 ) ;
#79888 = VERTEX_POINT ( 'NONE', #246548 ) ;
#79889 = ADVANCED_FACE ( 'NONE', ( #247844 ), #77910, .T. ) ;
#79890 = EDGE_LOOP ( 'NONE', ( #105552, #234953, #122567, #142694 ) ) ;
#79891 = EDGE_CURVE ( 'NONE', #251464, #89722, #105734, .T. ) ;
#79892 = DIRECTION ( 'NONE',  ( 1.000000000000000000, 0.000000000000000000, 0.000000000000000000 ) ) ;
#79893 = DIRECTION ( 'NONE',  ( 0.000000000000000000, 0.000000000000000000, 1.000000000000000000 ) ) ;
#79894 = VERTEX_POINT ( 'NONE', #165765 ) ;
#79895 = FACE_OUTER_BOUND ( 'NONE', #81535, .T. ) ;
#79896 = AXIS2_PLACEMENT_3D ( 'NONE', #189272, #74490, #50998 ) ;
#79897 = AXIS2_PLACEMENT_3D ( 'NONE', #182130, #42608, #201679 ) ;
#79899 = EDGE_CURVE ( 'NONE', #174422, #154105, #126613, .T. ) ;
#79898 = CARTESIAN_POINT ( 'NONE',  ( 23.14999999999999858, 5.599999999999996980, -12.40526601891309788 ) ) ;
#79900 = AXIS2_PLACEMENT_3D ( 'NONE', #210370, #151705, #171287 ) ;
#79901 = ORIENTED_EDGE ( 'NONE', *, *, #129390, .T. ) ;
#79902 = DIRECTION ( 'NONE',  ( -0.000000000000000000, -0.8814952561688430555, 0.4721928772777346239 ) ) ;
#79903 = CARTESIAN_POINT ( 'NONE',  ( -21.05000000000000071, 64.35000000001166143, -69.42310748452440805 ) ) ;
#79904 = ORIENTED_EDGE ( 'NONE', *, *, #231613, .T. ) ;
#79905 = VERTEX_POINT ( 'NONE', #131747 ) ;
#79906 = LINE ( 'NONE', #139896, #227656 ) ;
#79907 = ORIENTED_EDGE ( 'NONE', *, *, #107210, .F. ) ;
#79908 = DIRECTION ( 'NONE',  ( 0.000000000000000000, 0.000000000000000000, 1.000000000000000000 ) ) ;
#79910 = ORIENTED_EDGE ( 'NONE', *, *, #63567, .F. ) ;
#79909 = DIRECTION ( 'NONE',  ( 0.000000000000000000, 4.336808689942044242E-14, 1.000000000000000000 ) ) ;
#79911 = CARTESIAN_POINT ( 'NONE',  ( 20.94999999999999929, 87.39257802171739797, -72.59705706435616435 ) ) ;
#79912 = ORIENTED_EDGE ( 'NONE', *, *, #138256, .T. ) ;
#79913 = DIRECTION ( 'NONE',  ( 2.952720810173289112E-16, 1.000000000000000000, 6.982962677686266711E-15 ) ) ;
#79914 = EDGE_LOOP ( 'NONE', ( #85784, #179058, #88520, #210265 ) ) ;
#79916 = ORIENTED_EDGE ( 'NONE', *, *, #76872, .T. ) ;
#79915 = ORIENTED_EDGE ( 'NONE', *, *, #96991, .F. ) ;
#79917 = DIRECTION ( 'NONE',  ( 1.000000000000000000, -0.000000000000000000, -0.000000000000000000 ) ) ;
#79918 = ORIENTED_EDGE ( 'NONE', *, *, #107769, .T. ) ;
#79919 = CARTESIAN_POINT ( 'NONE',  ( -18.59999999999999787, 9.350000000011156942, -146.3500000000000227 ) ) ;
#79920 = EDGE_LOOP ( 'NONE', ( #91556, #130695, #16538, #70210 ) ) ;
#79921 = ADVANCED_FACE ( 'NONE', ( #195601 ), #54770, .T. ) ;
#79922 = EDGE_CURVE ( 'NONE', #234918, #228033, #114758, .T. ) ;
#79923 = VERTEX_POINT ( 'NONE', #112212 ) ;
#79924 = CARTESIAN_POINT ( 'NONE',  ( -21.44999999999999929, 7.150000000011155876, -45.85000000000000142 ) ) ;
#79926 = DIRECTION ( 'NONE',  ( 0.000000000000000000, 0.2128009952263604232, -0.9770955615653316162 ) ) ;
#79925 = AXIS2_PLACEMENT_3D ( 'NONE', #106919, #142204, #3976 ) ;
#79928 = ORIENTED_EDGE ( 'NONE', *, *, #169215, .T. ) ;
#79927 = DIRECTION ( 'NONE',  ( -1.000000000000000000, -0.000000000000000000, -0.000000000000000000 ) ) ;
#79929 = CARTESIAN_POINT ( 'NONE',  ( 20.94999999999999929, 5.499999999999998224, -12.40526601891309788 ) ) ;
#79930 = ORIENTED_EDGE ( 'NONE', *, *, #92632, .F. ) ;
#79931 = EDGE_CURVE ( 'NONE', #102379, #220040, #177896, .T. ) ;
#79933 = EDGE_CURVE ( 'NONE', #150745, #110468, #170933, .T. ) ;
#79932 = CARTESIAN_POINT ( 'NONE',  ( -20.54999999999999716, 61.88149656937975607, -248.1136133839584090 ) ) ;
#79934 = CARTESIAN_POINT ( 'NONE',  ( 20.94999999999999929, 44.34387878855809362, -247.3824414791181994 ) ) ;
#79935 = PLANE ( 'NONE',  #114780 ) ;
#79936 = AXIS2_PLACEMENT_3D ( 'NONE', #46729, #126268, #243657 ) ;
#79937 = ORIENTED_EDGE ( 'NONE', *, *, #59418, .F. ) ;
#79938 = CARTESIAN_POINT ( 'NONE',  ( 20.94999999999999929, 76.00000000001195133, -103.0231074845243171 ) ) ;
#79939 = CARTESIAN_POINT ( 'NONE',  ( -11.60000000000000320, -11.65000000000000036, 12.40000000000000391 ) ) ;
#79940 = CARTESIAN_POINT ( 'NONE',  ( -21.14999999999999858, 76.10000000001174669, -81.17267829206912211 ) ) ;
#79941 = AXIS2_PLACEMENT_3D ( 'NONE', #18359, #196979, #96582 ) ;
#79942 = EDGE_CURVE ( 'NONE', #147896, #77589, #210016, .T. ) ;
#79944 = VERTEX_POINT ( 'NONE', #254242 ) ;
#79943 = VECTOR ( 'NONE', #222038, 1000.000000000000227 ) ;
#79945 = DIRECTION ( 'NONE',  ( 0.000000000000000000, 0.8814952561688430555, -0.4721928772777346239 ) ) ;
#79946 = ORIENTED_EDGE ( 'NONE', *, *, #100180, .T. ) ;
#79947 = ORIENTED_EDGE ( 'NONE', *, *, #137418, .F. ) ;
#79948 = ADVANCED_FACE ( 'NONE', ( #213856 ), #153936, .F. ) ;
#79951 = EDGE_CURVE ( 'NONE', #135981, #155470, #193019, .T. ) ;
#79950 = EDGE_CURVE ( 'NONE', #236070, #119208, #15687, .T. ) ;
#79949 = CIRCLE ( 'NONE', #113305, 0.09999999999999939493 ) ;
#79952 = DIRECTION ( 'NONE',  ( -1.000000000000000000, 2.952720810173289112E-16, 2.061873921506763405E-30 ) ) ;
#79953 = VERTEX_POINT ( 'NONE', #113465 ) ;
#79954 = ORIENTED_EDGE ( 'NONE', *, *, #231477, .T. ) ;
#79955 = CARTESIAN_POINT ( 'NONE',  ( 28.12018973533754362, 11.62642356364896123, -347.0000000000001137 ) ) ;
#79956 = CARTESIAN_POINT ( 'NONE',  ( -16.93415306273742260, 9.995622260023671046, -188.4100569423603702 ) ) ;
#79957 = ORIENTED_EDGE ( 'NONE', *, *, #229143, .T. ) ;
#79958 = ADVANCED_FACE ( 'NONE', ( #155201 ), #95192, .F. ) ;
#79959 = VERTEX_POINT ( 'NONE', #173505 ) ;
#79960 = CARTESIAN_POINT ( 'NONE',  ( -21.29999999999995808, 10.69888912757691024, -235.6450824654141059 ) ) ;
#79961 = CIRCLE ( 'NONE', #134148, 0.09999999999999999167 ) ;
#79962 = FACE_OUTER_BOUND ( 'NONE', #156356, .T. ) ;
#79964 = ORIENTED_EDGE ( 'NONE', *, *, #70099, .T. ) ;
#79963 = CIRCLE ( 'NONE', #229841, 0.09999999999999939493 ) ;
#79965 = EDGE_CURVE ( 'NONE', #216782, #197918, #53500, .T. ) ;
#79966 = ORIENTED_EDGE ( 'NONE', *, *, #24063, .T. ) ;
#79967 = VECTOR ( 'NONE', #226439, 1000.000000000000000 ) ;
#79968 = EDGE_CURVE ( 'NONE', #209017, #118840, #198721, .T. ) ;
#79970 = EDGE_CURVE ( 'NONE', #230747, #53148, #73099, .T. ) ;
#79969 = CIRCLE ( 'NONE', #217533, 0.1000000000000028644 ) ;
#79971 = ORIENTED_EDGE ( 'NONE', *, *, #200111, .F. ) ;
#79972 = CIRCLE ( 'NONE', #67351, 12.77499999999999503 ) ;
#79973 = ADVANCED_FACE ( 'NONE', ( #151339 ), #150051, .T. ) ;
#79974 = FACE_OUTER_BOUND ( 'NONE', #215229, .T. ) ;
#79975 = CARTESIAN_POINT ( 'NONE',  ( 18.47073956224740954, 85.47172941248462052, -196.4144217317061134 ) ) ;
#79976 = AXIS2_PLACEMENT_3D ( 'NONE', #158844, #42718, #201785 ) ;
#79977 = FACE_OUTER_BOUND ( 'NONE', #188329, .T. ) ;
#79978 = DIRECTION ( 'NONE',  ( -0.000000000000000000, 0.000000000000000000, 1.000000000000000000 ) ) ;
#79979 = EDGE_CURVE ( 'NONE', #156671, #180654, #229578, .T. ) ;
#79980 = CARTESIAN_POINT ( 'NONE',  ( -23.15000000000000213, 59.07123845373075710, -221.0531397865252075 ) ) ;
#79981 = CARTESIAN_POINT ( 'NONE',  ( 21.05000000000000071, 75.90220970870393558, -209.7809220950004772 ) ) ;
#79982 = CARTESIAN_POINT ( 'NONE',  ( -17.11825945287482753, 65.95000000001262208, -190.8731074845244393 ) ) ;
#79984 = DIRECTION ( 'NONE',  ( -0.000000000000000000, -0.2617529984165031243, -0.9651348961777157509 ) ) ;
#79983 = CARTESIAN_POINT ( 'NONE',  ( -21.05000000000000071, 44.55458850188623643, -247.3966190010231969 ) ) ;
#79985 = DIRECTION ( 'NONE',  ( -1.000000000000000000, 0.000000000000000000, 0.000000000000000000 ) ) ;
#79987 = EDGE_CURVE ( 'NONE', #105113, #197047, #189051, .T. ) ;
#79986 = CARTESIAN_POINT ( 'NONE',  ( -16.77308656112215246, 22.97823775711153615, -230.9351546348684110 ) ) ;
#79988 = DIRECTION ( 'NONE',  ( 1.000000000000000000, 0.000000000000000000, 0.000000000000000000 ) ) ;
#79989 = AXIS2_PLACEMENT_3D ( 'NONE', #121906, #142721, #202706 ) ;
#79990 = DIRECTION ( 'NONE',  ( -1.000000000000000000, 0.000000000000000000, 0.000000000000000000 ) ) ;
#79991 = AXIS2_PLACEMENT_3D ( 'NONE', #76609, #253952, #117029 ) ;
#79992 = ORIENTED_EDGE ( 'NONE', *, *, #38458, .T. ) ;
#79993 = AXIS2_PLACEMENT_3D ( 'NONE', #16611, #111849, #171854 ) ;
#79995 = ORIENTED_EDGE ( 'NONE', *, *, #771, .T. ) ;
#79994 = CARTESIAN_POINT ( 'NONE',  ( -23.15000000000000213, 11.65000000000000036, -12.15000000000000036 ) ) ;
#79996 = ADVANCED_FACE ( 'NONE', ( #1201 ), #97724, .F. ) ;
#79997 = DIRECTION ( 'NONE',  ( 0.000000000000000000, -0.8700118002898356018, 0.4930308989875170078 ) ) ;
#79998 = CARTESIAN_POINT ( 'NONE',  ( -20.85000000000000142, 14.80545736607782814, -235.9842437978701639 ) ) ;
#79999 = CARTESIAN_POINT ( 'NONE',  ( 20.85000000000000142, -0.3238857010591806307, -167.4575895893140114 ) ) ;
#80000 = ORIENTED_EDGE ( 'NONE', *, *, #107691, .F. ) ;
#80001 = DIRECTION ( 'NONE',  ( 0.000000000000000000, 0.000000000000000000, 1.000000000000000000 ) ) ;
#80002 = LINE ( 'NONE', #239117, #7988 ) ;
#80003 = CIRCLE ( 'NONE', #225770, 11.75000000000001066 ) ;
#80004 = ORIENTED_EDGE ( 'NONE', *, *, #198860, .F. ) ;
#80005 = CARTESIAN_POINT ( 'NONE',  ( -21.05000000000000071, 11.65000000001115055, -140.7838656629781724 ) ) ;
#80006 = FACE_OUTER_BOUND ( 'NONE', #188117, .T. ) ;
#80007 = CARTESIAN_POINT ( 'NONE',  ( 17.74533788810829904, 53.39598356028773907, -230.1986723552803653 ) ) ;
#80008 = DIRECTION ( 'NONE',  ( 1.301042606982683418E-14, -0.8660254037844330455, 0.5000000000000096589 ) ) ;
#80010 = ORIENTED_EDGE ( 'NONE', *, *, #47240, .F. ) ;
#80009 = CARTESIAN_POINT ( 'NONE',  ( -21.14999999999994174, 74.16448838626247664, -47.62760213295649692 ) ) ;
#80012 = ORIENTED_EDGE ( 'NONE', *, *, #233630, .F. ) ;
#80011 = DIRECTION ( 'NONE',  ( 1.000000000000000000, -0.000000000000000000, -0.000000000000000000 ) ) ;
#80013 = FACE_OUTER_BOUND ( 'NONE', #37430, .T. ) ;
#80014 = CARTESIAN_POINT ( 'NONE',  ( 21.14999999999999858, -11.75000000000000000, -12.25000000000000000 ) ) ;
#80015 = DIRECTION ( 'NONE',  ( 0.000000000000000000, 0.000000000000000000, -1.000000000000000000 ) ) ;
#80016 = CARTESIAN_POINT ( 'NONE',  ( -13.88555196119803448, 9.457431528860066550, -182.4999169378996555 ) ) ;
#80017 = ADVANCED_FACE ( 'NONE', ( #178610 ), #157240, .T. ) ;
#80019 = DIRECTION ( 'NONE',  ( 0.000000000000000000, 0.000000000000000000, 1.000000000000000000 ) ) ;
#80018 = CARTESIAN_POINT ( 'NONE',  ( -16.94445028196807002, 63.05630424923659660, -213.0754291771441729 ) ) ;
#80020 = FACE_OUTER_BOUND ( 'NONE', #80915, .T. ) ;
#80021 = DIRECTION ( 'NONE',  ( 0.7071359030027419834, 0.000000000000000000, 0.7070776581709371511 ) ) ;
#80022 = CARTESIAN_POINT ( 'NONE',  ( 23.14999999999999858, 36.65892442174935439, -249.5511627012433848 ) ) ;
#80023 = CARTESIAN_POINT ( 'NONE',  ( -20.95000000000000284, 11.65000000001115232, -126.9851942293460922 ) ) ;
#80024 = EDGE_CURVE ( 'NONE', #108484, #238989, #65448, .T. ) ;
#80025 = CARTESIAN_POINT ( 'NONE',  ( 21.05000000000000071, 67.12338541492499644, -128.1380270056797031 ) ) ;
#80026 = VERTEX_POINT ( 'NONE', #61201 ) ;
#80027 = CARTESIAN_POINT ( 'NONE',  ( 18.49999999999999645, 76.00000000001165290, -69.52310748452431710 ) ) ;
#80028 = ORIENTED_EDGE ( 'NONE', *, *, #63485, .F. ) ;
#80029 = ORIENTED_EDGE ( 'NONE', *, *, #106886, .T. ) ;
#80030 = EDGE_CURVE ( 'NONE', #191527, #111919, #78094, .T. ) ;
#80031 = CARTESIAN_POINT ( 'NONE',  ( 20.97217846901851956, 67.12455827530222052, -94.52187980058714345 ) ) ;
#80032 = EDGE_CURVE ( 'NONE', #246278, #154279, #57236, .T. ) ;
#80033 = FACE_BOUND ( 'NONE', #82835, .T. ) ;
#80034 = EDGE_LOOP ( 'NONE', ( #15861, #257270, #242195 ) ) ;
#80035 = ORIENTED_EDGE ( 'NONE', *, *, #101479, .F. ) ;
#80036 = FILL_AREA_STYLE ('',( #523 ) ) ;
#80037 = CIRCLE ( 'NONE', #51006, 0.1999999999999999833 ) ;
#80038 = ORIENTED_EDGE ( 'NONE', *, *, #162024, .T. ) ;
#80039 = ORIENTED_EDGE ( 'NONE', *, *, #48872, .F. ) ;
#80040 = CIRCLE ( 'NONE', #234188, 0.1000000000000054040 ) ;
#80041 = EDGE_CURVE ( 'NONE', #116074, #175127, #20812, .T. ) ;
#80042 = DIRECTION ( 'NONE',  ( 0.000000000000000000, 0.000000000000000000, 1.000000000000000000 ) ) ;
#80043 = DIRECTION ( 'NONE',  ( 1.000000000000000000, 0.000000000000000000, 0.000000000000000000 ) ) ;
#80044 = DIRECTION ( 'NONE',  ( -1.836970198721029934E-16, -0.9651348961777157509, 0.2617529984165031243 ) ) ;
#80045 = DIRECTION ( 'NONE',  ( 0.7071359030027680737, 0.7070776581709111719, 0.000000000000000000 ) ) ;
#80046 = CARTESIAN_POINT ( 'NONE',  ( -21.45000000000000284, 7.708578643773852157, -155.2500000000000284 ) ) ;
#80047 = AXIS2_PLACEMENT_3D ( 'NONE', #122409, #7588, #3733 ) ;
#80048 = CARTESIAN_POINT ( 'NONE',  ( 23.15000000000000213, 88.41227409416214300, -173.0231074845242745 ) ) ;
#80050 = VERTEX_POINT ( 'NONE', #235972 ) ;
#80049 = DIRECTION ( 'NONE',  ( 0.000000000000000000, -1.000000000000000000, 0.000000000000000000 ) ) ;
#80052 = DIRECTION ( 'NONE',  ( -0.000000000000000000, 6.982962677686266711E-15, -1.000000000000000000 ) ) ;
#80051 = CARTESIAN_POINT ( 'NONE',  ( -16.87036670365548474, 63.08160062417908165, -212.9922606024214815 ) ) ;
#80053 = DIRECTION ( 'NONE',  ( 0.000000000000000000, 0.4999999999999689138, 0.8660254037844565822 ) ) ;
#80054 = VERTEX_POINT ( 'NONE', #217676 ) ;
#80055 = CARTESIAN_POINT ( 'NONE',  ( -16.94052228080552069, 63.06128592552281731, -213.0791574514314561 ) ) ;
#80056 = LINE ( 'NONE', #140048, #216642 ) ;
#80057 = VERTEX_POINT ( 'NONE', #121212 ) ;
#80058 = TOROIDAL_SURFACE ( 'NONE', #92565, 4.099999999999999645, 0.1000000000000000056 ) ;
#80061 = DIRECTION ( 'NONE',  ( 0.000000000000000000, 0.9908441862701791170, -0.1350103645450472789 ) ) ;
#80060 = AXIS2_PLACEMENT_3D ( 'NONE', #19342, #160163, #218807 ) ;
#80059 = CARTESIAN_POINT ( 'NONE',  ( -21.59142135623730852, 68.15000000001180069, -81.77310748452435973 ) ) ;
#80062 = FACE_OUTER_BOUND ( 'NONE', #149079, .T. ) ;
#80063 = EDGE_CURVE ( 'NONE', #217616, #192641, #211200, .T. ) ;
#80064 = VERTEX_POINT ( 'NONE', #200716 ) ;
#80065 = CARTESIAN_POINT ( 'NONE',  ( -18.59999999999999787, 11.75000000001115197, -40.51480577065400013 ) ) ;
#80066 = DIRECTION ( 'NONE',  ( 0.000000000000000000, 0.000000000000000000, -1.000000000000000000 ) ) ;
#80067 = DIRECTION ( 'NONE',  ( 1.000000000000000000, 0.000000000000000000, 1.073024830501117725E-15 ) ) ;
#80068 = DIRECTION ( 'NONE',  ( 0.000000000000000000, 0.000000000000000000, -1.000000000000000000 ) ) ;
#80069 = ORIENTED_EDGE ( 'NONE', *, *, #144711, .T. ) ;
#80070 = ADVANCED_FACE ( 'NONE', ( #119925 ), #7168, .T. ) ;
#80071 = CARTESIAN_POINT ( 'NONE',  ( -20.85000000000000142, 77.14957036958705316, -28.20719500002235236 ) ) ;
#80072 = AXIS2_PLACEMENT_3D ( 'NONE', #51985, #208533, #50692 ) ;
#80073 = VECTOR ( 'NONE', #240502, 999.9999999999998863 ) ;
#80074 = EDGE_CURVE ( 'NONE', #84708, #34506, #241143, .T. ) ;
#80075 = AXIS2_PLACEMENT_3D ( 'NONE', #213759, #234603, #19419 ) ;
#80076 = CARTESIAN_POINT ( 'NONE',  ( -23.15000000000000213, 1.115600667400684642E-11, -33.50000000000000000 ) ) ;
#80077 = LINE ( 'NONE', #194955, #20226 ) ;
#80078 = CARTESIAN_POINT ( 'NONE',  ( -18.59999999999999787, 77.83534155023598089, -57.96795619196132776 ) ) ;
#80079 = DIRECTION ( 'NONE',  ( 0.000000000000000000, -0.8814952561688428334, 0.4721928772777350680 ) ) ;
#80080 = CARTESIAN_POINT ( 'NONE',  ( -20.94999999999999929, 1.736257131608553550, -78.56865232901755292 ) ) ;
#80081 = ADVANCED_FACE ( 'NONE', ( #19521 ), #111245, .T. ) ;
#80083 = ORIENTED_EDGE ( 'NONE', *, *, #112848, .T. ) ;
#80082 = CARTESIAN_POINT ( 'NONE',  ( -21.07928932188134041, 6.328516656393293083, 0.09889514565439641580 ) ) ;
#80084 = DIRECTION ( 'NONE',  ( -0.000000000000000000, -0.9876197685951252359, -0.1568667991644863424 ) ) ;
#80085 = DIRECTION ( 'NONE',  ( 1.000000000000000000, -0.000000000000000000, -0.000000000000000000 ) ) ;
#80086 = CARTESIAN_POINT ( 'NONE',  ( 23.24999999999999289, 11.65000000001116298, -121.8500000000000369 ) ) ;
#80087 = FACE_OUTER_BOUND ( 'NONE', #48167, .T. ) ;
#80088 = CARTESIAN_POINT ( 'NONE',  ( 20.95512820512820085, 10.62384868372303615, -175.1649135690875880 ) ) ;
#80089 = EDGE_CURVE ( 'NONE', #87416, #245692, #152975, .T. ) ;
#80091 = VERTEX_POINT ( 'NONE', #161612 ) ;
#80090 = DIRECTION ( 'NONE',  ( -0.000000000000000000, 0.9770955615653313941, 0.2128009952263603954 ) ) ;
#80092 = PLANE ( 'NONE',  #96483 ) ;
#80093 = ADVANCED_FACE ( 'NONE', ( #220293 ), #99010, .F. ) ;
#80094 = FACE_OUTER_BOUND ( 'NONE', #36527, .T. ) ;
#80095 = DIRECTION ( 'NONE',  ( 0.000000000000000000, -6.789366196018718420E-15, 1.000000000000000000 ) ) ;
#80096 = VERTEX_POINT ( 'NONE', #42925 ) ;
#80097 = DIRECTION ( 'NONE',  ( 1.000000000000000000, 2.952720810173289112E-16, -0.000000000000000000 ) ) ;
#80098 = CARTESIAN_POINT ( 'NONE',  ( 21.05000000000000071, 75.94851711813097950, -176.3232873024375920 ) ) ;
#80099 = ADVANCED_FACE ( 'NONE', ( #201998 ), #237279, .F. ) ;
#80100 = AXIS2_PLACEMENT_3D ( 'NONE', #208315, #252540, #153510 ) ;
#80101 = FACE_OUTER_BOUND ( 'NONE', #243251, .T. ) ;
#80102 = CIRCLE ( 'NONE', #225857, 12.87499999999999822 ) ;
#80103 = DIRECTION ( 'NONE',  ( 0.000000000000000000, -0.6936040289657786628, -0.7203564749500342979 ) ) ;
#80104 = ORIENTED_EDGE ( 'NONE', *, *, #80202, .F. ) ;
#80105 = VERTEX_POINT ( 'NONE', #138147 ) ;
#80106 = CARTESIAN_POINT ( 'NONE',  ( 21.05000000000000071, 1.115653327213047955E-11, -104.8000000000000540 ) ) ;
#80107 = ADVANCED_FACE ( 'NONE', ( #102868 ), #39095, .T. ) ;
#80108 = AXIS2_PLACEMENT_3D ( 'NONE', #113987, #77417, #175293 ) ;
#80109 = DIRECTION ( 'NONE',  ( 0.000000000000000000, -0.3427706569149636118, 0.9394191166662961834 ) ) ;
#80110 = DIRECTION ( 'NONE',  ( 1.000000000000000000, 0.000000000000000000, 0.000000000000000000 ) ) ;
#80111 = ORIENTED_EDGE ( 'NONE', *, *, #13507, .F. ) ;
#80112 = CARTESIAN_POINT ( 'NONE',  ( 20.95556889135987788, 10.62194358774625513, -175.1423942218574723 ) ) ;
#80113 = VECTOR ( 'NONE', #216072, 1000.000000000000000 ) ;
#80114 = CARTESIAN_POINT ( 'NONE',  ( 20.74897398619114242, 11.98716974373489208, -206.2486471196630191 ) ) ;
#80115 = VECTOR ( 'NONE', #196668, 1000.000000000000000 ) ;
#80116 = DIRECTION ( 'NONE',  ( 1.000000000000000000, 0.000000000000000000, 0.000000000000000000 ) ) ;
#80117 = VECTOR ( 'NONE', #117506, 1000.000000000000000 ) ;
#80118 = CIRCLE ( 'NONE', #121872, 0.09999999999999939493 ) ;
#80119 = DIRECTION ( 'NONE',  ( -1.000000000000000000, -0.000000000000000000, -0.000000000000000000 ) ) ;
#80120 = CARTESIAN_POINT ( 'NONE',  ( 20.94999999999999574, 1.261786168576181755, -108.5864989635455089 ) ) ;
#80121 = AXIS2_PLACEMENT_3D ( 'NONE', #94878, #212288, #54470 ) ;
#80122 = ORIENTED_EDGE ( 'NONE', *, *, #18151, .T. ) ;
#80124 = ORIENTED_EDGE ( 'NONE', *, *, #83085, .T. ) ;
#80123 = CARTESIAN_POINT ( 'NONE',  ( 23.24999999999999645, 19.82851818057134707, -235.1178474969725016 ) ) ;
#80125 = CIRCLE ( 'NONE', #225881, 0.09999999999999939493 ) ;
#80126 = ORIENTED_EDGE ( 'NONE', *, *, #162341, .F. ) ;
#80127 = CARTESIAN_POINT ( 'NONE',  ( 18.49999999999999289, 11.65000000001115588, -134.0000000000000284 ) ) ;
#80128 = ORIENTED_EDGE ( 'NONE', *, *, #184766, .F. ) ;
#80129 = DIRECTION ( 'NONE',  ( -1.836970198721029934E-16, -0.9651348961777157509, 0.2617529984165031243 ) ) ;
#80130 = DIRECTION ( 'NONE',  ( 0.000000000000000000, 0.8814952561688430555, -0.4721928772777346239 ) ) ;
#80131 = CARTESIAN_POINT ( 'NONE',  ( 18.49999999999999645, -1.637172712970381694, -11.58215336547201701 ) ) ;
#80132 = ORIENTED_EDGE ( 'NONE', *, *, #98257, .T. ) ;
#80133 = DIRECTION ( 'NONE',  ( 1.000000000000000000, 0.000000000000000000, 0.000000000000000000 ) ) ;
#80134 = DIRECTION ( 'NONE',  ( -2.952720810173289112E-16, -1.000000000000000000, -6.982962677686266711E-15 ) ) ;
#80135 = AXIS2_PLACEMENT_3D ( 'NONE', #175657, #118239, #255124 ) ;
#80136 = ORIENTED_EDGE ( 'NONE', *, *, #214614, .T. ) ;
#80137 = CARTESIAN_POINT ( 'NONE',  ( -20.85000000000000142, 7.567413955921500346, -241.6205176796878504 ) ) ;
#80138 = AXIS2_PLACEMENT_3D ( 'NONE', #220589, #2799, #41966 ) ;
#80140 = EDGE_LOOP ( 'NONE', ( #136213, #56469, #66117, #5914 ) ) ;
#80139 = LINE ( 'NONE', #142708, #163253 ) ;
#80141 = DIRECTION ( 'NONE',  ( 0.000000000000000000, 0.5000000000000209832, 0.8660254037844264952 ) ) ;
#80142 = FACE_OUTER_BOUND ( 'NONE', #55414, .T. ) ;
#80143 = VECTOR ( 'NONE', #95925, 1000.000000000000000 ) ;
#80144 = CIRCLE ( 'NONE', #63422, 0.09999999999999935330 ) ;
#80145 = VECTOR ( 'NONE', #74698, 1000.000000000000000 ) ;
#80146 = ADVANCED_FACE ( 'NONE', ( #156488 ), #182447, .F. ) ;
#80147 = AXIS2_PLACEMENT_3D ( 'NONE', #102052, #6831, #150212 ) ;
#80148 = ORIENTED_EDGE ( 'NONE', *, *, #250642, .T. ) ;
#80149 = AXIS2_PLACEMENT_3D ( 'NONE', #247210, #9884, #51550 ) ;
#80150 = CARTESIAN_POINT ( 'NONE',  ( 5.899999999999996803, -11.75000000000000000, 14.10000000000000142 ) ) ;
#80151 = FACE_OUTER_BOUND ( 'NONE', #150141, .T. ) ;
#80152 = CARTESIAN_POINT ( 'NONE',  ( -23.15000000000000213, 76.00000000001195133, -103.0231074845243171 ) ) ;
#80153 = ORIENTED_EDGE ( 'NONE', *, *, #256880, .F. ) ;
#80154 = CARTESIAN_POINT ( 'NONE',  ( -21.55000000000000426, 10.20058289318835953, -211.4179224723290815 ) ) ;
#80155 = ADVANCED_FACE ( 'NONE', ( #126297 ), #40553, .T. ) ;
#80156 = CARTESIAN_POINT ( 'NONE',  ( -18.40000000000000213, 70.35000000001207354, -123.8731074845243398 ) ) ;
#80157 = CARTESIAN_POINT ( 'NONE',  ( -23.15000000000000213, 85.00000000001207923, -126.6291383618717816 ) ) ;
#80158 = EDGE_CURVE ( 'NONE', #147767, #81634, #49333, .T. ) ;
#80159 = EDGE_LOOP ( 'NONE', ( #207516, #183139, #222579 ) ) ;
#80160 = EDGE_CURVE ( 'NONE', #226915, #240562, #199495, .T. ) ;
#80161 = ORIENTED_EDGE ( 'NONE', *, *, #94963, .F. ) ;
#80162 = B_SPLINE_CURVE_WITH_KNOTS ( 'NONE', 3,
 ( #255164, #178286, #236945, #199104, #58287, #218650 ),
 .UNSPECIFIED., .F., .F.,
 ( 4, 2, 4 ),
 ( 0.000000000000000000, 0.0001496588209255877576, 0.0002993176418511755152 ),
 .UNSPECIFIED. ) ;
#80163 = CIRCLE ( 'NONE', #159338, 2.000000000000001776 ) ;
#80164 = AXIS2_PLACEMENT_3D ( 'NONE', #108108, #209775, #132815 ) ;
#80165 = CIRCLE ( 'NONE', #84245, 4.049999999999998046 ) ;
#80166 = ORIENTED_EDGE ( 'NONE', *, *, #213918, .F. ) ;
#80167 = ORIENTED_EDGE ( 'NONE', *, *, #63141, .F. ) ;
#80168 = CYLINDRICAL_SURFACE ( 'NONE', #56052, 12.87499999999999822 ) ;
#80169 = EDGE_CURVE ( 'NONE', #27906, #18097, #65048, .T. ) ;
#80170 = DIRECTION ( 'NONE',  ( 0.000000000000000000, 0.000000000000000000, 1.000000000000000000 ) ) ;
#80172 = EDGE_LOOP ( 'NONE', ( #183797, #98919, #218443, #172175 ) ) ;
#80171 = DIRECTION ( 'NONE',  ( -1.000000000000000000, -0.000000000000000000, -0.000000000000000000 ) ) ;
#80173 = CARTESIAN_POINT ( 'NONE',  ( 20.04142135623730070, 11.75000000000000355, -24.65000000000000213 ) ) ;
#80174 = CARTESIAN_POINT ( 'NONE',  ( -21.14999999999999858, -2.479040261793999722, -189.6172560698084624 ) ) ;
#80175 = EDGE_CURVE ( 'NONE', #230504, #200038, #217208, .T. ) ;
#80176 = DIRECTION ( 'NONE',  ( -0.000000000000000000, 1.000000000000000000, 1.734723475976807292E-15 ) ) ;
#80177 = CARTESIAN_POINT ( 'NONE',  ( 21.30000000000002558, 1.115600667400684642E-11, -104.5500000000000256 ) ) ;
#80178 = FACE_OUTER_BOUND ( 'NONE', #13074, .T. ) ;
#80179 = CARTESIAN_POINT ( 'NONE',  ( -21.64999999999999858, 65.95000000001152785, -48.77310748452439526 ) ) ;
#80181 = ORIENTED_EDGE ( 'NONE', *, *, #91180, .T. ) ;
#80180 = DIRECTION ( 'NONE',  ( -1.000000000000000000, -0.000000000000000000, -0.000000000000000000 ) ) ;
#80183 = ORIENTED_EDGE ( 'NONE', *, *, #143309, .F. ) ;
#80182 = DIRECTION ( 'NONE',  ( -1.000000000000000000, -0.000000000000000000, -0.000000000000000000 ) ) ;
#80184 = CARTESIAN_POINT ( 'NONE',  ( -16.89797118371629736, 60.89104750934725985, -221.1190723775698643 ) ) ;
#80185 = ORIENTED_EDGE ( 'NONE', *, *, #78124, .T. ) ;
#80186 = ORIENTED_EDGE ( 'NONE', *, *, #256442, .F. ) ;
#80187 = CARTESIAN_POINT ( 'NONE',  ( -21.05000000000000071, 2.953700692300310848, -208.6327728934509764 ) ) ;
#80188 = CIRCLE ( 'NONE', #134371, 0.1000000000000043771 ) ;
#80189 = CARTESIAN_POINT ( 'NONE',  ( 20.94999999999999929, 76.00000000001142553, -36.02310748452432421 ) ) ;
#80191 = EDGE_CURVE ( 'NONE', #198122, #223717, #252887, .T. ) ;
#80190 = LINE ( 'NONE', #76360, #130052 ) ;
#80192 = CIRCLE ( 'NONE', #225940, 0.1000000000000013933 ) ;
#80193 = FACE_OUTER_BOUND ( 'NONE', #165003, .T. ) ;
#80194 = EDGE_CURVE ( 'NONE', #1286, #148974, #28543, .T. ) ;
#80195 = EDGE_CURVE ( 'NONE', #197965, #44715, #173837, .T. ) ;
#80196 = CARTESIAN_POINT ( 'NONE',  ( -21.44999999999999929, 9.809744668562228043, -211.5030428704195913 ) ) ;
#80197 = CARTESIAN_POINT ( 'NONE',  ( 20.77526135991769607, 67.06799098339227783, -195.0545389417991657 ) ) ;
#80198 = LINE ( 'NONE', #243159, #256117 ) ;
#80199 = ORIENTED_EDGE ( 'NONE', *, *, #34357, .F. ) ;
#80200 = ORIENTED_EDGE ( 'NONE', *, *, #218609, .F. ) ;
#80201 = CARTESIAN_POINT ( 'NONE',  ( -18.50000000000000000, -1.293555411365099994, -227.7000673772910204 ) ) ;
#80202 = EDGE_CURVE ( 'NONE', #13871, #75744, #3798, .T. ) ;
#80203 = ORIENTED_EDGE ( 'NONE', *, *, #104002, .T. ) ;
#80204 = CYLINDRICAL_SURFACE ( 'NONE', #42901, 0.1000000000000008937 ) ;
#80205 = DIRECTION ( 'NONE',  ( 0.000000000000000000, 0.000000000000000000, -1.000000000000000000 ) ) ;
#80206 = CYLINDRICAL_SURFACE ( 'NONE', #68605, 0.09999999999999939493 ) ;
#80207 = CIRCLE ( 'NONE', #117837, 2.700000000000001066 ) ;
#80208 = DIRECTION ( 'NONE',  ( -1.000000000000000000, 2.952720810173289112E-16, 2.061873921506763405E-30 ) ) ;
#80209 = VERTEX_POINT ( 'NONE', #106725 ) ;
#80210 = DIRECTION ( 'NONE',  ( 0.000000000000000000, -0.2677755899090746849, 0.9634813093406884299 ) ) ;
#80211 = VERTEX_POINT ( 'NONE', #88434 ) ;
#80212 = CARTESIAN_POINT ( 'NONE',  ( -16.94107738177414291, 10.01423928514777373, -87.95000000000004547 ) ) ;
#80213 = ORIENTED_EDGE ( 'NONE', *, *, #224498, .F. ) ;
#80214 = EDGE_CURVE ( 'NONE', #226091, #62371, #186296, .T. ) ;
#80215 = DIRECTION ( 'NONE',  ( 0.000000000000000000, 2.891205793294679805E-16, -1.000000000000000000 ) ) ;
#80216 = EDGE_LOOP ( 'NONE', ( #49140, #201756, #194485, #234925 ) ) ;
#80218 = DIRECTION ( 'NONE',  ( 0.000000000000000000, -0.5000000000000144329, -0.8660254037844302699 ) ) ;
#80217 = VECTOR ( 'NONE', #187271, 1000.000000000000227 ) ;
#80220 = ORIENTED_EDGE ( 'NONE', *, *, #143369, .T. ) ;
#80219 = DIRECTION ( 'NONE',  ( -2.428612866367309808E-13, 0.4099100576505548821, 0.9121259477928028714 ) ) ;
#80221 = DIRECTION ( 'NONE',  ( -1.000000000000000000, 0.000000000000000000, -0.000000000000000000 ) ) ;
#80222 = ORIENTED_EDGE ( 'NONE', *, *, #149231, .F. ) ;
#80223 = VECTOR ( 'NONE', #169415, 999.9999999999998863 ) ;
#80224 = CIRCLE ( 'NONE', #80415, 0.5000000000000004441 ) ;
#80225 = ADVANCED_FACE ( 'NONE', ( #29816 ), #162897, .F. ) ;
#80226 = DIRECTION ( 'NONE',  ( 0.000000000000000000, 6.982962677686266711E-15, -1.000000000000000000 ) ) ;
#80227 = EDGE_LOOP ( 'NONE', ( #195749, #204512, #240465, #100653, #235555, #191277, #35762, #248961, #132494 ) ) ;
#80228 = FACE_OUTER_BOUND ( 'NONE', #56937, .T. ) ;
#80229 = DIRECTION ( 'NONE',  ( 0.7071359030027593029, 0.000000000000000000, 0.7070776581709197206 ) ) ;
#80230 = CARTESIAN_POINT ( 'NONE',  ( 20.94999999999999929, 5.850000000011160495, -190.8675027757220448 ) ) ;
#80231 = CARTESIAN_POINT ( 'NONE',  ( -16.86420534634261514, 9.970615445602874161, -121.4183365492374236 ) ) ;
#80232 = EDGE_CURVE ( 'NONE', #61015, #164661, #222826, .T. ) ;
#80233 = EDGE_CURVE ( 'NONE', #98769, #210485, #194664, .T. ) ;
#80234 = DIRECTION ( 'NONE',  ( 2.952720810173289112E-16, 1.000000000000000000, -6.088138035986627436E-46 ) ) ;
#80235 = CIRCLE ( 'NONE', #146889, 0.09999999999998898659 ) ;
#80236 = EDGE_LOOP ( 'NONE', ( #14, #16423, #212161, #175309 ) ) ;
#80237 = VECTOR ( 'NONE', #75177, 1000.000000000000000 ) ;
#80238 = CARTESIAN_POINT ( 'NONE',  ( -23.15000000000000213, 64.40000000001177227, -76.45131071479988805 ) ) ;
#80239 = CARTESIAN_POINT ( 'NONE',  ( -28.12018973533754362, 11.62642356364895413, 33.00000000000000000 ) ) ;
#80240 = CARTESIAN_POINT ( 'NONE',  ( 21.40925344232283223, 1.306104126701115531, -230.5013720119504228 ) ) ;
#80241 = ORIENTED_EDGE ( 'NONE', *, *, #116402, .T. ) ;
#80242 = DIRECTION ( 'NONE',  ( 0.000000000000000000, -0.1495327102803078179, 0.9887567792719429427 ) ) ;
#80243 = VERTEX_POINT ( 'NONE', #153627 ) ;
#80244 = DIRECTION ( 'NONE',  ( 1.000000000000000000, 0.000000000000000000, 0.000000000000000000 ) ) ;
#80245 = ORIENTED_EDGE ( 'NONE', *, *, #42319, .F. ) ;
#80246 = EDGE_CURVE ( 'NONE', #66550, #153829, #3072, .T. ) ;
#80247 = EDGE_CURVE ( 'NONE', #30387, #216303, #215468, .T. ) ;
#80248 = DIRECTION ( 'NONE',  ( 0.000000000000000000, 0.01562499999998609446, -0.9998779222360101304 ) ) ;
#80249 = CARTESIAN_POINT ( 'NONE',  ( -17.78241384942841208, 65.14442424721221414, -180.2721451569497049 ) ) ;
#80251 = ORIENTED_EDGE ( 'NONE', *, *, #251354, .F. ) ;
#80250 = TOROIDAL_SURFACE ( 'NONE', #9368, 0.6000000000000009770, 0.1000000000000000056 ) ;
#80253 = EDGE_LOOP ( 'NONE', ( #70125, #6793, #87415, #44342, #82050, #199923, #151507, #94155, #188469, #40202, #156050, #103578, #110837, #81543 ) ) ;
#80252 = CARTESIAN_POINT ( 'NONE',  ( 18.39999999999999858, 85.50000000001136868, -29.42291809330221497 ) ) ;
#80254 = CARTESIAN_POINT ( 'NONE',  ( 20.99999999999999645, 9.750000000011137757, -109.7500000000000426 ) ) ;
#80255 = VERTEX_POINT ( 'NONE', #70216 ) ;
#80256 = DIRECTION ( 'NONE',  ( 0.000000000000000000, -0.2128009952263485993, 0.9770955615653341697 ) ) ;
#80257 = AXIS2_PLACEMENT_3D ( 'NONE', #201351, #181796, #566 ) ;
#80258 = CIRCLE ( 'NONE', #180091, 11.74999999999999645 ) ;
#80259 = AXIS2_PLACEMENT_3D ( 'NONE', #151390, #206212, #49703 ) ;
#80260 = LINE ( 'NONE', #175568, #106060 ) ;
#80261 = ORIENTED_EDGE ( 'NONE', *, *, #219592, .F. ) ;
#80262 = AXIS2_PLACEMENT_3D ( 'NONE', #210656, #167708, #90697 ) ;
#80263 = ORIENTED_EDGE ( 'NONE', *, *, #43894, .F. ) ;
#80264 = EDGE_CURVE ( 'NONE', #205348, #107956, #90561, .T. ) ;
#80265 = FACE_BOUND ( 'NONE', #76118, .T. ) ;
#80266 = DIRECTION ( 'NONE',  ( -1.000000000000000000, 0.000000000000000000, -0.000000000000000000 ) ) ;
#80267 = EDGE_LOOP ( 'NONE', ( #124524, #196639, #150185, #220793 ) ) ;
#80268 = CARTESIAN_POINT ( 'NONE',  ( 20.99999999999999645, 66.25000000001202238, -115.6731074845243796 ) ) ;
#80269 = EDGE_CURVE ( 'NONE', #207515, #36105, #215644, .T. ) ;
#80270 = ORIENTED_EDGE ( 'NONE', *, *, #78938, .T. ) ;
#80271 = EDGE_LOOP ( 'NONE', ( #191659, #205241, #112938, #109140 ) ) ;
#80272 = LINE ( 'NONE', #41214, #34993 ) ;
#80273 = ADVANCED_FACE ( 'NONE', ( #188848 ), #72789, .T. ) ;
#80275 = ORIENTED_EDGE ( 'NONE', *, *, #240199, .F. ) ;
#80274 = DIRECTION ( 'NONE',  ( 0.000000000000000000, 0.000000000000000000, 1.000000000000000000 ) ) ;
#80276 = EDGE_CURVE ( 'NONE', #193505, #208696, #210986, .T. ) ;
#80277 = DIRECTION ( 'NONE',  ( 0.000000000000000000, -1.000000000000000000, -2.891205793294679805E-16 ) ) ;
#80278 = CARTESIAN_POINT ( 'NONE',  ( -20.94999999999999929, 64.35000000001171827, -69.52310748452438816 ) ) ;
#80279 = EDGE_CURVE ( 'NONE', #222808, #255460, #153163, .T. ) ;
#80280 = CARTESIAN_POINT ( 'NONE',  ( -16.78493211734301482, 63.08610022504905146, -213.1421742787360074 ) ) ;
#80282 = DIRECTION ( 'NONE',  ( 0.000000000000000000, 1.000000000000000000, 0.000000000000000000 ) ) ;
#80281 = CYLINDRICAL_SURFACE ( 'NONE', #156766, 0.09999999999999939493 ) ;
#80283 = CARTESIAN_POINT ( 'NONE',  ( -21.05000000000000071, 75.98514436511875658, -142.8674665265674264 ) ) ;
#80285 = ADVANCED_FACE ( 'NONE', ( #212282 ), #36634, .F. ) ;
#80284 = CARTESIAN_POINT ( 'NONE',  ( -23.25000000000000000, 4.150000000000001243, -21.14999999999999858 ) ) ;
#80286 = CARTESIAN_POINT ( 'NONE',  ( -22.59999999999999787, 11.74956712348939192, 0.1008583690987087389 ) ) ;
#80287 = DIRECTION ( 'NONE',  ( -1.000000000000000000, -0.000000000000000000, -0.000000000000000000 ) ) ;
#80288 = ORIENTED_EDGE ( 'NONE', *, *, #221486, .F. ) ;
#80289 = ORIENTED_EDGE ( 'NONE', *, *, #182148, .T. ) ;
#80290 = VECTOR ( 'NONE', #189972, 1000.000000000000114 ) ;
#80291 = ORIENTED_EDGE ( 'NONE', *, *, #47896, .T. ) ;
#80292 = DIRECTION ( 'NONE',  ( 0.000000000000000000, 0.000000000000000000, -1.000000000000000000 ) ) ;
#80293 = ORIENTED_EDGE ( 'NONE', *, *, #159504, .F. ) ;
#80294 = CARTESIAN_POINT ( 'NONE',  ( -20.94999999999999929, 64.40000000001195701, -109.9513107147998880 ) ) ;
#80295 = ADVANCED_FACE ( 'NONE', ( #248836 ), #11513, .F. ) ;
#80296 = EDGE_CURVE ( 'NONE', #190676, #176903, #34947, .T. ) ;
#80297 = CARTESIAN_POINT ( 'NONE',  ( -20.64999999999999858, 4.350000000011156054, -45.85000000000000142 ) ) ;
#80298 = CIRCLE ( 'NONE', #1213, 0.1000000000000026007 ) ;
#80299 = ORIENTED_EDGE ( 'NONE', *, *, #64019, .F. ) ;
#80300 = CIRCLE ( 'NONE', #151288, 0.1000000000000028644 ) ;
#80301 =( LENGTH_UNIT ( ) NAMED_UNIT ( * ) SI_UNIT ( .MILLI., .METRE. ) );
#80302 = CARTESIAN_POINT ( 'NONE',  ( -23.15000000000000213, 0.000000000000000000, -12.87499999999999822 ) ) ;
#80303 = AXIS2_PLACEMENT_3D ( 'NONE', #132626, #12701, #33568 ) ;
#80305 = ORIENTED_EDGE ( 'NONE', *, *, #31723, .F. ) ;
#80304 = ORIENTED_EDGE ( 'NONE', *, *, #58392, .F. ) ;
#80306 = ORIENTED_EDGE ( 'NONE', *, *, #191204, .F. ) ;
#80307 = ORIENTED_EDGE ( 'NONE', *, *, #39485, .T. ) ;
#80308 = TOROIDAL_SURFACE ( 'NONE', #217701, 0.6000000000000015321, 0.1000000000000000056 ) ;
#80309 = DIRECTION ( 'NONE',  ( 0.000000000000000000, 0.000000000000000000, -1.000000000000000000 ) ) ;
#80310 = DIRECTION ( 'NONE',  ( 0.000000000000000000, 0.000000000000000000, 1.000000000000000000 ) ) ;
#80312 = EDGE_LOOP ( 'NONE', ( #83792, #113413, #208108 ) ) ;
#80311 = FACE_OUTER_BOUND ( 'NONE', #248850, .T. ) ;
#80313 = DIRECTION ( 'NONE',  ( 0.000000000000000000, 0.2128009952263605620, -0.9770955615653315052 ) ) ;
#80314 = DIRECTION ( 'NONE',  ( 0.000000000000000000, -0.9908441862701420355, -0.1350103645453197554 ) ) ;
#80316 = ORIENTED_EDGE ( 'NONE', *, *, #200050, .T. ) ;
#80315 = DIRECTION ( 'NONE',  ( 0.7071067811865475727, -0.2890913453342130457, 0.6453109281988448354 ) ) ;
#80317 = CARTESIAN_POINT ( 'NONE',  ( -20.94999999999999929, 36.65892442174935439, -249.5511627012433848 ) ) ;
#80318 = ORIENTED_EDGE ( 'NONE', *, *, #179148, .T. ) ;
#80319 = CARTESIAN_POINT ( 'NONE',  ( 20.09999999999999787, 66.25000000001162448, -60.27310748452439526 ) ) ;
#80321 = VERTEX_POINT ( 'NONE', #152321 ) ;
#80320 = CARTESIAN_POINT ( 'NONE',  ( -18.40000000000000213, 5.649999999999983480, -12.65000000000000213 ) ) ;
#80322 = AXIS2_PLACEMENT_3D ( 'NONE', #14405, #93906, #233449 ) ;
#80323 = DIRECTION ( 'NONE',  ( 0.000000000000000000, -1.000000000000000000, 0.000000000000000000 ) ) ;
#80324 = CARTESIAN_POINT ( 'NONE',  ( 23.14999999999999858, 68.04894835573102796, -237.6803414396912046 ) ) ;
#80325 = CARTESIAN_POINT ( 'NONE',  ( -19.99999999999999645, 1.350000000000000089, 16.50000000000000000 ) ) ;
#80326 = ORIENTED_EDGE ( 'NONE', *, *, #17210, .F. ) ;
#80327 = AXIS2_PLACEMENT_3D ( 'NONE', #67439, #227794, #127423 ) ;
#80328 = ADVANCED_FACE ( 'NONE', ( #53187 ), #135273, .F. ) ;
#80330 = DIRECTION ( 'NONE',  ( 0.000000000000000000, 0.9371753822965326330, -0.3488585713686107592 ) ) ;
#80329 = CARTESIAN_POINT ( 'NONE',  ( -20.54999999999999716, 2.000000000011154189, -54.17537807723790166 ) ) ;
#80331 = CARTESIAN_POINT ( 'NONE',  ( -20.64999999999999858, 71.65000000001199965, -115.3731074845243256 ) ) ;
#80332 = CARTESIAN_POINT ( 'NONE',  ( 18.46163235739469499, 85.48015080693069478, -163.3654969446463383 ) ) ;
#80333 = EDGE_CURVE ( 'NONE', #26230, #201551, #149749, .T. ) ;
#80334 = CYLINDRICAL_SURFACE ( 'NONE', #101640, 0.09999999999999939493 ) ;
#80335 = DIRECTION ( 'NONE',  ( -0.000000000000000000, -6.982962677686266711E-15, 1.000000000000000000 ) ) ;
#80336 = EDGE_LOOP ( 'NONE', ( #99959, #141703, #137054 ) ) ;
#80337 = ORIENTED_EDGE ( 'NONE', *, *, #204325, .T. ) ;
#80338 = CIRCLE ( 'NONE', #100982, 0.1000000000000033223 ) ;
#80340 = ORIENTED_EDGE ( 'NONE', *, *, #207151, .T. ) ;
#80339 = AXIS2_PLACEMENT_3D ( 'NONE', #202133, #78314, #101709 ) ;
#80341 = DIRECTION ( 'NONE',  ( 0.000000000000000000, 0.000000000000000000, -1.000000000000000000 ) ) ;
#80342 = CIRCLE ( 'NONE', #155428, 0.1000000000000028644 ) ;
#80343 = VERTEX_POINT ( 'NONE', #250110 ) ;
#80344 = CARTESIAN_POINT ( 'NONE',  ( -20.54999999999999716, 0.000000000000000000, -12.97499999999999609 ) ) ;
#80345 = EDGE_LOOP ( 'NONE', ( #243598, #127474, #240249, #104796, #220950, #132621, #234668, #229325 ) ) ;
#80346 = DIRECTION ( 'NONE',  ( 2.694716079187273439E-16, -0.9770955615653316162, -0.2128009952263598958 ) ) ;
#80347 = CARTESIAN_POINT ( 'NONE',  ( 23.14999999999999858, 7.128833340094563376, -233.7327013124401276 ) ) ;
#80348 = ORIENTED_EDGE ( 'NONE', *, *, #163597, .T. ) ;
#80349 = DIRECTION ( 'NONE',  ( 0.000000000000000000, 0.9553114395362733990, 0.2956011730205631016 ) ) ;
#80350 =( NAMED_UNIT ( * ) PLANE_ANGLE_UNIT ( ) SI_UNIT ( $, .RADIAN. ) );
#80351 = EDGE_CURVE ( 'NONE', #37851, #118363, #71497, .T. ) ;
#80352 = AXIS2_PLACEMENT_3D ( 'NONE', #139563, #19649, #18354 ) ;
#80353 = AXIS2_PLACEMENT_3D ( 'NONE', #59642, #194079, #257821 ) ;
#80354 = ORIENTED_EDGE ( 'NONE', *, *, #14243, .T. ) ;
#80355 = AXIS2_PLACEMENT_3D ( 'NONE', #150813, #230343, #247338 ) ;
#80357 = EDGE_LOOP ( 'NONE', ( #22355, #251021, #257630, #205769 ) ) ;
#80356 = VECTOR ( 'NONE', #228155, 1000.000000000000000 ) ;
#80358 = ORIENTED_EDGE ( 'NONE', *, *, #195758, .T. ) ;
#80359 = DIRECTION ( 'NONE',  ( 0.000000000000000000, -1.000000000000000000, 0.000000000000000000 ) ) ;
#80360 = CARTESIAN_POINT ( 'NONE',  ( 22.40736611211992368, 76.00000000001276135, -215.1726782920691505 ) ) ;
#80361 = CARTESIAN_POINT ( 'NONE',  ( 20.85000000000000142, 69.06610602788553877, -99.23746165015076315 ) ) ;
#80362 = DIRECTION ( 'NONE',  ( -0.000000000000000000, 1.000000000000000000, 6.982962677686266711E-15 ) ) ;
#80363 = DIRECTION ( 'NONE',  ( 0.000000000000000000, 1.000000000000000000, 6.982962677686266711E-15 ) ) ;
#80364 = LINE ( 'NONE', #159959, #134418 ) ;
#80365 = LINE ( 'NONE', #19138, #145364 ) ;
#80366 = DIRECTION ( 'NONE',  ( -1.000000000000000000, -0.000000000000000000, -0.000000000000000000 ) ) ;
#80368 = ORIENTED_EDGE ( 'NONE', *, *, #60162, .F. ) ;
#80367 = CARTESIAN_POINT ( 'NONE',  ( 21.07928932188134397, 69.67148334361864670, -103.1220026301787414 ) ) ;
#80369 = CARTESIAN_POINT ( 'NONE',  ( 21.30000000000002558, 67.23127455305841238, -235.8551265064783991 ) ) ;
#80370 = EDGE_LOOP ( 'NONE', ( #59795, #53583, #53706, #144296 ) ) ;
#80371 = CARTESIAN_POINT ( 'NONE',  ( 18.49999999999999645, -1.637172712959225507, -78.58215336547205254 ) ) ;
#80372 = VERTEX_POINT ( 'NONE', #114449 ) ;
#80373 = ORIENTED_EDGE ( 'NONE', *, *, #239385, .T. ) ;
#80374 = LINE ( 'NONE', #159970, #104622 ) ;
#80375 = DIRECTION ( 'NONE',  ( -1.000000000000000000, 3.265361837132813093E-16, 2.280189983783949500E-30 ) ) ;
#80376 = DIRECTION ( 'NONE',  ( 1.000000000000000000, 0.000000000000000000, 0.000000000000000000 ) ) ;
#80377 = ORIENTED_EDGE ( 'NONE', *, *, #32149, .F. ) ;
#80378 = CARTESIAN_POINT ( 'NONE',  ( 18.59999999999999787, 77.83585931145526615, -58.01866831572577610 ) ) ;
#80379 = ORIENTED_EDGE ( 'NONE', *, *, #32949, .T. ) ;
#80380 = ORIENTED_EDGE ( 'NONE', *, *, #94470, .F. ) ;
#80381 = CARTESIAN_POINT ( 'NONE',  ( -23.15000000000000213, 64.35000000001150511, -48.17310748452440095 ) ) ;
#80382 = EDGE_LOOP ( 'NONE', ( #61722, #20067, #73820, #28659 ) ) ;
#80383 = CARTESIAN_POINT ( 'NONE',  ( -1.820710678118658388, -9.929289321870186313, -192.1499999999999488 ) ) ;
#80384 = ORIENTED_EDGE ( 'NONE', *, *, #210416, .F. ) ;
#80385 = LINE ( 'NONE', #175694, #223830 ) ;
#80386 = FACE_OUTER_BOUND ( 'NONE', #53924, .T. ) ;
#80387 = CARTESIAN_POINT ( 'NONE',  ( -21.07928932188134041, 75.90110485435833709, -209.8516241409176644 ) ) ;
#80388 = ORIENTED_EDGE ( 'NONE', *, *, #118809, .T. ) ;
#80389 = CARTESIAN_POINT ( 'NONE',  ( -23.25000000000000000, 71.75000000001199396, -115.3731074845243256 ) ) ;
#80390 = DIRECTION ( 'NONE',  ( 0.000000000000000000, -1.000000000000000000, 0.000000000000000000 ) ) ;
#80391 = ADVANCED_FACE ( 'NONE', ( #229273 ), #130149, .T. ) ;
#80392 = CARTESIAN_POINT ( 'NONE',  ( -21.14999999999994174, 87.50449464844290048, -34.18759587077607165 ) ) ;
#80394 = ORIENTED_EDGE ( 'NONE', *, *, #103688, .T. ) ;
#80393 = AXIS2_PLACEMENT_3D ( 'NONE', #196908, #193080, #217741 ) ;
#80395 = EDGE_CURVE ( 'NONE', #106574, #148927, #15367, .T. ) ;
#80397 = ORIENTED_EDGE ( 'NONE', *, *, #242384, .T. ) ;
#80396 = CARTESIAN_POINT ( 'NONE',  ( 23.15000000000000213, 84.59626168225496201, -112.4732350016745244 ) ) ;
#80398 = CARTESIAN_POINT ( 'NONE',  ( -22.49806830649814415, 12.56154382881637943, -223.4268007483960616 ) ) ;
#80399 = EDGE_CURVE ( 'NONE', #126928, #165593, #21779, .T. ) ;
#80400 = SPHERICAL_SURFACE ( 'NONE', #175459, 0.1000000000000000056 ) ;
#80401 = DIRECTION ( 'NONE',  ( 0.000000000000000000, 0.000000000000000000, -1.000000000000000000 ) ) ;
#80402 = CARTESIAN_POINT ( 'NONE',  ( -16.87487986503753845, 66.04999244492645971, -123.8731327448376334 ) ) ;
#80403 = VERTEX_POINT ( 'NONE', #97411 ) ;
#80404 = DIRECTION ( 'NONE',  ( 0.000000000000000000, 0.000000000000000000, 1.000000000000000000 ) ) ;
#80405 = CARTESIAN_POINT ( 'NONE',  ( -20.54999999999999716, 21.39147882631411335, -233.2615922652120730 ) ) ;
#80406 = CARTESIAN_POINT ( 'NONE',  ( -21.05000000000000071, 0.000000000000000000, -33.50000000000000000 ) ) ;
#80407 = FACE_OUTER_BOUND ( 'NONE', #231228, .T. ) ;
#80408 = TOROIDAL_SURFACE ( 'NONE', #134588, 11.65000000000000036, 0.1000000000000000056 ) ;
#80409 = EDGE_CURVE ( 'NONE', #76432, #187747, #69937, .T. ) ;
#80411 = DIRECTION ( 'NONE',  ( -1.000000000000000000, 0.000000000000000000, 0.000000000000000000 ) ) ;
#80410 = CIRCLE ( 'NONE', #109663, 11.75000000000001066 ) ;
#80412 = ORIENTED_EDGE ( 'NONE', *, *, #113172, .T. ) ;
#80413 = VERTEX_POINT ( 'NONE', #76596 ) ;
#80414 = DIRECTION ( 'NONE',  ( 0.000000000000000000, 0.000000000000000000, 1.000000000000000000 ) ) ;
#80416 = CARTESIAN_POINT ( 'NONE',  ( -18.59999999999999787, 68.92903212821303782, -99.27654326265604823 ) ) ;
#80415 = AXIS2_PLACEMENT_3D ( 'NONE', #79745, #120224, #180176 ) ;
#80417 = CARTESIAN_POINT ( 'NONE',  ( -22.50000000000000000, -3.092988775432913506, -228.1437074281570858 ) ) ;
#80418 = CARTESIAN_POINT ( 'NONE',  ( 21.14999999999999858, 64.25000000001237765, -169.9231074845244507 ) ) ;
#80419 = EDGE_CURVE ( 'NONE', #241603, #8263, #132267, .T. ) ;
#80420 = ORIENTED_EDGE ( 'NONE', *, *, #142693, .T. ) ;
#80421 = CARTESIAN_POINT ( 'NONE',  ( -18.41353343127311248, 46.96039402156218756, -255.3459641718773696 ) ) ;
#80422 = CARTESIAN_POINT ( 'NONE',  ( -18.50000000000000000, 1.115600667400684642E-11, -100.5000000000000284 ) ) ;
#80423 = CIRCLE ( 'NONE', #192902, 0.09999999999998898659 ) ;
#80424 = CIRCLE ( 'NONE', #138866, 0.1999999999999987899 ) ;
#80425 = CARTESIAN_POINT ( 'NONE',  ( -23.15000000000000213, 11.65000000001115588, -121.8500000000000369 ) ) ;
#80426 = CIRCLE ( 'NONE', #130919, 0.5000000000000004441 ) ;
#80427 = DIRECTION ( 'NONE',  ( 0.000000000000000000, 1.000000000000000000, 1.734723475976807292E-15 ) ) ;
#80428 = ORIENTED_EDGE ( 'NONE', *, *, #163894, .F. ) ;
#80429 = CARTESIAN_POINT ( 'NONE',  ( 20.94999999999999929, 76.00000000001190870, -103.0231074845243029 ) ) ;
#80430 = AXIS2_PLACEMENT_3D ( 'NONE', #113088, #252582, #15289 ) ;
#80431 = ORIENTED_EDGE ( 'NONE', *, *, #62141, .T. ) ;
#80432 = CARTESIAN_POINT ( 'NONE',  ( -21.05000000000000071, 64.35000000001249987, -177.0379132551784096 ) ) ;
#80433 = LINE ( 'NONE', #180871, #150658 ) ;
#80434 = LINE ( 'NONE', #177041, #182407 ) ;
#80435 = CARTESIAN_POINT ( 'NONE',  ( 18.57399277249656322, 65.66887361445313331, -63.93298459182691573 ) ) ;
#80437 = AXIS2_PLACEMENT_3D ( 'NONE', #145219, #244322, #128248 ) ;
#80436 = CARTESIAN_POINT ( 'NONE',  ( -18.50000000000000000, 11.74999999999999645, -21.35000000000000142 ) ) ;
#80438 = DIRECTION ( 'NONE',  ( 1.000000000000000000, -0.000000000000000000, 0.000000000000000000 ) ) ;
#80440 = DIRECTION ( 'NONE',  ( -1.000000000000000000, 1.207181226542539700E-16, -2.694675058168174199E-16 ) ) ;
#80439 = CIRCLE ( 'NONE', #188623, 0.09999999999998898659 ) ;
#80441 = CIRCLE ( 'NONE', #105398, 0.1000000000000028644 ) ;
#80442 = CARTESIAN_POINT ( 'NONE',  ( 21.05000000000005400, 67.85000000001119247, -3.123107484524795474 ) ) ;
#80444 = LINE ( 'NONE', #6068, #112267 ) ;
#80443 = AXIS2_PLACEMENT_3D ( 'NONE', #97083, #217049, #117973 ) ;
#80445 = CARTESIAN_POINT ( 'NONE',  ( 18.59999999999999076, 69.45000000001158469, -59.50608031408435039 ) ) ;
#80446 = LINE ( 'NONE', #40114, #64742 ) ;
#80447 = CARTESIAN_POINT ( 'NONE',  ( -22.39999999999999858, -2.598867842139048090, -189.5410128746472083 ) ) ;
#80448 = CARTESIAN_POINT ( 'NONE',  ( -21.05000000000000426, 69.66772772607600928, -69.48557142123871699 ) ) ;
#80449 = DIRECTION ( 'NONE',  ( 0.000000000000000000, -0.8368562265788574983, -0.5474227397872651890 ) ) ;
#80450 = EDGE_CURVE ( 'NONE', #189027, #37051, #203184, .T. ) ;
#80451 = ORIENTED_EDGE ( 'NONE', *, *, #28390, .T. ) ;
#80452 = CARTESIAN_POINT ( 'NONE',  ( 21.09096482362060243, 6.363544365404417036, 0.03944827877412642597 ) ) ;
#80453 = CARTESIAN_POINT ( 'NONE',  ( 20.85000000000000142, 11.75000000000000355, -26.71613433702190932 ) ) ;
#80454 = DIRECTION ( 'NONE',  ( -1.000000000000000000, -2.952720810173289112E-16, 0.000000000000000000 ) ) ;
#80455 = ADVANCED_FACE ( 'NONE', ( #199118 ), #242864, .T. ) ;
#80456 = ORIENTED_EDGE ( 'NONE', *, *, #257622, .T. ) ;
#80457 = CARTESIAN_POINT ( 'NONE',  ( -22.49072729836729678, 0.05648193274477467801, -55.34999175084509915 ) ) ;
#80458 = CARTESIAN_POINT ( 'NONE',  ( -23.15000000000000213, 64.25000000001260503, -191.2731074845244450 ) ) ;
#80459 = EDGE_CURVE ( 'NONE', #217297, #128950, #128184, .T. ) ;
#80460 = ORIENTED_EDGE ( 'NONE', *, *, #256161, .F. ) ;
#80462 = ADVANCED_FACE ( 'NONE', ( #16647 ), #96145, .T. ) ;
#80461 = CARTESIAN_POINT ( 'NONE',  ( -16.86578989773640913, 9.984809801269951990, -188.4646648866221881 ) ) ;
#80463 = CARTESIAN_POINT ( 'NONE',  ( 22.50000000000000000, 11.64957080754479968, 0.09999999999999592548 ) ) ;
#80464 = AXIS2_PLACEMENT_3D ( 'NONE', #52455, #210280, #212846 ) ;
#80465 = B_SPLINE_CURVE_WITH_KNOTS ( 'NONE', 3,
 ( #163842, #162572, #202954, #221222, #178293, #42604 ),
 .UNSPECIFIED., .F., .F.,
 ( 4, 2, 4 ),
 ( 0.000000000000000000, 0.0001496588209255873239, 0.0002993176418511746479 ),
 .UNSPECIFIED. ) ;
#80466 = ORIENTED_EDGE ( 'NONE', *, *, #145484, .T. ) ;
#80467 = ORIENTED_EDGE ( 'NONE', *, *, #162827, .F. ) ;
#80469 = DIRECTION ( 'NONE',  ( 1.000000000000000000, 0.000000000000000000, 0.000000000000000000 ) ) ;
#80468 = AXIS2_PLACEMENT_3D ( 'NONE', #239067, #96942, #216915 ) ;
#80470 = AXIS2_PLACEMENT_3D ( 'NONE', #212518, #233374, #191689 ) ;
#80471 = ADVANCED_FACE ( 'NONE', ( #17900 ), #38768, .T. ) ;
#80472 = ORIENTED_EDGE ( 'NONE', *, *, #115174, .T. ) ;
#80473 = EDGE_CURVE ( 'NONE', #180491, #238726, #19861, .T. ) ;
#80474 = CARTESIAN_POINT ( 'NONE',  ( 21.09107601085572981, 0.03930716471739142265, 6.363877975359904404 ) ) ;
#80475 = CARTESIAN_POINT ( 'NONE',  ( -21.05000000000000071, -11.64999999998884483, -170.4999999999999716 ) ) ;
#80477 = VECTOR ( 'NONE', #105431, 1000.000000000000000 ) ;
#80476 = DIRECTION ( 'NONE',  ( -0.000000000000000000, -0.000000000000000000, -1.000000000000000000 ) ) ;
#80478 = EDGE_CURVE ( 'NONE', #228703, #8664, #105109, .T. ) ;
#80479 = DIRECTION ( 'NONE',  ( -1.000000000000000000, -0.000000000000000000, -0.000000000000000000 ) ) ;
#80480 = CARTESIAN_POINT ( 'NONE',  ( -20.54999999999999716, 9.350000000011156942, -179.7499999999999716 ) ) ;
#80481 = DIRECTION ( 'NONE',  ( 0.000000000000000000, 0.000000000000000000, -1.000000000000000000 ) ) ;
#80482 = VECTOR ( 'NONE', #182940, 1000.000000000000000 ) ;
#80483 = FACE_OUTER_BOUND ( 'NONE', #179750, .T. ) ;
#80485 = DIRECTION ( 'NONE',  ( 8.673617379884087537E-15, 1.000000000000000000, 0.000000000000000000 ) ) ;
#80484 = AXIS2_PLACEMENT_3D ( 'NONE', #172738, #176558, #155727 ) ;
#80486 = AXIS2_PLACEMENT_3D ( 'NONE', #72967, #12987, #152501 ) ;
#80488 = ORIENTED_EDGE ( 'NONE', *, *, #16126, .F. ) ;
#80487 = CARTESIAN_POINT ( 'NONE',  ( 18.31572054635522306, 87.00872412986319659, -199.4107252354332616 ) ) ;
#80489 = ORIENTED_EDGE ( 'NONE', *, *, #212807, .T. ) ;
#80491 = CARTESIAN_POINT ( 'NONE',  ( -23.15000000000000213, 11.65000000000000036, -21.35000000000000142 ) ) ;
#80490 = DIRECTION ( 'NONE',  ( 1.000000000000000000, 0.000000000000000000, 0.000000000000000000 ) ) ;
#80492 = AXIS2_PLACEMENT_3D ( 'NONE', #134828, #196124, #17473 ) ;
#80494 = ORIENTED_EDGE ( 'NONE', *, *, #152050, .T. ) ;
#80493 = CARTESIAN_POINT ( 'NONE',  ( -16.80891096016323871, 60.93473447329584758, -221.0587747272457193 ) ) ;
#80495 = EDGE_LOOP ( 'NONE', ( #50956, #134979, #108834, #222915, #79220 ) ) ;
#80496 = DIRECTION ( 'NONE',  ( 0.000000000000000000, -0.5000000000000016653, 0.8660254037844377084 ) ) ;
#80497 = DIRECTION ( 'NONE',  ( 0.000000000000000000, 0.000000000000000000, 1.000000000000000000 ) ) ;
#80498 = VECTOR ( 'NONE', #242865, 1000.000000000000000 ) ;
#80500 = EDGE_CURVE ( 'NONE', #190492, #244261, #82903, .T. ) ;
#80499 = DIRECTION ( 'NONE',  ( 0.000000000000000000, 0.000000000000000000, -1.000000000000000000 ) ) ;
#80501 = DIRECTION ( 'NONE',  ( 0.000000000000000000, 1.000000000000000000, 8.717686153663073805E-15 ) ) ;
#80502 = ADVANCED_FACE ( 'NONE', ( #122156 ), #28253, .T. ) ;
#80503 = ADVANCED_FACE ( 'NONE', ( #183413 ), #204241, .F. ) ;
#80504 = CARTESIAN_POINT ( 'NONE',  ( -20.64999999999999858, -6.794814075650357665, -212.0940144922642219 ) ) ;
#80505 = AXIS2_PLACEMENT_3D ( 'NONE', #248146, #86474, #51196 ) ;
#80506 = DIRECTION ( 'NONE',  ( 0.000000000000000000, 0.9126074666063769270, 0.4088369013363283844 ) ) ;
#80507 = DIRECTION ( 'NONE',  ( 0.000000000000000000, 0.2617529984165152257, 0.9651348961777124202 ) ) ;
#80508 = VECTOR ( 'NONE', #168225, 1000.000000000000114 ) ;
#80509 = VERTEX_POINT ( 'NONE', #127285 ) ;
#80510 = EDGE_LOOP ( 'NONE', ( #257681, #204566, #65053, #156321 ) ) ;
#80511 = PLANE ( 'NONE',  #131415 ) ;
#80512 = ORIENTED_EDGE ( 'NONE', *, *, #105881, .T. ) ;
#80513 = CARTESIAN_POINT ( 'NONE',  ( 21.09107601085574402, 0.03930716472853410665, -27.13612202464005918 ) ) ;
#80514 = ORIENTED_EDGE ( 'NONE', *, *, #36101, .F. ) ;
#80516 = VECTOR ( 'NONE', #123600, 1000.000000000000114 ) ;
#80515 = CARTESIAN_POINT ( 'NONE',  ( -16.97683809663752186, 13.99889777621145903, -218.5199410132753144 ) ) ;
#80517 = CIRCLE ( 'NONE', #26404, 11.69999999999998863 ) ;
#80518 = AXIS2_PLACEMENT_3D ( 'NONE', #163651, #221038, #4555 ) ;
#80519 = CIRCLE ( 'NONE', #238782, 0.09999999999999913125 ) ;
#80520 = EDGE_CURVE ( 'NONE', #110463, #51771, #119825, .T. ) ;
#80521 = CARTESIAN_POINT ( 'NONE',  ( -14.87770893841227426, 49.47508301341329684, -233.4759538034894319 ) ) ;
#80522 = CARTESIAN_POINT ( 'NONE',  ( 20.94999999999999574, 7.128833340093095217, -233.7327013124392749 ) ) ;
#80523 = ADVANCED_FACE ( 'NONE', ( #245957 ), #142966, .T. ) ;
#80524 = DIRECTION ( 'NONE',  ( 0.000000000000000000, -6.938893903907233900E-15, 1.000000000000000000 ) ) ;
#80525 = CARTESIAN_POINT ( 'NONE',  ( 18.59999999999999076, 10.20857864377385127, -158.6500000000000057 ) ) ;
#80526 = ORIENTED_EDGE ( 'NONE', *, *, #171857, .T. ) ;
#80527 = CYLINDRICAL_SURFACE ( 'NONE', #225152, 0.1000000000000070832 ) ;
#80528 = VERTEX_POINT ( 'NONE', #84243 ) ;
#80529 = DIRECTION ( 'NONE',  ( 0.000000000000000000, 0.000000000000000000, 1.000000000000000000 ) ) ;
#80530 = DIRECTION ( 'NONE',  ( 1.000000000000000000, 0.000000000000000000, 0.000000000000000000 ) ) ;
#80531 = ADVANCED_FACE ( 'NONE', ( #43897 ), #222505, .F. ) ;
#80532 = DIRECTION ( 'NONE',  ( -1.000000000000000000, -0.000000000000000000, -0.000000000000000000 ) ) ;
#80533 = DIRECTION ( 'NONE',  ( -1.000000000000000000, -0.000000000000000000, -0.000000000000000000 ) ) ;
#80534 = ORIENTED_EDGE ( 'NONE', *, *, #82121, .F. ) ;
#80535 = CYLINDRICAL_SURFACE ( 'NONE', #135757, 0.09999999999999939493 ) ;
#80536 = AXIS2_PLACEMENT_3D ( 'NONE', #30574, #210482, #230035 ) ;
#80537 = ORIENTED_EDGE ( 'NONE', *, *, #68626, .T. ) ;
#80540 = ORIENTED_EDGE ( 'NONE', *, *, #149800, .T. ) ;
#80539 = DIRECTION ( 'NONE',  ( 0.000000000000000000, 6.853228547068871147E-15, -1.000000000000000000 ) ) ;
#80538 = DIRECTION ( 'NONE',  ( 1.186688945009010077E-16, -0.9770955615653316162, -0.2128009952263604232 ) ) ;
#80541 = CIRCLE ( 'NONE', #43170, 2.600000000000000089 ) ;
#80542 = AXIS2_PLACEMENT_3D ( 'NONE', #67117, #90520, #248321 ) ;
#80543 = CARTESIAN_POINT ( 'NONE',  ( -22.14074124539699540, 0.09905289585522827900, -160.1099221489562012 ) ) ;
#80544 = AXIS2_PLACEMENT_3D ( 'NONE', #133864, #187440, #49191 ) ;
#80545 = PLANE ( 'NONE',  #171184 ) ;
#80546 = ORIENTED_EDGE ( 'NONE', *, *, #97573, .T. ) ;
#80547 = DIRECTION ( 'NONE',  ( 4.239556034732056743E-17, -0.1298341882520022694, -0.9915357197604852679 ) ) ;
#80549 = CARTESIAN_POINT ( 'NONE',  ( -16.93211319090181988, 9.999986781168624717, -54.42250549927307191 ) ) ;
#80548 =( BOUNDED_SURFACE ( )  B_SPLINE_SURFACE ( 3, 2, ( 
 ( #132114, #190835, #189527 ),
 ( #146511, #250765, #128262 ),
 ( #10887, #12187, #229927 ),
 ( #51254, #72154, #151708 ) ),
 .UNSPECIFIED., .F., .F., .F. ) 
 B_SPLINE_SURFACE_WITH_KNOTS ( ( 4, 4 ),
 ( 3, 3 ),
 ( 0.0006461284895273917582, 0.0007503702773985995202 ),
 ( 0.000000000000000000, 1.000000000000000000 ),
 .UNSPECIFIED. ) 
 GEOMETRIC_REPRESENTATION_ITEM ( )  RATIONAL_B_SPLINE_SURFACE ( (
 ( 1.000000000000000000, 0.7071067811865475727, 1.000000000000000000),
 ( 1.000000000000000000, 0.7076476444648680530, 1.000000000000000000),
 ( 1.000000000000000000, 0.7075727925192004664, 1.000000000000000000),
 ( 1.000000000000000000, 0.7071067811865369146, 1.000000000000000000) ) ) 
 REPRESENTATION_ITEM ( '' )  SURFACE ( )  );
#80550 = FACE_OUTER_BOUND ( 'NONE', #203261, .T. ) ;
#80551 = UNCERTAINTY_MEASURE_WITH_UNIT (LENGTH_MEASURE( 1.000000000000000082E-05 ), #66681, 'distance_accuracy_value', 'NONE');
#80553 = ORIENTED_EDGE ( 'NONE', *, *, #253659, .F. ) ;
#80552 = CARTESIAN_POINT ( 'NONE',  ( 23.14999999999999503, 64.35000000001249987, -177.0379132551783812 ) ) ;
#80554 = ADVANCED_FACE ( 'NONE', ( #146826 ), #157440, .T. ) ;
#80555 = LINE ( 'NONE', #256600, #51775 ) ;
#80556 = ORIENTED_EDGE ( 'NONE', *, *, #51602, .T. ) ;
#80557 = ADVANCED_FACE ( 'NONE', ( #225072 ), #125989, .T. ) ;
#80558 = DIRECTION ( 'NONE',  ( 0.000000000000000000, 0.8814952561688430555, -0.4721928772777346239 ) ) ;
#80559 = DIRECTION ( 'NONE',  ( -1.000000000000000000, -3.265361837132813093E-16, 0.000000000000000000 ) ) ;
#80560 = CARTESIAN_POINT ( 'NONE',  ( -18.59999999999999787, -9.480686695267820596, -140.9411151687578752 ) ) ;
#80561 = ORIENTED_EDGE ( 'NONE', *, *, #70809, .T. ) ;
#80562 = CARTESIAN_POINT ( 'NONE',  ( -16.86422026484316916, 66.02955263915164608, -157.4408942588514151 ) ) ;
#80563 = ORIENTED_EDGE ( 'NONE', *, *, #46107, .F. ) ;
#80564 = CARTESIAN_POINT ( 'NONE',  ( 18.60000000000000142, 78.21362219944482774, -231.2727646510690249 ) ) ;
#80565 = ADVANCED_FACE ( 'NONE', ( #185972 ), #86849, .T. ) ;
#80566 = AXIS2_PLACEMENT_3D ( 'NONE', #25068, #66741, #141145 ) ;
#80567 = ADVANCED_FACE ( 'NONE', ( #47727 ), #28220, .T. ) ;
#80568 = CARTESIAN_POINT ( 'NONE',  ( 20.94999999999999929, 87.48912529308822172, -139.6231074845242688 ) ) ;
#80569 = FACE_OUTER_BOUND ( 'NONE', #241421, .T. ) ;
#80570 = ORIENTED_EDGE ( 'NONE', *, *, #141211, .F. ) ;
#80571 = CYLINDRICAL_SURFACE ( 'NONE', #162919, 0.1000000000000028644 ) ;
#80572 = EDGE_CURVE ( 'NONE', #173321, #199184, #257118, .T. ) ;
#80573 = CARTESIAN_POINT ( 'NONE',  ( -20.54999999999999716, 4.350000000011156054, -79.35000000000005116 ) ) ;
#80574 = CARTESIAN_POINT ( 'NONE',  ( -20.85000000000000142, 64.25000000001250555, -176.8069731475025321 ) ) ;
#80575 = ORIENTED_EDGE ( 'NONE', *, *, #48747, .T. ) ;
#80576 = DIRECTION ( 'NONE',  ( 0.000000000000000000, 6.982962677686266711E-15, -1.000000000000000000 ) ) ;
#80577 = LINE ( 'NONE', #19358, #106534 ) ;
#80578 = ORIENTED_EDGE ( 'NONE', *, *, #83244, .T. ) ;
#80580 = CARTESIAN_POINT ( 'NONE',  ( 18.59999999999999076, 10.20857864376269575, -21.35000000000000142 ) ) ;
#80579 = CIRCLE ( 'NONE', #118025, 0.1000000000000028644 ) ;
#80581 = EDGE_CURVE ( 'NONE', #229103, #164288, #186449, .T. ) ;
#80582 = CIRCLE ( 'NONE', #5760, 0.1000000000000002554 ) ;
#80583 = ORIENTED_EDGE ( 'NONE', *, *, #105570, .T. ) ;
#80584 = EDGE_CURVE ( 'NONE', #245973, #28383, #115710, .T. ) ;
#80585 = VERTEX_POINT ( 'NONE', #154286 ) ;
#80586 = AXIS2_PLACEMENT_3D ( 'NONE', #65307, #141014, #79715 ) ;
#80587 = DIRECTION ( 'NONE',  ( 1.000000000000000000, -0.000000000000000000, -0.000000000000000000 ) ) ;
#80588 = ORIENTED_EDGE ( 'NONE', *, *, #148933, .F. ) ;
#80590 = EDGE_LOOP ( 'NONE', ( #228126, #16161, #39967, #184037 ) ) ;
#80589 = CYLINDRICAL_SURFACE ( 'NONE', #59679, 7.899999999999990585 ) ;
#80591 = EDGE_CURVE ( 'NONE', #10090, #200329, #149048, .T. ) ;
#80594 = ORIENTED_EDGE ( 'NONE', *, *, #176201, .T. ) ;
#80593 = ORIENTED_EDGE ( 'NONE', *, *, #52716, .T. ) ;
#80592 = CARTESIAN_POINT ( 'NONE',  ( 20.94999999999999929, 5.400000000011154988, -188.5947339810868755 ) ) ;
#80595 = FACE_OUTER_BOUND ( 'NONE', #104617, .T. ) ;
#80596 = CARTESIAN_POINT ( 'NONE',  ( -21.07971444708686093, 0.08782343632898226282, -161.1702079183734213 ) ) ;
#80597 = PLANE ( 'NONE',  #227386 ) ;
#80598 = AXIS2_PLACEMENT_3D ( 'NONE', #228720, #129605, #212985 ) ;
#80599 = FACE_OUTER_BOUND ( 'NONE', #87326, .T. ) ;
#80600 = LINE ( 'NONE', #62358, #124242 ) ;
#80601 = ADVANCED_FACE ( 'NONE', ( #17304 ), #77249, .F. ) ;
#80602 = AXIS2_PLACEMENT_3D ( 'NONE', #168486, #169759, #71917 ) ;
#80603 = DIRECTION ( 'NONE',  ( -1.000000000000000000, 0.000000000000000000, 0.000000000000000000 ) ) ;
#80605 = DIRECTION ( 'NONE',  ( 0.000000000000000000, 0.8814952561688476074, -0.4721928772777262417 ) ) ;
#80604 = CARTESIAN_POINT ( 'NONE',  ( 18.59999999999999076, 70.22889768795992893, -198.1282601183952750 ) ) ;
#80606 = AXIS2_PLACEMENT_3D ( 'NONE', #32981, #92893, #214142 ) ;
#80607 = ORIENTED_EDGE ( 'NONE', *, *, #107506, .T. ) ;
#80608 = ORIENTED_EDGE ( 'NONE', *, *, #218882, .F. ) ;
#80609 = VECTOR ( 'NONE', #189011, 1000.000000000000000 ) ;
#80610 = EDGE_CURVE ( 'NONE', #207792, #190717, #65627, .T. ) ;
#80611 = DIRECTION ( 'NONE',  ( 0.000000000000000000, 0.2128009952263604510, -0.9770955615653315052 ) ) ;
#80613 = EDGE_LOOP ( 'NONE', ( #10596, #43386, #125595, #250018 ) ) ;
#80612 = DIRECTION ( 'NONE',  ( 0.000000000000000000, 2.891205793294679805E-16, -1.000000000000000000 ) ) ;
#80614 = CARTESIAN_POINT ( 'NONE',  ( 20.95000000000000284, 56.16603649944111254, -228.1013850343386480 ) ) ;
#80615 = ORIENTED_EDGE ( 'NONE', *, *, #118951, .T. ) ;
#80616 = DIRECTION ( 'NONE',  ( -1.000000000000000000, 1.207181226542539700E-16, -2.694675058168174199E-16 ) ) ;
#80617 = VERTEX_POINT ( 'NONE', #257131 ) ;
#80618 = EDGE_CURVE ( 'NONE', #216635, #151423, #7365, .T. ) ;
#80619 = DIRECTION ( 'NONE',  ( 0.000000000000000000, 0.000000000000000000, -1.000000000000000000 ) ) ;
#80620 = EDGE_CURVE ( 'NONE', #59200, #250188, #253250, .T. ) ;
#80621 = AXIS2_PLACEMENT_3D ( 'NONE', #123356, #239452, #158654 ) ;
#80622 = AXIS2_PLACEMENT_3D ( 'NONE', #91542, #147663, #227190 ) ;
#80623 = ORIENTED_EDGE ( 'NONE', *, *, #249823, .T. ) ;
#80624 = AXIS2_PLACEMENT_3D ( 'NONE', #224513, #23787, #142409 ) ;
#80625 = CARTESIAN_POINT ( 'NONE',  ( -20.94999999999999929, 1.115600667400684642E-11, -167.4999999999999716 ) ) ;
#80626 = DIRECTION ( 'NONE',  ( 0.000000000000000000, 0.000000000000000000, 1.000000000000000000 ) ) ;
#80628 = ORIENTED_EDGE ( 'NONE', *, *, #62158, .T. ) ;
#80627 = ORIENTED_EDGE ( 'NONE', *, *, #246180, .T. ) ;
#80629 = ORIENTED_EDGE ( 'NONE', *, *, #101516, .T. ) ;
#80630 = LINE ( 'NONE', #118522, #186341 ) ;
#80631 = EDGE_LOOP ( 'NONE', ( #21142, #31841, #236669, #197323 ) ) ;
#80632 = ORIENTED_EDGE ( 'NONE', *, *, #63786, .T. ) ;
#80634 = CARTESIAN_POINT ( 'NONE',  ( -20.85000000000000142, 76.00000000001170974, -69.52310748452431710 ) ) ;
#80633 = CIRCLE ( 'NONE', #101263, 2.599999999999998312 ) ;
#80636 = EDGE_LOOP ( 'NONE', ( #133342, #138265, #87522, #223745 ) ) ;
#80635 = DIRECTION ( 'NONE',  ( 1.000000000000000000, -0.000000000000000000, -0.000000000000000000 ) ) ;
#80637 = EDGE_CURVE ( 'NONE', #169297, #169606, #249174, .T. ) ;
#80639 = CARTESIAN_POINT ( 'NONE',  ( -16.88560720703333473, 60.93831840527001020, -221.0434021371021345 ) ) ;
#80638 = CARTESIAN_POINT ( 'NONE',  ( 20.94999999999999574, 60.83337574417771521, -225.3422414619149095 ) ) ;
#80640 = DIRECTION ( 'NONE',  ( 1.000000000000000000, -0.000000000000000000, -0.000000000000000000 ) ) ;
#80641 = CARTESIAN_POINT ( 'NONE',  ( -20.00857864376270001, 9.150000000011157653, -121.7500000000000426 ) ) ;
#80642 = CARTESIAN_POINT ( 'NONE',  ( 23.40000000000005542, 73.52684270758111040, -52.27034697567518862 ) ) ;
#80643 = EDGE_LOOP ( 'NONE', ( #215360, #105686, #225130, #56930 ) ) ;
#80644 = VECTOR ( 'NONE', #191792, 999.9999999999998863 ) ;
#80645 = B_SPLINE_CURVE_WITH_KNOTS ( 'NONE', 3,
 ( #88825, #91426, #53579, #189245, #74462, #207531, #171009, #191835, #52268, #172290 ),
 .UNSPECIFIED., .F., .F.,
 ( 4, 2, 2, 2, 4 ),
 ( 0.000000000000000000, 0.0003916577441626726262, 0.0005874866162440096169, 0.0006854010522846797114, 0.0007833154883253498060 ),
 .UNSPECIFIED. ) ;
#80646 = CIRCLE ( 'NONE', #230528, 0.1000000000000002554 ) ;
#80647 = AXIS2_PLACEMENT_3D ( 'NONE', #14141, #93651, #255234 ) ;
#80648 = ORIENTED_EDGE ( 'NONE', *, *, #200566, .F. ) ;
#80649 = AXIS2_PLACEMENT_3D ( 'NONE', #49994, #70877, #150399 ) ;
#80650 = CARTESIAN_POINT ( 'NONE',  ( 20.85000000000000142, 46.02130280899747561, -256.6489974955837852 ) ) ;
#80651 = ORIENTED_EDGE ( 'NONE', *, *, #28595, .T. ) ;
#80652 = LINE ( 'NONE', #18137, #132159 ) ;
#80653 = CARTESIAN_POINT ( 'NONE',  ( -18.59999999999999787, -1.362429037182155023, -141.8888812479212334 ) ) ;
#80654 = CARTESIAN_POINT ( 'NONE',  ( -13.43673303185028978, 12.44126776692609759, -213.7332981774226539 ) ) ;
#80655 = ORIENTED_EDGE ( 'NONE', *, *, #124593, .T. ) ;
#80656 = VERTEX_POINT ( 'NONE', #233781 ) ;
#80657 =( BOUNDED_SURFACE ( )  B_SPLINE_SURFACE ( 3, 2, ( 
 ( #14788, #137262, #211693 ),
 ( #194707, #236368, #250792 ),
 ( #96825, #176422, #13484 ),
 ( #255880, #175165, #231258 ),
 ( #76013, #93006, #172599 ),
 ( #72181, #135968, #232548 ),
 ( #53887, #133424, #55131 ),
 ( #212959, #12213, #94283 ),
 ( #115144, #254623, #34349 ),
 ( #173881, #74773, #134682 ) ),
 .UNSPECIFIED., .F., .F., .T. ) 
 B_SPLINE_SURFACE_WITH_KNOTS ( ( 4, 2, 2, 2, 4 ),
 ( 3, 3 ),
 ( 0.0001836757140119112878, 0.0004000170051583592156, 0.0005081876507315832067, 0.0005622729735181951479, 0.0006163582963048070892 ),
 ( 0.000000000000000000, 1.000000000000000000 ),
 .UNSPECIFIED. ) 
 GEOMETRIC_REPRESENTATION_ITEM ( )  RATIONAL_B_SPLINE_SURFACE ( (
 ( 1.000000000000000000, 0.7071067811865870967, 1.000000000000000000),
 ( 1.000000000000000000, 0.6461995200020528296, 1.000000000000000000),
 ( 1.000000000000000000, 0.5776453529561198508, 1.000000000000000000),
 ( 1.000000000000000000, 0.4585233068345995755, 1.000000000000000000),
 ( 1.000000000000000000, 0.4154092989941690628, 1.000000000000000000),
 ( 1.000000000000000000, 0.3550093145835241937, 1.000000000000000000),
 ( 1.000000000000000000, 0.3354498651686700361, 1.000000000000000000),
 ( 1.000000000000000000, 0.3060347992254511817, 1.000000000000000000),
 ( 1.000000000000000000, 0.2963555829627100846, 1.000000000000000000),
 ( 1.000000000000000000, 0.2966190024561151661, 1.000000000000000000) ) ) 
 REPRESENTATION_ITEM ( '' )  SURFACE ( )  );
#80658 = DIRECTION ( 'NONE',  ( 1.000000000000000000, 0.000000000000000000, 0.000000000000000000 ) ) ;
#80659 = EDGE_CURVE ( 'NONE', #103333, #183612, #120020, .T. ) ;
#80660 = DIRECTION ( 'NONE',  ( 0.000000000000000000, 0.000000000000000000, 1.000000000000000000 ) ) ;
#80661 = VERTEX_POINT ( 'NONE', #74739 ) ;
#80662 = DIRECTION ( 'NONE',  ( 0.000000000000000000, 1.000000000000000000, 6.982962677686266711E-15 ) ) ;
#80663 = VERTEX_POINT ( 'NONE', #194678 ) ;
#80664 = CARTESIAN_POINT ( 'NONE',  ( -20.54999999999999716, 68.85000000001154774, -52.77310748452437394 ) ) ;
#80665 = CARTESIAN_POINT ( 'NONE',  ( 18.49999999999999289, 68.97833521811179480, -99.18954208262705663 ) ) ;
#80667 = DIRECTION ( 'NONE',  ( 0.000000000000000000, -7.056502275159890043E-15, 1.000000000000000000 ) ) ;
#80666 = CARTESIAN_POINT ( 'NONE',  ( -22.16821283564876666, 10.69812671114206282, -227.0695021710342871 ) ) ;
#80668 = CYLINDRICAL_SURFACE ( 'NONE', #169856, 0.1000000000000028644 ) ;
#80669 = DIRECTION ( 'NONE',  ( 1.000000000000000000, 0.000000000000000000, 0.000000000000000000 ) ) ;
#80670 = AXIS2_PLACEMENT_3D ( 'NONE', #132467, #115459, #175468 ) ;
#80671 = AXIS2_PLACEMENT_3D ( 'NONE', #116320, #173767, #91604 ) ;
#80672 = ORIENTED_EDGE ( 'NONE', *, *, #224630, .T. ) ;
#80673 = CARTESIAN_POINT ( 'NONE',  ( -20.54999999999999716, -9.500000000000003553, -9.893969122652444881 ) ) ;
#80674 = EDGE_CURVE ( 'NONE', #46658, #15410, #195016, .T. ) ;
#80675 = AXIS2_PLACEMENT_3D ( 'NONE', #110666, #229343, #230626 ) ;
#80677 = ORIENTED_EDGE ( 'NONE', *, *, #213451, .T. ) ;
#80676 = ORIENTED_EDGE ( 'NONE', *, *, #118512, .F. ) ;
#80678 = ORIENTED_EDGE ( 'NONE', *, *, #31768, .F. ) ;
#80679 = ORIENTED_EDGE ( 'NONE', *, *, #214169, .T. ) ;
#80680 = DIRECTION ( 'NONE',  ( 1.000000000000000000, -0.000000000000000000, -0.000000000000000000 ) ) ;
#80681 = CARTESIAN_POINT ( 'NONE',  ( -18.59999999999999787, -1.162701749926853712, -142.1000000000000227 ) ) ;
#80682 = AXIS2_PLACEMENT_3D ( 'NONE', #255419, #235896, #241061 ) ;
#80683 = CARTESIAN_POINT ( 'NONE',  ( 20.04142135623730070, 64.35000000001177511, -78.37310748452439668 ) ) ;
#80684 = DIRECTION ( 'NONE',  ( 0.000000000000000000, 1.000000000000000000, 0.000000000000000000 ) ) ;
#80685 = DIRECTION ( 'NONE',  ( 1.000000000000000000, 0.000000000000000000, 0.000000000000000000 ) ) ;
#80687 = CARTESIAN_POINT ( 'NONE',  ( 21.05000000000000071, 58.86929801030535714, -225.7185417581880529 ) ) ;
#80686 = DIRECTION ( 'NONE',  ( 1.000000000000000000, 1.070816960479510500E-16, 0.000000000000000000 ) ) ;
#80688 = EDGE_LOOP ( 'NONE', ( #16770, #206802, #248070, #257280 ) ) ;
#80689 = CARTESIAN_POINT ( 'NONE',  ( -21.05000000000000071, 6.258842723548988296, -167.4679863068125769 ) ) ;
#80690 = ORIENTED_EDGE ( 'NONE', *, *, #19664, .F. ) ;
#80691 = CIRCLE ( 'NONE', #226421, 11.80000000000000426 ) ;
#80692 = CARTESIAN_POINT ( 'NONE',  ( -22.50000000000000000, 11.64957080755595520, -66.90000000000004832 ) ) ;
#80693 = ORIENTED_EDGE ( 'NONE', *, *, #242464, .F. ) ;
#80694 = VERTEX_POINT ( 'NONE', #215483 ) ;
#80695 = FACE_OUTER_BOUND ( 'NONE', #87675, .T. ) ;
#80696 = AXIS2_PLACEMENT_3D ( 'NONE', #160382, #243737, #23442 ) ;
#80697 = FACE_OUTER_BOUND ( 'NONE', #100752, .T. ) ;
#80698 = DIRECTION ( 'NONE',  ( 1.836970198721029934E-16, -1.000000000000000000, -0.000000000000000000 ) ) ;
#80699 = AXIS2_PLACEMENT_3D ( 'NONE', #5072, #84594, #243720 ) ;
#80700 = CARTESIAN_POINT ( 'NONE',  ( 13.76927104934456558, 9.455987233623895705, -82.01153116689783928 ) ) ;
#80701 = CIRCLE ( 'NONE', #1596, 0.09999999999999939493 ) ;
#80702 = CIRCLE ( 'NONE', #101114, 0.1000000000000060146 ) ;
#80703 = CARTESIAN_POINT ( 'NONE',  ( 21.00000000000000000, 6.644425182197215562, 9.641788261573355001 ) ) ;
#80704 = VERTEX_POINT ( 'NONE', #35603 ) ;
#80705 = EDGE_LOOP ( 'NONE', ( #94166, #254730, #141668, #78224 ) ) ;
#80706 = DIRECTION ( 'NONE',  ( 0.000000000000000000, 0.000000000000000000, -1.000000000000000000 ) ) ;
#80707 = ORIENTED_EDGE ( 'NONE', *, *, #79157, .T. ) ;
#80708 = DIRECTION ( 'NONE',  ( 0.000000000000000000, 0.000000000000000000, -1.000000000000000000 ) ) ;
#80710 = AXIS2_PLACEMENT_3D ( 'NONE', #217674, #242392, #20810 ) ;
#80709 = DIRECTION ( 'NONE',  ( -0.000000000000000000, -6.982962677686266711E-15, 1.000000000000000000 ) ) ;
#80711 = CARTESIAN_POINT ( 'NONE',  ( 23.15000000000000213, -8.999999999988844479, -110.3939691226524786 ) ) ;
#80712 = LINE ( 'NONE', #40367, #184023 ) ;
#80713 = CARTESIAN_POINT ( 'NONE',  ( -23.25000000000000000, 64.35000000001203091, -114.7731074845243882 ) ) ;
#80715 = DIRECTION ( 'NONE',  ( 0.000000000000000000, -7.172728831056617961E-15, 1.000000000000000000 ) ) ;
#80714 = CARTESIAN_POINT ( 'NONE',  ( -18.60000000000000142, 85.52395432076488646, -129.6410904276969518 ) ) ;
#80717 = ADVANCED_FACE ( 'NONE', ( #175132 ), #211577, .F. ) ;
#80716 = DIRECTION ( 'NONE',  ( 0.000000000000000000, 3.208737065390626061E-15, 1.000000000000000000 ) ) ;
#80718 = CARTESIAN_POINT ( 'NONE',  ( -21.07928932188134041, 6.162520550852570445, -199.5566553493337665 ) ) ;
#80719 = AXIS2_PLACEMENT_3D ( 'NONE', #175909, #238422, #18083 ) ;
#80720 = LINE ( 'NONE', #121190, #99488 ) ;
#80721 = DIRECTION ( 'NONE',  ( -1.000000000000000000, 0.000000000000000000, 0.000000000000000000 ) ) ;
#80722 = VECTOR ( 'NONE', #9698, 1000.000000000000114 ) ;
#80723 = VERTEX_POINT ( 'NONE', #115107 ) ;
#80724 = TOROIDAL_SURFACE ( 'NONE', #201534, 11.65000000000000036, 0.1000000000000000056 ) ;
#80725 = EDGE_CURVE ( 'NONE', #72480, #172095, #103387, .T. ) ;
#80726 = CARTESIAN_POINT ( 'NONE',  ( 20.95462737510932882, 10.55678195165489441, -41.06995005656229836 ) ) ;
#80727 = ORIENTED_EDGE ( 'NONE', *, *, #15541, .F. ) ;
#80728 = CARTESIAN_POINT ( 'NONE',  ( 18.41356215285961540, 85.50000000001209344, -129.4910380878245917 ) ) ;
#80729 = EDGE_CURVE ( 'NONE', #109631, #28235, #155552, .T. ) ;
#80730 = CARTESIAN_POINT ( 'NONE',  ( -18.34804628011471195, 11.47316190337353525, -109.7500000000000426 ) ) ;
#80731 = CARTESIAN_POINT ( 'NONE',  ( 22.39999999999999503, 64.35000000001194564, -103.1231074845243825 ) ) ;
#80732 = ORIENTED_EDGE ( 'NONE', *, *, #152482, .T. ) ;
#80733 = DIRECTION ( 'NONE',  ( 0.000000000000000000, 1.776356839400254803E-15, 1.000000000000000000 ) ) ;
#80734 = CARTESIAN_POINT ( 'NONE',  ( -23.15000000000000213, 64.35000000001228670, -157.8731074845244393 ) ) ;
#80735 = DIRECTION ( 'NONE',  ( 0.000000000000000000, 0.000000000000000000, -1.000000000000000000 ) ) ;
#80736 = EDGE_CURVE ( 'NONE', #36696, #9149, #236334, .T. ) ;
#80737 = AXIS2_PLACEMENT_3D ( 'NONE', #42102, #121638, #221964 ) ;
#80738 = TOROIDAL_SURFACE ( 'NONE', #130831, 7.800000000000000711, 0.1000000000000000056 ) ;
#80740 = DIRECTION ( 'NONE',  ( -0.000000000000000000, 1.000000000000000000, 6.982962677686266711E-15 ) ) ;
#80739 = AXIS2_PLACEMENT_3D ( 'NONE', #125844, #25489, #183269 ) ;
#80741 = DIRECTION ( 'NONE',  ( 0.000000000000000000, 6.982962677686266711E-15, -1.000000000000000000 ) ) ;
#80742 = DIRECTION ( 'NONE',  ( 0.000000000000000000, 0.000000000000000000, -1.000000000000000000 ) ) ;
#80743 = ORIENTED_EDGE ( 'NONE', *, *, #151432, .T. ) ;
#80744 = CARTESIAN_POINT ( 'NONE',  ( -23.25000000000000000, 87.65000000001269598, -203.5231074845243029 ) ) ;
#80746 = ORIENTED_EDGE ( 'NONE', *, *, #55290, .T. ) ;
#80745 = PLANE ( 'NONE',  #84399 ) ;
#80747 = CARTESIAN_POINT ( 'NONE',  ( -20.85000000000000142, 68.97833521811203639, -132.6895420826271277 ) ) ;
#80748 = DIRECTION ( 'NONE',  ( 1.000000000000000000, -0.000000000000000000, -0.000000000000000000 ) ) ;
#80749 = ADVANCED_FACE ( 'NONE', ( #98072 ), #40907, .T. ) ;
#80750 = DIRECTION ( 'NONE',  ( 0.000000000000000000, 0.000000000000000000, -1.000000000000000000 ) ) ;
#80751 = ORIENTED_EDGE ( 'NONE', *, *, #150307, .T. ) ;
#80752 = DIRECTION ( 'NONE',  ( 0.000000000000000000, 0.8660254037844377084, 0.5000000000000015543 ) ) ;
#80753 = APPLICATION_PROTOCOL_DEFINITION ( 'draft international standard', 'automotive_design', 1998, #229068 ) ;
#80755 = EDGE_CURVE ( 'NONE', #257455, #109848, #158168, .T. ) ;
#80754 = CARTESIAN_POINT ( 'NONE',  ( -20.54999999999999716, 7.128833340094563376, -233.7327013124401276 ) ) ;
#80756 = EDGE_LOOP ( 'NONE', ( #76780, #143121, #114680, #19798 ) ) ;
#80757 = CARTESIAN_POINT ( 'NONE',  ( 20.94999999999999929, 1.115600667400684642E-11, -79.87500000000004263 ) ) ;
#80758 = FACE_OUTER_BOUND ( 'NONE', #39606, .T. ) ;
#80759 = VECTOR ( 'NONE', #117108, 1000.000000000000000 ) ;
#80760 = CYLINDRICAL_SURFACE ( 'NONE', #212054, 0.1000000000000055844 ) ;
#80761 = ORIENTED_EDGE ( 'NONE', *, *, #100480, .F. ) ;
#80762 = ORIENTED_EDGE ( 'NONE', *, *, #53567, .F. ) ;
#80763 = DIRECTION ( 'NONE',  ( 0.000000000000000000, 6.982962677686266711E-15, -1.000000000000000000 ) ) ;
#80764 = CARTESIAN_POINT ( 'NONE',  ( 21.14999999999999858, -11.38316329222461754, -203.4791315943886048 ) ) ;
#80765 = EDGE_CURVE ( 'NONE', #222996, #64517, #78464, .T. ) ;
#80766 = DIRECTION ( 'NONE',  ( 1.000000000000000000, 0.000000000000000000, 0.000000000000000000 ) ) ;
#80767 = CARTESIAN_POINT ( 'NONE',  ( 22.49806830649814060, 64.35011034517360429, -203.6005718008499628 ) ) ;
#80768 = DIRECTION ( 'NONE',  ( 0.000000000000000000, -7.429790795770644761E-15, 1.000000000000000000 ) ) ;
#80769 = DIRECTION ( 'NONE',  ( 0.000000000000000000, 0.000000000000000000, 1.000000000000000000 ) ) ;
#80770 = CARTESIAN_POINT ( 'NONE',  ( 21.05000000000000071, -1.335782702529562771, -194.7974669479901593 ) ) ;
#80771 = DIRECTION ( 'NONE',  ( -0.000000000000000000, 1.000000000000000000, -0.000000000000000000 ) ) ;
#80772 = CYLINDRICAL_SURFACE ( 'NONE', #127096, 3.999999999999996447 ) ;
#80773 = CARTESIAN_POINT ( 'NONE',  ( -20.85000000000000142, -1.835859311432481045, -78.50443916879852679 ) ) ;
#80775 = DIRECTION ( 'NONE',  ( -0.000000000000000000, -0.2617529984165031243, -0.9651348961777157509 ) ) ;
#80774 = AXIS2_PLACEMENT_3D ( 'NONE', #198289, #36687, #253113 ) ;
#80776 = EDGE_LOOP ( 'NONE', ( #218010, #169869, #57479 ) ) ;
#80777 = AXIS2_PLACEMENT_3D ( 'NONE', #256512, #54524, #33733 ) ;
#80778 = ORIENTED_EDGE ( 'NONE', *, *, #55379, .F. ) ;
#80779 = DIRECTION ( 'NONE',  ( -1.000000000000000000, 0.000000000000000000, 0.000000000000000000 ) ) ;
#80781 = CARTESIAN_POINT ( 'NONE',  ( 21.10710606213542562, 67.22310597611939897, -191.2821109581250028 ) ) ;
#80780 = CIRCLE ( 'NONE', #101610, 0.09999999999999982514 ) ;
#80782 = ADVANCED_FACE ( 'NONE', ( #203628 ), #178972, .F. ) ;
#80783 = DIRECTION ( 'NONE',  ( 0.000000000000000000, -1.000000000000000000, 0.000000000000000000 ) ) ;
#80784 = DIRECTION ( 'NONE',  ( -1.000000000000000000, -0.000000000000000000, -0.000000000000000000 ) ) ;
#80785 = CARTESIAN_POINT ( 'NONE',  ( 18.54999999999999716, 62.09751964147213243, -221.3558313336858703 ) ) ;
#80786 = ORIENTED_EDGE ( 'NONE', *, *, #39770, .T. ) ;
#80787 = CYLINDRICAL_SURFACE ( 'NONE', #60041, 7.899999999999990585 ) ;
#80788 = EDGE_CURVE ( 'NONE', #94099, #246280, #82531, .T. ) ;
#80789 = ORIENTED_EDGE ( 'NONE', *, *, #75082, .F. ) ;
#80791 = CIRCLE ( 'NONE', #218346, 0.09999999999998898659 ) ;
#80790 = CARTESIAN_POINT ( 'NONE',  ( -13.77083647240106323, 9.457410930290160778, -18.49991590874628855 ) ) ;
#80792 = EDGE_LOOP ( 'NONE', ( #121563, #186672, #197984, #174637 ) ) ;
#80793 = ADVANCED_FACE ( 'NONE', ( #182805 ), #100639, .T. ) ;
#80794 = CARTESIAN_POINT ( 'NONE',  ( 23.14999999999999503, 11.65000000001116298, -88.35000000000003695 ) ) ;
#80795 = TOROIDAL_SURFACE ( 'NONE', #226532, 0.2000000000000000111, 0.1000000000000000056 ) ;
#80796 = ADVANCED_FACE ( 'NONE', ( #198489 ), #25019, .T. ) ;
#80798 = DIRECTION ( 'NONE',  ( 0.000000000000000000, 0.2128009952263056614, -0.9770955615653434956 ) ) ;
#80797 = CIRCLE ( 'NONE', #93285, 0.09999999999998898659 ) ;
#80799 = ORIENTED_EDGE ( 'NONE', *, *, #44106, .T. ) ;
#80800 = CARTESIAN_POINT ( 'NONE',  ( -17.05016517655715091, 66.05000000001636806, -190.8504094885308575 ) ) ;
#80801 = B_SPLINE_CURVE_WITH_KNOTS ( 'NONE', 3,
 ( #233640, #99227, #17169, #118834, #134, #18430, #159245, #176245, #15895, #154137, #255710, #238766, #77116, #156693, #60107, #97935, #135793, #236188, #219185 ),
 .UNSPECIFIED., .F., .F.,
 ( 4, 3, 3, 3, 3, 3, 4 ),
 ( 0.0001624081864585780774, 0.0001685232196531779832, 0.0001764526673566780949, 0.0001916878551483017082, 0.0002009890782182522653, 0.0002238845907554767498, 0.0002283406619926077572 ),
 .UNSPECIFIED. ) ;
#80802 = ADVANCED_FACE ( 'NONE', ( #240203 ), #43277, .T. ) ;
#80803 = EDGE_LOOP ( 'NONE', ( #188115, #52673, #112458, #206472 ) ) ;
#80804 = CYLINDRICAL_SURFACE ( 'NONE', #166221, 0.09999999999999939493 ) ;
#80805 = CARTESIAN_POINT ( 'NONE',  ( -20.94999999999999929, 74.16465844978819177, -191.9679561919613775 ) ) ;
#80806 = ADVANCED_FACE ( 'NONE', ( #122827 ), #62834, .T. ) ;
#80808 = FACE_OUTER_BOUND ( 'NONE', #161369, .T. ) ;
#80807 = AXIS2_PLACEMENT_3D ( 'NONE', #247601, #45552, #245035 ) ;
#80809 = EDGE_CURVE ( 'NONE', #150130, #113518, #45151, .T. ) ;
#80810 = CYLINDRICAL_SURFACE ( 'NONE', #209887, 1.749999999999999778 ) ;
#80813 = CARTESIAN_POINT ( 'NONE',  ( 18.49999999999998934, 65.70711192142385926, -131.0651054685122858 ) ) ;
#80812 = AXIS2_PLACEMENT_3D ( 'NONE', #177414, #56130, #256865 ) ;
#80811 = CARTESIAN_POINT ( 'NONE',  ( -21.45000000000000284, 7.708578643773852157, -155.1500000000000057 ) ) ;
#80814 = DIRECTION ( 'NONE',  ( 1.000000000000000000, 0.000000000000000000, 0.000000000000000000 ) ) ;
#80816 = EDGE_LOOP ( 'NONE', ( #177778, #94865, #178710, #199031, #126055, #52480, #31051, #137957, #139862, #33453 ) ) ;
#80815 = CARTESIAN_POINT ( 'NONE',  ( 20.54374330479327426, 65.49498968578909341, -128.7974238496362602 ) ) ;
#80818 = CARTESIAN_POINT ( 'NONE',  ( 20.94999999999999574, 4.158309866074138661, -211.9342015984041439 ) ) ;
#80817 = DIRECTION ( 'NONE',  ( 0.000000000000000000, -0.8700118002898356018, 0.4930308989875170078 ) ) ;
#80819 = AXIS2_PLACEMENT_3D ( 'NONE', #171372, #108776, #8407 ) ;
#80820 = ORIENTED_EDGE ( 'NONE', *, *, #41553, .F. ) ;
#80822 = ORIENTED_EDGE ( 'NONE', *, *, #5826, .T. ) ;
#80821 = CARTESIAN_POINT ( 'NONE',  ( -23.39999999999994529, 74.16448838626247664, -47.52760213295649550 ) ) ;
#80823 = ORIENTED_EDGE ( 'NONE', *, *, #73310, .T. ) ;
#80824 = CARTESIAN_POINT ( 'NONE',  ( 18.49999999999999645, -1.299733671219632791, -157.5281295228693637 ) ) ;
#80825 = CARTESIAN_POINT ( 'NONE',  ( -18.59999999999999787, -1.835859311432481045, -212.5044391687984842 ) ) ;
#80826 = PLANE ( 'NONE',  #130715 ) ;
#80827 = EDGE_CURVE ( 'NONE', #189976, #191026, #184059, .T. ) ;
#80828 = AXIS2_PLACEMENT_3D ( 'NONE', #63918, #224263, #209510 ) ;
#80829 = ORIENTED_EDGE ( 'NONE', *, *, #155397, .T. ) ;
#80830 = FACE_OUTER_BOUND ( 'NONE', #12996, .T. ) ;
#80831 = DIRECTION ( 'NONE',  ( 1.186688945009009831E-16, -1.000000000000000000, 0.000000000000000000 ) ) ;
#80832 = DIRECTION ( 'NONE',  ( 1.000000000000000000, 0.000000000000000000, 0.000000000000000000 ) ) ;
#80833 = EDGE_CURVE ( 'NONE', #217574, #14270, #90935, .T. ) ;
#80834 = DIRECTION ( 'NONE',  ( 0.000000000000000000, -6.547589603894034005E-15, 1.000000000000000000 ) ) ;
#80835 = AXIS2_PLACEMENT_3D ( 'NONE', #4187, #163286, #125440 ) ;
#80836 = CARTESIAN_POINT ( 'NONE',  ( 23.14999999999999858, 76.00000000001142553, -36.02310748452432421 ) ) ;
#80837 = CARTESIAN_POINT ( 'NONE',  ( 21.07933241753356768, 69.67135405163237749, -136.6164870749436488 ) ) ;
#80838 = ORIENTED_EDGE ( 'NONE', *, *, #193323, .T. ) ;
#80839 = ORIENTED_EDGE ( 'NONE', *, *, #104986, .T. ) ;
#80840 = DIRECTION ( 'NONE',  ( 0.000000000000000000, -0.9901894034181596416, -0.1397316906016281834 ) ) ;
#80841 = ORIENTED_EDGE ( 'NONE', *, *, #107191, .T. ) ;
#80842 = CARTESIAN_POINT ( 'NONE',  ( 21.05000000000000071, 1.835341550235569663, -112.0551512925630249 ) ) ;
#80843 = VERTEX_POINT ( 'NONE', #78534 ) ;
#80844 = CARTESIAN_POINT ( 'NONE',  ( 20.84999999999998721, 10.33248238083634440, -173.0948465439131496 ) ) ;
#80845 = EDGE_CURVE ( 'NONE', #218469, #44901, #24330, .T. ) ;
#80846 = CARTESIAN_POINT ( 'NONE',  ( -20.64999999999999858, 44.96555909964510533, -237.8856228368455845 ) ) ;
#80847 = DIRECTION ( 'NONE',  ( 0.000000000000000000, 0.4999999999999956701, -0.8660254037844411501 ) ) ;
#80848 = EDGE_CURVE ( 'NONE', #203482, #172794, #237629, .T. ) ;
#80849 = FACE_OUTER_BOUND ( 'NONE', #184994, .T. ) ;
#80850 = CARTESIAN_POINT ( 'NONE',  ( 5.900000000000060751, 64.25000000001119815, -22.12310748452479103 ) ) ;
#80851 = ORIENTED_EDGE ( 'NONE', *, *, #256149, .F. ) ;
#80852 = AXIS2_PLACEMENT_3D ( 'NONE', #15767, #215217, #36616 ) ;
#80853 = VECTOR ( 'NONE', #25410, 1000.000000000000000 ) ;
#80854 = EDGE_CURVE ( 'NONE', #45647, #1820, #242740, .T. ) ;
#80855 = DIRECTION ( 'NONE',  ( 0.000000000000000000, 1.224646799142015331E-16, 1.000000000000000000 ) ) ;
#80856 = CARTESIAN_POINT ( 'NONE',  ( -22.50000000000094147, 0.1008583691097610646, -88.75043287651061519 ) ) ;
#80857 = CARTESIAN_POINT ( 'NONE',  ( 20.94999999999999929, -1.162701749926853712, -108.4000000000000341 ) ) ;
#80858 = CIRCLE ( 'NONE', #64312, 11.65000000000000036 ) ;
#80859 = ORIENTED_EDGE ( 'NONE', *, *, #147576, .T. ) ;
#80861 = DIRECTION ( 'NONE',  ( 0.000000000000000000, 0.9126074666063735963, 0.4088369013363361004 ) ) ;
#80860 = CARTESIAN_POINT ( 'NONE',  ( -21.76363531954647357, 75.90099812571297377, -177.0360440323960916 ) ) ;
#80862 = ORIENTED_EDGE ( 'NONE', *, *, #19103, .F. ) ;
#80865 = ORIENTED_EDGE ( 'NONE', *, *, #145010, .F. ) ;
#80864 = DIRECTION ( 'NONE',  ( -1.000000000000000000, 0.000000000000000000, 0.000000000000000000 ) ) ;
#80863 = DIRECTION ( 'NONE',  ( 0.000000000000000000, 7.056502275159894776E-15, -1.000000000000000000 ) ) ;
#80866 = VERTEX_POINT ( 'NONE', #60256 ) ;
#80867 = CARTESIAN_POINT ( 'NONE',  ( -20.90000000000000213, 1.311673547813416718, -7.986648289447971116 ) ) ;
#80868 = AXIS2_PLACEMENT_3D ( 'NONE', #77017, #135699, #79571 ) ;
#80869 = DIRECTION ( 'NONE',  ( -5.551115123125807946E-13, -0.4608403197577645716, -0.8874830700839093645 ) ) ;
#80870 = DIRECTION ( 'NONE',  ( 1.000000000000000000, 0.000000000000000000, 0.000000000000000000 ) ) ;
#80871 = AXIS2_PLACEMENT_3D ( 'NONE', #236879, #234309, #257665 ) ;
#80872 = ORIENTED_EDGE ( 'NONE', *, *, #144711, .F. ) ;
#80873 = DIRECTION ( 'NONE',  ( -0.7071067811865474617, -0.7071067811865474617, -0.000000000000000000 ) ) ;
#80874 = DIRECTION ( 'NONE',  ( 0.000000000000000000, 0.000000000000000000, -1.000000000000000000 ) ) ;
#80875 = AXIS2_PLACEMENT_3D ( 'NONE', #53877, #154308, #69600 ) ;
#80877 = FACE_OUTER_BOUND ( 'NONE', #212364, .T. ) ;
#80876 = FACE_OUTER_BOUND ( 'NONE', #113156, .T. ) ;
#80879 = VERTEX_POINT ( 'NONE', #22448 ) ;
#80878 = DIRECTION ( 'NONE',  ( 1.000000000000000000, -0.000000000000000000, -0.000000000000000000 ) ) ;
#80880 = AXIS2_PLACEMENT_3D ( 'NONE', #46344, #68498, #125883 ) ;
#80881 = EDGE_CURVE ( 'NONE', #77128, #189866, #145092, .T. ) ;
#80882 = CIRCLE ( 'NONE', #189240, 0.09999999999999938105 ) ;
#80883 = AXIS2_PLACEMENT_3D ( 'NONE', #236868, #58213, #75263 ) ;
#80884 = ORIENTED_EDGE ( 'NONE', *, *, #189302, .T. ) ;
#80885 = EDGE_CURVE ( 'NONE', #29232, #171778, #181518, .T. ) ;
#80886 = AXIS2_PLACEMENT_3D ( 'NONE', #196376, #221068, #178128 ) ;
#80887 = DIRECTION ( 'NONE',  ( 0.000000000000000000, 0.000000000000000000, 1.000000000000000000 ) ) ;
#80888 = ORIENTED_EDGE ( 'NONE', *, *, #11560, .F. ) ;
#80889 = FACE_OUTER_BOUND ( 'NONE', #107759, .T. ) ;
#80890 = VERTEX_POINT ( 'NONE', #223179 ) ;
#80891 = CARTESIAN_POINT ( 'NONE',  ( -21.45000000000000284, 68.29142135624930177, -115.2731074845243455 ) ) ;
#80892 = ADVANCED_FACE ( 'NONE', ( #161958 ), #161704, .F. ) ;
#80893 = DIRECTION ( 'NONE',  ( -3.469446951953635015E-14, -1.000000000000000000, 0.000000000000000000 ) ) ;
#80894 = AXIS2_PLACEMENT_3D ( 'NONE', #62493, #13737, #127596 ) ;
#80895 = VERTEX_POINT ( 'NONE', #58947 ) ;
#80896 = DIRECTION ( 'NONE',  ( 0.000000000000000000, 0.000000000000000000, 1.000000000000000000 ) ) ;
#80897 = EDGE_CURVE ( 'NONE', #117463, #63493, #66692, .T. ) ;
#80898 = CIRCLE ( 'NONE', #122638, 11.65000000000000746 ) ;
#80899 = ADVANCED_FACE ( 'NONE', ( #127949 ), #95031, .T. ) ;
#80900 = CARTESIAN_POINT ( 'NONE',  ( -23.15000000000000213, 4.350000000011156054, -146.1500000000000341 ) ) ;
#80901 = AXIS2_PLACEMENT_3D ( 'NONE', #38323, #57852, #83503 ) ;
#80902 = EDGE_CURVE ( 'NONE', #68295, #193140, #11862, .T. ) ;
#80903 = ORIENTED_EDGE ( 'NONE', *, *, #194790, .F. ) ;
#80904 = AXIS2_PLACEMENT_3D ( 'NONE', #92988, #207841, #29218 ) ;
#80905 = VERTEX_POINT ( 'NONE', #186649 ) ;
#80907 = EDGE_CURVE ( 'NONE', #183616, #223717, #49689, .T. ) ;
#80906 = EDGE_CURVE ( 'NONE', #182351, #112914, #144919, .T. ) ;
#80908 = EDGE_LOOP ( 'NONE', ( #140581, #144692, #93511, #194742, #245584, #5917 ) ) ;
#80909 = DIRECTION ( 'NONE',  ( -0.000000000000000000, 0.2617529984165031243, 0.9651348961777157509 ) ) ;
#80910 = ORIENTED_EDGE ( 'NONE', *, *, #18426, .T. ) ;
#80912 = ORIENTED_EDGE ( 'NONE', *, *, #175922, .F. ) ;
#80911 = CARTESIAN_POINT ( 'NONE',  ( 15.39170923737818342, 66.61047060254585972, -185.7059995716307981 ) ) ;
#80913 = ORIENTED_EDGE ( 'NONE', *, *, #172473, .F. ) ;
#80916 = ORIENTED_EDGE ( 'NONE', *, *, #35728, .F. ) ;
#80915 = EDGE_LOOP ( 'NONE', ( #133791, #114217, #38195, #152314 ) ) ;
#80914 = DIRECTION ( 'NONE',  ( 2.952720810173289112E-16, 1.000000000000000000, 6.308085367188367561E-15 ) ) ;
#80917 = ORIENTED_EDGE ( 'NONE', *, *, #169577, .T. ) ;
#80918 = CARTESIAN_POINT ( 'NONE',  ( -18.59999999999999787, 64.35000000001150511, -48.17310748452440095 ) ) ;
#80919 = EDGE_CURVE ( 'NONE', #13549, #55661, #224208, .T. ) ;
#80920 = AXIS2_PLACEMENT_3D ( 'NONE', #257011, #156713, #78411 ) ;
#80921 = ADVANCED_FACE ( 'NONE', ( #126658 ), #32727, .T. ) ;
#80922 = LINE ( 'NONE', #155379, #226261 ) ;
#80923 = CARTESIAN_POINT ( 'NONE',  ( -23.25000000000000000, 11.65000000001115588, -45.65000000000000568 ) ) ;
#80924 = VERTEX_POINT ( 'NONE', #5395 ) ;
#80925 = EDGE_CURVE ( 'NONE', #200, #236713, #178456, .T. ) ;
#80926 = LINE ( 'NONE', #79641, #145417 ) ;
#80927 = CIRCLE ( 'NONE', #114261, 0.09999999999999854838 ) ;
#80929 = ORIENTED_EDGE ( 'NONE', *, *, #184504, .F. ) ;
#80928 = DIRECTION ( 'NONE',  ( 0.000000000000000000, 0.8814952561688436106, -0.4721928772777334027 ) ) ;
#80930 = DIRECTION ( 'NONE',  ( 0.000000000000000000, 0.9126074666063770380, 0.4088369013363281068 ) ) ;
#80932 = VERTEX_POINT ( 'NONE', #84926 ) ;
#80931 = CARTESIAN_POINT ( 'NONE',  ( 23.15000000000000213, -9.499999999988844479, -124.1060308773475924 ) ) ;
#80933 = ORIENTED_EDGE ( 'NONE', *, *, #174256, .T. ) ;
#80934 = ADVANCED_FACE ( 'NONE', ( #70572 ), #182547, .T. ) ;
#80936 = EDGE_CURVE ( 'NONE', #7289, #176897, #146210, .T. ) ;
#80935 = FACE_OUTER_BOUND ( 'NONE', #219038, .T. ) ;
#80937 = ORIENTED_EDGE ( 'NONE', *, *, #134080, .F. ) ;
#80938 = ORIENTED_EDGE ( 'NONE', *, *, #7895, .F. ) ;
#80939 = DIRECTION ( 'NONE',  ( 1.000000000000000000, -0.000000000000000000, -0.000000000000000000 ) ) ;
#80940 = DIRECTION ( 'NONE',  ( 1.000000000000000000, 0.000000000000000000, 0.000000000000000000 ) ) ;
#80942 = VERTEX_POINT ( 'NONE', #28895 ) ;
#80941 = ORIENTED_EDGE ( 'NONE', *, *, #200160, .T. ) ;
#80943 = AXIS2_PLACEMENT_3D ( 'NONE', #257836, #47489, #120978 ) ;
#80944 = EDGE_LOOP ( 'NONE', ( #106443, #57764, #100142, #199737 ) ) ;
#80945 = DIRECTION ( 'NONE',  ( 0.000000000000000000, 0.000000000000000000, 1.000000000000000000 ) ) ;
#80946 = ORIENTED_EDGE ( 'NONE', *, *, #41970, .F. ) ;
#80947 = ORIENTED_EDGE ( 'NONE', *, *, #232504, .T. ) ;
#80948 = LINE ( 'NONE', #103074, #209337 ) ;
#80949 = VERTEX_POINT ( 'NONE', #204895 ) ;
#80950 = EDGE_CURVE ( 'NONE', #183134, #87663, #86627, .T. ) ;
#80951 = DIRECTION ( 'NONE',  ( 1.000000000000000000, -0.000000000000000000, -0.000000000000000000 ) ) ;
#80953 = DIRECTION ( 'NONE',  ( 0.000000000000000000, 1.000000000000000000, 0.000000000000000000 ) ) ;
#80952 = FACE_OUTER_BOUND ( 'NONE', #49998, .T. ) ;
#80954 = EDGE_LOOP ( 'NONE', ( #220887, #60271, #158317, #202469 ) ) ;
#80956 = ORIENTED_EDGE ( 'NONE', *, *, #176246, .F. ) ;
#80955 = ORIENTED_EDGE ( 'NONE', *, *, #142423, .T. ) ;
#80957 = EDGE_CURVE ( 'NONE', #168958, #176891, #178278, .T. ) ;
#80958 = CARTESIAN_POINT ( 'NONE',  ( -23.25000000000000000, 76.00000000001239187, -162.1231074845243825 ) ) ;
#80959 = CARTESIAN_POINT ( 'NONE',  ( 20.27550659511088682, 60.75776438711819338, -224.5153016389302536 ) ) ;
#80960 = AXIS2_PLACEMENT_3D ( 'NONE', #211130, #207299, #147301 ) ;
#80961 = VERTEX_POINT ( 'NONE', #225733 ) ;
#80962 = AXIS2_PLACEMENT_3D ( 'NONE', #116756, #13806, #33410 ) ;
#80963 = AXIS2_PLACEMENT_3D ( 'NONE', #28492, #208390, #106678 ) ;
#80964 = CIRCLE ( 'NONE', #210002, 0.1999999999999987899 ) ;
#80965 = DIRECTION ( 'NONE',  ( 1.000000000000000000, 0.000000000000000000, 0.000000000000000000 ) ) ;
#80966 = ORIENTED_EDGE ( 'NONE', *, *, #20549, .F. ) ;
#80967 = EDGE_LOOP ( 'NONE', ( #67506, #183398 ) ) ;
#80968 =( GEOMETRIC_REPRESENTATION_CONTEXT ( 3 ) GLOBAL_UNCERTAINTY_ASSIGNED_CONTEXT ( ( #212038 ) ) GLOBAL_UNIT_ASSIGNED_CONTEXT ( ( #230116, #9783, #131015 ) ) REPRESENTATION_CONTEXT ( 'NONE', 'WORKASPACE' ) );
#80969 = CARTESIAN_POINT ( 'NONE',  ( -20.54999999999999716, 1.115600667400684642E-11, -46.47500000000000142 ) ) ;
#80970 = EDGE_CURVE ( 'NONE', #153127, #16840, #229618, .T. ) ;
#80971 = ORIENTED_EDGE ( 'NONE', *, *, #19807, .T. ) ;
#80972 = DIRECTION ( 'NONE',  ( 0.000000000000000000, 0.000000000000000000, -1.000000000000000000 ) ) ;
#80973 = DIRECTION ( 'NONE',  ( 0.000000000000000000, 0.9126074666063769270, 0.4088369013363283844 ) ) ;
#80974 = VERTEX_POINT ( 'NONE', #50946 ) ;
#80975 = CARTESIAN_POINT ( 'NONE',  ( 20.94999999999999929, 71.00000000001223555, -148.9283735034374843 ) ) ;
#80976 = CARTESIAN_POINT ( 'NONE',  ( -18.59999999999999787, 1.115600667400684642E-11, -134.0000000000000284 ) ) ;
#80978 = DIRECTION ( 'NONE',  ( 6.938893903907222067E-15, 1.000000000000000000, 6.982962677686266711E-15 ) ) ;
#80977 = CARTESIAN_POINT ( 'NONE',  ( 20.90000000000000213, 6.356682116888462630, 11.91686199900910381 ) ) ;
#80979 = DIRECTION ( 'NONE',  ( -1.836970198721029934E-16, -1.000000000000000000, -6.982962677686266711E-15 ) ) ;
#80980 = DIRECTION ( 'NONE',  ( -1.000000000000000000, 0.000000000000000000, 0.000000000000000000 ) ) ;
#80981 = CARTESIAN_POINT ( 'NONE',  ( -18.50000000000000000, 76.00000000001244871, -170.0231074845243597 ) ) ;
#80982 = DIRECTION ( 'NONE',  ( 0.8049926720990051576, -0.2425566999317299299, 0.5414360951997311266 ) ) ;
#80983 = DIRECTION ( 'NONE',  ( -1.000000000000000000, 0.000000000000000000, 0.000000000000000000 ) ) ;
#80984 = CARTESIAN_POINT ( 'NONE',  ( -21.14999999999999858, 11.65000000001115588, -33.60000000000000142 ) ) ;
#80985 = ORIENTED_EDGE ( 'NONE', *, *, #68522, .T. ) ;
#80986 = AXIS2_PLACEMENT_3D ( 'NONE', #34122, #135734, #53646 ) ;
#80987 = CIRCLE ( 'NONE', #247598, 11.64999999999999325 ) ;
#80989 = ORIENTED_EDGE ( 'NONE', *, *, #19899, .T. ) ;
#80988 = ORIENTED_EDGE ( 'NONE', *, *, #63785, .T. ) ;
#80990 = ORIENTED_EDGE ( 'NONE', *, *, #140611, .F. ) ;
#80991 = ORIENTED_EDGE ( 'NONE', *, *, #239245, .F. ) ;
#80992 = CARTESIAN_POINT ( 'NONE',  ( 22.39999999999999503, 12.67709964810648238, -223.3751320524553705 ) ) ;
#80993 = CYLINDRICAL_SURFACE ( 'NONE', #40462, 11.79999999999999361 ) ;
#80994 = DIRECTION ( 'NONE',  ( -1.000000000000000000, -0.000000000000000000, -0.000000000000000000 ) ) ;
#80995 = CARTESIAN_POINT ( 'NONE',  ( 21.14999999999999858, 76.00000000001169553, -76.06376443622556849 ) ) ;
#80996 = ORIENTED_EDGE ( 'NONE', *, *, #241618, .F. ) ;
#80997 = CIRCLE ( 'NONE', #114330, 12.97499999999998899 ) ;
#80998 = AXIS2_PLACEMENT_3D ( 'NONE', #118909, #215418, #77187 ) ;
#80999 = CARTESIAN_POINT ( 'NONE',  ( -20.94999999999999929, 10.29288807859936661, -105.9580020160122160 ) ) ;
#81000 = AXIS2_PLACEMENT_3D ( 'NONE', #183781, #27311, #128948 ) ;
#81001 = DIRECTION ( 'NONE',  ( 1.000000000000000000, 0.000000000000000000, 0.000000000000000000 ) ) ;
#81002 = LINE ( 'NONE', #19784, #247200 ) ;
#81003 = CARTESIAN_POINT ( 'NONE',  ( -16.89268316805465986, 9.951721813253337601, -87.85575247854558256 ) ) ;
#81005 = VERTEX_POINT ( 'NONE', #31449 ) ;
#81004 = AXIS2_PLACEMENT_3D ( 'NONE', #128046, #129323, #107180 ) ;
#81006 = B_SPLINE_CURVE_WITH_KNOTS ( 'NONE', 3,
 ( #88331, #150905, #190037, #13975 ),
 .UNSPECIFIED., .F., .F.,
 ( 4, 4 ),
 ( 0.000000000000000000, 7.713889350930496175E-05 ),
 .UNSPECIFIED. ) ;
#81007 = CARTESIAN_POINT ( 'NONE',  ( -21.05000000000000071, 76.00000000001188027, -98.92310748452429436 ) ) ;
#81008 = AXIS2_PLACEMENT_3D ( 'NONE', #2314, #84378, #205651 ) ;
#81009 = DIRECTION ( 'NONE',  ( 0.000000000000000000, 0.9908441862701605762, -0.1350103645451835310 ) ) ;
#81010 = ORIENTED_EDGE ( 'NONE', *, *, #9939, .F. ) ;
#81011 = FACE_OUTER_BOUND ( 'NONE', #105696, .T. ) ;
#81012 = CARTESIAN_POINT ( 'NONE',  ( -23.49999999999994316, 87.50449464844290048, -34.18759587077607165 ) ) ;
#81013 = CIRCLE ( 'NONE', #10321, 0.1000000000000091788 ) ;
#81014 = DIRECTION ( 'NONE',  ( 1.000000000000000000, -0.000000000000000000, -0.000000000000000000 ) ) ;
#81016 = ORIENTED_EDGE ( 'NONE', *, *, #125325, .F. ) ;
#81015 = AXIS2_PLACEMENT_3D ( 'NONE', #91125, #111987, #191543 ) ;
#81017 = CARTESIAN_POINT ( 'NONE',  ( -20.64999999999999858, -8.730841121495325652, -23.90192528101566793 ) ) ;
#81018 = CARTESIAN_POINT ( 'NONE',  ( 23.15000000000000213, -12.41227409413852811, -64.00000000000000000 ) ) ;
#81019 = DIRECTION ( 'NONE',  ( 0.000000000000000000, 0.000000000000000000, -1.000000000000000000 ) ) ;
#81021 = LINE ( 'NONE', #199731, #82971 ) ;
#81020 = DIRECTION ( 'NONE',  ( 1.000000000000000000, 0.000000000000000000, 0.000000000000000000 ) ) ;
#81023 = ADVANCED_FACE ( 'NONE', ( #110948 ), #244027, .F. ) ;
#81022 = CARTESIAN_POINT ( 'NONE',  ( -20.94999999999999929, 7.021664781911246322, -70.83356540189728889 ) ) ;
#81024 = DIRECTION ( 'NONE',  ( 1.000000000000000000, -0.000000000000000000, -0.000000000000000000 ) ) ;
#81025 = FACE_OUTER_BOUND ( 'NONE', #108968, .T. ) ;
#81027 = ORIENTED_EDGE ( 'NONE', *, *, #13846, .T. ) ;
#81026 = DIRECTION ( 'NONE',  ( 0.000000000000000000, 0.2617529984165031243, 0.9651348961777157509 ) ) ;
#81028 = ORIENTED_EDGE ( 'NONE', *, *, #37037, .F. ) ;
#81029 = ORIENTED_EDGE ( 'NONE', *, *, #134385, .T. ) ;
#81030 = EDGE_CURVE ( 'NONE', #140838, #116413, #45836, .T. ) ;
#81031 = DIRECTION ( 'NONE',  ( 2.952720810173289112E-16, 1.000000000000000000, 6.982962677686266711E-15 ) ) ;
#81032 = EDGE_CURVE ( 'NONE', #201937, #56611, #141032, .T. ) ;
#81033 = CIRCLE ( 'NONE', #31217, 0.1000000000000028644 ) ;
#81034 = CIRCLE ( 'NONE', #205955, 0.1000000000000028644 ) ;
#81035 = DIRECTION ( 'NONE',  ( 6.938893903907222856E-15, -0.4721928772777343464, -0.8814952561688431665 ) ) ;
#81036 = AXIS2_PLACEMENT_3D ( 'NONE', #81177, #160772, #180304 ) ;
#81037 = CARTESIAN_POINT ( 'NONE',  ( -21.44999999999999929, 68.85000000001151932, -48.27310748452437394 ) ) ;
#81038 = EDGE_CURVE ( 'NONE', #257964, #128012, #182740, .T. ) ;
#81039 = ORIENTED_EDGE ( 'NONE', *, *, #219474, .F. ) ;
#81040 = CYLINDRICAL_SURFACE ( 'NONE', #142866, 0.1000000000000028644 ) ;
#81041 = LINE ( 'NONE', #160635, #232586 ) ;
#81042 = LINE ( 'NONE', #2794, #52777 ) ;
#81043 = EDGE_CURVE ( 'NONE', #249207, #239900, #75692, .T. ) ;
#81044 = CIRCLE ( 'NONE', #47916, 0.1000000000000053346 ) ;
#81045 = EDGE_CURVE ( 'NONE', #10935, #191177, #61911, .T. ) ;
#81046 = CARTESIAN_POINT ( 'NONE',  ( -20.94999999999999929, 68.92903212821255465, -32.27654326265606954 ) ) ;
#81048 = ORIENTED_EDGE ( 'NONE', *, *, #226216, .F. ) ;
#81047 = DIRECTION ( 'NONE',  ( -0.000000000000000000, -0.8814952561688430555, 0.4721928772777346239 ) ) ;
#81050 = CARTESIAN_POINT ( 'NONE',  ( 20.94999999999999929, 43.08177281680065818, -239.3869926993485535 ) ) ;
#81049 = CYLINDRICAL_SURFACE ( 'NONE', #29948, 12.87500000000000178 ) ;
#81051 = DIRECTION ( 'NONE',  ( 0.000000000000000000, 0.000000000000000000, -1.000000000000000000 ) ) ;
#81052 = EDGE_CURVE ( 'NONE', #210192, #120740, #19744, .T. ) ;
#81053 = SURFACE_SIDE_STYLE ('',( #198454 ) ) ;
#81054 = ORIENTED_EDGE ( 'NONE', *, *, #170316, .F. ) ;
#81055 = AXIS2_PLACEMENT_3D ( 'NONE', #58199, #102443, #60773 ) ;
#81056 = CARTESIAN_POINT ( 'NONE',  ( 0.000000000000000000, 0.000000000000000000, 0.000000000000000000 ) ) ;
#81057 = CARTESIAN_POINT ( 'NONE',  ( -23.25000000000000355, 42.79061499530347845, -240.6131891775583824 ) ) ;
#81058 = AXIS2_PLACEMENT_3D ( 'NONE', #130531, #232230, #107118 ) ;
#81059 = DIRECTION ( 'NONE',  ( 0.000000000000000000, -0.7035695228903323661, -0.7106264324241465813 ) ) ;
#81060 = ADVANCED_FACE ( 'NONE', ( #233487 ), #57371, .F. ) ;
#81061 = CIRCLE ( 'NONE', #1950, 11.70000000000000284 ) ;
#81062 = ORIENTED_EDGE ( 'NONE', *, *, #54655, .T. ) ;
#81063 = CARTESIAN_POINT ( 'NONE',  ( -20.85000000000000142, 76.00000000001213607, -136.5231074845243313 ) ) ;
#81064 = DIRECTION ( 'NONE',  ( 0.000000000000000000, 0.000000000000000000, -1.000000000000000000 ) ) ;
#81065 = ORIENTED_EDGE ( 'NONE', *, *, #172699, .F. ) ;
#81066 = CARTESIAN_POINT ( 'NONE',  ( -18.50000000000000000, 1.162701749949165642, -108.6000000000000227 ) ) ;
#81067 = EDGE_CURVE ( 'NONE', #199384, #248274, #91393, .T. ) ;
#81068 = LINE ( 'NONE', #41983, #36822 ) ;
#81069 = DIRECTION ( 'NONE',  ( 1.000000000000000000, 0.000000000000000000, 0.000000000000000000 ) ) ;
#81070 = EDGE_LOOP ( 'NONE', ( #252555, #229628, #250163, #24078 ) ) ;
#81071 = ADVANCED_FACE ( 'NONE', ( #194367 ), #199280, .F. ) ;
#81072 = AXIS2_PLACEMENT_3D ( 'NONE', #16031, #56393, #159380 ) ;
#81073 = VERTEX_POINT ( 'NONE', #95233 ) ;
#81074 = ADVANCED_FACE ( 'NONE', ( #71842 ), #236025, .T. ) ;
#81075 = DIRECTION ( 'NONE',  ( 0.000000000000000000, 6.982962677686267499E-15, -1.000000000000000000 ) ) ;
#81077 = CIRCLE ( 'NONE', #80492, 11.79999999999999005 ) ;
#81076 = LINE ( 'NONE', #77229, #115138 ) ;
#81078 = CARTESIAN_POINT ( 'NONE',  ( 21.11701782572533048, 13.08179283168479579, -210.6830026332638681 ) ) ;
#81079 = CARTESIAN_POINT ( 'NONE',  ( -18.60000000000000853, -9.364240527579752893, -141.1802485818407717 ) ) ;
#81081 = DIRECTION ( 'NONE',  ( 3.265361837132813093E-16, 0.9651348961777157509, -0.2617529984165031243 ) ) ;
#81080 = CARTESIAN_POINT ( 'NONE',  ( -21.53699400384082807, 75.99999999999387512, -143.3108192777702072 ) ) ;
#81082 = CARTESIAN_POINT ( 'NONE',  ( -18.34374000495060386, 58.57934086597919077, -223.9244941873113817 ) ) ;
#81083 = DIRECTION ( 'NONE',  ( 0.000000000000000000, 0.000000000000000000, 1.000000000000000000 ) ) ;
#81084 = CARTESIAN_POINT ( 'NONE',  ( 18.50000000000000000, -9.419078080838367839, -107.3299253502083559 ) ) ;
#81085 = TOROIDAL_SURFACE ( 'NONE', #106021, 0.9750000000000019762, 0.1000000000000000056 ) ;
#81086 = VERTEX_POINT ( 'NONE', #113516 ) ;
#81087 = DIRECTION ( 'NONE',  ( -1.000000000000000000, 0.000000000000000000, 0.000000000000000000 ) ) ;
#81088 = AXIS2_PLACEMENT_3D ( 'NONE', #81888, #203154, #162767 ) ;
#81090 = ORIENTED_EDGE ( 'NONE', *, *, #229317, .T. ) ;
#81089 = DIRECTION ( 'NONE',  ( 0.000000000000000000, 0.000000000000000000, 1.000000000000000000 ) ) ;
#81091 = AXIS2_PLACEMENT_3D ( 'NONE', #210704, #8655, #28252 ) ;
#81092 = CARTESIAN_POINT ( 'NONE',  ( 21.05000000000000071, 69.09936979046463534, -247.6075824278584889 ) ) ;
#81093 = CARTESIAN_POINT ( 'NONE',  ( -22.39999999999999858, 33.38250548509083160, -242.4821227592188961 ) ) ;
#81095 = CARTESIAN_POINT ( 'NONE',  ( -23.49999999999994316, 74.16448838626247664, -47.52760213295649550 ) ) ;
#81094 = DIRECTION ( 'NONE',  ( 0.000000000000000000, -0.4088369013363276072, 0.9126074666063772600 ) ) ;
#81096 = ADVANCED_FACE ( 'NONE', ( #32738 ), #24507, .T. ) ;
#81097 = ORIENTED_EDGE ( 'NONE', *, *, #112206, .T. ) ;
#81099 = CARTESIAN_POINT ( 'NONE',  ( -20.94999999999999929, 1.162701749949165642, -108.6000000000000227 ) ) ;
#81098 = CARTESIAN_POINT ( 'NONE',  ( -16.87998658237755123, 66.05000000001159322, -56.65946791678611305 ) ) ;
#81100 = CARTESIAN_POINT ( 'NONE',  ( -18.50000000000000000, 66.75000000001179501, -81.87310748452438247 ) ) ;
#81101 = DIRECTION ( 'NONE',  ( 1.000000000000000000, 0.000000000000000000, 1.073024830501117725E-15 ) ) ;
#81102 = DIRECTION ( 'NONE',  ( -0.000000000000000000, 1.000000000000000000, 0.000000000000000000 ) ) ;
#81103 = CARTESIAN_POINT ( 'NONE',  ( -14.45422546970482713, 66.54939790392400312, -185.0792115214277089 ) ) ;
#81104 = VERTEX_POINT ( 'NONE', #172254 ) ;
#81105 = CARTESIAN_POINT ( 'NONE',  ( 18.39999999999999503, 64.25000000001182343, -82.17310748452439384 ) ) ;
#81106 = ORIENTED_EDGE ( 'NONE', *, *, #257321, .F. ) ;
#81107 = CARTESIAN_POINT ( 'NONE',  ( -16.78805706634180339, 9.948252493082335945, -54.34415320803185523 ) ) ;
#81108 = ORIENTED_EDGE ( 'NONE', *, *, #24643, .F. ) ;
#81110 = DIRECTION ( 'NONE',  ( 1.224646799147353700E-16, 0.4721928772777346239, 0.8814952561688430555 ) ) ;
#81109 = B_SPLINE_CURVE_WITH_KNOTS ( 'NONE', 3,
 ( #100618, #240183, #201041, #22432, #101910, #241460, #88774, #170959, #10560, #148786 ),
 .UNSPECIFIED., .F., .F.,
 ( 4, 3, 3, 4 ),
 ( 0.000000000000000000, 0.0002000000000008537104, 0.001000000000082977483, 0.001967863649483339323 ),
 .UNSPECIFIED. ) ;
#81111 = CIRCLE ( 'NONE', #226864, 12.87499999999999822 ) ;
#81112 = VERTEX_POINT ( 'NONE', #52237 ) ;
#81113 = EDGE_CURVE ( 'NONE', #90327, #105545, #82716, .T. ) ;
#81114 = FACE_OUTER_BOUND ( 'NONE', #245372, .T. ) ;
#81115 = CIRCLE ( 'NONE', #72794, 0.1000000000000026007 ) ;
#81116 = LINE ( 'NONE', #121585, #138724 ) ;
#81117 = VERTEX_POINT ( 'NONE', #215182 ) ;
#81118 = EDGE_CURVE ( 'NONE', #160208, #21528, #107687, .T. ) ;
#81119 = DIRECTION ( 'NONE',  ( -1.000000000000000000, -0.000000000000000000, -0.000000000000000000 ) ) ;
#81120 = PLANE ( 'NONE',  #50889 ) ;
#81121 = DIRECTION ( 'NONE',  ( -1.000000000000000000, -0.000000000000000000, -0.000000000000000000 ) ) ;
#81122 = EDGE_CURVE ( 'NONE', #162715, #43706, #157813, .T. ) ;
#81123 = EDGE_CURVE ( 'NONE', #84546, #172317, #45330, .T. ) ;
#81124 = CARTESIAN_POINT ( 'NONE',  ( 23.24999999999999645, 8.111588099649802430, -211.9294447938511325 ) ) ;
#81125 = CARTESIAN_POINT ( 'NONE',  ( 18.39999999999999503, 11.47316190337363828, -54.35000000000000142 ) ) ;
#81126 = CARTESIAN_POINT ( 'NONE',  ( 19.75857864376269291, 62.39550153362034024, -208.7959266050682459 ) ) ;
#81127 = EDGE_CURVE ( 'NONE', #17682, #8134, #216457, .T. ) ;
#81128 = ORIENTED_EDGE ( 'NONE', *, *, #106119, .T. ) ;
#81130 = EDGE_CURVE ( 'NONE', #122630, #53814, #178646, .T. ) ;
#81129 = DIRECTION ( 'NONE',  ( -0.000000000000000000, -0.000000000000000000, 1.000000000000000000 ) ) ;
#81131 = ORIENTED_EDGE ( 'NONE', *, *, #133779, .F. ) ;
#81133 = EDGE_LOOP ( 'NONE', ( #156375, #184949, #161787, #92227, #192678, #16417, #77746, #95965, #139196, #222645, #69327, #131033, #142498, #9588 ) ) ;
#81132 = DIRECTION ( 'NONE',  ( 1.000000000000000000, 0.000000000000000000, 0.000000000000000000 ) ) ;
#81134 = CIRCLE ( 'NONE', #143686, 0.09999999999998898659 ) ;
#81135 = ORIENTED_EDGE ( 'NONE', *, *, #212258, .T. ) ;
#81136 = VECTOR ( 'NONE', #76892, 1000.000000000000000 ) ;
#81137 = DIRECTION ( 'NONE',  ( -1.000000000000000000, 1.207181226542539946E-16, -2.694675058168174692E-16 ) ) ;
#81138 = CARTESIAN_POINT ( 'NONE',  ( -21.55000000000000426, 68.29142135624930177, -115.2731074845243455 ) ) ;
#81139 = DIRECTION ( 'NONE',  ( 1.000000000000000000, 0.000000000000000000, 0.000000000000000000 ) ) ;
#81140 = ADVANCED_FACE ( 'NONE', ( #221574 ), #95222, .F. ) ;
#81141 = CARTESIAN_POINT ( 'NONE',  ( -21.37071067811865532, 8.070710678129811910, -155.2500000000000284 ) ) ;
#81142 = ORIENTED_EDGE ( 'NONE', *, *, #221326, .T. ) ;
#81143 = DIRECTION ( 'NONE',  ( 1.186688945009010077E-16, 0.4088369013363281623, -0.9126074666063771490 ) ) ;
#81144 = CARTESIAN_POINT ( 'NONE',  ( -16.77683809663752257, 66.05416425680813575, -157.3591584654202222 ) ) ;
#81145 = ORIENTED_EDGE ( 'NONE', *, *, #178541, .T. ) ;
#81146 = CARTESIAN_POINT ( 'NONE',  ( 23.24999999999999289, 23.34004772283015683, -229.2004250369967338 ) ) ;
#81148 = VECTOR ( 'NONE', #113003, 1000.000000000000000 ) ;
#81147 = CARTESIAN_POINT ( 'NONE',  ( -16.83233564386401682, 9.930221796595741779, -79.77547933652442680 ) ) ;
#81149 = VERTEX_POINT ( 'NONE', #119967 ) ;
#81151 = DIRECTION ( 'NONE',  ( 1.000000000000000000, 6.779962435680481854E-15, 1.476603528521582099E-15 ) ) ;
#81150 = AXIS2_PLACEMENT_3D ( 'NONE', #169734, #131847, #28952 ) ;
#81152 = VECTOR ( 'NONE', #110324, 1000.000000000000000 ) ;
#81153 = ADVANCED_FACE ( 'NONE', ( #40435 ), #138188, .F. ) ;
#81154 = CARTESIAN_POINT ( 'NONE',  ( -20.94999999999999929, 77.84915357198738661, -24.41714086472725853 ) ) ;
#81155 = ORIENTED_EDGE ( 'NONE', *, *, #141451, .F. ) ;
#81156 = CARTESIAN_POINT ( 'NONE',  ( -18.39999999999999858, 11.47316190337362762, -176.8259460668079441 ) ) ;
#81157 =( GEOMETRIC_REPRESENTATION_CONTEXT ( 3 ) GLOBAL_UNCERTAINTY_ASSIGNED_CONTEXT ( ( #154644 ) ) GLOBAL_UNIT_ASSIGNED_CONTEXT ( ( #152890, #250651, #72044 ) ) REPRESENTATION_CONTEXT ( 'NONE', 'WORKASPACE' ) );
#81158 = EDGE_CURVE ( 'NONE', #139324, #88642, #165986, .T. ) ;
#81159 = DIRECTION ( 'NONE',  ( 1.000000000000000000, 0.000000000000000000, 0.000000000000000000 ) ) ;
#81160 = DIRECTION ( 'NONE',  ( 0.000000000000000000, 1.000000000000000000, 0.000000000000000000 ) ) ;
#81161 = EDGE_CURVE ( 'NONE', #56214, #3667, #22139, .T. ) ;
#81162 = DIRECTION ( 'NONE',  ( 0.000000000000000000, -1.000000000000000000, 0.000000000000000000 ) ) ;
#81163 = CARTESIAN_POINT ( 'NONE',  ( -23.25000000000000000, 1.115600667400684642E-11, -67.00000000000000000 ) ) ;
#81164 = VECTOR ( 'NONE', #26084, 1000.000000000000000 ) ;
#81165 = ORIENTED_EDGE ( 'NONE', *, *, #207633, .T. ) ;
#81166 = PRESENTATION_STYLE_ASSIGNMENT (( #100712 ) ) ;
#81167 = AXIS2_PLACEMENT_3D ( 'NONE', #201527, #98529, #178142 ) ;
#81168 = AXIS2_PLACEMENT_3D ( 'NONE', #87207, #226728, #10274 ) ;
#81169 = ORIENTED_EDGE ( 'NONE', *, *, #24392, .F. ) ;
#81170 = DIRECTION ( 'NONE',  ( 0.000000000000000000, -7.109473446599835262E-15, 1.000000000000000000 ) ) ;
#81171 = CARTESIAN_POINT ( 'NONE',  ( -20.94999999999999929, 43.86852340793510763, -246.3213511806884810 ) ) ;
#81173 = VERTEX_POINT ( 'NONE', #181210 ) ;
#81172 = DIRECTION ( 'NONE',  ( 0.000000000000000000, 1.000000000000000000, 0.000000000000000000 ) ) ;
#81174 = CARTESIAN_POINT ( 'NONE',  ( -18.47690164073605956, 85.46484453802433734, -129.8217265446881754 ) ) ;
#81175 = CARTESIAN_POINT ( 'NONE',  ( 18.39999999999999858, 85.40000000001246860, -181.7731074845243029 ) ) ;
#81176 = CARTESIAN_POINT ( 'NONE',  ( 21.08479644141222664, 75.94144555744786373, -109.3681461422561938 ) ) ;
#81177 = CARTESIAN_POINT ( 'NONE',  ( -18.79999999999999716, -8.250000000000005329, 22.10000000000000142 ) ) ;
#81178 = CIRCLE ( 'NONE', #10299, 0.09999999999999939493 ) ;
#81179 = SPHERICAL_SURFACE ( 'NONE', #30905, 0.1000000000000000056 ) ;
#81180 = AXIS2_PLACEMENT_3D ( 'NONE', #216160, #218719, #58352 ) ;
#81181 = CARTESIAN_POINT ( 'NONE',  ( -23.39999999999994529, 87.51781941433023349, -34.28670414799875488 ) ) ;
#81183 = EDGE_LOOP ( 'NONE', ( #144456, #152037, #57275, #74273 ) ) ;
#81182 = CARTESIAN_POINT ( 'NONE',  ( 21.30000000000002558, 10.69888912757691024, -235.6450824654141059 ) ) ;
#81184 = AXIS2_PLACEMENT_3D ( 'NONE', #12255, #48782, #111338 ) ;
#81185 = DIRECTION ( 'NONE',  ( -1.836970198721029934E-16, 1.000000000000000000, 0.000000000000000000 ) ) ;
#81186 = AXIS2_PLACEMENT_3D ( 'NONE', #13892, #12625, #49156 ) ;
#81187 = VERTEX_POINT ( 'NONE', #102912 ) ;
#81188 = ORIENTED_EDGE ( 'NONE', *, *, #245725, .T. ) ;
#81189 = AXIS2_PLACEMENT_3D ( 'NONE', #227682, #114161, #228985 ) ;
#81190 = DIRECTION ( 'NONE',  ( 0.000000000000000000, -0.3738317757009658182, 0.9274965247785366129 ) ) ;
#81191 = CARTESIAN_POINT ( 'NONE',  ( -18.50000000000000355, 85.40000000001262492, -196.2258477248610120 ) ) ;
#81192 = AXIS2_PLACEMENT_3D ( 'NONE', #193199, #15860, #118790 ) ;
#81194 = EDGE_LOOP ( 'NONE', ( #195234, #113934, #50712, #254624 ) ) ;
#81193 = AXIS2_PLACEMENT_3D ( 'NONE', #113257, #257843, #177111 ) ;
#81195 = EDGE_CURVE ( 'NONE', #103678, #123954, #153536, .T. ) ;
#81196 = EDGE_CURVE ( 'NONE', #100484, #25217, #161893, .T. ) ;
#81197 = ORIENTED_EDGE ( 'NONE', *, *, #44584, .F. ) ;
#81198 = CARTESIAN_POINT ( 'NONE',  ( -21.14999999999999858, -2.576749817950531707, -189.6385361693310756 ) ) ;
#81199 = CARTESIAN_POINT ( 'NONE',  ( -16.94037747912386394, 65.98646061752627645, -190.9719765265489286 ) ) ;
#81200 = EDGE_CURVE ( 'NONE', #131341, #133509, #220331, .T. ) ;
#81201 = ORIENTED_EDGE ( 'NONE', *, *, #244399, .F. ) ;
#81202 = ORIENTED_EDGE ( 'NONE', *, *, #149184, .T. ) ;
#81204 = EDGE_CURVE ( 'NONE', #150814, #77481, #213497, .T. ) ;
#81203 = CARTESIAN_POINT ( 'NONE',  ( 21.00000000000000000, 9.750000000011153745, -45.85000000000000142 ) ) ;
#81205 = ORIENTED_EDGE ( 'NONE', *, *, #155746, .F. ) ;
#81206 = DIRECTION ( 'NONE',  ( 0.000000000000000000, -0.1455152366551721865, -0.9893560106964475187 ) ) ;
#81207 = ORIENTED_EDGE ( 'NONE', *, *, #143859, .F. ) ;
#81209 = ORIENTED_EDGE ( 'NONE', *, *, #167727, .T. ) ;
#81208 = DIRECTION ( 'NONE',  ( 1.186688945009009584E-16, -0.4721928772777346239, -0.8814952561688430555 ) ) ;
#81210 = VERTEX_POINT ( 'NONE', #241182 ) ;
#81211 = CIRCLE ( 'NONE', #168782, 0.09999999999999939493 ) ;
#81212 = CARTESIAN_POINT ( 'NONE',  ( -23.15000000000000213, 76.00000000001213607, -136.5231074845242745 ) ) ;
#81213 = ORIENTED_EDGE ( 'NONE', *, *, #118738, .T. ) ;
#81214 = AXIS2_PLACEMENT_3D ( 'NONE', #255309, #59705, #235792 ) ;
#81216 = ORIENTED_EDGE ( 'NONE', *, *, #154756, .T. ) ;
#81215 = ORIENTED_EDGE ( 'NONE', *, *, #206222, .F. ) ;
#81217 = DIRECTION ( 'NONE',  ( 1.000000000000000000, 0.000000000000000000, 0.000000000000000000 ) ) ;
#81218 = AXIS2_PLACEMENT_3D ( 'NONE', #214941, #235780, #173305 ) ;
#81219 = CYLINDRICAL_SURFACE ( 'NONE', #160754, 0.09999999999998898659 ) ;
#81220 = ORIENTED_EDGE ( 'NONE', *, *, #225698, .F. ) ;
#81221 = EDGE_CURVE ( 'NONE', #138366, #62457, #191836, .T. ) ;
#81222 = EDGE_CURVE ( 'NONE', #163761, #159106, #195208, .T. ) ;
#81223 = AXIS2_PLACEMENT_3D ( 'NONE', #81198, #141203, #220733 ) ;
#81224 = TOROIDAL_SURFACE ( 'NONE', #135405, 0.2000000000000000111, 0.1000000000000000056 ) ;
#81225 = EDGE_LOOP ( 'NONE', ( #13029, #136282, #155353, #92607 ) ) ;
#81226 = CARTESIAN_POINT ( 'NONE',  ( -16.97683809663752186, 9.850000000011137402, -46.90236401819648648 ) ) ;
#81227 = LINE ( 'NONE', #160819, #143043 ) ;
#81229 = VERTEX_POINT ( 'NONE', #63816 ) ;
#81228 = DIRECTION ( 'NONE',  ( 1.000000000000000000, 0.000000000000000000, 0.000000000000000000 ) ) ;
#81230 = DIRECTION ( 'NONE',  ( 1.000000000000000000, 0.000000000000000000, 0.000000000000000000 ) ) ;
#81231 = ORIENTED_EDGE ( 'NONE', *, *, #185438, .F. ) ;
#81232 = LINE ( 'NONE', #177818, #24526 ) ;
#81233 = DIRECTION ( 'NONE',  ( 1.000000000000000000, -0.000000000000000000, 0.000000000000000000 ) ) ;
#81234 = AXIS2_PLACEMENT_3D ( 'NONE', #74656, #154197, #51161 ) ;
#81235 = ORIENTED_EDGE ( 'NONE', *, *, #44478, .T. ) ;
#81236 = CARTESIAN_POINT ( 'NONE',  ( -21.55000000000000071, 11.68239342655420110, -220.1014838121945161 ) ) ;
#81238 = EDGE_CURVE ( 'NONE', #110098, #146658, #191108, .T. ) ;
#81237 = DIRECTION ( 'NONE',  ( 0.000000000000000000, 0.000000000000000000, -1.000000000000000000 ) ) ;
#81239 = SPHERICAL_SURFACE ( 'NONE', #28349, 0.1000000000000000056 ) ;
#81240 = AXIS2_PLACEMENT_3D ( 'NONE', #32526, #247683, #169473 ) ;
#81241 = ORIENTED_EDGE ( 'NONE', *, *, #137390, .F. ) ;
#81242 = EDGE_CURVE ( 'NONE', #156141, #234175, #222875, .T. ) ;
#81243 = DIRECTION ( 'NONE',  ( 0.000000000000000000, 0.000000000000000000, -1.000000000000000000 ) ) ;
#81244 = ORIENTED_EDGE ( 'NONE', *, *, #151493, .F. ) ;
#81245 = VERTEX_POINT ( 'NONE', #97768 ) ;
#81246 = AXIS2_PLACEMENT_3D ( 'NONE', #158823, #21858, #41438 ) ;
#81247 = EDGE_LOOP ( 'NONE', ( #244666, #166759, #47969, #6489 ) ) ;
#81248 = ORIENTED_EDGE ( 'NONE', *, *, #147144, .F. ) ;
#81249 = DIRECTION ( 'NONE',  ( 1.000000000000000000, 0.000000000000000000, 0.000000000000000000 ) ) ;
#81250 = EDGE_LOOP ( 'NONE', ( #197438, #214361, #53055, #102344 ) ) ;
#81251 = CIRCLE ( 'NONE', #156325, 7.900000000000003908 ) ;
#81252 = ORIENTED_EDGE ( 'NONE', *, *, #159300, .T. ) ;
#81253 = EDGE_CURVE ( 'NONE', #86372, #27420, #177378, .T. ) ;
#81254 = LINE ( 'NONE', #57842, #185445 ) ;
#81255 = CARTESIAN_POINT ( 'NONE',  ( -21.05000000000000071, 74.14897176987101091, -91.36919421510182815 ) ) ;
#81256 = ORIENTED_EDGE ( 'NONE', *, *, #136335, .T. ) ;
#81257 = EDGE_LOOP ( 'NONE', ( #217785, #234641, #118639, #27196 ) ) ;
#81258 = EDGE_CURVE ( 'NONE', #195498, #96705, #246304, .T. ) ;
#81259 = VERTEX_POINT ( 'NONE', #145901 ) ;
#81260 = AXIS2_PLACEMENT_3D ( 'NONE', #224954, #120772, #46325 ) ;
#81261 = AXIS2_PLACEMENT_3D ( 'NONE', #136275, #138831, #114170 ) ;
#81262 = DIRECTION ( 'NONE',  ( 0.000000000000000000, 0.000000000000000000, 1.000000000000000000 ) ) ;
#81263 = DIRECTION ( 'NONE',  ( 1.000000000000000000, 0.000000000000000000, 0.000000000000000000 ) ) ;
#81264 = EDGE_CURVE ( 'NONE', #202859, #119125, #120256, .T. ) ;
#81265 = DIRECTION ( 'NONE',  ( 0.000000000000000000, 0.9908441862701596881, -0.1350103645451904977 ) ) ;
#81266 = DIRECTION ( 'NONE',  ( 0.000000000000000000, -1.000000000000000000, -6.352154140967427193E-15 ) ) ;
#81267 = CARTESIAN_POINT ( 'NONE',  ( 21.05000000000000426, 0.03486800302426367598, -127.7299141363108816 ) ) ;
#81268 = LINE ( 'NONE', #219510, #48115 ) ;
#81269 = ADVANCED_FACE ( 'NONE', ( #25980 ), #66178, .T. ) ;
#81271 = CARTESIAN_POINT ( 'NONE',  ( 21.05000000000000071, 34.01125473725045367, -243.8802146427659352 ) ) ;
#81270 = CARTESIAN_POINT ( 'NONE',  ( -20.94999999999994600, 67.65000000001118963, -25.49719488170504533 ) ) ;
#81272 = CARTESIAN_POINT ( 'NONE',  ( -21.07928932188134041, 75.90110485435729970, -75.85162414091762173 ) ) ;
#81273 = CYLINDRICAL_SURFACE ( 'NONE', #256874, 0.5000000000000007772 ) ;
#81274 = PLANE ( 'NONE',  #226842 ) ;
#81275 = CARTESIAN_POINT ( 'NONE',  ( 18.59999999999999432, 74.83729825007431202, -161.9231074845243654 ) ) ;
#81276 = VECTOR ( 'NONE', #492, 1000.000000000000000 ) ;
#81277 = ORIENTED_EDGE ( 'NONE', *, *, #175227, .T. ) ;
#81278 = AXIS2_PLACEMENT_3D ( 'NONE', #108073, #7696, #28585 ) ;
#81280 = VERTEX_POINT ( 'NONE', #46797 ) ;
#81279 = FACE_OUTER_BOUND ( 'NONE', #77240, .T. ) ;
#81281 = DIRECTION ( 'NONE',  ( -1.000000000000000000, -0.000000000000000000, -0.000000000000000000 ) ) ;
#81282 = CARTESIAN_POINT ( 'NONE',  ( 20.27550659511089037, 51.91893134239706598, -232.6162829946506179 ) ) ;
#81283 = CARTESIAN_POINT ( 'NONE',  ( -22.42253884134832020, 64.18009035189511735, -247.0980616929964242 ) ) ;
#81284 = EDGE_LOOP ( 'NONE', ( #194373, #133005, #180703, #124345 ) ) ;
#81285 = DIRECTION ( 'NONE',  ( 0.000000000000000000, 0.9999631594459053030, 0.008583690987162899758 ) ) ;
#81286 = CARTESIAN_POINT ( 'NONE',  ( 21.05000000000000426, 65.59652053147743800, -241.9470453418952900 ) ) ;
#81287 = VERTEX_POINT ( 'NONE', #126347 ) ;
#81289 = DIRECTION ( 'NONE',  ( 0.000000000000000000, 6.982962677686266711E-15, -1.000000000000000000 ) ) ;
#81288 = VECTOR ( 'NONE', #97247, 1000.000000000000000 ) ;
#81290 = AXIS2_PLACEMENT_3D ( 'NONE', #87154, #165439, #102856 ) ;
#81291 = DIRECTION ( 'NONE',  ( -1.000000000000000000, 0.000000000000000000, 0.000000000000000000 ) ) ;
#81292 = CARTESIAN_POINT ( 'NONE',  ( 20.10000000000000853, 5.552655413246003313, 16.61686199900910310 ) ) ;
#81293 = DIRECTION ( 'NONE',  ( 0.000000000000000000, -6.982962677686266711E-15, 1.000000000000000000 ) ) ;
#81295 = VERTEX_POINT ( 'NONE', #149794 ) ;
#81294 = CARTESIAN_POINT ( 'NONE',  ( -20.93975676684922504, 67.49344847133114911, -195.4961807846321733 ) ) ;
#81297 = EDGE_LOOP ( 'NONE', ( #80412, #65904 ) ) ;
#81296 = DIRECTION ( 'NONE',  ( -1.000000000000000000, -0.000000000000000000, -0.000000000000000000 ) ) ;
#81298 = CARTESIAN_POINT ( 'NONE',  ( -21.45000000000000284, 65.35370752038342346, -213.3282663891675952 ) ) ;
#81299 = DIRECTION ( 'NONE',  ( 0.000000000000000000, -1.000000000000000000, -6.982962677686266711E-15 ) ) ;
#81300 = DIRECTION ( 'NONE',  ( 0.000000000000000000, 0.000000000000000000, 1.000000000000000000 ) ) ;
#81301 = CARTESIAN_POINT ( 'NONE',  ( -23.25000000000000000, 55.39363411790988323, -234.6384634766556303 ) ) ;
#81303 = LINE ( 'NONE', #164736, #132734 ) ;
#81302 = DIRECTION ( 'NONE',  ( 0.000000000000000000, 1.000000000000000000, -6.308085367188393199E-16 ) ) ;
#81305 = EDGE_CURVE ( 'NONE', #201469, #62456, #24718, .T. ) ;
#81304 = DIRECTION ( 'NONE',  ( 0.000000000000000000, 0.2128009952263603677, -0.9770955615653313941 ) ) ;
#81306 = CARTESIAN_POINT ( 'NONE',  ( 20.95159278453404283, 40.76026667850895535, -237.9528832822917082 ) ) ;
#81307 = AXIS2_PLACEMENT_3D ( 'NONE', #138329, #38002, #58793 ) ;
#81308 = CARTESIAN_POINT ( 'NONE',  ( 20.94999999999999929, 87.29603075034691528, -66.47520832486038955 ) ) ;
#81309 = DIRECTION ( 'NONE',  ( 0.000000000000000000, -0.1335171055202901691, -0.9910465087640861759 ) ) ;
#81310 = CIRCLE ( 'NONE', #35415, 0.09999999999998898659 ) ;
#81311 = LINE ( 'NONE', #176617, #5791 ) ;
#81312 = CIRCLE ( 'NONE', #68906, 0.09999999999998898659 ) ;
#81313 = ORIENTED_EDGE ( 'NONE', *, *, #182684, .T. ) ;
#81314 = AXIS2_PLACEMENT_3D ( 'NONE', #73069, #55999, #232118 ) ;
#81315 = CARTESIAN_POINT ( 'NONE',  ( 21.04999999999999716, -0.01454569055747518061, -94.00298221356867145 ) ) ;
#81316 = ORIENTED_EDGE ( 'NONE', *, *, #65525, .T. ) ;
#81317 = ORIENTED_EDGE ( 'NONE', *, *, #254906, .T. ) ;
#81318 = FACE_OUTER_BOUND ( 'NONE', #40281, .T. ) ;
#81319 = EDGE_CURVE ( 'NONE', #319, #144708, #182733, .T. ) ;
#81320 = FACE_OUTER_BOUND ( 'NONE', #91074, .T. ) ;
#81321 = ORIENTED_EDGE ( 'NONE', *, *, #20499, .T. ) ;
#81322 = EDGE_CURVE ( 'NONE', #8981, #163251, #85908, .T. ) ;
#81323 = ORIENTED_EDGE ( 'NONE', *, *, #188615, .F. ) ;
#81324 = EDGE_LOOP ( 'NONE', ( #55634, #1965, #136923, #165781, #14214, #510, #32460, #134907, #231049, #63062, #173407 ) ) ;
#81325 = CARTESIAN_POINT ( 'NONE',  ( 20.94999999999999929, 71.18691588786234092, -91.08158972800052311 ) ) ;
#81326 = CIRCLE ( 'NONE', #227103, 11.74999999999999645 ) ;
#81327 = VERTEX_POINT ( 'NONE', #128930 ) ;
#81328 = AXIS2_PLACEMENT_3D ( 'NONE', #84447, #25812, #201882 ) ;
#81329 = CARTESIAN_POINT ( 'NONE',  ( -23.15000000000000213, 76.00000000001142553, -36.02310748452432421 ) ) ;
#81330 = LINE ( 'NONE', #180476, #111928 ) ;
#81331 = DIRECTION ( 'NONE',  ( -1.000000000000000000, 0.000000000000000000, 0.000000000000000000 ) ) ;
#81332 = VECTOR ( 'NONE', #20546, 1000.000000000000000 ) ;
#81333 = PLANE ( 'NONE',  #94990 ) ;
#81334 = CARTESIAN_POINT ( 'NONE',  ( 11.60000000000000320, -9.650000000000002132, 12.40000000000000391 ) ) ;
#81335 = ADVANCED_FACE ( 'NONE', ( #109335 ), #10271, .T. ) ;
#81336 = DIRECTION ( 'NONE',  ( 0.000000000000000000, 1.000000000000000000, 0.000000000000000000 ) ) ;
#81337 = ADVANCED_FACE ( 'NONE', ( #84609 ), #65999, .T. ) ;
#81338 = DIRECTION ( 'NONE',  ( 0.000000000000000000, 0.9908441862701596881, -0.1350103645451904977 ) ) ;
#81340 = ORIENTED_EDGE ( 'NONE', *, *, #97102, .F. ) ;
#81339 = CARTESIAN_POINT ( 'NONE',  ( -21.95218792049438861, 75.90097156021178648, -76.72461504577100300 ) ) ;
#81342 = DIRECTION ( 'NONE',  ( 0.000000000000000000, 0.9915357197604849349, -0.1298341882520056834 ) ) ;
#81341 = CARTESIAN_POINT ( 'NONE',  ( -16.90138253750127006, 66.05000000001224691, -149.3115447766198542 ) ) ;
#81343 = DIRECTION ( 'NONE',  ( 0.000000000000000000, 0.2128009952263485993, -0.9770955615653341697 ) ) ;
#81344 =( BOUNDED_SURFACE ( )  B_SPLINE_SURFACE ( 3, 2, ( 
 ( #253005, #177363, #114787 ),
 ( #194352, #215167, #15720 ),
 ( #36573, #16988, #183753 ),
 ( #63801, #80770, #241168 ),
 ( #224145, #85895, #164195 ),
 ( #162924, #243721, #22127 ) ),
 .UNSPECIFIED., .F., .F., .F. ) 
 B_SPLINE_SURFACE_WITH_KNOTS ( ( 4, 2, 4 ),
 ( 3, 3 ),
 ( 0.0001300404313046926664, 0.0003183318589266920175, 0.0005066232865486913414 ),
 ( 0.000000000000000000, 1.000000000000000000 ),
 .UNSPECIFIED. ) 
 GEOMETRIC_REPRESENTATION_ITEM ( )  RATIONAL_B_SPLINE_SURFACE ( (
 ( 1.000000000000000000, 0.7071067811865597852, 1.000000000000000000),
 ( 1.000000000000000000, 0.7625113560540101032, 1.000000000000000000),
 ( 1.000000000000000000, 0.8126073484688884907, 1.000000000000000000),
 ( 1.000000000000000000, 0.8923049332732615468, 1.000000000000000000),
 ( 1.000000000000000000, 0.9231914937769579721, 1.000000000000000000),
 ( 1.000000000000000000, 0.9238795325112791890, 1.000000000000000000) ) ) 
 REPRESENTATION_ITEM ( '' )  SURFACE ( )  );
#81345 = ORIENTED_EDGE ( 'NONE', *, *, #199004, .F. ) ;
#81346 = CIRCLE ( 'NONE', #227118, 4.150000000000001243 ) ;
#81347 = FACE_OUTER_BOUND ( 'NONE', #251851, .T. ) ;
#81348 = DIRECTION ( 'NONE',  ( 0.000000000000000000, 0.000000000000000000, 1.000000000000000000 ) ) ;
#81350 = EDGE_LOOP ( 'NONE', ( #89015, #91506, #203195, #62048, #168385, #158099, #248183, #188028, #237585, #163326, #123569, #76274, #97993, #99376 ) ) ;
#81349 = AXIS2_PLACEMENT_3D ( 'NONE', #243210, #205362, #64576 ) ;
#81352 = CARTESIAN_POINT ( 'NONE',  ( 22.00411653889212715, 75.90096189422493467, -76.77655035216474744 ) ) ;
#81351 = CARTESIAN_POINT ( 'NONE',  ( 22.50000000000000000, 64.35042919246686210, -69.62310748452439668 ) ) ;
#81353 = CARTESIAN_POINT ( 'NONE',  ( 21.05000000000000071, 1.115600667400684642E-11, -67.10000000000005116 ) ) ;
#81354 = EDGE_LOOP ( 'NONE', ( #194188, #151503, #16313, #64848 ) ) ;
#81355 = AXIS2_PLACEMENT_3D ( 'NONE', #154418, #136067, #235201 ) ;
#81356 = FACE_OUTER_BOUND ( 'NONE', #248771, .T. ) ;
#81357 = DIRECTION ( 'NONE',  ( -1.000000000000000000, 0.000000000000000000, -0.000000000000000000 ) ) ;
#81358 = ADVANCED_FACE ( 'NONE', ( #243733 ), #74115, .T. ) ;
#81359 = DIRECTION ( 'NONE',  ( 0.000000000000000000, 0.8814952561688359500, -0.4721928772777478911 ) ) ;
#81360 = DIRECTION ( 'NONE',  ( 1.000000000000000000, 0.000000000000000000, 0.000000000000000000 ) ) ;
#81361 = ORIENTED_EDGE ( 'NONE', *, *, #70628, .T. ) ;
#81362 = CIRCLE ( 'NONE', #168925, 0.1000000000000024342 ) ;
#81363 = CIRCLE ( 'NONE', #168928, 0.09999999999999939493 ) ;
#81364 = EDGE_CURVE ( 'NONE', #69117, #207515, #231894, .T. ) ;
#81365 = CARTESIAN_POINT ( 'NONE',  ( -17.04295772865475200, 65.97510057475101064, -182.6731074845244507 ) ) ;
#81366 = LINE ( 'NONE', #78808, #165989 ) ;
#81367 = DIRECTION ( 'NONE',  ( 0.000000000000000000, 0.2617529984165034573, 0.9651348961777156399 ) ) ;
#81368 = DIRECTION ( 'NONE',  ( 0.000000000000000000, 0.7071067811865472397, -0.7071067811865479058 ) ) ;
#81369 = CARTESIAN_POINT ( 'NONE',  ( -18.50000000000000000, 67.23127455305841238, -235.8551265064783991 ) ) ;
#81370 =( BOUNDED_CURVE ( )  B_SPLINE_CURVE ( 3, ( #63783, #143313, #44235, #217698 ),
 .UNSPECIFIED., .F., .F. ) 
 B_SPLINE_CURVE_WITH_KNOTS ( ( 4, 4 ),
 ( 2.589852378279005940, 2.850972632318389710 ),
 .UNSPECIFIED. ) 
 CURVE ( )  GEOMETRIC_REPRESENTATION_ITEM ( )  RATIONAL_B_SPLINE_CURVE ( ( 1.000000000000000000, 0.9943260843901262636, 0.9943260843901262636, 1.000000000000000000 ) ) 
 REPRESENTATION_ITEM ( '' )  );
#81372 = EDGE_LOOP ( 'NONE', ( #3015, #179836, #254780, #31985 ) ) ;
#81371 = DIRECTION ( 'NONE',  ( 1.000000000000000000, 0.000000000000000000, 0.000000000000000000 ) ) ;
#81373 = CARTESIAN_POINT ( 'NONE',  ( -21.13435531349800556, 6.493721063603304700, -33.50000000000000000 ) ) ;
#81374 = SPHERICAL_SURFACE ( 'NONE', #186399, 0.1000000000000000056 ) ;
#81375 = FACE_OUTER_BOUND ( 'NONE', #32547, .T. ) ;
#81376 = CARTESIAN_POINT ( 'NONE',  ( -20.64999999999999858, 0.000000000000000000, -12.97499999999999609 ) ) ;
#81377 = DIRECTION ( 'NONE',  ( 6.938893903907224433E-15, -1.000000000000000000, -2.891205793294679805E-16 ) ) ;
#81379 = EDGE_LOOP ( 'NONE', ( #126164, #234557, #74812, #39217 ) ) ;
#81378 = CARTESIAN_POINT ( 'NONE',  ( 21.05000000000000071, 1.115600667400684642E-11, -180.4749999999999659 ) ) ;
#81380 = DIRECTION ( 'NONE',  ( 0.000000000000000000, -0.9910827722268049644, -0.1332476588733589318 ) ) ;
#81381 = CARTESIAN_POINT ( 'NONE',  ( -23.25000000000000000, 67.23127455305835554, -235.8551265064784559 ) ) ;
#81382 = CARTESIAN_POINT ( 'NONE',  ( 20.88420186297724257, 67.49234744263520724, -195.4268335588911611 ) ) ;
#81383 = ORIENTED_EDGE ( 'NONE', *, *, #207699, .F. ) ;
#81384 = LINE ( 'NONE', #3150, #22022 ) ;
#81385 = CIRCLE ( 'NONE', #85852, 0.1000000000000028644 ) ;
#81386 = DIRECTION ( 'NONE',  ( 0.000000000000000000, -6.308085367188367561E-15, 1.000000000000000000 ) ) ;
#81387 = EDGE_CURVE ( 'NONE', #134756, #47818, #36263, .T. ) ;
#81389 = VECTOR ( 'NONE', #200217, 1000.000000000000000 ) ;
#81388 = DIRECTION ( 'NONE',  ( 0.000000000000000000, 0.000000000000000000, 1.000000000000000000 ) ) ;
#81390 = VECTOR ( 'NONE', #221037, 1000.000000000000000 ) ;
#81391 = CARTESIAN_POINT ( 'NONE',  ( 15.74999999999999645, 66.15000000001204228, -119.7731074845243739 ) ) ;
#81392 = DIRECTION ( 'NONE',  ( 0.000000000000000000, 0.000000000000000000, -1.000000000000000000 ) ) ;
#81393 = VERTEX_POINT ( 'NONE', #250154 ) ;
#81394 = ORIENTED_EDGE ( 'NONE', *, *, #87929, .F. ) ;
#81395 = AXIS2_PLACEMENT_3D ( 'NONE', #161767, #104310, #225536 ) ;
#81396 = ADVANCED_FACE ( 'NONE', ( #113204 ), #110638, .F. ) ;
#81397 = PLANE ( 'NONE',  #30887 ) ;
#81399 = EDGE_CURVE ( 'NONE', #226312, #168568, #75393, .T. ) ;
#81398 = DIRECTION ( 'NONE',  ( -1.000000000000000000, 0.000000000000000000, 0.000000000000000000 ) ) ;
#81400 = DIRECTION ( 'NONE',  ( -0.000000000000000000, -0.000000000000000000, 1.000000000000000000 ) ) ;
#81401 = CARTESIAN_POINT ( 'NONE',  ( 21.14999999999999858, 61.98366251160864238, -221.6357896648344195 ) ) ;
#81402 = ORIENTED_EDGE ( 'NONE', *, *, #29314, .F. ) ;
#81403 = EDGE_CURVE ( 'NONE', #210865, #255460, #41086, .T. ) ;
#81405 = EDGE_CURVE ( 'NONE', #61221, #146439, #220124, .T. ) ;
#81404 = VECTOR ( 'NONE', #42185, 1000.000000000000000 ) ;
#81407 = AXIS2_PLACEMENT_3D ( 'NONE', #171841, #94822, #37444 ) ;
#81406 = CARTESIAN_POINT ( 'NONE',  ( 20.94999999999999574, 0.5876173420563349792, -209.1618981382189588 ) ) ;
#81408 = CARTESIAN_POINT ( 'NONE',  ( 20.86036036209902633, 12.00918032940415969, -206.2305865399390257 ) ) ;
#81409 = AXIS2_PLACEMENT_3D ( 'NONE', #204544, #7641, #85851 ) ;
#81410 = EDGE_CURVE ( 'NONE', #227982, #19031, #57962, .T. ) ;
#81411 = DIRECTION ( 'NONE',  ( 0.000000000000000000, 0.1332476588733448597, -0.9910827722268067408 ) ) ;
#81412 = FACE_OUTER_BOUND ( 'NONE', #105489, .T. ) ;
#81413 = DIRECTION ( 'NONE',  ( -1.000000000000000000, 0.000000000000000000, 0.000000000000000000 ) ) ;
#81414 = ADVANCED_FACE ( 'NONE', ( #131484 ), #187019, .F. ) ;
#81416 = EDGE_CURVE ( 'NONE', #236893, #206400, #74599, .T. ) ;
#81415 = EDGE_CURVE ( 'NONE', #140599, #72959, #228706, .T. ) ;
#81417 = VERTEX_POINT ( 'NONE', #34995 ) ;
#81419 = VERTEX_POINT ( 'NONE', #12846 ) ;
#81418 = CARTESIAN_POINT ( 'NONE',  ( -17.01473183483380325, 66.05000000001153637, -48.77310748452438816 ) ) ;
#81420 = ORIENTED_EDGE ( 'NONE', *, *, #97023, .F. ) ;
#81421 = CARTESIAN_POINT ( 'NONE',  ( -20.54999999999999716, 78.50726470275243685, -228.6618886302502176 ) ) ;
#81422 = ORIENTED_EDGE ( 'NONE', *, *, #250234, .T. ) ;
#81423 = CARTESIAN_POINT ( 'NONE',  ( 20.85000000000000142, 77.73670573947921980, -58.00568489690056850 ) ) ;
#81424 = FACE_OUTER_BOUND ( 'NONE', #98737, .T. ) ;
#81426 = ORIENTED_EDGE ( 'NONE', *, *, #1096, .T. ) ;
#81425 = AXIS2_PLACEMENT_3D ( 'NONE', #78672, #236476, #98210 ) ;
#81427 = CARTESIAN_POINT ( 'NONE',  ( -16.87036670365549895, 66.01058118070992009, -57.00266760182645243 ) ) ;
#81428 = DIRECTION ( 'NONE',  ( 1.000000000000000000, 0.000000000000000000, 0.000000000000000000 ) ) ;
#81429 = VERTEX_POINT ( 'NONE', #72829 ) ;
#81430 = CARTESIAN_POINT ( 'NONE',  ( -16.87304349924914604, 9.961745077968330975, -54.38906667504524961 ) ) ;
#81431 = EDGE_CURVE ( 'NONE', #130735, #220463, #54509, .T. ) ;
#81433 = ORIENTED_EDGE ( 'NONE', *, *, #180410, .F. ) ;
#81432 = DIRECTION ( 'NONE',  ( 0.000000000000000000, 1.000000000000000000, 6.982962677686266711E-15 ) ) ;
#81434 = CYLINDRICAL_SURFACE ( 'NONE', #210673, 0.1000000000000028644 ) ;
#81435 = CARTESIAN_POINT ( 'NONE',  ( 20.94999999999999574, 74.16465844978819177, -191.9679561919613775 ) ) ;
#81436 = ADVANCED_FACE ( 'NONE', ( #115772 ), #94912, .T. ) ;
#81437 = EDGE_CURVE ( 'NONE', #152124, #41100, #207869, .T. ) ;
#81438 = CIRCLE ( 'NONE', #23235, 0.1000000000000028644 ) ;
#81439 = AXIS2_PLACEMENT_3D ( 'NONE', #61119, #256706, #235898 ) ;
#81440 = CIRCLE ( 'NONE', #169000, 12.87499999999999822 ) ;
#81441 = ORIENTED_EDGE ( 'NONE', *, *, #203677, .T. ) ;
#81442 = DIRECTION ( 'NONE',  ( -1.000000000000000000, 0.000000000000000000, 0.000000000000000000 ) ) ;
#81444 = ADVANCED_FACE ( 'NONE', ( #32424 ), #195337, .T. ) ;
#81443 = DIRECTION ( 'NONE',  ( 0.000000000000000000, 6.982962677686266711E-15, -1.000000000000000000 ) ) ;
#81445 = CARTESIAN_POINT ( 'NONE',  ( -18.50000000000000000, -1.164121893230052995, -141.9148480855716343 ) ) ;
#81446 = ORIENTED_EDGE ( 'NONE', *, *, #240222, .F. ) ;
#81447 = CARTESIAN_POINT ( 'NONE',  ( 20.94999999999999574, -1.736257131597395809, -11.56865232901749785 ) ) ;
#81448 = CARTESIAN_POINT ( 'NONE',  ( 12.25000000000000000, 48.12247445990688277, -234.1702647910923361 ) ) ;
#81449 = DIRECTION ( 'NONE',  ( 0.000000000000000000, 0.000000000000000000, 1.000000000000000000 ) ) ;
#81450 = EDGE_CURVE ( 'NONE', #214123, #3677, #92351, .T. ) ;
#81451 = EDGE_LOOP ( 'NONE', ( #57393, #254939, #171228, #211165, #199702, #43794, #3490 ) ) ;
#81452 = CIRCLE ( 'NONE', #114813, 0.1000000000000028644 ) ;
#81453 = ORIENTED_EDGE ( 'NONE', *, *, #146400, .F. ) ;
#81454 = AXIS2_PLACEMENT_3D ( 'NONE', #251095, #213260, #52906 ) ;
#81455 = ORIENTED_EDGE ( 'NONE', *, *, #54913, .T. ) ;
#81456 = CARTESIAN_POINT ( 'NONE',  ( 18.56579813702275317, 10.33025634371522194, -39.08709292826387838 ) ) ;
#81457 = CARTESIAN_POINT ( 'NONE',  ( -20.64999999999999858, 4.250000000000000000, -12.25000000000000000 ) ) ;
#81459 = ORIENTED_EDGE ( 'NONE', *, *, #103614, .F. ) ;
#81458 = CARTESIAN_POINT ( 'NONE',  ( -16.83199030136658081, 9.930648033124622742, -146.7724010226574762 ) ) ;
#81460 = CARTESIAN_POINT ( 'NONE',  ( 20.99749315643150638, 11.75000000001115907, -126.9851942312421045 ) ) ;
#81461 = LINE ( 'NONE', #218414, #20385 ) ;
#81462 = CARTESIAN_POINT ( 'NONE',  ( -23.25000000000000000, 11.75000000001115552, -122.2500000000000284 ) ) ;
#81463 = CARTESIAN_POINT ( 'NONE',  ( -20.85000000000000142, 64.25000000001250555, -176.8069731475025321 ) ) ;
#81464 = DIRECTION ( 'NONE',  ( 0.000000000000000000, 0.000000000000000000, 1.000000000000000000 ) ) ;
#81465 = CARTESIAN_POINT ( 'NONE',  ( 21.14999999999999858, 11.40444339177024169, -198.6185779617709670 ) ) ;
#81467 = ORIENTED_EDGE ( 'NONE', *, *, #246527, .T. ) ;
#81466 = DIRECTION ( 'NONE',  ( 1.000000000000000000, -2.952720810173289112E-16, -2.061873921506763405E-30 ) ) ;
#81469 = ORIENTED_EDGE ( 'NONE', *, *, #225763, .T. ) ;
#81468 = FACE_OUTER_BOUND ( 'NONE', #114617, .T. ) ;
#81470 = LINE ( 'NONE', #178060, #174599 ) ;
#81471 = ORIENTED_EDGE ( 'NONE', *, *, #211565, .T. ) ;
#81472 = ORIENTED_EDGE ( 'NONE', *, *, #1344, .F. ) ;
#81473 = CARTESIAN_POINT ( 'NONE',  ( -20.85000000000000142, -1.736705739456431807, -179.0174225876237415 ) ) ;
#81474 = DIRECTION ( 'NONE',  ( -0.000000000000000000, 1.000000000000000000, 6.982962677686266711E-15 ) ) ;
#81475 = CIRCLE ( 'NONE', #135665, 0.1000000000000028644 ) ;
#81476 = CIRCLE ( 'NONE', #248099, 0.5000000000000004441 ) ;
#81477 = DIRECTION ( 'NONE',  ( 0.000000000000000000, 0.000000000000000000, -1.000000000000000000 ) ) ;
#81478 = DIRECTION ( 'NONE',  ( 0.000000000000000000, 0.000000000000000000, -1.000000000000000000 ) ) ;
#81479 = DIRECTION ( 'NONE',  ( -0.000000000000000000, -6.982962677686266711E-15, 1.000000000000000000 ) ) ;
#81480 = DIRECTION ( 'NONE',  ( 0.000000000000000000, 0.000000000000000000, -1.000000000000000000 ) ) ;
#81481 = CARTESIAN_POINT ( 'NONE',  ( 21.05000000000000071, 10.39655183198267530, -207.4949966697317620 ) ) ;
#81483 = ORIENTED_EDGE ( 'NONE', *, *, #245811, .T. ) ;
#81482 = EDGE_CURVE ( 'NONE', #154251, #180754, #57787, .T. ) ;
#81484 = VERTEX_POINT ( 'NONE', #53235 ) ;
#81485 = CARTESIAN_POINT ( 'NONE',  ( 23.24999999999999289, 67.55989888862310977, -211.9120700681549465 ) ) ;
#81486 = CIRCLE ( 'NONE', #227268, 0.1000000000000028783 ) ;
#81487 = ADVANCED_FACE ( 'NONE', ( #81738 ), #201720, .F. ) ;
#81488 = CIRCLE ( 'NONE', #127320, 0.09999999999998898659 ) ;
#81489 = VERTEX_POINT ( 'NONE', #178338 ) ;
#81490 = LINE ( 'NONE', #39860, #117884 ) ;
#81491 = PLANE ( 'NONE',  #118436 ) ;
#81492 = AXIS2_PLACEMENT_3D ( 'NONE', #187588, #166753, #87159 ) ;
#81493 = AXIS2_PLACEMENT_3D ( 'NONE', #243856, #27425, #44397 ) ;
#81494 = CARTESIAN_POINT ( 'NONE',  ( -15.52965525596987817, 66.62446189796352769, -53.65323160353355547 ) ) ;
#81495 = DIRECTION ( 'NONE',  ( 0.000000000000000000, -6.982962677686266711E-15, 1.000000000000000000 ) ) ;
#81496 = EDGE_CURVE ( 'NONE', #141490, #73323, #257789, .T. ) ;
#81497 = ORIENTED_EDGE ( 'NONE', *, *, #50190, .T. ) ;
#81499 = EDGE_CURVE ( 'NONE', #99805, #244509, #241170, .T. ) ;
#81498 = CARTESIAN_POINT ( 'NONE',  ( -16.93658211146644987, 66.00589133767104499, -149.1188124145687652 ) ) ;
#81500 = ORIENTED_EDGE ( 'NONE', *, *, #181033, .T. ) ;
#81501 = CARTESIAN_POINT ( 'NONE',  ( -23.25000000000000000, 76.00000000001237765, -170.0231074845243597 ) ) ;
#81502 = ORIENTED_EDGE ( 'NONE', *, *, #232590, .T. ) ;
#81503 = CARTESIAN_POINT ( 'NONE',  ( 21.05000000000000071, 5.265981236333658899E-16, -4.300000000000032685 ) ) ;
#81504 = CARTESIAN_POINT ( 'NONE',  ( 13.12220780326572367, 9.430633469083952392, -182.7317657948241276 ) ) ;
#81505 = VERTEX_POINT ( 'NONE', #23110 ) ;
#81506 = CARTESIAN_POINT ( 'NONE',  ( 21.05000000000000071, 21.98309897467606433, -231.7335930323676791 ) ) ;
#81508 = ORIENTED_EDGE ( 'NONE', *, *, #201677, .F. ) ;
#81507 = CARTESIAN_POINT ( 'NONE',  ( -21.17356465864818205, 6.422803126252873973, -100.4010887589861625 ) ) ;
#81509 = DIRECTION ( 'NONE',  ( 0.000000000000000000, -1.000000000000000000, -6.982962677686266711E-15 ) ) ;
#81511 = VERTEX_POINT ( 'NONE', #219999 ) ;
#81510 = CIRCLE ( 'NONE', #14930, 4.149999999999987033 ) ;
#81512 = EDGE_CURVE ( 'NONE', #162009, #137285, #157504, .T. ) ;
#81514 = ADVANCED_FACE ( 'NONE', ( #156212 ), #79191, .F. ) ;
#81513 = CIRCLE ( 'NONE', #89736, 0.09999999999999939493 ) ;
#81515 = CARTESIAN_POINT ( 'NONE',  ( -16.77683809663752257, 52.34166666667822199, -52.77310748452448763 ) ) ;
#81516 = ORIENTED_EDGE ( 'NONE', *, *, #226100, .T. ) ;
#81517 = TOROIDAL_SURFACE ( 'NONE', #202182, 12.77499999999999858, 0.1000000000000000056 ) ;
#81518 = DIRECTION ( 'NONE',  ( -1.000000000000000000, 1.207181226542539700E-16, -2.694675058168174199E-16 ) ) ;
#81519 = DIRECTION ( 'NONE',  ( 0.000000000000000000, 1.000000000000000000, 0.000000000000000000 ) ) ;
#81520 = CARTESIAN_POINT ( 'NONE',  ( 20.94999999999999929, -1.835859311432481045, -145.5044391687985694 ) ) ;
#81521 = CARTESIAN_POINT ( 'NONE',  ( -16.93909480342659890, 66.00692163521003408, -56.92276046785206489 ) ) ;
#81522 = VECTOR ( 'NONE', #237381, 1000.000000000000000 ) ;
#81523 = VECTOR ( 'NONE', #117530, 1000.000000000000000 ) ;
#81524 = CARTESIAN_POINT ( 'NONE',  ( -20.54999999999999716, 4.768403829798271154, -213.4961173936592331 ) ) ;
#81525 = ORIENTED_EDGE ( 'NONE', *, *, #246602, .T. ) ;
#81527 = EDGE_CURVE ( 'NONE', #137697, #177256, #158777, .T. ) ;
#81526 = SPHERICAL_SURFACE ( 'NONE', #61125, 0.1000000000000000056 ) ;
#81528 = CARTESIAN_POINT ( 'NONE',  ( -20.64999999999999858, 1.115600667400684642E-11, -180.4749999999999659 ) ) ;
#81529 = CARTESIAN_POINT ( 'NONE',  ( -20.94999999999999929, 47.95459712139160047, -246.5019368548292675 ) ) ;
#81530 = ORIENTED_EDGE ( 'NONE', *, *, #125508, .F. ) ;
#81531 = EDGE_CURVE ( 'NONE', #89486, #15940, #53707, .T. ) ;
#81532 = CARTESIAN_POINT ( 'NONE',  ( -21.05000000000000071, 76.10000000001200249, -109.5637644362255543 ) ) ;
#81533 = VERTEX_POINT ( 'NONE', #118351 ) ;
#81534 = FACE_OUTER_BOUND ( 'NONE', #23195, .T. ) ;
#81535 = EDGE_LOOP ( 'NONE', ( #257102, #84204, #422, #195317 ) ) ;
#81536 = AXIS2_PLACEMENT_3D ( 'NONE', #27594, #186643, #203621 ) ;
#81537 = CARTESIAN_POINT ( 'NONE',  ( -11.60000000000000320, -8.279289321881350361, 18.97071067811866030 ) ) ;
#81538 = CARTESIAN_POINT ( 'NONE',  ( -20.93302460841142931, 10.31565961587945424, -72.53641941191781939 ) ) ;
#81539 = EDGE_LOOP ( 'NONE', ( #192170, #103458, #118841, #50186, #223213 ) ) ;
#81541 = ORIENTED_EDGE ( 'NONE', *, *, #217612, .T. ) ;
#81540 = DIRECTION ( 'NONE',  ( -7.304098846218201720E-16, 1.000000000000000000, 0.000000000000000000 ) ) ;
#81542 = DIRECTION ( 'NONE',  ( -1.000000000000000000, 0.000000000000000000, -0.000000000000000000 ) ) ;
#81543 = ORIENTED_EDGE ( 'NONE', *, *, #137946, .T. ) ;
#81544 = VECTOR ( 'NONE', #169380, 1000.000000000000000 ) ;
#81545 = VECTOR ( 'NONE', #107051, 1000.000000000000114 ) ;
#81546 = ADVANCED_FACE ( 'NONE', ( #21814 ), #109592, .T. ) ;
#81547 = CARTESIAN_POINT ( 'NONE',  ( -20.85000000000000142, 1.115600667400684642E-11, -67.00000000000000000 ) ) ;
#81548 = LINE ( 'NONE', #217218, #72988 ) ;
#81549 = EDGE_CURVE ( 'NONE', #221772, #670, #232796, .T. ) ;
#81550 = ORIENTED_EDGE ( 'NONE', *, *, #255333, .F. ) ;
#81551 = ORIENTED_EDGE ( 'NONE', *, *, #210599, .T. ) ;
#81552 = CARTESIAN_POINT ( 'NONE',  ( -20.94999999999999929, 68.96868720525668550, -99.41395654629704381 ) ) ;
#81553 = CARTESIAN_POINT ( 'NONE',  ( -16.89797118371758344, 14.20335419055749604, -219.3347526740980129 ) ) ;
#81554 = DIRECTION ( 'NONE',  ( 1.000000000000000000, 0.000000000000000000, 0.000000000000000000 ) ) ;
#81555 = EDGE_CURVE ( 'NONE', #216154, #45320, #203738, .T. ) ;
#81556 = ORIENTED_EDGE ( 'NONE', *, *, #87797, .F. ) ;
#81557 = ORIENTED_EDGE ( 'NONE', *, *, #194139, .F. ) ;
#81558 = CARTESIAN_POINT ( 'NONE',  ( 23.24999999999999289, 64.35000000001245724, -181.7731074845244450 ) ) ;
#81559 = EDGE_CURVE ( 'NONE', #178121, #217322, #128729, .T. ) ;
#81561 = VERTEX_POINT ( 'NONE', #160057 ) ;
#81560 = CARTESIAN_POINT ( 'NONE',  ( -16.79139129368504157, 9.944944162472829419, -46.17024463282581337 ) ) ;
#81562 = PLANE ( 'NONE',  #90117 ) ;
#81563 = AXIS2_PLACEMENT_3D ( 'NONE', #208892, #231051, #48534 ) ;
#81564 = CARTESIAN_POINT ( 'NONE',  ( -20.64999999999999858, 47.45383559552795560, -242.5236527704543334 ) ) ;
#81565 = ADVANCED_FACE ( 'NONE', ( #77915 ), #237009, .F. ) ;
#81567 = DIRECTION ( 'NONE',  ( 0.000000000000000000, -1.000000000000000000, -2.891205793294679805E-16 ) ) ;
#81566 = CARTESIAN_POINT ( 'NONE',  ( -17.73285935862681484, 65.14201819622762457, -126.2816692942949857 ) ) ;
#81568 = CARTESIAN_POINT ( 'NONE',  ( 18.59999999999999787, 7.783179459866048866, -245.3643104511423019 ) ) ;
#81569 = CIRCLE ( 'NONE', #198312, 0.09999999999999939493 ) ;
#81570 = CARTESIAN_POINT ( 'NONE',  ( 21.13736287352038445, 8.046642376395153562, -79.65000000000004832 ) ) ;
#81571 = CARTESIAN_POINT ( 'NONE',  ( 21.05000000000000071, 84.66355140188136374, -146.0472086025916099 ) ) ;
#81572 = LINE ( 'NONE', #161157, #209096 ) ;
#81574 = ORIENTED_EDGE ( 'NONE', *, *, #243215, .T. ) ;
#81573 = AXIS2_PLACEMENT_3D ( 'NONE', #2336, #242239, #121055 ) ;
#81575 = ORIENTED_EDGE ( 'NONE', *, *, #80395, .F. ) ;
#81576 = EDGE_CURVE ( 'NONE', #22846, #137667, #86994, .T. ) ;
#81577 = CARTESIAN_POINT ( 'NONE',  ( 20.04142135623730070, 11.75000000001115907, -54.85000000000000142 ) ) ;
#81578 = VERTEX_POINT ( 'NONE', #7368 ) ;
#81579 = CIRCLE ( 'NONE', #2501, 0.1000000000000013933 ) ;
#81580 = CARTESIAN_POINT ( 'NONE',  ( -20.15000000000000568, 66.70857864377455826, -90.77310748452437394 ) ) ;
#81581 = EDGE_LOOP ( 'NONE', ( #116981, #20688, #56245, #30891 ) ) ;
#81582 = CIRCLE ( 'NONE', #223092, 0.09999999999998898659 ) ;
#81583 =( NAMED_UNIT ( * ) PLANE_ANGLE_UNIT ( ) SI_UNIT ( $, .RADIAN. ) );
#81584 = DIRECTION ( 'NONE',  ( -1.000000000000000000, -0.000000000000000000, -0.000000000000000000 ) ) ;
#81586 = ORIENTED_EDGE ( 'NONE', *, *, #129279, .T. ) ;
#81585 = ORIENTED_EDGE ( 'NONE', *, *, #206206, .T. ) ;
#81587 = ORIENTED_EDGE ( 'NONE', *, *, #38928, .T. ) ;
#81588 = ORIENTED_EDGE ( 'NONE', *, *, #195970, .T. ) ;
#81589 = DIRECTION ( 'NONE',  ( -2.978066053179069723E-16, -1.000000000000000000, -4.764905685086511557E-15 ) ) ;
#81590 = CARTESIAN_POINT ( 'NONE',  ( -21.07928932188134041, 75.90110485435759813, -109.3516241409176075 ) ) ;
#81592 = ORIENTED_EDGE ( 'NONE', *, *, #256793, .T. ) ;
#81591 = DIRECTION ( 'NONE',  ( 1.000000000000000000, 0.000000000000000000, 0.000000000000000000 ) ) ;
#81593 = AXIS2_PLACEMENT_3D ( 'NONE', #127457, #227832, #6210 ) ;
#81594 = DIRECTION ( 'NONE',  ( 0.000000000000000000, 0.000000000000000000, 1.000000000000000000 ) ) ;
#81595 = CARTESIAN_POINT ( 'NONE',  ( 20.94999999999999929, 65.70711192142366031, -97.56510546851220056 ) ) ;
#81597 = ORIENTED_EDGE ( 'NONE', *, *, #27608, .F. ) ;
#81596 = DIRECTION ( 'NONE',  ( -0.000000000000000000, 1.000000000000000000, -0.000000000000000000 ) ) ;
#81598 = CARTESIAN_POINT ( 'NONE',  ( -22.32929514600008503, 0.09907567812507747651, -59.42135243462354310 ) ) ;
#81599 = ORIENTED_EDGE ( 'NONE', *, *, #243676, .T. ) ;
#81600 = LINE ( 'NONE', #240718, #154269 ) ;
#81602 = ORIENTED_EDGE ( 'NONE', *, *, #112441, .F. ) ;
#81601 = CARTESIAN_POINT ( 'NONE',  ( 21.97500000000000497, 9.750000000011153745, -45.75000000000000000 ) ) ;
#81603 = CARTESIAN_POINT ( 'NONE',  ( -20.94999999999999929, 87.75000000001236344, -166.9231074845242802 ) ) ;
#81604 = CYLINDRICAL_SURFACE ( 'NONE', #81761, 0.09999999999999935330 ) ;
#81605 = ORIENTED_EDGE ( 'NONE', *, *, #37411, .F. ) ;
#81607 = CARTESIAN_POINT ( 'NONE',  ( -21.05000000000000071, 70.15000000001178648, -79.65560470880227228 ) ) ;
#81606 = CARTESIAN_POINT ( 'NONE',  ( -17.11825945287481687, 9.950000000011140600, -121.3500000000000369 ) ) ;
#81608 = CYLINDRICAL_SURFACE ( 'NONE', #49389, 0.1000000000000098310 ) ;
#81609 = CARTESIAN_POINT ( 'NONE',  ( 18.48197441911657180, 85.51795479471881833, -163.1328958423161168 ) ) ;
#81610 = AXIS2_PLACEMENT_3D ( 'NONE', #112171, #229539, #232113 ) ;
#81611 = VECTOR ( 'NONE', #226599, 1000.000000000000000 ) ;
#81612 = CARTESIAN_POINT ( 'NONE',  ( -13.40000000000000213, -8.250000000000005329, 19.04142135623731491 ) ) ;
#81613 = VECTOR ( 'NONE', #77000, 1000.000000000000000 ) ;
#81615 = CARTESIAN_POINT ( 'NONE',  ( -20.94999999999999929, 36.18002604163306302, -236.0784499204090991 ) ) ;
#81614 = AXIS2_PLACEMENT_3D ( 'NONE', #228614, #108648, #169956 ) ;
#81616 = ORIENTED_EDGE ( 'NONE', *, *, #252478, .F. ) ;
#81617 = EDGE_LOOP ( 'NONE', ( #179112, #125545, #110806, #10406 ) ) ;
#81618 = ORIENTED_EDGE ( 'NONE', *, *, #155847, .T. ) ;
#81619 = CARTESIAN_POINT ( 'NONE',  ( 18.49999999999998934, 56.14960075277911500, -201.2428044267231257 ) ) ;
#81620 = ORIENTED_EDGE ( 'NONE', *, *, #87605, .F. ) ;
#81621 = CARTESIAN_POINT ( 'NONE',  ( 23.14999999999999503, 53.28269063671665151, -234.9266833317103647 ) ) ;
#81622 = ORIENTED_EDGE ( 'NONE', *, *, #19691, .T. ) ;
#81623 = CARTESIAN_POINT ( 'NONE',  ( -21.05000000000000071, -4.735542975717121905, -233.2463119243910796 ) ) ;
#81624 = ADVANCED_FACE ( 'NONE', ( #25661 ), #127892, .F. ) ;
#81625 = DIRECTION ( 'NONE',  ( 0.000000000000000000, -0.8814952561688430555, 0.4721928772777346239 ) ) ;
#81626 = EDGE_CURVE ( 'NONE', #205206, #135186, #41270, .T. ) ;
#81627 = EDGE_CURVE ( 'NONE', #215393, #110145, #7943, .T. ) ;
#81628 = ORIENTED_EDGE ( 'NONE', *, *, #212877, .T. ) ;
#81629 = AXIS2_PLACEMENT_3D ( 'NONE', #5332, #84858, #243968 ) ;
#81630 = CYLINDRICAL_SURFACE ( 'NONE', #256761, 0.09999999999998898659 ) ;
#81631 = CIRCLE ( 'NONE', #181644, 0.09999999999999939493 ) ;
#81632 = ORIENTED_EDGE ( 'NONE', *, *, #81403, .T. ) ;
#81633 = ORIENTED_EDGE ( 'NONE', *, *, #93626, .T. ) ;
#81634 = VERTEX_POINT ( 'NONE', #103880 ) ;
#81635 = DIRECTION ( 'NONE',  ( 0.000000000000000000, 0.000000000000000000, 1.000000000000000000 ) ) ;
#81636 = FACE_OUTER_BOUND ( 'NONE', #129400, .T. ) ;
#81637 = AXIS2_PLACEMENT_3D ( 'NONE', #193718, #192431, #131161 ) ;
#81638 = LINE ( 'NONE', #42541, #63415 ) ;
#81639 = CARTESIAN_POINT ( 'NONE',  ( 21.05000000000000071, 76.00000000001169553, -67.62310748452431142 ) ) ;
#81640 = CARTESIAN_POINT ( 'NONE',  ( -20.00857864376270001, 66.65000000001157332, -57.27310748452438816 ) ) ;
#81641 = CARTESIAN_POINT ( 'NONE',  ( -23.25000000000000000, -9.599999999988847676, -43.39396912265245021 ) ) ;
#81642 = EDGE_CURVE ( 'NONE', #236908, #207747, #164454, .T. ) ;
#81644 = DIRECTION ( 'NONE',  ( -0.000000000000000000, -0.000000000000000000, -1.000000000000000000 ) ) ;
#81643 = DIRECTION ( 'NONE',  ( 1.000000000000000000, 0.000000000000000000, 0.000000000000000000 ) ) ;
#81645 = DIRECTION ( 'NONE',  ( -1.000000000000000000, 0.000000000000000000, 0.000000000000000000 ) ) ;
#81647 = ORIENTED_EDGE ( 'NONE', *, *, #29131, .T. ) ;
#81646 = CARTESIAN_POINT ( 'NONE',  ( -23.15000000000000213, 87.65000000001172964, -72.62310748452422615 ) ) ;
#81648 = CARTESIAN_POINT ( 'NONE',  ( -23.15000000000000213, 1.115600667400684642E-11, -102.6000000000000512 ) ) ;
#81649 = CARTESIAN_POINT ( 'NONE',  ( -18.48550754432048748, -9.463399778548652108, -141.0487897524151322 ) ) ;
#81650 = VERTEX_POINT ( 'NONE', #187311 ) ;
#81651 = VERTEX_POINT ( 'NONE', #64773 ) ;
#81652 = CARTESIAN_POINT ( 'NONE',  ( -16.93860193097148326, 66.00689223268226158, -48.62296911721753645 ) ) ;
#81653 = CARTESIAN_POINT ( 'NONE',  ( -21.14999999999999858, 69.45934304831041572, -69.52310748452435973 ) ) ;
#81654 = CARTESIAN_POINT ( 'NONE',  ( 19.90621891164687440, 64.25000000001148237, -44.69466220664675404 ) ) ;
#81655 = EDGE_LOOP ( 'NONE', ( #243943, #5910, #160348, #68653 ) ) ;
#81656 = VECTOR ( 'NONE', #78393, 1000.000000000000000 ) ;
#81657 = CARTESIAN_POINT ( 'NONE',  ( 18.59999999999997655, 62.42744096235649920, -225.1319887738535499 ) ) ;
#81658 = VERTEX_POINT ( 'NONE', #6075 ) ;
#81659 = ORIENTED_EDGE ( 'NONE', *, *, #124436, .F. ) ;
#81660 = CARTESIAN_POINT ( 'NONE',  ( -23.15000000000000213, 52.81534179157633702, -244.1198638051726277 ) ) ;
#81662 = EDGE_LOOP ( 'NONE', ( #106784, #194674, #165851, #101039, #252488, #189808, #63455, #185208, #204092 ) ) ;
#81661 = ADVANCED_FACE ( 'NONE', ( #88160 ), #83022, .T. ) ;
#81663 = CARTESIAN_POINT ( 'NONE',  ( -16.94062896051973865, 60.88569912951715679, -221.0763738239286340 ) ) ;
#81664 = EDGE_CURVE ( 'NONE', #17135, #113369, #157996, .T. ) ;
#81665 = CARTESIAN_POINT ( 'NONE',  ( -18.41817142474042157, -9.498703066590927335, -174.1039654876370548 ) ) ;
#81666 = CARTESIAN_POINT ( 'NONE',  ( -18.59999999999999787, 38.20647789760820956, -236.0922579506644468 ) ) ;
#81667 = CARTESIAN_POINT ( 'NONE',  ( 22.48660254037844197, 11.65000000001115588, -133.9500000000000171 ) ) ;
#81668 = ORIENTED_EDGE ( 'NONE', *, *, #147242, .T. ) ;
#81669 = DIRECTION ( 'NONE',  ( 1.000000000000000000, -0.000000000000000000, -0.000000000000000000 ) ) ;
#81670 = FACE_OUTER_BOUND ( 'NONE', #88181, .T. ) ;
#81671 = EDGE_CURVE ( 'NONE', #191947, #11272, #26968, .T. ) ;
#81672 = VECTOR ( 'NONE', #99358, 1000.000000000000000 ) ;
#81673 = DIRECTION ( 'NONE',  ( -1.000000000000000000, 0.000000000000000000, 0.000000000000000000 ) ) ;
#81674 = AXIS2_PLACEMENT_3D ( 'NONE', #84239, #47722, #105105 ) ;
#81675 = AXIS2_PLACEMENT_3D ( 'NONE', #223977, #200573, #239711 ) ;
#81676 = VERTEX_POINT ( 'NONE', #143008 ) ;
#81677 = COLOUR_RGB ( '', 0.08235294, 0.09019608, 0.10196078) ;
#81679 = EDGE_LOOP ( 'NONE', ( #14569, #249554 ) ) ;
#81678 = CARTESIAN_POINT ( 'NONE',  ( 18.59999999999999076, 69.45000000001149942, -48.27310748452436684 ) ) ;
#81680 = DIRECTION ( 'NONE',  ( -1.073024830501117725E-15, -6.982962677686266711E-15, 1.000000000000000000 ) ) ;
#81681 = CARTESIAN_POINT ( 'NONE',  ( 18.52165635395197185, 78.22063626114007207, -231.5569302423936335 ) ) ;
#81682 = DIRECTION ( 'NONE',  ( -1.000000000000000000, 0.000000000000000000, 0.000000000000000000 ) ) ;
#81683 = DIRECTION ( 'NONE',  ( -1.000000000000000000, 0.000000000000000000, -0.000000000000000000 ) ) ;
#81684 = CARTESIAN_POINT ( 'NONE',  ( -18.50000000000000000, -1.135018845899022466, -74.71697688343232358 ) ) ;
#81685 = DIRECTION ( 'NONE',  ( 4.504528286903032433E-15, 0.1298341882520054891, 0.9915357197604850459 ) ) ;
#81686 = ORIENTED_EDGE ( 'NONE', *, *, #185164, .T. ) ;
#81687 = ADVANCED_FACE ( 'NONE', ( #24394 ), #149593, .T. ) ;
#81688 = DIRECTION ( 'NONE',  ( -1.000000000000000000, 0.000000000000000000, -0.000000000000000000 ) ) ;
#81689 = CARTESIAN_POINT ( 'NONE',  ( 16.27683809663749770, 66.65000000001209912, -127.2731074845243597 ) ) ;
#81690 = CARTESIAN_POINT ( 'NONE',  ( -18.59999999999999787, 1.162701749949165642, -108.5000000000000426 ) ) ;
#81691 = CARTESIAN_POINT ( 'NONE',  ( -18.59999999999999787, 2.859758780633683273, -208.6670499591424459 ) ) ;
#81692 = AXIS2_PLACEMENT_3D ( 'NONE', #189228, #152693, #90099 ) ;
#81693 = CARTESIAN_POINT ( 'NONE',  ( 20.44999100639871514, 65.56028929679979456, -61.76403175855386962 ) ) ;
#81694 =( BOUNDED_CURVE ( )  B_SPLINE_CURVE ( 3, ( #166356, #224981, #26839, #47629 ),
 .UNSPECIFIED., .F., .T. ) 
 B_SPLINE_CURVE_WITH_KNOTS ( ( 4, 4 ),
 ( 5.733388419619901200, 5.983100554402347449 ),
 .UNSPECIFIED. ) 
 CURVE ( )  GEOMETRIC_REPRESENTATION_ITEM ( )  RATIONAL_B_SPLINE_CURVE ( ( 1.000000000000000000, 0.9948104011409417691, 0.9948104011409417691, 1.000000000000000000 ) ) 
 REPRESENTATION_ITEM ( '' )  );
#81695 = VECTOR ( 'NONE', #36005, 1000.000000000000000 ) ;
#81696 = ORIENTED_EDGE ( 'NONE', *, *, #24639, .T. ) ;
#81697 = ORIENTED_EDGE ( 'NONE', *, *, #92158, .T. ) ;
#81698 = DIRECTION ( 'NONE',  ( 0.000000000000000000, 1.000000000000000000, 1.224646799147352961E-16 ) ) ;
#81699 = DIRECTION ( 'NONE',  ( 0.000000000000000000, 0.4088369013363281623, -0.9126074666063771490 ) ) ;
#81700 = EDGE_CURVE ( 'NONE', #115794, #180734, #62089, .T. ) ;
#81701 = CARTESIAN_POINT ( 'NONE',  ( -21.05000000000000071, 69.69257478044727350, -203.5062876161387635 ) ) ;
#81702 = CARTESIAN_POINT ( 'NONE',  ( -16.81744102076749314, 22.97806745954242302, -230.9350634111226270 ) ) ;
#81703 = AXIS2_PLACEMENT_3D ( 'NONE', #222909, #224194, #109373 ) ;
#81704 = ORIENTED_EDGE ( 'NONE', *, *, #1548, .F. ) ;
#81705 = DIRECTION ( 'NONE',  ( -1.000000000000000000, 0.000000000000000000, 0.000000000000000000 ) ) ;
#81706 = AXIS2_PLACEMENT_3D ( 'NONE', #161375, #203045, #217462 ) ;
#81707 = ADVANCED_FACE ( 'NONE', ( #49047 ), #191294, .F. ) ;
#81708 = EDGE_CURVE ( 'NONE', #21234, #51100, #78807, .T. ) ;
#81709 = CARTESIAN_POINT ( 'NONE',  ( -17.11825945287482753, 10.05000000001113847, -113.1500000000000341 ) ) ;
#81710 = DIRECTION ( 'NONE',  ( 1.000000000000000000, -1.335000415235278971E-16, 2.979993593738921214E-16 ) ) ;
#81711 = LINE ( 'NONE', #158753, #41275 ) ;
#81712 = EDGE_CURVE ( 'NONE', #148222, #157687, #224569, .T. ) ;
#81713 = CIRCLE ( 'NONE', #48435, 11.74999999999999822 ) ;
#81714 = EDGE_CURVE ( 'NONE', #200257, #194069, #45198, .T. ) ;
#81715 = COLOUR_RGB ( '', 0.72549020, 0.75294118, 0.79215686) ;
#81716 = ORIENTED_EDGE ( 'NONE', *, *, #126761, .F. ) ;
#81718 = DIRECTION ( 'NONE',  ( -1.000000000000000000, -4.163336342344362270E-13, 0.000000000000000000 ) ) ;
#81717 = CIRCLE ( 'NONE', #164961, 0.1999999999999996503 ) ;
#81719 = ORIENTED_EDGE ( 'NONE', *, *, #220050, .T. ) ;
#81720 = DIRECTION ( 'NONE',  ( 0.000000000000000000, -7.105427357601027102E-15, -1.000000000000000000 ) ) ;
#81722 = EDGE_CURVE ( 'NONE', #26416, #161732, #178833, .T. ) ;
#81721 = CARTESIAN_POINT ( 'NONE',  ( 23.14999999999999503, 69.35000000001151932, -48.27310748452436684 ) ) ;
#81723 = AXIS2_PLACEMENT_3D ( 'NONE', #2022, #41197, #118140 ) ;
#81724 = CARTESIAN_POINT ( 'NONE',  ( 18.52643265882457868, 65.68026841930880266, -63.97257401318892533 ) ) ;
#81725 = DIRECTION ( 'NONE',  ( 0.000000000000000000, 0.2558827019433787542, -0.9667078373770204847 ) ) ;
#81726 = CARTESIAN_POINT ( 'NONE',  ( 20.95595012432476523, 18.83168586542424094, -227.9718358157221019 ) ) ;
#81727 = CARTESIAN_POINT ( 'NONE',  ( -18.59999999999999787, 64.25000000001210765, -129.5083017138703667 ) ) ;
#81728 = DIRECTION ( 'NONE',  ( 0.000000000000000000, 1.000000000000000000, 0.000000000000000000 ) ) ;
#81729 = DIRECTION ( 'NONE',  ( -2.602085213965226419E-14, 6.982962677686266711E-15, -1.000000000000000000 ) ) ;
#81730 = EDGE_CURVE ( 'NONE', #178236, #216194, #99649, .T. ) ;
#81731 = CARTESIAN_POINT ( 'NONE',  ( -18.59999999999999787, 7.249999999999999112, -21.35000000000000142 ) ) ;
#81732 = DIRECTION ( 'NONE',  ( 1.000000000000000000, 0.000000000000000000, 0.000000000000000000 ) ) ;
#81733 = VECTOR ( 'NONE', #201545, 1000.000000000000000 ) ;
#81734 = CARTESIAN_POINT ( 'NONE',  ( -20.85000000000000142, 78.48087866980282001, -232.8271061603568910 ) ) ;
#81735 = EDGE_CURVE ( 'NONE', #164130, #24822, #206845, .T. ) ;
#81736 = ADVANCED_FACE ( 'NONE', ( #146845 ), #148149, .F. ) ;
#81737 = CARTESIAN_POINT ( 'NONE',  ( -21.05000000000000071, 69.74218538953553548, -69.62089777583315708 ) ) ;
#81738 = FACE_OUTER_BOUND ( 'NONE', #215034, .T. ) ;
#81739 = ORIENTED_EDGE ( 'NONE', *, *, #214664, .F. ) ;
#81740 = CARTESIAN_POINT ( 'NONE',  ( 20.90000000000000213, 3.461118860469513336, 28.84309995045515507 ) ) ;
#81742 = ADVANCED_FACE ( 'NONE', ( #187297 ), #126010, .F. ) ;
#81741 = FACE_OUTER_BOUND ( 'NONE', #101754, .T. ) ;
#81743 = ORIENTED_EDGE ( 'NONE', *, *, #117730, .F. ) ;
#81744 = DIRECTION ( 'NONE',  ( -0.000000000000000000, 0.8814952561688430555, -0.4721928772777346239 ) ) ;
#81745 = ADVANCED_FACE ( 'NONE', ( #46466 ), #183437, .T. ) ;
#81746 = AXIS2_PLACEMENT_3D ( 'NONE', #107832, #247335, #67421 ) ;
#81747 = ADVANCED_FACE ( 'NONE', ( #247237 ), #223819, .F. ) ;
#81748 = CIRCLE ( 'NONE', #144118, 0.09999999999999022171 ) ;
#81749 = DIRECTION ( 'NONE',  ( 0.000000000000000000, -7.116814260417660624E-15, 1.000000000000000000 ) ) ;
#81750 = ORIENTED_EDGE ( 'NONE', *, *, #67911, .T. ) ;
#81751 = CARTESIAN_POINT ( 'NONE',  ( -23.15000000000000213, 47.40541193113006813, -242.6436572752161283 ) ) ;
#81752 = AXIS2_PLACEMENT_3D ( 'NONE', #100237, #39031, #136821 ) ;
#81753 = EDGE_CURVE ( 'NONE', #214318, #227579, #158186, .T. ) ;
#81754 = VERTEX_POINT ( 'NONE', #127306 ) ;
#81755 = CIRCLE ( 'NONE', #65222, 2.599999999999998312 ) ;
#81756 = ORIENTED_EDGE ( 'NONE', *, *, #38611, .T. ) ;
#81757 = FACE_OUTER_BOUND ( 'NONE', #9045, .T. ) ;
#81758 = ORIENTED_EDGE ( 'NONE', *, *, #104557, .F. ) ;
#81759 = EDGE_CURVE ( 'NONE', #40685, #214000, #97994, .T. ) ;
#81761 = AXIS2_PLACEMENT_3D ( 'NONE', #58208, #38673, #240726 ) ;
#81760 = CARTESIAN_POINT ( 'NONE',  ( -23.25000000000000000, -11.74999999998884448, -134.0000000000000000 ) ) ;
#81762 = DIRECTION ( 'NONE',  ( 0.000000000000000000, -1.000000000000000000, -6.982962677686267499E-15 ) ) ;
#81764 = CYLINDRICAL_SURFACE ( 'NONE', #111965, 0.1000000000000124678 ) ;
#81763 = PRODUCT_DEFINITION_CONTEXT ( 'detailed design', #139160, 'design' ) ;
#81765 = DIRECTION ( 'NONE',  ( 0.000000000000000000, -7.026728003956683390E-15, 1.000000000000000000 ) ) ;
#81766 = AXIS2_PLACEMENT_3D ( 'NONE', #115402, #54140, #213208 ) ;
#81767 = CARTESIAN_POINT ( 'NONE',  ( -16.87333278164147643, 66.11739021543357353, -156.8899396783708369 ) ) ;
#81768 = B_SPLINE_CURVE_WITH_KNOTS ( 'NONE', 3,
 ( #114378, #213472, #193930, #174408 ),
 .UNSPECIFIED., .F., .F.,
 ( 4, 4 ),
 ( 0.000000000000000000, 0.0002118541922231925311 ),
 .UNSPECIFIED. ) ;
#81769 = LINE ( 'NONE', #124793, #95999 ) ;
#81770 = AXIS2_PLACEMENT_3D ( 'NONE', #6688, #86200, #247872 ) ;
#81771 = CARTESIAN_POINT ( 'NONE',  ( 23.14999999999998437, 80.05000000001213323, -136.5231074845242460 ) ) ;
#81772 = DIRECTION ( 'NONE',  ( 1.000000000000000000, 0.000000000000000000, 0.000000000000000000 ) ) ;
#81774 = ORIENTED_EDGE ( 'NONE', *, *, #11028, .T. ) ;
#81773 = LINE ( 'NONE', #160088, #185908 ) ;
#81775 = EDGE_LOOP ( 'NONE', ( #246688, #74566, #117879, #96072 ) ) ;
#81777 = DIRECTION ( 'NONE',  ( 0.000000000000000000, -0.000000000000000000, 1.000000000000000000 ) ) ;
#81776 = CARTESIAN_POINT ( 'NONE',  ( 22.59999999999999432, 0.1008583690987118475, 11.74956712348939547 ) ) ;
#81778 = B_SPLINE_CURVE_WITH_KNOTS ( 'NONE', 3,
 ( #191885, #129311, #14528, #112331, #232289, #168488, #48481, #70655, #207582, #53631, #113600, #211419, #130582, #92738, #251821, #212712, #151463, #73221, #34105, #208850, #150176, #133167 ),
 .UNSPECIFIED., .F., .F.,
 ( 4, 3, 3, 3, 3, 3, 3, 4 ),
 ( 0.000000000000000000, 7.307836821082208987E-06, 4.161455748548728312E-05, 7.576591810647690176E-05, 0.0001098090429817481030, 0.0001438003617351081207, 0.0001777914035423621027, 0.0002117966137402666057 ),
 .UNSPECIFIED. ) ;
#81779 = VERTEX_POINT ( 'NONE', #222532 ) ;
#81780 = VERTEX_POINT ( 'NONE', #43916 ) ;
#81781 = FACE_OUTER_BOUND ( 'NONE', #9706, .T. ) ;
#81782 = DIRECTION ( 'NONE',  ( -1.000000000000000000, 1.207181226542539700E-16, -2.694675058168174199E-16 ) ) ;
#81783 = CARTESIAN_POINT ( 'NONE',  ( -21.05000000000000071, 2.859758780633683273, -208.6670499591424459 ) ) ;
#81785 = FACE_OUTER_BOUND ( 'NONE', #98932, .T. ) ;
#81784 = AXIS2_PLACEMENT_3D ( 'NONE', #154455, #233950, #90575 ) ;
#81786 = CARTESIAN_POINT ( 'NONE',  ( -23.25000000000000000, 25.94586868676353575, -241.5435999122864530 ) ) ;
#81787 = CARTESIAN_POINT ( 'NONE',  ( -23.25000000000000355, 5.650000000011139001, -176.7499999999999716 ) ) ;
#81789 = ORIENTED_EDGE ( 'NONE', *, *, #212001, .T. ) ;
#81788 = EDGE_CURVE ( 'NONE', #221948, #185034, #123458, .T. ) ;
#81790 = ORIENTED_EDGE ( 'NONE', *, *, #52488, .T. ) ;
#81791 = DIRECTION ( 'NONE',  ( 0.000000000000000000, 1.000000000000000000, 0.000000000000000000 ) ) ;
#81792 = VECTOR ( 'NONE', #83893, 1000.000000000000000 ) ;
#81793 = AXIS2_PLACEMENT_3D ( 'NONE', #172800, #67230, #146738 ) ;
#81794 = ADVANCED_FACE ( 'NONE', ( #90730 ), #32083, .T. ) ;
#81795 = EDGE_LOOP ( 'NONE', ( #176421, #94266, #215421, #191904 ) ) ;
#81796 = AXIS2_PLACEMENT_3D ( 'NONE', #12269, #209150, #30546 ) ;
#81798 = FACE_OUTER_BOUND ( 'NONE', #208685, .T. ) ;
#81797 = AXIS2_PLACEMENT_3D ( 'NONE', #128819, #188776, #20432 ) ;
#81799 = EDGE_LOOP ( 'NONE', ( #165650, #171674, #3627, #73679, #66419 ) ) ;
#81800 = FACE_OUTER_BOUND ( 'NONE', #191061, .T. ) ;
#81801 = CARTESIAN_POINT ( 'NONE',  ( 22.50000000000000000, 75.90000000001202807, -114.7731074845243029 ) ) ;
#81802 = CARTESIAN_POINT ( 'NONE',  ( -21.14999999999999858, 76.00000000001271871, -210.0637644362255969 ) ) ;
#81803 = VERTEX_POINT ( 'NONE', #210692 ) ;
#81804 = DIRECTION ( 'NONE',  ( 0.000000000000000000, -0.000000000000000000, -1.000000000000000000 ) ) ;
#81805 = ORIENTED_EDGE ( 'NONE', *, *, #99994, .T. ) ;
#81806 = DIRECTION ( 'NONE',  ( 1.000000000000000000, 0.000000000000000000, 0.000000000000000000 ) ) ;
#81807 = LINE ( 'NONE', #161405, #139670 ) ;
#81808 = CYLINDRICAL_SURFACE ( 'NONE', #54861, 0.1000000000000038219 ) ;
#81809 = AXIS2_PLACEMENT_3D ( 'NONE', #22726, #18842, #57952 ) ;
#81810 = CARTESIAN_POINT ( 'NONE',  ( -2.995603634470891112E-16, 69.35000000001180354, -81.87310748452435405 ) ) ;
#81811 = EDGE_CURVE ( 'NONE', #25443, #236903, #174755, .T. ) ;
#81812 = VERTEX_POINT ( 'NONE', #94588 ) ;
#81813 = CIRCLE ( 'NONE', #36077, 0.09999999999999939493 ) ;
#81815 = CARTESIAN_POINT ( 'NONE',  ( -21.64999999999999858, 63.34400729675436281, -222.1083394899400503 ) ) ;
#81814 = AXIS2_PLACEMENT_3D ( 'NONE', #199586, #60026, #5171 ) ;
#81816 = ORIENTED_EDGE ( 'NONE', *, *, #10764, .F. ) ;
#81819 = ORIENTED_EDGE ( 'NONE', *, *, #142843, .F. ) ;
#81818 = CARTESIAN_POINT ( 'NONE',  ( 21.05000000000000071, 6.540656951712400691, -67.10000000000005116 ) ) ;
#81817 = CARTESIAN_POINT ( 'NONE',  ( 18.49351773456738357, 47.07696351123693290, -255.2313122348375316 ) ) ;
#81820 = LINE ( 'NONE', #240941, #85306 ) ;
#81821 = ORIENTED_EDGE ( 'NONE', *, *, #103532, .F. ) ;
#81822 = CYLINDRICAL_SURFACE ( 'NONE', #112692, 0.09999999999999939493 ) ;
#81823 = CIRCLE ( 'NONE', #61006, 0.1000000000000054040 ) ;
#81824 = VERTEX_POINT ( 'NONE', #228982 ) ;
#81825 = CARTESIAN_POINT ( 'NONE',  ( 18.33683296300455012, 85.51114997114484595, -129.6174000718142736 ) ) ;
#81826 = CARTESIAN_POINT ( 'NONE',  ( 21.05000000000000071, -1.736257131586239844, -179.0686523290174819 ) ) ;
#81828 = ORIENTED_EDGE ( 'NONE', *, *, #144866, .F. ) ;
#81827 = CARTESIAN_POINT ( 'NONE',  ( -18.58671080940900566, 8.966855012152855409, -245.3888429975481813 ) ) ;
#81829 = DIRECTION ( 'NONE',  ( 1.000000000000000000, 0.000000000000000000, 0.000000000000000000 ) ) ;
#81830 = ORIENTED_EDGE ( 'NONE', *, *, #180699, .F. ) ;
#81831 = CARTESIAN_POINT ( 'NONE',  ( 21.14999999999999858, 21.17283678855157802, -243.7231193059830048 ) ) ;
#81832 = CARTESIAN_POINT ( 'NONE',  ( 18.59999999999999432, -1.866714910046153308, -78.75267524628205251 ) ) ;
#81833 = CARTESIAN_POINT ( 'NONE',  ( -15.39946565075091378, 66.61046543766559580, -154.3482981801345204 ) ) ;
#81834 = CIRCLE ( 'NONE', #32019, 10.00000000000000178 ) ;
#81835 = ORIENTED_EDGE ( 'NONE', *, *, #156392, .T. ) ;
#81836 = CARTESIAN_POINT ( 'NONE',  ( -20.64999999999999858, 2.000000000011154189, -46.72462192276210402 ) ) ;
#81837 = ORIENTED_EDGE ( 'NONE', *, *, #112003, .T. ) ;
#81838 = CARTESIAN_POINT ( 'NONE',  ( -21.05000000000000071, 76.00000000001126921, -203.5231074845248997 ) ) ;
#81839 = B_SPLINE_CURVE_WITH_KNOTS ( 'NONE', 3,
 ( #28718, #229443, #42153, #88615, #87340, #29982 ),
 .UNSPECIFIED., .F., .F.,
 ( 4, 2, 4 ),
 ( 0.000000000000000000, 0.0001891491689349495266, 0.0003782983378698990531 ),
 .UNSPECIFIED. ) ;
#81840 = DIRECTION ( 'NONE',  ( 0.000000000000000000, 6.982962677686266711E-15, -1.000000000000000000 ) ) ;
#81841 = FACE_OUTER_BOUND ( 'NONE', #131277, .T. ) ;
#81843 = ORIENTED_EDGE ( 'NONE', *, *, #115538, .T. ) ;
#81842 = DIRECTION ( 'NONE',  ( -0.000000000000000000, 0.000000000000000000, -1.000000000000000000 ) ) ;
#81844 = CARTESIAN_POINT ( 'NONE',  ( -20.64999999999999858, 71.65000000001151648, -48.27310748452435263 ) ) ;
#81845 = EDGE_CURVE ( 'NONE', #206918, #77606, #191484, .T. ) ;
#81846 = LINE ( 'NONE', #178452, #30590 ) ;
#81847 = DIRECTION ( 'NONE',  ( -0.000000000000000000, 0.4721928772777346239, 0.8814952561688430555 ) ) ;
#81848 = EDGE_CURVE ( 'NONE', #112987, #204749, #74792, .T. ) ;
#81849 = ORIENTED_EDGE ( 'NONE', *, *, #180090, .F. ) ;
#81850 = TOROIDAL_SURFACE ( 'NONE', #131960, 0.2000000000000000111, 0.1000000000000000056 ) ;
#81851 = CARTESIAN_POINT ( 'NONE',  ( -18.59999999999999787, 42.98415524044398950, -233.9519173640448173 ) ) ;
#81852 = DIRECTION ( 'NONE',  ( 0.000000000000000000, 0.000000000000000000, -1.000000000000000000 ) ) ;
#81853 = EDGE_LOOP ( 'NONE', ( #256872, #140046, #4828, #215321 ) ) ;
#81854 = CARTESIAN_POINT ( 'NONE',  ( -22.00411653889203834, 65.23707900167231344, -242.8297538143244481 ) ) ;
#81855 = VECTOR ( 'NONE', #159254, 1000.000000000000000 ) ;
#81856 = AXIS2_PLACEMENT_3D ( 'NONE', #172746, #116579, #35778 ) ;
#81857 = VERTEX_POINT ( 'NONE', #154606 ) ;
#81858 = ORIENTED_EDGE ( 'NONE', *, *, #158963, .F. ) ;
#81859 = AXIS2_PLACEMENT_3D ( 'NONE', #237593, #158100, #135897 ) ;
#81860 = ADVANCED_FACE ( 'NONE', ( #232846 ), #136210, .F. ) ;
#81861 = CARTESIAN_POINT ( 'NONE',  ( -21.05000000000000071, 46.53760404070597900, -243.0973507280067167 ) ) ;
#81862 = VERTEX_POINT ( 'NONE', #129859 ) ;
#81864 = ORIENTED_EDGE ( 'NONE', *, *, #215891, .T. ) ;
#81863 = DIRECTION ( 'NONE',  ( -0.000000000000000000, 6.982962677686266711E-15, -1.000000000000000000 ) ) ;
#81865 = EDGE_CURVE ( 'NONE', #39697, #156342, #62266, .T. ) ;
#81866 = EDGE_CURVE ( 'NONE', #64185, #54287, #149782, .T. ) ;
#81869 = ORIENTED_EDGE ( 'NONE', *, *, #221857, .T. ) ;
#81868 = ORIENTED_EDGE ( 'NONE', *, *, #61182, .F. ) ;
#81867 = CARTESIAN_POINT ( 'NONE',  ( 20.94999999999999929, 28.58935552370083144, -258.2621935127861548 ) ) ;
#81870 = CARTESIAN_POINT ( 'NONE',  ( -21.07928932188134041, 0.09889514566555068775, -161.1714833436066669 ) ) ;
#81871 = DIRECTION ( 'NONE',  ( 4.504528286903032433E-15, -0.1298341882520124002, -0.9915357197604841577 ) ) ;
#81872 = EDGE_CURVE ( 'NONE', #69378, #96547, #183084, .T. ) ;
#81873 = CARTESIAN_POINT ( 'NONE',  ( 23.14999999999999503, 11.65000000000000746, -12.15000000000000036 ) ) ;
#81874 = DIRECTION ( 'NONE',  ( 0.000000000000000000, 0.000000000000000000, -1.000000000000000000 ) ) ;
#81875 = VECTOR ( 'NONE', #36872, 1000.000000000000000 ) ;
#81876 = CARTESIAN_POINT ( 'NONE',  ( 23.15000000000000213, -11.64999999998883595, -97.40000000000004832 ) ) ;
#81877 = DIRECTION ( 'NONE',  ( 2.557131231893036492E-16, -0.8496786552930076786, -0.5273008465188218086 ) ) ;
#81879 = DIRECTION ( 'NONE',  ( 0.000000000000000000, 0.1568667991644355497, -0.9876197685951332295 ) ) ;
#81878 = FACE_OUTER_BOUND ( 'NONE', #213215, .T. ) ;
#81880 = VECTOR ( 'NONE', #74845, 1000.000000000000000 ) ;
#81881 = ORIENTED_EDGE ( 'NONE', *, *, #167829, .F. ) ;
#81882 = ORIENTED_EDGE ( 'NONE', *, *, #220677, .F. ) ;
#81883 = CARTESIAN_POINT ( 'NONE',  ( 20.94999999999999929, 1.115600667400684642E-11, -169.4000000000000625 ) ) ;
#81885 = ORIENTED_EDGE ( 'NONE', *, *, #91262, .T. ) ;
#81884 = CARTESIAN_POINT ( 'NONE',  ( 13.99999999999999822, 9.850000000011137402, -83.75000000000004263 ) ) ;
#81886 = ORIENTED_EDGE ( 'NONE', *, *, #204811, .F. ) ;
#81887 = ADVANCED_FACE ( 'NONE', ( #110305 ), #237252, .T. ) ;
#81888 = CARTESIAN_POINT ( 'NONE',  ( 13.99999999999999822, 66.15000000001185754, -86.27310748452437394 ) ) ;
#81889 = ORIENTED_EDGE ( 'NONE', *, *, #148382, .T. ) ;
#81890 = DIRECTION ( 'NONE',  ( -1.000000000000000000, 0.000000000000000000, 0.000000000000000000 ) ) ;
#81891 = AXIS2_PLACEMENT_3D ( 'NONE', #30656, #151892, #52748 ) ;
#81892 = ORIENTED_EDGE ( 'NONE', *, *, #57923, .F. ) ;
#81893 = CARTESIAN_POINT ( 'NONE',  ( 20.04142135623730070, 31.44980407958351165, -233.5445995079518866 ) ) ;
#81896 = ORIENTED_EDGE ( 'NONE', *, *, #165133, .F. ) ;
#81895 = ORIENTED_EDGE ( 'NONE', *, *, #100693, .F. ) ;
#81894 = CIRCLE ( 'NONE', #119365, 3.970710678118657189 ) ;
#81897 = VERTEX_POINT ( 'NONE', #191155 ) ;
#81898 = DIRECTION ( 'NONE',  ( -1.000000000000000000, 0.000000000000000000, 0.000000000000000000 ) ) ;
#81899 = VECTOR ( 'NONE', #129480, 1000.000000000000114 ) ;
#81900 = ORIENTED_EDGE ( 'NONE', *, *, #113708, .F. ) ;
#81901 = AXIS2_PLACEMENT_3D ( 'NONE', #235377, #56710, #136258 ) ;
#81902 = ORIENTED_EDGE ( 'NONE', *, *, #159256, .F. ) ;
#81903 = DIRECTION ( 'NONE',  ( 1.000000000000000000, 3.265361837132813093E-16, -0.000000000000000000 ) ) ;
#81905 = ORIENTED_EDGE ( 'NONE', *, *, #234578, .F. ) ;
#81904 = CARTESIAN_POINT ( 'NONE',  ( 18.48197441911674588, -9.517954794694565734, -107.3902116422077313 ) ) ;
#81907 = DIRECTION ( 'NONE',  ( 0.000000000000000000, 0.8814952561688476074, -0.4721928772777262417 ) ) ;
#81906 = DIRECTION ( 'NONE',  ( 1.000000000000000000, 7.304098846218134667E-16, 0.000000000000000000 ) ) ;
#81908 = FACE_OUTER_BOUND ( 'NONE', #193786, .T. ) ;
#81909 = DIRECTION ( 'NONE',  ( 1.000000000000000000, -7.304098846218134667E-16, -5.100424963727256530E-30 ) ) ;
#81910 = CARTESIAN_POINT ( 'NONE',  ( -18.59999999999999787, 85.40000000001187175, -96.14106563635156988 ) ) ;
#81911 = ORIENTED_EDGE ( 'NONE', *, *, #49390, .T. ) ;
#81912 = ORIENTED_EDGE ( 'NONE', *, *, #170106, .T. ) ;
#81913 = DIRECTION ( 'NONE',  ( 0.000000000000000000, -0.2128009952263603677, 0.9770955615653313941 ) ) ;
#81914 = DIRECTION ( 'NONE',  ( 0.000000000000000000, 0.9908441862701605762, -0.1350103645451835310 ) ) ;
#81915 = DIRECTION ( 'NONE',  ( -2.252264143451594314E-15, 0.1298341882520054891, 0.9915357197604850459 ) ) ;
#81916 = EDGE_LOOP ( 'NONE', ( #108491, #255816, #177903, #175111 ) ) ;
#81917 = DIRECTION ( 'NONE',  ( 0.000000000000000000, 0.4721928772777346239, 0.8814952561688430555 ) ) ;
#81918 = ADVANCED_FACE ( 'NONE', ( #55435 ), #253782, .T. ) ;
#81919 = CARTESIAN_POINT ( 'NONE',  ( -18.59999999999999787, 13.71992543034163958, -238.5823796952984992 ) ) ;
#81920 = FACE_OUTER_BOUND ( 'NONE', #122011, .T. ) ;
#81921 = ORIENTED_EDGE ( 'NONE', *, *, #243178, .T. ) ;
#81922 = ORIENTED_EDGE ( 'NONE', *, *, #8284, .F. ) ;
#81923 = CARTESIAN_POINT ( 'NONE',  ( -21.05000000000000071, 1.162701749949165642, -142.1000000000000227 ) ) ;
#81924 = DIRECTION ( 'NONE',  ( 0.7071067811865474617, -0.6824534298470372740, 0.1850873201762209819 ) ) ;
#81925 = ORIENTED_EDGE ( 'NONE', *, *, #21664, .F. ) ;
#81926 = FACE_OUTER_BOUND ( 'NONE', #200293, .T. ) ;
#81927 = ORIENTED_EDGE ( 'NONE', *, *, #69706, .T. ) ;
#81928 = DIRECTION ( 'NONE',  ( 0.000000000000000000, -6.938893903907222067E-15, 1.000000000000000000 ) ) ;
#81930 = EDGE_CURVE ( 'NONE', #100083, #194844, #9923, .T. ) ;
#81929 = FACE_OUTER_BOUND ( 'NONE', #94512, .T. ) ;
#81932 = CARTESIAN_POINT ( 'NONE',  ( -20.87600722750343252, 68.10911674539558192, -224.1414149070238864 ) ) ;
#81931 = DIRECTION ( 'NONE',  ( -0.7071067811865474617, -0.7071067811865474617, -0.000000000000000000 ) ) ;
#81933 = AXIS2_PLACEMENT_3D ( 'NONE', #7128, #231348, #226149 ) ;
#81934 = DIRECTION ( 'NONE',  ( 1.000000000000000000, 0.000000000000000000, 0.000000000000000000 ) ) ;
#81935 = AXIS2_PLACEMENT_3D ( 'NONE', #187108, #72289, #130966 ) ;
#81936 = DIRECTION ( 'NONE',  ( 4.504528286903032433E-15, -0.1298341882520124002, -0.9915357197604841577 ) ) ;
#81937 = EDGE_CURVE ( 'NONE', #232261, #69456, #12913, .T. ) ;
#81939 = EDGE_CURVE ( 'NONE', #22794, #147164, #78864, .T. ) ;
#81938 = VECTOR ( 'NONE', #164729, 1000.000000000000000 ) ;
#81940 = VECTOR ( 'NONE', #24615, 1000.000000000000000 ) ;
#81941 = EDGE_LOOP ( 'NONE', ( #242641, #12200, #165515, #22620 ) ) ;
#81942 = CARTESIAN_POINT ( 'NONE',  ( 22.47071067811865319, -1.546016791165055304, -193.4356622592196970 ) ) ;
#81944 = EDGE_LOOP ( 'NONE', ( #50053, #13292, #107213 ) ) ;
#81943 = ORIENTED_EDGE ( 'NONE', *, *, #56019, .F. ) ;
#81945 = ORIENTED_EDGE ( 'NONE', *, *, #145996, .T. ) ;
#81946 = ORIENTED_EDGE ( 'NONE', *, *, #102220, .F. ) ;
#81947 = CARTESIAN_POINT ( 'NONE',  ( -16.89268316805466341, 66.04827818677011919, -157.3788599630699707 ) ) ;
#81948 = CARTESIAN_POINT ( 'NONE',  ( -22.45305610364635385, 76.10085836911046897, -81.27267460801373034 ) ) ;
#81949 = DIRECTION ( 'NONE',  ( 1.000000000000000000, 7.304098846218134667E-16, -0.000000000000000000 ) ) ;
#81950 = DIRECTION ( 'NONE',  ( 0.000000000000000000, -0.9770955615653548199, -0.2128009952262535920 ) ) ;
#81951 = CARTESIAN_POINT ( 'NONE',  ( 18.59999999999998721, 19.88098775990103562, -199.0038892813511779 ) ) ;
#81952 = EDGE_CURVE ( 'NONE', #198456, #95913, #49793, .T. ) ;
#81954 = CARTESIAN_POINT ( 'NONE',  ( 20.95512820512820085, 58.98414156600839675, -225.6766266970810193 ) ) ;
#81953 = CARTESIAN_POINT ( 'NONE',  ( 20.50589344625226929, 10.48318793147603145, -7.572994978672304534 ) ) ;
#81956 = ORIENTED_EDGE ( 'NONE', *, *, #59661, .T. ) ;
#81955 = DIRECTION ( 'NONE',  ( 0.000000000000000000, 0.000000000000000000, -1.000000000000000000 ) ) ;
#81957 = FACE_OUTER_BOUND ( 'NONE', #184185, .T. ) ;
#81958 = ORIENTED_EDGE ( 'NONE', *, *, #243645, .F. ) ;
#81959 = ADVANCED_FACE ( 'NONE', ( #58014 ), #37212, .F. ) ;
#81960 = PLANE ( 'NONE',  #221677 ) ;
#81961 = ORIENTED_EDGE ( 'NONE', *, *, #7633, .T. ) ;
#81962 = VERTEX_POINT ( 'NONE', #256171 ) ;
#81963 = CARTESIAN_POINT ( 'NONE',  ( 20.94999999999999929, 64.35000000001146248, -42.80697314750249660 ) ) ;
#81964 = VECTOR ( 'NONE', #40420, 1000.000000000000000 ) ;
#81965 = DIRECTION ( 'NONE',  ( 0.000000000000000000, 0.000000000000000000, -1.000000000000000000 ) ) ;
#81966 = DIRECTION ( 'NONE',  ( 0.000000000000000000, 0.000000000000000000, 1.000000000000000000 ) ) ;
#81967 = DIRECTION ( 'NONE',  ( -0.000000000000000000, 0.9126074666063770380, 0.4088369013363281068 ) ) ;
#81968 = B_SPLINE_CURVE_WITH_KNOTS ( 'NONE', 3,
 ( #161565, #241102, #203232, #104110, #62451, #6304 ),
 .UNSPECIFIED., .F., .F.,
 ( 4, 2, 4 ),
 ( 0.000000000000000000, 0.0002113392456166052376, 0.0004226784912332104752 ),
 .UNSPECIFIED. ) ;
#81969 = AXIS2_PLACEMENT_3D ( 'NONE', #250732, #72119, #132081 ) ;
#81970 = CARTESIAN_POINT ( 'NONE',  ( 20.73486653747088582, 63.54522198573869929, -221.7484608313106094 ) ) ;
#81971 = ORIENTED_EDGE ( 'NONE', *, *, #186669, .F. ) ;
#81972 = ORIENTED_EDGE ( 'NONE', *, *, #205128, .F. ) ;
#81973 = EDGE_CURVE ( 'NONE', #219363, #222383, #87192, .T. ) ;
#81974 = CARTESIAN_POINT ( 'NONE',  ( 20.73486653747088226, 68.75000000001183764, -90.37310748452435405 ) ) ;
#81976 = ORIENTED_EDGE ( 'NONE', *, *, #66088, .F. ) ;
#81975 = ADVANCED_FACE ( 'NONE', ( #219673 ), #1900, .F. ) ;
#81977 = CARTESIAN_POINT ( 'NONE',  ( -21.14999999999999858, 64.25000000001165290, -69.42310748452440805 ) ) ;
#81978 = DIRECTION ( 'NONE',  ( -1.000000000000000000, 0.000000000000000000, 0.000000000000000000 ) ) ;
#81979 = ADVANCED_FACE ( 'NONE', ( #217090 ), #20212, .F. ) ;
#81980 = DIRECTION ( 'NONE',  ( 0.000000000000000000, -0.9651348961777157509, 0.2617529984165031243 ) ) ;
#81981 = DIRECTION ( 'NONE',  ( 1.000000000000000000, 0.000000000000000000, 0.000000000000000000 ) ) ;
#81982 = DIRECTION ( 'NONE',  ( -0.000000000000000000, 1.000000000000000000, 6.982962677686266711E-15 ) ) ;
#81983 = CARTESIAN_POINT ( 'NONE',  ( 20.94999999999999929, -3.770473190032740174, -225.9805569534692324 ) ) ;
#81984 = DIRECTION ( 'NONE',  ( 1.000000000000000000, 0.000000000000000000, 0.000000000000000000 ) ) ;
#81985 = DIRECTION ( 'NONE',  ( 0.000000000000000000, 0.9876197685951252359, -0.1568667991644863424 ) ) ;
#81986 = FACE_OUTER_BOUND ( 'NONE', #229020, .T. ) ;
#81987 = FACE_OUTER_BOUND ( 'NONE', #81581, .T. ) ;
#81988 = CIRCLE ( 'NONE', #40374, 0.09999999999998898659 ) ;
#81990 = AXIS2_PLACEMENT_3D ( 'NONE', #193308, #96732, #216708 ) ;
#81989 = PLANE ( 'NONE',  #186277 ) ;
#81991 = VECTOR ( 'NONE', #2936, 1000.000000000000000 ) ;
#81992 = TOROIDAL_SURFACE ( 'NONE', #77913, 0.2000000000000000111, 0.1000000000000000056 ) ;
#81993 = VERTEX_POINT ( 'NONE', #80131 ) ;
#81994 = CARTESIAN_POINT ( 'NONE',  ( -16.89081410710458542, 30.21083495796404250, -234.8079631709592832 ) ) ;
#81995 = VERTEX_POINT ( 'NONE', #159721 ) ;
#81996 = DIRECTION ( 'NONE',  ( 0.000000000000000000, -1.000000000000000000, 0.000000000000000000 ) ) ;
#81997 = FACE_OUTER_BOUND ( 'NONE', #159066, .T. ) ;
#81998 = CARTESIAN_POINT ( 'NONE',  ( 23.14999999999998437, 76.00000000001213607, -136.5231074845242745 ) ) ;
#81999 = ORIENTED_EDGE ( 'NONE', *, *, #121340, .T. ) ;
#82000 = EDGE_CURVE ( 'NONE', #214701, #140884, #70674, .T. ) ;
#82001 = DIRECTION ( 'NONE',  ( 1.000000000000000000, -0.000000000000000000, -3.469446951953515108E-14 ) ) ;
#82002 = CIRCLE ( 'NONE', #102278, 1.500000000000001332 ) ;
#82003 = CARTESIAN_POINT ( 'NONE',  ( 22.59999999999999787, 64.35042919246686210, -69.62310748452439668 ) ) ;
#82004 = CARTESIAN_POINT ( 'NONE',  ( 23.14999999999999858, 28.52545328903799415, -239.5221046041717443 ) ) ;
#82005 = AXIS2_PLACEMENT_3D ( 'NONE', #169296, #248802, #70182 ) ;
#82006 = AXIS2_PLACEMENT_3D ( 'NONE', #26915, #2165, #102529 ) ;
#82007 = DIRECTION ( 'NONE',  ( 0.000000000000000000, 0.000000000000000000, -1.000000000000000000 ) ) ;
#82008 = CARTESIAN_POINT ( 'NONE',  ( -16.93211319090181632, 9.999986781168624717, -121.4225054992731003 ) ) ;
#82009 = DIRECTION ( 'NONE',  ( 0.000000000000000000, 7.086529944415894657E-15, -1.000000000000000000 ) ) ;
#82010 = CIRCLE ( 'NONE', #215315, 0.09999999999998898659 ) ;
#82011 = VERTEX_POINT ( 'NONE', #200128 ) ;
#82012 = DIRECTION ( 'NONE',  ( 2.978066053179066272E-16, 1.000000000000000000, 9.529811370173012070E-15 ) ) ;
#82014 = ORIENTED_EDGE ( 'NONE', *, *, #132726, .F. ) ;
#82013 = LINE ( 'NONE', #84565, #13725 ) ;
#82015 = CARTESIAN_POINT ( 'NONE',  ( 20.73486653747088582, 11.52084357182978458, -219.8296352432475658 ) ) ;
#82016 = ADVANCED_FACE ( 'NONE', ( #215807 ), #235383, .T. ) ;
#82017 = CARTESIAN_POINT ( 'NONE',  ( -21.05000000000000071, 1.162701749949165642, -75.10000000000003695 ) ) ;
#82018 = DIRECTION ( 'NONE',  ( 0.000000000000000000, 0.8814952561688437216, -0.4721928772777331806 ) ) ;
#82019 = ORIENTED_EDGE ( 'NONE', *, *, #164477, .F. ) ;
#82020 = DIRECTION ( 'NONE',  ( 1.000000000000000000, -0.000000000000000000, -0.000000000000000000 ) ) ;
#82021 = EDGE_CURVE ( 'NONE', #209722, #15820, #100967, .T. ) ;
#82022 = APPLICATION_PROTOCOL_DEFINITION ( 'draft international standard', 'automotive_design', 1998, #202408 ) ;
#82023 = CYLINDRICAL_SURFACE ( 'NONE', #13222, 0.09999999999999939493 ) ;
#82024 = ORIENTED_EDGE ( 'NONE', *, *, #103176, .F. ) ;
#82026 = ADVANCED_FACE ( 'NONE', ( #214537, #35931 ), #195006, .T. ) ;
#82025 = FACE_OUTER_BOUND ( 'NONE', #224880, .T. ) ;
#82027 = CARTESIAN_POINT ( 'NONE',  ( -20.94999999999999929, 86.30329675166747450, -209.4258251677035787 ) ) ;
#82028 = ADVANCED_FACE ( 'NONE', ( #38484 ), #254892, .F. ) ;
#82029 = ADVANCED_FACE ( 'NONE', ( #118012 ), #56717, .F. ) ;
#82030 = DIRECTION ( 'NONE',  ( -1.000000000000000000, 0.000000000000000000, -0.000000000000000000 ) ) ;
#82031 = EDGE_LOOP ( 'NONE', ( #175471, #210508, #232708, #195799 ) ) ;
#82032 = EDGE_LOOP ( 'NONE', ( #39309, #96760, #121314, #109501 ) ) ;
#82033 = CARTESIAN_POINT ( 'NONE',  ( 23.24999999999999645, 5.649999999999983480, -20.84999999999999432 ) ) ;
#82034 = VECTOR ( 'NONE', #173182, 1000.000000000000000 ) ;
#82035 = FACE_OUTER_BOUND ( 'NONE', #246227, .T. ) ;
#82036 = DIRECTION ( 'NONE',  ( -0.7071067811865475727, -0.7071067811865475727, 0.000000000000000000 ) ) ;
#82037 = CARTESIAN_POINT ( 'NONE',  ( -23.15000000000000213, 11.65000000001115588, -88.35000000000003695 ) ) ;
#82038 = CARTESIAN_POINT ( 'NONE',  ( -21.05000000000000071, 1.261786168576181755, -142.0864989635454947 ) ) ;
#82041 = FACE_OUTER_BOUND ( 'NONE', #32350, .T. ) ;
#82040 = AXIS2_PLACEMENT_3D ( 'NONE', #112581, #210401, #113852 ) ;
#82039 = CARTESIAN_POINT ( 'NONE',  ( -21.05000000000000071, 87.48912529308822172, -139.5231074845243029 ) ) ;
#82042 = LINE ( 'NONE', #181202, #7063 ) ;
#82043 = DIRECTION ( 'NONE',  ( 0.000000000000000000, 0.000000000000000000, -1.000000000000000000 ) ) ;
#82044 = CARTESIAN_POINT ( 'NONE',  ( 23.14999999999999858, 0.000000000000000000, -33.50000000000000000 ) ) ;
#82045 = CARTESIAN_POINT ( 'NONE',  ( -16.86379686415369861, 9.975217759264314310, -146.5666101109097497 ) ) ;
#82046 = AXIS2_PLACEMENT_3D ( 'NONE', #119684, #21859, #59666 ) ;
#82047 = VERTEX_POINT ( 'NONE', #39798 ) ;
#82048 = AXIS2_PLACEMENT_3D ( 'NONE', #163414, #242932, #223363 ) ;
#82049 = ADVANCED_FACE ( 'NONE', ( #176723 ), #25363, .F. ) ;
#82050 = ORIENTED_EDGE ( 'NONE', *, *, #192, .F. ) ;
#82051 = CARTESIAN_POINT ( 'NONE',  ( 20.94999999999999929, 76.00000000001190870, -103.0231074845243029 ) ) ;
#82052 = EDGE_CURVE ( 'NONE', #88561, #153107, #33264, .T. ) ;
#82053 = CARTESIAN_POINT ( 'NONE',  ( -20.94999999999999929, 87.75000000001236344, -167.1231074845242688 ) ) ;
#82055 = CARTESIAN_POINT ( 'NONE',  ( 21.13920837816993270, 67.21675294989267968, -191.2731074845244166 ) ) ;
#82054 = CARTESIAN_POINT ( 'NONE',  ( -18.50000000000000000, 69.15387683765929694, -99.28538121767448388 ) ) ;
#82056 = PRODUCT_DEFINITION_FORMATION_WITH_SPECIFIED_SOURCE ( 'ANY', '', #68063, .NOT_KNOWN. ) ;
#82057 = AXIS2_PLACEMENT_3D ( 'NONE', #155748, #78722, #115295 ) ;
#82058 = CARTESIAN_POINT ( 'NONE',  ( -33.72168855820452649, 26.68086916408615750, -212.3318337774905160 ) ) ;
#82060 = EDGE_CURVE ( 'NONE', #101850, #20227, #143986, .T. ) ;
#82059 = DIRECTION ( 'NONE',  ( 0.000000000000000000, 0.2128009952263598958, -0.9770955615653316162 ) ) ;
#82061 = CIRCLE ( 'NONE', #252766, 4.000000000000002665 ) ;
#82062 = DIRECTION ( 'NONE',  ( 2.952720810173289112E-16, -1.000000000000000000, 0.000000000000000000 ) ) ;
#82063 = EDGE_LOOP ( 'NONE', ( #21566, #108230, #164569, #104281 ) ) ;
#82064 = DIRECTION ( 'NONE',  ( 0.000000000000000000, 0.9910465087640860649, -0.1335171055202901413 ) ) ;
#82065 = VERTEX_POINT ( 'NONE', #184402 ) ;
#82066 = ADVANCED_FACE ( 'NONE', ( #83973 ), #112355, .F. ) ;
#82067 = DIRECTION ( 'NONE',  ( 1.000000000000000000, 0.000000000000000000, 0.000000000000000000 ) ) ;
#82068 = VERTEX_POINT ( 'NONE', #145269 ) ;
#82069 = LINE ( 'NONE', #61258, #109823 ) ;
#82070 = EDGE_CURVE ( 'NONE', #28671, #162629, #66561, .T. ) ;
#82071 = TOROIDAL_SURFACE ( 'NONE', #115413, 12.97499999999999787, 0.1000000000000000056 ) ;
#82072 = AXIS2_PLACEMENT_3D ( 'NONE', #173666, #154092, #254395 ) ;
#82073 = CARTESIAN_POINT ( 'NONE',  ( -22.50000000000000000, 76.00000000001276135, -215.1726782920691505 ) ) ;
#82074 = EDGE_CURVE ( 'NONE', #156363, #213344, #163571, .T. ) ;
#82075 = AXIS2_PLACEMENT_3D ( 'NONE', #132021, #192020, #133315 ) ;
#82077 = ORIENTED_EDGE ( 'NONE', *, *, #225997, .T. ) ;
#82076 = AXIS2_PLACEMENT_3D ( 'NONE', #78608, #57758, #35676 ) ;
#82078 =( BOUNDED_CURVE ( )  B_SPLINE_CURVE ( 3, ( #251689, #73096, #152625, #189152 ),
 .UNSPECIFIED., .F., .F. ) 
 B_SPLINE_CURVE_WITH_KNOTS ( ( 4, 4 ),
 ( 1.570796326794896558, 3.141592653589793116 ),
 .UNSPECIFIED. ) 
 CURVE ( )  GEOMETRIC_REPRESENTATION_ITEM ( )  RATIONAL_B_SPLINE_CURVE ( ( 1.000000000000000000, 0.8047378541243649375, 0.8047378541243649375, 1.000000000000000000 ) ) 
 REPRESENTATION_ITEM ( '' )  );
#82079 = VERTEX_POINT ( 'NONE', #205240 ) ;
#82080 = VECTOR ( 'NONE', #23529, 1000.000000000000000 ) ;
#82081 = LINE ( 'NONE', #241205, #257892 ) ;
#82082 = AXIS2_PLACEMENT_3D ( 'NONE', #235246, #197399, #78726 ) ;
#82083 = ADVANCED_FACE ( 'NONE', ( #104832 ), #202685, .F. ) ;
#82084 = DIRECTION ( 'NONE',  ( -1.000000000000000000, 0.000000000000000000, 0.000000000000000000 ) ) ;
#82085 = CARTESIAN_POINT ( 'NONE',  ( 20.94999999999999929, 69.35000000001222986, -148.7731074845244166 ) ) ;
#82086 = FACE_OUTER_BOUND ( 'NONE', #42128, .T. ) ;
#82087 = CARTESIAN_POINT ( 'NONE',  ( -20.54999999999999716, 67.23127455305841238, -235.8551265064783991 ) ) ;
#82089 = DIRECTION ( 'NONE',  ( 0.000000000000000000, 0.9126074666063770380, 0.4088369013363283289 ) ) ;
#82088 = FACE_OUTER_BOUND ( 'NONE', #171476, .T. ) ;
#82090 = DIRECTION ( 'NONE',  ( 1.000000000000000000, 0.000000000000000000, 0.000000000000000000 ) ) ;
#82092 = ORIENTED_EDGE ( 'NONE', *, *, #40887, .F. ) ;
#82091 = CARTESIAN_POINT ( 'NONE',  ( 20.22516295850462598, 66.10063570456183868, -128.6130417724335473 ) ) ;
#82094 = DIRECTION ( 'NONE',  ( 1.186688945009009831E-16, 1.000000000000000000, 6.982962677686266711E-15 ) ) ;
#82093 = CARTESIAN_POINT ( 'NONE',  ( 18.49999999999998934, 19.85039924724470950, -102.7803030578013903 ) ) ;
#82095 = VERTEX_POINT ( 'NONE', #124451 ) ;
#82097 = EDGE_LOOP ( 'NONE', ( #210211, #208649, #3253, #232976 ) ) ;
#82096 = DIRECTION ( 'NONE',  ( -0.000000000000000000, -0.000000000000000000, 1.000000000000000000 ) ) ;
#82098 = VECTOR ( 'NONE', #183949, 1000.000000000000114 ) ;
#82099 = ORIENTED_EDGE ( 'NONE', *, *, #162146, .F. ) ;
#82100 = CARTESIAN_POINT ( 'NONE',  ( -21.05000000000000071, 87.48912529308798014, -99.92310748452423752 ) ) ;
#82101 = AXIS2_PLACEMENT_3D ( 'NONE', #140703, #258038, #159020 ) ;
#82102 = CYLINDRICAL_SURFACE ( 'NONE', #163661, 0.09999999999999939493 ) ;
#82103 = CARTESIAN_POINT ( 'NONE',  ( -21.05000000000000071, -1.835341550213255957, -179.0551512925629538 ) ) ;
#82104 = ORIENTED_EDGE ( 'NONE', *, *, #164073, .F. ) ;
#82105 = DIRECTION ( 'NONE',  ( 0.5932847527679298016, 0.3291107096594074188, -0.7346423231209712190 ) ) ;
#82106 = DIRECTION ( 'NONE',  ( 1.000000000000000000, -7.304098846218134667E-16, -5.100424963727256530E-30 ) ) ;
#82107 = CARTESIAN_POINT ( 'NONE',  ( 18.46905048506369695, 38.07034010913391597, -261.0545764982895776 ) ) ;
#82108 = DIRECTION ( 'NONE',  ( 1.000000000000000000, 0.000000000000000000, -0.000000000000000000 ) ) ;
#82109 = CARTESIAN_POINT ( 'NONE',  ( -22.39999999999999858, 64.35000000001166143, -69.52310748452438816 ) ) ;
#82110 = AXIS2_PLACEMENT_3D ( 'NONE', #92861, #195852, #211541 ) ;
#82111 = AXIS2_PLACEMENT_3D ( 'NONE', #224654, #51135, #108573 ) ;
#82112 = DIRECTION ( 'NONE',  ( 1.000000000000000000, 0.000000000000000000, 0.000000000000000000 ) ) ;
#82113 = ORIENTED_EDGE ( 'NONE', *, *, #226088, .T. ) ;
#82114 = ORIENTED_EDGE ( 'NONE', *, *, #35563, .F. ) ;
#82115 = LINE ( 'NONE', #162990, #197862 ) ;
#82116 = VERTEX_POINT ( 'NONE', #46176 ) ;
#82117 = CARTESIAN_POINT ( 'NONE',  ( 23.14999999999999858, 76.00000000001213607, -136.5231074845243313 ) ) ;
#82118 = ORIENTED_EDGE ( 'NONE', *, *, #203059, .T. ) ;
#82119 = CARTESIAN_POINT ( 'NONE',  ( -18.50000000000000000, 19.09764897702175546, -235.7051342141560042 ) ) ;
#82120 = AXIS2_PLACEMENT_3D ( 'NONE', #137704, #56868, #140270 ) ;
#82121 = EDGE_CURVE ( 'NONE', #206325, #18470, #166352, .T. ) ;
#82122 = DIRECTION ( 'NONE',  ( 0.000000000000000000, -0.4721928772777344019, -0.8814952561688432775 ) ) ;
#82123 = FACE_OUTER_BOUND ( 'NONE', #148437, .T. ) ;
#82124 = DIRECTION ( 'NONE',  ( 1.000000000000000000, 0.000000000000000000, 0.000000000000000000 ) ) ;
#82125 = VERTEX_POINT ( 'NONE', #86565 ) ;
#82126 = AXIS2_PLACEMENT_3D ( 'NONE', #36380, #37658, #257908 ) ;
#82127 = CIRCLE ( 'NONE', #48827, 0.1000000000000028644 ) ;
#82128 = TOROIDAL_SURFACE ( 'NONE', #107100, 0.2000000000000000111, 0.1000000000000000056 ) ;
#82129 = AXIS2_PLACEMENT_3D ( 'NONE', #199063, #235605, #238169 ) ;
#82130 = CARTESIAN_POINT ( 'NONE',  ( -16.86578989773640913, 66.01519019875374283, -182.5584425979022285 ) ) ;
#82131 = DIRECTION ( 'NONE',  ( 1.000000000000000000, 7.304098846218134667E-16, 5.100424963727256530E-30 ) ) ;
#82133 = EDGE_CURVE ( 'NONE', #179647, #154572, #245673, .T. ) ;
#82132 = CARTESIAN_POINT ( 'NONE',  ( -21.65000000000000213, 21.67479455268075128, -232.7326951115107647 ) ) ;
#82134 = ORIENTED_EDGE ( 'NONE', *, *, #252839, .F. ) ;
#82136 = DIRECTION ( 'NONE',  ( 0.000000000000000000, 6.982962677686266711E-15, -1.000000000000000000 ) ) ;
#82135 = DIRECTION ( 'NONE',  ( -1.000000000000000000, 0.000000000000000000, 0.000000000000000000 ) ) ;
#82137 = EDGE_LOOP ( 'NONE', ( #215344, #112743, #221488, #204243, #10000 ) ) ;
#82140 = ORIENTED_EDGE ( 'NONE', *, *, #8333, .F. ) ;
#82139 = DIRECTION ( 'NONE',  ( 0.000000000000000000, 0.000000000000000000, -1.000000000000000000 ) ) ;
#82138 = DIRECTION ( 'NONE',  ( 0.000000000000000000, 1.000000000000000000, 6.982962677686266711E-15 ) ) ;
#82141 = VECTOR ( 'NONE', #256665, 1000.000000000000000 ) ;
#82142 = ORIENTED_EDGE ( 'NONE', *, *, #38426, .F. ) ;
#82143 = CARTESIAN_POINT ( 'NONE',  ( -20.94999999999999574, 11.62071067812980907, -127.1315833476590740 ) ) ;
#82144 = DIRECTION ( 'NONE',  ( 0.000000000000000000, 0.000000000000000000, 1.000000000000000000 ) ) ;
#82145 = CARTESIAN_POINT ( 'NONE',  ( 20.85000000000000142, 64.35000000001245724, -170.0231074845244166 ) ) ;
#82146 = ORIENTED_EDGE ( 'NONE', *, *, #181856, .F. ) ;
#82147 = CARTESIAN_POINT ( 'NONE',  ( -20.64999999999999858, 84.73084112150785074, -179.6211822035086243 ) ) ;
#82149 = FACE_OUTER_BOUND ( 'NONE', #176973, .T. ) ;
#82148 = CARTESIAN_POINT ( 'NONE',  ( -21.14999999999999858, 6.540656951712397138, -167.4999999999999716 ) ) ;
#82150 = AXIS2_PLACEMENT_3D ( 'NONE', #175963, #92533, #136796 ) ;
#82152 = EDGE_LOOP ( 'NONE', ( #146475, #36918, #250890, #243342, #144771, #35073, #51497, #193491, #140968 ) ) ;
#82151 = DIRECTION ( 'NONE',  ( 0.000000000000000000, 0.9126074666063660468, 0.4088369013363524762 ) ) ;
#82153 = AXIS2_PLACEMENT_3D ( 'NONE', #59600, #40106, #41382 ) ;
#82154 = B_SPLINE_CURVE_WITH_KNOTS ( 'NONE', 3,
 ( #226854, #69087, #209874, #49508, #243847, #206016, #48216, #130309, #26105, #105594 ),
 .UNSPECIFIED., .F., .F.,
 ( 4, 3, 3, 4 ),
 ( 0.000000000000000000, 0.0002000000000008585893, 0.001000000000082977483, 0.001967863649483336721 ),
 .UNSPECIFIED. ) ;
#82155 = ORIENTED_EDGE ( 'NONE', *, *, #23851, .T. ) ;
#82156 = FACE_OUTER_BOUND ( 'NONE', #48988, .T. ) ;
#82157 = CIRCLE ( 'NONE', #136318, 0.09999999999999530098 ) ;
#82158 = DIRECTION ( 'NONE',  ( 1.000000000000000000, 0.000000000000000000, 0.000000000000000000 ) ) ;
#82159 = ORIENTED_EDGE ( 'NONE', *, *, #130853, .F. ) ;
#82160 = CYLINDRICAL_SURFACE ( 'NONE', #168729, 0.1000000000000106914 ) ;
#82161 = VERTEX_POINT ( 'NONE', #67037 ) ;
#82162 = FACE_OUTER_BOUND ( 'NONE', #66291, .T. ) ;
#82163 = CARTESIAN_POINT ( 'NONE',  ( -18.59999999999999787, 68.97833521811203639, -132.6895420826271277 ) ) ;
#82164 = FACE_OUTER_BOUND ( 'NONE', #28345, .T. ) ;
#82165 = EDGE_LOOP ( 'NONE', ( #83843, #163027, #154259 ) ) ;
#82166 = DIRECTION ( 'NONE',  ( 0.000000000000000000, 0.9126074666063771490, 0.4088369013363276627 ) ) ;
#82167 = EDGE_CURVE ( 'NONE', #127120, #135639, #53906, .T. ) ;
#82168 = AXIS2_PLACEMENT_3D ( 'NONE', #174780, #133050, #134297 ) ;
#82169 = CIRCLE ( 'NONE', #28066, 0.2000000000000057288 ) ;
#82170 = FACE_OUTER_BOUND ( 'NONE', #35133, .T. ) ;
#82171 = CIRCLE ( 'NONE', #227961, 0.09999999999999939493 ) ;
#82172 = CIRCLE ( 'NONE', #98730, 0.1000000000000028644 ) ;
#82173 = VERTEX_POINT ( 'NONE', #47448 ) ;
#82174 = EDGE_LOOP ( 'NONE', ( #251328, #59095, #37349, #119789 ) ) ;
#82175 =( BOUNDED_SURFACE ( )  B_SPLINE_SURFACE ( 3, 2, ( 
 ( #158813, #19273, #81776 ),
 ( #98766, #178374, #238311 ),
 ( #239613, #59650, #218734 ),
 ( #179648, #953, #140486 ) ),
 .UNSPECIFIED., .F., .F., .F. ) 
 B_SPLINE_SURFACE_WITH_KNOTS ( ( 4, 4 ),
 ( 3, 3 ),
 ( -2.710505431213761085E-20, 0.0003124336600439507920 ),
 ( 0.000000000000000000, 1.000000000000000000 ),
 .UNSPECIFIED. ) 
 GEOMETRIC_REPRESENTATION_ITEM ( )  RATIONAL_B_SPLINE_SURFACE ( (
 ( 1.000000000000000000, 0.7071067811865536790, 1.000000000000000000),
 ( 1.000000000000000000, 0.7089187706049598914, 1.000000000000000000),
 ( 1.000000000000000000, 0.7039288185052290370, 1.000000000000000000),
 ( 1.000000000000000000, 0.7040654476015686392, 1.000000000000000000) ) ) 
 REPRESENTATION_ITEM ( '' )  SURFACE ( )  );
#82176 = ORIENTED_EDGE ( 'NONE', *, *, #19281, .T. ) ;
#82177 = EDGE_CURVE ( 'NONE', #81993, #250275, #199667, .T. ) ;
#82178 = CARTESIAN_POINT ( 'NONE',  ( 18.49999999999999645, 77.83585931145526615, -58.01866831572577610 ) ) ;
#82179 = ORIENTED_EDGE ( 'NONE', *, *, #2040, .T. ) ;
#82181 = EDGE_LOOP ( 'NONE', ( #254038, #185214, #91899, #189670 ) ) ;
#82180 = CARTESIAN_POINT ( 'NONE',  ( 15.74999999999999645, 66.65000000001258229, -186.7731074845244166 ) ) ;
#82182 = ADVANCED_FACE ( 'NONE', ( #107441 ), #187006, .T. ) ;
#82183 = EDGE_LOOP ( 'NONE', ( #18324, #218962 ) ) ;
#82186 = EDGE_LOOP ( 'NONE', ( #115980, #199710, #56335, #9897 ) ) ;
#82185 = ORIENTED_EDGE ( 'NONE', *, *, #179175, .T. ) ;
#82184 = CARTESIAN_POINT ( 'NONE',  ( 18.39999999999999858, 78.24390740893980478, -231.6169762517609172 ) ) ;
#82187 = AXIS2_PLACEMENT_3D ( 'NONE', #104565, #47167, #66765 ) ;
#82188 = VECTOR ( 'NONE', #76941, 1000.000000000000227 ) ;
#82190 = ADVANCED_FACE ( 'NONE', ( #121886 ), #116454, .F. ) ;
#82189 = VERTEX_POINT ( 'NONE', #243096 ) ;
#82191 = DIRECTION ( 'NONE',  ( 1.000000000000000000, 0.000000000000000000, 0.000000000000000000 ) ) ;
#82192 = DIRECTION ( 'NONE',  ( -0.5735764363510457153, 0.8191520442889921316, 0.000000000000000000 ) ) ;
#82193 = ORIENTED_EDGE ( 'NONE', *, *, #67398, .F. ) ;
#82194 = CARTESIAN_POINT ( 'NONE',  ( -23.25000000000000000, 76.00000000001162448, -65.47310748452431994 ) ) ;
#82196 = ORIENTED_EDGE ( 'NONE', *, *, #10092, .T. ) ;
#82195 = DIRECTION ( 'NONE',  ( 1.000000000000000000, 0.000000000000000000, 0.000000000000000000 ) ) ;
#82197 = LINE ( 'NONE', #240032, #217121 ) ;
#82199 = VERTEX_POINT ( 'NONE', #87853 ) ;
#82198 = DIRECTION ( 'NONE',  ( -1.000000000000000000, 3.151514657663852580E-16, -8.547182517843351137E-17 ) ) ;
#82200 = EDGE_CURVE ( 'NONE', #78926, #144360, #220953, .T. ) ;
#82201 = ORIENTED_EDGE ( 'NONE', *, *, #171140, .F. ) ;
#82202 = DIRECTION ( 'NONE',  ( 1.000000000000000000, -0.000000000000000000, 0.000000000000000000 ) ) ;
#82203 = VERTEX_POINT ( 'NONE', #43624 ) ;
#82204 = VERTEX_POINT ( 'NONE', #82704 ) ;
#82205 = CARTESIAN_POINT ( 'NONE',  ( -16.97683810757273193, 9.950000000011137047, -180.7635767124612300 ) ) ;
#82206 = DIRECTION ( 'NONE',  ( -1.000000000000000000, 0.000000000000000000, 0.000000000000000000 ) ) ;
#82208 = ORIENTED_EDGE ( 'NONE', *, *, #69482, .F. ) ;
#82207 = EDGE_LOOP ( 'NONE', ( #170942, #176637, #181846 ) ) ;
#82209 = ORIENTED_EDGE ( 'NONE', *, *, #86269, .F. ) ;
#82210 = CARTESIAN_POINT ( 'NONE',  ( 21.04999999999908411, 61.94334680800506732, -221.8238859006714279 ) ) ;
#82211 = ORIENTED_EDGE ( 'NONE', *, *, #118886, .T. ) ;
#82212 = ORIENTED_EDGE ( 'NONE', *, *, #150686, .F. ) ;
#82213 = DIRECTION ( 'NONE',  ( 1.000000000000000000, 0.000000000000000000, 0.000000000000000000 ) ) ;
#82215 = ORIENTED_EDGE ( 'NONE', *, *, #123934, .T. ) ;
#82214 = CARTESIAN_POINT ( 'NONE',  ( 18.59999999999999076, 10.90071697730193456, -220.2717246083756208 ) ) ;
#82216 = DIRECTION ( 'NONE',  ( -0.000000000000000000, -0.4721928772777346794, -0.8814952561688431665 ) ) ;
#82217 = CIRCLE ( 'NONE', #115566, 0.1000000000000046685 ) ;
#82219 = DIRECTION ( 'NONE',  ( 1.000000000000000000, 0.000000000000000000, 0.000000000000000000 ) ) ;
#82218 = FACE_OUTER_BOUND ( 'NONE', #158466, .T. ) ;
#82220 = ADVANCED_FACE ( 'NONE', ( #123161 ), #103564, .T. ) ;
#82221 = ORIENTED_EDGE ( 'NONE', *, *, #218554, .T. ) ;
#82223 = ORIENTED_EDGE ( 'NONE', *, *, #81158, .T. ) ;
#82222 = VERTEX_POINT ( 'NONE', #93014 ) ;
#82224 = AXIS2_PLACEMENT_3D ( 'NONE', #200787, #78255, #221604 ) ;
#82225 = LINE ( 'NONE', #219192, #152853 ) ;
#82226 = CARTESIAN_POINT ( 'NONE',  ( 22.39999999999999503, 11.38316329224760892, -198.5208684056144079 ) ) ;
#82227 = ORIENTED_EDGE ( 'NONE', *, *, #193579, .F. ) ;
#82228 = AXIS2_PLACEMENT_3D ( 'NONE', #133483, #95628, #171374 ) ;
#82229 = AXIS2_PLACEMENT_3D ( 'NONE', #121123, #221443, #24578 ) ;
#82230 = ADVANCED_FACE ( 'NONE', ( #14798 ), #241523, .F. ) ;
#82231 = DIRECTION ( 'NONE',  ( 0.000000000000000000, 0.2128009952263604787, -0.9770955615653315052 ) ) ;
#82232 = CIRCLE ( 'NONE', #2961, 0.09999999999999736877 ) ;
#82233 = ORIENTED_EDGE ( 'NONE', *, *, #45262, .T. ) ;
#82234 = ORIENTED_EDGE ( 'NONE', *, *, #59113, .F. ) ;
#82235 = DIRECTION ( 'NONE',  ( 1.000000000000000000, -0.000000000000000000, -0.000000000000000000 ) ) ;
#82236 = CIRCLE ( 'NONE', #103098, 0.09999999999999982514 ) ;
#82237 = VERTEX_POINT ( 'NONE', #249538 ) ;
#82238 = DIRECTION ( 'NONE',  ( 0.000000000000000000, 0.000000000000000000, -1.000000000000000000 ) ) ;
#82239 = CARTESIAN_POINT ( 'NONE',  ( 21.05000000000000071, 76.01681986839764704, -109.3305327040896913 ) ) ;
#82240 = ORIENTED_EDGE ( 'NONE', *, *, #138283, .F. ) ;
#82241 = FACE_OUTER_BOUND ( 'NONE', #111781, .T. ) ;
#82243 = EDGE_CURVE ( 'NONE', #115670, #221119, #228696, .T. ) ;
#82242 = CARTESIAN_POINT ( 'NONE',  ( -18.59999999999999787, 77.83534155023598089, -57.96795619196132776 ) ) ;
#82245 = CARTESIAN_POINT ( 'NONE',  ( 23.24999999999999289, 11.65000000001116298, -21.75000000000000355 ) ) ;
#82244 = DIRECTION ( 'NONE',  ( 0.000000000000000000, 1.000000000000000000, 0.000000000000000000 ) ) ;
#82246 = DIRECTION ( 'NONE',  ( 0.000000000000000000, 0.000000000000000000, -1.000000000000000000 ) ) ;
#82247 = CARTESIAN_POINT ( 'NONE',  ( -6.000000000000002665, -11.75000000000000000, 13.90000000000000213 ) ) ;
#82248 = CARTESIAN_POINT ( 'NONE',  ( -23.25000000000000000, 64.35000000001245724, -181.7731074845244450 ) ) ;
#82249 = CARTESIAN_POINT ( 'NONE',  ( 21.05000000000000426, 76.03753606329787829, -142.8553797584599749 ) ) ;
#82250 = DIRECTION ( 'NONE',  ( -0.000000000000000000, 0.9126074666063769270, 0.4088369013363280513 ) ) ;
#82251 = EDGE_CURVE ( 'NONE', #41250, #165976, #112530, .T. ) ;
#82252 = TOROIDAL_SURFACE ( 'NONE', #244585, 7.800000000000000711, 0.1000000000000000056 ) ;
#82253 = ORIENTED_EDGE ( 'NONE', *, *, #61241, .F. ) ;
#82254 = AXIS2_PLACEMENT_3D ( 'NONE', #178130, #17728, #13909 ) ;
#82257 = ORIENTED_EDGE ( 'NONE', *, *, #23368, .F. ) ;
#82256 = EDGE_LOOP ( 'NONE', ( #229246, #233239, #47079, #102173 ) ) ;
#82255 = CIRCLE ( 'NONE', #165511, 0.1999999999999999833 ) ;
#82258 = VERTEX_POINT ( 'NONE', #252087 ) ;
#82259 = VECTOR ( 'NONE', #133160, 1000.000000000000000 ) ;
#82260 = CYLINDRICAL_SURFACE ( 'NONE', #182105, 0.09999999999998898659 ) ;
#82261 = EDGE_CURVE ( 'NONE', #34777, #60192, #162424, .T. ) ;
#82262 = CARTESIAN_POINT ( 'NONE',  ( -20.94999999999999929, 77.16270174995064224, -195.4231074845243370 ) ) ;
#82263 = AXIS2_PLACEMENT_3D ( 'NONE', #1004, #44022, #201805 ) ;
#82265 = CARTESIAN_POINT ( 'NONE',  ( -16.93388492042259230, 9.988541822527057690, -146.5994548768138372 ) ) ;
#82264 = CARTESIAN_POINT ( 'NONE',  ( 21.14999999999999858, 11.65000000001115943, -167.5999999999999659 ) ) ;
#82266 = CARTESIAN_POINT ( 'NONE',  ( 18.59999999999999787, 77.26327546522965406, -162.1212428177779543 ) ) ;
#82267 = ORIENTED_EDGE ( 'NONE', *, *, #43261, .F. ) ;
#82268 = EDGE_CURVE ( 'NONE', #18296, #79169, #231268, .T. ) ;
#82269 = DIRECTION ( 'NONE',  ( 0.000000000000000000, -1.000000000000000000, 0.000000000000000000 ) ) ;
#82270 =( NAMED_UNIT ( * ) PLANE_ANGLE_UNIT ( ) SI_UNIT ( $, .RADIAN. ) );
#82271 = EDGE_CURVE ( 'NONE', #118509, #197481, #33452, .T. ) ;
#82272 = CARTESIAN_POINT ( 'NONE',  ( -18.59999999999999787, 46.53760404070597900, -243.0973507280067167 ) ) ;
#82273 = DIRECTION ( 'NONE',  ( -1.000000000000000000, 0.000000000000000000, -0.000000000000000000 ) ) ;
#82274 = CARTESIAN_POINT ( 'NONE',  ( 21.05000000000000071, 74.16465844978765176, -124.9679561919613207 ) ) ;
#82275 = EDGE_LOOP ( 'NONE', ( #194552, #201179, #235036, #39011 ) ) ;
#82276 = AXIS2_PLACEMENT_3D ( 'NONE', #75587, #153867, #215065 ) ;
#82277 = AXIS2_PLACEMENT_3D ( 'NONE', #34016, #69265, #130495 ) ;
#82278 = TOROIDAL_SURFACE ( 'NONE', #232175, 0.2000000000000000111, 0.1000000000000000056 ) ;
#82279 = CARTESIAN_POINT ( 'NONE',  ( 20.94999999999999574, -11.39257802170567224, -3.073949579831933843 ) ) ;
#82280 = EDGE_CURVE ( 'NONE', #59875, #53618, #94291, .T. ) ;
#82281 = CARTESIAN_POINT ( 'NONE',  ( -21.13422380239045850, 1.115526128501326264E-11, -94.00667348519432664 ) ) ;
#82282 = EDGE_LOOP ( 'NONE', ( #164243, #176885, #151210, #52068 ) ) ;
#82283 = DIRECTION ( 'NONE',  ( 0.000000000000000000, 0.000000000000000000, -1.000000000000000000 ) ) ;
#82284 = DIRECTION ( 'NONE',  ( 1.000000000000000000, 0.000000000000000000, 0.000000000000000000 ) ) ;
#82285 = EDGE_CURVE ( 'NONE', #88353, #135481, #25073, .T. ) ;
#82286 = DIRECTION ( 'NONE',  ( 0.000000000000000000, 0.000000000000000000, -1.000000000000000000 ) ) ;
#82287 = DIRECTION ( 'NONE',  ( -1.000000000000000000, 0.000000000000000000, 0.000000000000000000 ) ) ;
#82288 = EDGE_CURVE ( 'NONE', #129965, #104663, #211703, .T. ) ;
#82289 = CARTESIAN_POINT ( 'NONE',  ( 5.899999999999995914, -11.25000000000000000, 10.10000000000000142 ) ) ;
#82290 = ORIENTED_EDGE ( 'NONE', *, *, #83284, .T. ) ;
#82291 = CARTESIAN_POINT ( 'NONE',  ( -21.64999999999999858, 65.95000000001225260, -149.2731074845244450 ) ) ;
#82292 = CARTESIAN_POINT ( 'NONE',  ( 18.60000000000000497, 7.128833340093095217, -233.7327013124392749 ) ) ;
#82293 = CARTESIAN_POINT ( 'NONE',  ( -21.09096482362056335, 0.03944827878534100385, -60.63645563459576948 ) ) ;
#82294 = CIRCLE ( 'NONE', #228079, 0.09999999999999609201 ) ;
#82296 = CARTESIAN_POINT ( 'NONE',  ( -21.44999999999999929, 68.85000000001205933, -124.1731074845243370 ) ) ;
#82295 = CYLINDRICAL_SURFACE ( 'NONE', #78339, 12.87499999999999822 ) ;
#82297 = CARTESIAN_POINT ( 'NONE',  ( -16.77683809663752257, 22.98839712131283974, -230.9453208111996503 ) ) ;
#82298 = FILL_AREA_STYLE ('',( #219262 ) ) ;
#82300 = DIRECTION ( 'NONE',  ( 1.000000000000000000, 0.000000000000000000, 0.000000000000000000 ) ) ;
#82299 = TOROIDAL_SURFACE ( 'NONE', #49001, 0.9750000000000019762, 0.1000000000000000056 ) ;
#82302 = ORIENTED_EDGE ( 'NONE', *, *, #249707, .F. ) ;
#82301 = LINE ( 'NONE', #214440, #219384 ) ;
#82303 = VECTOR ( 'NONE', #189697, 1000.000000000000000 ) ;
#82304 = ORIENTED_EDGE ( 'NONE', *, *, #25120, .T. ) ;
#82305 = EDGE_CURVE ( 'NONE', #211121, #37986, #104132, .T. ) ;
#82306 = ADVANCED_FACE ( 'NONE', ( #229959 ), #39568, .T. ) ;
#82307 = CARTESIAN_POINT ( 'NONE',  ( -18.59999999999999787, 76.00000000001170974, -69.52310748452431710 ) ) ;
#82308 = VECTOR ( 'NONE', #207104, 1000.000000000000000 ) ;
#82309 = AXIS2_PLACEMENT_3D ( 'NONE', #31703, #192051, #251996 ) ;
#82310 = EDGE_CURVE ( 'NONE', #69230, #167893, #54240, .T. ) ;
#82311 = CARTESIAN_POINT ( 'NONE',  ( -18.59999999999999787, 65.66751761918619934, -30.42826094061123854 ) ) ;
#82312 = AXIS2_PLACEMENT_3D ( 'NONE', #172940, #110346, #251123 ) ;
#82313 = CARTESIAN_POINT ( 'NONE',  ( 12.24999999999999822, 9.350000000011139178, -150.5215193718251498 ) ) ;
#82314 = ORIENTED_EDGE ( 'NONE', *, *, #161533, .T. ) ;
#82315 = CIRCLE ( 'NONE', #7512, 0.1000000000000028644 ) ;
#82316 = CARTESIAN_POINT ( 'NONE',  ( -21.65000000000000213, 10.05000000001113847, -154.8500000000000227 ) ) ;
#82317 = CARTESIAN_POINT ( 'NONE',  ( -0.8999999999999438449, 67.65000000001118963, -5.981686128287480919 ) ) ;
#82318 = CARTESIAN_POINT ( 'NONE',  ( 23.14999999999999503, 64.35000000001195986, -110.0379132551783243 ) ) ;
#82319 = ORIENTED_EDGE ( 'NONE', *, *, #192141, .T. ) ;
#82320 = FACE_OUTER_BOUND ( 'NONE', #140472, .T. ) ;
#82322 = EDGE_LOOP ( 'NONE', ( #203532, #3551, #78894, #113857 ) ) ;
#82321 = CYLINDRICAL_SURFACE ( 'NONE', #34421, 0.1000000000000028644 ) ;
#82324 = CARTESIAN_POINT ( 'NONE',  ( 21.14999999999999858, 0.000000000000000000, 6.540656951701244282 ) ) ;
#82323 = LINE ( 'NONE', #217986, #200604 ) ;
#82325 = CARTESIAN_POINT ( 'NONE',  ( 20.41140022480505323, 65.58956915761068274, -162.4081061808921902 ) ) ;
#82326 = FACE_OUTER_BOUND ( 'NONE', #154322, .T. ) ;
#82327 = ORIENTED_EDGE ( 'NONE', *, *, #46379, .F. ) ;
#82328 = AXIS2_PLACEMENT_3D ( 'NONE', #203970, #25366, #184404 ) ;
#82329 = EDGE_CURVE ( 'NONE', #37872, #152840, #129100, .T. ) ;
#82330 = DIRECTION ( 'NONE',  ( 0.000000000000000000, 0.000000000000000000, 1.000000000000000000 ) ) ;
#82331 = DIRECTION ( 'NONE',  ( -1.000000000000000000, -0.000000000000000000, -0.000000000000000000 ) ) ;
#82332 = DIRECTION ( 'NONE',  ( 1.000000000000000000, 0.000000000000000000, 0.000000000000000000 ) ) ;
#82333 = ORIENTED_EDGE ( 'NONE', *, *, #104727, .T. ) ;
#82334 = ADVANCED_FACE ( 'NONE', ( #91737, #90434 ), #108729, .F. ) ;
#82335 = CIRCLE ( 'NONE', #119803, 0.1000000000000028644 ) ;
#82336 = CYLINDRICAL_SURFACE ( 'NONE', #88735, 0.09999999999999939493 ) ;
#82337 = DIRECTION ( 'NONE',  ( -0.000000000000000000, 0.000000000000000000, -1.000000000000000000 ) ) ;
#82338 = ADVANCED_FACE ( 'NONE', ( #155601 ), #255890, .T. ) ;
#82339 = DIRECTION ( 'NONE',  ( 0.000000000000000000, -0.2617529984165031243, -0.9651348961777157509 ) ) ;
#82340 = ORIENTED_EDGE ( 'NONE', *, *, #60547, .T. ) ;
#82341 = ORIENTED_EDGE ( 'NONE', *, *, #233295, .F. ) ;
#82342 = ADVANCED_FACE ( 'NONE', ( #198533 ), #98118, .T. ) ;
#82343 = CARTESIAN_POINT ( 'NONE',  ( -23.25000000000000000, -0.09999999998884338825, -21.85042919245520210 ) ) ;
#82344 = DIRECTION ( 'NONE',  ( -1.000000000000000000, 0.000000000000000000, 0.000000000000000000 ) ) ;
#82345 = CARTESIAN_POINT ( 'NONE',  ( -21.55000000000000426, 10.16011026985487398, -211.4267369781599939 ) ) ;
#82346 = ADVANCED_FACE ( 'NONE', ( #18620 ), #139834, .T. ) ;
#82348 = DIRECTION ( 'NONE',  ( 0.000000000000000000, 0.2617529984165028467, 0.9651348961777159730 ) ) ;
#82347 = CARTESIAN_POINT ( 'NONE',  ( -16.81930730667006912, 12.41766554746485518, -211.3206651839645360 ) ) ;
#82349 = AXIS2_PLACEMENT_3D ( 'NONE', #171281, #250756, #72145 ) ;
#82350 = CARTESIAN_POINT ( 'NONE',  ( -18.47140463609786920, -9.671474685220882606, -40.17276045827407671 ) ) ;
#82351 = CARTESIAN_POINT ( 'NONE',  ( -20.64999999999999858, 2.500000000011154633, -53.77537807723790309 ) ) ;
#82352 = CIRCLE ( 'NONE', #69938, 0.1000000000000021844 ) ;
#82353 = CARTESIAN_POINT ( 'NONE',  ( -16.94445028196807002, 66.00793639031427062, -115.6304376629428106 ) ) ;
#82354 = ORIENTED_EDGE ( 'NONE', *, *, #166282, .F. ) ;
#82355 = DIRECTION ( 'NONE',  ( -1.000000000000000000, -0.000000000000000000, -0.000000000000000000 ) ) ;
#82356 = EDGE_CURVE ( 'NONE', #79411, #183734, #254631, .T. ) ;
#82358 = ORIENTED_EDGE ( 'NONE', *, *, #82603, .F. ) ;
#82357 = CARTESIAN_POINT ( 'NONE',  ( 13.43663047529819288, 62.93307127222839625, -215.6135269849708891 ) ) ;
#82359 = CARTESIAN_POINT ( 'NONE',  ( 20.95420533658165141, 65.45413552525306500, -195.9556014638312149 ) ) ;
#82361 = EDGE_CURVE ( 'NONE', #77787, #177623, #253974, .T. ) ;
#82360 = ADVANCED_FACE ( 'NONE', ( #235107 ), #257171, .T. ) ;
#82362 = SPHERICAL_SURFACE ( 'NONE', #236612, 0.1000000000000000056 ) ;
#82363 = DIRECTION ( 'NONE',  ( 0.000000000000000000, 1.000000000000000000, -0.000000000000000000 ) ) ;
#82364 = ORIENTED_EDGE ( 'NONE', *, *, #228860, .F. ) ;
#82366 = DIRECTION ( 'NONE',  ( 1.000000000000000000, 0.000000000000000000, 0.000000000000000000 ) ) ;
#82365 = DIRECTION ( 'NONE',  ( 0.000000000000000000, 0.6728388485993177515, -0.7397890806274072251 ) ) ;
#82368 = ADVANCED_FACE ( 'NONE', ( #117713 ), #237669, .F. ) ;
#82367 = FACE_OUTER_BOUND ( 'NONE', #239029, .T. ) ;
#82369 = CARTESIAN_POINT ( 'NONE',  ( 18.39999999999999503, 11.75000000001113953, -54.35000000000000142 ) ) ;
#82370 = LINE ( 'NONE', #161965, #111857 ) ;
#82371 = CARTESIAN_POINT ( 'NONE',  ( -15.57281606413131314, 66.62934494888905590, -185.9972842285434069 ) ) ;
#82372 = ORIENTED_EDGE ( 'NONE', *, *, #233274, .T. ) ;
#82373 = ORIENTED_EDGE ( 'NONE', *, *, #24691, .F. ) ;
#82374 = AXIS2_PLACEMENT_3D ( 'NONE', #79260, #57127, #136678 ) ;
#82376 = AXIS2_PLACEMENT_3D ( 'NONE', #108720, #145258, #168749 ) ;
#82375 = FACE_OUTER_BOUND ( 'NONE', #233297, .T. ) ;
#82377 = VERTEX_POINT ( 'NONE', #158176 ) ;
#82378 = DIRECTION ( 'NONE',  ( 3.265361837132813093E-16, 1.000000000000000000, 6.982962677686266711E-15 ) ) ;
#82379 = EDGE_CURVE ( 'NONE', #147021, #134468, #212499, .T. ) ;
#82380 = EDGE_CURVE ( 'NONE', #235551, #69086, #220683, .T. ) ;
#82381 = ORIENTED_EDGE ( 'NONE', *, *, #246668, .F. ) ;
#82383 = CARTESIAN_POINT ( 'NONE',  ( 22.50000000000000000, -2.402702137741712818, -189.4978470520862288 ) ) ;
#82382 = AXIS2_PLACEMENT_3D ( 'NONE', #257967, #38989, #238456 ) ;
#82384 = ADVANCED_FACE ( 'NONE', ( #78581 ), #40783, .F. ) ;
#82385 = DIRECTION ( 'NONE',  ( 0.000000000000000000, 0.9126074666064696306, 0.4088369013361213278 ) ) ;
#82386 = ORIENTED_EDGE ( 'NONE', *, *, #159415, .F. ) ;
#82387 = EDGE_CURVE ( 'NONE', #116521, #95061, #179016, .T. ) ;
#82388 = CARTESIAN_POINT ( 'NONE',  ( -16.80100914604134132, 9.943149094114721365, -87.81704412728768716 ) ) ;
#82389 = DIRECTION ( 'NONE',  ( -1.000000000000000000, 0.000000000000000000, 0.000000000000000000 ) ) ;
#82390 = EDGE_CURVE ( 'NONE', #92040, #243492, #158345, .T. ) ;
#82391 = DIRECTION ( 'NONE',  ( -4.408576920032448588E-17, 0.1350103645451876666, -0.9908441862701600211 ) ) ;
#82392 = CARTESIAN_POINT ( 'NONE',  ( -16.81744102076748959, 30.20632856012693424, -234.8070450048000737 ) ) ;
#82393 = DIRECTION ( 'NONE',  ( 0.000000000000000000, 0.000000000000000000, 1.000000000000000000 ) ) ;
#82394 = CARTESIAN_POINT ( 'NONE',  ( -23.15000000000000213, 1.115600667400684642E-11, -167.4999999999999716 ) ) ;
#82395 = CARTESIAN_POINT ( 'NONE',  ( 14.22821877134047774, 62.03415779510191896, -218.8921516991029819 ) ) ;
#82396 = CIRCLE ( 'NONE', #219975, 0.1999999999999987899 ) ;
#82397 = ORIENTED_EDGE ( 'NONE', *, *, #254255, .T. ) ;
#82399 = LINE ( 'NONE', #5433, #203334 ) ;
#82398 = DIRECTION ( 'NONE',  ( 0.000000000000000000, 1.156482317317873105E-15, -1.000000000000000000 ) ) ;
#82401 = ORIENTED_EDGE ( 'NONE', *, *, #117789, .F. ) ;
#82400 = AXIS2_PLACEMENT_3D ( 'NONE', #164654, #104629, #227175 ) ;
#82403 = ORIENTED_EDGE ( 'NONE', *, *, #152471, .F. ) ;
#82402 = DIRECTION ( 'NONE',  ( -1.000000000000000000, -2.952720810173289112E-16, 0.000000000000000000 ) ) ;
#82404 = CIRCLE ( 'NONE', #24771, 4.150000000000003020 ) ;
#82405 = VERTEX_POINT ( 'NONE', #138535 ) ;
#82406 = LINE ( 'NONE', #162001, #211378 ) ;
#82407 = DIRECTION ( 'NONE',  ( -0.000000000000000000, -0.01283462868040327436, 0.9999176327611370985 ) ) ;
#82408 = CARTESIAN_POINT ( 'NONE',  ( 21.14999999999999858, 60.09787988008870485, -221.2279614330287245 ) ) ;
#82409 = DIRECTION ( 'NONE',  ( 0.000000000000000000, -7.056502275159894776E-15, 1.000000000000000000 ) ) ;
#82410 = ORIENTED_EDGE ( 'NONE', *, *, #446, .F. ) ;
#82411 = EDGE_CURVE ( 'NONE', #241382, #178265, #79847, .T. ) ;
#82412 = CARTESIAN_POINT ( 'NONE',  ( -20.94999999999999929, -1.851028230129704522, -179.1539132694224463 ) ) ;
#82413 = TOROIDAL_SURFACE ( 'NONE', #69798, 3.899999999999999467, 0.1000000000000000056 ) ;
#82414 = DIRECTION ( 'NONE',  ( 0.000000000000000000, 0.2128009952263485993, -0.9770955615653340587 ) ) ;
#82415 = ORIENTED_EDGE ( 'NONE', *, *, #234988, .F. ) ;
#82416 = CARTESIAN_POINT ( 'NONE',  ( -20.86777300164945004, 10.33200063079656417, -39.09316749566428939 ) ) ;
#82417 = EDGE_CURVE ( 'NONE', #246051, #70703, #16681, .T. ) ;
#82418 = FACE_OUTER_BOUND ( 'NONE', #244571, .T. ) ;
#82419 = EDGE_LOOP ( 'NONE', ( #68391, #202775, #250876, #99761 ) ) ;
#82420 = AXIS2_PLACEMENT_3D ( 'NONE', #137442, #158347, #257344 ) ;
#82421 = DIRECTION ( 'NONE',  ( 0.000000000000000000, 6.982962677686266711E-15, -1.000000000000000000 ) ) ;
#82422 = CARTESIAN_POINT ( 'NONE',  ( 20.27550659511088682, 66.78395627750320784, -123.8731074845243683 ) ) ;
#82424 = ORIENTED_EDGE ( 'NONE', *, *, #146560, .F. ) ;
#82423 = CIRCLE ( 'NONE', #40798, 11.80000000000000426 ) ;
#82425 = CARTESIAN_POINT ( 'NONE',  ( 21.05000000000005400, 64.35000000001120668, -36.02310748452479316 ) ) ;
#82426 = EDGE_CURVE ( 'NONE', #162338, #16939, #154327, .T. ) ;
#82427 = CARTESIAN_POINT ( 'NONE',  ( -23.15000000000000213, 64.35000000001205933, -124.3731074845243825 ) ) ;
#82429 = CYLINDRICAL_SURFACE ( 'NONE', #189149, 0.9000000000000014655 ) ;
#82428 =( REPRESENTATION_RELATIONSHIP ('NONE','NONE', #36900, #135069 ) REPRESENTATION_RELATIONSHIP_WITH_TRANSFORMATION ( #109305 )SHAPE_REPRESENTATION_RELATIONSHIP( ) );
#82430 = DIRECTION ( 'NONE',  ( -1.000000000000000000, -0.000000000000000000, -0.000000000000000000 ) ) ;
#82431 = VECTOR ( 'NONE', #153017, 1000.000000000000000 ) ;
#82432 = DIRECTION ( 'NONE',  ( -2.812466655313719426E-14, 0.1350103645451904977, 0.9908441862701596881 ) ) ;
#82434 = ADVANCED_FACE ( 'NONE', ( #55139 ), #194715, .F. ) ;
#82433 = DIRECTION ( 'NONE',  ( -1.000000000000000000, -0.000000000000000000, -0.000000000000000000 ) ) ;
#82436 = CARTESIAN_POINT ( 'NONE',  ( -18.50000000000000000, 66.65000000001157332, -57.37310748452438247 ) ) ;
#82435 = CIRCLE ( 'NONE', #32439, 6.258578643762700899 ) ;
#82437 = ORIENTED_EDGE ( 'NONE', *, *, #35616, .T. ) ;
#82439 = DIRECTION ( 'NONE',  ( 0.000000000000000000, -0.9770955615653318382, -0.2128009952263588411 ) ) ;
#82438 = DIRECTION ( 'NONE',  ( 1.000000000000000000, 0.000000000000000000, 0.000000000000000000 ) ) ;
#82440 = AXIS2_PLACEMENT_3D ( 'NONE', #248728, #132633, #207034 ) ;
#82441 = CIRCLE ( 'NONE', #228238, 0.1000000000000028644 ) ;
#82442 = ORIENTED_EDGE ( 'NONE', *, *, #75838, .T. ) ;
#82443 = AXIS2_PLACEMENT_3D ( 'NONE', #233262, #31229, #92424 ) ;
#82444 = DIRECTION ( 'NONE',  ( 0.000000000000000000, 0.000000000000000000, -1.000000000000000000 ) ) ;
#82445 = CARTESIAN_POINT ( 'NONE',  ( -18.50000000000000000, 9.350000000011156942, -179.6499999999999773 ) ) ;
#82447 = ORIENTED_EDGE ( 'NONE', *, *, #87305, .T. ) ;
#82446 = CARTESIAN_POINT ( 'NONE',  ( -21.05000000000000071, 1.115600667400684642E-11, -100.5000000000000426 ) ) ;
#82449 = ORIENTED_EDGE ( 'NONE', *, *, #16433, .T. ) ;
#82448 = DIRECTION ( 'NONE',  ( 0.000000000000000000, -1.000000000000000000, -1.734723475976807292E-15 ) ) ;
#82450 = AXIS2_PLACEMENT_3D ( 'NONE', #231659, #253755, #256262 ) ;
#82451 = CARTESIAN_POINT ( 'NONE',  ( 18.54116936837186458, 46.96053119008168153, -255.3059777784767448 ) ) ;
#82452 = CARTESIAN_POINT ( 'NONE',  ( -1.820710678118657944, 24.25730123604973087, -254.1720964594295538 ) ) ;
#82453 = DIRECTION ( 'NONE',  ( 0.000000000000000000, 0.000000000000000000, -1.000000000000000000 ) ) ;
#82454 = DIRECTION ( 'NONE',  ( -1.000000000000000000, 0.000000000000000000, 0.000000000000000000 ) ) ;
#82456 = ORIENTED_EDGE ( 'NONE', *, *, #174564, .F. ) ;
#82455 = CARTESIAN_POINT ( 'NONE',  ( 21.08804582317328169, 67.12183383292037320, -157.6731076551165245 ) ) ;
#82457 = CIRCLE ( 'NONE', #228254, 0.4000000000000114575 ) ;
#82458 = AXIS2_PLACEMENT_3D ( 'NONE', #34295, #91666, #33029 ) ;
#82459 = CARTESIAN_POINT ( 'NONE',  ( -18.40000000000000213, 64.52683809664958403, -123.9731074845243768 ) ) ;
#82460 = ORIENTED_EDGE ( 'NONE', *, *, #146241, .F. ) ;
#82461 = ORIENTED_EDGE ( 'NONE', *, *, #109401, .T. ) ;
#82462 = CARTESIAN_POINT ( 'NONE',  ( -18.52309608778527306, 85.64247632006693323, -62.80851114335471408 ) ) ;
#82463 = CARTESIAN_POINT ( 'NONE',  ( 23.15000000000000213, -9.600000000000001421, -9.893969122652443104 ) ) ;
#82464 = ORIENTED_EDGE ( 'NONE', *, *, #157619, .T. ) ;
#82465 = DIRECTION ( 'NONE',  ( -1.000000000000000000, 0.000000000000000000, 0.000000000000000000 ) ) ;
#82466 = AXIS2_PLACEMENT_3D ( 'NONE', #140352, #41299, #218597 ) ;
#82467 = EDGE_CURVE ( 'NONE', #88959, #102162, #145834, .T. ) ;
#82468 = AXIS2_PLACEMENT_3D ( 'NONE', #64970, #42852, #23317 ) ;
#82469 = DIRECTION ( 'NONE',  ( 0.000000000000000000, 0.000000000000000000, -1.000000000000000000 ) ) ;
#82471 = ORIENTED_EDGE ( 'NONE', *, *, #96920, .F. ) ;
#82470 = CIRCLE ( 'NONE', #3377, 6.258578643762724880 ) ;
#82472 = DIRECTION ( 'NONE',  ( 0.000000000000000000, -6.982962677686266711E-15, 1.000000000000000000 ) ) ;
#82474 = LINE ( 'NONE', #50741, #26383 ) ;
#82473 = AXIS2_PLACEMENT_3D ( 'NONE', #124293, #244206, #145110 ) ;
#82475 = ORIENTED_EDGE ( 'NONE', *, *, #176340, .F. ) ;
#82476 = EDGE_LOOP ( 'NONE', ( #18576, #119474, #161014, #243803 ) ) ;
#82477 = CARTESIAN_POINT ( 'NONE',  ( 20.90000000000000213, 11.49641995933507843, 1.885425182446133885 ) ) ;
#82478 = ORIENTED_EDGE ( 'NONE', *, *, #137773, .T. ) ;
#82479 = EDGE_CURVE ( 'NONE', #183385, #59708, #166731, .T. ) ;
#82480 = DIRECTION ( 'NONE',  ( 0.000000000000000000, -0.9893560106964500722, 0.1455152366551550613 ) ) ;
#82481 = VERTEX_POINT ( 'NONE', #182854 ) ;
#82483 = ORIENTED_EDGE ( 'NONE', *, *, #258100, .F. ) ;
#82482 = CARTESIAN_POINT ( 'NONE',  ( 23.14999999999999858, 5.174642216963899699, -234.1583033028928753 ) ) ;
#82484 = CIRCLE ( 'NONE', #11822, 0.4000000000000114575 ) ;
#82486 = EDGE_CURVE ( 'NONE', #2147, #172709, #54065, .T. ) ;
#82485 = CARTESIAN_POINT ( 'NONE',  ( -33.72168855820451938, 66.05000000001180638, -82.17310748452433700 ) ) ;
#82487 = ORIENTED_EDGE ( 'NONE', *, *, #95201, .F. ) ;
#82488 = DIRECTION ( 'NONE',  ( 0.000000000000000000, -1.000000000000000000, 0.000000000000000000 ) ) ;
#82489 = AXIS2_PLACEMENT_3D ( 'NONE', #71459, #148414, #130113 ) ;
#82490 = CIRCLE ( 'NONE', #36781, 0.1000000000000028644 ) ;
#82491 = ORIENTED_EDGE ( 'NONE', *, *, #231279, .F. ) ;
#82493 = EDGE_LOOP ( 'NONE', ( #50797, #166166, #79992, #247577 ) ) ;
#82492 = VERTEX_POINT ( 'NONE', #105829 ) ;
#82494 = CARTESIAN_POINT ( 'NONE',  ( 21.04999999999999716, 69.70076908992525944, -136.6215449845243768 ) ) ;
#82495 = VECTOR ( 'NONE', #96868, 1000.000000000000000 ) ;
#82496 = DIRECTION ( 'NONE',  ( -1.000000000000000000, 0.000000000000000000, -0.000000000000000000 ) ) ;
#82498 = EDGE_CURVE ( 'NONE', #105444, #101145, #87381, .T. ) ;
#82497 = ORIENTED_EDGE ( 'NONE', *, *, #174472, .T. ) ;
#82499 = AXIS2_PLACEMENT_3D ( 'NONE', #254116, #212456, #114621 ) ;
#82500 = EDGE_CURVE ( 'NONE', #214061, #225466, #120741, .T. ) ;
#82501 = ADVANCED_FACE ( 'NONE', ( #43326 ), #45880, .F. ) ;
#82502 = ORIENTED_EDGE ( 'NONE', *, *, #57085, .T. ) ;
#82503 = CARTESIAN_POINT ( 'NONE',  ( -23.15000000000000213, 1.115600667400684642E-11, -189.1999999999999602 ) ) ;
#82504 = DIRECTION ( 'NONE',  ( 0.000000000000000000, -6.982962677686266711E-15, 1.000000000000000000 ) ) ;
#82506 = ORIENTED_EDGE ( 'NONE', *, *, #189190, .T. ) ;
#82505 = FACE_OUTER_BOUND ( 'NONE', #33990, .T. ) ;
#82507 = CARTESIAN_POINT ( 'NONE',  ( 18.59999999999999432, 43.48442877397276618, -245.2193771921251084 ) ) ;
#82508 = EDGE_LOOP ( 'NONE', ( #246908, #147503, #2963, #94307 ) ) ;
#82509 = EDGE_CURVE ( 'NONE', #37909, #176555, #83275, .T. ) ;
#82510 = CARTESIAN_POINT ( 'NONE',  ( -18.54148534481894117, 65.67467670974440352, -130.9531731826884879 ) ) ;
#82511 = CARTESIAN_POINT ( 'NONE',  ( -21.05000000000000071, 77.16270174995010223, -128.4231074845242802 ) ) ;
#82512 = VERTEX_POINT ( 'NONE', #104538 ) ;
#82513 = LINE ( 'NONE', #102082, #23922 ) ;
#82514 = CARTESIAN_POINT ( 'NONE',  ( 21.05000000000000071, 70.50000000001185185, -90.61784146561124942 ) ) ;
#82515 = ADVANCED_FACE ( 'NONE', ( #224515 ), #84974, .T. ) ;
#82516 = ORIENTED_EDGE ( 'NONE', *, *, #77688, .T. ) ;
#82517 = VERTEX_POINT ( 'NONE', #141143 ) ;
#82518 = AXIS2_PLACEMENT_3D ( 'NONE', #246342, #205923, #164251 ) ;
#82520 = VERTEX_POINT ( 'NONE', #203675 ) ;
#82519 = VERTEX_POINT ( 'NONE', #124154 ) ;
#82521 = EDGE_LOOP ( 'NONE', ( #171071, #219368, #244495, #80380 ) ) ;
#82522 = CARTESIAN_POINT ( 'NONE',  ( -21.05000000000000071, 76.00000000001142553, -36.02310748452432421 ) ) ;
#82523 = EDGE_LOOP ( 'NONE', ( #133063, #21287, #89815, #100154 ) ) ;
#82524 = CARTESIAN_POINT ( 'NONE',  ( -16.92209698673592300, 66.05000000001153637, -48.73374305157589959 ) ) ;
#82525 = VERTEX_POINT ( 'NONE', #26331 ) ;
#82526 = DIRECTION ( 'NONE',  ( -1.000000000000000000, -0.000000000000000000, -0.000000000000000000 ) ) ;
#82527 = DIRECTION ( 'NONE',  ( 0.000000000000000000, -0.9651348961777053148, 0.2617529984165415380 ) ) ;
#82528 = EDGE_CURVE ( 'NONE', #50377, #116815, #83681, .T. ) ;
#82529 = ORIENTED_EDGE ( 'NONE', *, *, #236152, .F. ) ;
#82530 = ORIENTED_EDGE ( 'NONE', *, *, #52719, .T. ) ;
#82531 = CIRCLE ( 'NONE', #7553, 0.09999999999998898659 ) ;
#82532 = TOROIDAL_SURFACE ( 'NONE', #7554, 11.90000000000000391, 0.1000000000000000056 ) ;
#82533 = VECTOR ( 'NONE', #215954, 1000.000000000000114 ) ;
#82534 = CIRCLE ( 'NONE', #74235, 0.09999999999999693856 ) ;
#82535 = VERTEX_POINT ( 'NONE', #25065 ) ;
#82536 = ADVANCED_FACE ( 'NONE', ( #65440 ), #121603, .T. ) ;
#82537 = DIRECTION ( 'NONE',  ( 0.000000000000000000, 0.000000000000000000, 1.000000000000000000 ) ) ;
#82538 = EDGE_LOOP ( 'NONE', ( #149313, #8815, #70782, #121577 ) ) ;
#82539 = CARTESIAN_POINT ( 'NONE',  ( 20.97224591636398827, 12.98858666785727323, -210.7083050095600925 ) ) ;
#82540 = DIRECTION ( 'NONE',  ( 1.000000000000000000, 0.000000000000000000, 0.000000000000000000 ) ) ;
#82541 = DIRECTION ( 'NONE',  ( 1.000000000000000000, 0.000000000000000000, 0.000000000000000000 ) ) ;
#82542 = CARTESIAN_POINT ( 'NONE',  ( 18.54999999999999716, 67.25000000001156764, -60.27310748452438816 ) ) ;
#82543 = CARTESIAN_POINT ( 'NONE',  ( 23.15000000000000213, -8.999999999988844479, -43.39396912265245021 ) ) ;
#82544 = LINE ( 'NONE', #245521, #140241 ) ;
#82547 = CARTESIAN_POINT ( 'NONE',  ( 21.07928932188134397, 6.328516656404459262, -100.4011048543456468 ) ) ;
#82546 = AXIS2_PLACEMENT_3D ( 'NONE', #214202, #229906, #189504 ) ;
#82545 = DIRECTION ( 'NONE',  ( -1.000000000000000000, -0.000000000000000000, -0.000000000000000000 ) ) ;
#82548 = CARTESIAN_POINT ( 'NONE',  ( 20.04142135623730070, 64.35000000001222986, -148.6731074845244507 ) ) ;
#82549 = DIRECTION ( 'NONE',  ( -1.000000000000000000, 1.186688945009010077E-16, 8.286604613020808509E-31 ) ) ;
#82550 = CIRCLE ( 'NONE', #145112, 12.87499999999999822 ) ;
#82551 = FACE_OUTER_BOUND ( 'NONE', #195261, .T. ) ;
#82552 = CARTESIAN_POINT ( 'NONE',  ( -20.90000000000000213, 7.900000000000000355, -1.212568896937008089 ) ) ;
#82553 = VERTEX_POINT ( 'NONE', #125431 ) ;
#82554 = EDGE_CURVE ( 'NONE', #168580, #119060, #146016, .T. ) ;
#82555 = VECTOR ( 'NONE', #94775, 1000.000000000000000 ) ;
#82557 = ORIENTED_EDGE ( 'NONE', *, *, #193323, .F. ) ;
#82556 = DIRECTION ( 'NONE',  ( -0.000000000000000000, -0.2128009952263605620, 0.9770955615653313941 ) ) ;
#82558 = ORIENTED_EDGE ( 'NONE', *, *, #92021, .T. ) ;
#82559 = DIRECTION ( 'NONE',  ( 1.186688945009010077E-16, 1.000000000000000000, 6.982962677686266711E-15 ) ) ;
#82560 = EDGE_CURVE ( 'NONE', #7029, #206656, #225779, .T. ) ;
#82561 = CARTESIAN_POINT ( 'NONE',  ( -17.11825945287481332, 9.950000000011138823, -54.25000000000000711 ) ) ;
#82562 = ORIENTED_EDGE ( 'NONE', *, *, #72054, .T. ) ;
#82563 = EDGE_CURVE ( 'NONE', #92859, #98991, #206245, .T. ) ;
#82564 = EDGE_CURVE ( 'NONE', #217227, #96734, #1610, .T. ) ;
#82565 = CARTESIAN_POINT ( 'NONE',  ( -23.15000000000000213, 27.91464654983916205, -239.9322955902566719 ) ) ;
#82566 = PRESENTATION_LAYER_ASSIGNMENT (  '', '', ( #120252 ) ) ;
#82567 = CARTESIAN_POINT ( 'NONE',  ( 21.05000000000000071, 65.61575147395463148, -242.1939180743342774 ) ) ;
#82568 = ORIENTED_EDGE ( 'NONE', *, *, #169257, .F. ) ;
#82569 = CIRCLE ( 'NONE', #178497, 0.1999999999999987899 ) ;
#82570 = CARTESIAN_POINT ( 'NONE',  ( -21.12844524849339223, 11.75000000001115197, -140.9044134708424565 ) ) ;
#82571 = DIRECTION ( 'NONE',  ( 1.000000000000000000, 0.000000000000000000, 0.000000000000000000 ) ) ;
#82572 = DIRECTION ( 'NONE',  ( 0.000000000000000000, -0.9651348961777157509, 0.2617529984165031243 ) ) ;
#82573 = EDGE_CURVE ( 'NONE', #73566, #82125, #209781, .T. ) ;
#82574 = DIRECTION ( 'NONE',  ( -0.000000000000000000, 0.1298341882519953583, 0.9915357197604862671 ) ) ;
#82576 = ORIENTED_EDGE ( 'NONE', *, *, #69667, .F. ) ;
#82575 = DIRECTION ( 'NONE',  ( -0.000000000000000000, 0.000000000000000000, 1.000000000000000000 ) ) ;
#82577 = AXIS2_PLACEMENT_3D ( 'NONE', #53860, #229928, #175141 ) ;
#82578 = DIRECTION ( 'NONE',  ( 0.000000000000000000, -6.982962677686266711E-15, 1.000000000000000000 ) ) ;
#82580 = VERTEX_POINT ( 'NONE', #129275 ) ;
#82579 = CARTESIAN_POINT ( 'NONE',  ( -18.40000000000000213, 85.68240343348826116, -96.36626410711144786 ) ) ;
#82581 = CARTESIAN_POINT ( 'NONE',  ( -23.25000000000000000, 7.128833340093095217, -233.7327013124392749 ) ) ;
#82582 = DIRECTION ( 'NONE',  ( -2.561896900575096011E-15, 0.3589373870825449120, -0.9333616406058026227 ) ) ;
#82583 = CARTESIAN_POINT ( 'NONE',  ( -16.94445028196808778, 66.00793639031455484, -157.4157773061059800 ) ) ;
#82584 = CARTESIAN_POINT ( 'NONE',  ( -15.75000000000000355, 9.350000000011140955, -184.2499999999999716 ) ) ;
#82586 = CARTESIAN_POINT ( 'NONE',  ( -22.50000000000000000, 67.23127455305841238, -235.8551265064783991 ) ) ;
#82585 = LINE ( 'NONE', #65621, #61608 ) ;
#82587 = LINE ( 'NONE', #17507, #107816 ) ;
#82588 = CARTESIAN_POINT ( 'NONE',  ( 16.87683809663750267, 66.05000000001157900, -56.87310748452439668 ) ) ;
#82589 = CARTESIAN_POINT ( 'NONE',  ( -20.94999999999999929, 64.25000000001233502, -163.0083017138704236 ) ) ;
#82590 = DIRECTION ( 'NONE',  ( 1.000000000000000000, 0.000000000000000000, 0.000000000000000000 ) ) ;
#82591 = AXIS2_PLACEMENT_3D ( 'NONE', #171708, #183865, #251189 ) ;
#82592 = FACE_OUTER_BOUND ( 'NONE', #248765, .T. ) ;
#82593 = ORIENTED_EDGE ( 'NONE', *, *, #93575, .F. ) ;
#82594 = EDGE_CURVE ( 'NONE', #116043, #200421, #33655, .T. ) ;
#82595 = DIRECTION ( 'NONE',  ( 1.000000000000000000, 0.000000000000000000, 0.000000000000000000 ) ) ;
#82596 = VECTOR ( 'NONE', #38140, 1000.000000000000227 ) ;
#82597 = VERTEX_POINT ( 'NONE', #150140 ) ;
#82598 = EDGE_LOOP ( 'NONE', ( #60570, #4636, #71467, #55545 ) ) ;
#82599 = CARTESIAN_POINT ( 'NONE',  ( -20.94999999999999929, 11.74999999999999289, -26.71613433702190576 ) ) ;
#82600 = LINE ( 'NONE', #164752, #19408 ) ;
#82601 = EDGE_CURVE ( 'NONE', #73622, #155471, #92830, .T. ) ;
#82602 = ORIENTED_EDGE ( 'NONE', *, *, #104116, .F. ) ;
#82603 = EDGE_CURVE ( 'NONE', #81962, #218111, #83453, .T. ) ;
#82604 = AXIS2_PLACEMENT_3D ( 'NONE', #19858, #161941, #47084 ) ;
#82605 = ORIENTED_EDGE ( 'NONE', *, *, #141869, .F. ) ;
#82606 = EDGE_CURVE ( 'NONE', #244695, #18621, #129283, .T. ) ;
#82607 = VECTOR ( 'NONE', #234769, 1000.000000000000000 ) ;
#82608 = ORIENTED_EDGE ( 'NONE', *, *, #183288, .T. ) ;
#82609 = DIRECTION ( 'NONE',  ( -0.000000000000000000, -1.000000000000000000, -6.982962677686266711E-15 ) ) ;
#82610 = ORIENTED_EDGE ( 'NONE', *, *, #2091, .F. ) ;
#82612 = CARTESIAN_POINT ( 'NONE',  ( -18.59999999999999787, 11.65000000001115232, -79.15000000000003411 ) ) ;
#82611 = AXIS2_PLACEMENT_3D ( 'NONE', #108585, #9477, #149016 ) ;
#82613 = DIRECTION ( 'NONE',  ( 0.000000000000000000, -0.9126074666063769270, -0.4088369013363280513 ) ) ;
#82614 = DIRECTION ( 'NONE',  ( 1.000000000000000000, 0.000000000000000000, 0.000000000000000000 ) ) ;
#82615 = AXIS2_PLACEMENT_3D ( 'NONE', #254470, #195841, #253211 ) ;
#82616 = LINE ( 'NONE', #223434, #219890 ) ;
#82617 = CARTESIAN_POINT ( 'NONE',  ( -23.25000000000000000, 0.000000000000000000, -41.40000000000000568 ) ) ;
#82618 = VECTOR ( 'NONE', #248629, 1000.000000000000000 ) ;
#82619 = DIRECTION ( 'NONE',  ( 0.000000000000000000, 0.1495327102803586661, -0.9887567792719350601 ) ) ;
#82620 = DIRECTION ( 'NONE',  ( -0.7071067811865456854, -0.7071067811865493491, -4.937700262164544098E-15 ) ) ;
#82622 = ORIENTED_EDGE ( 'NONE', *, *, #158862, .T. ) ;
#82621 = CARTESIAN_POINT ( 'NONE',  ( -22.14074124539699895, 75.90094710416764201, -76.91318533556810166 ) ) ;
#82624 = CARTESIAN_POINT ( 'NONE',  ( 18.59999999999999432, 85.48068669529034480, -29.08199231576640287 ) ) ;
#82623 = CARTESIAN_POINT ( 'NONE',  ( 20.95496329884391784, 65.43256679391856778, -61.94879755223957574 ) ) ;
#82625 = VECTOR ( 'NONE', #90578, 1000.000000000000114 ) ;
#82626 = DIRECTION ( 'NONE',  ( 0.000000000000000000, 0.2128009952263485993, -0.9770955615653341697 ) ) ;
#82627 = ORIENTED_EDGE ( 'NONE', *, *, #241584, .F. ) ;
#82628 = CARTESIAN_POINT ( 'NONE',  ( -14.77738660682463845, 9.436552840015579591, -115.6779554727603738 ) ) ;
#82629 = PRESENTATION_STYLE_ASSIGNMENT (( #159643 ) ) ;
#82630 = ORIENTED_EDGE ( 'NONE', *, *, #100841, .F. ) ;
#82631 = EDGE_CURVE ( 'NONE', #8209, #242007, #191854, .T. ) ;
#82633 = CARTESIAN_POINT ( 'NONE',  ( -23.15000000000000213, 1.115600667400684642E-11, -33.50000000000000000 ) ) ;
#82632 = DIRECTION ( 'NONE',  ( 0.000000000000000000, -1.000000000000000000, -6.982962677686266711E-15 ) ) ;
#82634 = EDGE_CURVE ( 'NONE', #7645, #18611, #237611, .T. ) ;
#82635 = DIRECTION ( 'NONE',  ( 0.000000000000000000, -6.530723674265620862E-15, 1.000000000000000000 ) ) ;
#82636 = AXIS2_PLACEMENT_3D ( 'NONE', #4871, #84384, #58435 ) ;
#82638 = ORIENTED_EDGE ( 'NONE', *, *, #74434, .F. ) ;
#82637 = CIRCLE ( 'NONE', #24442, 1.900000000000005906 ) ;
#82639 = FACE_OUTER_BOUND ( 'NONE', #107517, .T. ) ;
#82640 = DIRECTION ( 'NONE',  ( 0.000000000000000000, 0.9876197685951241256, 0.1568667991644932258 ) ) ;
#82641 = FACE_OUTER_BOUND ( 'NONE', #132933, .T. ) ;
#82642 = ADVANCED_FACE ( 'NONE', ( #71881 ), #195930, .F. ) ;
#82643 = CARTESIAN_POINT ( 'NONE',  ( -20.64999999999999858, 85.00000000001207923, -126.6291383618717816 ) ) ;
#82644 = ORIENTED_EDGE ( 'NONE', *, *, #186812, .T. ) ;
#82645 = CIRCLE ( 'NONE', #195139, 0.09999999999998898659 ) ;
#82646 = EDGE_CURVE ( 'NONE', #215970, #217929, #204266, .T. ) ;
#82647 = AXIS2_PLACEMENT_3D ( 'NONE', #242538, #46892, #125177 ) ;
#82648 = PLANE ( 'NONE',  #181698 ) ;
#82649 = FACE_OUTER_BOUND ( 'NONE', #103718, .T. ) ;
#82650 = CARTESIAN_POINT ( 'NONE',  ( -16.88460203013674388, 30.22258428227766558, -234.8103539652946665 ) ) ;
#82651 = ADVANCED_FACE ( 'NONE', ( #127996 ), #181211, .F. ) ;
#82652 = AXIS2_PLACEMENT_3D ( 'NONE', #125081, #104202, #41697 ) ;
#82653 = CARTESIAN_POINT ( 'NONE',  ( 20.94999999999999574, 87.48912529308871910, -200.6231074845242688 ) ) ;
#82654 = DIRECTION ( 'NONE',  ( 0.000000000000000000, -0.2617529984165034573, -0.9651348961777156399 ) ) ;
#82655 = AXIS2_PLACEMENT_3D ( 'NONE', #120804, #142878, #21688 ) ;
#82656 = EDGE_CURVE ( 'NONE', #217285, #40334, #137620, .T. ) ;
#82658 = EDGE_LOOP ( 'NONE', ( #157362, #80388, #3262, #127878 ) ) ;
#82657 = DIRECTION ( 'NONE',  ( 1.000000000000000000, 0.000000000000000000, 0.000000000000000000 ) ) ;
#82659 = CARTESIAN_POINT ( 'NONE',  ( -21.05000000000000071, 6.413662734880689165, -33.58559286336213034 ) ) ;
#82660 = ADVANCED_FACE ( 'NONE', ( #88834 ), #104307, .F. ) ;
#82661 = DIRECTION ( 'NONE',  ( -1.000000000000000000, 0.000000000000000000, 1.156482317317870344E-15 ) ) ;
#82662 = DIRECTION ( 'NONE',  ( 0.000000000000000000, 0.000000000000000000, 1.000000000000000000 ) ) ;
#82663 = DIRECTION ( 'NONE',  ( 1.000000000000000000, -0.000000000000000000, -0.000000000000000000 ) ) ;
#82664 = LINE ( 'NONE', #145228, #525 ) ;
#82665 = VERTEX_POINT ( 'NONE', #228383 ) ;
#82666 = DIRECTION ( 'NONE',  ( -0.000000000000000000, 0.1298341882519953583, 0.9915357197604862671 ) ) ;
#82667 = CARTESIAN_POINT ( 'NONE',  ( -20.85000000000000142, -1.835859311432481045, -212.5044391687984842 ) ) ;
#82668 = CARTESIAN_POINT ( 'NONE',  ( 20.94403535211772294, 67.49374512151688066, -195.5131169347613991 ) ) ;
#82669 = ORIENTED_EDGE ( 'NONE', *, *, #105661, .T. ) ;
#82670 = FACE_OUTER_BOUND ( 'NONE', #218097, .T. ) ;
#82671 = CARTESIAN_POINT ( 'NONE',  ( 21.05000000000000071, 75.96798630682472719, -176.2819502080616871 ) ) ;
#82672 = AXIS2_PLACEMENT_3D ( 'NONE', #59890, #67290, #23390 ) ;
#82673 = DIRECTION ( 'NONE',  ( 2.915501640297156255E-16, 1.000000000000000000, 6.997203936713175802E-15 ) ) ;
#82674 = CIRCLE ( 'NONE', #3590, 0.5000000000000014433 ) ;
#82675 = CARTESIAN_POINT ( 'NONE',  ( 22.39999999999999503, 11.65000000001116298, -133.9000000000000057 ) ) ;
#82676 = VERTEX_POINT ( 'NONE', #249229 ) ;
#82677 = FACE_OUTER_BOUND ( 'NONE', #108682, .T. ) ;
#82678 = EDGE_CURVE ( 'NONE', #86031, #227593, #54440, .T. ) ;
#82679 = EDGE_CURVE ( 'NONE', #163431, #115258, #179357, .T. ) ;
#82680 = VERTEX_POINT ( 'NONE', #117412 ) ;
#82681 = ORIENTED_EDGE ( 'NONE', *, *, #172597, .F. ) ;
#82682 = CARTESIAN_POINT ( 'NONE',  ( 23.24999999999999645, 11.75000000001113953, -76.25000000000004263 ) ) ;
#82683 = CARTESIAN_POINT ( 'NONE',  ( 21.05000000000000071, 72.02722222756959525, -225.1832529173024398 ) ) ;
#82684 = ADVANCED_FACE ( 'NONE', ( #95278 ), #220840, .T. ) ;
#82685 = CARTESIAN_POINT ( 'NONE',  ( -21.05000000000000071, 1.835341550235569663, -112.0551512925630249 ) ) ;
#82686 = DIRECTION ( 'NONE',  ( 1.000000000000000000, 0.000000000000000000, 0.000000000000000000 ) ) ;
#82687 = EDGE_LOOP ( 'NONE', ( #140329, #28866, #131146, #122667 ) ) ;
#82688 = DIRECTION ( 'NONE',  ( 1.000000000000000000, 0.000000000000000000, 0.000000000000000000 ) ) ;
#82689 = DIRECTION ( 'NONE',  ( 0.000000000000000000, -1.000000000000000000, -6.860497997771532351E-15 ) ) ;
#82690 = EDGE_CURVE ( 'NONE', #141210, #43598, #234791, .T. ) ;
#82691 = CARTESIAN_POINT ( 'NONE',  ( 21.11344571971334361, 12.98064790059219575, -210.7060374374014771 ) ) ;
#82692 = EDGE_CURVE ( 'NONE', #199332, #23607, #35346, .T. ) ;
#82693 = DIRECTION ( 'NONE',  ( 0.000000000000000000, 0.000000000000000000, -1.000000000000000000 ) ) ;
#82694 = DIRECTION ( 'NONE',  ( -0.000000000000000000, 6.982962677686266711E-15, -1.000000000000000000 ) ) ;
#82695 = CARTESIAN_POINT ( 'NONE',  ( 18.50000324121758055, 10.29307482169092403, -206.4586421466939328 ) ) ;
#82696 = ORIENTED_EDGE ( 'NONE', *, *, #227569, .T. ) ;
#82698 = VERTEX_POINT ( 'NONE', #236069 ) ;
#82697 = DIRECTION ( 'NONE',  ( -1.000000000000000000, 0.000000000000000000, 0.000000000000000000 ) ) ;
#82699 = EDGE_LOOP ( 'NONE', ( #81956, #100870, #49808, #198805 ) ) ;
#82700 = FACE_OUTER_BOUND ( 'NONE', #23573, .T. ) ;
#82701 = VERTEX_POINT ( 'NONE', #138233 ) ;
#82702 = CARTESIAN_POINT ( 'NONE',  ( -23.25000000000000000, -0.1008583690875562017, -55.25043287651065782 ) ) ;
#82703 = CARTESIAN_POINT ( 'NONE',  ( -21.45000000000000284, 68.29142135624881860, -48.27310748452437394 ) ) ;
#82704 = CARTESIAN_POINT ( 'NONE',  ( -18.69999999999999929, -8.150000000000005684, 32.89999999999999858 ) ) ;
#82705 = EDGE_LOOP ( 'NONE', ( #97805, #150833, #220861, #220162 ) ) ;
#82706 = ADVANCED_FACE ( 'NONE', ( #198223 ), #207876, .T. ) ;
#82707 = LINE ( 'NONE', #162301, #161490 ) ;
#82708 = DIRECTION ( 'NONE',  ( -4.408576920032448588E-17, -0.1350103645451807832, -0.9908441862701610203 ) ) ;
#82709 = ORIENTED_EDGE ( 'NONE', *, *, #227089, .F. ) ;
#82710 = DIRECTION ( 'NONE',  ( 0.000000000000000000, 0.000000000000000000, 1.000000000000000000 ) ) ;
#82712 = ORIENTED_EDGE ( 'NONE', *, *, #106316, .F. ) ;
#82711 = CYLINDRICAL_SURFACE ( 'NONE', #50773, 0.1000000000000024342 ) ;
#82713 = DIRECTION ( 'NONE',  ( 0.000000000000000000, -0.2605042016806647931, -0.9654727137038724427 ) ) ;
#82714 = CARTESIAN_POINT ( 'NONE',  ( -18.39999999999999858, -9.599999999988849453, -140.6001893912220737 ) ) ;
#82715 = EDGE_CURVE ( 'NONE', #241306, #148485, #156575, .T. ) ;
#82716 = CIRCLE ( 'NONE', #174382, 0.09999999999998898659 ) ;
#82717 = AXIS2_PLACEMENT_3D ( 'NONE', #25196, #160852, #1740 ) ;
#82718 = VECTOR ( 'NONE', #117656, 1000.000000000000000 ) ;
#82719 = ORIENTED_EDGE ( 'NONE', *, *, #128497, .T. ) ;
#82720 = DIRECTION ( 'NONE',  ( 0.000000000000000000, -7.304098846218085561E-15, 1.000000000000000000 ) ) ;
#82721 = CARTESIAN_POINT ( 'NONE',  ( 21.05000000000000071, 10.72371710471867701, -79.15000000000004832 ) ) ;
#82722 = AXIS2_PLACEMENT_3D ( 'NONE', #201318, #181765, #81338 ) ;
#82723 = DIRECTION ( 'NONE',  ( 1.000000000000000000, 0.000000000000000000, 0.000000000000000000 ) ) ;
#82724 = EDGE_LOOP ( 'NONE', ( #10108, #152005, #143881, #123207, #240940 ) ) ;
#82725 = LINE ( 'NONE', #41097, #71666 ) ;
#82726 = EDGE_CURVE ( 'NONE', #256518, #231259, #208414, .T. ) ;
#82727 = LINE ( 'NONE', #175056, #210071 ) ;
#82728 = CARTESIAN_POINT ( 'NONE',  ( -21.51976009735018991, 6.910458441670358276, -100.5000000000000284 ) ) ;
#82729 = VERTEX_POINT ( 'NONE', #58693 ) ;
#82730 = VECTOR ( 'NONE', #237763, 1000.000000000000114 ) ;
#82731 = VECTOR ( 'NONE', #4039, 1000.000000000000000 ) ;
#82732 = AXIS2_PLACEMENT_3D ( 'NONE', #53272, #32456, #174556 ) ;
#82733 = CIRCLE ( 'NONE', #145297, 0.1000000000000102612 ) ;
#82734 = ORIENTED_EDGE ( 'NONE', *, *, #171755, .T. ) ;
#82735 = ORIENTED_EDGE ( 'NONE', *, *, #126226, .F. ) ;
#82736 = CARTESIAN_POINT ( 'NONE',  ( 18.50211644919734866, 10.30207779524869061, -38.98955207167824000 ) ) ;
#82737 = CARTESIAN_POINT ( 'NONE',  ( -16.87998658237729188, 66.05000000001255955, -182.8867470522638143 ) ) ;
#82739 = ORIENTED_EDGE ( 'NONE', *, *, #154409, .F. ) ;
#82738 = DIRECTION ( 'NONE',  ( 0.000000000000000000, -0.9651348961777157509, 0.2617529984165031243 ) ) ;
#82740 = CYLINDRICAL_SURFACE ( 'NONE', #132523, 0.1000000000000089151 ) ;
#82741 = LINE ( 'NONE', #227424, #111575 ) ;
#82742 = CYLINDRICAL_SURFACE ( 'NONE', #246248, 0.1000000000000028644 ) ;
#82743 = CARTESIAN_POINT ( 'NONE',  ( -16.89081410710458542, 51.62234474387415872, -231.9434644128527054 ) ) ;
#82744 = CARTESIAN_POINT ( 'NONE',  ( -20.94999999999999929, 77.13501884592184865, -61.80613060109197932 ) ) ;
#82745 = DIRECTION ( 'NONE',  ( 0.000000000000000000, 0.000000000000000000, -1.000000000000000000 ) ) ;
#82747 = ORIENTED_EDGE ( 'NONE', *, *, #187578, .T. ) ;
#82746 = LINE ( 'NONE', #162346, #248837 ) ;
#82749 = ORIENTED_EDGE ( 'NONE', *, *, #51237, .F. ) ;
#82748 = PLANE ( 'NONE',  #165222 ) ;
#82750 = CARTESIAN_POINT ( 'NONE',  ( 20.85000000000000142, 0.000000000000000000, -33.50000000000000000 ) ) ;
#82751 = ORIENTED_EDGE ( 'NONE', *, *, #72708, .T. ) ;
#82752 = ORIENTED_EDGE ( 'NONE', *, *, #217362, .T. ) ;
#82753 = CARTESIAN_POINT ( 'NONE',  ( 21.30000000000002558, 67.23127455305841238, -235.8551265064783991 ) ) ;
#82754 = CIRCLE ( 'NONE', #20461, 0.09999999999998898659 ) ;
#82755 = CARTESIAN_POINT ( 'NONE',  ( -17.29158576265543346, 65.63525233399469982, -192.1058657293165766 ) ) ;
#82756 = CARTESIAN_POINT ( 'NONE',  ( 18.49999999999998934, 6.550000000011156231, -155.2500000000000284 ) ) ;
#82758 = DIRECTION ( 'NONE',  ( -1.000000000000000000, -0.000000000000000000, -0.000000000000000000 ) ) ;
#82757 = CIRCLE ( 'NONE', #49491, 0.09999999999998898659 ) ;
#82759 = LINE ( 'NONE', #159783, #44848 ) ;
#82760 = EDGE_LOOP ( 'NONE', ( #151858, #104299, #215966, #224445 ) ) ;
#82761 = CARTESIAN_POINT ( 'NONE',  ( 21.05000000000061888, 10.48215802087101700, -207.4378900153776328 ) ) ;
#82762 = VERTEX_POINT ( 'NONE', #215228 ) ;
#82763 = ORIENTED_EDGE ( 'NONE', *, *, #76820, .T. ) ;
#82764 = EDGE_CURVE ( 'NONE', #7471, #56118, #63504, .T. ) ;
#82765 = CARTESIAN_POINT ( 'NONE',  ( -18.34374000495060386, 64.52683809664941350, -93.77310748452440237 ) ) ;
#82766 = AXIS2_PLACEMENT_3D ( 'NONE', #67766, #163042, #45644 ) ;
#82767 = CIRCLE ( 'NONE', #78694, 0.09999999999998807065 ) ;
#82768 = VERTEX_POINT ( 'NONE', #39184 ) ;
#82769 = CARTESIAN_POINT ( 'NONE',  ( 21.93340585898254247, 76.00000000001243450, -177.3472545066566681 ) ) ;
#82770 = CARTESIAN_POINT ( 'NONE',  ( -18.46907102845853643, 86.89089698701586428, -199.5596099339830971 ) ) ;
#82771 = VERTEX_POINT ( 'NONE', #143033 ) ;
#82772 = DIRECTION ( 'NONE',  ( -1.000000000000000000, -0.000000000000000000, -0.000000000000000000 ) ) ;
#82773 = ORIENTED_EDGE ( 'NONE', *, *, #1928, .F. ) ;
#82774 = DIRECTION ( 'NONE',  ( 0.000000000000000000, 1.000000000000000000, 6.982962677686266711E-15 ) ) ;
#82775 = VERTEX_POINT ( 'NONE', #118714 ) ;
#82776 = AXIS2_PLACEMENT_3D ( 'NONE', #39677, #236550, #158349 ) ;
#82777 = EDGE_CURVE ( 'NONE', #166638, #43854, #57416, .T. ) ;
#82778 = CARTESIAN_POINT ( 'NONE',  ( 12.47034474403012894, 9.375538102059163492, -183.3698758809907758 ) ) ;
#82779 = ORIENTED_EDGE ( 'NONE', *, *, #186174, .T. ) ;
#82780 = FACE_OUTER_BOUND ( 'NONE', #179575, .T. ) ;
#82781 = CIRCLE ( 'NONE', #45418, 0.09999999999999939493 ) ;
#82783 = ORIENTED_EDGE ( 'NONE', *, *, #162865, .T. ) ;
#82782 = CARTESIAN_POINT ( 'NONE',  ( 23.24999999999999645, 0.000000000000000000, -33.50000000000000000 ) ) ;
#82784 = CARTESIAN_POINT ( 'NONE',  ( 21.05000000000000071, 10.42338541492406279, -107.9920519238701218 ) ) ;
#82785 = ORIENTED_EDGE ( 'NONE', *, *, #134350, .F. ) ;
#82786 = AXIS2_PLACEMENT_3D ( 'NONE', #92557, #174730, #95140 ) ;
#82787 = AXIS2_PLACEMENT_3D ( 'NONE', #23423, #67649, #2525 ) ;
#82788 = AXIS2_PLACEMENT_3D ( 'NONE', #231449, #232735, #225313 ) ;
#82789 = CIRCLE ( 'NONE', #116186, 0.09999999999999414912 ) ;
#82790 = EDGE_CURVE ( 'NONE', #212843, #220745, #12782, .T. ) ;
#82792 = CARTESIAN_POINT ( 'NONE',  ( -16.84421487269769102, 66.05000000001261640, -190.8536053620794632 ) ) ;
#82791 =( BOUNDED_SURFACE ( )  B_SPLINE_SURFACE ( 3, 2, ( 
 ( #111436, #113991, #73625 ),
 ( #13625, #93145, #54026 ),
 ( #193552, #87993, #227521 ),
 ( #48888, #128434, #188401 ) ),
 .UNSPECIFIED., .F., .F., .F. ) 
 B_SPLINE_SURFACE_WITH_KNOTS ( ( 4, 4 ),
 ( 3, 3 ),
 ( 0.0006461284895273852530, 0.0007503702773986309620 ),
 ( 0.000000000000000000, 1.000000000000000000 ),
 .UNSPECIFIED. ) 
 GEOMETRIC_REPRESENTATION_ITEM ( )  RATIONAL_B_SPLINE_SURFACE ( (
 ( 1.000000000000000000, 0.7071067811865561215, 1.000000000000000000),
 ( 1.000000000000000000, 0.7076476444647564756, 1.000000000000000000),
 ( 1.000000000000000000, 0.7075727925193199264, 1.000000000000000000),
 ( 1.000000000000000000, 0.7071067811865359154, 1.000000000000000000) ) ) 
 REPRESENTATION_ITEM ( '' )  SURFACE ( )  );
#82793 = ADVANCED_FACE ( 'NONE', ( #173591 ), #253060, .F. ) ;
#82794 = ORIENTED_EDGE ( 'NONE', *, *, #97874, .T. ) ;
#82796 = AXIS2_PLACEMENT_3D ( 'NONE', #213102, #216942, #215656 ) ;
#82795 = DIRECTION ( 'NONE',  ( -0.000000000000000000, -6.982962677686266711E-15, 1.000000000000000000 ) ) ;
#82797 = DIRECTION ( 'NONE',  ( -0.000000000000000000, -0.000000000000000000, -1.000000000000000000 ) ) ;
#82798 = DIRECTION ( 'NONE',  ( 0.000000000000000000, 0.9126074666063770380, 0.4088369013363281068 ) ) ;
#82799 = CARTESIAN_POINT ( 'NONE',  ( -16.86578989773640913, 9.984809801269951990, -121.4646648866222733 ) ) ;
#82800 = EDGE_CURVE ( 'NONE', #163039, #17816, #100204, .T. ) ;
#82801 = CARTESIAN_POINT ( 'NONE',  ( -15.52965525596988172, 66.62446189796456508, -187.6532316035334702 ) ) ;
#82802 = DIRECTION ( 'NONE',  ( 0.000000000000000000, -1.000000000000000000, -6.982962677686266711E-15 ) ) ;
#82803 = ORIENTED_EDGE ( 'NONE', *, *, #141988, .F. ) ;
#82804 = CARTESIAN_POINT ( 'NONE',  ( -16.90987985657660886, 66.04219248183281366, -182.6538203956407926 ) ) ;
#82805 = CARTESIAN_POINT ( 'NONE',  ( 23.24999999999999645, 11.75000000001113953, -113.1500000000000483 ) ) ;
#82806 = CARTESIAN_POINT ( 'NONE',  ( -20.94999999999999929, 87.65000000001163016, -66.62310748452424036 ) ) ;
#82807 = EDGE_CURVE ( 'NONE', #42422, #177843, #134381, .T. ) ;
#82808 = DIRECTION ( 'NONE',  ( -1.000000000000000000, 0.000000000000000000, 0.000000000000000000 ) ) ;
#82809 = ORIENTED_EDGE ( 'NONE', *, *, #38468, .F. ) ;
#82810 = CARTESIAN_POINT ( 'NONE',  ( 20.89192007715127630, 68.10318897902124036, -224.1464165264002872 ) ) ;
#82812 = ORIENTED_EDGE ( 'NONE', *, *, #80191, .T. ) ;
#82811 = AXIS2_PLACEMENT_3D ( 'NONE', #62013, #180672, #77692 ) ;
#82814 = CIRCLE ( 'NONE', #228624, 12.87499999999999822 ) ;
#82813 = CARTESIAN_POINT ( 'NONE',  ( -18.50000000000000000, 7.021664781911246322, -70.83356540189728889 ) ) ;
#82815 = ORIENTED_EDGE ( 'NONE', *, *, #216443, .T. ) ;
#82816 = EDGE_CURVE ( 'NONE', #6368, #11590, #105161, .T. ) ;
#82817 = CARTESIAN_POINT ( 'NONE',  ( -20.85000000000000142, 77.83585931145498193, -24.51866831572578320 ) ) ;
#82818 = CARTESIAN_POINT ( 'NONE',  ( -20.88420186297724257, 10.33025634372637391, -72.58709292826388548 ) ) ;
#82819 = ORIENTED_EDGE ( 'NONE', *, *, #34800, .F. ) ;
#82821 = VERTEX_POINT ( 'NONE', #187335 ) ;
#82820 = PLANE ( 'NONE',  #144630 ) ;
#82822 = DIRECTION ( 'NONE',  ( 1.000000000000000000, 0.000000000000000000, 0.000000000000000000 ) ) ;
#82823 = ORIENTED_EDGE ( 'NONE', *, *, #139279, .T. ) ;
#82824 = FACE_OUTER_BOUND ( 'NONE', #134108, .T. ) ;
#82825 = CIRCLE ( 'NONE', #33033, 2.100000000000004974 ) ;
#82826 = DIRECTION ( 'NONE',  ( 0.000000000000000000, -0.2818822000685679008, 0.9594490217226259166 ) ) ;
#82827 = AXIS2_PLACEMENT_3D ( 'NONE', #28962, #84999, #104563 ) ;
#82829 = EDGE_CURVE ( 'NONE', #141897, #110495, #26987, .T. ) ;
#82828 = ORIENTED_EDGE ( 'NONE', *, *, #51699, .F. ) ;
#82830 = ORIENTED_EDGE ( 'NONE', *, *, #207928, .F. ) ;
#82831 = CARTESIAN_POINT ( 'NONE',  ( -23.25000000000000000, 52.81534179157633702, -244.1198638051726277 ) ) ;
#82832 = CARTESIAN_POINT ( 'NONE',  ( -16.89318236219976299, 14.16159327252907651, -219.2597579924957358 ) ) ;
#82833 = CIRCLE ( 'NONE', #116216, 4.300000000000033573 ) ;
#82834 = CARTESIAN_POINT ( 'NONE',  ( 19.75857864376268935, 64.25000000001148237, -44.67310748452440095 ) ) ;
#82835 = EDGE_LOOP ( 'NONE', ( #118939, #73535 ) ) ;
#82836 = VERTEX_POINT ( 'NONE', #225134 ) ;
#82837 = CIRCLE ( 'NONE', #166124, 11.89999999999999325 ) ;
#82839 = ORIENTED_EDGE ( 'NONE', *, *, #182180, .F. ) ;
#82838 = DIRECTION ( 'NONE',  ( 1.000000000000000000, 0.000000000000000000, 0.000000000000000000 ) ) ;
#82840 = CARTESIAN_POINT ( 'NONE',  ( -21.14999999999999858, 78.47509609352879068, -238.9045489380306435 ) ) ;
#82841 = VECTOR ( 'NONE', #125045, 1000.000000000000000 ) ;
#82842 = CARTESIAN_POINT ( 'NONE',  ( -22.41119224318417125, 76.00000000001173817, -81.17267829206912211 ) ) ;
#82843 = CARTESIAN_POINT ( 'NONE',  ( -16.85312964099709276, 63.05615751446485007, -213.3757143580369302 ) ) ;
#82844 = VECTOR ( 'NONE', #220765, 999.9999999999998863 ) ;
#82846 = FACE_OUTER_BOUND ( 'NONE', #164337, .T. ) ;
#82845 = CARTESIAN_POINT ( 'NONE',  ( 21.05000000000000071, 65.49889199258218753, -241.8691648588935266 ) ) ;
#82847 = FACE_OUTER_BOUND ( 'NONE', #209829, .T. ) ;
#82848 = DIRECTION ( 'NONE',  ( 0.000000000000000000, 0.000000000000000000, -1.000000000000000000 ) ) ;
#82849 = FACE_OUTER_BOUND ( 'NONE', #227619, .T. ) ;
#82850 = CARTESIAN_POINT ( 'NONE',  ( 22.57320508075687115, 11.75000000001115552, -134.0000000000000000 ) ) ;
#82851 = ORIENTED_EDGE ( 'NONE', *, *, #19743, .F. ) ;
#82852 = ADVANCED_FACE ( 'NONE', ( #208183 ), #91857, .F. ) ;
#82853 = EDGE_CURVE ( 'NONE', #233410, #113090, #112712, .T. ) ;
#82854 = ORIENTED_EDGE ( 'NONE', *, *, #243117, .T. ) ;
#82855 = CYLINDRICAL_SURFACE ( 'NONE', #81260, 2.000000000000013323 ) ;
#82856 = VERTEX_POINT ( 'NONE', #186035 ) ;
#82857 = ADVANCED_FACE ( 'NONE', ( #165187 ), #64794, .F. ) ;
#82859 = EDGE_CURVE ( 'NONE', #76904, #205599, #124786, .T. ) ;
#82858 =( BOUNDED_SURFACE ( )  B_SPLINE_SURFACE ( 3, 2, ( 
 ( #163946, #120992, #85643 ),
 ( #45276, #66122, #182230 ),
 ( #220065, #100084, #62273 ),
 ( #80513, #200501, #63544 ),
 ( #24459, #222600, #126078 ),
 ( #21870, #101340, #3570 ) ),
 .UNSPECIFIED., .F., .F., .F. ) 
 B_SPLINE_SURFACE_WITH_KNOTS ( ( 4, 2, 4 ),
 ( 3, 3 ),
 ( 0.0001300404313046605199, 0.0003183318589266607925, 0.0005066232865486610922 ),
 ( 0.000000000000000000, 1.000000000000000000 ),
 .UNSPECIFIED. ) 
 GEOMETRIC_REPRESENTATION_ITEM ( )  RATIONAL_B_SPLINE_SURFACE ( (
 ( 1.000000000000000000, 0.7071067811865475727, 1.000000000000000000),
 ( 1.000000000000000000, 0.7625113560538873125, 1.000000000000000000),
 ( 1.000000000000000000, 0.8126073484690201632, 1.000000000000000000),
 ( 1.000000000000000000, 0.8923049332730712546, 1.000000000000000000),
 ( 1.000000000000000000, 0.9231914937770823171, 1.000000000000000000),
 ( 1.000000000000000000, 0.9238795325112901802, 1.000000000000000000) ) ) 
 REPRESENTATION_ITEM ( '' )  SURFACE ( )  );
#82860 = CARTESIAN_POINT ( 'NONE',  ( -23.25000000000000000, 87.65000000001204228, -114.7731074845242318 ) ) ;
#82861 = VERTEX_POINT ( 'NONE', #7387 ) ;
#82862 = EDGE_CURVE ( 'NONE', #8158, #20774, #148186, .T. ) ;
#82863 = CARTESIAN_POINT ( 'NONE',  ( 20.86777300164945004, 65.66799936921553638, -130.9299399888601272 ) ) ;
#82864 = EDGE_CURVE ( 'NONE', #104329, #17273, #184735, .T. ) ;
#82866 = ORIENTED_EDGE ( 'NONE', *, *, #63535, .T. ) ;
#82865 = EDGE_LOOP ( 'NONE', ( #227946, #183309 ) ) ;
#82867 = DIRECTION ( 'NONE',  ( 0.000000000000000000, 0.000000000000000000, 1.000000000000000000 ) ) ;
#82868 = EDGE_LOOP ( 'NONE', ( #142846, #130663, #186239, #248180, #177933 ) ) ;
#82869 = EDGE_CURVE ( 'NONE', #92030, #209902, #89484, .T. ) ;
#82870 = EDGE_LOOP ( 'NONE', ( #81029, #207852, #51414 ) ) ;
#82871 = DIRECTION ( 'NONE',  ( 0.000000000000000000, 0.000000000000000000, -1.000000000000000000 ) ) ;
#82872 = CARTESIAN_POINT ( 'NONE',  ( 20.94999999999999929, 30.43677443282724937, -239.5249545687858870 ) ) ;
#82874 = ORIENTED_EDGE ( 'NONE', *, *, #186790, .F. ) ;
#82873 = CARTESIAN_POINT ( 'NONE',  ( 20.95000000000005613, 66.15000000001120384, -4.623107484524796362 ) ) ;
#82875 = EDGE_CURVE ( 'NONE', #56118, #44033, #200191, .T. ) ;
#82876 = CARTESIAN_POINT ( 'NONE',  ( 20.97565083910961548, 39.29220182519587468, -236.8938058441740964 ) ) ;
#82877 = CARTESIAN_POINT ( 'NONE',  ( 20.94788355080264353, 65.69792220476320210, -97.53355541284612684 ) ) ;
#82879 = VERTEX_POINT ( 'NONE', #144305 ) ;
#82878 = CARTESIAN_POINT ( 'NONE',  ( 20.95575313997065336, 10.61455330328599089, -141.6212907019448437 ) ) ;
#82880 = DIRECTION ( 'NONE',  ( 1.186688945009010077E-16, -1.000000000000000000, -0.000000000000000000 ) ) ;
#82881 = ORIENTED_EDGE ( 'NONE', *, *, #87371, .T. ) ;
#82882 = CARTESIAN_POINT ( 'NONE',  ( 21.05000000000000071, 4.999999999999997335, -12.40526601891309788 ) ) ;
#82884 = EDGE_LOOP ( 'NONE', ( #35157, #241307, #57, #115145 ) ) ;
#82883 = CARTESIAN_POINT ( 'NONE',  ( -23.25000000000000000, 77.16412189325258453, -28.10825939895270764 ) ) ;
#82885 = DIRECTION ( 'NONE',  ( 1.000000000000000000, 0.000000000000000000, 0.000000000000000000 ) ) ;
#82887 = EDGE_CURVE ( 'NONE', #46873, #28860, #204295, .T. ) ;
#82886 = CARTESIAN_POINT ( 'NONE',  ( -18.59999999999999787, 10.33248238083634440, -72.59484654391314962 ) ) ;
#82888 = CARTESIAN_POINT ( 'NONE',  ( -22.39999999999999858, 76.00000000001237765, -170.1231074845243540 ) ) ;
#82889 = ORIENTED_EDGE ( 'NONE', *, *, #77965, .F. ) ;
#82890 = VECTOR ( 'NONE', #63480, 1000.000000000000000 ) ;
#82893 = CARTESIAN_POINT ( 'NONE',  ( 20.58091095332318332, 9.018470153363605135, -108.9186501821586006 ) ) ;
#82892 = VECTOR ( 'NONE', #100520, 1000.000000000000000 ) ;
#82891 = FACE_OUTER_BOUND ( 'NONE', #111951, .T. ) ;
#82894 = ADVANCED_FACE ( 'NONE', ( #248570 ), #233358, .F. ) ;
#82895 = VECTOR ( 'NONE', #67319, 1000.000000000000000 ) ;
#82897 = EDGE_CURVE ( 'NONE', #18238, #41248, #67373, .T. ) ;
#82896 = AXIS2_PLACEMENT_3D ( 'NONE', #213134, #79711, #159290 ) ;
#82898 = CARTESIAN_POINT ( 'NONE',  ( 20.95512820512820440, 65.37615131630040821, -157.8731074845244393 ) ) ;
#82899 = DIRECTION ( 'NONE',  ( 0.000000000000000000, 0.008583690987124399305, -0.9999631594459055250 ) ) ;
#82900 = CARTESIAN_POINT ( 'NONE',  ( -23.15000000000000213, -11.41227409413852811, -64.00000000000000000 ) ) ;
#82901 = EDGE_LOOP ( 'NONE', ( #102999, #210561, #228344, #183229 ) ) ;
#82902 = ORIENTED_EDGE ( 'NONE', *, *, #177266, .F. ) ;
#82903 =( BOUNDED_CURVE ( )  B_SPLINE_CURVE ( 3, ( #63443, #8627, #24353, #103842 ),
 .UNSPECIFIED., .F., .F. ) 
 B_SPLINE_CURVE_WITH_KNOTS ( ( 4, 4 ),
 ( 5.733388419619902088, 5.983100554402347449 ),
 .UNSPECIFIED. ) 
 CURVE ( )  GEOMETRIC_REPRESENTATION_ITEM ( )  RATIONAL_B_SPLINE_CURVE ( ( 1.000000000000000000, 0.9948104011409417691, 0.9948104011409417691, 1.000000000000000000 ) ) 
 REPRESENTATION_ITEM ( '' )  );
#82904 = ORIENTED_EDGE ( 'NONE', *, *, #226660, .F. ) ;
#82905 = ADVANCED_FACE ( 'NONE', ( #146881 ), #226417, .F. ) ;
#82906 = AXIS2_PLACEMENT_3D ( 'NONE', #120237, #243986, #65352 ) ;
#82907 = ORIENTED_EDGE ( 'NONE', *, *, #205583, .F. ) ;
#82908 = FACE_OUTER_BOUND ( 'NONE', #145057, .T. ) ;
#82909 = VERTEX_POINT ( 'NONE', #107778 ) ;
#82910 = DIRECTION ( 'NONE',  ( 0.000000000000000000, 0.9915357197604849349, -0.1298341882520056834 ) ) ;
#82911 = DIRECTION ( 'NONE',  ( 0.000000000000000000, 0.000000000000000000, -1.000000000000000000 ) ) ;
#82912 = EDGE_CURVE ( 'NONE', #209093, #14211, #109052, .T. ) ;
#82913 = ADVANCED_FACE ( 'NONE', ( #227713 ), #24422, .T. ) ;
#82914 = AXIS2_PLACEMENT_3D ( 'NONE', #102724, #181025, #41524 ) ;
#82915 = AXIS2_PLACEMENT_3D ( 'NONE', #112191, #255475, #212567 ) ;
#82916 = ORIENTED_EDGE ( 'NONE', *, *, #107954, .F. ) ;
#82917 = TOROIDAL_SURFACE ( 'NONE', #28846, 7.791421356237335338, 0.1000000000000000056 ) ;
#82918 = FACE_OUTER_BOUND ( 'NONE', #95646, .T. ) ;
#82919 = SURFACE_SIDE_STYLE ('',( #219894 ) ) ;
#82920 = EDGE_LOOP ( 'NONE', ( #132877, #115338, #54561 ) ) ;
#82921 = AXIS2_PLACEMENT_3D ( 'NONE', #14667, #39370, #195866 ) ;
#82922 = EDGE_LOOP ( 'NONE', ( #78953, #130223, #8185, #187541, #38093 ) ) ;
#82923 = ORIENTED_EDGE ( 'NONE', *, *, #21237, .T. ) ;
#82924 = CARTESIAN_POINT ( 'NONE',  ( 21.05000000000000071, 87.48912529308798014, -105.9231074845242091 ) ) ;
#82925 = LINE ( 'NONE', #38709, #70053 ) ;
#82926 = CARTESIAN_POINT ( 'NONE',  ( -23.25000000000000000, 1.115650265596050101E-11, -163.4499999999999886 ) ) ;
#82927 = DIRECTION ( 'NONE',  ( -4.408576920032448588E-17, 0.1350103645451876666, 0.9908441862701600211 ) ) ;
#82928 = DIRECTION ( 'NONE',  ( -0.000000000000000000, 0.4721928772777345684, 0.8814952561688429444 ) ) ;
#82929 = DIRECTION ( 'NONE',  ( 0.000000000000000000, -7.086529944415894657E-15, 1.000000000000000000 ) ) ;
#82931 = LINE ( 'NONE', #119545, #170139 ) ;
#82930 = DIRECTION ( 'NONE',  ( -1.000000000000000000, -2.952720810173289112E-16, 0.000000000000000000 ) ) ;
#82932 = CARTESIAN_POINT ( 'NONE',  ( 21.05000000000000071, 10.72371710471867701, -45.65000000000000568 ) ) ;
#82934 = ORIENTED_EDGE ( 'NONE', *, *, #143716, .F. ) ;
#82933 = CARTESIAN_POINT ( 'NONE',  ( 21.95218792049437795, 68.79849243876529385, -103.1221359243242688 ) ) ;
#82935 = CARTESIAN_POINT ( 'NONE',  ( -16.91247567987037570, 12.41838062070308624, -211.2201679100434717 ) ) ;
#82936 = CARTESIAN_POINT ( 'NONE',  ( -18.52186455168995849, -9.481018481431584988, -141.0250164779142210 ) ) ;
#82937 = ORIENTED_EDGE ( 'NONE', *, *, #200976, .F. ) ;
#82938 = CARTESIAN_POINT ( 'NONE',  ( 18.49999999999999645, 74.16465844978715438, -57.96795619196135618 ) ) ;
#82939 = CARTESIAN_POINT ( 'NONE',  ( 19.75857864376269291, 64.25000000001148237, -44.67310748452440095 ) ) ;
#82940 = ORIENTED_EDGE ( 'NONE', *, *, #4048, .T. ) ;
#82941 = AXIS2_PLACEMENT_3D ( 'NONE', #25044, #146232, #5420 ) ;
#82942 = PLANE ( 'NONE',  #152437 ) ;
#82943 = DIRECTION ( 'NONE',  ( 0.000000000000000000, 6.982962677686267499E-15, -1.000000000000000000 ) ) ;
#82944 = ORIENTED_EDGE ( 'NONE', *, *, #184073, .T. ) ;
#82945 = ORIENTED_EDGE ( 'NONE', *, *, #34455, .T. ) ;
#82946 = DIRECTION ( 'NONE',  ( 1.000000000000000000, 0.000000000000000000, 6.938893903907270030E-14 ) ) ;
#82947 = ORIENTED_EDGE ( 'NONE', *, *, #170528, .F. ) ;
#82948 = CARTESIAN_POINT ( 'NONE',  ( 19.96434256916586847, 5.572646937746800866, 16.50000000334722472 ) ) ;
#82950 = DIRECTION ( 'NONE',  ( 1.000000000000000000, 3.265361837132813093E-16, -0.000000000000000000 ) ) ;
#82949 = AXIS2_PLACEMENT_3D ( 'NONE', #111461, #73649, #252241 ) ;
#82951 = CARTESIAN_POINT ( 'NONE',  ( -16.97683809663752186, 9.949999999999983302, -20.09763598180368405 ) ) ;
#82952 = CARTESIAN_POINT ( 'NONE',  ( 22.49533356619864222, 11.65000000631534149, -133.9348774196772069 ) ) ;
#82953 = ORIENTED_EDGE ( 'NONE', *, *, #52572, .T. ) ;
#82954 = DIRECTION ( 'NONE',  ( -1.000000000000000000, 0.000000000000000000, 0.000000000000000000 ) ) ;
#82955 = EDGE_CURVE ( 'NONE', #135869, #54023, #37904, .T. ) ;
#82956 = DIRECTION ( 'NONE',  ( -0.000000000000000000, 1.000000000000000000, 6.352154140967427193E-15 ) ) ;
#82957 = CARTESIAN_POINT ( 'NONE',  ( -21.64999999999999858, 68.75000000001206502, -124.2731074845243455 ) ) ;
#82958 = AXIS2_PLACEMENT_3D ( 'NONE', #196197, #35862, #114082 ) ;
#82959 = EDGE_CURVE ( 'NONE', #87934, #195497, #16404, .T. ) ;
#82960 = AXIS2_PLACEMENT_3D ( 'NONE', #133672, #248490, #90686 ) ;
#82961 = EDGE_LOOP ( 'NONE', ( #85980, #104811, #212286, #150684 ) ) ;
#82962 = TOROIDAL_SURFACE ( 'NONE', #8008, 4.149999999999999467, 0.1000000000000000056 ) ;
#82963 = EDGE_CURVE ( 'NONE', #214167, #127799, #104479, .T. ) ;
#82965 = ORIENTED_EDGE ( 'NONE', *, *, #47979, .T. ) ;
#82964 = DIRECTION ( 'NONE',  ( -1.000000000000000000, 7.304098846218134667E-16, 5.100424963727256530E-30 ) ) ;
#82966 = EDGE_CURVE ( 'NONE', #55509, #26533, #231589, .T. ) ;
#82967 = CARTESIAN_POINT ( 'NONE',  ( -20.94999999999999929, 64.40000000001234071, -163.0949042542488883 ) ) ;
#82968 = DIRECTION ( 'NONE',  ( 0.000000000000000000, 1.000000000000000000, -0.000000000000000000 ) ) ;
#82969 = DIRECTION ( 'NONE',  ( 0.000000000000000000, 0.000000000000000000, -1.000000000000000000 ) ) ;
#82970 = FACE_OUTER_BOUND ( 'NONE', #6969, .T. ) ;
#82971 = VECTOR ( 'NONE', #45765, 1000.000000000000114 ) ;
#82972 = DIRECTION ( 'NONE',  ( -1.000000000000000000, -0.000000000000000000, -0.000000000000000000 ) ) ;
#82973 = CYLINDRICAL_SURFACE ( 'NONE', #232122, 7.900000000000003908 ) ;
#82974 = AXIS2_PLACEMENT_3D ( 'NONE', #256175, #241503, #62859 ) ;
#82975 = VERTEX_POINT ( 'NONE', #149501 ) ;
#82976 = CARTESIAN_POINT ( 'NONE',  ( 23.24999999999999645, 8.822561741677553471, -176.7499999999999716 ) ) ;
#82977 = CARTESIAN_POINT ( 'NONE',  ( 15.51872946208854565, 9.376580978055097049, -51.12694624701192225 ) ) ;
#82978 = LINE ( 'NONE', #105106, #4939 ) ;
#82979 = CARTESIAN_POINT ( 'NONE',  ( 20.94999999999999929, 5.500000000011153745, -155.0947339810869323 ) ) ;
#82980 = DIRECTION ( 'NONE',  ( 0.000000000000000000, 0.000000000000000000, 1.000000000000000000 ) ) ;
#82982 = ADVANCED_FACE ( 'NONE', ( #251118 ), #33419, .T. ) ;
#82981 = CIRCLE ( 'NONE', #49879, 0.09999999999999939493 ) ;
#82984 = ORIENTED_EDGE ( 'NONE', *, *, #165463, .F. ) ;
#82983 = AXIS2_PLACEMENT_3D ( 'NONE', #83866, #22683, #163456 ) ;
#82985 = ORIENTED_EDGE ( 'NONE', *, *, #206210, .F. ) ;
#82986 = CARTESIAN_POINT ( 'NONE',  ( -16.87683809663752399, 12.31632387104345305, -211.2641690508233125 ) ) ;
#82987 = AXIS2_PLACEMENT_3D ( 'NONE', #46661, #104060, #242306 ) ;
#82988 = CARTESIAN_POINT ( 'NONE',  ( 23.15000000000000213, 85.50000000001188027, -93.12913836187179584 ) ) ;
#82989 = LINE ( 'NONE', #43903, #159870 ) ;
#82990 = CARTESIAN_POINT ( 'NONE',  ( 20.94999999999999218, 17.16609282392353109, -224.6038045889790453 ) ) ;
#82991 = CIRCLE ( 'NONE', #174667, 0.09999999999999939493 ) ;
#82992 = ORIENTED_EDGE ( 'NONE', *, *, #201617, .F. ) ;
#82993 = CARTESIAN_POINT ( 'NONE',  ( -20.64999999999999858, 4.350000000011156054, -79.35000000000005116 ) ) ;
#82994 = CARTESIAN_POINT ( 'NONE',  ( -18.59999999999999787, 31.44980407958351165, -233.5445995079518866 ) ) ;
#82995 = FACE_OUTER_BOUND ( 'NONE', #236079, .T. ) ;
#82996 = ADVANCED_FACE ( 'NONE', ( #153373 ), #174216, .F. ) ;
#82997 = PRODUCT_DEFINITION_SHAPE ( 'NONE', 'NONE',  #99334 ) ;
#82998 = DIRECTION ( 'NONE',  ( 0.000000000000000000, 1.000000000000000000, -6.308085367188393199E-16 ) ) ;
#82999 = EDGE_CURVE ( 'NONE', #29322, #173155, #92058, .T. ) ;
#83000 = CIRCLE ( 'NONE', #237168, 0.09999999999998898659 ) ;
#83001 = ORIENTED_EDGE ( 'NONE', *, *, #80725, .F. ) ;
#83002 = CARTESIAN_POINT ( 'NONE',  ( -23.15000000000000213, 76.00000000001190870, -103.0231074845243029 ) ) ;
#83003 = ORIENTED_EDGE ( 'NONE', *, *, #129127, .T. ) ;
#83004 = LINE ( 'NONE', #162594, #184905 ) ;
#83005 = DIRECTION ( 'NONE',  ( 1.000000000000000000, 0.000000000000000000, 0.000000000000000000 ) ) ;
#83006 = DIRECTION ( 'NONE',  ( 0.000000000000000000, -7.147358527629762208E-15, 1.000000000000000000 ) ) ;
#83007 = EDGE_CURVE ( 'NONE', #192064, #84058, #250260, .T. ) ;
#83008 = CARTESIAN_POINT ( 'NONE',  ( 18.50211644919734866, 65.69792220476298894, -64.03355541284614105 ) ) ;
#83009 = CARTESIAN_POINT ( 'NONE',  ( -23.15000000000000213, 1.115600667400684642E-11, -138.0500000000000114 ) ) ;
#83010 = CARTESIAN_POINT ( 'NONE',  ( -20.94999999999999929, 1.736257131608553550, -145.5686523290175387 ) ) ;
#83011 = FACE_OUTER_BOUND ( 'NONE', #85420, .T. ) ;
#83012 = DIRECTION ( 'NONE',  ( -0.7071067811865475727, 0.7071067811865475727, 4.937700262164531476E-15 ) ) ;
#83013 = ADVANCED_FACE ( 'NONE', ( #191199 ), #110341, .F. ) ;
#83014 = CIRCLE ( 'NONE', #187131, 1.749999999999999778 ) ;
#83015 = CARTESIAN_POINT ( 'NONE',  ( 21.53752568622133978, 0.09897446127743518562, -93.71319212545147082 ) ) ;
#83016 = DIRECTION ( 'NONE',  ( 1.000000000000000000, 0.000000000000000000, 0.000000000000000000 ) ) ;
#83017 = VECTOR ( 'NONE', #149029, 1000.000000000000000 ) ;
#83018 = DIRECTION ( 'NONE',  ( -1.000000000000000000, -3.265361837132813093E-16, 0.000000000000000000 ) ) ;
#83019 = FACE_OUTER_BOUND ( 'NONE', #98690, .T. ) ;
#83020 = EDGE_CURVE ( 'NONE', #141666, #94057, #154639, .T. ) ;
#83021 = DIRECTION ( 'NONE',  ( 1.000000000000000000, -2.952720810173289112E-16, -2.061873921506763405E-30 ) ) ;
#83022 = SPHERICAL_SURFACE ( 'NONE', #28829, 0.1000000000000000056 ) ;
#83023 = CIRCLE ( 'NONE', #66498, 0.09999999999998898659 ) ;
#83024 = VERTEX_POINT ( 'NONE', #55466 ) ;
#83025 = CARTESIAN_POINT ( 'NONE',  ( 21.07954763557440359, 6.329290990037726772, 0.06587591861843060392 ) ) ;
#83026 = CARTESIAN_POINT ( 'NONE',  ( -18.59999999999999787, 13.98997548377051459, -210.4902890347897255 ) ) ;
#83027 = EDGE_CURVE ( 'NONE', #197069, #204834, #137814, .T. ) ;
#83028 = ORIENTED_EDGE ( 'NONE', *, *, #38334, .F. ) ;
#83029 = DIRECTION ( 'NONE',  ( -0.000000000000000000, -1.000000000000000000, 6.308085367188393199E-16 ) ) ;
#83030 = CIRCLE ( 'NONE', #183043, 0.09999999999999520384 ) ;
#83031 = CARTESIAN_POINT ( 'NONE',  ( -17.29838795457644807, 10.37154985795008599, -189.6047412826164020 ) ) ;
#83032 = EDGE_CURVE ( 'NONE', #7989, #138601, #158714, .T. ) ;
#83033 = AXIS2_PLACEMENT_3D ( 'NONE', #126798, #147645, #227173 ) ;
#83034 = ORIENTED_EDGE ( 'NONE', *, *, #65183, .T. ) ;
#83035 = SPHERICAL_SURFACE ( 'NONE', #121311, 0.1000000000000000056 ) ;
#83036 = DIRECTION ( 'NONE',  ( 1.000000000000000000, 0.000000000000000000, 0.000000000000000000 ) ) ;
#83037 = ORIENTED_EDGE ( 'NONE', *, *, #230464, .T. ) ;
#83038 = CIRCLE ( 'NONE', #183049, 0.09999999999998898659 ) ;
#83039 = ORIENTED_EDGE ( 'NONE', *, *, #62928, .F. ) ;
#83040 = CARTESIAN_POINT ( 'NONE',  ( -21.05000000000000071, 75.96636726467835388, -109.2819246792058010 ) ) ;
#83041 = ORIENTED_EDGE ( 'NONE', *, *, #244043, .T. ) ;
#83042 = CARTESIAN_POINT ( 'NONE',  ( 21.07928932188134041, 0.09889514565463336515, 6.328516656398708307 ) ) ;
#83043 = FACE_OUTER_BOUND ( 'NONE', #219001, .T. ) ;
#83044 = CARTESIAN_POINT ( 'NONE',  ( 21.05000000000000071, 5.000000000011153745, -54.59473398108690390 ) ) ;
#83045 = CARTESIAN_POINT ( 'NONE',  ( -22.47007471830799474, 68.27928934808619488, -203.5231074845244166 ) ) ;
#83046 = CARTESIAN_POINT ( 'NONE',  ( -16.97683810757273193, 66.05000000001230376, -156.7595307720631013 ) ) ;
#83047 = CARTESIAN_POINT ( 'NONE',  ( 20.94999999999999929, 71.00000000001151079, -48.42837350343745584 ) ) ;
#83048 = DIRECTION ( 'NONE',  ( 0.000000000000000000, 0.8814952561688438326, -0.4721928772777334582 ) ) ;
#83049 = DIRECTION ( 'NONE',  ( -0.000000000000000000, -6.982962677686266711E-15, 1.000000000000000000 ) ) ;
#83051 = ORIENTED_EDGE ( 'NONE', *, *, #207818, .F. ) ;
#83050 = CARTESIAN_POINT ( 'NONE',  ( 18.49999999999999289, 55.04793976901536467, -229.8170162380219494 ) ) ;
#83052 = ORIENTED_EDGE ( 'NONE', *, *, #255740, .T. ) ;
#83055 = CARTESIAN_POINT ( 'NONE',  ( -20.64999999999999858, 4.349999999999999645, -21.15000000000000213 ) ) ;
#83054 = DIRECTION ( 'NONE',  ( 0.000000000000000000, 0.000000000000000000, 1.000000000000000000 ) ) ;
#83053 = VECTOR ( 'NONE', #239609, 1000.000000000000000 ) ;
#83057 = ORIENTED_EDGE ( 'NONE', *, *, #183956, .T. ) ;
#83056 = FACE_OUTER_BOUND ( 'NONE', #218755, .T. ) ;
#83058 = ORIENTED_EDGE ( 'NONE', *, *, #184590, .T. ) ;
#83059 = CARTESIAN_POINT ( 'NONE',  ( 20.94999999999999574, -1.835341550224411922, -11.65515129256297833 ) ) ;
#83060 = CARTESIAN_POINT ( 'NONE',  ( 20.97565083910961548, 10.47461740128996510, -175.0779431765885192 ) ) ;
#83061 = CARTESIAN_POINT ( 'NONE',  ( -21.05000000000000071, -0.9150442794618510733, -196.7984890852706030 ) ) ;
#83062 = CYLINDRICAL_SURFACE ( 'NONE', #144076, 0.09999999999998898659 ) ;
#83063 = CARTESIAN_POINT ( 'NONE',  ( 21.05000000000000071, 28.32080209959243788, -238.8452605374484676 ) ) ;
#83064 = DIRECTION ( 'NONE',  ( 0.000000000000000000, -0.1455152366551522025, -0.9893560106964505163 ) ) ;
#83065 = AXIS2_PLACEMENT_3D ( 'NONE', #4477, #206544, #27943 ) ;
#83066 = ORIENTED_EDGE ( 'NONE', *, *, #98787, .T. ) ;
#83068 = VERTEX_POINT ( 'NONE', #52933 ) ;
#83067 = B_SPLINE_CURVE_WITH_KNOTS ( 'NONE', 3,
 ( #144222, #102510, #43865, #41321 ),
 .UNSPECIFIED., .F., .F.,
 ( 4, 4 ),
 ( 0.000000000000000000, 0.001767853679387137913 ),
 .UNSPECIFIED. ) ;
#83069 = CIRCLE ( 'NONE', #66372, 0.2000000000000057288 ) ;
#83070 = DIRECTION ( 'NONE',  ( 1.000000000000000000, 0.000000000000000000, 0.000000000000000000 ) ) ;
#83071 = AXIS2_PLACEMENT_3D ( 'NONE', #192128, #249524, #9605 ) ;
#83072 = CIRCLE ( 'NONE', #74797, 0.1000000000000028644 ) ;
#83073 = VERTEX_POINT ( 'NONE', #150761 ) ;
#83074 = CARTESIAN_POINT ( 'NONE',  ( -21.05000000000000071, 87.75000000001173817, -72.42310748452422331 ) ) ;
#83075 = ORIENTED_EDGE ( 'NONE', *, *, #23990, .T. ) ;
#83076 = CARTESIAN_POINT ( 'NONE',  ( -16.78493211734303614, 9.945835743215324598, -154.8360509808959478 ) ) ;
#83077 = AXIS2_PLACEMENT_3D ( 'NONE', #157788, #138150, #133052 ) ;
#83078 = DIRECTION ( 'NONE',  ( 0.000000000000000000, 0.9126074666063844765, 0.4088369013363113980 ) ) ;
#83079 = EDGE_CURVE ( 'NONE', #249684, #146711, #115474, .T. ) ;
#83080 = CARTESIAN_POINT ( 'NONE',  ( 18.49999999999999289, 65.79142135392832813, -44.82060061889436753 ) ) ;
#83081 = DIRECTION ( 'NONE',  ( 0.7071067811865487940, 0.000000000000000000, -0.7071067811865463515 ) ) ;
#83082 = ORIENTED_EDGE ( 'NONE', *, *, #32918, .T. ) ;
#83083 = CARTESIAN_POINT ( 'NONE',  ( -18.59999999999999787, 64.35000000001187459, -90.87310748452438247 ) ) ;
#83084 = ORIENTED_EDGE ( 'NONE', *, *, #249637, .F. ) ;
#83085 = EDGE_CURVE ( 'NONE', #2697, #34062, #73818, .T. ) ;
#83086 = CARTESIAN_POINT ( 'NONE',  ( -21.05000000000000071, 77.16270174994990327, -94.92310748452430857 ) ) ;
#83088 = ADVANCED_FACE ( 'NONE', ( #34684 ), #183631, .T. ) ;
#83087 = CIRCLE ( 'NONE', #95766, 0.1000000000000000888 ) ;
#83089 = CARTESIAN_POINT ( 'NONE',  ( 21.05000000000000071, 8.776282895303632259, -146.1500000000000341 ) ) ;
#83091 = TOROIDAL_SURFACE ( 'NONE', #208055, 0.2000000000000000111, 0.1000000000000000056 ) ;
#83090 = DIRECTION ( 'NONE',  ( 0.000000000000000000, 1.000000000000000000, 6.982962677686266711E-15 ) ) ;
#83092 = DIRECTION ( 'NONE',  ( 1.000000000000000000, -0.000000000000000000, -0.000000000000000000 ) ) ;
#83093 = ORIENTED_EDGE ( 'NONE', *, *, #47166, .T. ) ;
#83094 = CARTESIAN_POINT ( 'NONE',  ( 22.50000000000000000, 75.90000000001219860, -144.3138870828976792 ) ) ;
#83095 = ORIENTED_EDGE ( 'NONE', *, *, #135431, .F. ) ;
#83098 = EDGE_LOOP ( 'NONE', ( #25438, #48912, #9554, #253137 ) ) ;
#83097 = CARTESIAN_POINT ( 'NONE',  ( 18.43709777086140278, -9.682403433465237796, -107.1568433774128835 ) ) ;
#83096 = CARTESIAN_POINT ( 'NONE',  ( 23.14999999999999858, 1.115649653272650466E-11, -130.0000000000000284 ) ) ;
#83099 = AXIS2_PLACEMENT_3D ( 'NONE', #88710, #189123, #30077 ) ;
#83100 = CARTESIAN_POINT ( 'NONE',  ( 23.24999999999999645, 3.900000000011155432, -134.0000000000000284 ) ) ;
#83101 = ORIENTED_EDGE ( 'NONE', *, *, #199471, .T. ) ;
#83102 = CARTESIAN_POINT ( 'NONE',  ( -20.64999999999999858, 7.150000000011155876, -188.6499999999999488 ) ) ;
#83103 = VERTEX_POINT ( 'NONE', #114195 ) ;
#83104 = CARTESIAN_POINT ( 'NONE',  ( 20.95000000000005258, 64.35000000001120668, -29.92310748452479174 ) ) ;
#83105 = ADVANCED_FACE ( 'NONE', ( #90766 ), #72523, .T. ) ;
#83106 = CARTESIAN_POINT ( 'NONE',  ( -16.87331047859651179, 12.41403342719998726, -211.2428889513006993 ) ) ;
#83107 = DIRECTION ( 'NONE',  ( 0.000000000000000000, 0.000000000000000000, -1.000000000000000000 ) ) ;
#83108 = UNCERTAINTY_MEASURE_WITH_UNIT (LENGTH_MEASURE( 1.000000000000000082E-05 ), #7985, 'distance_accuracy_value', 'NONE');
#83109 = DIRECTION ( 'NONE',  ( -2.915501640297152804E-16, -1.000000000000000000, -6.997203936713167125E-15 ) ) ;
#83110 = DIRECTION ( 'NONE',  ( 0.000000000000000000, -7.272083257015735086E-15, 1.000000000000000000 ) ) ;
#83111 = ORIENTED_EDGE ( 'NONE', *, *, #238546, .F. ) ;
#83112 = DIRECTION ( 'NONE',  ( 0.000000000000000000, 0.9770955615653259541, 0.2128009952263860971 ) ) ;
#83113 = DIRECTION ( 'NONE',  ( 0.000000000000000000, 0.4999999999999348299, -0.8660254037844762331 ) ) ;
#83114 = CARTESIAN_POINT ( 'NONE',  ( -18.48408745364672967, -9.664322258652003228, -140.6830785333283416 ) ) ;
#83115 = CIRCLE ( 'NONE', #58006, 0.4999999999999978351 ) ;
#83116 = VERTEX_POINT ( 'NONE', #32120 ) ;
#83117 = DIRECTION ( 'NONE',  ( 0.000000000000000000, 0.9908441862701791170, -0.1350103645450472789 ) ) ;
#83118 = ORIENTED_EDGE ( 'NONE', *, *, #57836, .T. ) ;
#83119 = CARTESIAN_POINT ( 'NONE',  ( 18.39999999999999858, 8.780520186313291120, -245.4165333277510115 ) ) ;
#83120 = EDGE_CURVE ( 'NONE', #134698, #50347, #237791, .T. ) ;
#83121 = DIRECTION ( 'NONE',  ( 1.000000000000000000, 0.000000000000000000, 0.000000000000000000 ) ) ;
#83122 = CARTESIAN_POINT ( 'NONE',  ( 20.96077737575343747, 36.10128815642510602, -236.0658802525694568 ) ) ;
#83123 = EDGE_CURVE ( 'NONE', #53539, #201670, #200163, .T. ) ;
#83124 = AXIS2_PLACEMENT_3D ( 'NONE', #14657, #216682, #194582 ) ;
#83126 = EDGE_LOOP ( 'NONE', ( #14244, #131605, #32771, #129811 ) ) ;
#83125 = CARTESIAN_POINT ( 'NONE',  ( -16.94333152886235894, 9.990342011461637028, -146.6079684689456144 ) ) ;
#83127 = FACE_OUTER_BOUND ( 'NONE', #35542, .T. ) ;
#83128 = CARTESIAN_POINT ( 'NONE',  ( -23.25000000000000355, 10.05000000001113847, -113.2500000000000284 ) ) ;
#83129 = CARTESIAN_POINT ( 'NONE',  ( -20.54999999999999716, -11.74999999998884626, -79.35000000000005116 ) ) ;
#83131 = EDGE_CURVE ( 'NONE', #36544, #104788, #63111, .T. ) ;
#83130 = ORIENTED_EDGE ( 'NONE', *, *, #96457, .F. ) ;
#83132 = SPHERICAL_SURFACE ( 'NONE', #160142, 0.1000000000000000056 ) ;
#83133 = CARTESIAN_POINT ( 'NONE',  ( 20.94999999999999574, 87.48912529308842068, -167.1231074845242688 ) ) ;
#83134 = VERTEX_POINT ( 'NONE', #119343 ) ;
#83135 = AXIS2_PLACEMENT_3D ( 'NONE', #23747, #244032, #84929 ) ;
#83136 = AXIS2_PLACEMENT_3D ( 'NONE', #182841, #47124, #203660 ) ;
#83137 = ORIENTED_EDGE ( 'NONE', *, *, #171033, .F. ) ;
#83138 = DIRECTION ( 'NONE',  ( 0.000000000000000000, 0.4999999999999478195, -0.8660254037844686836 ) ) ;
#83139 = ORIENTED_EDGE ( 'NONE', *, *, #198246, .T. ) ;
#83141 = ORIENTED_EDGE ( 'NONE', *, *, #163657, .F. ) ;
#83140 = CARTESIAN_POINT ( 'NONE',  ( -21.64999999999999858, 53.08776555244186568, -234.2469744149522626 ) ) ;
#83142 = AXIS2_PLACEMENT_3D ( 'NONE', #7279, #201636, #101209 ) ;
#83143 = TOROIDAL_SURFACE ( 'NONE', #183166, 0.2000000000000000111, 0.1000000000000000056 ) ;
#83144 = AXIS2_PLACEMENT_3D ( 'NONE', #122851, #235389, #118016 ) ;
#83148 = EDGE_CURVE ( 'NONE', #208580, #111080, #118047, .T. ) ;
#83147 = ORIENTED_EDGE ( 'NONE', *, *, #19678, .F. ) ;
#83146 = ORIENTED_EDGE ( 'NONE', *, *, #185154, .T. ) ;
#83145 = CARTESIAN_POINT ( 'NONE',  ( -16.87683809663752399, 9.850000000011140955, -79.65000000000004832 ) ) ;
#83149 = CARTESIAN_POINT ( 'NONE',  ( 20.85000000000000142, 1.115600667400684642E-11, -200.9999999999999432 ) ) ;
#83150 = CARTESIAN_POINT ( 'NONE',  ( 21.05000000000000071, 5.000000000011153745, -88.09473398108696074 ) ) ;
#83151 = DIRECTION ( 'NONE',  ( 1.186688945009010077E-16, 1.000000000000000000, 6.982962677686266711E-15 ) ) ;
#83153 = DIRECTION ( 'NONE',  ( -3.265361837132813093E-16, 1.000000000000000000, 0.000000000000000000 ) ) ;
#83152 = FACE_OUTER_BOUND ( 'NONE', #21248, .T. ) ;
#83154 = FACE_OUTER_BOUND ( 'NONE', #78668, .T. ) ;
#83155 = CARTESIAN_POINT ( 'NONE',  ( -22.45305610364634674, 25.97741635855165399, -254.4468634167652681 ) ) ;
#83156 = CIRCLE ( 'NONE', #199752, 0.1000000000000124678 ) ;
#83157 = SPHERICAL_SURFACE ( 'NONE', #197239, 0.1000000000000000056 ) ;
#83159 = CARTESIAN_POINT ( 'NONE',  ( 23.15000000000000213, -11.39257802169451139, -97.42605042016811012 ) ) ;
#83158 = CYLINDRICAL_SURFACE ( 'NONE', #101127, 0.1000000000000028644 ) ;
#83160 = AXIS2_PLACEMENT_3D ( 'NONE', #101276, #4768, #223825 ) ;
#83161 = TOROIDAL_SURFACE ( 'NONE', #124907, 7.791421356237335338, 0.1000000000000000056 ) ;
#83162 = ORIENTED_EDGE ( 'NONE', *, *, #92479, .F. ) ;
#83163 = CIRCLE ( 'NONE', #20686, 0.1000000000000028644 ) ;
#83165 = ORIENTED_EDGE ( 'NONE', *, *, #106189, .F. ) ;
#83164 = TOROIDAL_SURFACE ( 'NONE', #141458, 12.97499999999999787, 0.1000000000000000056 ) ;
#83166 = ADVANCED_FACE ( 'NONE', ( #138856 ), #203257, .F. ) ;
#83167 = CARTESIAN_POINT ( 'NONE',  ( -20.96077737575346944, 64.37609936600699712, -76.38231552741797259 ) ) ;
#83168 = ADVANCED_FACE ( 'NONE', ( #76333 ), #237984, .F. ) ;
#83170 = ORIENTED_EDGE ( 'NONE', *, *, #44679, .F. ) ;
#83169 = DIRECTION ( 'NONE',  ( 0.000000000000000000, -0.07893460099012301889, 0.9968797965484754720 ) ) ;
#83171 = VERTEX_POINT ( 'NONE', #20248 ) ;
#83172 = CIRCLE ( 'NONE', #108173, 0.1000000000000029060 ) ;
#83173 = DIRECTION ( 'NONE',  ( -0.000000000000000000, 0.1350103645451835865, 0.9908441862701605762 ) ) ;
#83174 = ORIENTED_EDGE ( 'NONE', *, *, #11962, .F. ) ;
#83175 = CYLINDRICAL_SURFACE ( 'NONE', #237716, 0.09999999999998898659 ) ;
#83176 = EDGE_CURVE ( 'NONE', #96815, #80054, #141920, .T. ) ;
#83177 = ADVANCED_FACE ( 'NONE', ( #217120 ), #239288, .F. ) ;
#83178 = ORIENTED_EDGE ( 'NONE', *, *, #96936, .F. ) ;
#83179 = CARTESIAN_POINT ( 'NONE',  ( -18.50000000000000000, 66.65000000001259650, -191.1731074845244223 ) ) ;
#83180 = DIRECTION ( 'NONE',  ( -0.000000000000000000, 0.9770955615653313941, 0.2128009952263606730 ) ) ;
#83181 = EDGE_CURVE ( 'NONE', #179010, #38660, #180598, .T. ) ;
#83183 = ORIENTED_EDGE ( 'NONE', *, *, #193734, .T. ) ;
#83182 = VERTEX_POINT ( 'NONE', #256200 ) ;
#83184 = EDGE_LOOP ( 'NONE', ( #84443, #187244 ) ) ;
#83187 = EDGE_CURVE ( 'NONE', #6496, #171633, #21337, .T. ) ;
#83186 = EDGE_CURVE ( 'NONE', #5245, #78167, #240569, .T. ) ;
#83185 = CARTESIAN_POINT ( 'NONE',  ( 18.59999999999998366, 76.00000000001190870, -103.0231074845243029 ) ) ;
#83188 = VERTEX_POINT ( 'NONE', #235413 ) ;
#83189 = ORIENTED_EDGE ( 'NONE', *, *, #241156, .T. ) ;
#83190 = CARTESIAN_POINT ( 'NONE',  ( -21.05000000000000071, -11.29603075032412463, -164.4521008403361577 ) ) ;
#83191 = DIRECTION ( 'NONE',  ( 1.000000000000000000, -0.000000000000000000, -0.000000000000000000 ) ) ;
#83193 = ORIENTED_EDGE ( 'NONE', *, *, #167173, .F. ) ;
#83192 = FACE_OUTER_BOUND ( 'NONE', #50364, .T. ) ;
#83194 = ADVANCED_FACE ( 'NONE', ( #136297 ), #215842, .F. ) ;
#83196 = FACE_OUTER_BOUND ( 'NONE', #121715, .T. ) ;
#83195 = DIRECTION ( 'NONE',  ( 0.000000000000000000, 0.000000000000000000, -1.000000000000000000 ) ) ;
#83197 = CARTESIAN_POINT ( 'NONE',  ( 21.10257677756355932, 0.02495074957913740246, -60.60161825746730102 ) ) ;
#83198 = SPHERICAL_SURFACE ( 'NONE', #252671, 0.1000000000000000056 ) ;
#83199 = DIRECTION ( 'NONE',  ( -0.000000000000000000, 0.1332476588733589318, 0.9910827722268050755 ) ) ;
#83200 = ORIENTED_EDGE ( 'NONE', *, *, #200928, .F. ) ;
#83201 = CIRCLE ( 'NONE', #178951, 6.329289321881370611 ) ;
#83202 = ORIENTED_EDGE ( 'NONE', *, *, #85862, .T. ) ;
#83203 = CARTESIAN_POINT ( 'NONE',  ( 18.49999999999999289, 65.79142135624951493, -145.2559501969990379 ) ) ;
#83205 = EDGE_CURVE ( 'NONE', #136568, #214442, #71211, .T. ) ;
#83204 = CARTESIAN_POINT ( 'NONE',  ( -20.94999999999999929, 4.272272088314018390, -245.4186996786394843 ) ) ;
#83206 = VECTOR ( 'NONE', #125198, 1000.000000000000000 ) ;
#83207 = ORIENTED_EDGE ( 'NONE', *, *, #114094, .T. ) ;
#83208 = CARTESIAN_POINT ( 'NONE',  ( 21.17356465864818560, 0.09891124102502621418, -27.07719687375827533 ) ) ;
#83209 = EDGE_CURVE ( 'NONE', #23059, #37930, #222256, .T. ) ;
#83210 = ADVANCED_FACE ( 'NONE', ( #25394 ), #146577, .T. ) ;
#83211 = CIRCLE ( 'NONE', #62404, 12.97499999999999964 ) ;
#83212 = FACE_OUTER_BOUND ( 'NONE', #180358, .T. ) ;
#83213 = CARTESIAN_POINT ( 'NONE',  ( 18.59999999999999076, 76.00000000001244871, -170.0231074845243597 ) ) ;
#83214 = ORIENTED_EDGE ( 'NONE', *, *, #81848, .T. ) ;
#83215 = ORIENTED_EDGE ( 'NONE', *, *, #173941, .F. ) ;
#83216 = ADVANCED_FACE ( 'NONE', ( #29276 ), #185738, .F. ) ;
#83217 = DIRECTION ( 'NONE',  ( 0.000000000000000000, 1.000000000000000000, 0.000000000000000000 ) ) ;
#83218 = DIRECTION ( 'NONE',  ( 0.000000000000000000, -6.982962677686267499E-15, 1.000000000000000000 ) ) ;
#83219 = ORIENTED_EDGE ( 'NONE', *, *, #175367, .F. ) ;
#83220 = CARTESIAN_POINT ( 'NONE',  ( 20.94999999999999929, 63.43511439055885148, -224.4466865888566360 ) ) ;
#83221 = ORIENTED_EDGE ( 'NONE', *, *, #4076, .F. ) ;
#83222 = DIRECTION ( 'NONE',  ( 0.000000000000000000, -0.2617529984165023471, -0.9651348961777159730 ) ) ;
#83224 = DIRECTION ( 'NONE',  ( 0.000000000000000000, 0.9126074666063545004, 0.4088369013363783999 ) ) ;
#83223 = DIRECTION ( 'NONE',  ( -0.000000000000000000, -1.000000000000000000, -7.272083257015735086E-15 ) ) ;
#83225 = EDGE_CURVE ( 'NONE', #221499, #190980, #33828, .T. ) ;
#83226 = CIRCLE ( 'NONE', #112312, 2.000000000000001776 ) ;
#83227 = CARTESIAN_POINT ( 'NONE',  ( 22.47110162079220785, 0.02879741281384913879, -55.35006406331571327 ) ) ;
#83228 = CARTESIAN_POINT ( 'NONE',  ( 23.24999999999999289, 64.35000000001237197, -170.0231074845244166 ) ) ;
#83229 = TOROIDAL_SURFACE ( 'NONE', #120695, 11.65000000000000036, 0.1000000000000000056 ) ;
#83230 = EDGE_CURVE ( 'NONE', #24547, #38614, #129459, .T. ) ;
#83231 = ORIENTED_EDGE ( 'NONE', *, *, #239697, .T. ) ;
#83232 = CARTESIAN_POINT ( 'NONE',  ( -16.78270389226383230, 63.08596654800939518, -213.1367957079248185 ) ) ;
#83233 = CIRCLE ( 'NONE', #75099, 0.09999999999999917288 ) ;
#83234 =( BOUNDED_CURVE ( )  B_SPLINE_CURVE ( 3, ( #106525, #21886, #201792, #72578 ),
 .UNSPECIFIED., .F., .T. ) 
 B_SPLINE_CURVE_WITH_KNOTS ( ( 4, 4 ),
 ( 3.141592653589791784, 4.712388980384688786 ),
 .UNSPECIFIED. ) 
 CURVE ( )  GEOMETRIC_REPRESENTATION_ITEM ( )  RATIONAL_B_SPLINE_CURVE ( ( 1.000000000000000000, 0.8047378541243649375, 0.8047378541243649375, 1.000000000000000000 ) ) 
 REPRESENTATION_ITEM ( '' )  );
#83236 = EDGE_LOOP ( 'NONE', ( #44972, #237911, #141901, #152755 ) ) ;
#83235 = ORIENTED_EDGE ( 'NONE', *, *, #198958, .T. ) ;
#83237 = VERTEX_POINT ( 'NONE', #127042 ) ;
#83238 = ORIENTED_EDGE ( 'NONE', *, *, #133135, .T. ) ;
#83239 = DIRECTION ( 'NONE',  ( 0.000000000000000000, 6.938893903907222067E-15, -1.000000000000000000 ) ) ;
#83240 = FACE_OUTER_BOUND ( 'NONE', #208759, .T. ) ;
#83241 = DIRECTION ( 'NONE',  ( 0.000000000000000000, 0.000000000000000000, 1.000000000000000000 ) ) ;
#83242 = DIRECTION ( 'NONE',  ( -1.000000000000000000, 0.000000000000000000, 0.000000000000000000 ) ) ;
#83243 = DIRECTION ( 'NONE',  ( -0.000000000000000000, 0.9651348961777158619, -0.2617529984165031243 ) ) ;
#83244 = EDGE_CURVE ( 'NONE', #107897, #215945, #164889, .T. ) ;
#83246 = DIRECTION ( 'NONE',  ( 7.304098846218132695E-16, -0.9770955615653315052, -0.2128009952263603954 ) ) ;
#83245 = CARTESIAN_POINT ( 'NONE',  ( 22.41477678272288188, -3.139831800996500721, -228.2311238840898397 ) ) ;
#83248 = ORIENTED_EDGE ( 'NONE', *, *, #195597, .T. ) ;
#83247 = DIRECTION ( 'NONE',  ( 0.000000000000000000, -0.9915357197604982575, 0.1298341882519033486 ) ) ;
#83249 = CARTESIAN_POINT ( 'NONE',  ( 20.94999999999999574, 87.48912529308842068, -166.9231074845242802 ) ) ;
#83250 = VERTEX_POINT ( 'NONE', #104864 ) ;
#83251 = CARTESIAN_POINT ( 'NONE',  ( 21.53551880898956838, 33.79472821003547267, -243.3997680843710611 ) ) ;
#83252 = ORIENTED_EDGE ( 'NONE', *, *, #146864, .F. ) ;
#83253 = ORIENTED_EDGE ( 'NONE', *, *, #257141, .F. ) ;
#83254 = DIRECTION ( 'NONE',  ( -1.000000000000000000, 0.000000000000000000, 0.000000000000000000 ) ) ;
#83255 = CARTESIAN_POINT ( 'NONE',  ( 0.9000000000000547562, 66.35000000001119247, -7.423107484524793520 ) ) ;
#83256 = CARTESIAN_POINT ( 'NONE',  ( -16.87998658237717109, 66.05000000001153637, -48.88674705226281958 ) ) ;
#83257 = CARTESIAN_POINT ( 'NONE',  ( 15.39793903038208001, 9.389686005666810331, -82.67284350635134160 ) ) ;
#83258 = CIRCLE ( 'NONE', #245605, 0.1999999999999987899 ) ;
#83259 = VECTOR ( 'NONE', #110043, 1000.000000000000114 ) ;
#83260 = CARTESIAN_POINT ( 'NONE',  ( -18.59999999999999787, 1.851028230140860487, -11.65391326942249250 ) ) ;
#83261 = ORIENTED_EDGE ( 'NONE', *, *, #177493, .T. ) ;
#83262 = ORIENTED_EDGE ( 'NONE', *, *, #75351, .T. ) ;
#83263 = LINE ( 'NONE', #6312, #165564 ) ;
#83264 = VERTEX_POINT ( 'NONE', #5782 ) ;
#83265 = CARTESIAN_POINT ( 'NONE',  ( 20.94999999999999574, 1.835341550235567887, -145.5551512925629822 ) ) ;
#83266 = CARTESIAN_POINT ( 'NONE',  ( -16.93658623642902938, 9.980381671668283161, -46.11190272912921273 ) ) ;
#83267 = LINE ( 'NONE', #162861, #107141 ) ;
#83268 = DIRECTION ( 'NONE',  ( 1.000000000000000000, 0.000000000000000000, 0.000000000000000000 ) ) ;
#83269 = CARTESIAN_POINT ( 'NONE',  ( -22.32929514600008503, 75.90092432189828742, -144.1017550499008166 ) ) ;
#83270 = CARTESIAN_POINT ( 'NONE',  ( 20.94999999999999929, 5.850000000011156942, -157.3675027757221017 ) ) ;
#83271 = CARTESIAN_POINT ( 'NONE',  ( -0.8999999999999437339, 67.75000000001118394, -7.423107484524793520 ) ) ;
#83272 = DIRECTION ( 'NONE',  ( 0.000000000000000000, 0.3738317757009345654, 0.9274965247785492695 ) ) ;
#83273 = CARTESIAN_POINT ( 'NONE',  ( 18.59999999999999076, 10.20857864376269575, -24.75000000000000000 ) ) ;
#83274 = CARTESIAN_POINT ( 'NONE',  ( -21.05000000000000071, 69.09936979046463534, -247.6075824278584889 ) ) ;
#83275 = CIRCLE ( 'NONE', #116614, 0.09999999999998904210 ) ;
#83276 = ADVANCED_FACE ( 'NONE', ( #68361 ), #34996, .F. ) ;
#83277 = DIRECTION ( 'NONE',  ( 1.000000000000000000, 0.000000000000000000, 0.000000000000000000 ) ) ;
#83278 = AXIS2_PLACEMENT_3D ( 'NONE', #257640, #76493, #217274 ) ;
#83279 = VECTOR ( 'NONE', #110537, 1000.000000000000000 ) ;
#83280 = DIRECTION ( 'NONE',  ( 1.000000000000000000, 3.448943450116721596E-16, 6.438528483529603700E-16 ) ) ;
#83281 = EDGE_CURVE ( 'NONE', #117646, #94122, #154442, .T. ) ;
#83282 = ORIENTED_EDGE ( 'NONE', *, *, #120711, .T. ) ;
#83283 = VECTOR ( 'NONE', #103847, 1000.000000000000000 ) ;
#83284 = EDGE_CURVE ( 'NONE', #12967, #143950, #211735, .T. ) ;
#83285 = CARTESIAN_POINT ( 'NONE',  ( -18.59999999999999787, 7.021664781911246322, -70.83356540189728889 ) ) ;
#83286 = ADVANCED_FACE ( 'NONE', ( #233853 ), #108606, .T. ) ;
#83287 = EDGE_LOOP ( 'NONE', ( #173423, #117499, #81900, #4206 ) ) ;
#83288 =( BOUNDED_SURFACE ( )  B_SPLINE_SURFACE ( 3, 2, ( 
 ( #177735, #77307, #257182 ),
 ( #40791, #194726, #214266 ),
 ( #137281, #16094, #159441 ),
 ( #78592, #76034, #195998 ),
 ( #18628, #238971, #158188 ),
 ( #235117, #98128, #81147 ),
 ( #215538, #39513, #237679 ),
 ( #55153, #36949, #100692 ),
 ( #59004, #155612, #236388 ),
 ( #216817, #115164, #197264 ) ),
 .UNSPECIFIED., .F., .F., .F. ) 
 B_SPLINE_SURFACE_WITH_KNOTS ( ( 4, 2, 2, 2, 4 ),
 ( 3, 3 ),
 ( 0.002161241639767785133, 0.002579950749617447234, 0.002789305304542278284, 0.002893982582004694243, 0.002998659859467109768 ),
 ( 0.000000000000000000, 1.000000000000000000 ),
 .UNSPECIFIED. ) 
 GEOMETRIC_REPRESENTATION_ITEM ( )  RATIONAL_B_SPLINE_SURFACE ( (
 ( 1.000000000000000000, 0.7071067811864923947, 1.000000000000000000),
 ( 1.000000000000000000, 0.7632447400663529002, 1.000000000000000000),
 ( 1.000000000000000000, 0.8158073005109872655, 1.000000000000000000),
 ( 1.000000000000000000, 0.8906973462395572083, 1.000000000000000000),
 ( 1.000000000000000000, 0.9149408947799931857, 1.000000000000000000),
 ( 1.000000000000000000, 0.9493368785275779764, 1.000000000000000000),
 ( 1.000000000000000000, 0.9605194247155937060, 1.000000000000000000),
 ( 1.000000000000000000, 0.9803630264781856285, 1.000000000000000000),
 ( 1.000000000000000000, 0.9900844824270625955, 1.000000000000000000),
 ( 1.000000000000000000, 0.9894588281429246290, 1.000000000000000000) ) ) 
 REPRESENTATION_ITEM ( '' )  SURFACE ( )  );
#83289 = LINE ( 'NONE', #145846, #112614 ) ;
#83290 = CARTESIAN_POINT ( 'NONE',  ( -18.39999999999999858, -9.499999999988849808, -140.6001893912220737 ) ) ;
#83291 = DIRECTION ( 'NONE',  ( 1.000000000000000000, 0.000000000000000000, -0.000000000000000000 ) ) ;
#83292 = ORIENTED_EDGE ( 'NONE', *, *, #180886, .T. ) ;
#83294 = AXIS2_PLACEMENT_3D ( 'NONE', #152441, #251497, #212400 ) ;
#83293 = CARTESIAN_POINT ( 'NONE',  ( -18.59999999999999787, 1.115600667400684642E-11, -134.0000000000000000 ) ) ;
#83295 = CARTESIAN_POINT ( 'NONE',  ( -20.65000000000000568, 70.35000000001160458, -60.27310748452436684 ) ) ;
#83296 = DIRECTION ( 'NONE',  ( 1.000000000000000000, 3.190570557967288949E-16, 6.948722487160392945E-17 ) ) ;
#83297 = DIRECTION ( 'NONE',  ( 1.000000000000000000, 0.000000000000000000, 0.000000000000000000 ) ) ;
#83298 = DIRECTION ( 'NONE',  ( 1.000000000000000000, 0.000000000000000000, 0.000000000000000000 ) ) ;
#83299 = CARTESIAN_POINT ( 'NONE',  ( 22.47110162079220785, 75.97120258720977404, -181.6730434212086891 ) ) ;
#83300 = ORIENTED_EDGE ( 'NONE', *, *, #202166, .F. ) ;
#83301 = DIRECTION ( 'NONE',  ( -2.952720810173289112E-16, 1.000000000000000000, 0.000000000000000000 ) ) ;
#83303 = ORIENTED_EDGE ( 'NONE', *, *, #86451, .T. ) ;
#83302 = CARTESIAN_POINT ( 'NONE',  ( 22.48970261584622321, 11.65000000001115588, -167.4446305117825773 ) ) ;
#83304 = DIRECTION ( 'NONE',  ( 1.000000000000000000, 0.000000000000000000, 0.000000000000000000 ) ) ;
#83305 = DIRECTION ( 'NONE',  ( -3.469446951953515108E-14, 0.000000000000000000, 1.000000000000000000 ) ) ;
#83306 = SURFACE_STYLE_FILL_AREA ( #140745 ) ;
#83307 = EDGE_LOOP ( 'NONE', ( #135256, #177539, #185307, #214232, #120011, #224293, #47254, #188042, #33314, #121107, #99037, #200558, #143421, #175825 ) ) ;
#83308 = FACE_OUTER_BOUND ( 'NONE', #184719, .T. ) ;
#83309 = DIRECTION ( 'NONE',  ( 1.000000000000000000, -0.000000000000000000, -0.000000000000000000 ) ) ;
#83310 = ORIENTED_EDGE ( 'NONE', *, *, #54643, .F. ) ;
#83311 = FACE_OUTER_BOUND ( 'NONE', #188611, .T. ) ;
#83312 = LINE ( 'NONE', #82027, #242554 ) ;
#83313 = CIRCLE ( 'NONE', #229094, 0.1000000000000028644 ) ;
#83314 = EDGE_CURVE ( 'NONE', #14771, #2240, #62815, .T. ) ;
#83315 = CARTESIAN_POINT ( 'NONE',  ( -21.05000000000000071, 2.859758780633683273, -208.6670499591424459 ) ) ;
#83316 = ORIENTED_EDGE ( 'NONE', *, *, #225671, .F. ) ;
#83317 = AXIS2_PLACEMENT_3D ( 'NONE', #239809, #201961, #40356 ) ;
#83318 = ORIENTED_EDGE ( 'NONE', *, *, #208019, .F. ) ;
#83319 = LINE ( 'NONE', #5065, #189009 ) ;
#83320 = DIRECTION ( 'NONE',  ( -0.000000000000000000, -6.982962677686266711E-15, 1.000000000000000000 ) ) ;
#83321 = EDGE_CURVE ( 'NONE', #91629, #141665, #162793, .T. ) ;
#83322 = LINE ( 'NONE', #2520, #94743 ) ;
#83323 = CYLINDRICAL_SURFACE ( 'NONE', #111041, 11.75000000000000178 ) ;
#83324 = CARTESIAN_POINT ( 'NONE',  ( 18.49999999999999289, 10.34378108836433263, -125.3284452778770373 ) ) ;
#83325 = SPHERICAL_SURFACE ( 'NONE', #134677, 0.1000000000000000056 ) ;
#83326 = ADVANCED_FACE ( 'NONE', ( #149198 ), #10957, .F. ) ;
#83328 = CARTESIAN_POINT ( 'NONE',  ( -18.41353343127311248, -9.499999999988851584, -74.03206939669972542 ) ) ;
#83327 = CARTESIAN_POINT ( 'NONE',  ( 22.00411653962170533, 7.253442868370061802, 0.09903810578604116399 ) ) ;
#83329 = CARTESIAN_POINT ( 'NONE',  ( 21.05000000000000071, 11.65000000001116298, -59.98519422934605672 ) ) ;
#83330 = LINE ( 'NONE', #178649, #160462 ) ;
#83331 = DIRECTION ( 'NONE',  ( 0.000000000000000000, 0.9126074666063920260, 0.4088369013362946891 ) ) ;
#83332 = CARTESIAN_POINT ( 'NONE',  ( 20.95203847575071521, 18.75769682750340905, -228.0491834549998771 ) ) ;
#83333 = AXIS2_PLACEMENT_3D ( 'NONE', #127646, #89782, #247587 ) ;
#83334 = VERTEX_POINT ( 'NONE', #50070 ) ;
#83335 = ORIENTED_EDGE ( 'NONE', *, *, #192730, .F. ) ;
#83336 = PLANE ( 'NONE',  #94262 ) ;
#83337 = AXIS2_PLACEMENT_3D ( 'NONE', #202072, #65116, #23465 ) ;
#83338 = CARTESIAN_POINT ( 'NONE',  ( -18.37013991200266361, 64.50025238380023040, -145.7300844740073273 ) ) ;
#83340 = DIRECTION ( 'NONE',  ( 1.000000000000000000, 0.000000000000000000, 0.000000000000000000 ) ) ;
#83339 = LINE ( 'NONE', #199493, #221349 ) ;
#83341 = EDGE_CURVE ( 'NONE', #49841, #248091, #229992, .T. ) ;
#83342 = CIRCLE ( 'NONE', #124886, 0.09999999999999939493 ) ;
#83343 = FACE_OUTER_BOUND ( 'NONE', #220466, .T. ) ;
#83344 = DIRECTION ( 'NONE',  ( 0.000000000000000000, 0.000000000000000000, 1.000000000000000000 ) ) ;
#83345 = DIRECTION ( 'NONE',  ( 0.000000000000000000, 0.000000000000000000, -1.000000000000000000 ) ) ;
#83346 = ADVANCED_FACE ( 'NONE', ( #51325 ), #31829, .F. ) ;
#83347 = AXIS2_PLACEMENT_3D ( 'NONE', #170601, #68897, #169305 ) ;
#83348 = ADVANCED_FACE ( 'NONE', ( #252119 ), #189600, .F. ) ;
#83349 = CARTESIAN_POINT ( 'NONE',  ( 22.60000000000000142, 11.74956712350054744, -66.89914163090134025 ) ) ;
#83350 = AXIS2_PLACEMENT_3D ( 'NONE', #104226, #62560, #200780 ) ;
#83351 = ORIENTED_EDGE ( 'NONE', *, *, #72926, .F. ) ;
#83352 = LINE ( 'NONE', #45545, #247061 ) ;
#83353 = EDGE_CURVE ( 'NONE', #236784, #215460, #130889, .T. ) ;
#83354 = ORIENTED_EDGE ( 'NONE', *, *, #181033, .F. ) ;
#83355 = CARTESIAN_POINT ( 'NONE',  ( -20.54999999999999716, 1.940186915887848196, -20.67088078894667547 ) ) ;
#83356 = VECTOR ( 'NONE', #215730, 1000.000000000000000 ) ;
#83358 = CIRCLE ( 'NONE', #212585, 0.09999999999999971412 ) ;
#83357 = CARTESIAN_POINT ( 'NONE',  ( -20.94999999999994600, 65.15000000001120384, -4.423107484524790856 ) ) ;
#83359 = TOROIDAL_SURFACE ( 'NONE', #125102, 0.2000000000000000111, 0.1000000000000000056 ) ;
#83360 = CIRCLE ( 'NONE', #70955, 0.09999999999999939493 ) ;
#83361 = VERTEX_POINT ( 'NONE', #73523 ) ;
#83362 = DIRECTION ( 'NONE',  ( 0.000000000000000000, -0.9126074666063660468, -0.4088369013363524762 ) ) ;
#83363 = ADVANCED_FACE ( 'NONE', ( #113900 ), #170822, .T. ) ;
#83364 = ORIENTED_EDGE ( 'NONE', *, *, #151538, .T. ) ;
#83365 = DIRECTION ( 'NONE',  ( 1.000000000000000000, 0.000000000000000000, 0.000000000000000000 ) ) ;
#83366 = DIRECTION ( 'NONE',  ( 1.836970198721029934E-16, -1.000000000000000000, -0.000000000000000000 ) ) ;
#83367 = CARTESIAN_POINT ( 'NONE',  ( -18.50000000000000000, 9.150000000011157653, -79.35000000000005116 ) ) ;
#83368 = CARTESIAN_POINT ( 'NONE',  ( -18.47690164073607377, 77.21658254787745079, -241.7530424840200851 ) ) ;
#83369 = CARTESIAN_POINT ( 'NONE',  ( 23.15000000000000213, -11.64999999999999147, -30.39999999999999503 ) ) ;
#83370 = CIRCLE ( 'NONE', #229154, 0.2000000000000057288 ) ;
#83371 = CARTESIAN_POINT ( 'NONE',  ( -21.70464131381649509, 7.095358018979010417, -134.0000000000000000 ) ) ;
#83372 = DIRECTION ( 'NONE',  ( 0.000000000000000000, -0.4999999999999673039, -0.8660254037844573594 ) ) ;
#83374 = ORIENTED_EDGE ( 'NONE', *, *, #238012, .F. ) ;
#83373 = LINE ( 'NONE', #164242, #123560 ) ;
#83376 = DIRECTION ( 'NONE',  ( 0.000000000000000000, -0.1298341882519953583, -0.9915357197604861561 ) ) ;
#83375 = DIRECTION ( 'NONE',  ( -1.000000000000000000, -0.000000000000000000, -0.000000000000000000 ) ) ;
#83377 = ORIENTED_EDGE ( 'NONE', *, *, #19429, .F. ) ;
#83379 = ORIENTED_EDGE ( 'NONE', *, *, #198032, .T. ) ;
#83378 = CARTESIAN_POINT ( 'NONE',  ( 21.05000000000000071, 8.776282895303632259, -112.6500000000000341 ) ) ;
#83380 = ORIENTED_EDGE ( 'NONE', *, *, #147771, .F. ) ;
#83381 = CARTESIAN_POINT ( 'NONE',  ( 20.04142135623730070, 11.75000000001115907, -91.65000000000004832 ) ) ;
#83382 = CARTESIAN_POINT ( 'NONE',  ( -21.07928932188134041, 30.84304088367084162, -252.0482413927653340 ) ) ;
#83383 = DIRECTION ( 'NONE',  ( -1.000000000000000000, 0.000000000000000000, 0.000000000000000000 ) ) ;
#83384 = EDGE_LOOP ( 'NONE', ( #79815, #57929, #146947, #20563 ) ) ;
#83385 = DIRECTION ( 'NONE',  ( 0.000000000000000000, 0.000000000000000000, 1.000000000000000000 ) ) ;
#83386 = DIRECTION ( 'NONE',  ( 1.000000000000000000, 0.000000000000000000, 0.000000000000000000 ) ) ;
#83387 = DIRECTION ( 'NONE',  ( 2.342056488767301376E-15, -0.1350103645451904977, -0.9908441862701596881 ) ) ;
#83388 = EDGE_LOOP ( 'NONE', ( #135275, #15419, #153833 ) ) ;
#83389 = TOROIDAL_SURFACE ( 'NONE', #8414, 7.800000000000000711, 0.1000000000000000056 ) ;
#83390 = FACE_OUTER_BOUND ( 'NONE', #104647, .T. ) ;
#83391 = AXIS2_PLACEMENT_3D ( 'NONE', #24516, #45339, #205685 ) ;
#83392 = CARTESIAN_POINT ( 'NONE',  ( 21.14999999999999858, 69.45934304831089889, -136.5231074845243313 ) ) ;
#83393 = ORIENTED_EDGE ( 'NONE', *, *, #172982, .F. ) ;
#83394 = ORIENTED_EDGE ( 'NONE', *, *, #223654, .F. ) ;
#83395 = CARTESIAN_POINT ( 'NONE',  ( -23.25000000000000000, -1.835859311432481045, -78.60443916879853532 ) ) ;
#83396 = VECTOR ( 'NONE', #126274, 1000.000000000000114 ) ;
#83397 = EDGE_CURVE ( 'NONE', #111333, #204479, #162405, .T. ) ;
#83398 = ORIENTED_EDGE ( 'NONE', *, *, #189785, .F. ) ;
#83399 = DIRECTION ( 'NONE',  ( -1.000000000000000000, 2.952720810173289112E-16, 2.061873921506763405E-30 ) ) ;
#83400 = ORIENTED_EDGE ( 'NONE', *, *, #111425, .F. ) ;
#83401 = DIRECTION ( 'NONE',  ( 0.000000000000000000, -0.4999999999999088507, -0.8660254037844913322 ) ) ;
#83402 = DIRECTION ( 'NONE',  ( -0.000000000000000000, 6.982962677686266711E-15, -1.000000000000000000 ) ) ;
#83403 = DIRECTION ( 'NONE',  ( 0.000000000000000000, 0.8660254037844411501, 0.4999999999999956701 ) ) ;
#83404 = ADVANCED_FACE ( 'NONE', ( #52632 ), #133466, .F. ) ;
#83405 = DIRECTION ( 'NONE',  ( -0.000000000000000000, -1.000000000000000000, -6.982962677686266711E-15 ) ) ;
#83406 = PLANE ( 'NONE',  #120497 ) ;
#83407 = VERTEX_POINT ( 'NONE', #212996 ) ;
#83408 = AXIS2_PLACEMENT_3D ( 'NONE', #72165, #173871, #111283 ) ;
#83409 = AXIS2_PLACEMENT_3D ( 'NONE', #202524, #256328, #76467 ) ;
#83410 = ADVANCED_FACE ( 'NONE', ( #91772 ), #171357, .T. ) ;
#83411 = ADVANCED_FACE ( 'NONE', ( #253405 ), #143075, .T. ) ;
#83412 = CARTESIAN_POINT ( 'NONE',  ( -22.40000000000000213, 1.115486932051692071E-11, -88.74956710754142364 ) ) ;
#83413 = DIRECTION ( 'NONE',  ( 0.000000000000000000, -7.487053152578134969E-15, 1.000000000000000000 ) ) ;
#83414 = EDGE_LOOP ( 'NONE', ( #189884, #231122, #111556, #70301 ) ) ;
#83417 = DIRECTION ( 'NONE',  ( 0.000000000000000000, 2.891205793294679805E-16, -1.000000000000000000 ) ) ;
#83416 = CARTESIAN_POINT ( 'NONE',  ( -23.25000000000000000, 85.60000000001197407, -112.9170766071766820 ) ) ;
#83415 = CIRCLE ( 'NONE', #241838, 0.1000000000000033223 ) ;
#83418 = ORIENTED_EDGE ( 'NONE', *, *, #54712, .F. ) ;
#83421 = EDGE_LOOP ( 'NONE', ( #145863, #201023, #184788, #244538, #57010 ) ) ;
#83420 = DIRECTION ( 'NONE',  ( 1.186688945009010077E-16, 1.000000000000000000, 6.982962677686266711E-15 ) ) ;
#83419 = FILL_AREA_STYLE ('',( #44338 ) ) ;
#83422 = CIRCLE ( 'NONE', #137586, 0.5000000000000004441 ) ;
#83423 = VERTEX_POINT ( 'NONE', #199878 ) ;
#83424 = LINE ( 'NONE', #3922, #168419 ) ;
#83425 = CARTESIAN_POINT ( 'NONE',  ( -23.15000000000000213, 11.65000000001115588, -54.85000000000000142 ) ) ;
#83426 = DIRECTION ( 'NONE',  ( 0.000000000000000000, 0.4088369013363281068, -0.9126074666063770380 ) ) ;
#83427 = EDGE_LOOP ( 'NONE', ( #206200, #170352, #162774, #219964 ) ) ;
#83428 = CARTESIAN_POINT ( 'NONE',  ( 21.05000000000000071, -11.48912529306489994, -97.50000000000004263 ) ) ;
#83429 = ADVANCED_FACE ( 'NONE', ( #235137 ), #196022, .F. ) ;
#83430 = CARTESIAN_POINT ( 'NONE',  ( 21.05000000000000071, 1.115600667400684642E-11, -167.5000000000000284 ) ) ;
#83431 = ADVANCED_FACE ( 'NONE', ( #79877 ), #219401, .F. ) ;
#83433 = CARTESIAN_POINT ( 'NONE',  ( -23.25000000000000000, 77.73670573947940454, -91.50568489690056140 ) ) ;
#83432 = DIRECTION ( 'NONE',  ( 2.342056488767301376E-15, -0.1350103645451904977, -0.9908441862701596881 ) ) ;
#83435 = ORIENTED_EDGE ( 'NONE', *, *, #86688, .F. ) ;
#83434 = CARTESIAN_POINT ( 'NONE',  ( 20.94999999999999929, 1.115600667400684642E-11, -146.8750000000000000 ) ) ;
#83436 = TOROIDAL_SURFACE ( 'NONE', #95916, 0.2000000000000000111, 0.1000000000000000056 ) ;
#83437 = CIRCLE ( 'NONE', #25222, 0.5000000000000004441 ) ;
#83438 = VERTEX_POINT ( 'NONE', #120360 ) ;
#83439 = CYLINDRICAL_SURFACE ( 'NONE', #82647, 11.80000000000000426 ) ;
#83440 = CARTESIAN_POINT ( 'NONE',  ( -18.40000000000000213, 11.48667500176882328, -176.7499999999999716 ) ) ;
#83441 = CARTESIAN_POINT ( 'NONE',  ( -20.54999999999999716, 85.40000000001178648, -79.41707660717668205 ) ) ;
#83442 = ORIENTED_EDGE ( 'NONE', *, *, #106544, .T. ) ;
#83443 = DIRECTION ( 'NONE',  ( 0.000000000000000000, 1.000000000000000000, 0.000000000000000000 ) ) ;
#83444 = ORIENTED_EDGE ( 'NONE', *, *, #218085, .T. ) ;
#83445 = EDGE_CURVE ( 'NONE', #108089, #118009, #16664, .T. ) ;
#83446 = PLANE ( 'NONE',  #251528 ) ;
#83448 = EDGE_CURVE ( 'NONE', #75238, #71995, #229040, .T. ) ;
#83447 = CARTESIAN_POINT ( 'NONE',  ( 21.05000000000000071, 87.48912529308779540, -72.42310748452423752 ) ) ;
#83449 = DIRECTION ( 'NONE',  ( -0.000000000000000000, 1.000000000000000000, 6.982962677686266711E-15 ) ) ;
#83450 = EDGE_CURVE ( 'NONE', #82771, #251013, #140946, .T. ) ;
#83451 = ORIENTED_EDGE ( 'NONE', *, *, #166967, .T. ) ;
#83452 = DIRECTION ( 'NONE',  ( -1.000000000000000000, -0.000000000000000000, -0.000000000000000000 ) ) ;
#83453 = CIRCLE ( 'NONE', #58519, 0.1000000000000002554 ) ;
#83454 = CIRCLE ( 'NONE', #8481, 12.87499999999999822 ) ;
#83455 = ADVANCED_FACE ( 'NONE', ( #1638 ), #176465, .F. ) ;
#83456 = CIRCLE ( 'NONE', #146019, 0.1000000000000028644 ) ;
#83457 = CARTESIAN_POINT ( 'NONE',  ( 18.69999999999999929, -1.410778198689825569, -7.973296578895943121 ) ) ;
#83458 = ORIENTED_EDGE ( 'NONE', *, *, #187038, .F. ) ;
#83459 = TOROIDAL_SURFACE ( 'NONE', #137630, 0.2000000000000000111, 0.1000000000000000056 ) ;
#83460 = ORIENTED_EDGE ( 'NONE', *, *, #55181, .T. ) ;
#83461 = ORIENTED_EDGE ( 'NONE', *, *, #79386, .F. ) ;
#83462 = CARTESIAN_POINT ( 'NONE',  ( -23.15000000000000213, 78.47509609352879068, -238.9045489380306435 ) ) ;
#83463 = ORIENTED_EDGE ( 'NONE', *, *, #224783, .T. ) ;
#83465 = ORIENTED_EDGE ( 'NONE', *, *, #136536, .F. ) ;
#83464 = CARTESIAN_POINT ( 'NONE',  ( -23.15000000000000213, 71.65000000001228386, -157.7731074845243882 ) ) ;
#83466 = ORIENTED_EDGE ( 'NONE', *, *, #95193, .T. ) ;
#83467 = CIRCLE ( 'NONE', #141748, 11.65000000000000036 ) ;
#83471 = EDGE_CURVE ( 'NONE', #159456, #130340, #20772, .T. ) ;
#83470 = EDGE_LOOP ( 'NONE', ( #153588, #72924, #156300, #163076 ) ) ;
#83469 = ORIENTED_EDGE ( 'NONE', *, *, #74921, .T. ) ;
#83468 = CARTESIAN_POINT ( 'NONE',  ( 18.54116936837188234, 78.20986773458183450, -231.5294484859616375 ) ) ;
#83472 = VERTEX_POINT ( 'NONE', #160765 ) ;
#83473 = CARTESIAN_POINT ( 'NONE',  ( -20.94999999999999929, 36.65892442174935439, -249.5511627012433848 ) ) ;
#83474 = CARTESIAN_POINT ( 'NONE',  ( -18.50000000000000000, 9.350000000011156942, -179.8499999999999943 ) ) ;
#83475 = DIRECTION ( 'NONE',  ( 1.000000000000000000, 0.000000000000000000, 0.000000000000000000 ) ) ;
#83476 = ORIENTED_EDGE ( 'NONE', *, *, #18720, .F. ) ;
#83477 = EDGE_CURVE ( 'NONE', #183242, #210699, #116597, .T. ) ;
#83478 = CARTESIAN_POINT ( 'NONE',  ( -20.54999999999999716, 4.350000000011156054, -88.25000000000005684 ) ) ;
#83480 = ORIENTED_EDGE ( 'NONE', *, *, #220656, .F. ) ;
#83479 = DIRECTION ( 'NONE',  ( -1.000000000000000000, 3.151514657663852580E-16, -8.547182517843351137E-17 ) ) ;
#83481 = DIRECTION ( 'NONE',  ( -1.000000000000000000, -2.952720810173289112E-16, 0.000000000000000000 ) ) ;
#83483 = ORIENTED_EDGE ( 'NONE', *, *, #17839, .F. ) ;
#83482 = CARTESIAN_POINT ( 'NONE',  ( -21.05000000000000071, 61.95000000001210338, -131.0094124137634140 ) ) ;
#83484 = AXIS2_PLACEMENT_3D ( 'NONE', #4737, #62180, #20497 ) ;
#83485 = ORIENTED_EDGE ( 'NONE', *, *, #203602, .T. ) ;
#83486 = EDGE_CURVE ( 'NONE', #240778, #189087, #8841, .T. ) ;
#83487 = CIRCLE ( 'NONE', #17101, 0.09999999999999938105 ) ;
#83488 = ORIENTED_EDGE ( 'NONE', *, *, #163470, .T. ) ;
#83489 = ORIENTED_EDGE ( 'NONE', *, *, #171444, .F. ) ;
#83491 = AXIS2_PLACEMENT_3D ( 'NONE', #210451, #207894, #189601 ) ;
#83490 = CARTESIAN_POINT ( 'NONE',  ( -16.89155683852451162, 9.950000000011137047, -180.7773718495396622 ) ) ;
#83492 = FACE_OUTER_BOUND ( 'NONE', #204746, .T. ) ;
#83493 = EDGE_CURVE ( 'NONE', #15384, #177806, #38229, .T. ) ;
#83495 = VERTEX_POINT ( 'NONE', #115187 ) ;
#83494 = ORIENTED_EDGE ( 'NONE', *, *, #55409, .F. ) ;
#83496 = ORIENTED_EDGE ( 'NONE', *, *, #126329, .T. ) ;
#83498 = ADVANCED_FACE ( 'NONE', ( #254655 ), #16111, .T. ) ;
#83497 = PLANE ( 'NONE',  #165879 ) ;
#83499 = ORIENTED_EDGE ( 'NONE', *, *, #176621, .F. ) ;
#83500 = ORIENTED_EDGE ( 'NONE', *, *, #83148, .T. ) ;
#83501 = DIRECTION ( 'NONE',  ( 1.000000000000000000, -2.986185139342070877E-16, 6.665775143889692774E-16 ) ) ;
#83502 = TOROIDAL_SURFACE ( 'NONE', #245846, 0.2000000000000000111, 0.1000000000000000056 ) ;
#83504 = ORIENTED_EDGE ( 'NONE', *, *, #164318, .F. ) ;
#83503 = DIRECTION ( 'NONE',  ( 0.000000000000000000, -0.8814952561688437216, 0.4721928772777334582 ) ) ;
#83505 = DIRECTION ( 'NONE',  ( 0.000000000000000000, 0.8814952561688476074, -0.4721928772777262417 ) ) ;
#83507 = CARTESIAN_POINT ( 'NONE',  ( 18.43579564894463374, -9.519327535281719932, -107.4729766438598944 ) ) ;
#83506 = FACE_OUTER_BOUND ( 'NONE', #195863, .T. ) ;
#83508 = ORIENTED_EDGE ( 'NONE', *, *, #78141, .T. ) ;
#83510 = ORIENTED_EDGE ( 'NONE', *, *, #170213, .T. ) ;
#83509 = EDGE_LOOP ( 'NONE', ( #139433, #146226, #9403, #7720 ) ) ;
#83511 = DIRECTION ( 'NONE',  ( -1.000000000000000000, -0.000000000000000000, -0.000000000000000000 ) ) ;
#83513 = VERTEX_POINT ( 'NONE', #95613 ) ;
#83512 = VECTOR ( 'NONE', #98735, 1000.000000000000000 ) ;
#83515 = EDGE_CURVE ( 'NONE', #77508, #89874, #175211, .T. ) ;
#83514 = AXIS2_PLACEMENT_3D ( 'NONE', #253703, #176767, #214579 ) ;
#83516 = CARTESIAN_POINT ( 'NONE',  ( -18.46856557590793457, 85.47421590779836720, -95.92112124364196291 ) ) ;
#83517 = VERTEX_POINT ( 'NONE', #36969 ) ;
#83518 = VERTEX_POINT ( 'NONE', #117748 ) ;
#83519 = VECTOR ( 'NONE', #120245, 1000.000000000000227 ) ;
#83520 = EDGE_CURVE ( 'NONE', #208327, #237460, #18653, .T. ) ;
#83521 = DIRECTION ( 'NONE',  ( -0.000000000000000000, 0.4088369013363281623, -0.9126074666063771490 ) ) ;
#83522 = VERTEX_POINT ( 'NONE', #119046 ) ;
#83523 = CARTESIAN_POINT ( 'NONE',  ( -21.14999999999999858, 11.65000000001115588, -100.5000000000000284 ) ) ;
#83524 = DIRECTION ( 'NONE',  ( -1.000000000000000000, 0.000000000000000000, 1.073024830501117725E-15 ) ) ;
#83525 = ORIENTED_EDGE ( 'NONE', *, *, #144375, .T. ) ;
#83526 = VECTOR ( 'NONE', #55070, 1000.000000000000000 ) ;
#83527 = CARTESIAN_POINT ( 'NONE',  ( 19.97071067695833690, 64.27928932305385956, -145.3468540517209249 ) ) ;
#83529 = AXIS2_PLACEMENT_3D ( 'NONE', #49085, #206887, #128647 ) ;
#83528 = CARTESIAN_POINT ( 'NONE',  ( -16.77683809663752257, 9.945835743215301505, -79.66394901910425119 ) ) ;
#83531 = CARTESIAN_POINT ( 'NONE',  ( -16.96982749440706328, 9.950000000011137047, -120.8752215911883070 ) ) ;
#83530 = DIRECTION ( 'NONE',  ( 1.000000000000000000, -2.849773892568378313E-16, 7.728835255496647986E-17 ) ) ;
#83532 = CARTESIAN_POINT ( 'NONE',  ( 21.00000000000000000, 66.25000000001151079, -48.27310748452438816 ) ) ;
#83533 = CARTESIAN_POINT ( 'NONE',  ( 20.94999999999999929, 70.50000000001199396, -115.4283735034374274 ) ) ;
#83535 = EDGE_CURVE ( 'NONE', #119824, #69468, #149941, .T. ) ;
#83534 = DIRECTION ( 'NONE',  ( 1.000000000000000000, 0.000000000000000000, -0.000000000000000000 ) ) ;
#83536 = CARTESIAN_POINT ( 'NONE',  ( 20.84999999999998721, 64.25000000001190870, -103.0231074845243882 ) ) ;
#83537 = FACE_OUTER_BOUND ( 'NONE', #219162, .T. ) ;
#83538 = EDGE_CURVE ( 'NONE', #14341, #188719, #104112, .T. ) ;
#83539 = VERTEX_POINT ( 'NONE', #163310 ) ;
#83540 = AXIS2_PLACEMENT_3D ( 'NONE', #244954, #27233, #66329 ) ;
#83541 = AXIS2_PLACEMENT_3D ( 'NONE', #253308, #109947, #113807 ) ;
#83542 = AXIS2_PLACEMENT_3D ( 'NONE', #63417, #81669, #120872 ) ;
#83543 = AXIS2_PLACEMENT_3D ( 'NONE', #156447, #171195, #151614 ) ;
#83544 = AXIS2_PLACEMENT_3D ( 'NONE', #131408, #251352, #88411 ) ;
#83546 = EDGE_LOOP ( 'NONE', ( #229868, #17284, #221729, #50902, #33565 ) ) ;
#83545 = EDGE_LOOP ( 'NONE', ( #19291, #184296, #100513, #224708 ) ) ;
#83547 = ORIENTED_EDGE ( 'NONE', *, *, #53225, .T. ) ;
#83548 = CARTESIAN_POINT ( 'NONE',  ( -20.64999999999999858, 1.940186915899004161, -154.6708807889467039 ) ) ;
#83549 = DIRECTION ( 'NONE',  ( 0.000000000000000000, 6.982962677686266711E-15, -1.000000000000000000 ) ) ;
#83550 = EDGE_CURVE ( 'NONE', #180612, #22197, #98129, .T. ) ;
#83552 = CARTESIAN_POINT ( 'NONE',  ( -12.60206096961792532, 9.389686005655656587, -15.67284350635130430 ) ) ;
#83551 = CARTESIAN_POINT ( 'NONE',  ( -18.59999999999999787, -1.164121893230052995, -141.9148480855716343 ) ) ;
#83553 = EDGE_CURVE ( 'NONE', #1348, #153879, #242827, .T. ) ;
#83554 = CARTESIAN_POINT ( 'NONE',  ( 21.04999999999999716, 67.12872031401667527, -161.4644784893834810 ) ) ;
#83555 = VERTEX_POINT ( 'NONE', #143728 ) ;
#83556 = VECTOR ( 'NONE', #206041, 1000.000000000000000 ) ;
#83557 = DIRECTION ( 'NONE',  ( -1.000000000000000000, 2.952720810173289112E-16, 2.061873921506763405E-30 ) ) ;
#83558 = CARTESIAN_POINT ( 'NONE',  ( -23.25000000000000000, 87.75000000001193712, -103.0231074845242318 ) ) ;
#83559 = FACE_OUTER_BOUND ( 'NONE', #114398, .T. ) ;
#83560 = ORIENTED_EDGE ( 'NONE', *, *, #203819, .T. ) ;
#83561 = DIRECTION ( 'NONE',  ( 0.000000000000000000, -0.4999999999999088507, 0.8660254037844913322 ) ) ;
#83562 = CARTESIAN_POINT ( 'NONE',  ( -21.05000000000000071, -0.09999999998884476216, -93.95934304829879125 ) ) ;
#83563 = ORIENTED_EDGE ( 'NONE', *, *, #162333, .T. ) ;
#83564 = CARTESIAN_POINT ( 'NONE',  ( -17.71734398241074970, 65.15764277154805484, -193.2482457375300271 ) ) ;
#83565 = CARTESIAN_POINT ( 'NONE',  ( 23.14999999999999858, 5.900000000011162093, -190.7809002353436085 ) ) ;
#83566 = DIRECTION ( 'NONE',  ( 0.000000000000000000, 0.000000000000000000, 1.000000000000000000 ) ) ;
#83567 = DIRECTION ( 'NONE',  ( 0.000000000000000000, 0.000000000000000000, -1.000000000000000000 ) ) ;
#83568 = DIRECTION ( 'NONE',  ( -1.000000000000000000, 0.000000000000000000, 0.000000000000000000 ) ) ;
#83569 = CARTESIAN_POINT ( 'NONE',  ( -0.8999999999999980238, -11.65000000000000036, 28.60000000000000142 ) ) ;
#83570 = ORIENTED_EDGE ( 'NONE', *, *, #52353, .F. ) ;
#83571 = DIRECTION ( 'NONE',  ( -0.000000000000000000, -0.000000000000000000, -1.000000000000000000 ) ) ;
#83572 = CARTESIAN_POINT ( 'NONE',  ( -18.79999999999999716, 6.726092018229619995, 9.512212474619552438 ) ) ;
#83573 = AXIS2_PLACEMENT_3D ( 'NONE', #202152, #24827, #28694 ) ;
#83574 = DIRECTION ( 'NONE',  ( 0.000000000000000000, 0.000000000000000000, 1.000000000000000000 ) ) ;
#83576 = CARTESIAN_POINT ( 'NONE',  ( 22.39999999999999503, 10.71943444926881384, -226.8179467668883831 ) ) ;
#83575 = CARTESIAN_POINT ( 'NONE',  ( -17.11825945287481332, 9.950000000011138823, -121.2500000000000426 ) ) ;
#83577 = CARTESIAN_POINT ( 'NONE',  ( -18.39999999999999858, 85.68240343348880117, -163.3662641071115047 ) ) ;
#83578 = DIRECTION ( 'NONE',  ( 0.000000000000000000, 0.8814952561688437216, -0.4721928772777334582 ) ) ;
#83579 = CARTESIAN_POINT ( 'NONE',  ( 23.14999999999999858, 1.115600667400684642E-11, -200.9999999999999432 ) ) ;
#83582 = VERTEX_POINT ( 'NONE', #65475 ) ;
#83581 = CIRCLE ( 'NONE', #229373, 11.64999999999999325 ) ;
#83580 = CARTESIAN_POINT ( 'NONE',  ( -17.22767730082391680, 10.34924421247984583, -145.3575713094252819 ) ) ;
#83583 = EDGE_CURVE ( 'NONE', #6496, #152492, #206282, .T. ) ;
#83584 = CIRCLE ( 'NONE', #141864, 0.1000000000000047656 ) ;
#83585 = DIRECTION ( 'NONE',  ( -0.000000000000000000, 1.000000000000000000, -0.000000000000000000 ) ) ;
#83586 = AXIS2_PLACEMENT_3D ( 'NONE', #14619, #32921, #92836 ) ;
#83587 = CARTESIAN_POINT ( 'NONE',  ( -18.55121869061588669, 65.67252876774480796, -30.44570419949945617 ) ) ;
#83588 = ADVANCED_FACE ( 'NONE', ( #145002 ), #142445, .T. ) ;
#83589 = DIRECTION ( 'NONE',  ( 1.000000000000000000, 0.000000000000000000, 0.000000000000000000 ) ) ;
#83590 = VECTOR ( 'NONE', #127863, 1000.000000000000000 ) ;
#83591 = ORIENTED_EDGE ( 'NONE', *, *, #162978, .T. ) ;
#83592 = AXIS2_PLACEMENT_3D ( 'NONE', #51808, #250034, #209625 ) ;
#83593 = CARTESIAN_POINT ( 'NONE',  ( -16.97683809663752186, 66.15000000001153069, -49.42547150272071121 ) ) ;
#83594 = CARTESIAN_POINT ( 'NONE',  ( 21.13461538461538325, 65.38541703798603066, -57.17310748452439384 ) ) ;
#83596 = CARTESIAN_POINT ( 'NONE',  ( -18.59999999999999787, 65.66751761918668251, -97.42826094061121012 ) ) ;
#83595 = TOROIDAL_SURFACE ( 'NONE', #220985, 0.4000000000000015210, 0.1000000000000000056 ) ;
#83597 = ORIENTED_EDGE ( 'NONE', *, *, #131549, .T. ) ;
#83598 = DIRECTION ( 'NONE',  ( 0.000000000000000000, 0.000000000000000000, 1.000000000000000000 ) ) ;
#83600 = ORIENTED_EDGE ( 'NONE', *, *, #50600, .T. ) ;
#83599 = LINE ( 'NONE', #184015, #30133 ) ;
#83602 = CARTESIAN_POINT ( 'NONE',  ( -20.64999999999999858, 2.000000000011154189, -154.2753780772379173 ) ) ;
#83601 = CARTESIAN_POINT ( 'NONE',  ( 18.54999999999999716, 42.27269979661959098, -221.1123729563994402 ) ) ;
#83603 =( BOUNDED_CURVE ( )  B_SPLINE_CURVE ( 3, ( #193450, #14826, #173918, #253402 ),
 .UNSPECIFIED., .F., .F. ) 
 B_SPLINE_CURVE_WITH_KNOTS ( ( 4, 4 ),
 ( 4.712388980384690562, 6.283185307179586232 ),
 .UNSPECIFIED. ) 
 CURVE ( )  GEOMETRIC_REPRESENTATION_ITEM ( )  RATIONAL_B_SPLINE_CURVE ( ( 1.000000000000000000, 0.8047378541243652705, 0.8047378541243652705, 1.000000000000000000 ) ) 
 REPRESENTATION_ITEM ( '' )  );
#83604 = DIRECTION ( 'NONE',  ( 0.000000000000000000, 0.000000000000000000, -1.000000000000000000 ) ) ;
#83605 = ORIENTED_EDGE ( 'NONE', *, *, #31700, .F. ) ;
#83606 =( NAMED_UNIT ( * ) SI_UNIT ( $, .STERADIAN. ) SOLID_ANGLE_UNIT ( ) );
#83607 = DIRECTION ( 'NONE',  ( 1.000000000000000000, 0.000000000000000000, 0.000000000000000000 ) ) ;
#83608 = DIRECTION ( 'NONE',  ( 1.652117596168391306E-15, 0.4721928772777346239, 0.8814952561688430555 ) ) ;
#83609 = AXIS2_PLACEMENT_3D ( 'NONE', #88575, #148576, #38904 ) ;
#83610 = VERTEX_POINT ( 'NONE', #224547 ) ;
#83611 = CARTESIAN_POINT ( 'NONE',  ( 20.99999999999998934, -1.311673547813416718, -7.986648289447971116 ) ) ;
#83612 = FACE_OUTER_BOUND ( 'NONE', #219464, .T. ) ;
#83613 = CARTESIAN_POINT ( 'NONE',  ( -21.05000000000000071, 5.850000000011108092, -110.6324972242780120 ) ) ;
#83614 = CARTESIAN_POINT ( 'NONE',  ( -22.42253884134832020, 0.001932351146464877023, -122.3503943026515799 ) ) ;
#83615 = ORIENTED_EDGE ( 'NONE', *, *, #215391, .T. ) ;
#83616 = ORIENTED_EDGE ( 'NONE', *, *, #26787, .T. ) ;
#83617 = DIRECTION ( 'NONE',  ( -0.000000000000000000, -0.4791956752371546724, -0.8777080977375153470 ) ) ;
#83618 = DIRECTION ( 'NONE',  ( -0.000000000000000000, -0.000000000000000000, 1.000000000000000000 ) ) ;
#83619 = DIRECTION ( 'NONE',  ( 0.000000000000000000, 0.9908441862701605762, -0.1350103645451835310 ) ) ;
#83620 = AXIS2_PLACEMENT_3D ( 'NONE', #192456, #195041, #175477 ) ;
#83621 = DIRECTION ( 'NONE',  ( -1.000000000000000000, -0.000000000000000000, -0.000000000000000000 ) ) ;
#83623 = CARTESIAN_POINT ( 'NONE',  ( -20.94999999999999929, 77.16412189325330928, -128.6082593989527254 ) ) ;
#83622 = CIRCLE ( 'NONE', #8653, 0.5999999999999894307 ) ;
#83624 = AXIS2_PLACEMENT_3D ( 'NONE', #5731, #244357, #68310 ) ;
#83625 = EDGE_CURVE ( 'NONE', #119515, #24606, #104577, .T. ) ;
#83628 = CYLINDRICAL_SURFACE ( 'NONE', #132748, 0.09999999999999939493 ) ;
#83627 = CIRCLE ( 'NONE', #225292, 0.1000000000000001582 ) ;
#83626 = CARTESIAN_POINT ( 'NONE',  ( -16.80468759584936933, 12.41488287255450373, -211.2836609135854928 ) ) ;
#83629 = CARTESIAN_POINT ( 'NONE',  ( -18.50000000000000000, 66.75000000001179501, -81.67310748452437963 ) ) ;
#83630 = DIRECTION ( 'NONE',  ( -1.000000000000000000, 7.304098846218135653E-16, 4.639676173203994055E-30 ) ) ;
#83631 = CARTESIAN_POINT ( 'NONE',  ( -18.47079683080319867, 47.01888943380454577, -255.2887095692685193 ) ) ;
#83632 = CARTESIAN_POINT ( 'NONE',  ( 21.05000000000005400, 67.82483145523551116, -25.59432346794077162 ) ) ;
#83634 = VERTEX_POINT ( 'NONE', #26364 ) ;
#83633 = DIRECTION ( 'NONE',  ( 0.000000000000000000, 0.5000000000000004441, 0.8660254037844384856 ) ) ;
#83635 = CIRCLE ( 'NONE', #237800, 4.299999999999970512 ) ;
#83636 = CARTESIAN_POINT ( 'NONE',  ( -21.29999999999995808, 76.00000000001237765, -170.0231074845243597 ) ) ;
#83637 = LINE ( 'NONE', #203626, #132582 ) ;
#83639 = DIRECTION ( 'NONE',  ( -0.000000000000000000, -6.982962677686266711E-15, 1.000000000000000000 ) ) ;
#83638 = CARTESIAN_POINT ( 'NONE',  ( 21.07094088545368038, 75.90110629745977633, -109.3432747064414343 ) ) ;
#83640 = EDGE_CURVE ( 'NONE', #230716, #139488, #62453, .T. ) ;
#83641 = ORIENTED_EDGE ( 'NONE', *, *, #199590, .T. ) ;
#83643 = LINE ( 'NONE', #163235, #159253 ) ;
#83642 = CARTESIAN_POINT ( 'NONE',  ( -18.59999999999999787, 70.10000000001213039, -126.3040077198679398 ) ) ;
#83644 = LINE ( 'NONE', #242744, #170724 ) ;
#83645 = CARTESIAN_POINT ( 'NONE',  ( -18.59999999999999787, 6.982009704867601307, -171.1961521182563217 ) ) ;
#83646 = CYLINDRICAL_SURFACE ( 'NONE', #236721, 4.049999999999998046 ) ;
#83647 = DIRECTION ( 'NONE',  ( -1.000000000000000000, -0.000000000000000000, -0.000000000000000000 ) ) ;
#83648 = EDGE_CURVE ( 'NONE', #50249, #69777, #37509, .T. ) ;
#83649 = ORIENTED_EDGE ( 'NONE', *, *, #186029, .T. ) ;
#83651 = VERTEX_POINT ( 'NONE', #42093 ) ;
#83650 = TOROIDAL_SURFACE ( 'NONE', #112907, 0.2000000000000000111, 0.1000000000000000056 ) ;
#83652 = CYLINDRICAL_SURFACE ( 'NONE', #67831, 0.09999999999999939493 ) ;
#83653 = EDGE_CURVE ( 'NONE', #208166, #56768, #137424, .T. ) ;
#83654 = ORIENTED_EDGE ( 'NONE', *, *, #120412, .T. ) ;
#83655 = VERTEX_POINT ( 'NONE', #82445 ) ;
#83656 = CARTESIAN_POINT ( 'NONE',  ( -20.94999999999999929, 1.115600667400684642E-11, -200.9999999999999432 ) ) ;
#83657 = FACE_OUTER_BOUND ( 'NONE', #182890, .T. ) ;
#83658 = DIRECTION ( 'NONE',  ( 1.000000000000000000, -0.000000000000000000, -0.000000000000000000 ) ) ;
#83659 = VERTEX_POINT ( 'NONE', #105865 ) ;
#83660 = EDGE_CURVE ( 'NONE', #26765, #204919, #237415, .T. ) ;
#83661 = CIRCLE ( 'NONE', #212717, 0.1000000000000124678 ) ;
#83662 = CARTESIAN_POINT ( 'NONE',  ( -21.14999999999999858, 64.35000000001268461, -203.5231074845244166 ) ) ;
#83663 = CARTESIAN_POINT ( 'NONE',  ( 21.05000000000000071, 6.412126976762841046, -199.7058512474018244 ) ) ;
#83664 = CARTESIAN_POINT ( 'NONE',  ( -23.15000000000000213, 76.00000000001165290, -69.52310748452431710 ) ) ;
#83665 = CIRCLE ( 'NONE', #254376, 4.000000000000003553 ) ;
#83666 = DIRECTION ( 'NONE',  ( 0.000000000000000000, 0.000000000000000000, -1.000000000000000000 ) ) ;
#83667 = FACE_OUTER_BOUND ( 'NONE', #29359, .T. ) ;
#83668 = LINE ( 'NONE', #4164, #241423 ) ;
#83670 = DIRECTION ( 'NONE',  ( 0.000000000000000000, -6.982962677686266711E-15, 1.000000000000000000 ) ) ;
#83669 = AXIS2_PLACEMENT_3D ( 'NONE', #5480, #22527, #60335 ) ;
#83671 = ORIENTED_EDGE ( 'NONE', *, *, #177242, .F. ) ;
#83673 = CARTESIAN_POINT ( 'NONE',  ( -22.47120815636973745, 75.97109617810887983, -215.1730394732778393 ) ) ;
#83672 = DIRECTION ( 'NONE',  ( -0.000000000000000000, 0.8700118002898356018, -0.4930308989875170078 ) ) ;
#83674 = EDGE_LOOP ( 'NONE', ( #124348, #187281, #76764 ) ) ;
#83676 = ORIENTED_EDGE ( 'NONE', *, *, #74020, .T. ) ;
#83675 = CARTESIAN_POINT ( 'NONE',  ( 20.94999999999999929, 77.83534155023646406, -124.9679561919612922 ) ) ;
#83677 = ORIENTED_EDGE ( 'NONE', *, *, #162200, .F. ) ;
#83678 = DIRECTION ( 'NONE',  ( -1.000000000000000000, -0.000000000000000000, 0.000000000000000000 ) ) ;
#83679 = DIRECTION ( 'NONE',  ( 0.000000000000000000, -0.2128009952263403282, 0.9770955615653358350 ) ) ;
#83680 = CARTESIAN_POINT ( 'NONE',  ( -20.94999999999999929, 46.01637179467461891, -256.6614375746592600 ) ) ;
#83681 = LINE ( 'NONE', #242789, #187571 ) ;
#83682 = AXIS2_PLACEMENT_3D ( 'NONE', #10823, #173804, #168663 ) ;
#83683 = ORIENTED_EDGE ( 'NONE', *, *, #13825, .F. ) ;
#83684 = LINE ( 'NONE', #86267, #68131 ) ;
#83685 = FACE_OUTER_BOUND ( 'NONE', #126919, .T. ) ;
#83686 = VERTEX_POINT ( 'NONE', #223258 ) ;
#83687 = CARTESIAN_POINT ( 'NONE',  ( -20.94999999999999929, 10.29288807858821109, -38.95800201601217339 ) ) ;
#83688 = LINE ( 'NONE', #201115, #151616 ) ;
#83689 = AXIS2_PLACEMENT_3D ( 'NONE', #239271, #4492, #243113 ) ;
#83690 = EDGE_LOOP ( 'NONE', ( #121296, #92404, #201202 ) ) ;
#83691 = CARTESIAN_POINT ( 'NONE',  ( 20.90000000000000213, 11.49641995933507843, -1.885425182446133885 ) ) ;
#83692 = AXIS2_PLACEMENT_3D ( 'NONE', #60632, #119353, #184447 ) ;
#83693 = EDGE_CURVE ( 'NONE', #213545, #132227, #154615, .T. ) ;
#83694 = CIRCLE ( 'NONE', #250156, 7.791421356237310469 ) ;
#83695 = DIRECTION ( 'NONE',  ( 0.000000000000000000, 0.000000000000000000, -1.000000000000000000 ) ) ;
#83696 = EDGE_LOOP ( 'NONE', ( #217326, #145104, #83721, #190521 ) ) ;
#83697 = LINE ( 'NONE', #257191, #150393 ) ;
#83699 =( BOUNDED_SURFACE ( )  B_SPLINE_SURFACE ( 3, 2, ( 
 ( #123572, #201818, #61017 ),
 ( #199266, #20639, #200537 ),
 ( #137978, #101384, #143111 ),
 ( #179708, #1017, #220107 ) ),
 .UNSPECIFIED., .F., .F., .T. ) 
 B_SPLINE_SURFACE_WITH_KNOTS ( ( 4, 4 ),
 ( 3, 3 ),
 ( 0.04058434257139476031, 0.04256401539001600232 ),
 ( 0.000000000000000000, 1.000000000000000000 ),
 .UNSPECIFIED. ) 
 GEOMETRIC_REPRESENTATION_ITEM ( )  RATIONAL_B_SPLINE_SURFACE ( (
 ( 1.000000000000000000, 0.7103081912008184506, 1.000000000000000000),
 ( 1.000000000000000000, 0.7104998333554868317, 1.000000000000000000),
 ( 1.000000000000000000, 0.7107238315755806113, 1.000000000000000000),
 ( 1.000000000000000000, 0.7110073749539497223, 1.000000000000000000) ) ) 
 REPRESENTATION_ITEM ( '' )  SURFACE ( )  );
#83698 = CIRCLE ( 'NONE', #229497, 0.1000000000000028644 ) ;
#83700 = DIRECTION ( 'NONE',  ( 0.000000000000000000, 0.09425075112713275638, 0.9955484899852801162 ) ) ;
#83701 = DIRECTION ( 'NONE',  ( -0.000000000000000000, 0.000000000000000000, 1.000000000000000000 ) ) ;
#83702 = AXIS2_PLACEMENT_3D ( 'NONE', #128753, #111750, #191319 ) ;
#83704 = ADVANCED_FACE ( 'NONE', ( #202425 ), #44643, .F. ) ;
#83703 = AXIS2_PLACEMENT_3D ( 'NONE', #145312, #4517, #187051 ) ;
#83705 = CARTESIAN_POINT ( 'NONE',  ( 18.59999999999999432, -0.6576273345615495369, -242.5323337003318898 ) ) ;
#83706 = EDGE_CURVE ( 'NONE', #222722, #69101, #221954, .T. ) ;
#83707 = CARTESIAN_POINT ( 'NONE',  ( -18.39999999999999858, 64.25000000001210765, -127.2731074845243882 ) ) ;
#83708 = FACE_OUTER_BOUND ( 'NONE', #67068, .T. ) ;
#83709 = AXIS2_PLACEMENT_3D ( 'NONE', #167710, #124709, #42599 ) ;
#83711 = CARTESIAN_POINT ( 'NONE',  ( -18.59999999999999787, 70.22659352830977753, -197.9852579278363578 ) ) ;
#83710 = CIRCLE ( 'NONE', #79459, 0.1000000000000054040 ) ;
#83712 = AXIS2_PLACEMENT_3D ( 'NONE', #26259, #256118, #185320 ) ;
#83713 = VERTEX_POINT ( 'NONE', #186735 ) ;
#83715 = DIRECTION ( 'NONE',  ( 0.000000000000000000, 0.4999999999999608646, 0.8660254037844612451 ) ) ;
#83714 = CARTESIAN_POINT ( 'NONE',  ( -18.59999999999999787, 74.26374286841446803, -91.45445515550682103 ) ) ;
#83716 = VECTOR ( 'NONE', #181950, 1000.000000000000227 ) ;
#83717 = ORIENTED_EDGE ( 'NONE', *, *, #99344, .T. ) ;
#83718 = CARTESIAN_POINT ( 'NONE',  ( -18.39999999999999858, 85.50000000001242029, -163.4229180933022576 ) ) ;
#83719 = DIRECTION ( 'NONE',  ( 0.000000000000000000, 0.000000000000000000, 1.000000000000000000 ) ) ;
#83722 = EDGE_CURVE ( 'NONE', #44033, #158124, #8286, .T. ) ;
#83721 = ORIENTED_EDGE ( 'NONE', *, *, #22693, .T. ) ;
#83720 = DIRECTION ( 'NONE',  ( 0.000000000000000000, 0.000000000000000000, 1.000000000000000000 ) ) ;
#83724 = EDGE_LOOP ( 'NONE', ( #10469, #208501 ) ) ;
#83723 = CARTESIAN_POINT ( 'NONE',  ( 21.04105312098505109, 67.12466737696794894, -57.19460073731235639 ) ) ;
#83725 = CARTESIAN_POINT ( 'NONE',  ( -21.05000000000000071, 70.10000000001163301, -59.30400771986794695 ) ) ;
#83726 = DIRECTION ( 'NONE',  ( -0.000000000000000000, -0.000000000000000000, 1.000000000000000000 ) ) ;
#83727 = DIRECTION ( 'NONE',  ( -0.000000000000000000, 0.9126074666063769270, 0.4088369013363280513 ) ) ;
#83728 = ADVANCED_FACE ( 'NONE', ( #4210 ), #203714, .T. ) ;
#83729 = DIRECTION ( 'NONE',  ( 0.000000000000000000, 0.000000000000000000, -1.000000000000000000 ) ) ;
#83730 = CIRCLE ( 'NONE', #116898, 0.5000000000000004441 ) ;
#83732 = ORIENTED_EDGE ( 'NONE', *, *, #70060, .T. ) ;
#83731 = FACE_OUTER_BOUND ( 'NONE', #180631, .T. ) ;
#83734 = EDGE_CURVE ( 'NONE', #22457, #126736, #145623, .T. ) ;
#83733 = DIRECTION ( 'NONE',  ( 0.000000000000000000, 8.673617379884087537E-15, 1.000000000000000000 ) ) ;
#83735 = ORIENTED_EDGE ( 'NONE', *, *, #169783, .F. ) ;
#83736 = ORIENTED_EDGE ( 'NONE', *, *, #138619, .F. ) ;
#83738 = ADVANCED_FACE ( 'NONE', ( #49770 ), #69352, .F. ) ;
#83737 = CARTESIAN_POINT ( 'NONE',  ( -20.94999999999999929, 11.75000000001115552, -107.5148057706540357 ) ) ;
#83739 = DIRECTION ( 'NONE',  ( 0.5932847527679299127, 0.8049926720990051576, 4.984624513800587583E-15 ) ) ;
#83740 = EDGE_CURVE ( 'NONE', #145909, #32455, #152761, .T. ) ;
#83741 = ORIENTED_EDGE ( 'NONE', *, *, #77297, .T. ) ;
#83742 = LINE ( 'NONE', #191909, #116733 ) ;
#83743 = AXIS2_PLACEMENT_3D ( 'NONE', #59728, #218814, #102702 ) ;
#83744 = FACE_OUTER_BOUND ( 'NONE', #242806, .T. ) ;
#83745 = ORIENTED_EDGE ( 'NONE', *, *, #11076, .T. ) ;
#83746 = CARTESIAN_POINT ( 'NONE',  ( 21.14250536705908345, 6.368877103560281583, -199.6129264737045048 ) ) ;
#83747 = CARTESIAN_POINT ( 'NONE',  ( -21.05000000000000071, -11.64999999998884483, -36.50000000000000711 ) ) ;
#83749 = ORIENTED_EDGE ( 'NONE', *, *, #250783, .T. ) ;
#83748 = CIRCLE ( 'NONE', #46194, 0.1000000000000028644 ) ;
#83750 = ORIENTED_EDGE ( 'NONE', *, *, #256461, .T. ) ;
#83751 = DIRECTION ( 'NONE',  ( -1.000000000000000000, -0.000000000000000000, -0.000000000000000000 ) ) ;
#83752 = EDGE_CURVE ( 'NONE', #255583, #41396, #190590, .T. ) ;
#83753 = ORIENTED_EDGE ( 'NONE', *, *, #169239, .F. ) ;
#83754 = EDGE_CURVE ( 'NONE', #29044, #233526, #81778, .T. ) ;
#83755 = CARTESIAN_POINT ( 'NONE',  ( 18.54286124688533732, -0.8401192457767151511, -242.3674794292616923 ) ) ;
#83756 = ORIENTED_EDGE ( 'NONE', *, *, #102171, .F. ) ;
#83758 = EDGE_LOOP ( 'NONE', ( #237857, #120986, #113601, #79317 ) ) ;
#83757 = DIRECTION ( 'NONE',  ( 0.000000000000000000, -0.8700118002898359348, 0.4930308989875165082 ) ) ;
#83759 = CARTESIAN_POINT ( 'NONE',  ( 23.14999999999999503, 69.35000000001205933, -124.3731074845243540 ) ) ;
#83760 = ORIENTED_EDGE ( 'NONE', *, *, #106822, .T. ) ;
#83761 = CARTESIAN_POINT ( 'NONE',  ( -18.50000000000000000, 1.835341550235567887, -78.55515129256302487 ) ) ;
#83762 = ORIENTED_EDGE ( 'NONE', *, *, #240635, .F. ) ;
#83765 = ADVANCED_FACE ( 'NONE', ( #193151 ), #250535, .T. ) ;
#83764 = ORIENTED_EDGE ( 'NONE', *, *, #106969, .F. ) ;
#83763 = ORIENTED_EDGE ( 'NONE', *, *, #236304, .T. ) ;
#83766 = FACE_OUTER_BOUND ( 'NONE', #58845, .T. ) ;
#83767 = CARTESIAN_POINT ( 'NONE',  ( -21.05315837636350196, 56.18370557670049692, -227.9291052944747094 ) ) ;
#83768 = VECTOR ( 'NONE', #246215, 1000.000000000000114 ) ;
#83769 = ORIENTED_EDGE ( 'NONE', *, *, #145704, .T. ) ;
#83770 = AXIS2_PLACEMENT_3D ( 'NONE', #241982, #42493, #63332 ) ;
#83771 = AXIS2_PLACEMENT_3D ( 'NONE', #217517, #257891, #19338 ) ;
#83772 = ORIENTED_EDGE ( 'NONE', *, *, #37540, .T. ) ;
#83773 = CARTESIAN_POINT ( 'NONE',  ( -22.59999999999999787, 36.65892442174472876, -249.5511627012454596 ) ) ;
#83774 = LINE ( 'NONE', #159521, #22286 ) ;
#83776 = VERTEX_POINT ( 'NONE', #94022 ) ;
#83775 = DIRECTION ( 'NONE',  ( 7.304098846218134667E-16, 1.000000000000000000, 6.982962677686267499E-15 ) ) ;
#83777 = DIRECTION ( 'NONE',  ( 0.000000000000000000, -1.000000000000000000, 0.000000000000000000 ) ) ;
#83778 = ORIENTED_EDGE ( 'NONE', *, *, #128599, .T. ) ;
#83779 = DIRECTION ( 'NONE',  ( 1.000000000000000000, 0.000000000000000000, 0.000000000000000000 ) ) ;
#83780 = CARTESIAN_POINT ( 'NONE',  ( 20.94999999999999929, 85.40000000001198543, -112.9170766071766820 ) ) ;
#83782 = ORIENTED_EDGE ( 'NONE', *, *, #218707, .F. ) ;
#83781 = EDGE_CURVE ( 'NONE', #183680, #74897, #83437, .T. ) ;
#83783 = DIRECTION ( 'NONE',  ( -1.186688945009010077E-16, -0.4088369013363280513, 0.9126074666063769270 ) ) ;
#83784 = CARTESIAN_POINT ( 'NONE',  ( 18.59999999999999432, 74.83729825007408465, -128.5231074845243029 ) ) ;
#83785 = AXIS2_PLACEMENT_3D ( 'NONE', #36997, #201175, #236446 ) ;
#83786 = ADVANCED_FACE ( 'NONE', ( #228428 ), #250069, .T. ) ;
#83787 = ORIENTED_EDGE ( 'NONE', *, *, #89388, .T. ) ;
#83788 = DIRECTION ( 'NONE',  ( 1.000000000000000000, 0.000000000000000000, 0.000000000000000000 ) ) ;
#83789 = EDGE_LOOP ( 'NONE', ( #28967, #128896, #9430, #231242, #107968, #35764 ) ) ;
#83790 = EDGE_CURVE ( 'NONE', #147579, #53002, #253096, .T. ) ;
#83792 = ORIENTED_EDGE ( 'NONE', *, *, #93633, .T. ) ;
#83791 = ORIENTED_EDGE ( 'NONE', *, *, #42790, .T. ) ;
#83793 = ORIENTED_EDGE ( 'NONE', *, *, #255873, .F. ) ;
#83795 = EDGE_CURVE ( 'NONE', #222562, #238367, #87544, .T. ) ;
#83794 = CARTESIAN_POINT ( 'NONE',  ( -18.34804628011471195, 11.47316190337353525, -42.75000000000000000 ) ) ;
#83796 = VERTEX_POINT ( 'NONE', #88875 ) ;
#83797 = CARTESIAN_POINT ( 'NONE',  ( 22.50000000000000000, 68.20922040163857503, -103.1231074845243540 ) ) ;
#83798 = ORIENTED_EDGE ( 'NONE', *, *, #49109, .F. ) ;
#83799 = CARTESIAN_POINT ( 'NONE',  ( 18.59999999999999787, -8.350000000000004974, 32.89999999999999858 ) ) ;
#83800 = ADVANCED_FACE ( 'NONE', ( #10653 ), #249270, .T. ) ;
#83801 = DIRECTION ( 'NONE',  ( 0.000000000000000000, 0.4088369013362687654, -0.9126074666064034613 ) ) ;
#83802 = EDGE_LOOP ( 'NONE', ( #122029, #134681, #152918, #24627 ) ) ;
#83803 = CIRCLE ( 'NONE', #79732, 11.75000000000000000 ) ;
#83804 = CIRCLE ( 'NONE', #58884, 0.1000000000000064587 ) ;
#83805 = ORIENTED_EDGE ( 'NONE', *, *, #225628, .F. ) ;
#83806 = AXIS2_PLACEMENT_3D ( 'NONE', #169010, #112845, #33349 ) ;
#83807 = ORIENTED_EDGE ( 'NONE', *, *, #134142, .F. ) ;
#83808 = EDGE_CURVE ( 'NONE', #140862, #191837, #194446, .T. ) ;
#83809 = EDGE_CURVE ( 'NONE', #3592, #36158, #12764, .T. ) ;
#83810 = CARTESIAN_POINT ( 'NONE',  ( -16.92570016628983609, 66.04121104227196781, -82.14375815456340035 ) ) ;
#83811 = EDGE_LOOP ( 'NONE', ( #50708, #79585, #85714, #104605, #85388 ) ) ;
#83812 = EDGE_CURVE ( 'NONE', #4584, #150591, #29340, .T. ) ;
#83813 = DIRECTION ( 'NONE',  ( -1.000000000000000000, 0.000000000000000000, -0.000000000000000000 ) ) ;
#83814 = CARTESIAN_POINT ( 'NONE',  ( -5.900000000000002132, -11.65000000000000036, 13.90000000000000213 ) ) ;
#83815 = CARTESIAN_POINT ( 'NONE',  ( 20.85000000000000142, 64.35000000001190301, -103.0231074845243882 ) ) ;
#83816 = CARTESIAN_POINT ( 'NONE',  ( -21.05000000000000071, 11.75000000001115197, -127.1583993101029790 ) ) ;
#83817 = DIRECTION ( 'NONE',  ( 0.000000000000000000, 0.000000000000000000, -1.000000000000000000 ) ) ;
#83818 = VECTOR ( 'NONE', #230571, 1000.000000000000000 ) ;
#83819 = CARTESIAN_POINT ( 'NONE',  ( -23.15000000000000213, 74.00000000001254818, -182.7477294072864709 ) ) ;
#83820 = CARTESIAN_POINT ( 'NONE',  ( -23.25000000000000000, 64.35000000001203091, -114.7731074845243882 ) ) ;
#83822 = CARTESIAN_POINT ( 'NONE',  ( 21.05000000000000071, 34.10066453776878603, -243.7889862147425788 ) ) ;
#83821 = FACE_OUTER_BOUND ( 'NONE', #87902, .T. ) ;
#83823 = DIRECTION ( 'NONE',  ( -0.000000000000000000, -0.000000000000000000, 1.000000000000000000 ) ) ;
#83824 = CARTESIAN_POINT ( 'NONE',  ( -18.40000000000000213, 13.76412598303084778, -210.9488531877278206 ) ) ;
#83825 = DIRECTION ( 'NONE',  ( 0.000000000000000000, -0.9667078373770112698, -0.2558827019434132821 ) ) ;
#83826 = EDGE_CURVE ( 'NONE', #55121, #153815, #256910, .T. ) ;
#83827 = B_SPLINE_CURVE_WITH_KNOTS ( 'NONE', 3,
 ( #47337, #185584, #145156, #142584, #8247, #244256, #4365, #87753, #27832, #128187 ),
 .UNSPECIFIED., .F., .F.,
 ( 4, 3, 3, 4 ),
 ( -2.000561356210515597E-06, 0.000000000000000000, 1.787822682428821068E-05, 4.206475347089863842E-05 ),
 .UNSPECIFIED. ) ;
#83828 = VERTEX_POINT ( 'NONE', #36665 ) ;
#83829 = EDGE_CURVE ( 'NONE', #212715, #17807, #149972, .T. ) ;
#83831 = VERTEX_POINT ( 'NONE', #54892 ) ;
#83830 = CARTESIAN_POINT ( 'NONE',  ( -23.49999999999994316, 64.35000000001120668, -7.323107484524790323 ) ) ;
#83832 = ORIENTED_EDGE ( 'NONE', *, *, #105148, .T. ) ;
#83833 = DIRECTION ( 'NONE',  ( -1.000000000000000000, 0.000000000000000000, 0.000000000000000000 ) ) ;
#83834 = EDGE_CURVE ( 'NONE', #250417, #124544, #106747, .T. ) ;
#83835 = CARTESIAN_POINT ( 'NONE',  ( 20.84451136049652575, 10.62014191481791947, -141.4939245595324167 ) ) ;
#83836 = LINE ( 'NONE', #225927, #256976 ) ;
#83837 = EDGE_CURVE ( 'NONE', #255703, #88829, #4335, .T. ) ;
#83838 = ORIENTED_EDGE ( 'NONE', *, *, #2752, .T. ) ;
#83839 = VECTOR ( 'NONE', #113813, 1000.000000000000227 ) ;
#83840 = CARTESIAN_POINT ( 'NONE',  ( -20.05000000000000426, 52.17883100310857003, -232.4626431718731396 ) ) ;
#83841 = AXIS2_PLACEMENT_3D ( 'NONE', #214617, #681, #118095 ) ;
#83842 = DIRECTION ( 'NONE',  ( 0.000000000000000000, 0.000000000000000000, -1.000000000000000000 ) ) ;
#83843 = ORIENTED_EDGE ( 'NONE', *, *, #188663, .T. ) ;
#83844 = CARTESIAN_POINT ( 'NONE',  ( 20.94999999999999929, 6.550000000011156231, -146.2500000000000284 ) ) ;
#83845 = LINE ( 'NONE', #119176, #21391 ) ;
#83846 = AXIS2_PLACEMENT_3D ( 'NONE', #25274, #23996, #78785 ) ;
#83847 = CARTESIAN_POINT ( 'NONE',  ( -20.54999999999999716, 85.50000000001197975, -112.9170766071766820 ) ) ;
#83848 = CIRCLE ( 'NONE', #13188, 0.09999999999998898659 ) ;
#83849 = EDGE_CURVE ( 'NONE', #49363, #36582, #79167, .T. ) ;
#83850 = PLANE ( 'NONE',  #220155 ) ;
#83852 = EDGE_LOOP ( 'NONE', ( #66435, #71318, #158794, #215833 ) ) ;
#83851 = CARTESIAN_POINT ( 'NONE',  ( -20.87600722750343252, 67.49230083716666684, -195.4236814984208763 ) ) ;
#83853 = DIRECTION ( 'NONE',  ( -0.000000000000000000, 0.2605042016806385363, 0.9654727137038795481 ) ) ;
#83855 = ORIENTED_EDGE ( 'NONE', *, *, #201434, .T. ) ;
#83854 = CARTESIAN_POINT ( 'NONE',  ( 21.05000000000000071, 76.00000000001190870, -103.0231074845243029 ) ) ;
#83856 = CARTESIAN_POINT ( 'NONE',  ( -21.65000000000000213, 7.250000000011138646, -46.15000000000000568 ) ) ;
#83858 = AXIS2_PLACEMENT_3D ( 'NONE', #183012, #242957, #43491 ) ;
#83857 = LINE ( 'NONE', #222100, #179025 ) ;
#83859 = EDGE_LOOP ( 'NONE', ( #150168, #194654, #122948, #6514 ) ) ;
#83860 = DIRECTION ( 'NONE',  ( 0.000000000000000000, -0.000000000000000000, -1.000000000000000000 ) ) ;
#83861 = CARTESIAN_POINT ( 'NONE',  ( -23.25000000000000000, -9.599999999988847676, -177.3939691226524076 ) ) ;
#83863 = DIRECTION ( 'NONE',  ( 1.000000000000000000, 0.000000000000000000, 0.000000000000000000 ) ) ;
#83862 = CARTESIAN_POINT ( 'NONE',  ( -16.93433913041102912, 63.05405028161031566, -213.0305799143420984 ) ) ;
#83864 = CARTESIAN_POINT ( 'NONE',  ( 18.39999999999999503, 5.649999999999983480, -20.85000000000000142 ) ) ;
#83865 = CARTESIAN_POINT ( 'NONE',  ( 20.95443524775735256, 40.81698247481438102, -237.9596272153440850 ) ) ;
#83866 = CARTESIAN_POINT ( 'NONE',  ( -18.59999999999999787, 15.92646454033039305, -219.3818586450342707 ) ) ;
#83867 = CARTESIAN_POINT ( 'NONE',  ( -20.64999999999999858, 78.89331866122350334, -228.7665898296168052 ) ) ;
#83868 = DIRECTION ( 'NONE',  ( 0.000000000000000000, 0.000000000000000000, -1.000000000000000000 ) ) ;
#83869 = CIRCLE ( 'NONE', #108851, 0.1000000000000028644 ) ;
#83870 = ORIENTED_EDGE ( 'NONE', *, *, #191094, .F. ) ;
#83871 = DIRECTION ( 'NONE',  ( 1.000000000000000000, 0.000000000000000000, 0.000000000000000000 ) ) ;
#83872 = ORIENTED_EDGE ( 'NONE', *, *, #99311, .F. ) ;
#83873 = AXIS2_PLACEMENT_3D ( 'NONE', #69896, #252344, #227651 ) ;
#83874 = ORIENTED_EDGE ( 'NONE', *, *, #47642, .T. ) ;
#83875 = EDGE_CURVE ( 'NONE', #37720, #197779, #137606, .T. ) ;
#83876 = DIRECTION ( 'NONE',  ( -1.000000000000000000, 0.000000000000000000, -0.000000000000000000 ) ) ;
#83877 = CARTESIAN_POINT ( 'NONE',  ( -21.05000000000000071, 3.338403738567107926, -231.7022719401450388 ) ) ;
#83878 = ORIENTED_EDGE ( 'NONE', *, *, #254506, .F. ) ;
#83879 = TOROIDAL_SURFACE ( 'NONE', #163062, 11.65000000000000036, 0.1000000000000000056 ) ;
#83880 = ORIENTED_EDGE ( 'NONE', *, *, #122398, .F. ) ;
#83881 =( NAMED_UNIT ( * ) SI_UNIT ( $, .STERADIAN. ) SOLID_ANGLE_UNIT ( ) );
#83882 = EDGE_CURVE ( 'NONE', #34950, #133581, #100256, .T. ) ;
#83884 = ORIENTED_EDGE ( 'NONE', *, *, #251627, .T. ) ;
#83883 = CIRCLE ( 'NONE', #146448, 0.09999999999999939493 ) ;
#83885 = LINE ( 'NONE', #163472, #45936 ) ;
#83886 = AXIS2_PLACEMENT_3D ( 'NONE', #105434, #203293, #139448 ) ;
#83887 = ORIENTED_EDGE ( 'NONE', *, *, #34187, .F. ) ;
#83888 = LINE ( 'NONE', #146456, #158835 ) ;
#83889 = DIRECTION ( 'NONE',  ( -1.000000000000000000, 0.000000000000000000, 0.000000000000000000 ) ) ;
#83891 = DIRECTION ( 'NONE',  ( 0.000000000000000000, -7.026728003956683390E-15, 1.000000000000000000 ) ) ;
#83890 = TOROIDAL_SURFACE ( 'NONE', #54889, 1.900000000000002576, 0.1000000000000000056 ) ;
#83892 = DIRECTION ( 'NONE',  ( 0.000000000000000000, -0.9915357197604971473, 0.1298341882519111479 ) ) ;
#83893 = DIRECTION ( 'NONE',  ( 1.000000000000000000, -0.000000000000000000, -0.000000000000000000 ) ) ;
#83894 = DIRECTION ( 'NONE',  ( 0.000000000000000000, 0.9126074666063844765, 0.4088369013363114535 ) ) ;
#83895 = CARTESIAN_POINT ( 'NONE',  ( 18.39999999999999503, 11.47316190337363828, -79.65000000000004832 ) ) ;
#83897 = EDGE_LOOP ( 'NONE', ( #136444, #6756, #230539, #255293 ) ) ;
#83896 = CARTESIAN_POINT ( 'NONE',  ( -22.50000000000000000, 75.90000000001214175, -136.5231074845242745 ) ) ;
#83899 = DIRECTION ( 'NONE',  ( 1.000000000000000000, 0.000000000000000000, 0.000000000000000000 ) ) ;
#83898 = CARTESIAN_POINT ( 'NONE',  ( 20.95462737510932882, 65.44321804836786782, -61.95315742796210401 ) ) ;
#83900 = CARTESIAN_POINT ( 'NONE',  ( 20.27550659511089037, 29.85975963366233543, -235.4540239816438429 ) ) ;
#83901 = VERTEX_POINT ( 'NONE', #195733 ) ;
#83902 = CYLINDRICAL_SURFACE ( 'NONE', #43931, 12.87499999999999822 ) ;
#83903 = PLANE ( 'NONE',  #58393 ) ;
#83904 = ORIENTED_EDGE ( 'NONE', *, *, #76086, .T. ) ;
#83906 = DIRECTION ( 'NONE',  ( -0.000000000000000000, 0.9910465087640860649, -0.1335171055202901413 ) ) ;
#83905 = CARTESIAN_POINT ( 'NONE',  ( -23.15000000000000213, 64.25000000001151079, -48.17310748452440805 ) ) ;
#83907 = FACE_OUTER_BOUND ( 'NONE', #77964, .T. ) ;
#83908 = ORIENTED_EDGE ( 'NONE', *, *, #92891, .T. ) ;
#83909 = DIRECTION ( 'NONE',  ( 0.000000000000000000, 0.8814952561688430555, -0.4721928772777346239 ) ) ;
#83910 = DIRECTION ( 'NONE',  ( 0.000000000000000000, -0.2617529984164955192, -0.9651348961777178603 ) ) ;
#83911 = CARTESIAN_POINT ( 'NONE',  ( 21.05000000000000071, 1.115600667400684642E-11, -67.00000000000000000 ) ) ;
#83912 = CARTESIAN_POINT ( 'NONE',  ( -22.50000000000094147, 0.1008583691097610785, -122.2504328765106010 ) ) ;
#83913 = ORIENTED_EDGE ( 'NONE', *, *, #145410, .F. ) ;
#83914 = ORIENTED_EDGE ( 'NONE', *, *, #123623, .T. ) ;
#83915 = TOROIDAL_SURFACE ( 'NONE', #138119, 12.97499999999999787, 0.1000000000000000056 ) ;
#83916 = EDGE_CURVE ( 'NONE', #179923, #161541, #75769, .T. ) ;
#83917 = CARTESIAN_POINT ( 'NONE',  ( 23.15000000000000213, -9.599999999988842347, -157.6060308773475640 ) ) ;
#83918 = DIRECTION ( 'NONE',  ( 0.000000000000000000, -1.000000000000000000, 0.000000000000000000 ) ) ;
#83919 = CARTESIAN_POINT ( 'NONE',  ( -21.00000000000000000, 7.986648289447971116, 1.311673547813416718 ) ) ;
#83920 = DIRECTION ( 'NONE',  ( 0.000000000000000000, -0.4088369013363280513, 0.9126074666063769270 ) ) ;
#83921 = DIRECTION ( 'NONE',  ( -0.000000000000000000, -0.9910465087640860649, 0.1335171055202901413 ) ) ;
#83922 = DIRECTION ( 'NONE',  ( 1.000000000000000000, 0.000000000000000000, 0.000000000000000000 ) ) ;
#83923 = AXIS2_PLACEMENT_3D ( 'NONE', #239160, #98318, #141341 ) ;
#83925 = ORIENTED_EDGE ( 'NONE', *, *, #3645, .T. ) ;
#83924 = CARTESIAN_POINT ( 'NONE',  ( -21.05000000000000071, 4.260086453440760756, -245.2296700999207246 ) ) ;
#83926 = CARTESIAN_POINT ( 'NONE',  ( -21.05000000000000071, 6.478078221105890933, -33.59999993530665563 ) ) ;
#83927 = CARTESIAN_POINT ( 'NONE',  ( -20.54999999999999716, -8.663551401858001100, -191.4758988819326646 ) ) ;
#83928 = FACE_OUTER_BOUND ( 'NONE', #21888, .T. ) ;
#83929 = CARTESIAN_POINT ( 'NONE',  ( -20.64999999999999858, 47.48953316408024961, -242.5895867826444601 ) ) ;
#83930 = EDGE_CURVE ( 'NONE', #64533, #172048, #241357, .T. ) ;
#83931 = CARTESIAN_POINT ( 'NONE',  ( 0.8999999999999980238, -8.250000000000005329, 21.95857864376268864 ) ) ;
#83933 = ORIENTED_EDGE ( 'NONE', *, *, #37178, .T. ) ;
#83932 = DIRECTION ( 'NONE',  ( 1.000000000000000000, 0.000000000000000000, 0.000000000000000000 ) ) ;
#83935 = CYLINDRICAL_SURFACE ( 'NONE', #183997, 0.09999999999999933942 ) ;
#83934 = APPLICATION_CONTEXT ( 'automotive_design' ) ;
#83936 = CARTESIAN_POINT ( 'NONE',  ( -18.54148534481894117, 65.67467670974468774, -164.4531731826884879 ) ) ;
#83937 = DIRECTION ( 'NONE',  ( -1.000000000000000000, -1.836970198721029934E-16, -3.186635328391151676E-31 ) ) ;
#83938 = DIRECTION ( 'NONE',  ( 0.000000000000000000, 0.9550021345545507412, -0.2965989261549202838 ) ) ;
#83939 = EDGE_CURVE ( 'NONE', #90874, #200975, #91841, .T. ) ;
#83940 = VERTEX_POINT ( 'NONE', #120052 ) ;
#83941 = CARTESIAN_POINT ( 'NONE',  ( -15.31895204843004521, 66.60346600605832634, -152.1171677053511075 ) ) ;
#83942 = CARTESIAN_POINT ( 'NONE',  ( -16.85722902420155478, 66.05000000001200533, -115.7886549582948845 ) ) ;
#83943 = CARTESIAN_POINT ( 'NONE',  ( 21.00000000000000000, 63.38346053167636995, -212.7939182281409956 ) ) ;
#83945 = AXIS2_PLACEMENT_3D ( 'NONE', #185299, #65342, #180178 ) ;
#83944 = CARTESIAN_POINT ( 'NONE',  ( 22.59999999999999432, 11.74987124438766273, -167.4345704089863034 ) ) ;
#83946 = ADVANCED_FACE ( 'NONE', ( #204671 ), #224243, .F. ) ;
#83947 = EDGE_LOOP ( 'NONE', ( #150947, #12697, #257806, #10098 ) ) ;
#83949 = CIRCLE ( 'NONE', #229745, 4.149999999999999467 ) ;
#83948 = CARTESIAN_POINT ( 'NONE',  ( -16.77431908686106610, 9.945805754529134290, -87.83583921765028890 ) ) ;
#83950 = ORIENTED_EDGE ( 'NONE', *, *, #254983, .T. ) ;
#83951 = AXIS2_PLACEMENT_3D ( 'NONE', #122516, #101611, #181209 ) ;
#83952 = EDGE_CURVE ( 'NONE', #195393, #135120, #191651, .T. ) ;
#83953 = CARTESIAN_POINT ( 'NONE',  ( 21.00000000000000000, 14.04870287383362992, -219.6884709798077893 ) ) ;
#83954 = CARTESIAN_POINT ( 'NONE',  ( -12.25000000000000178, 9.350000000011139178, -50.25000000000000000 ) ) ;
#83955 = FACE_OUTER_BOUND ( 'NONE', #234477, .T. ) ;
#83956 = CARTESIAN_POINT ( 'NONE',  ( 18.49999999999999645, -1.866714910046153308, -179.2526752462819672 ) ) ;
#83957 = ORIENTED_EDGE ( 'NONE', *, *, #147089, .F. ) ;
#83958 = ADVANCED_FACE ( 'NONE', ( #160461 ), #24806, .T. ) ;
#83959 = CARTESIAN_POINT ( 'NONE',  ( -20.54999999999999716, 76.00000000001165290, -69.52310748452431710 ) ) ;
#83960 = ADVANCED_FACE ( 'NONE', ( #143428 ), #183841, .F. ) ;
#83961 = CARTESIAN_POINT ( 'NONE',  ( 18.59999999999999787, -1.835859311432481045, -212.5044391687984842 ) ) ;
#83962 = CARTESIAN_POINT ( 'NONE',  ( 13.88638282980483574, 9.457426452488901347, -18.50004186840002873 ) ) ;
#83963 = CARTESIAN_POINT ( 'NONE',  ( -16.93710578446422943, 9.949999999999983302, -20.58119601620066064 ) ) ;
#83964 = CARTESIAN_POINT ( 'NONE',  ( 20.94999999999999929, -9.499999999988844479, -191.1060308773475072 ) ) ;
#83965 = ORIENTED_EDGE ( 'NONE', *, *, #146273, .F. ) ;
#83967 = ORIENTED_EDGE ( 'NONE', *, *, #180447, .T. ) ;
#83966 = CARTESIAN_POINT ( 'NONE',  ( -23.39999999999994529, 77.83551161375991967, -47.52760213295649550 ) ) ;
#83968 = ORIENTED_EDGE ( 'NONE', *, *, #109677, .F. ) ;
#83969 = DIRECTION ( 'NONE',  ( 0.000000000000000000, -0.2617529984164915779, -0.9651348961777189706 ) ) ;
#83970 = ORIENTED_EDGE ( 'NONE', *, *, #38786, .T. ) ;
#83971 = CARTESIAN_POINT ( 'NONE',  ( 21.07888907270776002, 65.27493078649683866, -124.3019138976911790 ) ) ;
#83972 = CARTESIAN_POINT ( 'NONE',  ( 20.85000000000000142, 7.128833340094563376, -233.7327013124401276 ) ) ;
#83973 = FACE_OUTER_BOUND ( 'NONE', #189589, .T. ) ;
#83974 = VERTEX_POINT ( 'NONE', #101702 ) ;
#83975 = DIRECTION ( 'NONE',  ( -1.000000000000000000, 0.000000000000000000, 0.000000000000000000 ) ) ;
#83976 = CARTESIAN_POINT ( 'NONE',  ( -23.25000000000000000, 1.148907358139439339E-11, -201.0000000000015064 ) ) ;
#83977 = ORIENTED_EDGE ( 'NONE', *, *, #144120, .T. ) ;
#83978 = ADVANCED_FACE ( 'NONE', ( #182581 ), #161741, .T. ) ;
#83979 = DIRECTION ( 'NONE',  ( 0.000000000000000000, 0.000000000000000000, 1.000000000000000000 ) ) ;
#83981 = ORIENTED_EDGE ( 'NONE', *, *, #93778, .F. ) ;
#83980 = DIRECTION ( 'NONE',  ( 0.000000000000000000, 0.000000000000000000, 1.000000000000000000 ) ) ;
#83982 = AXIS2_PLACEMENT_3D ( 'NONE', #69638, #110026, #210434 ) ;
#83983 = AXIS2_PLACEMENT_3D ( 'NONE', #13805, #93333, #172927 ) ;
#83984 = FACE_OUTER_BOUND ( 'NONE', #65235, .T. ) ;
#83985 = B_SPLINE_CURVE_WITH_KNOTS ( 'NONE', 3,
 ( #112759, #72366, #115314, #133594, #151909, #198398, #103130, #246506, #147412, #144827, #245239, #43184, #101833, #105685, #24920, #161865, #23650, #182705, #183970 ),
 .UNSPECIFIED., .F., .F.,
 ( 4, 3, 3, 3, 3, 3, 4 ),
 ( 0.000000000000000000, 1.655171619026472483E-05, 2.773500582848447571E-05, 5.941817267378177332E-05, 0.0001114174635873370778, 0.0001914169455916087017, 0.0002627181070750251170 ),
 .UNSPECIFIED. ) ;
#83986 = DIRECTION ( 'NONE',  ( -1.000000000000000000, -0.000000000000000000, 0.000000000000000000 ) ) ;
#83987 = AXIS2_PLACEMENT_3D ( 'NONE', #95822, #253616, #175415 ) ;
#83988 = ORIENTED_EDGE ( 'NONE', *, *, #22895, .T. ) ;
#83989 = DIRECTION ( 'NONE',  ( -1.000000000000000000, -0.000000000000000000, -0.000000000000000000 ) ) ;
#83991 = ADVANCED_FACE ( 'NONE', ( #123883 ), #44346, .T. ) ;
#83990 = PLANE ( 'NONE',  #21227 ) ;
#83992 = DIRECTION ( 'NONE',  ( -1.652117596168391700E-15, 0.9651348961777157509, -0.2617529984165031243 ) ) ;
#83993 = EDGE_LOOP ( 'NONE', ( #114946, #169694, #122828 ) ) ;
#83994 = DIRECTION ( 'NONE',  ( -6.938893903907221278E-15, 0.9770955615653313941, 0.2128009952263606730 ) ) ;
#83995 = CARTESIAN_POINT ( 'NONE',  ( -20.64999999999999858, 85.40000000001221281, -146.4170766071767389 ) ) ;
#83996 = CIRCLE ( 'NONE', #4903, 0.1000000000000013933 ) ;
#83997 = VERTEX_POINT ( 'NONE', #121345 ) ;
#83998 = ADVANCED_FACE ( 'NONE', ( #239978 ), #5173, .F. ) ;
#83999 = ADVANCED_FACE ( 'NONE', ( #26068 ), #142143, .F. ) ;
#84000 = ORIENTED_EDGE ( 'NONE', *, *, #14494, .T. ) ;
#84001 = CARTESIAN_POINT ( 'NONE',  ( 21.05000000000000071, 65.27628288308754634, -191.3468678833862668 ) ) ;
#84002 = ORIENTED_EDGE ( 'NONE', *, *, #56877, .F. ) ;
#84003 = CARTESIAN_POINT ( 'NONE',  ( 18.49999999999999289, 10.29270135740183179, -38.95736188715193293 ) ) ;
#84004 = CARTESIAN_POINT ( 'NONE',  ( -18.59999999999999787, 67.84340367245323478, -228.0791829662263410 ) ) ;
#84005 = VECTOR ( 'NONE', #52381, 1000.000000000000000 ) ;
#84008 = ADVANCED_FACE ( 'NONE', ( #145992 ), #245782, .T. ) ;
#84007 = VERTEX_POINT ( 'NONE', #43058 ) ;
#84006 = CARTESIAN_POINT ( 'NONE',  ( -21.05000000000000071, -1.249999999988843369, -108.5000000000000426 ) ) ;
#84009 = FACE_OUTER_BOUND ( 'NONE', #112651, .T. ) ;
#84010 = CARTESIAN_POINT ( 'NONE',  ( 21.08489834409762054, 10.62232389474667293, -112.8500000000000369 ) ) ;
#84011 = DIRECTION ( 'NONE',  ( -1.000000000000000000, 0.000000000000000000, 0.000000000000000000 ) ) ;
#84012 = CARTESIAN_POINT ( 'NONE',  ( -21.14999999999999858, 6.257814610487270279, -133.9022097086912311 ) ) ;
#84013 = FACE_OUTER_BOUND ( 'NONE', #18646, .T. ) ;
#84014 = AXIS2_PLACEMENT_3D ( 'NONE', #155173, #172184, #13082 ) ;
#84015 = ADVANCED_FACE ( 'NONE', ( #45626 ), #202127, .F. ) ;
#84016 = DIRECTION ( 'NONE',  ( 2.694716079187271467E-16, -0.4721928772777345129, -0.8814952561688430555 ) ) ;
#84017 = ADVANCED_FACE ( 'NONE', ( #105551 ), #2624, .T. ) ;
#84019 = ORIENTED_EDGE ( 'NONE', *, *, #95857, .T. ) ;
#84018 = CARTESIAN_POINT ( 'NONE',  ( -18.48550754432008958, -9.463399778548764019, -107.5487897524156580 ) ) ;
#84021 = ORIENTED_EDGE ( 'NONE', *, *, #67681, .F. ) ;
#84020 = CARTESIAN_POINT ( 'NONE',  ( 22.88900146558018989, 10.47295594553888343, -208.1859343425765303 ) ) ;
#84022 = FACE_OUTER_BOUND ( 'NONE', #182173, .T. ) ;
#84023 = ORIENTED_EDGE ( 'NONE', *, *, #69625, .F. ) ;
#84024 = CIRCLE ( 'NONE', #34048, 0.09999999999998898659 ) ;
#84025 = CARTESIAN_POINT ( 'NONE',  ( -20.64999999999999858, 26.18196512540240661, -241.1028522842020152 ) ) ;
#84026 = AXIS2_PLACEMENT_3D ( 'NONE', #211297, #234713, #54775 ) ;
#84027 = EDGE_CURVE ( 'NONE', #242320, #5729, #186428, .T. ) ;
#84028 = AXIS2_PLACEMENT_3D ( 'NONE', #45171, #21775, #43893 ) ;
#84029 = DIRECTION ( 'NONE',  ( 0.000000000000000000, 0.000000000000000000, -1.000000000000000000 ) ) ;
#84030 = DIRECTION ( 'NONE',  ( 0.000000000000000000, -0.2617529984165031243, -0.9651348961777157509 ) ) ;
#84031 = CARTESIAN_POINT ( 'NONE',  ( 21.05000000000000071, 4.813084112160680661, -145.9415177565238366 ) ) ;
#84032 = CIRCLE ( 'NONE', #250673, 7.899999999999990585 ) ;
#84033 = ORIENTED_EDGE ( 'NONE', *, *, #179730, .F. ) ;
#84034 = DIRECTION ( 'NONE',  ( 0.000000000000000000, -0.8777080977375715243, 0.4791956752370512551 ) ) ;
#84035 = VECTOR ( 'NONE', #193626, 1000.000000000000227 ) ;
#84036 = ORIENTED_EDGE ( 'NONE', *, *, #122668, .T. ) ;
#84037 = DIRECTION ( 'NONE',  ( 1.000000000000000000, 0.000000000000000000, 0.000000000000000000 ) ) ;
#84038 = AXIS2_PLACEMENT_3D ( 'NONE', #225156, #186059, #47807 ) ;
#84039 = ORIENTED_EDGE ( 'NONE', *, *, #34128, .F. ) ;
#84040 = CIRCLE ( 'NONE', #155050, 0.09999999999999939493 ) ;
#84041 = CARTESIAN_POINT ( 'NONE',  ( -23.25000000000000000, 14.73746888278882494, -235.8584165281851028 ) ) ;
#84042 = CIRCLE ( 'NONE', #866, 0.1000000000000070832 ) ;
#84043 = DIRECTION ( 'NONE',  ( -1.000000000000000000, -0.000000000000000000, -0.000000000000000000 ) ) ;
#84044 = ORIENTED_EDGE ( 'NONE', *, *, #103004, .F. ) ;
#84045 = CARTESIAN_POINT ( 'NONE',  ( 20.94999999999999929, 77.83534155023671985, -158.4679561919613491 ) ) ;
#84046 = EDGE_CURVE ( 'NONE', #141595, #130365, #33438, .T. ) ;
#84047 = ORIENTED_EDGE ( 'NONE', *, *, #254426, .F. ) ;
#84048 = EDGE_CURVE ( 'NONE', #196016, #243821, #242529, .T. ) ;
#84050 = VECTOR ( 'NONE', #563, 1000.000000000000000 ) ;
#84049 = CARTESIAN_POINT ( 'NONE',  ( -14.77738660682464022, 9.436552840015577814, -48.67795547276032408 ) ) ;
#84051 = ORIENTED_EDGE ( 'NONE', *, *, #192530, .F. ) ;
#84052 = CARTESIAN_POINT ( 'NONE',  ( -21.05000000000000071, 77.16270174994990327, -95.12310748452431142 ) ) ;
#84053 = CARTESIAN_POINT ( 'NONE',  ( -21.05000000000000071, 0.9150442794848296924, -205.2015109147324097 ) ) ;
#84054 = EDGE_LOOP ( 'NONE', ( #202455, #252093, #174230, #19013 ) ) ;
#84055 = EDGE_CURVE ( 'NONE', #61516, #6907, #10359, .T. ) ;
#84056 = LINE ( 'NONE', #243175, #202766 ) ;
#84058 = VERTEX_POINT ( 'NONE', #132870 ) ;
#84057 = DIRECTION ( 'NONE',  ( -0.000000000000000000, -0.000000000000000000, 1.000000000000000000 ) ) ;
#84059 = CIRCLE ( 'NONE', #21587, 0.4999999999999935607 ) ;
#84061 = ORIENTED_EDGE ( 'NONE', *, *, #154228, .F. ) ;
#84060 = CIRCLE ( 'NONE', #883, 0.09999999999999939493 ) ;
#84062 = CIRCLE ( 'NONE', #234131, 0.09999999999999939493 ) ;
#84063 = AXIS2_PLACEMENT_3D ( 'NONE', #251337, #110549, #90988 ) ;
#84064 = B_SPLINE_CURVE_WITH_KNOTS ( 'NONE', 3,
 ( #202379, #238947, #1597, #216796, #57714, #60284, #139821, #38188, #240238, #61584, #220664, #42040, #181551, #2873, #82395, #241506, #62865, #104526, #68000, #144951, #66726, #164547, #204926, #84961, #107120, #143678 ),
 .UNSPECIFIED., .F., .F.,
 ( 4, 2, 2, 2, 2, 2, 2, 2, 2, 2, 2, 2, 4 ),
 ( 0.005476422646581336103, 0.006160811967703527965, 0.006845201288825720695, 0.007187395949386819229, 0.007529590609947917762, 0.007871785270509017163, 0.008213979931070114829, 0.008556174591631212495, 0.008898369252192311896, 0.009240563912753411296, 0.009582758573314508962, 0.01026714789443677021, 0.01095153721555903320 ),
 .UNSPECIFIED. ) ;
#84065 = VERTEX_POINT ( 'NONE', #151150 ) ;
#84066 = CARTESIAN_POINT ( 'NONE',  ( 18.59999999999999076, 70.05000000001165006, -59.21740517948951066 ) ) ;
#84067 = CARTESIAN_POINT ( 'NONE',  ( -20.94999999999999929, -1.162701749926853712, -141.9000000000000341 ) ) ;
#84068 = LINE ( 'NONE', #244472, #216076 ) ;
#84069 = CARTESIAN_POINT ( 'NONE',  ( -23.25000000000000000, 64.25000000001219291, -143.5379132551784096 ) ) ;
#84070 = CARTESIAN_POINT ( 'NONE',  ( 25.10847955711010115, 9.068702471349586958, 33.00000000000000000 ) ) ;
#84071 = ORIENTED_EDGE ( 'NONE', *, *, #117975, .F. ) ;
#84072 = CARTESIAN_POINT ( 'NONE',  ( -18.79999999999999716, -1.300000000000000044, -7.900000000000000355 ) ) ;
#84073 = CARTESIAN_POINT ( 'NONE',  ( -12.25000000000000178, 9.850000000011133849, -117.2500000000000284 ) ) ;
#84074 = DIRECTION ( 'NONE',  ( 0.000000000000000000, 0.9908441862701596881, 0.1350103645451904977 ) ) ;
#84075 = DIRECTION ( 'NONE',  ( 0.000000000000000000, 0.9908441862701596881, -0.1350103645451904977 ) ) ;
#84076 = ADVANCED_FACE ( 'NONE', ( #49470 ), #69053, .T. ) ;
#84077 = ORIENTED_EDGE ( 'NONE', *, *, #227965, .F. ) ;
#84079 = CYLINDRICAL_SURFACE ( 'NONE', #172089, 7.900000000000010125 ) ;
#84078 = AXIS2_PLACEMENT_3D ( 'NONE', #247115, #68501, #227562 ) ;
#84080 = ORIENTED_EDGE ( 'NONE', *, *, #138459, .T. ) ;
#84081 = CARTESIAN_POINT ( 'NONE',  ( 15.74999999999999645, 9.350000000011139178, -117.2500000000000284 ) ) ;
#84082 = ORIENTED_EDGE ( 'NONE', *, *, #247270, .F. ) ;
#84083 = DIRECTION ( 'NONE',  ( -1.000000000000000000, 0.000000000000000000, -0.000000000000000000 ) ) ;
#84084 = CARTESIAN_POINT ( 'NONE',  ( -20.90851465518106167, 10.32532329027886320, -72.56993430183595706 ) ) ;
#84085 = ORIENTED_EDGE ( 'NONE', *, *, #84544, .T. ) ;
#84088 = EDGE_LOOP ( 'NONE', ( #120273, #23612, #197410 ) ) ;
#84087 = EDGE_CURVE ( 'NONE', #132946, #8700, #145817, .T. ) ;
#84086 = DIRECTION ( 'NONE',  ( 0.000000000000000000, -2.771150684185008344E-14, -1.000000000000000000 ) ) ;
#84089 = DIRECTION ( 'NONE',  ( -2.952720810173289112E-16, -0.9651348961777157509, 0.2617529984165031243 ) ) ;
#84090 = ORIENTED_EDGE ( 'NONE', *, *, #254107, .T. ) ;
#84091 = CARTESIAN_POINT ( 'NONE',  ( 21.30000000000002558, 67.23127455305841238, -235.8551265064783991 ) ) ;
#84092 = ADVANCED_FACE ( 'NONE', ( #228119 ), #33800, .T. ) ;
#84093 = DIRECTION ( 'NONE',  ( 0.000000000000000000, 0.1350103645451876666, -0.9908441862701600211 ) ) ;
#84094 = ORIENTED_EDGE ( 'NONE', *, *, #108317, .T. ) ;
#84095 = DIRECTION ( 'NONE',  ( 1.000000000000000000, -0.000000000000000000, -0.000000000000000000 ) ) ;
#84096 = ADVANCED_FACE ( 'NONE', ( #230686 ), #52013, .T. ) ;
#84097 = FACE_OUTER_BOUND ( 'NONE', #130664, .T. ) ;
#84098 = ORIENTED_EDGE ( 'NONE', *, *, #176789, .F. ) ;
#84099 = ORIENTED_EDGE ( 'NONE', *, *, #193394, .T. ) ;
#84100 = EDGE_CURVE ( 'NONE', #125361, #170795, #99997, .T. ) ;
#84101 = TOROIDAL_SURFACE ( 'NONE', #34131, 0.2000000000000000111, 0.1000000000000000056 ) ;
#84104 = EDGE_CURVE ( 'NONE', #146761, #54754, #246389, .T. ) ;
#84103 = EDGE_CURVE ( 'NONE', #83582, #114637, #108417, .T. ) ;
#84102 = DIRECTION ( 'NONE',  ( 1.000000000000000000, 0.000000000000000000, 0.000000000000000000 ) ) ;
#84106 = ORIENTED_EDGE ( 'NONE', *, *, #239227, .F. ) ;
#84105 = CARTESIAN_POINT ( 'NONE',  ( 23.14999999999999858, 45.93587830916155212, -239.9163948487882863 ) ) ;
#84107 = CARTESIAN_POINT ( 'NONE',  ( 23.04999999999999716, 8.822561741677553471, -109.7500000000000426 ) ) ;
#84108 = DIRECTION ( 'NONE',  ( 0.000000000000000000, 0.8814952561688476074, -0.4721928772777262417 ) ) ;
#84109 = CARTESIAN_POINT ( 'NONE',  ( -22.39999999999999858, 75.90000000001219860, -144.3138870828977076 ) ) ;
#84111 = CARTESIAN_POINT ( 'NONE',  ( -18.59999999999999787, 64.35000000001247145, -181.7731074845244450 ) ) ;
#84110 = CARTESIAN_POINT ( 'NONE',  ( -16.93302609847409457, 66.00331747920864700, -90.43671898916183238 ) ) ;
#84112 = CARTESIAN_POINT ( 'NONE',  ( 21.05000000000000071, 10.62950747927179229, -108.1279793999968035 ) ) ;
#84113 = LINE ( 'NONE', #3329, #2653 ) ;
#84114 = AXIS2_PLACEMENT_3D ( 'NONE', #246541, #31396, #73093 ) ;
#84115 = DIRECTION ( 'NONE',  ( 0.000000000000000000, -0.9126074666059857954, -0.4088369013372012972 ) ) ;
#84116 = CARTESIAN_POINT ( 'NONE',  ( 21.05000000000000071, 5.000000000011153745, -188.5947339810868755 ) ) ;
#84117 = EDGE_CURVE ( 'NONE', #67578, #173670, #129438, .T. ) ;
#84118 = ADVANCED_FACE ( 'NONE', ( #130275 ), #79347, .F. ) ;
#84119 = TOROIDAL_SURFACE ( 'NONE', #146524, 0.2000000000000000111, 0.1000000000000000056 ) ;
#84120 = VERTEX_POINT ( 'NONE', #209834 ) ;
#84121 = EDGE_LOOP ( 'NONE', ( #40210, #5614, #83649, #146784 ) ) ;
#84122 = EDGE_CURVE ( 'NONE', #2981, #88364, #47126, .T. ) ;
#84123 = FACE_OUTER_BOUND ( 'NONE', #158077, .T. ) ;
#84124 = ORIENTED_EDGE ( 'NONE', *, *, #168996, .T. ) ;
#84125 = DIRECTION ( 'NONE',  ( 1.000000000000000000, 0.000000000000000000, 0.000000000000000000 ) ) ;
#84126 = ADVANCED_FACE ( 'NONE', ( #12939 ), #200180, .F. ) ;
#84127 = ORIENTED_EDGE ( 'NONE', *, *, #30268, .F. ) ;
#84128 = VECTOR ( 'NONE', #187453, 1000.000000000000000 ) ;
#84129 =( NAMED_UNIT ( * ) PLANE_ANGLE_UNIT ( ) SI_UNIT ( $, .RADIAN. ) );
#84130 = CARTESIAN_POINT ( 'NONE',  ( 20.87600722750343252, 65.66887361445355964, -130.9329845918269370 ) ) ;
#84131 = EDGE_CURVE ( 'NONE', #163251, #84480, #192007, .T. ) ;
#84132 = VERTEX_POINT ( 'NONE', #9055 ) ;
#84133 = CARTESIAN_POINT ( 'NONE',  ( -20.94999999999999929, 1.851028230140860487, -11.65391326942249250 ) ) ;
#84134 = ORIENTED_EDGE ( 'NONE', *, *, #37874, .T. ) ;
#84135 = ORIENTED_EDGE ( 'NONE', *, *, #187472, .T. ) ;
#84136 = DIRECTION ( 'NONE',  ( 0.000000000000000000, 0.2617529984165026247, 0.9651348961777158619 ) ) ;
#84137 = CARTESIAN_POINT ( 'NONE',  ( -23.25000000000000000, -1.835859311432481045, -112.0044391687985694 ) ) ;
#84139 = ORIENTED_EDGE ( 'NONE', *, *, #82509, .T. ) ;
#84138 = DIRECTION ( 'NONE',  ( 1.000000000000000000, 0.000000000000000000, 0.000000000000000000 ) ) ;
#84140 = EDGE_CURVE ( 'NONE', #54663, #75721, #245969, .T. ) ;
#84141 = CARTESIAN_POINT ( 'NONE',  ( 19.75857864376269291, 11.75000000001116263, -158.8500000000000227 ) ) ;
#84143 = ORIENTED_EDGE ( 'NONE', *, *, #202515, .F. ) ;
#84142 = DIRECTION ( 'NONE',  ( -3.265361837132813093E-16, 0.9770955615653316162, 0.2128009952263604232 ) ) ;
#84144 = ORIENTED_EDGE ( 'NONE', *, *, #142531, .T. ) ;
#84145 = DIRECTION ( 'NONE',  ( 0.000000000000000000, 0.000000000000000000, -1.000000000000000000 ) ) ;
#84147 = ORIENTED_EDGE ( 'NONE', *, *, #73215, .F. ) ;
#84146 = FACE_OUTER_BOUND ( 'NONE', #227279, .T. ) ;
#84148 = DIRECTION ( 'NONE',  ( 0.000000000000000000, 6.982962677686266711E-15, -1.000000000000000000 ) ) ;
#84149 = DIRECTION ( 'NONE',  ( -0.000000000000000000, -0.1298341882519805091, -0.9915357197604881545 ) ) ;
#84150 = CIRCLE ( 'NONE', #54966, 0.09999999999999939493 ) ;
#84151 = AXIS2_PLACEMENT_3D ( 'NONE', #118983, #56409, #134657 ) ;
#84152 = FACE_OUTER_BOUND ( 'NONE', #202810, .T. ) ;
#84153 = AXIS2_PLACEMENT_3D ( 'NONE', #16039, #155557, #235068 ) ;
#84155 = EDGE_CURVE ( 'NONE', #114284, #177411, #166896, .T. ) ;
#84154 = EDGE_LOOP ( 'NONE', ( #154778, #232723, #13338, #161449 ) ) ;
#84156 = CYLINDRICAL_SURFACE ( 'NONE', #120645, 4.000000000000002665 ) ;
#84157 = CYLINDRICAL_SURFACE ( 'NONE', #215948, 0.09999999999999939493 ) ;
#84158 = CARTESIAN_POINT ( 'NONE',  ( 20.97224591636398472, 65.37484658384866520, -157.7731815798608466 ) ) ;
#84159 = PLANE ( 'NONE',  #214113 ) ;
#84160 = CARTESIAN_POINT ( 'NONE',  ( -17.11825945287482753, 44.22674245267958781, -235.2580479164737994 ) ) ;
#84161 = ORIENTED_EDGE ( 'NONE', *, *, #123635, .T. ) ;
#84162 = ORIENTED_EDGE ( 'NONE', *, *, #60601, .T. ) ;
#84163 = ORIENTED_EDGE ( 'NONE', *, *, #217423, .F. ) ;
#84164 = CARTESIAN_POINT ( 'NONE',  ( 18.59999999999999076, 76.00000000001213607, -136.5231074845243313 ) ) ;
#84165 = ORIENTED_EDGE ( 'NONE', *, *, #17235, .F. ) ;
#84166 = DIRECTION ( 'NONE',  ( 0.000000000000000000, 0.000000000000000000, 1.000000000000000000 ) ) ;
#84167 = EDGE_LOOP ( 'NONE', ( #197826, #43934, #246599, #137802 ) ) ;
#84168 = EDGE_CURVE ( 'NONE', #75088, #241392, #241862, .T. ) ;
#84169 = SURFACE_SIDE_STYLE ('',( #125911 ) ) ;
#84170 = AXIS2_PLACEMENT_3D ( 'NONE', #242767, #161988, #4160 ) ;
#84171 = EDGE_LOOP ( 'NONE', ( #182192, #57684, #201702 ) ) ;
#84172 = LINE ( 'NONE', #244583, #94481 ) ;
#84173 = VECTOR ( 'NONE', #195823, 999.9999999999998863 ) ;
#84174 = ORIENTED_EDGE ( 'NONE', *, *, #28259, .F. ) ;
#84175 = EDGE_LOOP ( 'NONE', ( #199700, #122354, #58490, #2668 ) ) ;
#84176 = ORIENTED_EDGE ( 'NONE', *, *, #105804, .T. ) ;
#84177 = FACE_OUTER_BOUND ( 'NONE', #185652, .T. ) ;
#84178 = DIRECTION ( 'NONE',  ( 0.000000000000000000, 0.2128009952263598958, -0.9770955615653316162 ) ) ;
#84179 = CARTESIAN_POINT ( 'NONE',  ( 20.94999999999999929, 1.115600667400684642E-11, -113.4750000000000369 ) ) ;
#84180 = CARTESIAN_POINT ( 'NONE',  ( 15.51872946208854565, 27.09445758862755582, -233.7906081272070651 ) ) ;
#84181 = SPHERICAL_SURFACE ( 'NONE', #210645, 0.1000000000000000056 ) ;
#84182 = CARTESIAN_POINT ( 'NONE',  ( 22.50000000000000000, 7.750000000011162626, -133.9000000000000057 ) ) ;
#84183 = AXIS2_PLACEMENT_3D ( 'NONE', #207335, #246445, #67802 ) ;
#84185 = DIRECTION ( 'NONE',  ( -1.000000000000000000, -0.000000000000000000, -0.000000000000000000 ) ) ;
#84184 = DIRECTION ( 'NONE',  ( -0.000000000000000000, 7.109473446599835262E-15, -1.000000000000000000 ) ) ;
#84186 = CARTESIAN_POINT ( 'NONE',  ( 21.05000000000000071, 61.00122447389660607, -225.2976766370351527 ) ) ;
#84188 = EDGE_LOOP ( 'NONE', ( #148065, #252608, #87924, #190763 ) ) ;
#84187 = DIRECTION ( 'NONE',  ( 0.000000000000000000, 0.000000000000000000, 1.000000000000000000 ) ) ;
#84190 = CARTESIAN_POINT ( 'NONE',  ( 21.08198257630413508, 69.66340326599689092, -103.0957508083089635 ) ) ;
#84189 = CARTESIAN_POINT ( 'NONE',  ( -21.00250684356851849, 11.75000000001115197, -40.51480576875963635 ) ) ;
#84191 = DIRECTION ( 'NONE',  ( 0.000000000000000000, -0.4721928772777285732, -0.8814952561688463861 ) ) ;
#84192 = ORIENTED_EDGE ( 'NONE', *, *, #75961, .F. ) ;
#84193 = DIRECTION ( 'NONE',  ( 0.000000000000000000, -0.2128009952263603677, 0.9770955615653313941 ) ) ;
#84194 = AXIS2_PLACEMENT_3D ( 'NONE', #2466, #81982, #102838 ) ;
#84195 = DIRECTION ( 'NONE',  ( 0.000000000000000000, -1.000000000000000000, -0.000000000000000000 ) ) ;
#84196 = CARTESIAN_POINT ( 'NONE',  ( -20.94999999999999929, -11.41227409413852811, -164.6000000000000227 ) ) ;
#84197 = VERTEX_POINT ( 'NONE', #178428 ) ;
#84198 = AXIS2_PLACEMENT_3D ( 'NONE', #104291, #183849, #24812 ) ;
#84199 = AXIS2_PLACEMENT_3D ( 'NONE', #171110, #155380, #75812 ) ;
#84200 = TOROIDAL_SURFACE ( 'NONE', #230008, 6.258578643762712446, 0.1000000000000000056 ) ;
#84201 = CARTESIAN_POINT ( 'NONE',  ( -22.59999999999999787, 0.09999999999999939493, 11.64957080754479968 ) ) ;
#84202 = CARTESIAN_POINT ( 'NONE',  ( 23.14999999999998437, 76.00000000001267608, -203.5231074845243597 ) ) ;
#84203 = AXIS2_PLACEMENT_3D ( 'NONE', #59896, #118635, #78187 ) ;
#84204 = ORIENTED_EDGE ( 'NONE', *, *, #186282, .T. ) ;
#84205 = ORIENTED_EDGE ( 'NONE', *, *, #11543, .F. ) ;
#84206 = CIRCLE ( 'NONE', #180145, 0.1999999999999987899 ) ;
#84207 = DIRECTION ( 'NONE',  ( 0.000000000000000000, -0.4088369013363280513, 0.9126074666063769270 ) ) ;
#84208 = ORIENTED_EDGE ( 'NONE', *, *, #40833, .T. ) ;
#84209 = CARTESIAN_POINT ( 'NONE',  ( 19.90000000000000568, 5.488301202077012775, 16.50000000000000000 ) ) ;
#84210 = CARTESIAN_POINT ( 'NONE',  ( -18.49372193242244933, -9.442484523346822201, -174.2647812600350505 ) ) ;
#84211 = CYLINDRICAL_SURFACE ( 'NONE', #11599, 0.09999999999999939493 ) ;
#84212 = DIRECTION ( 'NONE',  ( 0.000000000000000000, 0.000000000000000000, 1.000000000000000000 ) ) ;
#84213 = ORIENTED_EDGE ( 'NONE', *, *, #136665, .F. ) ;
#84214 = AXIS2_PLACEMENT_3D ( 'NONE', #240763, #101193, #125921 ) ;
#84216 = CIRCLE ( 'NONE', #200810, 0.1000000000000028644 ) ;
#84215 = LINE ( 'NONE', #163825, #183725 ) ;
#84218 = EDGE_CURVE ( 'NONE', #144320, #155936, #197947, .T. ) ;
#84217 = DIRECTION ( 'NONE',  ( 0.7071067811865463515, -0.7071067811865487940, -5.696443396193425170E-15 ) ) ;
#84220 = DIRECTION ( 'NONE',  ( 1.000000000000000000, 0.000000000000000000, 0.000000000000000000 ) ) ;
#84219 = AXIS2_PLACEMENT_3D ( 'NONE', #162354, #204022, #63215 ) ;
#84221 = AXIS2_PLACEMENT_3D ( 'NONE', #153859, #71717, #251621 ) ;
#84222 = CARTESIAN_POINT ( 'NONE',  ( 18.52928932188133970, 51.94054103949330425, -231.4415386711587530 ) ) ;
#84223 = ORIENTED_EDGE ( 'NONE', *, *, #7245, .F. ) ;
#84224 = CIRCLE ( 'NONE', #105673, 0.6000000000000033085 ) ;
#84225 = AXIS2_PLACEMENT_3D ( 'NONE', #8616, #32054, #208116 ) ;
#84227 = ORIENTED_EDGE ( 'NONE', *, *, #104881, .T. ) ;
#84226 = DIRECTION ( 'NONE',  ( 1.000000000000000000, -7.049440681616512959E-16, 1.911869773728117674E-16 ) ) ;
#84228 = CARTESIAN_POINT ( 'NONE',  ( 20.94999999999999574, 74.83729825007388570, -95.02310748452431710 ) ) ;
#84229 = CARTESIAN_POINT ( 'NONE',  ( 18.50000000000000355, 78.21986117685452200, -231.3317312752311068 ) ) ;
#84230 = ADVANCED_FACE ( 'NONE', ( #58422 ), #79530, .T. ) ;
#84231 = CIRCLE ( 'NONE', #171820, 0.2000000000000057288 ) ;
#84232 = CARTESIAN_POINT ( 'NONE',  ( 18.50000000000000000, 85.50000000001244871, -181.7731074845243029 ) ) ;
#84233 = DIRECTION ( 'NONE',  ( -0.8660254037844884456, -0.1064004976131806557, 0.4885477807825773788 ) ) ;
#84234 = LINE ( 'NONE', #62172, #246597 ) ;
#84235 = DIRECTION ( 'NONE',  ( 0.000000000000000000, 0.000000000000000000, 1.000000000000000000 ) ) ;
#84236 = EDGE_CURVE ( 'NONE', #117799, #60665, #196664, .T. ) ;
#84237 = ORIENTED_EDGE ( 'NONE', *, *, #61772, .T. ) ;
#84238 = CARTESIAN_POINT ( 'NONE',  ( 18.59999999999999432, 74.83729825007408465, -128.4231074845243086 ) ) ;
#84239 = CARTESIAN_POINT ( 'NONE',  ( 18.59999999999999076, 69.35000000001222986, -148.6731074845243938 ) ) ;
#84240 = PLANE ( 'NONE',  #84028 ) ;
#84241 = CARTESIAN_POINT ( 'NONE',  ( 20.73486653747088226, 9.775875410973629442, -211.8174516384118533 ) ) ;
#84242 = AXIS2_PLACEMENT_3D ( 'NONE', #49035, #9908, #69914 ) ;
#84243 = CARTESIAN_POINT ( 'NONE',  ( 18.39999999999998082, 64.52683809664983983, -160.7731074845244450 ) ) ;
#84244 = AXIS2_PLACEMENT_3D ( 'NONE', #89806, #208509, #130215 ) ;
#84245 = AXIS2_PLACEMENT_3D ( 'NONE', #84202, #208086, #206784 ) ;
#84246 = ORIENTED_EDGE ( 'NONE', *, *, #170074, .F. ) ;
#84247 = ORIENTED_EDGE ( 'NONE', *, *, #35369, .F. ) ;
#84248 = CARTESIAN_POINT ( 'NONE',  ( 20.99999999999998934, 1.212568896937007645, -7.900000000000000355 ) ) ;
#84249 = CYLINDRICAL_SURFACE ( 'NONE', #84388, 0.1000000000000024342 ) ;
#84250 = EDGE_CURVE ( 'NONE', #79944, #248319, #158700, .T. ) ;
#84251 = DIRECTION ( 'NONE',  ( 0.000000000000000000, 7.109473446599835262E-15, -1.000000000000000000 ) ) ;
#84252 = CARTESIAN_POINT ( 'NONE',  ( -16.89020380669787968, 23.07274987706156111, -230.9857821902007231 ) ) ;
#84253 = ADVANCED_FACE ( 'NONE', ( #157597 ), #37626, .F. ) ;
#84254 = ORIENTED_EDGE ( 'NONE', *, *, #17272, .F. ) ;
#84255 = DIRECTION ( 'NONE',  ( 2.952720810173289112E-16, -1.000000000000000000, -0.000000000000000000 ) ) ;
#84256 = ADVANCED_FACE ( 'NONE', ( #217501 ), #176618, .T. ) ;
#84257 = DIRECTION ( 'NONE',  ( 1.000000000000000000, 0.000000000000000000, 0.000000000000000000 ) ) ;
#84258 = DIRECTION ( 'NONE',  ( 1.000000000000000000, -0.000000000000000000, -0.000000000000000000 ) ) ;
#84259 = EDGE_CURVE ( 'NONE', #253379, #201937, #66894, .T. ) ;
#84260 = CARTESIAN_POINT ( 'NONE',  ( -16.94275863009466576, 9.989496048662386940, -12.60830261795888241 ) ) ;
#84261 = CIRCLE ( 'NONE', #38354, 0.09999999999998898659 ) ;
#84262 = EDGE_CURVE ( 'NONE', #252467, #171058, #187728, .T. ) ;
#84263 = ORIENTED_EDGE ( 'NONE', *, *, #181360, .T. ) ;
#84264 = DIRECTION ( 'NONE',  ( 0.000000000000000000, 0.000000000000000000, 1.000000000000000000 ) ) ;
#84265 = VECTOR ( 'NONE', #195947, 1000.000000000000000 ) ;
#84266 = EDGE_LOOP ( 'NONE', ( #223154, #199899, #150961, #130763 ) ) ;
#84267 = DIRECTION ( 'NONE',  ( 0.000000000000000000, 0.000000000000000000, -1.000000000000000000 ) ) ;
#84268 = DIRECTION ( 'NONE',  ( 0.000000000000000000, 1.000000000000000000, 0.000000000000000000 ) ) ;
#84269 = PLANE ( 'NONE',  #211805 ) ;
#84270 = FACE_OUTER_BOUND ( 'NONE', #77168, .T. ) ;
#84271 = PLANE ( 'NONE',  #93684 ) ;
#84272 = CARTESIAN_POINT ( 'NONE',  ( -18.46946985241261174, -9.509317228711573478, -6.986662565499634603 ) ) ;
#84273 = FACE_OUTER_BOUND ( 'NONE', #242923, .T. ) ;
#84274 = EDGE_CURVE ( 'NONE', #4548, #17499, #40200, .T. ) ;
#84275 = DIRECTION ( 'NONE',  ( -0.000000000000000000, 0.8660254037844502539, 0.4999999999999799050 ) ) ;
#84276 = CARTESIAN_POINT ( 'NONE',  ( -20.00857864376270001, 9.150000000011157653, -155.2500000000000284 ) ) ;
#84277 = LINE ( 'NONE', #64767, #156546 ) ;
#84278 = CARTESIAN_POINT ( 'NONE',  ( 21.05000000000000071, 32.73471231533727632, -251.3091613769917103 ) ) ;
#84279 = DIRECTION ( 'NONE',  ( -1.000000000000000000, 8.623019343401623015E-17, 8.389849937938898203E-16 ) ) ;
#84280 = CARTESIAN_POINT ( 'NONE',  ( 23.14999999999999858, 76.00000000001170974, -69.52310748452431710 ) ) ;
#84281 = AXIS2_PLACEMENT_3D ( 'NONE', #95834, #155857, #175426 ) ;
#84282 = ORIENTED_EDGE ( 'NONE', *, *, #41744, .T. ) ;
#84283 = CARTESIAN_POINT ( 'NONE',  ( -21.64999999999999858, 9.350000000011133849, -46.15000000000000568 ) ) ;
#84284 = DIRECTION ( 'NONE',  ( 0.000000000000000000, 1.000000000000000000, 0.000000000000000000 ) ) ;
#84285 = ORIENTED_EDGE ( 'NONE', *, *, #183240, .F. ) ;
#84286 = CARTESIAN_POINT ( 'NONE',  ( -18.50000000000000000, 77.16412189325258453, -28.10825939895270764 ) ) ;
#84287 = CYLINDRICAL_SURFACE ( 'NONE', #164914, 12.87499999999999822 ) ;
#84288 = DIRECTION ( 'NONE',  ( -0.000000000000000000, -1.000000000000000000, -7.272083257015735086E-15 ) ) ;
#84289 = VERTEX_POINT ( 'NONE', #174611 ) ;
#84290 = DIRECTION ( 'NONE',  ( 0.000000000000000000, -0.1350103645451557199, -0.9908441862701644620 ) ) ;
#84291 = CARTESIAN_POINT ( 'NONE',  ( 22.50014994443965222, 31.77938584363926466, -238.8622469772242596 ) ) ;
#84292 = VECTOR ( 'NONE', #63438, 1000.000000000000227 ) ;
#84293 = ORIENTED_EDGE ( 'NONE', *, *, #255652, .T. ) ;
#84294 = AXIS2_PLACEMENT_3D ( 'NONE', #183800, #23478, #104239 ) ;
#84295 = EDGE_CURVE ( 'NONE', #127544, #246315, #179347, .T. ) ;
#84296 = ORIENTED_EDGE ( 'NONE', *, *, #54612, .F. ) ;
#84297 = CARTESIAN_POINT ( 'NONE',  ( -21.05000000000000426, 76.10000000001200249, -109.5001745056490563 ) ) ;
#84298 = VECTOR ( 'NONE', #235607, 1000.000000000000000 ) ;
#84299 =( BOUNDED_SURFACE ( )  B_SPLINE_SURFACE ( 3, 2, ( 
 ( #164344, #123935, #104331 ),
 ( #43105, #45669, #108215 ),
 ( #241315, #206028, #24854 ),
 ( #67793, #28719, #3970 ) ),
 .UNSPECIFIED., .F., .F., .F. ) 
 B_SPLINE_SURFACE_WITH_KNOTS ( ( 4, 4 ),
 ( 3, 3 ),
 ( 0.0002700421466196637442, 0.0004789321604330607179 ),
 ( 0.000000000000000000, 1.000000000000000000 ),
 .UNSPECIFIED. ) 
 GEOMETRIC_REPRESENTATION_ITEM ( )  RATIONAL_B_SPLINE_SURFACE ( (
 ( 1.000000000000000000, 0.7071067811865475727, 1.000000000000000000),
 ( 1.000000000000000000, 0.7163411249511738577, 1.000000000000000000),
 ( 1.000000000000000000, 0.7221957104842052777, 1.000000000000000000),
 ( 1.000000000000000000, 0.7250110520819876836, 1.000000000000000000) ) ) 
 REPRESENTATION_ITEM ( '' )  SURFACE ( )  );
#84300 = ORIENTED_EDGE ( 'NONE', *, *, #171145, .F. ) ;
#84301 = DIRECTION ( 'NONE',  ( -1.000000000000000000, 0.000000000000000000, 0.000000000000000000 ) ) ;
#84302 = EDGE_CURVE ( 'NONE', #30925, #184847, #236983, .T. ) ;
#84304 = ADVANCED_FACE ( 'NONE', ( #55850 ), #156303, .T. ) ;
#84303 = CARTESIAN_POINT ( 'NONE',  ( 18.49999999999999289, 11.65000000000000391, -24.85000000000000142 ) ) ;
#84305 = CARTESIAN_POINT ( 'NONE',  ( -23.15000000000000213, 74.00000000001180922, -82.74772940728641402 ) ) ;
#84307 = DIRECTION ( 'NONE',  ( -3.265361837132813093E-16, -1.000000000000000000, -6.982962677686266711E-15 ) ) ;
#84306 = PRODUCT_DEFINITION_CONTEXT ( 'detailed design', #10884, 'design' ) ;
#84308 = FACE_OUTER_BOUND ( 'NONE', #242567, .T. ) ;
#84309 = CARTESIAN_POINT ( 'NONE',  ( 18.39999999999999503, 64.25000000001153921, -48.67310748452440805 ) ) ;
#84310 = DIRECTION ( 'NONE',  ( -1.000000000000000000, 0.000000000000000000, 0.000000000000000000 ) ) ;
#84311 = AXIS2_PLACEMENT_3D ( 'NONE', #84116, #65898, #48898 ) ;
#84312 = EDGE_CURVE ( 'NONE', #190582, #61048, #183606, .T. ) ;
#84313 = DIRECTION ( 'NONE',  ( -0.000000000000000000, -6.982962677686266711E-15, 1.000000000000000000 ) ) ;
#84315 = DIRECTION ( 'NONE',  ( -1.000000000000000000, -0.000000000000000000, -0.000000000000000000 ) ) ;
#84314 = CIRCLE ( 'NONE', #76010, 7.899999999999990585 ) ;
#84316 = EDGE_CURVE ( 'NONE', #12552, #75515, #221350, .T. ) ;
#84318 = VERTEX_POINT ( 'NONE', #162696 ) ;
#84317 = CARTESIAN_POINT ( 'NONE',  ( -18.51555513499624439, -9.352657054493677791, -40.69516989569750365 ) ) ;
#84319 = EDGE_LOOP ( 'NONE', ( #27143, #159981, #186659, #146655 ) ) ;
#84321 = DIRECTION ( 'NONE',  ( 1.000000000000000000, 0.000000000000000000, 0.000000000000000000 ) ) ;
#84320 = DIRECTION ( 'NONE',  ( -1.836970198721029934E-16, -1.000000000000000000, -6.982962677686266711E-15 ) ) ;
#84323 = EDGE_LOOP ( 'NONE', ( #225872, #17958, #30009 ) ) ;
#84322 = CARTESIAN_POINT ( 'NONE',  ( -18.59999999999999787, 1.115600667400684642E-11, -100.5000000000000426 ) ) ;
#84324 = EDGE_CURVE ( 'NONE', #31772, #118151, #41977, .T. ) ;
#84325 = VERTEX_POINT ( 'NONE', #200525 ) ;
#84326 = CARTESIAN_POINT ( 'NONE',  ( 21.05000000000000071, 76.00000000001190870, -103.0231074845243029 ) ) ;
#84327 = EDGE_CURVE ( 'NONE', #191177, #142271, #92016, .T. ) ;
#84328 = DIRECTION ( 'NONE',  ( -0.000000000000000000, 0.1298341882519668811, 0.9915357197604899309 ) ) ;
#84330 = EDGE_CURVE ( 'NONE', #252130, #53966, #254317, .T. ) ;
#84329 = LINE ( 'NONE', #7406, #79967 ) ;
#84331 = CIRCLE ( 'NONE', #230128, 0.09999999999998898659 ) ;
#84332 = CARTESIAN_POINT ( 'NONE',  ( 20.46382478191414833, 8.901379558713770734, -109.0457280948831453 ) ) ;
#84333 = DIRECTION ( 'NONE',  ( 1.000000000000000000, 0.000000000000000000, 0.000000000000000000 ) ) ;
#84334 = FACE_OUTER_BOUND ( 'NONE', #92610, .T. ) ;
#84335 = CIRCLE ( 'NONE', #34527, 4.150000000000001243 ) ;
#84336 = AXIS2_PLACEMENT_3D ( 'NONE', #209482, #229060, #30881 ) ;
#84337 = VECTOR ( 'NONE', #99382, 1000.000000000000000 ) ;
#84339 = AXIS2_PLACEMENT_3D ( 'NONE', #186193, #166658, #149649 ) ;
#84338 = DIRECTION ( 'NONE',  ( 0.000000000000000000, -1.000000000000000000, 0.000000000000000000 ) ) ;
#84340 = ORIENTED_EDGE ( 'NONE', *, *, #89081, .T. ) ;
#84341 = VERTEX_POINT ( 'NONE', #25743 ) ;
#84342 = LINE ( 'NONE', #103933, #85580 ) ;
#84343 = ORIENTED_EDGE ( 'NONE', *, *, #202580, .T. ) ;
#84344 = DIRECTION ( 'NONE',  ( 0.000000000000000000, 0.2617529984164856383, 0.9651348961777204138 ) ) ;
#84345 = ORIENTED_EDGE ( 'NONE', *, *, #127709, .F. ) ;
#84346 = CARTESIAN_POINT ( 'NONE',  ( 18.59999999999999076, 36.65892442174935439, -249.5511627012433848 ) ) ;
#84347 = EDGE_CURVE ( 'NONE', #140862, #256921, #125352, .T. ) ;
#84348 = CARTESIAN_POINT ( 'NONE',  ( 21.05000000000000071, 5.000000000011153745, -121.9947339810869380 ) ) ;
#84349 = ADVANCED_FACE ( 'NONE', ( #222632 ), #81822, .T. ) ;
#84350 = CARTESIAN_POINT ( 'NONE',  ( -21.09316766718153247, 75.96073659769805886, -209.8932607969990727 ) ) ;
#84351 = ORIENTED_EDGE ( 'NONE', *, *, #3406, .F. ) ;
#84352 = EDGE_CURVE ( 'NONE', #247600, #140944, #54426, .T. ) ;
#84353 = CARTESIAN_POINT ( 'NONE',  ( -20.95613430942416144, 11.75000000000000000, -6.857162648220172407 ) ) ;
#84354 = VERTEX_POINT ( 'NONE', #182257 ) ;
#84355 = DIRECTION ( 'NONE',  ( -1.000000000000000000, 0.000000000000000000, -0.000000000000000000 ) ) ;
#84356 = LINE ( 'NONE', #140523, #226989 ) ;
#84357 = CARTESIAN_POINT ( 'NONE',  ( 20.85000000000000142, 6.846123162363745074, -137.7377262668498759 ) ) ;
#84358 = SPHERICAL_SURFACE ( 'NONE', #223846, 0.1000000000000000056 ) ;
#84359 = EDGE_LOOP ( 'NONE', ( #197198, #3236, #42159, #70418, #178170, #163769, #147649, #163344, #98412, #92695, #101119 ) ) ;
#84360 = VECTOR ( 'NONE', #90461, 1000.000000000000000 ) ;
#84361 = CARTESIAN_POINT ( 'NONE',  ( -22.94999999999999929, 11.61130914238355771, -1.800000000000000044 ) ) ;
#84362 = ORIENTED_EDGE ( 'NONE', *, *, #76829, .F. ) ;
#84365 = ORIENTED_EDGE ( 'NONE', *, *, #93076, .F. ) ;
#84364 = DIRECTION ( 'NONE',  ( 0.000000000000000000, 0.000000000000000000, 1.000000000000000000 ) ) ;
#84363 = CARTESIAN_POINT ( 'NONE',  ( 18.46082813848040161, 47.00025378330893489, -255.3070137009749772 ) ) ;
#84366 = VECTOR ( 'NONE', #234618, 1000.000000000000000 ) ;
#84367 = CARTESIAN_POINT ( 'NONE',  ( -18.59999999999999787, 64.35000000001190301, -96.00830171387039513 ) ) ;
#84368 = VERTEX_POINT ( 'NONE', #4858 ) ;
#84369 = CARTESIAN_POINT ( 'NONE',  ( -23.25000000000000000, 28.37802281961254636, -258.4449340416662722 ) ) ;
#84370 = EDGE_LOOP ( 'NONE', ( #152372, #233962, #227155, #218425, #88281, #131534, #207469, #230637, #32579, #32482, #188529, #196705, #53406, #88708 ) ) ;
#84371 = CARTESIAN_POINT ( 'NONE',  ( 22.47007471830798053, 76.00000000001219291, -144.2438181364507841 ) ) ;
#84372 = AXIS2_PLACEMENT_3D ( 'NONE', #86702, #65883, #247072 ) ;
#84373 = DIRECTION ( 'NONE',  ( 0.000000000000000000, -7.056502275159890043E-15, 1.000000000000000000 ) ) ;
#84374 = DIRECTION ( 'NONE',  ( 0.000000000000000000, 0.000000000000000000, -1.000000000000000000 ) ) ;
#84375 =( BOUNDED_CURVE ( )  B_SPLINE_CURVE ( 3, ( #68892, #66310, #49305, #10197 ),
 .UNSPECIFIED., .F., .F. ) 
 B_SPLINE_CURVE_WITH_KNOTS ( ( 4, 4 ),
 ( 0.3000847527772395051, 0.5517402753107892854 ),
 .UNSPECIFIED. ) 
 CURVE ( )  GEOMETRIC_REPRESENTATION_ITEM ( )  RATIONAL_B_SPLINE_CURVE ( ( 1.000000000000000000, 0.9947294176030464508, 0.9947294176030464508, 1.000000000000000000 ) ) 
 REPRESENTATION_ITEM ( '' )  );
#84376 = CARTESIAN_POINT ( 'NONE',  ( -18.54118089899633048, 8.873505991743348531, -245.4030529781414884 ) ) ;
#84377 = AXIS2_PLACEMENT_3D ( 'NONE', #65992, #124695, #84212 ) ;
#84378 = DIRECTION ( 'NONE',  ( 1.000000000000000000, 0.000000000000000000, 0.000000000000000000 ) ) ;
#84379 = AXIS2_PLACEMENT_3D ( 'NONE', #204370, #25748, #105231 ) ;
#84380 = ORIENTED_EDGE ( 'NONE', *, *, #99395, .F. ) ;
#84381 = AXIS2_PLACEMENT_3D ( 'NONE', #97594, #115920, #179748 ) ;
#84382 = AXIS2_PLACEMENT_3D ( 'NONE', #216308, #117225, #13013 ) ;
#84383 = DIRECTION ( 'NONE',  ( 0.000000000000000000, 0.8855159391400492241, -0.4646089985449236570 ) ) ;
#84384 = DIRECTION ( 'NONE',  ( -0.000000000000000000, 1.000000000000000000, -0.000000000000000000 ) ) ;
#84385 = CARTESIAN_POINT ( 'NONE',  ( -18.37151313414693732, -9.571014125767270286, -140.8166629092384596 ) ) ;
#84386 = ORIENTED_EDGE ( 'NONE', *, *, #238929, .T. ) ;
#84387 = CARTESIAN_POINT ( 'NONE',  ( 23.14999999999999858, 0.000000000000000000, -33.50000000000000000 ) ) ;
#84389 = VERTEX_POINT ( 'NONE', #66148 ) ;
#84388 = AXIS2_PLACEMENT_3D ( 'NONE', #225076, #45179, #148135 ) ;
#84390 = DIRECTION ( 'NONE',  ( 0.000000000000000000, 7.086529944415894657E-15, -1.000000000000000000 ) ) ;
#84391 = AXIS2_PLACEMENT_3D ( 'NONE', #135381, #36317, #92410 ) ;
#84392 = DIRECTION ( 'NONE',  ( -1.000000000000000000, -0.000000000000000000, -0.000000000000000000 ) ) ;
#84393 = CARTESIAN_POINT ( 'NONE',  ( -20.94999999999999929, -11.29603075033528548, -3.047899159663867152 ) ) ;
#84395 = VERTEX_POINT ( 'NONE', #204365 ) ;
#84394 = CARTESIAN_POINT ( 'NONE',  ( -16.89268316805466341, 9.951721813253341153, -146.6442475214544743 ) ) ;
#84396 = CARTESIAN_POINT ( 'NONE',  ( 20.12500000000000000, 11.25287472715600146, -206.8511660127314826 ) ) ;
#84397 = AXIS2_PLACEMENT_3D ( 'NONE', #133638, #80044, #20124 ) ;
#84398 = DIRECTION ( 'NONE',  ( 0.000000000000000000, -0.2128009952263361926, 0.9770955615653368342 ) ) ;
#84399 = AXIS2_PLACEMENT_3D ( 'NONE', #140739, #255500, #179886 ) ;
#84400 = EDGE_CURVE ( 'NONE', #135784, #195479, #105224, .T. ) ;
#84401 = CARTESIAN_POINT ( 'NONE',  ( -17.11825945287481332, 65.95000000001255103, -182.6731074845244223 ) ) ;
#84402 = ORIENTED_EDGE ( 'NONE', *, *, #99074, .T. ) ;
#84403 = AXIS2_PLACEMENT_3D ( 'NONE', #125817, #187111, #91840 ) ;
#84404 = DIRECTION ( 'NONE',  ( -1.000000000000000000, -0.000000000000000000, -0.000000000000000000 ) ) ;
#84406 = ADVANCED_FACE ( 'NONE', ( #101371 ), #140536, .T. ) ;
#84405 = DIRECTION ( 'NONE',  ( -1.000000000000000000, -0.000000000000000000, 0.000000000000000000 ) ) ;
#84407 = ORIENTED_EDGE ( 'NONE', *, *, #223611, .T. ) ;
#84408 = CARTESIAN_POINT ( 'NONE',  ( 22.50000000000000000, 55.96169194136206215, -232.9023299069559130 ) ) ;
#84409 = VECTOR ( 'NONE', #39265, 1000.000000000000000 ) ;
#84410 = ORIENTED_EDGE ( 'NONE', *, *, #129387, .F. ) ;
#84412 =( BOUNDED_SURFACE ( )  B_SPLINE_SURFACE ( 3, 2, ( 
 ( #231655, #34748, #109108 ),
 ( #132541, #193799, #114257 ),
 ( #154697, #33481, #252466 ),
 ( #192514, #253751, #75162 ),
 ( #169136, #55525, #1992 ),
 ( #97210, #37307, #116827 ) ),
 .UNSPECIFIED., .F., .F., .F. ) 
 B_SPLINE_SURFACE_WITH_KNOTS ( ( 4, 2, 4 ),
 ( 3, 3 ),
 ( 1.570796326794897668, 2.356194490192346169, 3.141592653589794448 ),
 ( 0.000000000000000000, 1.000000000000000000 ),
 .UNSPECIFIED. ) 
 GEOMETRIC_REPRESENTATION_ITEM ( )  RATIONAL_B_SPLINE_SURFACE ( (
 ( 1.000000000000000000, 0.7071067811865597852, 1.000000000000000000),
 ( 1.000000000000000000, 0.6611148371776831567, 1.000000000000000000),
 ( 1.000000000000000000, 0.6092287576699134677, 1.000000000000000000),
 ( 1.000000000000000000, 0.5278258667055114595, 1.000000000000000000),
 ( 1.000000000000000000, 0.4993418825336375932, 1.000000000000000000),
 ( 1.000000000000000000, 0.4999999999999704681, 1.000000000000000000) ) ) 
 REPRESENTATION_ITEM ( '' )  SURFACE ( )  );
#84411 = CIRCLE ( 'NONE', #155247, 0.1000000000000028644 ) ;
#84413 = AXIS2_PLACEMENT_3D ( 'NONE', #18358, #125171, #88579 ) ;
#84414 = EDGE_CURVE ( 'NONE', #37010, #77399, #108590, .T. ) ;
#84415 = LINE ( 'NONE', #164014, #183390 ) ;
#84416 = PRESENTATION_LAYER_ASSIGNMENT (  '', '', ( #22518 ) ) ;
#84419 = ADVANCED_FACE ( 'NONE', ( #3600 ), #80545, .T. ) ;
#84418 = ORIENTED_EDGE ( 'NONE', *, *, #48926, .F. ) ;
#84417 = DIRECTION ( 'NONE',  ( -0.000000000000000000, -0.2128009952263604232, 0.9770955615653316162 ) ) ;
#84422 = ORIENTED_EDGE ( 'NONE', *, *, #98194, .F. ) ;
#84421 = ORIENTED_EDGE ( 'NONE', *, *, #89125, .F. ) ;
#84420 = DIRECTION ( 'NONE',  ( -0.000000000000000000, -0.2605042016806452532, -0.9654727137038777718 ) ) ;
#84423 = CARTESIAN_POINT ( 'NONE',  ( -18.50000000000000000, 66.75000000001253397, -182.1731074845244223 ) ) ;
#84424 = DIRECTION ( 'NONE',  ( 2.827886303505249259E-16, 0.8660254037844377084, 0.5000000000000016653 ) ) ;
#84425 = DIRECTION ( 'NONE',  ( 1.000000000000000000, 0.000000000000000000, 0.000000000000000000 ) ) ;
#84427 = DIRECTION ( 'NONE',  ( 1.000000000000000000, 1.794895427898103559E-16, 3.909090864890002444E-17 ) ) ;
#84426 = DIRECTION ( 'NONE',  ( 0.000000000000000000, 0.000000000000000000, -1.000000000000000000 ) ) ;
#84428 = DIRECTION ( 'NONE',  ( 0.000000000000000000, 6.982962677686266711E-15, -1.000000000000000000 ) ) ;
#84429 = TOROIDAL_SURFACE ( 'NONE', #92853, 0.2000000000000000111, 0.1000000000000000056 ) ;
#84430 = CARTESIAN_POINT ( 'NONE',  ( -16.94445028196808778, 44.07934375239701552, -235.2779890399608576 ) ) ;
#84431 = AXIS2_PLACEMENT_3D ( 'NONE', #122225, #120963, #124794 ) ;
#84432 = DIRECTION ( 'NONE',  ( -0.000000000000000000, -1.000000000000000000, -0.000000000000000000 ) ) ;
#84433 = EDGE_CURVE ( 'NONE', #185664, #43467, #251, .T. ) ;
#84434 = LINE ( 'NONE', #106592, #218177 ) ;
#84435 = ADVANCED_FACE ( 'NONE', ( #143102 ), #62804, .F. ) ;
#84436 = VERTEX_POINT ( 'NONE', #239660 ) ;
#84437 = ORIENTED_EDGE ( 'NONE', *, *, #245045, .F. ) ;
#84438 = PLANE ( 'NONE',  #170984 ) ;
#84440 = ORIENTED_EDGE ( 'NONE', *, *, #182122, .F. ) ;
#84439 = DIRECTION ( 'NONE',  ( 0.000000000000000000, 0.000000000000000000, -1.000000000000000000 ) ) ;
#84441 = EDGE_LOOP ( 'NONE', ( #12980, #110301, #103793, #14228 ) ) ;
#84442 = DIRECTION ( 'NONE',  ( 0.000000000000000000, -0.1455152366551721865, -0.9893560106964475187 ) ) ;
#84443 = ORIENTED_EDGE ( 'NONE', *, *, #8178, .T. ) ;
#84444 = CARTESIAN_POINT ( 'NONE',  ( -21.05000000000000071, 69.45934304831089889, -136.4231074845243654 ) ) ;
#84445 = EDGE_CURVE ( 'NONE', #154130, #116413, #104469, .T. ) ;
#84446 = ORIENTED_EDGE ( 'NONE', *, *, #2605, .T. ) ;
#84447 = CARTESIAN_POINT ( 'NONE',  ( 23.40000000000005187, 84.00000000001119815, -37.18565239344504647 ) ) ;
#84448 = DIRECTION ( 'NONE',  ( -0.000000000000000000, -0.000000000000000000, -1.000000000000000000 ) ) ;
#84449 = EDGE_CURVE ( 'NONE', #111732, #185160, #61005, .T. ) ;
#84450 = CIRCLE ( 'NONE', #230244, 1.749999999999998002 ) ;
#84452 = VERTEX_POINT ( 'NONE', #175242 ) ;
#84451 = EDGE_LOOP ( 'NONE', ( #120814, #172486, #127411, #216724, #165628, #86091, #127114 ) ) ;
#84453 = ORIENTED_EDGE ( 'NONE', *, *, #98074, .F. ) ;
#84454 = DIRECTION ( 'NONE',  ( 0.000000000000000000, -0.9770955615653307280, -0.2128009952263641702 ) ) ;
#84455 = ORIENTED_EDGE ( 'NONE', *, *, #86411, .F. ) ;
#84456 = ORIENTED_EDGE ( 'NONE', *, *, #27177, .T. ) ;
#84457 = DIRECTION ( 'NONE',  ( -0.000000000000000000, 0.000000000000000000, 1.000000000000000000 ) ) ;
#84458 = CARTESIAN_POINT ( 'NONE',  ( -20.94999999999999929, -1.261786168553869603, -108.5864989635455089 ) ) ;
#84459 = AXIS2_PLACEMENT_3D ( 'NONE', #50038, #128308, #51293 ) ;
#84461 = ORIENTED_EDGE ( 'NONE', *, *, #234307, .T. ) ;
#84460 = DIRECTION ( 'NONE',  ( -1.000000000000000000, 2.952720810173289112E-16, 2.061873921506763405E-30 ) ) ;
#84462 = EDGE_CURVE ( 'NONE', #55215, #206656, #89548, .T. ) ;
#84463 = LINE ( 'NONE', #222726, #149251 ) ;
#84465 = VERTEX_POINT ( 'NONE', #46567 ) ;
#84464 = PLANE ( 'NONE',  #218973 ) ;
#84466 = CARTESIAN_POINT ( 'NONE',  ( -17.29838795458774570, 10.37154985796137296, -178.8952587173804716 ) ) ;
#84467 = ORIENTED_EDGE ( 'NONE', *, *, #72276, .F. ) ;
#84468 = SPHERICAL_SURFACE ( 'NONE', #220180, 0.1000000000000000056 ) ;
#84469 = ADVANCED_FACE ( 'NONE', ( #194785 ), #71310, .F. ) ;
#84470 = ORIENTED_EDGE ( 'NONE', *, *, #194505, .T. ) ;
#84471 = CARTESIAN_POINT ( 'NONE',  ( -23.15000000000000213, 36.65892442174935439, -249.5511627012433848 ) ) ;
#84472 = CARTESIAN_POINT ( 'NONE',  ( 20.94999999999999929, 76.00000000001126921, -203.5231074845248997 ) ) ;
#84474 = ADVANCED_FACE ( 'NONE', ( #128704 ), #233885, .F. ) ;
#84473 = ORIENTED_EDGE ( 'NONE', *, *, #69742, .T. ) ;
#84475 = CARTESIAN_POINT ( 'NONE',  ( 22.47071067811865319, 0.09909245471376171288, -25.77992525550195424 ) ) ;
#84476 = AXIS2_PLACEMENT_3D ( 'NONE', #257145, #58965, #255866 ) ;
#84477 = CARTESIAN_POINT ( 'NONE',  ( -23.25000000000000000, -11.74999999998884448, -134.0000000000000000 ) ) ;
#84478 = DIRECTION ( 'NONE',  ( -1.000000000000000000, 2.952720810173289112E-16, 2.061873921506763405E-30 ) ) ;
#84479 = ORIENTED_EDGE ( 'NONE', *, *, #59936, .T. ) ;
#84480 = VERTEX_POINT ( 'NONE', #208245 ) ;
#84481 = DIRECTION ( 'NONE',  ( 1.000000000000000000, 0.000000000000000000, 0.000000000000000000 ) ) ;
#84482 = FACE_OUTER_BOUND ( 'NONE', #47637, .T. ) ;
#84483 = ORIENTED_EDGE ( 'NONE', *, *, #139837, .F. ) ;
#84484 = DIRECTION ( 'NONE',  ( 1.000000000000000000, 0.000000000000000000, 0.000000000000000000 ) ) ;
#84485 = ORIENTED_EDGE ( 'NONE', *, *, #19883, .T. ) ;
#84486 = EDGE_CURVE ( 'NONE', #167915, #45115, #25408, .T. ) ;
#84487 = CARTESIAN_POINT ( 'NONE',  ( -23.25000000000000000, -1.149570369564537842, -74.81591248450196474 ) ) ;
#84489 = CARTESIAN_POINT ( 'NONE',  ( -21.14999999999999858, 76.00000000001213607, -136.5231074845242745 ) ) ;
#84488 = LINE ( 'NONE', #167624, #198822 ) ;
#84490 = CARTESIAN_POINT ( 'NONE',  ( 22.50000000000000000, 0.1000000000111554016, -55.35042919245524473 ) ) ;
#84492 = ADVANCED_FACE ( 'NONE', ( #247345 ), #146948, .F. ) ;
#84491 = CARTESIAN_POINT ( 'NONE',  ( -16.87036670365548474, 66.01058118071016168, -82.04354736722233099 ) ) ;
#84493 = ORIENTED_EDGE ( 'NONE', *, *, #43314, .T. ) ;
#84494 = AXIS2_PLACEMENT_3D ( 'NONE', #171572, #210663, #211964 ) ;
#84495 = CARTESIAN_POINT ( 'NONE',  ( 20.85000000000000142, 56.27731819600170837, -227.9967441372480437 ) ) ;
#84496 = VECTOR ( 'NONE', #190227, 1000.000000000000000 ) ;
#84498 = ORIENTED_EDGE ( 'NONE', *, *, #201783, .T. ) ;
#84497 = ORIENTED_EDGE ( 'NONE', *, *, #82887, .F. ) ;
#84499 = EDGE_LOOP ( 'NONE', ( #192764, #59955, #104590 ) ) ;
#84500 = ORIENTED_EDGE ( 'NONE', *, *, #59638, .F. ) ;
#84501 = AXIS2_PLACEMENT_3D ( 'NONE', #72086, #173795, #8569 ) ;
#84502 = CARTESIAN_POINT ( 'NONE',  ( 21.53551880898956838, 6.784797761427480367, -33.40103026542833931 ) ) ;
#84503 = DIRECTION ( 'NONE',  ( -1.000000000000000000, 0.000000000000000000, 0.000000000000000000 ) ) ;
#84504 = FACE_BOUND ( 'NONE', #82183, .T. ) ;
#84505 = CARTESIAN_POINT ( 'NONE',  ( 20.85000000000000142, 77.83585931145600512, -158.4186683157258244 ) ) ;
#84506 = DIRECTION ( 'NONE',  ( 0.000000000000000000, -0.9908441862701782288, -0.1350103645450542456 ) ) ;
#84508 = DIRECTION ( 'NONE',  ( -1.000000000000000000, 3.265361837132813093E-16, 2.280189983783949500E-30 ) ) ;
#84507 = CARTESIAN_POINT ( 'NONE',  ( 21.53551880898956838, 69.21520223859533871, -69.62207721909604174 ) ) ;
#84510 = ORIENTED_EDGE ( 'NONE', *, *, #7788, .T. ) ;
#84509 = DIRECTION ( 'NONE',  ( 1.000000000000000000, -0.000000000000000000, -0.000000000000000000 ) ) ;
#84511 = LINE ( 'NONE', #66292, #216398 ) ;
#84512 = VERTEX_POINT ( 'NONE', #95647 ) ;
#84513 = CARTESIAN_POINT ( 'NONE',  ( -22.50000000000000000, 1.115600667400684642E-11, -155.8504291924551808 ) ) ;
#84514 = ORIENTED_EDGE ( 'NONE', *, *, #181856, .T. ) ;
#84515 = ORIENTED_EDGE ( 'NONE', *, *, #117544, .F. ) ;
#84516 = CARTESIAN_POINT ( 'NONE',  ( -23.15000000000000213, 24.87281074564535288, -251.9822168787707710 ) ) ;
#84518 = AXIS2_PLACEMENT_3D ( 'NONE', #201912, #104066, #140645 ) ;
#84517 = DIRECTION ( 'NONE',  ( 0.000000000000000000, 0.2617529984165031243, 0.9651348961777157509 ) ) ;
#84519 = CARTESIAN_POINT ( 'NONE',  ( -16.88705144915408596, 66.05000000001153637, -48.95408607923688038 ) ) ;
#84520 = CIRCLE ( 'NONE', #117867, 0.9000000000000014655 ) ;
#84521 = LINE ( 'NONE', #243644, #204132 ) ;
#84522 = AXIS2_PLACEMENT_3D ( 'NONE', #55434, #60593, #154605 ) ;
#84523 = DIRECTION ( 'NONE',  ( 0.000000000000000000, 6.982962677686266711E-15, -1.000000000000000000 ) ) ;
#84524 = ORIENTED_EDGE ( 'NONE', *, *, #52032, .F. ) ;
#84525 = ORIENTED_EDGE ( 'NONE', *, *, #41844, .F. ) ;
#84526 = AXIS2_PLACEMENT_3D ( 'NONE', #79061, #119520, #62103 ) ;
#84527 = DIRECTION ( 'NONE',  ( 1.000000000000000000, 0.000000000000000000, 0.000000000000000000 ) ) ;
#84528 = VERTEX_POINT ( 'NONE', #126103 ) ;
#84529 = CARTESIAN_POINT ( 'NONE',  ( -20.93284271247462058, 11.75000000001115019, -126.9851942293460922 ) ) ;
#84530 = DIRECTION ( 'NONE',  ( 1.000000000000000000, -2.952720810173289112E-16, -2.061873921506763405E-30 ) ) ;
#84531 = FACE_OUTER_BOUND ( 'NONE', #202693, .T. ) ;
#84532 = DIRECTION ( 'NONE',  ( 0.000000000000000000, 0.000000000000000000, 1.000000000000000000 ) ) ;
#84533 = DIRECTION ( 'NONE',  ( 0.000000000000000000, 0.000000000000000000, -1.000000000000000000 ) ) ;
#84534 = CARTESIAN_POINT ( 'NONE',  ( 21.70464131381650219, 7.095358018979006864, -67.00000000000004263 ) ) ;
#84535 = DIRECTION ( 'NONE',  ( 1.000000000000000000, 0.000000000000000000, 0.000000000000000000 ) ) ;
#84536 = AXIS2_PLACEMENT_3D ( 'NONE', #146494, #203918, #226017 ) ;
#84538 = DIRECTION ( 'NONE',  ( 0.000000000000000000, 0.000000000000000000, -1.000000000000000000 ) ) ;
#84537 = TOROIDAL_SURFACE ( 'NONE', #167813, 0.2000000000000000111, 0.1000000000000000056 ) ;
#84540 = CARTESIAN_POINT ( 'NONE',  ( -20.64999999999999858, 21.35054858842500281, -233.1262234518673893 ) ) ;
#84539 = AXIS2_PLACEMENT_3D ( 'NONE', #188906, #208490, #50651 ) ;
#84541 = CIRCLE ( 'NONE', #5454, 0.09999999999999939493 ) ;
#84542 = CARTESIAN_POINT ( 'NONE',  ( -21.04999999999999361, 6.134002965570138244, -199.5633345488312784 ) ) ;
#84544 = EDGE_CURVE ( 'NONE', #112231, #90455, #106535, .T. ) ;
#84543 = CARTESIAN_POINT ( 'NONE',  ( -20.85000000000000142, 77.85161776048025217, -24.41991776492064758 ) ) ;
#84545 = CARTESIAN_POINT ( 'NONE',  ( -20.15000000000000568, 52.16189642417536021, -232.4248417328940093 ) ) ;
#84546 = VERTEX_POINT ( 'NONE', #70025 ) ;
#84547 = CARTESIAN_POINT ( 'NONE',  ( -16.89208623190940273, 30.21172107852033406, -234.8081435470708982 ) ) ;
#84548 = ADVANCED_FACE ( 'NONE', ( #188658 ), #55213, .F. ) ;
#84549 = EDGE_LOOP ( 'NONE', ( #6913, #114779, #225236, #198748, #201467 ) ) ;
#84550 = CYLINDRICAL_SURFACE ( 'NONE', #220921, 0.1000000000000028644 ) ;
#84551 = DIRECTION ( 'NONE',  ( 0.000000000000000000, 0.000000000000000000, 1.000000000000000000 ) ) ;
#84553 = ADVANCED_FACE ( 'NONE', ( #155669 ), #150488, .T. ) ;
#84552 = CARTESIAN_POINT ( 'NONE',  ( 21.04999999999999716, 61.94813849985776244, -221.8062180090915376 ) ) ;
#84554 = ADVANCED_FACE ( 'NONE', ( #35716 ), #250423, .F. ) ;
#84555 = ORIENTED_EDGE ( 'NONE', *, *, #129643, .T. ) ;
#84556 = DIRECTION ( 'NONE',  ( 0.000000000000000000, 0.9964539953858966292, 0.08413937888696132461 ) ) ;
#84557 = VECTOR ( 'NONE', #61576, 1000.000000000000000 ) ;
#84558 = LINE ( 'NONE', #83295, #214610 ) ;
#84560 = AXIS2_PLACEMENT_3D ( 'NONE', #198704, #20083, #25226 ) ;
#84559 = DIRECTION ( 'NONE',  ( 0.000000000000000000, 0.2868887416115947775, -0.9579639084728169829 ) ) ;
#84561 = DIRECTION ( 'NONE',  ( -1.000000000000000000, -3.265361837132813093E-16, 0.000000000000000000 ) ) ;
#84562 = CARTESIAN_POINT ( 'NONE',  ( 22.49066049874202022, 75.94365674848023673, -181.6731197220414629 ) ) ;
#84563 = ORIENTED_EDGE ( 'NONE', *, *, #74206, .F. ) ;
#84564 = LINE ( 'NONE', #218983, #12415 ) ;
#84566 = ORIENTED_EDGE ( 'NONE', *, *, #155826, .T. ) ;
#84565 = CARTESIAN_POINT ( 'NONE',  ( -23.15000000000000213, 54.14029358995846763, -238.9803212882090691 ) ) ;
#84567 = DIRECTION ( 'NONE',  ( -1.000000000000000000, 0.000000000000000000, -0.000000000000000000 ) ) ;
#84568 = EDGE_CURVE ( 'NONE', #250305, #95482, #67086, .T. ) ;
#84569 = CARTESIAN_POINT ( 'NONE',  ( 18.49999999999999645, -1.866714910046153308, -145.7526752462820241 ) ) ;
#84570 = EDGE_LOOP ( 'NONE', ( #228977, #13571, #246524, #172775 ) ) ;
#84571 = CARTESIAN_POINT ( 'NONE',  ( -22.50000000000000000, 75.90736249940275115, -148.1728046915650339 ) ) ;
#84572 = VECTOR ( 'NONE', #189170, 1000.000000000000000 ) ;
#84573 = APPLICATION_PROTOCOL_DEFINITION ( 'draft international standard', 'automotive_design', 1998, #248882 ) ;
#84575 = CIRCLE ( 'NONE', #130412, 0.1999999999999987899 ) ;
#84574 = DIRECTION ( 'NONE',  ( -0.000000000000000000, 0.000000000000000000, -1.000000000000000000 ) ) ;
#84576 = ORIENTED_EDGE ( 'NONE', *, *, #176292, .F. ) ;
#84577 = VECTOR ( 'NONE', #98243, 1000.000000000000000 ) ;
#84578 = DIRECTION ( 'NONE',  ( 0.000000000000000000, 0.000000000000000000, 1.000000000000000000 ) ) ;
#84579 = CARTESIAN_POINT ( 'NONE',  ( 20.85000000000000142, 87.65000000001141700, -36.02310748452423894 ) ) ;
#84580 = TOROIDAL_SURFACE ( 'NONE', #183778, 2.100000000000002309, 0.1000000000000000056 ) ;
#84581 = PRODUCT_DEFINITION_SHAPE ( 'NONE', 'NONE',  #163264 ) ;
#84582 = AXIS2_PLACEMENT_3D ( 'NONE', #196336, #80208, #37291 ) ;
#84583 = LINE ( 'NONE', #62511, #141134 ) ;
#84584 = EDGE_CURVE ( 'NONE', #254207, #66328, #8819, .T. ) ;
#84585 = ORIENTED_EDGE ( 'NONE', *, *, #28727, .T. ) ;
#84586 = VERTEX_POINT ( 'NONE', #186102 ) ;
#84587 = DIRECTION ( 'NONE',  ( 1.000000000000000000, 0.000000000000000000, 0.000000000000000000 ) ) ;
#84588 = LINE ( 'NONE', #145883, #171535 ) ;
#84590 = VECTOR ( 'NONE', #14705, 1000.000000000000000 ) ;
#84589 = CARTESIAN_POINT ( 'NONE',  ( 20.94999999999999574, 76.00000000001165290, -69.52310748452431710 ) ) ;
#84592 = AXIS2_PLACEMENT_3D ( 'NONE', #202745, #140183, #219733 ) ;
#84591 = DIRECTION ( 'NONE',  ( -1.000000000000000000, 0.000000000000000000, -0.000000000000000000 ) ) ;
#84593 = DIRECTION ( 'NONE',  ( 0.000000000000000000, 0.2128009952263608395, -0.9770955615653315052 ) ) ;
#84594 = DIRECTION ( 'NONE',  ( 1.836970198721029934E-16, -1.000000000000000000, -0.000000000000000000 ) ) ;
#84595 = EDGE_CURVE ( 'NONE', #145620, #61360, #86965, .T. ) ;
#84597 = CARTESIAN_POINT ( 'NONE',  ( -18.45068461519105796, -9.486506529077932015, -74.06877716890477359 ) ) ;
#84596 = CARTESIAN_POINT ( 'NONE',  ( 20.94999999999999929, 70.15000000001235492, -159.8906102602464330 ) ) ;
#84598 = AXIS2_PLACEMENT_3D ( 'NONE', #90542, #247044, #170137 ) ;
#84599 = LINE ( 'NONE', #125070, #73726 ) ;
#84600 = LINE ( 'NONE', #160368, #239540 ) ;
#84601 = FACE_OUTER_BOUND ( 'NONE', #123851, .T. ) ;
#84602 = DIRECTION ( 'NONE',  ( -1.000000000000000000, -0.000000000000000000, -0.000000000000000000 ) ) ;
#84603 = ORIENTED_EDGE ( 'NONE', *, *, #136231, .F. ) ;
#84604 = ORIENTED_EDGE ( 'NONE', *, *, #36075, .F. ) ;
#84605 = CARTESIAN_POINT ( 'NONE',  ( -21.14999999999999858, 1.115600667400684642E-11, -26.95934304829875927 ) ) ;
#84606 = CIRCLE ( 'NONE', #9639, 0.1000000000000024342 ) ;
#84607 = CARTESIAN_POINT ( 'NONE',  ( 23.24999999999999645, 70.35000000001159037, -56.87310748452435405 ) ) ;
#84609 = FACE_OUTER_BOUND ( 'NONE', #256242, .T. ) ;
#84608 = CARTESIAN_POINT ( 'NONE',  ( -23.25000000000000000, 87.48912529308822172, -139.6231074845242688 ) ) ;
#84610 = VECTOR ( 'NONE', #177685, 1000.000000000000114 ) ;
#84611 = CIRCLE ( 'NONE', #180518, 11.74999999999999645 ) ;
#84612 = CIRCLE ( 'NONE', #167888, 4.049999999999998934 ) ;
#84613 = DIRECTION ( 'NONE',  ( 0.000000000000000000, 1.000000000000000000, 0.000000000000000000 ) ) ;
#84614 = FACE_OUTER_BOUND ( 'NONE', #31521, .T. ) ;
#84615 = LINE ( 'NONE', #68974, #206483 ) ;
#84616 = CARTESIAN_POINT ( 'NONE',  ( 22.59080734064468032, 11.75000000001115552, -66.96925029190298062 ) ) ;
#84617 = ORIENTED_EDGE ( 'NONE', *, *, #161599, .T. ) ;
#84618 = EDGE_CURVE ( 'NONE', #994, #159949, #187395, .T. ) ;
#84619 = CARTESIAN_POINT ( 'NONE',  ( -16.92570016628984320, 51.64205409960519688, -231.9264490580749225 ) ) ;
#84620 = VERTEX_POINT ( 'NONE', #11312 ) ;
#84621 = CARTESIAN_POINT ( 'NONE',  ( -20.64999999999999858, 76.00000000001155342, -56.64810748452432421 ) ) ;
#84622 = AXIS2_PLACEMENT_3D ( 'NONE', #250868, #45307, #123562 ) ;
#84623 = AXIS2_PLACEMENT_3D ( 'NONE', #254936, #60633, #43668 ) ;
#84624 = VECTOR ( 'NONE', #251176, 1000.000000000000114 ) ;
#84625 = AXIS2_PLACEMENT_3D ( 'NONE', #195155, #239395, #59424 ) ;
#84626 = DIRECTION ( 'NONE',  ( -1.000000000000000000, 0.000000000000000000, 0.000000000000000000 ) ) ;
#84627 = EDGE_CURVE ( 'NONE', #58091, #70573, #208752, .T. ) ;
#84628 = ADVANCED_FACE ( 'NONE', ( #239025 ), #77362, .T. ) ;
#84629 = ORIENTED_EDGE ( 'NONE', *, *, #31496, .F. ) ;
#84630 = CARTESIAN_POINT ( 'NONE',  ( -23.15000000000000213, 66.33592547490526670, -222.9197737850312251 ) ) ;
#84631 = ORIENTED_EDGE ( 'NONE', *, *, #199235, .T. ) ;
#84632 = ADVANCED_FACE ( 'NONE', ( #17406 ), #104640, .F. ) ;
#84634 = EDGE_CURVE ( 'NONE', #138502, #191355, #137332, .T. ) ;
#84633 = DIRECTION ( 'NONE',  ( 0.000000000000000000, 1.000000000000000000, -0.000000000000000000 ) ) ;
#84635 = CARTESIAN_POINT ( 'NONE',  ( -18.40000000000000213, 11.33174054713631662, -46.15000000000000568 ) ) ;
#84636 = CARTESIAN_POINT ( 'NONE',  ( -23.15000000000000213, 1.115600667400684642E-11, -67.00000000000000000 ) ) ;
#84637 = LINE ( 'NONE', #1276, #150040 ) ;
#84638 = LINE ( 'NONE', #243757, #164093 ) ;
#84639 = DIRECTION ( 'NONE',  ( 0.000000000000000000, -0.000000000000000000, 1.000000000000000000 ) ) ;
#84640 = EDGE_CURVE ( 'NONE', #163227, #89054, #220742, .T. ) ;
#84641 = DIRECTION ( 'NONE',  ( -3.265361837132813093E-16, -1.000000000000000000, -6.982962677686266711E-15 ) ) ;
#84642 = DIRECTION ( 'NONE',  ( 0.000000000000000000, 0.000000000000000000, -1.000000000000000000 ) ) ;
#84644 = ORIENTED_EDGE ( 'NONE', *, *, #56936, .T. ) ;
#84643 = DIRECTION ( 'NONE',  ( -0.000000000000000000, -0.9371753822965326330, 0.3488585713686107592 ) ) ;
#84646 = DIRECTION ( 'NONE',  ( -0.000000000000000000, 0.000000000000000000, 1.000000000000000000 ) ) ;
#84645 = CARTESIAN_POINT ( 'NONE',  ( 21.05000000000000071, -0.09999999999999939493, 6.540656951701244282 ) ) ;
#84647 = ORIENTED_EDGE ( 'NONE', *, *, #145128, .F. ) ;
#84649 = VERTEX_POINT ( 'NONE', #21289 ) ;
#84648 = CYLINDRICAL_SURFACE ( 'NONE', #210924, 0.1000000000000028644 ) ;
#84650 = EDGE_CURVE ( 'NONE', #182460, #90874, #62863, .T. ) ;
#84651 = ORIENTED_EDGE ( 'NONE', *, *, #134485, .F. ) ;
#84652 = CARTESIAN_POINT ( 'NONE',  ( 19.75857864376268935, 11.75000000001115907, -91.85000000000003695 ) ) ;
#84654 = ADVANCED_FACE ( 'NONE', ( #198603 ), #19994, .T. ) ;
#84653 = EDGE_CURVE ( 'NONE', #32681, #230513, #29691, .T. ) ;
#84655 = CYLINDRICAL_SURFACE ( 'NONE', #113412, 0.1000000000000000472 ) ;
#84656 = AXIS2_PLACEMENT_3D ( 'NONE', #104541, #43328, #122869 ) ;
#84657 = EDGE_LOOP ( 'NONE', ( #230503, #126562, #201477, #251312 ) ) ;
#84658 = DIRECTION ( 'NONE',  ( -1.000000000000000000, 0.000000000000000000, 0.000000000000000000 ) ) ;
#84659 = FACE_OUTER_BOUND ( 'NONE', #249990, .T. ) ;
#84660 = CARTESIAN_POINT ( 'NONE',  ( 20.85000000000000142, 11.75000000001115907, -93.71613433702195550 ) ) ;
#84661 = CARTESIAN_POINT ( 'NONE',  ( -21.05000000000000071, 68.48451787451661232, -224.2224406095231757 ) ) ;
#84662 = CARTESIAN_POINT ( 'NONE',  ( -16.77828822459933633, 51.60887986673044026, -231.9550730111018026 ) ) ;
#84663 = EDGE_CURVE ( 'NONE', #213743, #49254, #125528, .T. ) ;
#84664 = CARTESIAN_POINT ( 'NONE',  ( -22.94999999999999929, 0.000000000000000000, 0.000000000000000000 ) ) ;
#84665 = ORIENTED_EDGE ( 'NONE', *, *, #6035, .F. ) ;
#84666 = ORIENTED_EDGE ( 'NONE', *, *, #123595, .F. ) ;
#84667 = CARTESIAN_POINT ( 'NONE',  ( 0.8999999999999992450, -8.279289321881350361, 29.97071067811866030 ) ) ;
#84668 = EDGE_CURVE ( 'NONE', #127037, #215121, #187901, .T. ) ;
#84670 = EDGE_CURVE ( 'NONE', #255780, #6055, #146184, .T. ) ;
#84669 = VECTOR ( 'NONE', #29293, 1000.000000000000000 ) ;
#84671 = AXIS2_PLACEMENT_3D ( 'NONE', #182821, #160702, #121579 ) ;
#84672 = EDGE_LOOP ( 'NONE', ( #63223, #33842, #103251, #82828 ) ) ;
#84673 = CARTESIAN_POINT ( 'NONE',  ( 21.05000000000000071, 5.500000000011153745, -121.5947339810869465 ) ) ;
#84674 = ORIENTED_EDGE ( 'NONE', *, *, #160647, .T. ) ;
#84675 = CARTESIAN_POINT ( 'NONE',  ( 23.14999999999999858, 76.00000000001168132, -65.52310748452430289 ) ) ;
#84676 = VECTOR ( 'NONE', #35515, 1000.000000000000000 ) ;
#84677 = ADVANCED_FACE ( 'NONE', ( #176498 ), #196249, .F. ) ;
#84678 = LINE ( 'NONE', #224220, #10282 ) ;
#84679 = DIRECTION ( 'NONE',  ( -0.000000000000000000, -6.982962677686266711E-15, 1.000000000000000000 ) ) ;
#84680 = FACE_OUTER_BOUND ( 'NONE', #198920, .T. ) ;
#84681 = ORIENTED_EDGE ( 'NONE', *, *, #1587, .F. ) ;
#84682 = ADVANCED_FACE ( 'NONE', ( #120398 ), #154596, .F. ) ;
#84683 = FACE_OUTER_BOUND ( 'NONE', #171433, .T. ) ;
#84685 = AXIS2_PLACEMENT_3D ( 'NONE', #80157, #200152, #159741 ) ;
#84684 = DIRECTION ( 'NONE',  ( 2.952720810173289112E-16, -1.000000000000000000, 0.000000000000000000 ) ) ;
#84686 = LINE ( 'NONE', #65155, #52981 ) ;
#84687 = CARTESIAN_POINT ( 'NONE',  ( -20.54999999999999716, 76.00000000001267608, -203.5231074845243597 ) ) ;
#84688 = ORIENTED_EDGE ( 'NONE', *, *, #124270, .T. ) ;
#84690 = LINE ( 'NONE', #221654, #10891 ) ;
#84689 = DIRECTION ( 'NONE',  ( 0.000000000000000000, 0.000000000000000000, -1.000000000000000000 ) ) ;
#84692 = VERTEX_POINT ( 'NONE', #218148 ) ;
#84691 = TOROIDAL_SURFACE ( 'NONE', #176335, 7.791421356237335338, 0.1000000000000000056 ) ;
#84695 = ORIENTED_EDGE ( 'NONE', *, *, #251919, .F. ) ;
#84694 = CARTESIAN_POINT ( 'NONE',  ( 13.99999999999999822, 66.15000000001155911, -52.77310748452440237 ) ) ;
#84693 = CARTESIAN_POINT ( 'NONE',  ( 20.94999999999999929, 53.86595165227826243, -236.3638196928718855 ) ) ;
#84696 = VERTEX_POINT ( 'NONE', #102050 ) ;
#84697 = CARTESIAN_POINT ( 'NONE',  ( 18.59999999999999076, 77.83585931145498193, -24.51866831572578675 ) ) ;
#84698 = AXIS2_PLACEMENT_3D ( 'NONE', #60189, #138424, #98011 ) ;
#84700 = DIRECTION ( 'NONE',  ( 0.000000000000000000, 0.000000000000000000, -1.000000000000000000 ) ) ;
#84699 = TOROIDAL_SURFACE ( 'NONE', #76328, 7.791421356237335338, 0.1000000000000000056 ) ;
#84701 = CARTESIAN_POINT ( 'NONE',  ( -23.25000000000000355, 5.650000000011139001, -76.25000000000004263 ) ) ;
#84702 = VERTEX_POINT ( 'NONE', #181632 ) ;
#84703 = CARTESIAN_POINT ( 'NONE',  ( 18.54999999999999716, 52.34166666667924517, -186.7731074845245303 ) ) ;
#84704 = CARTESIAN_POINT ( 'NONE',  ( -18.50000000000000000, 11.65000000001115232, -88.75000000000004263 ) ) ;
#84706 = FACE_OUTER_BOUND ( 'NONE', #199079, .T. ) ;
#84705 = CARTESIAN_POINT ( 'NONE',  ( 18.54999999999999716, 63.08573235307424198, -213.1276215869287398 ) ) ;
#84708 = VERTEX_POINT ( 'NONE', #235175 ) ;
#84707 = CARTESIAN_POINT ( 'NONE',  ( 21.22070241538126467, 0.09891903053502529297, 6.469946272869620429 ) ) ;
#84709 = AXIS2_PLACEMENT_3D ( 'NONE', #21690, #118216, #77783 ) ;
#84710 = VECTOR ( 'NONE', #205041, 1000.000000000000000 ) ;
#84711 = TOROIDAL_SURFACE ( 'NONE', #251335, 11.65000000000000036, 0.1000000000000000056 ) ;
#84712 = ORIENTED_EDGE ( 'NONE', *, *, #159369, .F. ) ;
#84713 = CARTESIAN_POINT ( 'NONE',  ( 20.00000000000000355, 64.25000000001176659, -78.37310748452439668 ) ) ;
#84714 = CARTESIAN_POINT ( 'NONE',  ( -18.35235881385853318, 11.47341900772405054, -176.7499999999999716 ) ) ;
#84715 = FACE_OUTER_BOUND ( 'NONE', #52799, .T. ) ;
#84716 = ORIENTED_EDGE ( 'NONE', *, *, #16135, .F. ) ;
#84717 = CARTESIAN_POINT ( 'NONE',  ( -16.83199318825829494, 9.930646127992320160, -188.2275851882091615 ) ) ;
#84718 = VERTEX_POINT ( 'NONE', #18688 ) ;
#84720 = AXIS2_PLACEMENT_3D ( 'NONE', #204154, #106327, #4665 ) ;
#84719 = CARTESIAN_POINT ( 'NONE',  ( 20.94999999999999929, 18.81166555858609257, -229.8642012822692777 ) ) ;
#84721 = CARTESIAN_POINT ( 'NONE',  ( -22.49231231312463208, 64.35001509633508476, -170.0841603721258082 ) ) ;
#84722 = CARTESIAN_POINT ( 'NONE',  ( -21.64999999999999858, 68.65000000001150227, -48.37310748452437537 ) ) ;
#84723 = ORIENTED_EDGE ( 'NONE', *, *, #54913, .F. ) ;
#84724 = CARTESIAN_POINT ( 'NONE',  ( -21.14999999999999858, -0.09999999998884338825, -122.3504291924552234 ) ) ;
#84725 = CIRCLE ( 'NONE', #14055, 0.09999999999999939493 ) ;
#84726 = VECTOR ( 'NONE', #39242, 1000.000000000000000 ) ;
#84727 = CIRCLE ( 'NONE', #209676, 0.09999999999998898659 ) ;
#84728 = EDGE_CURVE ( 'NONE', #255891, #191184, #136038, .T. ) ;
#84730 = EDGE_CURVE ( 'NONE', #231688, #177774, #38263, .T. ) ;
#84729 = DIRECTION ( 'NONE',  ( -1.073024830501117725E-15, -0.2617529984165031243, -0.9651348961777157509 ) ) ;
#84731 = ORIENTED_EDGE ( 'NONE', *, *, #122669, .F. ) ;
#84732 = ORIENTED_EDGE ( 'NONE', *, *, #197142, .T. ) ;
#84733 = ORIENTED_EDGE ( 'NONE', *, *, #13514, .T. ) ;
#84734 = EDGE_CURVE ( 'NONE', #47133, #52893, #59587, .T. ) ;
#84735 = CARTESIAN_POINT ( 'NONE',  ( -18.50000000000000000, 66.75000000001151079, -48.17310748452438673 ) ) ;
#84736 = ORIENTED_EDGE ( 'NONE', *, *, #133036, .F. ) ;
#84739 = EDGE_CURVE ( 'NONE', #178001, #252623, #62951, .T. ) ;
#84738 = ORIENTED_EDGE ( 'NONE', *, *, #220915, .F. ) ;
#84737 = CARTESIAN_POINT ( 'NONE',  ( -20.64999999999999858, 2.000000000011154189, -54.17537807723790166 ) ) ;
#84740 = EDGE_LOOP ( 'NONE', ( #249623, #164495, #128162, #224919 ) ) ;
#84743 = VERTEX_POINT ( 'NONE', #105901 ) ;
#84742 = ORIENTED_EDGE ( 'NONE', *, *, #47843, .T. ) ;
#84741 = CARTESIAN_POINT ( 'NONE',  ( 21.05000000000000071, 56.06656052939784729, -228.0911609752645290 ) ) ;
#84744 = AXIS2_PLACEMENT_3D ( 'NONE', #225120, #144290, #128622 ) ;
#84745 = CARTESIAN_POINT ( 'NONE',  ( 21.05000000000000071, 76.00000000001244871, -170.0231074845243597 ) ) ;
#84746 = ORIENTED_EDGE ( 'NONE', *, *, #76144, .F. ) ;
#84747 = CARTESIAN_POINT ( 'NONE',  ( -23.25000000000000000, 10.33248238083634440, -106.0948465439131922 ) ) ;
#84748 = VECTOR ( 'NONE', #140812, 1000.000000000000000 ) ;
#84749 = CARTESIAN_POINT ( 'NONE',  ( 21.05000000000000426, 69.74118280533048164, -103.0567402198579998 ) ) ;
#84750 =( BOUNDED_SURFACE ( )  B_SPLINE_SURFACE ( 3, 2, ( 
 ( #112936, #252422, #155938 ),
 ( #13836, #235428, #15124 ),
 ( #56771, #256217, #196309 ),
 ( #114214, #116780, #17666 ),
 ( #192471, #77626, #93359 ),
 ( #136312, #133770, #37267 ),
 ( #236711, #94642, #172950 ),
 ( #197593, #153387, #73837 ),
 ( #232906, #54228, #193754 ),
 ( #58067, #137605, #154656 ) ),
 .UNSPECIFIED., .F., .F., .T. ) 
 B_SPLINE_SURFACE_WITH_KNOTS ( ( 4, 2, 2, 2, 4 ),
 ( 3, 3 ),
 ( 0.002161241639767249104, 0.002579950749615824834, 0.002789305304540112482, 0.002893982582002256523, 0.002998659859464400564 ),
 ( 0.000000000000000000, 1.000000000000000000 ),
 .UNSPECIFIED. ) 
 GEOMETRIC_REPRESENTATION_ITEM ( )  RATIONAL_B_SPLINE_SURFACE ( (
 ( 1.000000000000000000, 0.7071067811865475727, 1.000000000000000000),
 ( 1.000000000000000000, 0.7632447400642182744, 1.000000000000000000),
 ( 1.000000000000000000, 0.8158073005138901657, 1.000000000000000000),
 ( 1.000000000000000000, 0.8906973462381438944, 1.000000000000000000),
 ( 1.000000000000000000, 0.9149408947793837843, 1.000000000000000000),
 ( 1.000000000000000000, 0.9493368785279248101, 1.000000000000000000),
 ( 1.000000000000000000, 0.9605194247155099951, 1.000000000000000000),
 ( 1.000000000000000000, 0.9803630264783056436, 1.000000000000000000),
 ( 1.000000000000000000, 0.9900844824269788846, 1.000000000000000000),
 ( 1.000000000000000000, 0.9894588281429261833, 1.000000000000000000) ) ) 
 REPRESENTATION_ITEM ( '' )  SURFACE ( )  );
#84751 = EDGE_CURVE ( 'NONE', #146114, #57422, #78342, .T. ) ;
#84752 = CARTESIAN_POINT ( 'NONE',  ( -18.50000000000000000, 42.98415524044399660, -233.9519173640447889 ) ) ;
#84753 = EDGE_CURVE ( 'NONE', #146247, #156025, #109493, .T. ) ;
#84754 = VERTEX_POINT ( 'NONE', #207617 ) ;
#84755 = AXIS2_PLACEMENT_3D ( 'NONE', #52256, #251761, #232224 ) ;
#84756 = FACE_OUTER_BOUND ( 'NONE', #19400, .T. ) ;
#84757 = AXIS2_PLACEMENT_3D ( 'NONE', #99250, #161840, #238789 ) ;
#84759 = EDGE_LOOP ( 'NONE', ( #113435, #132841, #119657 ) ) ;
#84758 = LINE ( 'NONE', #67800, #145131 ) ;
#84760 = CARTESIAN_POINT ( 'NONE',  ( -16.77977881697927032, 9.946601933544062746, -180.1613785731150017 ) ) ;
#84762 = ORIENTED_EDGE ( 'NONE', *, *, #213030, .F. ) ;
#84761 = DIRECTION ( 'NONE',  ( -1.000000000000000000, 0.000000000000000000, -0.000000000000000000 ) ) ;
#84763 = EDGE_LOOP ( 'NONE', ( #47294, #103611, #6869, #44833 ) ) ;
#84764 = CARTESIAN_POINT ( 'NONE',  ( -20.00857864376270001, 9.350000000011156942, -79.25000000000004263 ) ) ;
#84765 = VECTOR ( 'NONE', #244979, 1000.000000000000000 ) ;
#84766 = CIRCLE ( 'NONE', #118120, 0.09999999999999939493 ) ;
#84768 = ORIENTED_EDGE ( 'NONE', *, *, #127819, .F. ) ;
#84767 = CIRCLE ( 'NONE', #105625, 11.70000000000000284 ) ;
#84769 = ADVANCED_FACE ( 'NONE', ( #142476 ), #27719, .T. ) ;
#84770 = ORIENTED_EDGE ( 'NONE', *, *, #150787, .F. ) ;
#84771 = AXIS2_PLACEMENT_3D ( 'NONE', #189398, #171166, #150284 ) ;
#84772 = DIRECTION ( 'NONE',  ( 1.000000000000000000, 0.000000000000000000, 0.000000000000000000 ) ) ;
#84773 = DIRECTION ( 'NONE',  ( 0.000000000000000000, 0.000000000000000000, 1.000000000000000000 ) ) ;
#84774 = ADVANCED_FACE ( 'NONE', ( #43390 ), #122937, .T. ) ;
#84775 = AXIS2_PLACEMENT_3D ( 'NONE', #1672, #18683, #387 ) ;
#84777 = EDGE_LOOP ( 'NONE', ( #29020, #230970, #74038, #107147 ) ) ;
#84776 = ORIENTED_EDGE ( 'NONE', *, *, #86466, .T. ) ;
#84778 = EDGE_LOOP ( 'NONE', ( #143473, #12998, #70140 ) ) ;
#84779 = DIRECTION ( 'NONE',  ( 1.000000000000000000, 0.000000000000000000, 0.000000000000000000 ) ) ;
#84780 = VERTEX_POINT ( 'NONE', #44685 ) ;
#84781 = ORIENTED_EDGE ( 'NONE', *, *, #28656, .F. ) ;
#84782 = DIRECTION ( 'NONE',  ( 1.000000000000000000, 0.000000000000000000, 0.000000000000000000 ) ) ;
#84784 = ORIENTED_EDGE ( 'NONE', *, *, #147771, .T. ) ;
#84783 = CARTESIAN_POINT ( 'NONE',  ( -21.05000000000000071, -11.64999999998884483, -70.00000000000004263 ) ) ;
#84785 = DIRECTION ( 'NONE',  ( 0.000000000000000000, 0.000000000000000000, -1.000000000000000000 ) ) ;
#84786 = CIRCLE ( 'NONE', #159852, 11.80000000000000426 ) ;
#84788 = CARTESIAN_POINT ( 'NONE',  ( 18.50000000000000000, -9.399999999988823518, -107.7972597596632909 ) ) ;
#84787 = DIRECTION ( 'NONE',  ( 1.000000000000000000, -0.000000000000000000, 0.000000000000000000 ) ) ;
#84789 = EDGE_CURVE ( 'NONE', #74531, #87436, #50362, .T. ) ;
#84790 = ORIENTED_EDGE ( 'NONE', *, *, #188098, .F. ) ;
#84791 = ADVANCED_FACE ( 'NONE', ( #182917 ), #25133, .F. ) ;
#84793 = EDGE_LOOP ( 'NONE', ( #106611, #29136, #66502, #151142 ) ) ;
#84792 = ORIENTED_EDGE ( 'NONE', *, *, #48179, .F. ) ;
#84794 = DIRECTION ( 'NONE',  ( 0.000000000000000000, 0.8814952561688429444, -0.4721928772777349570 ) ) ;
#84795 = ORIENTED_EDGE ( 'NONE', *, *, #224177, .F. ) ;
#84796 = AXIS2_PLACEMENT_3D ( 'NONE', #113983, #111431, #233940 ) ;
#84797 = VECTOR ( 'NONE', #79913, 1000.000000000000000 ) ;
#84798 = EDGE_CURVE ( 'NONE', #88042, #176438, #104608, .T. ) ;
#84799 = AXIS2_PLACEMENT_3D ( 'NONE', #245963, #67309, #222512 ) ;
#84800 = DIRECTION ( 'NONE',  ( 0.000000000000000000, -0.9908441862701791170, 0.1350103645450472789 ) ) ;
#84801 = ORIENTED_EDGE ( 'NONE', *, *, #171401, .F. ) ;
#84802 = ORIENTED_EDGE ( 'NONE', *, *, #29457, .T. ) ;
#84803 = CARTESIAN_POINT ( 'NONE',  ( -20.54999999999999716, -8.730841121495329205, -9.598074718984332065 ) ) ;
#84804 = ORIENTED_EDGE ( 'NONE', *, *, #190067, .F. ) ;
#84805 = CARTESIAN_POINT ( 'NONE',  ( 23.14999999999999503, 64.25000000001175238, -76.53791325517833855 ) ) ;
#84806 = CARTESIAN_POINT ( 'NONE',  ( 21.05000000000000426, 34.06939550845276443, -243.8530697005520267 ) ) ;
#84807 = EDGE_LOOP ( 'NONE', ( #224209, #166596, #14974, #121364 ) ) ;
#84808 = ADVANCED_FACE ( 'NONE', ( #65509 ), #45953, .T. ) ;
#84809 = CARTESIAN_POINT ( 'NONE',  ( 19.81427058490525894, 64.33143601963044489, -145.2731074845244166 ) ) ;
#84811 = LINE ( 'NONE', #226925, #245445 ) ;
#84810 =( BOUNDED_CURVE ( )  B_SPLINE_CURVE ( 3, ( #77405, #196098, #60420, #199960 ),
 .UNSPECIFIED., .F., .F. ) 
 B_SPLINE_CURVE_WITH_KNOTS ( ( 4, 4 ),
 ( 4.712388980384690562, 6.283185307179586232 ),
 .UNSPECIFIED. ) 
 CURVE ( )  GEOMETRIC_REPRESENTATION_ITEM ( )  RATIONAL_B_SPLINE_CURVE ( ( 1.000000000000000000, 0.8047378541243652705, 0.8047378541243652705, 1.000000000000000000 ) ) 
 REPRESENTATION_ITEM ( '' )  );
#84812 = DIRECTION ( 'NONE',  ( 1.000000000000000000, 0.000000000000000000, 0.000000000000000000 ) ) ;
#84813 = DIRECTION ( 'NONE',  ( 0.000000000000000000, 0.2128009952263982818, -0.9770955615653232895 ) ) ;
#84814 = SPHERICAL_SURFACE ( 'NONE', #103518, 0.1000000000000000056 ) ;
#84815 = LINE ( 'NONE', #121448, #236264 ) ;
#84817 = ADVANCED_FACE ( 'NONE', ( #246713 ), #52355, .F. ) ;
#84816 = DIRECTION ( 'NONE',  ( 1.000000000000000000, 0.000000000000000000, 0.000000000000000000 ) ) ;
#84818 = CIRCLE ( 'NONE', #138974, 0.09999999999999939493 ) ;
#84820 = EDGE_LOOP ( 'NONE', ( #6760, #59097, #13903, #194861 ) ) ;
#84819 = VECTOR ( 'NONE', #236421, 1000.000000000000000 ) ;
#84821 = AXIS2_PLACEMENT_3D ( 'NONE', #120699, #238041, #3270 ) ;
#84822 = CIRCLE ( 'NONE', #80739, 0.09999999999999939493 ) ;
#84824 = ORIENTED_EDGE ( 'NONE', *, *, #40651, .T. ) ;
#84823 = VERTEX_POINT ( 'NONE', #130626 ) ;
#84825 = ORIENTED_EDGE ( 'NONE', *, *, #161191, .T. ) ;
#84827 = ADVANCED_FACE ( 'NONE', ( #49805 ), #150210, .T. ) ;
#84826 = CARTESIAN_POINT ( 'NONE',  ( -22.39999999999999858, 0.000000000000000000, 6.249999999999998224 ) ) ;
#84828 = CARTESIAN_POINT ( 'NONE',  ( -18.50000000000000000, 11.65000000001115588, -134.0000000000000284 ) ) ;
#84830 = CARTESIAN_POINT ( 'NONE',  ( -13.77178122865954180, 9.456028260507913785, -15.01119803506572659 ) ) ;
#84829 = DIRECTION ( 'NONE',  ( 0.000000000000000000, 0.000000000000000000, -1.000000000000000000 ) ) ;
#84831 = CARTESIAN_POINT ( 'NONE',  ( -20.64999999999999858, 54.18213181965657554, -236.9344197582443883 ) ) ;
#84832 = ORIENTED_EDGE ( 'NONE', *, *, #75807, .F. ) ;
#84833 = LINE ( 'NONE', #124013, #183912 ) ;
#84834 = DIRECTION ( 'NONE',  ( 0.000000000000000000, 6.982962677686266711E-15, -1.000000000000000000 ) ) ;
#84835 = DIRECTION ( 'NONE',  ( 0.000000000000000000, -0.2617529984165031243, -0.9651348961777158619 ) ) ;
#84836 = CARTESIAN_POINT ( 'NONE',  ( -21.05000000000000071, 56.55475276915903038, -225.2974176673762940 ) ) ;
#84837 = VERTEX_POINT ( 'NONE', #152799 ) ;
#84838 = CARTESIAN_POINT ( 'NONE',  ( 22.39999999999999503, 7.790779598384535376, -134.0000000000000000 ) ) ;
#84839 = AXIS2_PLACEMENT_3D ( 'NONE', #61292, #183803, #26025 ) ;
#84840 = CARTESIAN_POINT ( 'NONE',  ( -18.59999999999999787, 78.48087866980282001, -232.8271061603568910 ) ) ;
#84841 = VERTEX_POINT ( 'NONE', #168522 ) ;
#84842 = ORIENTED_EDGE ( 'NONE', *, *, #68477, .F. ) ;
#84843 = DIRECTION ( 'NONE',  ( 0.000000000000000000, 0.1335171055202901413, -0.9910465087640860649 ) ) ;
#84844 = CARTESIAN_POINT ( 'NONE',  ( 22.39999999999999503, 1.115600667400684642E-11, -88.85042919245522341 ) ) ;
#84845 = DIRECTION ( 'NONE',  ( -1.000000000000000000, 0.000000000000000000, 0.000000000000000000 ) ) ;
#84846 = CARTESIAN_POINT ( 'NONE',  ( -22.59999999999999787, 76.00000000001213607, -136.5231074845242745 ) ) ;
#84847 = LINE ( 'NONE', #182723, #227412 ) ;
#84848 = CARTESIAN_POINT ( 'NONE',  ( -22.50000000000000000, 0.1000000000111554016, -159.7092204016265384 ) ) ;
#84849 = ORIENTED_EDGE ( 'NONE', *, *, #114190, .F. ) ;
#84850 = DIRECTION ( 'NONE',  ( 0.000000000000000000, 0.8814952561688437216, -0.4721928772777334582 ) ) ;
#84851 = DIRECTION ( 'NONE',  ( 0.000000000000000000, -0.9908441862701605762, 0.1350103645451835310 ) ) ;
#84852 = CARTESIAN_POINT ( 'NONE',  ( 20.95595624212472075, 12.00415041844581054, -206.1941058355727989 ) ) ;
#84854 = CARTESIAN_POINT ( 'NONE',  ( 20.85000000000000142, 64.25000000001146816, -42.80697314750249660 ) ) ;
#84853 = CARTESIAN_POINT ( 'NONE',  ( 19.58285714285715073, 66.98499851036301322, -61.10245466844266815 ) ) ;
#84855 = CARTESIAN_POINT ( 'NONE',  ( -18.52328366898032996, 85.64232108905365237, -163.3082881469542826 ) ) ;
#84856 = SURFACE_SIDE_STYLE ('',( #204830 ) ) ;
#84857 = CARTESIAN_POINT ( 'NONE',  ( 20.01715728752538936, 4.611773100472912112, 22.11686199900910665 ) ) ;
#84858 = DIRECTION ( 'NONE',  ( 0.000000000000000000, 6.982962677686266711E-15, -1.000000000000000000 ) ) ;
#84859 = AXIS2_PLACEMENT_3D ( 'NONE', #77054, #134443, #196992 ) ;
#84861 = VERTEX_POINT ( 'NONE', #211452 ) ;
#84860 = DIRECTION ( 'NONE',  ( 0.000000000000000000, 0.1298341882520022972, 0.9915357197604853789 ) ) ;
#84862 = AXIS2_PLACEMENT_3D ( 'NONE', #29861, #50653, #225441 ) ;
#84863 = CIRCLE ( 'NONE', #209807, 0.6000000000000033085 ) ;
#84864 = EDGE_CURVE ( 'NONE', #22402, #144975, #212747, .T. ) ;
#84865 = CARTESIAN_POINT ( 'NONE',  ( 21.53551880898956838, 6.784797761427480367, -100.4010302654283606 ) ) ;
#84866 = ADVANCED_FACE ( 'NONE', ( #32858 ), #232324, .T. ) ;
#84867 = EDGE_CURVE ( 'NONE', #5985, #11624, #111065, .T. ) ;
#84869 = CARTESIAN_POINT ( 'NONE',  ( -18.58222699835055280, 65.66799936921481162, -30.42993998886009521 ) ) ;
#84868 = CIRCLE ( 'NONE', #234948, 7.720710678118692272 ) ;
#84870 = PLANE ( 'NONE',  #42053 ) ;
#84871 = EDGE_LOOP ( 'NONE', ( #31571, #124117, #42854, #15901 ) ) ;
#84872 = AXIS2_PLACEMENT_3D ( 'NONE', #15815, #117459, #20949 ) ;
#84873 = LINE ( 'NONE', #82316, #184583 ) ;
#84874 = AXIS2_PLACEMENT_3D ( 'NONE', #141798, #237064, #216197 ) ;
#84875 = DIRECTION ( 'NONE',  ( 0.000000000000000000, -0.5868805631290353597, -0.8096735173027127530 ) ) ;
#84876 = CARTESIAN_POINT ( 'NONE',  ( -18.59999999999999787, 11.75000000001115197, -141.0148057706539930 ) ) ;
#84877 = CIRCLE ( 'NONE', #143158, 0.09999999999999736877 ) ;
#84878 = ORIENTED_EDGE ( 'NONE', *, *, #160038, .F. ) ;
#84879 = DIRECTION ( 'NONE',  ( 1.000000000000000000, 0.000000000000000000, 0.000000000000000000 ) ) ;
#84881 = ORIENTED_EDGE ( 'NONE', *, *, #158617, .T. ) ;
#84880 = DIRECTION ( 'NONE',  ( 0.000000000000000000, -0.8454177738465993297, -0.5341055959866553016 ) ) ;
#84883 = CARTESIAN_POINT ( 'NONE',  ( -21.55000000000000071, 7.250000000011155521, -179.8499999999999943 ) ) ;
#84882 = DIRECTION ( 'NONE',  ( 2.952720810173290098E-16, -0.4721928772777359007, -0.8814952561688425003 ) ) ;
#84884 = EDGE_CURVE ( 'NONE', #155087, #47711, #133709, .T. ) ;
#84885 = DIRECTION ( 'NONE',  ( 1.000000000000000000, 0.000000000000000000, -0.000000000000000000 ) ) ;
#84886 = ORIENTED_EDGE ( 'NONE', *, *, #148616, .T. ) ;
#84887 = CARTESIAN_POINT ( 'NONE',  ( 23.50000000000005684, 64.35000000001120668, -51.02310748452479316 ) ) ;
#84888 = CIRCLE ( 'NONE', #9909, 0.09999999999999939493 ) ;
#84889 = DIRECTION ( 'NONE',  ( 1.000000000000000000, 0.000000000000000000, 0.000000000000000000 ) ) ;
#84891 = CARTESIAN_POINT ( 'NONE',  ( 5.999999999999995559, -11.65000000000000036, 10.10000000000000142 ) ) ;
#84890 = CIRCLE ( 'NONE', #5794, 0.1000000000000000472 ) ;
#84893 = AXIS2_PLACEMENT_3D ( 'NONE', #76990, #35345, #255580 ) ;
#84892 = DIRECTION ( 'NONE',  ( 0.000000000000000000, 0.4088369013363281068, -0.9126074666063770380 ) ) ;
#84894 = DIRECTION ( 'NONE',  ( 0.000000000000000000, -0.8814952561688425003, 0.4721928772777359007 ) ) ;
#84895 = EDGE_LOOP ( 'NONE', ( #207144, #15912, #43072, #242907 ) ) ;
#84896 = DIRECTION ( 'NONE',  ( 0.000000000000000000, -1.000000000000000000, -7.272083257015735086E-15 ) ) ;
#84897 = VECTOR ( 'NONE', #159475, 1000.000000000000000 ) ;
#84898 = DIRECTION ( 'NONE',  ( -0.8660254037843878594, 0.000000000000000000, 0.5000000000000880407 ) ) ;
#84899 = CIRCLE ( 'NONE', #134977, 0.09999999999999939493 ) ;
#84900 = LINE ( 'NONE', #83613, #170098 ) ;
#84901 = CARTESIAN_POINT ( 'NONE',  ( -22.39999999999999858, 1.115600667400684642E-11, -122.3504291924552234 ) ) ;
#84902 = EDGE_CURVE ( 'NONE', #91774, #212797, #96282, .T. ) ;
#84903 = ORIENTED_EDGE ( 'NONE', *, *, #257091, .T. ) ;
#84904 = ADVANCED_FACE ( 'NONE', ( #171090 ), #53662, .T. ) ;
#84905 = VERTEX_POINT ( 'NONE', #112365 ) ;
#84906 = VECTOR ( 'NONE', #18360, 1000.000000000000000 ) ;
#84907 = CARTESIAN_POINT ( 'NONE',  ( 22.40000000000010516, 76.00000000001269029, -81.27354037698326295 ) ) ;
#84908 = CIRCLE ( 'NONE', #243157, 0.09999999999998898659 ) ;
#84909 = AXIS2_PLACEMENT_3D ( 'NONE', #43915, #4759, #84267 ) ;
#84910 = FACE_OUTER_BOUND ( 'NONE', #220926, .T. ) ;
#84911 = DIRECTION ( 'NONE',  ( -1.000000000000000000, 0.000000000000000000, 0.000000000000000000 ) ) ;
#84912 = DIRECTION ( 'NONE',  ( -0.000000000000000000, 1.000000000000000000, -0.000000000000000000 ) ) ;
#84913 = LINE ( 'NONE', #87498, #115985 ) ;
#84914 = ADVANCED_FACE ( 'NONE', ( #169800 ), #34137, .F. ) ;
#84916 = DIRECTION ( 'NONE',  ( -1.000000000000000000, 0.000000000000000000, -0.000000000000000000 ) ) ;
#84915 = CARTESIAN_POINT ( 'NONE',  ( -16.79139129368503802, 12.41340146879463724, -211.2637457794402280 ) ) ;
#84917 = CARTESIAN_POINT ( 'NONE',  ( -33.72168855820452649, 11.47316190337362940, -57.75000000000000711 ) ) ;
#84918 = CARTESIAN_POINT ( 'NONE',  ( -22.59999999999999787, 12.58798907299599179, -223.3278890275437050 ) ) ;
#84919 = CARTESIAN_POINT ( 'NONE',  ( -18.59999996769639097, 47.04086122480761389, -255.1600965361087106 ) ) ;
#84920 = FACE_OUTER_BOUND ( 'NONE', #78975, .T. ) ;
#84922 = ORIENTED_EDGE ( 'NONE', *, *, #84730, .F. ) ;
#84921 = CARTESIAN_POINT ( 'NONE',  ( 15.31784899511109010, 62.84948463577723032, -216.1128043527995999 ) ) ;
#84923 = CARTESIAN_POINT ( 'NONE',  ( -20.95613430942437105, 64.25000000001207923, -129.6659448363049023 ) ) ;
#84924 = CARTESIAN_POINT ( 'NONE',  ( -18.70000000000000284, 1.212568896937007645, -7.900000000000000355 ) ) ;
#84926 = CARTESIAN_POINT ( 'NONE',  ( -20.64999999999999858, 1.115600667400684642E-11, -65.00000000000000000 ) ) ;
#84925 = DIRECTION ( 'NONE',  ( 0.000000000000000000, 0.9126074666063545004, 0.4088369013363783999 ) ) ;
#84927 = VERTEX_POINT ( 'NONE', #208881 ) ;
#84928 = CARTESIAN_POINT ( 'NONE',  ( -16.82055514392384410, 66.05000000001159322, -56.84630940998236781 ) ) ;
#84929 = DIRECTION ( 'NONE',  ( 0.000000000000000000, 0.000000000000000000, 1.000000000000000000 ) ) ;
#84930 = FACE_OUTER_BOUND ( 'NONE', #107401, .T. ) ;
#84931 = CARTESIAN_POINT ( 'NONE',  ( 21.07928932188134397, 76.00000000001195133, -103.0231074845243171 ) ) ;
#84932 = CARTESIAN_POINT ( 'NONE',  ( -12.42749937872396160, 66.62931007840991526, -185.9966423578633510 ) ) ;
#84933 = ORIENTED_EDGE ( 'NONE', *, *, #234291, .F. ) ;
#84934 = ORIENTED_EDGE ( 'NONE', *, *, #189210, .F. ) ;
#84935 = EDGE_CURVE ( 'NONE', #31477, #87486, #250567, .T. ) ;
#84936 = AXIS2_PLACEMENT_3D ( 'NONE', #11907, #249218, #151412 ) ;
#84937 = AXIS2_PLACEMENT_3D ( 'NONE', #99762, #159774, #39844 ) ;
#84938 = CARTESIAN_POINT ( 'NONE',  ( 18.49999999999998934, 69.35000000001205933, -124.1731074845243370 ) ) ;
#84939 = ORIENTED_EDGE ( 'NONE', *, *, #95352, .T. ) ;
#84940 = DIRECTION ( 'NONE',  ( 0.000000000000000000, 0.000000000000000000, -1.000000000000000000 ) ) ;
#84941 = ORIENTED_EDGE ( 'NONE', *, *, #149491, .F. ) ;
#84942 = CARTESIAN_POINT ( 'NONE',  ( -23.15000000000000213, 76.00000000001247713, -173.9231074845243654 ) ) ;
#84943 = CARTESIAN_POINT ( 'NONE',  ( -21.05000000000000071, 1.835341550224411922, -11.65515129256298010 ) ) ;
#84944 = AXIS2_PLACEMENT_3D ( 'NONE', #155315, #101689, #45609 ) ;
#84945 = EDGE_CURVE ( 'NONE', #248066, #95768, #10688, .T. ) ;
#84946 = AXIS2_PLACEMENT_3D ( 'NONE', #122386, #242319, #147061 ) ;
#84947 = CARTESIAN_POINT ( 'NONE',  ( -21.05000000000000071, 62.99095723518624368, -207.1734234082435364 ) ) ;
#84948 = ORIENTED_EDGE ( 'NONE', *, *, #36449, .T. ) ;
#84949 = AXIS2_PLACEMENT_3D ( 'NONE', #213232, #34636, #253637 ) ;
#84950 = EDGE_CURVE ( 'NONE', #12445, #116181, #254493, .T. ) ;
#84952 = EDGE_CURVE ( 'NONE', #243292, #146605, #221191, .T. ) ;
#84951 = DIRECTION ( 'NONE',  ( -0.000000000000000000, -1.156482317317873105E-15, -1.000000000000000000 ) ) ;
#84953 = DIRECTION ( 'NONE',  ( 0.000000000000000000, -6.982962677686266711E-15, 1.000000000000000000 ) ) ;
#84955 = AXIS2_PLACEMENT_3D ( 'NONE', #205736, #70117, #68819 ) ;
#84954 = CARTESIAN_POINT ( 'NONE',  ( 21.05315837450969596, 11.75000000001116085, -160.6583560044166745 ) ) ;
#84956 = DIRECTION ( 'NONE',  ( -0.000000000000000000, 0.8814952561688430555, -0.4721928772777346239 ) ) ;
#84958 = AXIS2_PLACEMENT_3D ( 'NONE', #205868, #70250, #229302 ) ;
#84957 = CARTESIAN_POINT ( 'NONE',  ( -16.86132326855786090, 44.17986708625154790, -235.2790475031096378 ) ) ;
#84959 = CARTESIAN_POINT ( 'NONE',  ( -18.59999999999999787, 7.783179459866048866, -245.3643104511423019 ) ) ;
#84960 = AXIS2_PLACEMENT_3D ( 'NONE', #29725, #130058, #70132 ) ;
#84961 = CARTESIAN_POINT ( 'NONE',  ( 15.70340296795548873, 62.46518123923912214, -217.6854569796042256 ) ) ;
#84962 = VERTEX_POINT ( 'NONE', #89759 ) ;
#84964 = CARTESIAN_POINT ( 'NONE',  ( -17.71734398241073905, 10.84235722847571814, -43.77486174699441079 ) ) ;
#84963 = CARTESIAN_POINT ( 'NONE',  ( 18.59999999999999076, 13.59055429284667227, -238.6121134008722038 ) ) ;
#84965 = ORIENTED_EDGE ( 'NONE', *, *, #7332, .T. ) ;
#84967 = ORIENTED_EDGE ( 'NONE', *, *, #28203, .T. ) ;
#84966 = CARTESIAN_POINT ( 'NONE',  ( 18.39999999999999503, 5.650000000011139001, -158.2500000000000284 ) ) ;
#84968 = EDGE_CURVE ( 'NONE', #63666, #209650, #62982, .T. ) ;
#84969 = VERTEX_POINT ( 'NONE', #49368 ) ;
#84970 = LINE ( 'NONE', #189251, #240588 ) ;
#84971 = EDGE_CURVE ( 'NONE', #166706, #73306, #222856, .T. ) ;
#84972 = CARTESIAN_POINT ( 'NONE',  ( 18.49999999999998934, 10.29288807859941457, -72.45800201601215917 ) ) ;
#84973 = CARTESIAN_POINT ( 'NONE',  ( -23.15000000000000213, -9.000000000000003553, -9.393969122652443104 ) ) ;
#84974 = CYLINDRICAL_SURFACE ( 'NONE', #175114, 0.09999999999999939493 ) ;
#84975 = VERTEX_POINT ( 'NONE', #164189 ) ;
#84976 = CARTESIAN_POINT ( 'NONE',  ( 19.75857864376268935, 11.75000000001115907, -125.3500000000000512 ) ) ;
#84979 = ADVANCED_FACE ( 'NONE', ( #6380 ), #87183, .F. ) ;
#84978 = CARTESIAN_POINT ( 'NONE',  ( -16.85312841634287295, 66.08639382269207374, -157.1259343512318480 ) ) ;
#84977 = AXIS2_PLACEMENT_3D ( 'NONE', #222177, #106083, #141377 ) ;
#84980 = ORIENTED_EDGE ( 'NONE', *, *, #25759, .T. ) ;
#84981 = CARTESIAN_POINT ( 'NONE',  ( -20.85000000000000142, 10.33248238082518711, -39.09484654391314962 ) ) ;
#84982 = AXIS2_PLACEMENT_3D ( 'NONE', #89298, #207998, #91876 ) ;
#84983 = EDGE_CURVE ( 'NONE', #57597, #785, #242217, .T. ) ;
#84984 = CARTESIAN_POINT ( 'NONE',  ( -21.29999999999995808, 0.000000000000000000, -4.049999999999998934 ) ) ;
#84985 = ORIENTED_EDGE ( 'NONE', *, *, #108147, .T. ) ;
#84986 = CARTESIAN_POINT ( 'NONE',  ( -16.85697194749123540, 9.908543714134728120, -146.9350042676138628 ) ) ;
#84987 = EDGE_CURVE ( 'NONE', #81210, #96897, #166779, .T. ) ;
#84988 = EDGE_CURVE ( 'NONE', #200797, #14640, #208463, .T. ) ;
#84989 = AXIS2_PLACEMENT_3D ( 'NONE', #49549, #50803, #246461 ) ;
#84990 = CIRCLE ( 'NONE', #22687, 0.09999999999999753530 ) ;
#84991 = ORIENTED_EDGE ( 'NONE', *, *, #126126, .T. ) ;
#84992 = AXIS2_PLACEMENT_3D ( 'NONE', #83953, #163542, #243072 ) ;
#84993 = LINE ( 'NONE', #241532, #121486 ) ;
#84994 = ORIENTED_EDGE ( 'NONE', *, *, #12267, .T. ) ;
#84995 = DIRECTION ( 'NONE',  ( 0.000000000000000000, 0.008583690987124399305, -0.9999631594459055250 ) ) ;
#84996 = EDGE_CURVE ( 'NONE', #116221, #149669, #113229, .T. ) ;
#84997 = CARTESIAN_POINT ( 'NONE',  ( -23.49999999999994316, 77.83551161375991967, -47.52760213295649550 ) ) ;
#84998 = DIRECTION ( 'NONE',  ( -0.000000000000000000, -6.982962677686266711E-15, 1.000000000000000000 ) ) ;
#84999 = DIRECTION ( 'NONE',  ( 1.000000000000000000, 2.952720810173289112E-16, -0.000000000000000000 ) ) ;
#85000 = EDGE_CURVE ( 'NONE', #225371, #79959, #129802, .T. ) ;
#85001 = EDGE_CURVE ( 'NONE', #43854, #3631, #250598, .T. ) ;
#85002 = ADVANCED_FACE ( 'NONE', ( #109315 ), #246287, .T. ) ;
#85003 = AXIS2_PLACEMENT_3D ( 'NONE', #181302, #83432, #196978 ) ;
#85004 = CYLINDRICAL_SURFACE ( 'NONE', #105611, 0.09999999999999939493 ) ;
#85005 = AXIS2_PLACEMENT_3D ( 'NONE', #251136, #235429, #114216 ) ;
#85006 = AXIS2_PLACEMENT_3D ( 'NONE', #54982, #77134, #96664 ) ;
#85007 = LINE ( 'NONE', #122893, #89591 ) ;
#85008 = ORIENTED_EDGE ( 'NONE', *, *, #134048, .F. ) ;
#85010 = DIRECTION ( 'NONE',  ( -1.000000000000000000, -0.000000000000000000, -0.000000000000000000 ) ) ;
#85009 = CARTESIAN_POINT ( 'NONE',  ( -21.04999999999954241, 69.55922910635037226, -170.0055102975150021 ) ) ;
#85011 = ORIENTED_EDGE ( 'NONE', *, *, #12345, .T. ) ;
#85012 = CARTESIAN_POINT ( 'NONE',  ( -16.92570016628985030, 12.41637551217347379, -211.2123415523068104 ) ) ;
#85014 = ORIENTED_EDGE ( 'NONE', *, *, #184590, .F. ) ;
#85013 = CARTESIAN_POINT ( 'NONE',  ( 20.94999999999999574, 79.23417978893664326, -236.1056577391152587 ) ) ;
#85016 = ORIENTED_EDGE ( 'NONE', *, *, #159478, .T. ) ;
#85015 = CARTESIAN_POINT ( 'NONE',  ( 18.59999999999999432, -1.299733671219632791, -90.52812952286942050 ) ) ;
#85017 = ADVANCED_FACE ( 'NONE', ( #27272 ), #169354, .T. ) ;
#85018 = DIRECTION ( 'NONE',  ( 0.000000000000000000, -0.8103668758649471560, 0.5859227990963360444 ) ) ;
#85019 = CARTESIAN_POINT ( 'NONE',  ( 21.05000000000000071, 76.00000000001126921, -203.5231074845248997 ) ) ;
#85020 = DIRECTION ( 'NONE',  ( -2.952720810173288619E-16, 0.4721928772777346239, 0.8814952561688430555 ) ) ;
#85021 = EDGE_CURVE ( 'NONE', #91225, #9710, #24696, .T. ) ;
#85022 = DIRECTION ( 'NONE',  ( 0.000000000000000000, -0.9126074666063769270, -0.4088369013363280513 ) ) ;
#85025 = ORIENTED_EDGE ( 'NONE', *, *, #18856, .T. ) ;
#85024 = CARTESIAN_POINT ( 'NONE',  ( -23.25000000000000355, 64.25000000001253397, -179.2731074845244450 ) ) ;
#85023 = B_SPLINE_CURVE_WITH_KNOTS ( 'NONE', 3,
 ( #148417, #106692, #150980, #149718 ),
 .UNSPECIFIED., .F., .F.,
 ( 4, 4 ),
 ( 0.000000000000000000, 0.001767853679387110157 ),
 .UNSPECIFIED. ) ;
#85026 = CARTESIAN_POINT ( 'NONE',  ( -18.40000000000000213, 64.66825945288690036, -123.8731074845243683 ) ) ;
#85027 = PRESENTATION_LAYER_ASSIGNMENT (  '', '', ( #197476 ) ) ;
#85028 = ORIENTED_EDGE ( 'NONE', *, *, #242992, .T. ) ;
#85029 = VERTEX_POINT ( 'NONE', #147175 ) ;
#85030 = CARTESIAN_POINT ( 'NONE',  ( -20.94999999999999929, 77.16270174994990327, -94.92310748452430857 ) ) ;
#85031 = DIRECTION ( 'NONE',  ( 0.000000000000000000, 1.000000000000000000, 6.982962677686266711E-15 ) ) ;
#85032 = ORIENTED_EDGE ( 'NONE', *, *, #11828, .F. ) ;
#85033 = DIRECTION ( 'NONE',  ( 0.000000000000000000, -1.000000000000000000, 0.000000000000000000 ) ) ;
#85034 = EDGE_CURVE ( 'NONE', #34375, #196293, #84588, .T. ) ;
#85035 = ORIENTED_EDGE ( 'NONE', *, *, #29598, .T. ) ;
#85036 = CIRCLE ( 'NONE', #230653, 0.09999999999999609201 ) ;
#85038 = ADVANCED_FACE ( 'NONE', ( #243713 ), #127622, .F. ) ;
#85037 = CARTESIAN_POINT ( 'NONE',  ( 23.15000000000000213, -9.599999999988842347, -90.60603087734760663 ) ) ;
#85039 = CIRCLE ( 'NONE', #47461, 0.09999999999999939493 ) ;
#85040 = CIRCLE ( 'NONE', #155832, 0.09999999999999938105 ) ;
#85041 = AXIS2_PLACEMENT_3D ( 'NONE', #6260, #84478, #45401 ) ;
#85042 = ORIENTED_EDGE ( 'NONE', *, *, #222057, .T. ) ;
#85043 = VERTEX_POINT ( 'NONE', #68951 ) ;
#85044 = CARTESIAN_POINT ( 'NONE',  ( -18.54260524012594047, -9.624219390062449975, -73.74077304577103575 ) ) ;
#85045 = VERTEX_POINT ( 'NONE', #224138 ) ;
#85046 = CARTESIAN_POINT ( 'NONE',  ( -16.90137573187933384, 9.950000000011135270, -46.28841742409689175 ) ) ;
#85047 = EDGE_LOOP ( 'NONE', ( #179211, #2941, #32339 ) ) ;
#85049 = ORIENTED_EDGE ( 'NONE', *, *, #28306, .T. ) ;
#85048 = FACE_OUTER_BOUND ( 'NONE', #233319, .T. ) ;
#85050 = DIRECTION ( 'NONE',  ( 0.000000000000000000, 0.2617529984165032908, 0.9651348961777156399 ) ) ;
#85051 = ORIENTED_EDGE ( 'NONE', *, *, #175806, .F. ) ;
#85052 = FACE_OUTER_BOUND ( 'NONE', #200497, .T. ) ;
#85053 = EDGE_LOOP ( 'NONE', ( #131295, #84644, #92918, #250314 ) ) ;
#85055 = VERTEX_POINT ( 'NONE', #45513 ) ;
#85054 = ORIENTED_EDGE ( 'NONE', *, *, #236624, .T. ) ;
#85057 = CARTESIAN_POINT ( 'NONE',  ( 21.13422380239043719, 69.50667348520650535, -136.5231074845243313 ) ) ;
#85056 = AXIS2_PLACEMENT_3D ( 'NONE', #3902, #80847, #83403 ) ;
#85058 = EDGE_CURVE ( 'NONE', #81417, #127618, #50667, .T. ) ;
#85059 = LINE ( 'NONE', #244155, #239839 ) ;
#85060 = ORIENTED_EDGE ( 'NONE', *, *, #226498, .F. ) ;
#85061 = CIRCLE ( 'NONE', #234952, 14.30833333333333890 ) ;
#85062 = AXIS2_PLACEMENT_3D ( 'NONE', #29597, #188636, #169116 ) ;
#85063 = AXIS2_PLACEMENT_3D ( 'NONE', #115571, #54304, #232978 ) ;
#85064 = CIRCLE ( 'NONE', #89188, 4.049999999999998046 ) ;
#85065 = ORIENTED_EDGE ( 'NONE', *, *, #206211, .T. ) ;
#85066 = CARTESIAN_POINT ( 'NONE',  ( -21.05000000000000071, -1.261786168553869603, -41.58649896354548048 ) ) ;
#85067 = CARTESIAN_POINT ( 'NONE',  ( 18.49999999999999645, 76.00000000001126921, -203.5231074845248997 ) ) ;
#85069 = ORIENTED_EDGE ( 'NONE', *, *, #240068, .F. ) ;
#85068 = DIRECTION ( 'NONE',  ( 1.000000000000000000, 0.000000000000000000, 0.000000000000000000 ) ) ;
#85070 = ORIENTED_EDGE ( 'NONE', *, *, #156495, .T. ) ;
#85071 = CARTESIAN_POINT ( 'NONE',  ( 22.47071067811865319, 7.720074744509199505, -133.9009075452974002 ) ) ;
#85072 = CARTESIAN_POINT ( 'NONE',  ( -23.15000000000000213, 87.41227409416161720, -106.0231074845242176 ) ) ;
#85073 = AXIS2_PLACEMENT_3D ( 'NONE', #96727, #38091, #199735 ) ;
#85074 = ORIENTED_EDGE ( 'NONE', *, *, #105692, .T. ) ;
#85075 = AXIS2_PLACEMENT_3D ( 'NONE', #238618, #40457, #59954 ) ;
#85076 = DIRECTION ( 'NONE',  ( 1.000000000000000000, 0.000000000000000000, 0.000000000000000000 ) ) ;
#85077 = DIRECTION ( 'NONE',  ( -0.000000000000000000, 0.2617529984165031243, 0.9651348961777157509 ) ) ;
#85078 = AXIS2_PLACEMENT_3D ( 'NONE', #92057, #150760, #51618 ) ;
#85079 = ORIENTED_EDGE ( 'NONE', *, *, #52682, .F. ) ;
#85080 = DIRECTION ( 'NONE',  ( 1.000000000000000000, 0.000000000000000000, 0.000000000000000000 ) ) ;
#85081 = ORIENTED_EDGE ( 'NONE', *, *, #12800, .F. ) ;
#85082 = AXIS2_PLACEMENT_3D ( 'NONE', #74078, #76602, #139108 ) ;
#85085 = EDGE_LOOP ( 'NONE', ( #157150, #128204, #141123, #12459, #180342 ) ) ;
#85084 = EDGE_LOOP ( 'NONE', ( #147634, #54015, #194399 ) ) ;
#85083 = AXIS2_PLACEMENT_3D ( 'NONE', #197640, #58113, #97218 ) ;
#85086 = VERTEX_POINT ( 'NONE', #126326 ) ;
#85087 = CARTESIAN_POINT ( 'NONE',  ( -16.98495255085916611, 65.99443563401777624, -182.6577246907449421 ) ) ;
#85088 = ORIENTED_EDGE ( 'NONE', *, *, #213514, .F. ) ;
#85089 = DIRECTION ( 'NONE',  ( 1.000000000000000000, 0.000000000000000000, 0.000000000000000000 ) ) ;
#85090 = EDGE_LOOP ( 'NONE', ( #14864, #3991, #58893, #24277 ) ) ;
#85091 = DIRECTION ( 'NONE',  ( 0.000000000000000000, 0.2617529984165030132, 0.9651348961777157509 ) ) ;
#85092 = CIRCLE ( 'NONE', #239259, 0.09999999999999939493 ) ;
#85093 = CARTESIAN_POINT ( 'NONE',  ( 20.85000000000000142, 1.115600667400684642E-11, -167.5000000000000284 ) ) ;
#85094 = EDGE_CURVE ( 'NONE', #199662, #191690, #764, .T. ) ;
#85095 = ORIENTED_EDGE ( 'NONE', *, *, #27775, .T. ) ;
#85096 = EDGE_CURVE ( 'NONE', #103624, #158615, #231877, .T. ) ;
#85097 = EDGE_LOOP ( 'NONE', ( #13838, #210589, #155456, #55503 ) ) ;
#85098 = ORIENTED_EDGE ( 'NONE', *, *, #218868, .T. ) ;
#85099 = ADVANCED_FACE ( 'NONE', ( #152348 ), #234404, .F. ) ;
#85100 = ORIENTED_EDGE ( 'NONE', *, *, #106205, .F. ) ;
#85101 = LINE ( 'NONE', #162134, #95894 ) ;
#85104 = ADVANCED_FACE ( 'NONE', ( #36244 ), #15389, .T. ) ;
#85103 = EDGE_LOOP ( 'NONE', ( #55722, #59618, #202928, #168770 ) ) ;
#85102 = DIRECTION ( 'NONE',  ( -1.000000000000000000, 0.000000000000000000, 0.000000000000000000 ) ) ;
#85105 = DIRECTION ( 'NONE',  ( -1.000000000000000000, 0.000000000000000000, -0.000000000000000000 ) ) ;
#85106 = CARTESIAN_POINT ( 'NONE',  ( -20.96077737575350142, 11.62390063401584861, -127.1407919571063729 ) ) ;
#85107 = CARTESIAN_POINT ( 'NONE',  ( -17.04295772865421910, 12.48721732318495548, -211.2269502790635727 ) ) ;
#85108 = DIRECTION ( 'NONE',  ( 0.000000000000000000, -1.000000000000000000, -6.982962677686265922E-15 ) ) ;
#85109 = CARTESIAN_POINT ( 'NONE',  ( 18.54999999999999716, 67.25000000001185185, -93.77310748452437394 ) ) ;
#85110 = CIRCLE ( 'NONE', #35123, 0.09999999999999363565 ) ;
#85112 = CARTESIAN_POINT ( 'NONE',  ( 21.11927991906888025, 6.448493118502572230, -100.4909163205261393 ) ) ;
#85111 = CARTESIAN_POINT ( 'NONE',  ( -23.15000000000000213, 66.21323668544584962, -222.9901119748073484 ) ) ;
#85113 = DIRECTION ( 'NONE',  ( 0.000000000000000000, -1.000000000000000000, -6.982962677686265922E-15 ) ) ;
#85114 = DIRECTION ( 'NONE',  ( 0.000000000000000000, 0.000000000000000000, 1.000000000000000000 ) ) ;
#85115 = CIRCLE ( 'NONE', #64310, 0.1000000000000028783 ) ;
#85116 = ADVANCED_FACE ( 'NONE', ( #71520, #209726 ), #92336, .T. ) ;
#85118 = CARTESIAN_POINT ( 'NONE',  ( 20.94999999999999929, -11.29603075032412640, -197.9521008403361009 ) ) ;
#85117 = CIRCLE ( 'NONE', #110092, 0.09999999999998898659 ) ;
#85119 = ORIENTED_EDGE ( 'NONE', *, *, #232525, .F. ) ;
#85120 = VECTOR ( 'NONE', #103633, 1000.000000000000000 ) ;
#85121 = VECTOR ( 'NONE', #248756, 1000.000000000000114 ) ;
#85123 = ORIENTED_EDGE ( 'NONE', *, *, #166865, .F. ) ;
#85122 = CYLINDRICAL_SURFACE ( 'NONE', #57310, 0.1000000000000028644 ) ;
#85124 = ORIENTED_EDGE ( 'NONE', *, *, #147990, .F. ) ;
#85126 = EDGE_CURVE ( 'NONE', #130475, #240172, #246330, .T. ) ;
#85125 = DIRECTION ( 'NONE',  ( 1.000000000000000000, 0.000000000000000000, 0.000000000000000000 ) ) ;
#85127 =( BOUNDED_SURFACE ( )  B_SPLINE_SURFACE ( 3, 2, ( 
 ( #256758, #100278, #37790 ),
 ( #118607, #18205, #178594 ),
 ( #242374, #101553, #136862 ),
 ( #258050, #79438, #238532 ) ),
 .UNSPECIFIED., .F., .F., .F. ) 
 B_SPLINE_SURFACE_WITH_KNOTS ( ( 4, 4 ),
 ( 3, 3 ),
 ( 0.3000847527772381729, 0.5552748953338751958 ),
 ( 0.000000000000000000, 1.000000000000000000 ),
 .UNSPECIFIED. ) 
 GEOMETRIC_REPRESENTATION_ITEM ( )  RATIONAL_B_SPLINE_SURFACE ( (
 ( 1.000000000000000000, 0.9152888060719349683, 1.000000000000000000),
 ( 1.000000000000000000, 0.9104333467450302919, 1.000000000000000000),
 ( 1.000000000000000000, 0.9035312726220549040, 1.000000000000000000),
 ( 1.000000000000000000, 0.8946697475932153809, 1.000000000000000000) ) ) 
 REPRESENTATION_ITEM ( '' )  SURFACE ( )  );
#85128 = CARTESIAN_POINT ( 'NONE',  ( -16.87331047859649757, 9.950000000011138823, -54.35000000000000142 ) ) ;
#85129 = TOROIDAL_SURFACE ( 'NONE', #80875, 2.699999999999999734, 0.1000000000000000056 ) ;
#85130 = VERTEX_POINT ( 'NONE', #16674 ) ;
#85131 = AXIS2_PLACEMENT_3D ( 'NONE', #226250, #84142, #69795 ) ;
#85132 = AXIS2_PLACEMENT_3D ( 'NONE', #46472, #129864, #69930 ) ;
#85133 = CARTESIAN_POINT ( 'NONE',  ( 18.79999999999999716, 1.901609089591594470, -11.59510167572422112 ) ) ;
#85134 = TOROIDAL_SURFACE ( 'NONE', #189241, 11.65000000000000036, 0.1000000000000000056 ) ;
#85135 = DIRECTION ( 'NONE',  ( -1.000000000000000000, 0.000000000000000000, 0.000000000000000000 ) ) ;
#85136 = ORIENTED_EDGE ( 'NONE', *, *, #92670, .F. ) ;
#85137 = DIRECTION ( 'NONE',  ( 1.000000000000000000, 0.000000000000000000, 0.000000000000000000 ) ) ;
#85138 = CARTESIAN_POINT ( 'NONE',  ( 23.24999999999999645, 67.17743825834517679, -56.87310748452437537 ) ) ;
#85139 = B_SPLINE_CURVE_WITH_KNOTS ( 'NONE', 3,
 ( #181760, #3094, #43540, #123077, #164766, #172519, #109905, #231180, #53800, #132054, #188184, #211600, #92911, #210318 ),
 .UNSPECIFIED., .F., .F.,
 ( 4, 2, 2, 2, 2, 2, 4 ),
 ( 1.040834085586084257E-17, 0.0003823333598417850043, 0.0005735000397626870746, 0.0006690833797231381368, 0.0007168750497033463207, 0.0007407708846934460759, 0.0007646667196835457226 ),
 .UNSPECIFIED. ) ;
#85140 = CARTESIAN_POINT ( 'NONE',  ( -20.85000000000000142, 42.90983634497241894, -254.2202269430244996 ) ) ;
#85141 = CARTESIAN_POINT ( 'NONE',  ( 20.94999999999999574, 6.550000000011159784, -43.34382208968312966 ) ) ;
#85143 = ORIENTED_EDGE ( 'NONE', *, *, #145216, .F. ) ;
#85142 = CARTESIAN_POINT ( 'NONE',  ( 20.94999999999999929, 69.45000000001229523, -157.7731074845244166 ) ) ;
#85144 = AXIS2_PLACEMENT_3D ( 'NONE', #197199, #280, #257128 ) ;
#85145 = DIRECTION ( 'NONE',  ( 1.000000000000000000, -0.000000000000000000, 0.000000000000000000 ) ) ;
#85146 = DIRECTION ( 'NONE',  ( 0.000000000000000000, 0.000000000000000000, -1.000000000000000000 ) ) ;
#85147 = CARTESIAN_POINT ( 'NONE',  ( -20.85000000000000142, 77.16412189325360771, -162.1082593989527254 ) ) ;
#85148 = LINE ( 'NONE', #100849, #25074 ) ;
#85149 = ORIENTED_EDGE ( 'NONE', *, *, #52920, .T. ) ;
#85150 = DIRECTION ( 'NONE',  ( 1.000000000000000000, 0.000000000000000000, 0.000000000000000000 ) ) ;
#85151 = CARTESIAN_POINT ( 'NONE',  ( -23.15000000000000213, 76.00000000001216449, -140.6731074845242802 ) ) ;
#85152 = CIRCLE ( 'NONE', #64353, 0.09999999999999939493 ) ;
#85154 = FACE_BOUND ( 'NONE', #163782, .T. ) ;
#85153 = DIRECTION ( 'NONE',  ( 0.000000000000000000, 0.7397360091702792628, -0.6728971962616790981 ) ) ;
#85155 = FACE_OUTER_BOUND ( 'NONE', #24833, .T. ) ;
#85156 = CARTESIAN_POINT ( 'NONE',  ( -23.15000000000000213, -11.64999999998884483, -155.7499999999999716 ) ) ;
#85157 = LINE ( 'NONE', #227273, #26883 ) ;
#85158 = AXIS2_PLACEMENT_3D ( 'NONE', #248726, #25830, #149642 ) ;
#85160 = ORIENTED_EDGE ( 'NONE', *, *, #253358, .F. ) ;
#85159 = CIRCLE ( 'NONE', #18574, 12.77500000000000391 ) ;
#85161 = EDGE_CURVE ( 'NONE', #32558, #151632, #190171, .T. ) ;
#85162 = DIRECTION ( 'NONE',  ( -1.000000000000000000, 0.000000000000000000, 0.000000000000000000 ) ) ;
#85163 = AXIS2_PLACEMENT_3D ( 'NONE', #138507, #14774, #159401 ) ;
#85164 = ORIENTED_EDGE ( 'NONE', *, *, #143649, .F. ) ;
#85165 = VERTEX_POINT ( 'NONE', #11535 ) ;
#85166 = CARTESIAN_POINT ( 'NONE',  ( -18.59999999999999787, 43.57568952063339651, -245.1784935019914826 ) ) ;
#85167 = DIRECTION ( 'NONE',  ( 0.000000000000000000, -0.9908441862701782288, -0.1350103645450542456 ) ) ;
#85168 = ORIENTED_EDGE ( 'NONE', *, *, #76753, .F. ) ;
#85169 = EDGE_CURVE ( 'NONE', #72626, #54754, #221358, .T. ) ;
#85170 = ORIENTED_EDGE ( 'NONE', *, *, #192729, .F. ) ;
#85171 = ADVANCED_FACE ( 'NONE', ( #131468 ), #252681, .T. ) ;
#85172 =( NAMED_UNIT ( * ) PLANE_ANGLE_UNIT ( ) SI_UNIT ( $, .RADIAN. ) );
#85173 = EDGE_CURVE ( 'NONE', #13347, #106308, #213011, .T. ) ;
#85174 = ORIENTED_EDGE ( 'NONE', *, *, #245933, .F. ) ;
#85175 = FACE_OUTER_BOUND ( 'NONE', #257714, .T. ) ;
#85176 = CIRCLE ( 'NONE', #185364, 0.09999999999999907574 ) ;
#85177 = ORIENTED_EDGE ( 'NONE', *, *, #146951, .F. ) ;
#85178 = CARTESIAN_POINT ( 'NONE',  ( -15.75000000000000355, 9.850000000011133849, -117.2500000000000284 ) ) ;
#85179 = FACE_OUTER_BOUND ( 'NONE', #202101, .T. ) ;
#85180 = CARTESIAN_POINT ( 'NONE',  ( -20.00857864376270001, 63.93636616954134411, -213.0474835168086827 ) ) ;
#85181 = CARTESIAN_POINT ( 'NONE',  ( -18.59999999999999787, -10.64999999999999325, 31.59999999999999787 ) ) ;
#85182 = CARTESIAN_POINT ( 'NONE',  ( -20.94999999999999929, 76.00000000001190870, -103.0231074845243029 ) ) ;
#85183 = AXIS2_PLACEMENT_3D ( 'NONE', #198173, #142047, #221564 ) ;
#85184 = CARTESIAN_POINT ( 'NONE',  ( 21.05000000000000071, 10.72371710471867701, -175.1649135690875880 ) ) ;
#85185 = CARTESIAN_POINT ( 'NONE',  ( -23.15000000000000213, -6.794814075650357665, -212.0940144922642219 ) ) ;
#85187 = ORIENTED_EDGE ( 'NONE', *, *, #47699, .F. ) ;
#85186 = CARTESIAN_POINT ( 'NONE',  ( 21.05000000000000071, 9.765296417674898422, -220.4624455711005737 ) ) ;
#85189 = CARTESIAN_POINT ( 'NONE',  ( -21.14999999999999858, 11.65000000001115588, -100.6000000000000369 ) ) ;
#85188 = CARTESIAN_POINT ( 'NONE',  ( -23.15000000000000213, 86.22912497777053886, -209.4057091359527192 ) ) ;
#85190 = EDGE_CURVE ( 'NONE', #255363, #199581, #229296, .T. ) ;
#85191 = CARTESIAN_POINT ( 'NONE',  ( -22.47071067811865319, 75.90090754530910999, -77.24318222902239484 ) ) ;
#85192 = ORIENTED_EDGE ( 'NONE', *, *, #135401, .T. ) ;
#85193 = FACE_OUTER_BOUND ( 'NONE', #238110, .T. ) ;
#85194 = LINE ( 'NONE', #8280, #202156 ) ;
#85196 = ADVANCED_FACE ( 'NONE', ( #14109 ), #75374, .T. ) ;
#85195 = CARTESIAN_POINT ( 'NONE',  ( -18.40000000000000213, 45.89348038176515843, -239.2231437130149061 ) ) ;
#85197 = VERTEX_POINT ( 'NONE', #151041 ) ;
#85199 = LINE ( 'NONE', #206473, #112430 ) ;
#85198 = DIRECTION ( 'NONE',  ( 0.000000000000000000, 0.2617529984165031243, 0.9651348961777157509 ) ) ;
#85200 = CARTESIAN_POINT ( 'NONE',  ( 21.14999999999999858, 36.75018516840536620, -249.5102790111118338 ) ) ;
#85201 = EDGE_LOOP ( 'NONE', ( #38027, #128983, #214274, #146032, #7569, #172399 ) ) ;
#85202 = AXIS2_PLACEMENT_3D ( 'NONE', #128362, #207915, #25420 ) ;
#85204 = SURFACE_STYLE_USAGE ( .BOTH. , #26575 ) ;
#85203 = AXIS2_PLACEMENT_3D ( 'NONE', #89196, #12262, #74821 ) ;
#85205 = DIRECTION ( 'NONE',  ( 0.000000000000000000, 1.445602896647339410E-16, -1.000000000000000000 ) ) ;
#85206 = EDGE_CURVE ( 'NONE', #30038, #89812, #133889, .T. ) ;
#85207 = CARTESIAN_POINT ( 'NONE',  ( -22.50000000000094147, 0.1008583691097610785, -21.75043287651059387 ) ) ;
#85208 = CARTESIAN_POINT ( 'NONE',  ( -22.60000000000094289, 0.1008583691096561485, -122.2504328765106010 ) ) ;
#85209 = EDGE_CURVE ( 'NONE', #7281, #40759, #17388, .T. ) ;
#85210 = ORIENTED_EDGE ( 'NONE', *, *, #168412, .T. ) ;
#85211 = ADVANCED_FACE ( 'NONE', ( #51903 ), #191476, .F. ) ;
#85212 = VERTEX_POINT ( 'NONE', #93625 ) ;
#85213 = DIRECTION ( 'NONE',  ( 0.000000000000000000, -6.982962677686266711E-15, 1.000000000000000000 ) ) ;
#85214 = CARTESIAN_POINT ( 'NONE',  ( 21.05000000000000426, 10.72371710471867878, -41.09441739161312057 ) ) ;
#85215 = CARTESIAN_POINT ( 'NONE',  ( -23.15000000000000213, 11.65000000001115588, -146.2500000000000284 ) ) ;
#85216 = CARTESIAN_POINT ( 'NONE',  ( -21.05000000000000071, 76.00000000001195133, -103.0231074845243171 ) ) ;
#85217 = CIRCLE ( 'NONE', #197672, 4.300000000000025580 ) ;
#85218 = FACE_OUTER_BOUND ( 'NONE', #29391, .T. ) ;
#85219 = CIRCLE ( 'NONE', #151924, 0.09999999999999939493 ) ;
#85220 = DIRECTION ( 'NONE',  ( 1.000000000000000000, 0.000000000000000000, 0.000000000000000000 ) ) ;
#85222 = EDGE_LOOP ( 'NONE', ( #30220, #35381, #242658, #51794 ) ) ;
#85221 = VECTOR ( 'NONE', #37452, 1000.000000000000114 ) ;
#85223 = CARTESIAN_POINT ( 'NONE',  ( -20.85000000000000142, 65.66751761918668251, -97.42826094061121012 ) ) ;
#85224 = AXIS2_PLACEMENT_3D ( 'NONE', #85296, #146562, #26662 ) ;
#85226 = ORIENTED_EDGE ( 'NONE', *, *, #235456, .F. ) ;
#85225 = CARTESIAN_POINT ( 'NONE',  ( 20.94999999999999574, 65.37642973952952730, -162.5311622812938879 ) ) ;
#85227 = CARTESIAN_POINT ( 'NONE',  ( -21.05000000000000071, 6.497017786443051612, -33.51454569056947008 ) ) ;
#85228 = DIRECTION ( 'NONE',  ( 0.000000000000000000, 1.000000000000000000, 1.224646799147353207E-16 ) ) ;
#85229 = LINE ( 'NONE', #163521, #100402 ) ;
#85231 = CYLINDRICAL_SURFACE ( 'NONE', #205366, 0.1000000000000028644 ) ;
#85230 = MECHANICAL_DESIGN_GEOMETRIC_PRESENTATION_REPRESENTATION (  '', ( #47647 ), #151933 ) ;
#85232 = CYLINDRICAL_SURFACE ( 'NONE', #125622, 0.09999999999998898659 ) ;
#85234 = ORIENTED_EDGE ( 'NONE', *, *, #3911, .F. ) ;
#85233 = DIRECTION ( 'NONE',  ( 1.000000000000000000, 0.000000000000000000, 0.000000000000000000 ) ) ;
#85235 = DIRECTION ( 'NONE',  ( 0.000000000000000000, 1.265107689135680095E-16, -1.000000000000000000 ) ) ;
#85236 = CARTESIAN_POINT ( 'NONE',  ( 18.49999999999999289, 6.450000000011156587, -144.0170271704400307 ) ) ;
#85237 = DIRECTION ( 'NONE',  ( -1.000000000000000000, -0.000000000000000000, -0.000000000000000000 ) ) ;
#85238 = LINE ( 'NONE', #126972, #198950 ) ;
#85239 = ORIENTED_EDGE ( 'NONE', *, *, #82251, .T. ) ;
#85240 = LINE ( 'NONE', #9585, #96970 ) ;
#85241 = CARTESIAN_POINT ( 'NONE',  ( -16.96982749440706328, 66.05000000001201954, -116.1478858933360954 ) ) ;
#85242 = CARTESIAN_POINT ( 'NONE',  ( 22.59999999999999432, 11.74987124438766273, -100.4345704089863602 ) ) ;
#85243 = EDGE_CURVE ( 'NONE', #43971, #118880, #96172, .T. ) ;
#85244 = CARTESIAN_POINT ( 'NONE',  ( -18.59999996769639097, 78.14787437627062161, -231.3748811062230857 ) ) ;
#85245 = TOROIDAL_SURFACE ( 'NONE', #163831, 0.2000000000000000111, 0.1000000000000000056 ) ;
#85246 = ORIENTED_EDGE ( 'NONE', *, *, #90372, .T. ) ;
#85247 = CARTESIAN_POINT ( 'NONE',  ( -16.97683809663752186, 9.950000000011137047, -87.09763598180373378 ) ) ;
#85248 = CIRCLE ( 'NONE', #231054, 0.1000000000000033362 ) ;
#85249 = ORIENTED_EDGE ( 'NONE', *, *, #131215, .F. ) ;
#85250 = AXIS2_PLACEMENT_3D ( 'NONE', #228814, #204086, #149290 ) ;
#85251 = FACE_OUTER_BOUND ( 'NONE', #46750, .T. ) ;
#85252 = DIRECTION ( 'NONE',  ( -1.000000000000000000, 0.000000000000000000, 0.000000000000000000 ) ) ;
#85253 = EDGE_CURVE ( 'NONE', #38706, #89168, #229759, .T. ) ;
#85254 = FILL_AREA_STYLE_COLOUR ( '', #99763 ) ;
#85255 = DIRECTION ( 'NONE',  ( 0.000000000000000000, 0.9876197685951241256, 0.1568667991644932258 ) ) ;
#85256 = ORIENTED_EDGE ( 'NONE', *, *, #242454, .T. ) ;
#85257 = CIRCLE ( 'NONE', #27061, 0.1999999999999987899 ) ;
#85258 = EDGE_CURVE ( 'NONE', #199652, #183080, #54783, .T. ) ;
#85259 = CIRCLE ( 'NONE', #131084, 0.09999999999998898659 ) ;
#85260 = SPHERICAL_SURFACE ( 'NONE', #192026, 0.1000000000000000056 ) ;
#85261 = CIRCLE ( 'NONE', #160346, 0.2000000000000058675 ) ;
#85262 = DIRECTION ( 'NONE',  ( 1.000000000000000000, 0.000000000000000000, 0.000000000000000000 ) ) ;
#85263 = ADVANCED_FACE ( 'NONE', ( #256482 ), #114915, .T. ) ;
#85264 = DIRECTION ( 'NONE',  ( -0.000000000000000000, 0.8814952561688430555, -0.4721928772777346239 ) ) ;
#85265 = AXIS2_PLACEMENT_3D ( 'NONE', #194606, #215417, #155489 ) ;
#85266 = CARTESIAN_POINT ( 'NONE',  ( -23.15000000000000213, 13.98997548377051814, -210.4902890347897255 ) ) ;
#85267 = DIRECTION ( 'NONE',  ( 2.659396599871503635E-15, 0.6132151058540549204, -0.7899159663865520375 ) ) ;
#85268 = ORIENTED_EDGE ( 'NONE', *, *, #60333, .T. ) ;
#85270 = ORIENTED_EDGE ( 'NONE', *, *, #210495, .F. ) ;
#85269 = DIRECTION ( 'NONE',  ( 0.000000000000000000, 0.000000000000000000, 1.000000000000000000 ) ) ;
#85271 = EDGE_CURVE ( 'NONE', #22402, #46601, #117342, .T. ) ;
#85272 = CIRCLE ( 'NONE', #235157, 0.09999999999999939493 ) ;
#85273 = ORIENTED_EDGE ( 'NONE', *, *, #240855, .F. ) ;
#85274 = DIRECTION ( 'NONE',  ( 1.000000000000000000, 0.000000000000000000, 0.000000000000000000 ) ) ;
#85275 = ADVANCED_FACE ( 'NONE', ( #902 ), #161316, .T. ) ;
#85276 = ORIENTED_EDGE ( 'NONE', *, *, #94094, .F. ) ;
#85277 = DIRECTION ( 'NONE',  ( -0.000000000000000000, 0.1298341882520009927, 0.9915357197604854900 ) ) ;
#85278 = AXIS2_PLACEMENT_3D ( 'NONE', #210696, #109013, #94592 ) ;
#85279 = DIRECTION ( 'NONE',  ( 0.000000000000000000, 0.000000000000000000, 1.000000000000000000 ) ) ;
#85280 = CARTESIAN_POINT ( 'NONE',  ( -23.15000000000000213, 87.48912529308822172, -139.6231074845242688 ) ) ;
#85281 = ORIENTED_EDGE ( 'NONE', *, *, #225939, .T. ) ;
#85283 = VECTOR ( 'NONE', #22893, 1000.000000000000000 ) ;
#85282 = DIRECTION ( 'NONE',  ( 0.000000000000000000, -1.000000000000000000, 0.000000000000000000 ) ) ;
#85284 = DIRECTION ( 'NONE',  ( 0.000000000000000000, 7.026728003956683390E-15, -1.000000000000000000 ) ) ;
#85285 = DIRECTION ( 'NONE',  ( 0.000000000000000000, -0.9126074666063771490, -0.4088369013363281623 ) ) ;
#85286 = AXIS2_PLACEMENT_3D ( 'NONE', #178392, #132834, #192804 ) ;
#85287 = VERTEX_POINT ( 'NONE', #200427 ) ;
#85288 = FACE_OUTER_BOUND ( 'NONE', #52109, .T. ) ;
#85290 = ORIENTED_EDGE ( 'NONE', *, *, #174157, .T. ) ;
#85289 = FACE_OUTER_BOUND ( 'NONE', #99831, .T. ) ;
#85291 = DIRECTION ( 'NONE',  ( -1.000000000000000000, -0.000000000000000000, -0.000000000000000000 ) ) ;
#85292 = FACE_OUTER_BOUND ( 'NONE', #16483, .T. ) ;
#85293 = EDGE_CURVE ( 'NONE', #6683, #141753, #233867, .T. ) ;
#85294 = EDGE_CURVE ( 'NONE', #153656, #229115, #62204, .T. ) ;
#85295 = ORIENTED_EDGE ( 'NONE', *, *, #82764, .T. ) ;
#85296 = CARTESIAN_POINT ( 'NONE',  ( 20.94999999999999929, 76.00000000001244871, -170.0231074845243597 ) ) ;
#85297 = CARTESIAN_POINT ( 'NONE',  ( -18.35668295345803713, 11.47316190336247388, -24.25000000000001066 ) ) ;
#85298 = CARTESIAN_POINT ( 'NONE',  ( 21.05000000000000071, 39.17763777304804762, -236.9343730377117083 ) ) ;
#85299 = ORIENTED_EDGE ( 'NONE', *, *, #177498, .F. ) ;
#85300 = DIRECTION ( 'NONE',  ( 1.186688945009010077E-16, -1.000000000000000000, -0.000000000000000000 ) ) ;
#85301 = ADVANCED_FACE ( 'NONE', ( #177040 ), #59036, .T. ) ;
#85302 = FACE_OUTER_BOUND ( 'NONE', #210605, .T. ) ;
#85303 = CIRCLE ( 'NONE', #64494, 0.1000000000000054040 ) ;
#85304 = ORIENTED_EDGE ( 'NONE', *, *, #77210, .T. ) ;
#85305 = EDGE_CURVE ( 'NONE', #158625, #192232, #221251, .T. ) ;
#85306 = VECTOR ( 'NONE', #62296, 1000.000000000000227 ) ;
#85307 = TOROIDAL_SURFACE ( 'NONE', #205959, 0.2000000000000000111, 0.1000000000000000056 ) ;
#85308 = EDGE_CURVE ( 'NONE', #228375, #2313, #208912, .T. ) ;
#85309 = ORIENTED_EDGE ( 'NONE', *, *, #26937, .T. ) ;
#85310 = CARTESIAN_POINT ( 'NONE',  ( -20.94999999999999929, 76.00000000001142553, -36.02310748452432421 ) ) ;
#85311 = CIRCLE ( 'NONE', #81223, 0.1000000000000099282 ) ;
#85312 = EDGE_CURVE ( 'NONE', #245959, #209103, #80433, .T. ) ;
#85313 = AXIS2_PLACEMENT_3D ( 'NONE', #159310, #217951, #98000 ) ;
#85314 = EDGE_LOOP ( 'NONE', ( #77752, #37433, #34257, #141770 ) ) ;
#85315 = CARTESIAN_POINT ( 'NONE',  ( 18.39999999999997371, 11.47316190337362940, -91.25000000000005684 ) ) ;
#85316 = DIRECTION ( 'NONE',  ( 0.000000000000000000, 0.000000000000000000, 1.000000000000000000 ) ) ;
#85318 = ORIENTED_EDGE ( 'NONE', *, *, #75132, .F. ) ;
#85317 = CARTESIAN_POINT ( 'NONE',  ( -16.87683809663753465, 9.864913778549572854, -147.2757156356385622 ) ) ;
#85319 = CARTESIAN_POINT ( 'NONE',  ( 20.99551997958415583, 11.75000000001125144, -127.1516591376888954 ) ) ;
#85320 = CARTESIAN_POINT ( 'NONE',  ( -23.39999999999994529, 77.75000000001119815, -47.64205752314703801 ) ) ;
#85321 = DIRECTION ( 'NONE',  ( 0.000000000000000000, 0.9770955615653259541, 0.2128009952263860971 ) ) ;
#85322 = CARTESIAN_POINT ( 'NONE',  ( 21.05000000000000071, 76.00000000001126921, -203.5231074845248997 ) ) ;
#85323 = DIRECTION ( 'NONE',  ( 0.000000000000000000, 0.4999999999999088507, -0.8660254037844913322 ) ) ;
#85324 = EDGE_CURVE ( 'NONE', #92189, #237605, #4867, .T. ) ;
#85325 = CARTESIAN_POINT ( 'NONE',  ( -18.44362607810620602, 85.49049615809693137, -129.4651536176771174 ) ) ;
#85326 = CIRCLE ( 'NONE', #139507, 12.87499999999999822 ) ;
#85327 = CARTESIAN_POINT ( 'NONE',  ( -22.50000000000000000, 76.00000000001213607, -136.5231074845242745 ) ) ;
#85328 = CARTESIAN_POINT ( 'NONE',  ( -18.40000000000000213, -9.499999999988851584, -107.5320693966996970 ) ) ;
#85330 = VERTEX_POINT ( 'NONE', #23095 ) ;
#85329 = DIRECTION ( 'NONE',  ( 1.000000000000000000, 7.304098846218134667E-16, 0.000000000000000000 ) ) ;
#85331 = DIRECTION ( 'NONE',  ( -0.000000000000000000, -0.000000000000000000, -1.000000000000000000 ) ) ;
#85332 = TOROIDAL_SURFACE ( 'NONE', #47925, 0.2000000000000000111, 0.1000000000000000056 ) ;
#85333 = EDGE_LOOP ( 'NONE', ( #233755, #136063, #243372, #102422 ) ) ;
#85334 = LINE ( 'NONE', #124500, #230730 ) ;
#85335 = CARTESIAN_POINT ( 'NONE',  ( -18.59999999999999787, -1.835859311432481045, -212.5044391687984842 ) ) ;
#85336 = CARTESIAN_POINT ( 'NONE',  ( 11.60000000000000142, -8.250000000000005329, 10.95857864376269575 ) ) ;
#85337 = AXIS2_PLACEMENT_3D ( 'NONE', #207031, #208331, #89628 ) ;
#85338 = CARTESIAN_POINT ( 'NONE',  ( 20.59588692710267921, 65.63127657884351152, -195.8840263900140144 ) ) ;
#85339 = LINE ( 'NONE', #65804, #122309 ) ;
#85340 = VERTEX_POINT ( 'NONE', #156195 ) ;
#85341 = CARTESIAN_POINT ( 'NONE',  ( -22.59080734064477625, 64.25000000001165290, -69.55385719262143596 ) ) ;
#85342 = CARTESIAN_POINT ( 'NONE',  ( -23.15000000000000213, 85.50000000001179501, -79.41707660717668205 ) ) ;
#85343 = VERTEX_POINT ( 'NONE', #118335 ) ;
#85344 = CIRCLE ( 'NONE', #193721, 0.2000000000000057288 ) ;
#85345 = CARTESIAN_POINT ( 'NONE',  ( 21.07928932188134397, 75.90110485435809551, -209.8516241409230645 ) ) ;
#85346 = AXIS2_PLACEMENT_3D ( 'NONE', #69288, #127968, #87530 ) ;
#85347 = CARTESIAN_POINT ( 'NONE',  ( -16.94225986326251032, 61.01702495231255341, -220.7553535118148602 ) ) ;
#85348 = ORIENTED_EDGE ( 'NONE', *, *, #231016, .T. ) ;
#85349 = ADVANCED_FACE ( 'NONE', ( #4776 ), #105291, .F. ) ;
#85350 = DIRECTION ( 'NONE',  ( -1.000000000000000000, 0.000000000000000000, 0.000000000000000000 ) ) ;
#85351 = ORIENTED_EDGE ( 'NONE', *, *, #94074, .F. ) ;
#85352 = CARTESIAN_POINT ( 'NONE',  ( -21.55000000000000426, 7.708578643773852157, -188.6499999999999488 ) ) ;
#85353 = ORIENTED_EDGE ( 'NONE', *, *, #216028, .F. ) ;
#85354 = CARTESIAN_POINT ( 'NONE',  ( 18.52928932188133970, 55.04340642595498423, -230.0514932066152198 ) ) ;
#85355 = CARTESIAN_POINT ( 'NONE',  ( 13.54556439290363912, 9.450592112144859058, -182.5561883188083527 ) ) ;
#85356 = ORIENTED_EDGE ( 'NONE', *, *, #129430, .F. ) ;
#85357 = CARTESIAN_POINT ( 'NONE',  ( 18.59999999999999076, 7.120270961708750512, -204.6595630418393057 ) ) ;
#85359 = ORIENTED_EDGE ( 'NONE', *, *, #65866, .F. ) ;
#85358 = SURFACE_STYLE_USAGE ( .BOTH. , #167530 ) ;
#85360 = ADVANCED_FACE ( 'NONE', ( #64910 ), #70086, .T. ) ;
#85361 = DIRECTION ( 'NONE',  ( 0.000000000000000000, -0.2128009952263628934, 0.9770955615653310611 ) ) ;
#85362 = CIRCLE ( 'NONE', #118742, 0.1999999999999987899 ) ;
#85363 = ORIENTED_EDGE ( 'NONE', *, *, #15282, .T. ) ;
#85364 = VECTOR ( 'NONE', #15400, 1000.000000000000114 ) ;
#85365 = VERTEX_POINT ( 'NONE', #128758 ) ;
#85366 = DIRECTION ( 'NONE',  ( 0.000000000000000000, 0.4088369013363149507, -0.9126074666063829222 ) ) ;
#85367 = DIRECTION ( 'NONE',  ( -0.000000000000000000, 1.000000000000000000, -0.000000000000000000 ) ) ;
#85368 = CARTESIAN_POINT ( 'NONE',  ( -20.54999999999999716, 7.150000000000000355, -12.34999999999999964 ) ) ;
#85369 = CARTESIAN_POINT ( 'NONE',  ( -23.15000000000000213, 85.00000000001261924, -193.6291383618718385 ) ) ;
#85370 = DIRECTION ( 'NONE',  ( 0.000000000000000000, 0.000000000000000000, 1.000000000000000000 ) ) ;
#85371 = DIRECTION ( 'NONE',  ( 0.000000000000000000, 1.000000000000000000, 0.000000000000000000 ) ) ;
#85372 = VERTEX_POINT ( 'NONE', #104018 ) ;
#85373 = DIRECTION ( 'NONE',  ( 1.000000000000000000, 0.000000000000000000, 0.000000000000000000 ) ) ;
#85374 = CARTESIAN_POINT ( 'NONE',  ( 18.54999999999999716, 67.25000000001229239, -160.7731074845244166 ) ) ;
#85375 = LINE ( 'NONE', #204067, #211863 ) ;
#85376 = FACE_OUTER_BOUND ( 'NONE', #26019, .T. ) ;
#85377 = VERTEX_POINT ( 'NONE', #183591 ) ;
#85378 = CARTESIAN_POINT ( 'NONE',  ( 20.94999999999999929, 68.00366762990589109, -224.2307594727497815 ) ) ;
#85379 = ORIENTED_EDGE ( 'NONE', *, *, #252188, .T. ) ;
#85380 = CARTESIAN_POINT ( 'NONE',  ( -21.05000000000000071, 64.25000000001176659, -76.53791325517833855 ) ) ;
#85381 = EDGE_LOOP ( 'NONE', ( #172428, #170841, #139634, #190508, #228299, #182750, #165109, #178043, #11753, #197539, #121949 ) ) ;
#85382 = VECTOR ( 'NONE', #92156, 1000.000000000000000 ) ;
#85383 = CIRCLE ( 'NONE', #206048, 0.5999999999999978684 ) ;
#85384 = CARTESIAN_POINT ( 'NONE',  ( -15.06774609480955540, 25.11447974268060435, -232.6833957968052005 ) ) ;
#85385 = CARTESIAN_POINT ( 'NONE',  ( -23.25000000000000000, 38.51006445970392633, -250.5427677435266389 ) ) ;
#85386 = ORIENTED_EDGE ( 'NONE', *, *, #2790, .F. ) ;
#85388 = ORIENTED_EDGE ( 'NONE', *, *, #186854, .F. ) ;
#85387 = CARTESIAN_POINT ( 'NONE',  ( 23.14999999999999858, 87.75000000001246292, -181.7731074845242745 ) ) ;
#85389 = DIRECTION ( 'NONE',  ( -1.000000000000000000, -0.000000000000000000, -0.000000000000000000 ) ) ;
#85390 = ORIENTED_EDGE ( 'NONE', *, *, #62978, .T. ) ;
#85391 = CARTESIAN_POINT ( 'NONE',  ( -20.54999999999999716, 1.999999999999998224, -20.27537807723789953 ) ) ;
#85392 = ADVANCED_FACE ( 'NONE', ( #68778 ), #8805, .F. ) ;
#85393 = CARTESIAN_POINT ( 'NONE',  ( -18.57399277249657032, 65.66887361445314752, -63.93298459182690863 ) ) ;
#85394 = EDGE_LOOP ( 'NONE', ( #56165, #10170, #236336 ) ) ;
#85395 = LINE ( 'NONE', #106261, #193615 ) ;
#85396 = EDGE_CURVE ( 'NONE', #173670, #232908, #28405, .T. ) ;
#85398 = DIRECTION ( 'NONE',  ( 0.000000000000000000, -0.4721928772776973204, -0.8814952561688629284 ) ) ;
#85397 = AXIS2_PLACEMENT_3D ( 'NONE', #55551, #135108, #214656 ) ;
#85399 = VECTOR ( 'NONE', #209801, 1000.000000000000114 ) ;
#85400 = ORIENTED_EDGE ( 'NONE', *, *, #122167, .F. ) ;
#85401 = CIRCLE ( 'NONE', #6331, 0.1000000000000013933 ) ;
#85402 = DIRECTION ( 'NONE',  ( 0.000000000000000000, 0.000000000000000000, 1.000000000000000000 ) ) ;
#85403 = PRESENTATION_LAYER_ASSIGNMENT (  '', '', ( #1851 ) ) ;
#85404 = EDGE_CURVE ( 'NONE', #171512, #129596, #117516, .T. ) ;
#85405 = EDGE_CURVE ( 'NONE', #68443, #246745, #134067, .T. ) ;
#85406 = DIRECTION ( 'NONE',  ( 0.000000000000000000, 1.000000000000000000, 0.000000000000000000 ) ) ;
#85408 = ORIENTED_EDGE ( 'NONE', *, *, #145237, .F. ) ;
#85407 = DIRECTION ( 'NONE',  ( 1.000000000000000000, 0.000000000000000000, 0.000000000000000000 ) ) ;
#85409 = FACE_OUTER_BOUND ( 'NONE', #41805, .T. ) ;
#85410 = CARTESIAN_POINT ( 'NONE',  ( -22.49917693094574389, 75.91477003579007032, -81.17290326905498432 ) ) ;
#85411 = DIRECTION ( 'NONE',  ( 0.7071067811865388020, -0.7071067811865561215, 0.000000000000000000 ) ) ;
#85413 = DIRECTION ( 'NONE',  ( 0.000000000000000000, 0.4721928772777346239, 0.8814952561688430555 ) ) ;
#85412 = DIRECTION ( 'NONE',  ( 0.000000000000000000, 0.000000000000000000, 1.000000000000000000 ) ) ;
#85414 = CARTESIAN_POINT ( 'NONE',  ( -20.85882249326303040, 65.66751761918722252, -164.4282609406112670 ) ) ;
#85415 = FACE_OUTER_BOUND ( 'NONE', #204158, .T. ) ;
#85416 = EDGE_CURVE ( 'NONE', #169843, #224621, #9189, .T. ) ;
#85417 = CARTESIAN_POINT ( 'NONE',  ( -21.45000000000000284, 7.708578643773852157, -79.35000000000005116 ) ) ;
#85418 = CARTESIAN_POINT ( 'NONE',  ( -23.15000000000000213, 2.500000000011156409, -180.7246219227620543 ) ) ;
#85419 = CIRCLE ( 'NONE', #102174, 11.69999999999998863 ) ;
#85420 = EDGE_LOOP ( 'NONE', ( #46642, #2656, #13949, #209618, #238159 ) ) ;
#85421 = CIRCLE ( 'NONE', #197881, 0.8750000000000007772 ) ;
#85422 = VECTOR ( 'NONE', #109029, 1000.000000000000000 ) ;
#85423 = EDGE_LOOP ( 'NONE', ( #222007, #174959, #78142, #256784 ) ) ;
#85424 = CARTESIAN_POINT ( 'NONE',  ( 21.05000000000000071, -10.76604040606816959, -206.3127087229280789 ) ) ;
#85425 = ORIENTED_EDGE ( 'NONE', *, *, #221941, .F. ) ;
#85426 = EDGE_CURVE ( 'NONE', #151457, #7914, #138335, .T. ) ;
#85427 = CARTESIAN_POINT ( 'NONE',  ( -16.87383368123029825, 9.950000000011138823, -146.6500000000000341 ) ) ;
#85428 = AXIS2_PLACEMENT_3D ( 'NONE', #133435, #212970, #176435 ) ;
#85429 = AXIS2_PLACEMENT_3D ( 'NONE', #110337, #96853, #170370 ) ;
#85430 = AXIS2_PLACEMENT_3D ( 'NONE', #175282, #236493, #237788 ) ;
#85431 = ORIENTED_EDGE ( 'NONE', *, *, #215235, .T. ) ;
#85432 = FILL_AREA_STYLE ('',( #30661 ) ) ;
#85433 = CARTESIAN_POINT ( 'NONE',  ( -23.15000000000000213, 67.23127455305835554, -235.8551265064784559 ) ) ;
#85434 = EDGE_LOOP ( 'NONE', ( #158145, #79521, #105949, #190950 ) ) ;
#85435 = CARTESIAN_POINT ( 'NONE',  ( -23.25000000000000000, -1.835859311432481045, -179.0044391687985410 ) ) ;
#85436 = EDGE_LOOP ( 'NONE', ( #207221, #716, #112715, #31256 ) ) ;
#85437 = ORIENTED_EDGE ( 'NONE', *, *, #105061, .F. ) ;
#85439 = CARTESIAN_POINT ( 'NONE',  ( 21.14999999999999858, 1.148907358139439339E-11, -201.0000000000015064 ) ) ;
#85438 = AXIS2_PLACEMENT_3D ( 'NONE', #2003, #45001, #123255 ) ;
#85440 = DIRECTION ( 'NONE',  ( 1.000000000000000000, -0.000000000000000000, 0.000000000000000000 ) ) ;
#85442 = ORIENTED_EDGE ( 'NONE', *, *, #122153, .T. ) ;
#85441 = DIRECTION ( 'NONE',  ( 0.000000000000000000, -0.1332476588733448597, 0.9910827722268067408 ) ) ;
#85443 = AXIS2_PLACEMENT_3D ( 'NONE', #100770, #142497, #216901 ) ;
#85444 = CARTESIAN_POINT ( 'NONE',  ( 20.92356734117541706, 65.68026841930900162, -97.47257401318893244 ) ) ;
#85446 = ORIENTED_EDGE ( 'NONE', *, *, #95479, .T. ) ;
#85445 = CYLINDRICAL_SURFACE ( 'NONE', #22654, 0.09999999999999939493 ) ;
#85447 = CARTESIAN_POINT ( 'NONE',  ( 20.85000000000000142, 18.60970618848721259, -231.2322896185303875 ) ) ;
#85448 = CIRCLE ( 'NONE', #93872, 1.749999999999999778 ) ;
#85449 = DIRECTION ( 'NONE',  ( -0.000000000000000000, 0.000000000000000000, -1.000000000000000000 ) ) ;
#85450 = CIRCLE ( 'NONE', #231273, 0.09999999999999441280 ) ;
#85453 = EDGE_CURVE ( 'NONE', #113415, #213775, #239731, .T. ) ;
#85452 = VERTEX_POINT ( 'NONE', #87024 ) ;
#85451 = DIRECTION ( 'NONE',  ( -1.000000000000000000, 0.000000000000000000, -0.000000000000000000 ) ) ;
#85454 = CARTESIAN_POINT ( 'NONE',  ( -20.54999999999999716, 76.00000000001190870, -103.0231074845243029 ) ) ;
#85455 = CARTESIAN_POINT ( 'NONE',  ( -15.51798037960204724, 27.09559348180860283, -233.7911270184622197 ) ) ;
#85456 = DIRECTION ( 'NONE',  ( 0.000000000000000000, -0.1568667991644355497, 0.9876197685951332295 ) ) ;
#85458 = CARTESIAN_POINT ( 'NONE',  ( -21.08479644141222664, 69.65496134228079939, -203.5816619270885610 ) ) ;
#85457 = DIRECTION ( 'NONE',  ( 0.000000000000000000, -0.9770955615653317272, -0.2128009952263598126 ) ) ;
#85459 = CARTESIAN_POINT ( 'NONE',  ( 18.50000000000189360, 10.44006789215571551, -91.76711774888565287 ) ) ;
#85460 = CARTESIAN_POINT ( 'NONE',  ( -18.59999999999999787, 11.65000000001115232, -155.7499999999999716 ) ) ;
#85461 = FACE_OUTER_BOUND ( 'NONE', #185189, .T. ) ;
#85462 = DIRECTION ( 'NONE',  ( 0.000000000000000000, 1.000000000000000000, 0.000000000000000000 ) ) ;
#85463 = ORIENTED_EDGE ( 'NONE', *, *, #145662, .T. ) ;
#85464 = ORIENTED_EDGE ( 'NONE', *, *, #104113, .F. ) ;
#85465 = VERTEX_POINT ( 'NONE', #169189 ) ;
#85466 = EDGE_CURVE ( 'NONE', #75563, #160332, #147008, .T. ) ;
#85467 = DIRECTION ( 'NONE',  ( 0.000000000000000000, -6.938893903907030216E-14, 1.000000000000000000 ) ) ;
#85468 = VERTEX_POINT ( 'NONE', #149619 ) ;
#85469 = DIRECTION ( 'NONE',  ( -0.000000000000000000, -0.1350103645451876666, 0.9908441862701600211 ) ) ;
#85470 = ORIENTED_EDGE ( 'NONE', *, *, #189221, .F. ) ;
#85471 = LINE ( 'NONE', #141633, #206732 ) ;
#85472 = DIRECTION ( 'NONE',  ( 0.000000000000000000, 0.000000000000000000, -1.000000000000000000 ) ) ;
#85473 = EDGE_CURVE ( 'NONE', #119594, #168638, #25950, .T. ) ;
#85474 = AXIS2_PLACEMENT_3D ( 'NONE', #124801, #6109, #25696 ) ;
#85475 = VERTEX_POINT ( 'NONE', #49206 ) ;
#85476 = CARTESIAN_POINT ( 'NONE',  ( 15.39170923737819585, 9.389529397477897277, -151.8171079128937890 ) ) ;
#85477 = ADVANCED_FACE ( 'NONE', ( #29679 ), #203146, .T. ) ;
#85478 = AXIS2_PLACEMENT_3D ( 'NONE', #11631, #12925, #209816 ) ;
#85479 = VERTEX_POINT ( 'NONE', #50463 ) ;
#85480 = VERTEX_POINT ( 'NONE', #47911 ) ;
#85481 = VERTEX_POINT ( 'NONE', #24536 ) ;
#85482 = AXIS2_PLACEMENT_3D ( 'NONE', #234866, #36694, #56198 ) ;
#85483 = DIRECTION ( 'NONE',  ( 0.7071067811865460184, 0.6824534298470606997, -0.1850873201761399356 ) ) ;
#85484 = LINE ( 'NONE', #244590, #11807 ) ;
#85485 = DIRECTION ( 'NONE',  ( 1.000000000000000000, -0.000000000000000000, -0.000000000000000000 ) ) ;
#85486 = CARTESIAN_POINT ( 'NONE',  ( 13.88638282980483751, 27.90226189425599657, -234.1316127586029836 ) ) ;
#85487 = CARTESIAN_POINT ( 'NONE',  ( -21.05000000000000071, 5.850000000011108092, -177.6324972242779268 ) ) ;
#85488 = DIRECTION ( 'NONE',  ( -0.000000000000000000, -1.000000000000000000, 6.308085367188393199E-16 ) ) ;
#85489 = EDGE_CURVE ( 'NONE', #85754, #12539, #171711, .T. ) ;
#85491 = DIRECTION ( 'NONE',  ( 0.000000000000000000, -7.304098846218085561E-15, 1.000000000000000000 ) ) ;
#85490 = FACE_OUTER_BOUND ( 'NONE', #253593, .T. ) ;
#85493 = ORIENTED_EDGE ( 'NONE', *, *, #209862, .F. ) ;
#85492 = CARTESIAN_POINT ( 'NONE',  ( -20.87600722750343252, 10.33112638556969465, -139.5901228926975080 ) ) ;
#85495 = CARTESIAN_POINT ( 'NONE',  ( -18.39999999999999858, 77.17949092533254429, -241.9177572069595783 ) ) ;
#85494 = DIRECTION ( 'NONE',  ( -1.000000000000000000, -2.952720810173289112E-16, 0.000000000000000000 ) ) ;
#85496 = CARTESIAN_POINT ( 'NONE',  ( -20.94999999999999929, 55.59258605799641373, -234.6589115948038966 ) ) ;
#85497 = AXIS2_PLACEMENT_3D ( 'NONE', #17468, #38333, #197382 ) ;
#85498 = EDGE_LOOP ( 'NONE', ( #217762, #13337, #206993, #174178 ) ) ;
#85499 = CARTESIAN_POINT ( 'NONE',  ( 20.95568717954149562, 10.60199405390297400, -74.60250836826870113 ) ) ;
#85500 = VECTOR ( 'NONE', #84509, 1000.000000000000000 ) ;
#85501 = CARTESIAN_POINT ( 'NONE',  ( 21.14999999999999858, 76.00000000001271871, -210.0637644362255969 ) ) ;
#85503 = EDGE_CURVE ( 'NONE', #228920, #109505, #107895, .T. ) ;
#85502 = CARTESIAN_POINT ( 'NONE',  ( 19.75857864376269291, 64.35000000001147669, -44.77310748452440947 ) ) ;
#85505 = EDGE_CURVE ( 'NONE', #118818, #177703, #253812, .T. ) ;
#85504 = ORIENTED_EDGE ( 'NONE', *, *, #123280, .T. ) ;
#85506 = CIRCLE ( 'NONE', #181430, 0.1000000000000026840 ) ;
#85507 = DIRECTION ( 'NONE',  ( -1.000000000000000000, 0.000000000000000000, 0.000000000000000000 ) ) ;
#85508 = CARTESIAN_POINT ( 'NONE',  ( -23.25000000000000000, 73.40000000001205649, -123.2984855617622202 ) ) ;
#85509 = DIRECTION ( 'NONE',  ( 0.000000000000000000, 0.000000000000000000, -1.000000000000000000 ) ) ;
#85510 = ORIENTED_EDGE ( 'NONE', *, *, #246527, .F. ) ;
#85511 = ORIENTED_EDGE ( 'NONE', *, *, #226088, .F. ) ;
#85512 = EDGE_CURVE ( 'NONE', #211510, #251815, #170496, .T. ) ;
#85513 = FACE_OUTER_BOUND ( 'NONE', #156121, .T. ) ;
#85514 = VERTEX_POINT ( 'NONE', #233007 ) ;
#85515 = CARTESIAN_POINT ( 'NONE',  ( 21.46681500593265568, 6.857511159395777156, -67.00000000000004263 ) ) ;
#85516 = CARTESIAN_POINT ( 'NONE',  ( -18.43459694179555441, -9.494210124986889099, -174.1170052026611188 ) ) ;
#85517 = AXIS2_PLACEMENT_3D ( 'NONE', #95675, #134787, #99508 ) ;
#85518 = DIRECTION ( 'NONE',  ( 1.000000000000000000, 0.000000000000000000, 0.000000000000000000 ) ) ;
#85520 = EDGE_CURVE ( 'NONE', #18414, #51864, #142456, .T. ) ;
#85519 = FACE_OUTER_BOUND ( 'NONE', #214031, .T. ) ;
#85521 = ORIENTED_EDGE ( 'NONE', *, *, #249770, .F. ) ;
#85522 = EDGE_CURVE ( 'NONE', #241513, #251180, #213403, .T. ) ;
#85523 = CARTESIAN_POINT ( 'NONE',  ( -13.11924609551134857, 9.431689550535258704, -118.7792900322360907 ) ) ;
#85524 = DIRECTION ( 'NONE',  ( -1.000000000000000000, -0.000000000000000000, -0.000000000000000000 ) ) ;
#85525 = AXIS2_PLACEMENT_3D ( 'NONE', #223065, #126546, #44453 ) ;
#85526 = EDGE_LOOP ( 'NONE', ( #167870, #196296, #230606, #183637, #16996 ) ) ;
#85527 = AXIS2_PLACEMENT_3D ( 'NONE', #118023, #97132, #217102 ) ;
#85528 = CARTESIAN_POINT ( 'NONE',  ( 20.94999675878240808, 10.29307482167955357, -38.95864214669402514 ) ) ;
#85530 = VERTEX_POINT ( 'NONE', #252530 ) ;
#85529 = CARTESIAN_POINT ( 'NONE',  ( -20.85000000000000142, 77.14957036958807635, -162.2071950000224092 ) ) ;
#85531 = EDGE_CURVE ( 'NONE', #247198, #221706, #150874, .T. ) ;
#85532 = CARTESIAN_POINT ( 'NONE',  ( 21.05000000000000071, 6.650000000011155876, -177.3438220896830728 ) ) ;
#85533 = CYLINDRICAL_SURFACE ( 'NONE', #82006, 0.09999999999999867328 ) ;
#85534 = ADVANCED_FACE ( 'NONE', ( #130007 ), #80058, .F. ) ;
#85535 = CARTESIAN_POINT ( 'NONE',  ( -16.87036670365548474, 9.989418819312801290, -87.97956011730209980 ) ) ;
#85536 = CYLINDRICAL_SURFACE ( 'NONE', #150500, 0.5000000000000004441 ) ;
#85537 = DIRECTION ( 'NONE',  ( 0.000000000000000000, -0.9394191166662618775, -0.3427706569150580362 ) ) ;
#85538 = CARTESIAN_POINT ( 'NONE',  ( -21.14999999999999858, 87.65000000001195701, -103.0231074845242318 ) ) ;
#85539 = ORIENTED_EDGE ( 'NONE', *, *, #92786, .F. ) ;
#85540 = LINE ( 'NONE', #28212, #117851 ) ;
#85541 = LINE ( 'NONE', #206816, #35942 ) ;
#85542 = DIRECTION ( 'NONE',  ( -0.000000000000000000, 6.982962677686266711E-15, -1.000000000000000000 ) ) ;
#85543 = ADVANCED_FACE ( 'NONE', ( #234251 ), #193864, .F. ) ;
#85544 = CIRCLE ( 'NONE', #164702, 3.899999999999996803 ) ;
#85545 = DIRECTION ( 'NONE',  ( 0.000000000000000000, 0.000000000000000000, -1.000000000000000000 ) ) ;
#85546 = DIRECTION ( 'NONE',  ( 0.000000000000000000, 1.000000000000000000, 6.982962677686266711E-15 ) ) ;
#85547 = EDGE_LOOP ( 'NONE', ( #40298, #257852, #138003 ) ) ;
#85548 = ORIENTED_EDGE ( 'NONE', *, *, #246349, .T. ) ;
#85549 = DIRECTION ( 'NONE',  ( 0.000000000000000000, -0.4721928772777331251, -0.8814952561688439436 ) ) ;
#85551 = SPHERICAL_SURFACE ( 'NONE', #105469, 0.1000000000000000056 ) ;
#85550 = CIRCLE ( 'NONE', #243813, 0.1000000000000028644 ) ;
#85552 = CARTESIAN_POINT ( 'NONE',  ( 20.95000000000000284, 17.04749343158541919, -224.5908524457890678 ) ) ;
#85553 = CARTESIAN_POINT ( 'NONE',  ( -23.15000000000000213, 67.23127455305841238, -235.8551265064783991 ) ) ;
#85554 = DIRECTION ( 'NONE',  ( -0.000000000000000000, -0.000000000000000000, -1.000000000000000000 ) ) ;
#85555 = EDGE_CURVE ( 'NONE', #10156, #2919, #30965, .T. ) ;
#85556 = CARTESIAN_POINT ( 'NONE',  ( -21.05000000000000071, -1.851028230129704522, -179.1539132694224463 ) ) ;
#85557 = CARTESIAN_POINT ( 'NONE',  ( -20.96077737575358668, 17.02684875966442846, -224.5570219545468262 ) ) ;
#85558 = EDGE_CURVE ( 'NONE', #126259, #21323, #229944, .T. ) ;
#85559 = CIRCLE ( 'NONE', #152275, 0.09999999999998898659 ) ;
#85560 = STYLED_ITEM ( 'NONE', ( #106722 ), #198479 ) ;
#85561 = ORIENTED_EDGE ( 'NONE', *, *, #95234, .F. ) ;
#85562 = DIRECTION ( 'NONE',  ( -0.000000000000000000, -6.982962677686266711E-15, 1.000000000000000000 ) ) ;
#85563 = EDGE_CURVE ( 'NONE', #82975, #23626, #73940, .T. ) ;
#85564 = VERTEX_POINT ( 'NONE', #94745 ) ;
#85565 = LINE ( 'NONE', #46465, #64289 ) ;
#85566 = CARTESIAN_POINT ( 'NONE',  ( -18.59999999999999787, 44.18876898710608003, -236.1516686502934590 ) ) ;
#85567 = CARTESIAN_POINT ( 'NONE',  ( -23.25000000000000000, 6.855069093508307176, -220.2576993407411692 ) ) ;
#85568 = DIRECTION ( 'NONE',  ( 0.000000000000000000, -0.9274965247785323941, -0.3738317757009769760 ) ) ;
#85569 = CARTESIAN_POINT ( 'NONE',  ( -16.81095280782811230, 9.950000000011138823, -46.14999999999913172 ) ) ;
#85571 = ADVANCED_FACE ( 'NONE', ( #174345 ), #113036, .T. ) ;
#85570 = CARTESIAN_POINT ( 'NONE',  ( -18.40000000000000213, 64.52683809664954140, -45.32293673299014358 ) ) ;
#85572 = CARTESIAN_POINT ( 'NONE',  ( -18.42609945526394455, -9.499999710490698135, -6.999362490248241642 ) ) ;
#85573 = CARTESIAN_POINT ( 'NONE',  ( 18.59999999999999076, -1.851617760468904805, -45.10318971960366241 ) ) ;
#85574 = DIRECTION ( 'NONE',  ( 0.000000000000000000, 0.000000000000000000, -1.000000000000000000 ) ) ;
#85575 = CYLINDRICAL_SURFACE ( 'NONE', #113162, 0.09999999999998898659 ) ;
#85576 = EDGE_CURVE ( 'NONE', #41617, #13199, #111755, .T. ) ;
#85577 = PLANE ( 'NONE',  #160637 ) ;
#85578 = FACE_OUTER_BOUND ( 'NONE', #126675, .T. ) ;
#85579 = CIRCLE ( 'NONE', #247933, 0.09999999999999609201 ) ;
#85580 = VECTOR ( 'NONE', #160109, 1000.000000000000000 ) ;
#85581 = DIRECTION ( 'NONE',  ( 0.000000000000000000, 3.469446951953514729E-13, -1.000000000000000000 ) ) ;
#85583 = CARTESIAN_POINT ( 'NONE',  ( -20.94999999999999929, -11.65000000000000036, -2.900000000000003464 ) ) ;
#85582 = TOROIDAL_SURFACE ( 'NONE', #231387, 0.4000000000000003553, 0.1000000000000000056 ) ;
#85584 = AXIS2_PLACEMENT_3D ( 'NONE', #6528, #164342, #41842 ) ;
#85585 = EDGE_CURVE ( 'NONE', #49859, #19071, #125867, .T. ) ;
#85587 = EDGE_CURVE ( 'NONE', #134440, #161509, #143174, .T. ) ;
#85586 = EDGE_CURVE ( 'NONE', #59875, #170174, #113429, .T. ) ;
#85588 = VERTEX_POINT ( 'NONE', #11370 ) ;
#85589 = CARTESIAN_POINT ( 'NONE',  ( 18.49505816908824229, 85.43787255322325791, -129.7454502828534260 ) ) ;
#85590 = DIRECTION ( 'NONE',  ( -1.000000000000000000, 0.000000000000000000, 0.000000000000000000 ) ) ;
#85591 = EDGE_LOOP ( 'NONE', ( #142621, #56189, #72702, #109811 ) ) ;
#85592 = DIRECTION ( 'NONE',  ( 1.000000000000000000, 0.000000000000000000, 0.000000000000000000 ) ) ;
#85593 = DIRECTION ( 'NONE',  ( 0.000000000000000000, 0.9126074666063772600, 0.4088369013363274407 ) ) ;
#85594 = DIRECTION ( 'NONE',  ( 1.000000000000000000, 0.000000000000000000, 0.000000000000000000 ) ) ;
#85595 = ORIENTED_EDGE ( 'NONE', *, *, #199968, .F. ) ;
#85596 = CARTESIAN_POINT ( 'NONE',  ( 18.40916198585732388, -9.499999999988844479, -174.1001896318244349 ) ) ;
#85597 = DIRECTION ( 'NONE',  ( 4.504528286903031644E-15, 0.08413937888703756918, -0.9964539953858901900 ) ) ;
#85598 = VERTEX_POINT ( 'NONE', #51749 ) ;
#85599 = EDGE_CURVE ( 'NONE', #168004, #111850, #179897, .T. ) ;
#85600 = EDGE_CURVE ( 'NONE', #46741, #16741, #946, .T. ) ;
#85601 = TOROIDAL_SURFACE ( 'NONE', #64788, 0.2000000000000000111, 0.1000000000000000056 ) ;
#85602 = AXIS2_PLACEMENT_3D ( 'NONE', #150890, #225268, #226552 ) ;
#85603 = AXIS2_PLACEMENT_3D ( 'NONE', #179988, #160443, #239959 ) ;
#85604 = FACE_OUTER_BOUND ( 'NONE', #14992, .T. ) ;
#85605 = ADVANCED_FACE ( 'NONE', ( #120767 ), #26593, .T. ) ;
#85606 = ORIENTED_EDGE ( 'NONE', *, *, #134753, .F. ) ;
#85607 = AXIS2_PLACEMENT_3D ( 'NONE', #26324, #224508, #127987 ) ;
#85608 = DIRECTION ( 'NONE',  ( 1.000000000000000000, -3.448943450116722089E-16, -6.438528483529608630E-16 ) ) ;
#85609 = EDGE_CURVE ( 'NONE', #54116, #8349, #78070, .T. ) ;
#85610 = DIRECTION ( 'NONE',  ( 0.000000000000000000, 0.000000000000000000, -1.000000000000000000 ) ) ;
#85611 = CARTESIAN_POINT ( 'NONE',  ( 21.08134388332232234, 33.99988033202343729, -243.8010834761945773 ) ) ;
#85613 = DIRECTION ( 'NONE',  ( 0.000000000000000000, -0.2605042016806647931, -0.9654727137038724427 ) ) ;
#85612 = AXIS2_PLACEMENT_3D ( 'NONE', #36644, #135694, #176144 ) ;
#85614 = DIRECTION ( 'NONE',  ( 0.000000000000000000, 1.224646799142185182E-16, 1.000000000000000000 ) ) ;
#85615 = ADVANCED_FACE ( 'NONE', ( #162450 ), #98557, .T. ) ;
#85616 = FACE_OUTER_BOUND ( 'NONE', #233492, .T. ) ;
#85617 = CARTESIAN_POINT ( 'NONE',  ( -23.25000000000000000, -1.164121893230052995, -175.4148480855716059 ) ) ;
#85618 = DIRECTION ( 'NONE',  ( 0.000000000000000000, -6.652207440891584540E-15, 1.000000000000000000 ) ) ;
#85620 = ORIENTED_EDGE ( 'NONE', *, *, #180761, .F. ) ;
#85619 = DIRECTION ( 'NONE',  ( 0.000000000000000000, -0.000000000000000000, 1.000000000000000000 ) ) ;
#85621 = VERTEX_POINT ( 'NONE', #221107 ) ;
#85623 = PLANE ( 'NONE',  #185295 ) ;
#85622 = DIRECTION ( 'NONE',  ( 0.000000000000000000, -0.9126074666063769270, -0.4088369013363280513 ) ) ;
#85625 = ORIENTED_EDGE ( 'NONE', *, *, #38278, .T. ) ;
#85624 = DIRECTION ( 'NONE',  ( 0.000000000000000000, 0.2128009952263650861, -0.9770955615653305060 ) ) ;
#85626 = ORIENTED_EDGE ( 'NONE', *, *, #213416, .F. ) ;
#85627 = DIRECTION ( 'NONE',  ( -1.000000000000000000, 0.000000000000000000, 0.000000000000000000 ) ) ;
#85628 = CARTESIAN_POINT ( 'NONE',  ( 18.59999999999999432, 77.83585931145546510, -91.51866831572576189 ) ) ;
#85629 = TOROIDAL_SURFACE ( 'NONE', #231427, 0.4000000000000005773, 0.1000000000000000056 ) ;
#85630 = AXIS2_PLACEMENT_3D ( 'NONE', #2833, #122819, #23736 ) ;
#85631 = FACE_OUTER_BOUND ( 'NONE', #33474, .T. ) ;
#85632 = DIRECTION ( 'NONE',  ( 1.000000000000000000, 0.000000000000000000, 0.000000000000000000 ) ) ;
#85633 = EDGE_CURVE ( 'NONE', #48041, #135481, #42484, .T. ) ;
#85634 = AXIS2_PLACEMENT_3D ( 'NONE', #179930, #200761, #61251 ) ;
#85635 = CARTESIAN_POINT ( 'NONE',  ( 21.00000000000000000, 52.06567329910104291, -231.9654557484363409 ) ) ;
#85636 = AXIS2_PLACEMENT_3D ( 'NONE', #227443, #29296, #100604 ) ;
#85637 = DIRECTION ( 'NONE',  ( -0.000000000000000000, 1.000000000000000000, -0.000000000000000000 ) ) ;
#85638 = EDGE_CURVE ( 'NONE', #176438, #205324, #188250, .T. ) ;
#85639 = ORIENTED_EDGE ( 'NONE', *, *, #32886, .F. ) ;
#85640 = ORIENTED_EDGE ( 'NONE', *, *, #42533, .F. ) ;
#85641 = DIRECTION ( 'NONE',  ( 0.000000000000000000, 0.1568667991644863147, -0.9876197685951252359 ) ) ;
#85642 = EDGE_LOOP ( 'NONE', ( #46631, #81235, #176323, #249048 ) ) ;
#85643 = CARTESIAN_POINT ( 'NONE',  ( 21.05000000000000071, -0.09999999998884512298, -26.95934304829875927 ) ) ;
#85644 = EDGE_LOOP ( 'NONE', ( #21002, #177567, #153801, #196471 ) ) ;
#85645 = DIRECTION ( 'NONE',  ( 0.000000000000000000, 0.000000000000000000, 1.000000000000000000 ) ) ;
#85646 = DIRECTION ( 'NONE',  ( -1.000000000000000000, 0.000000000000000000, -0.000000000000000000 ) ) ;
#85647 = B_SPLINE_CURVE_WITH_KNOTS ( 'NONE', 3,
 ( #53425, #15618, #132980, #149985, #250341, #112139, #194251, #95120, #191692, #113404 ),
 .UNSPECIFIED., .F., .F.,
 ( 4, 3, 3, 4 ),
 ( -2.000561356219677529E-06, 0.000000000000000000, 1.787822682429502760E-05, 4.206475347090109142E-05 ),
 .UNSPECIFIED. ) ;
#85648 = EDGE_CURVE ( 'NONE', #87492, #239369, #67435, .T. ) ;
#85649 = CARTESIAN_POINT ( 'NONE',  ( -21.13498764882296044, 75.99834360528140564, -210.0187256279983217 ) ) ;
#85650 = VERTEX_POINT ( 'NONE', #159885 ) ;
#85651 = CARTESIAN_POINT ( 'NONE',  ( -20.00857864376270001, 66.65000000001205649, -124.2731074845243597 ) ) ;
#85652 = VERTEX_POINT ( 'NONE', #215965 ) ;
#85653 = TOROIDAL_SURFACE ( 'NONE', #52361, 0.2000000000000000111, 0.1000000000000000056 ) ;
#85654 = LINE ( 'NONE', #106517, #113331 ) ;
#85655 = CARTESIAN_POINT ( 'NONE',  ( -20.94999999999994600, 65.35000000001120668, -4.423107484524790856 ) ) ;
#85656 = TOROIDAL_SURFACE ( 'NONE', #98139, 7.791421356237316687, 0.1000000000000000056 ) ;
#85657 = DIRECTION ( 'NONE',  ( -6.938893903907222067E-15, -1.000000000000000000, -6.982962677686266711E-15 ) ) ;
#85658 = FACE_OUTER_BOUND ( 'NONE', #105636, .T. ) ;
#85659 = AXIS2_PLACEMENT_3D ( 'NONE', #223905, #201786, #60992 ) ;
#85660 = ORIENTED_EDGE ( 'NONE', *, *, #57942, .F. ) ;
#85661 = DIRECTION ( 'NONE',  ( 0.000000000000000000, -7.304098846218085561E-15, 1.000000000000000000 ) ) ;
#85662 = ORIENTED_EDGE ( 'NONE', *, *, #175107, .T. ) ;
#85665 = ORIENTED_EDGE ( 'NONE', *, *, #169308, .F. ) ;
#85664 = LINE ( 'NONE', #32179, #147009 ) ;
#85663 = CARTESIAN_POINT ( 'NONE',  ( 21.30000000000002558, 1.115650265596050101E-11, -163.4499999999999886 ) ) ;
#85666 = ADVANCED_FACE ( 'NONE', ( #176882 ), #157324, .T. ) ;
#85667 = DIRECTION ( 'NONE',  ( 0.000000000000000000, -1.000000000000000000, 0.000000000000000000 ) ) ;
#85668 = EDGE_LOOP ( 'NONE', ( #103041, #74973, #52505, #142387 ) ) ;
#85669 = CIRCLE ( 'NONE', #244106, 7.899999999999990585 ) ;
#85670 = ADVANCED_BREP_SHAPE_REPRESENTATION ( '', ( #107560, #2425 ), #252228 ) ;
#85671 = CARTESIAN_POINT ( 'NONE',  ( -19.99999999999999645, 11.61130914238355771, 22.00000000000000355 ) ) ;
#85672 = ORIENTED_EDGE ( 'NONE', *, *, #20323, .T. ) ;
#85673 = DIRECTION ( 'NONE',  ( 1.000000000000000000, 0.000000000000000000, 0.000000000000000000 ) ) ;
#85674 = DIRECTION ( 'NONE',  ( 0.000000000000000000, 0.2617529984165044565, 0.9651348961777151958 ) ) ;
#85675 = DIRECTION ( 'NONE',  ( 0.000000000000000000, 6.982962677686267499E-15, -1.000000000000000000 ) ) ;
#85676 = AXIS2_PLACEMENT_3D ( 'NONE', #105671, #223069, #242630 ) ;
#85677 = UNCERTAINTY_MEASURE_WITH_UNIT (LENGTH_MEASURE( 1.000000000000000082E-05 ), #111500, 'distance_accuracy_value', 'NONE');
#85678 = CARTESIAN_POINT ( 'NONE',  ( -20.94999999999999929, 77.83534155023646406, -124.9679561919612922 ) ) ;
#85679 = AXIS2_PLACEMENT_3D ( 'NONE', #102496, #238175, #59518 ) ;
#85680 = CARTESIAN_POINT ( 'NONE',  ( -18.59999999999999787, 11.65000000001115232, -54.85000000000000142 ) ) ;
#85681 = VERTEX_POINT ( 'NONE', #138977 ) ;
#85682 = DIRECTION ( 'NONE',  ( 1.000000000000000000, 0.000000000000000000, 0.000000000000000000 ) ) ;
#85683 = CARTESIAN_POINT ( 'NONE',  ( -16.90128866880175806, 9.953795777214113016, -188.3626761833886292 ) ) ;
#85684 = CARTESIAN_POINT ( 'NONE',  ( -15.06774609480957849, 66.58234804117127226, -154.6643200920840115 ) ) ;
#85685 = VERTEX_POINT ( 'NONE', #140274 ) ;
#85686 = CARTESIAN_POINT ( 'NONE',  ( -18.59999999999999787, 4.273531877263399892, -211.9976340888692050 ) ) ;
#85687 = ORIENTED_EDGE ( 'NONE', *, *, #209547, .F. ) ;
#85688 = CARTESIAN_POINT ( 'NONE',  ( -23.15000000000000213, 11.65000000001115588, -79.15000000000003411 ) ) ;
#85689 = DIRECTION ( 'NONE',  ( 0.000000000000000000, 0.9915357197604849349, -0.1298341882520056834 ) ) ;
#85690 = CARTESIAN_POINT ( 'NONE',  ( -2.995603634470891112E-16, 87.75000000001180922, -81.77310748452421763 ) ) ;
#85691 = AXIS2_PLACEMENT_3D ( 'NONE', #234243, #92173, #252520 ) ;
#85693 = ORIENTED_EDGE ( 'NONE', *, *, #133513, .F. ) ;
#85692 = LINE ( 'NONE', #161443, #123620 ) ;
#85694 = DIRECTION ( 'NONE',  ( -1.000000000000000000, 0.000000000000000000, -0.000000000000000000 ) ) ;
#85695 = CARTESIAN_POINT ( 'NONE',  ( -12.25000000000000000, 62.62192211835339606, -217.1300186905772307 ) ) ;
#85696 = ADVANCED_FACE ( 'NONE', ( #122022 ), #21658, .F. ) ;
#85697 = DIRECTION ( 'NONE',  ( 0.000000000000000000, 0.000000000000000000, -1.000000000000000000 ) ) ;
#85698 = VERTEX_POINT ( 'NONE', #218523 ) ;
#85699 = CARTESIAN_POINT ( 'NONE',  ( 21.05000000000000071, 84.66355140188177586, -193.9990063664569959 ) ) ;
#85700 = CARTESIAN_POINT ( 'NONE',  ( 18.49999999999999645, 47.95459712139159336, -246.5019368548292675 ) ) ;
#85701 = ORIENTED_EDGE ( 'NONE', *, *, #230400, .F. ) ;
#85702 = CARTESIAN_POINT ( 'NONE',  ( -21.05000000000000071, 1.115600667400684642E-11, -100.5000000000000426 ) ) ;
#85703 = VECTOR ( 'NONE', #223738, 1000.000000000000000 ) ;
#85704 = AXIS2_PLACEMENT_3D ( 'NONE', #210427, #111314, #190879 ) ;
#85705 = AXIS2_PLACEMENT_3D ( 'NONE', #52509, #149080, #89073 ) ;
#85706 = ORIENTED_EDGE ( 'NONE', *, *, #102861, .F. ) ;
#85707 = PLANE ( 'NONE',  #87682 ) ;
#85709 = ORIENTED_EDGE ( 'NONE', *, *, #153925, .F. ) ;
#85708 = DIRECTION ( 'NONE',  ( 1.000000000000000000, 0.000000000000000000, 0.000000000000000000 ) ) ;
#85710 = EDGE_CURVE ( 'NONE', #56126, #109657, #221542, .T. ) ;
#85711 = EDGE_CURVE ( 'NONE', #44449, #159674, #5057, .T. ) ;
#85714 = ORIENTED_EDGE ( 'NONE', *, *, #110891, .F. ) ;
#85713 = EDGE_LOOP ( 'NONE', ( #155647, #29939, #128097, #9629 ) ) ;
#85712 = CARTESIAN_POINT ( 'NONE',  ( 21.14999999999999858, -0.09999999998884338825, -122.3504291924552234 ) ) ;
#85715 = PLANE ( 'NONE',  #257864 ) ;
#85716 = FACE_OUTER_BOUND ( 'NONE', #39627, .T. ) ;
#85717 = CARTESIAN_POINT ( 'NONE',  ( -20.85000000000000142, 7.021664781911246322, -70.83356540189728889 ) ) ;
#85718 = AXIS2_PLACEMENT_3D ( 'NONE', #235954, #58591, #75633 ) ;
#85720 = DIRECTION ( 'NONE',  ( 1.000000000000000000, 0.000000000000000000, 0.000000000000000000 ) ) ;
#85719 = CARTESIAN_POINT ( 'NONE',  ( 22.42196299218230493, 0.002441673998456600492, -88.85038829735056254 ) ) ;
#85721 = DIRECTION ( 'NONE',  ( 0.000000000000000000, -7.272083257015735086E-15, 1.000000000000000000 ) ) ;
#85722 = CYLINDRICAL_SURFACE ( 'NONE', #106705, 0.1000000000000106914 ) ;
#85723 = AXIS2_PLACEMENT_3D ( 'NONE', #163444, #146420, #85146 ) ;
#85724 = EDGE_CURVE ( 'NONE', #25027, #205348, #81572, .T. ) ;
#85725 = CARTESIAN_POINT ( 'NONE',  ( -16.89268316805466341, 44.12952801035616801, -235.2997120924900969 ) ) ;
#85726 = DIRECTION ( 'NONE',  ( 1.000000000000000000, -3.265361837132813093E-16, -2.280189983783949500E-30 ) ) ;
#85727 = CARTESIAN_POINT ( 'NONE',  ( 0.9000000000000546452, 67.72071067812984779, -13.99381816264344813 ) ) ;
#85728 = ORIENTED_EDGE ( 'NONE', *, *, #30030, .F. ) ;
#85729 = VERTEX_POINT ( 'NONE', #22948 ) ;
#85730 = EDGE_CURVE ( 'NONE', #111333, #12223, #257614, .T. ) ;
#85731 = DIRECTION ( 'NONE',  ( 1.000000000000000000, -0.000000000000000000, 0.000000000000000000 ) ) ;
#85732 = VECTOR ( 'NONE', #172911, 1000.000000000000000 ) ;
#85735 = ORIENTED_EDGE ( 'NONE', *, *, #238737, .T. ) ;
#85734 = EDGE_CURVE ( 'NONE', #240580, #122934, #129961, .T. ) ;
#85733 = DIRECTION ( 'NONE',  ( 0.000000000000000000, 0.8814952561688476074, -0.4721928772777262417 ) ) ;
#85736 = ORIENTED_EDGE ( 'NONE', *, *, #110845, .F. ) ;
#85737 = CARTESIAN_POINT ( 'NONE',  ( 21.07016717456946253, 6.320940838111409832, -100.5000000000000568 ) ) ;
#85738 = ORIENTED_EDGE ( 'NONE', *, *, #24193, .T. ) ;
#85739 = CARTESIAN_POINT ( 'NONE',  ( 19.75857864376268935, 16.76897757977919312, -222.7804130109902871 ) ) ;
#85740 = ADVANCED_FACE ( 'NONE', ( #144128 ), #243238, .F. ) ;
#85741 = ORIENTED_EDGE ( 'NONE', *, *, #255942, .F. ) ;
#85742 = EDGE_CURVE ( 'NONE', #189515, #200872, #185843, .T. ) ;
#85743 = CARTESIAN_POINT ( 'NONE',  ( -16.94333152882356330, 66.00965798855413880, -82.13107595342289358 ) ) ;
#85744 = CARTESIAN_POINT ( 'NONE',  ( 23.14999999999999858, 65.65271564877468791, -222.5736063831752176 ) ) ;
#85747 = VERTEX_POINT ( 'NONE', #25500 ) ;
#85746 = ORIENTED_EDGE ( 'NONE', *, *, #219950, .F. ) ;
#85745 = AXIS2_PLACEMENT_3D ( 'NONE', #147681, #229775, #246759 ) ;
#85748 = ORIENTED_EDGE ( 'NONE', *, *, #218976, .T. ) ;
#85749 = CARTESIAN_POINT ( 'NONE',  ( 21.05000000000000071, 10.72371710471867701, -45.66119029412745078 ) ) ;
#85750 = ORIENTED_EDGE ( 'NONE', *, *, #169861, .T. ) ;
#85751 = VERTEX_POINT ( 'NONE', #85418 ) ;
#85752 = CARTESIAN_POINT ( 'NONE',  ( 21.00000000000000000, 0.000000000000000000, 0.000000000000000000 ) ) ;
#85753 = CARTESIAN_POINT ( 'NONE',  ( 20.94999999999999574, 46.50671693017397246, -243.2369495081682942 ) ) ;
#85754 = VERTEX_POINT ( 'NONE', #184547 ) ;
#85755 = DIRECTION ( 'NONE',  ( 1.000000000000000000, -2.952720810173289112E-16, -2.061873921506763405E-30 ) ) ;
#85756 = FACE_OUTER_BOUND ( 'NONE', #214945, .T. ) ;
#85758 = ORIENTED_EDGE ( 'NONE', *, *, #145611, .F. ) ;
#85757 = FACE_OUTER_BOUND ( 'NONE', #174870, .T. ) ;
#85759 = CARTESIAN_POINT ( 'NONE',  ( -17.80356949364085040, 10.87673139701448299, -177.7869269757790676 ) ) ;
#85760 = ORIENTED_EDGE ( 'NONE', *, *, #127016, .T. ) ;
#85761 = CARTESIAN_POINT ( 'NONE',  ( -20.94999999999999929, 72.05339752741123505, -225.0867394276846483 ) ) ;
#85763 = EDGE_CURVE ( 'NONE', #64432, #102962, #196612, .T. ) ;
#85762 = ORIENTED_EDGE ( 'NONE', *, *, #221357, .T. ) ;
#85764 = CARTESIAN_POINT ( 'NONE',  ( -18.79999999999999716, 1.885425182446133885, -11.49641995933507843 ) ) ;
#85765 = DIRECTION ( 'NONE',  ( -1.000000000000000000, 0.000000000000000000, 0.000000000000000000 ) ) ;
#85766 = TOROIDAL_SURFACE ( 'NONE', #248119, 3.899999999999999467, 0.1000000000000000056 ) ;
#85767 = ORIENTED_EDGE ( 'NONE', *, *, #189882, .T. ) ;
#85769 = DIRECTION ( 'NONE',  ( 0.000000000000000000, -6.217248937900876626E-15, -1.000000000000000000 ) ) ;
#85768 = CYLINDRICAL_SURFACE ( 'NONE', #90621, 0.1000000000000124678 ) ;
#85770 = AXIS2_PLACEMENT_3D ( 'NONE', #134746, #130921, #211753 ) ;
#85771 = CIRCLE ( 'NONE', #14914, 0.09999999999999507894 ) ;
#85772 = CIRCLE ( 'NONE', #231568, 0.1000000000000002554 ) ;
#85773 = DIRECTION ( 'NONE',  ( 0.000000000000000000, -0.8660254037844383745, 0.5000000000000003331 ) ) ;
#85774 = DIRECTION ( 'NONE',  ( 0.000000000000000000, -0.2617529984165152257, -0.9651348961777124202 ) ) ;
#85775 = ORIENTED_EDGE ( 'NONE', *, *, #70948, .F. ) ;
#85776 = ORIENTED_EDGE ( 'NONE', *, *, #111502, .T. ) ;
#85777 = EDGE_CURVE ( 'NONE', #109034, #46953, #92747, .T. ) ;
#85778 = DIRECTION ( 'NONE',  ( 0.000000000000000000, 0.9126074666063772600, 0.4088369013363277182 ) ) ;
#85779 = DIRECTION ( 'NONE',  ( 0.000000000000000000, -0.2128009952263511806, 0.9770955615653335036 ) ) ;
#85780 = ORIENTED_EDGE ( 'NONE', *, *, #221028, .F. ) ;
#85781 = DIRECTION ( 'NONE',  ( -0.000000000000000000, 0.8814952561688430555, -0.4721928772777346239 ) ) ;
#85782 = ORIENTED_EDGE ( 'NONE', *, *, #243223, .T. ) ;
#85783 = LINE ( 'NONE', #164083, #152419 ) ;
#85784 = ORIENTED_EDGE ( 'NONE', *, *, #209585, .T. ) ;
#85785 = DIRECTION ( 'NONE',  ( 1.000000000000000000, -1.541976423090492636E-14, 0.000000000000000000 ) ) ;
#85786 = CARTESIAN_POINT ( 'NONE',  ( 18.49999999999999289, 55.08797342919077522, -230.1090097671678905 ) ) ;
#85787 = DIRECTION ( 'NONE',  ( -1.000000000000000000, 0.000000000000000000, 0.000000000000000000 ) ) ;
#85788 = ORIENTED_EDGE ( 'NONE', *, *, #244147, .T. ) ;
#85789 = DIRECTION ( 'NONE',  ( 0.000000000000000000, -0.9229812358756199764, 0.3848449534832346086 ) ) ;
#85790 = CIRCLE ( 'NONE', #144067, 1.899999999999999023 ) ;
#85791 = EDGE_CURVE ( 'NONE', #218866, #101771, #230115, .T. ) ;
#85792 = EDGE_LOOP ( 'NONE', ( #144205, #61521, #89837, #197215 ) ) ;
#85793 = ORIENTED_EDGE ( 'NONE', *, *, #11765, .T. ) ;
#85794 = AXIS2_PLACEMENT_3D ( 'NONE', #199234, #244749, #220071 ) ;
#85795 = ORIENTED_EDGE ( 'NONE', *, *, #221891, .F. ) ;
#85796 = CARTESIAN_POINT ( 'NONE',  ( 22.49544290803779489, 64.25012976215485594, -136.5884194437818735 ) ) ;
#85797 = DIRECTION ( 'NONE',  ( 0.000000000000000000, 0.000000000000000000, -1.000000000000000000 ) ) ;
#85798 = CARTESIAN_POINT ( 'NONE',  ( 23.14999999999999858, 6.650000000011155876, -179.8499999999999943 ) ) ;
#85799 = CYLINDRICAL_SURFACE ( 'NONE', #219515, 2.599999999999998312 ) ;
#85800 = DIRECTION ( 'NONE',  ( 1.000000000000000000, 0.000000000000000000, 0.000000000000000000 ) ) ;
#85801 = EDGE_CURVE ( 'NONE', #137338, #31610, #254993, .T. ) ;
#85803 = CARTESIAN_POINT ( 'NONE',  ( 20.95262331984806181, 59.07243101476477420, -225.8083546741112571 ) ) ;
#85802 = CARTESIAN_POINT ( 'NONE',  ( -20.00857864376270001, 9.350000000011156942, -88.25000000000005684 ) ) ;
#85805 = ORIENTED_EDGE ( 'NONE', *, *, #25297, .F. ) ;
#85804 = DIRECTION ( 'NONE',  ( -0.000000000000000000, 0.000000000000000000, -1.000000000000000000 ) ) ;
#85806 = DIRECTION ( 'NONE',  ( 0.000000000000000000, 0.000000000000000000, -1.000000000000000000 ) ) ;
#85807 = ORIENTED_EDGE ( 'NONE', *, *, #31126, .F. ) ;
#85808 = CIRCLE ( 'NONE', #81706, 0.09999999999998898659 ) ;
#85809 = CARTESIAN_POINT ( 'NONE',  ( 20.97239005616516394, 8.874843841361279573, -79.25015280215322377 ) ) ;
#85810 = CIRCLE ( 'NONE', #231598, 0.5999999999999992006 ) ;
#85811 = EDGE_LOOP ( 'NONE', ( #72772, #122933, #212359 ) ) ;
#85812 = ORIENTED_EDGE ( 'NONE', *, *, #229620, .T. ) ;
#85813 = CARTESIAN_POINT ( 'NONE',  ( -20.85000000000000142, 43.35377423437995503, -245.1717807829448930 ) ) ;
#85815 = EDGE_CURVE ( 'NONE', #4597, #124911, #100899, .T. ) ;
#85814 = CARTESIAN_POINT ( 'NONE',  ( -21.05000000000000071, 87.65000000001192859, -100.0231074845242318 ) ) ;
#85816 = EDGE_CURVE ( 'NONE', #2443, #31458, #205165, .T. ) ;
#85817 = CARTESIAN_POINT ( 'NONE',  ( 18.59999999999999076, 76.00000000001244871, -170.0231074845243597 ) ) ;
#85818 = EDGE_CURVE ( 'NONE', #143703, #135186, #26131, .T. ) ;
#85819 = CIRCLE ( 'NONE', #23541, 0.1000000000000013933 ) ;
#85820 = LINE ( 'NONE', #204509, #254761 ) ;
#85822 = ORIENTED_EDGE ( 'NONE', *, *, #221033, .T. ) ;
#85821 = CIRCLE ( 'NONE', #6750, 12.87500000000000000 ) ;
#85823 = ORIENTED_EDGE ( 'NONE', *, *, #79553, .F. ) ;
#85824 = AXIS2_PLACEMENT_3D ( 'NONE', #2198, #162592, #161313 ) ;
#85825 = EDGE_CURVE ( 'NONE', #55215, #217779, #145423, .T. ) ;
#85826 = DIRECTION ( 'NONE',  ( 0.000000000000000000, -1.000000000000000000, -6.982962677686266711E-15 ) ) ;
#85827 = EDGE_LOOP ( 'NONE', ( #28973, #49168, #70735, #239612 ) ) ;
#85828 = FACE_OUTER_BOUND ( 'NONE', #227207, .T. ) ;
#85829 = DIRECTION ( 'NONE',  ( 0.000000000000000000, -0.9126074666063660468, -0.4088369013363524762 ) ) ;
#85830 = CARTESIAN_POINT ( 'NONE',  ( 23.15000000000000213, 87.48912529308779540, -72.52310748452423184 ) ) ;
#85831 = CARTESIAN_POINT ( 'NONE',  ( 18.59999999999999076, 1.115600667400684642E-11, -167.5000000000000284 ) ) ;
#85832 = VECTOR ( 'NONE', #128725, 1000.000000000000000 ) ;
#85833 = CARTESIAN_POINT ( 'NONE',  ( -16.92209698673559970, 66.05000000001209060, -123.8124719174716546 ) ) ;
#85834 = CARTESIAN_POINT ( 'NONE',  ( -21.05000000000000071, 77.85102823015347440, -191.8691942151018566 ) ) ;
#85835 = ORIENTED_EDGE ( 'NONE', *, *, #127501, .T. ) ;
#85836 = DIRECTION ( 'NONE',  ( 0.000000000000000000, -1.000000000000000000, 0.000000000000000000 ) ) ;
#85837 = SPHERICAL_SURFACE ( 'NONE', #16759, 0.1000000000000000056 ) ;
#85838 = LINE ( 'NONE', #165422, #46002 ) ;
#85839 = CARTESIAN_POINT ( 'NONE',  ( -18.59999999999999787, 64.35000000001247145, -181.7731074845244450 ) ) ;
#85840 = CARTESIAN_POINT ( 'NONE',  ( 21.05000000000000071, 74.83729825007462466, -195.6231074845243540 ) ) ;
#85841 = TOROIDAL_SURFACE ( 'NONE', #60913, 4.149999999999999467, 0.1000000000000000056 ) ;
#85842 = CARTESIAN_POINT ( 'NONE',  ( -20.54999999999999716, 68.85000000001228670, -157.6731074845243938 ) ) ;
#85843 = EDGE_CURVE ( 'NONE', #133095, #191642, #124600, .T. ) ;
#85844 = ORIENTED_EDGE ( 'NONE', *, *, #107151, .F. ) ;
#85845 = CARTESIAN_POINT ( 'NONE',  ( -22.47007471830799474, 68.27928934808565486, -136.5231074845243597 ) ) ;
#85846 = VERTEX_POINT ( 'NONE', #47599 ) ;
#85847 = ADVANCED_FACE ( 'NONE', ( #63316 ), #89299, .F. ) ;
#85848 =( REPRESENTATION_RELATIONSHIP ('NONE','NONE', #36900, #223420 ) REPRESENTATION_RELATIONSHIP_WITH_TRANSFORMATION ( #222193 )SHAPE_REPRESENTATION_RELATIONSHIP( ) );
#85849 = ADVANCED_FACE ( 'NONE', ( #204112 ), #200902, .F. ) ;
#85850 = DIRECTION ( 'NONE',  ( -1.073024830501117725E-15, -6.982962677686266711E-15, 1.000000000000000000 ) ) ;
#85852 = AXIS2_PLACEMENT_3D ( 'NONE', #166878, #145981, #125158 ) ;
#85851 = DIRECTION ( 'NONE',  ( 0.000000000000000000, 0.8814952561688437216, -0.4721928772777334582 ) ) ;
#85853 = CARTESIAN_POINT ( 'NONE',  ( 21.08804582317334209, 61.89529605692450076, -221.6118240886515309 ) ) ;
#85855 = ORIENTED_EDGE ( 'NONE', *, *, #22204, .T. ) ;
#85854 = VECTOR ( 'NONE', #66380, 1000.000000000000227 ) ;
#85856 = FACE_OUTER_BOUND ( 'NONE', #82538, .T. ) ;
#85857 = DIRECTION ( 'NONE',  ( -1.000000000000000000, 2.952720810173289112E-16, 2.061873921506763405E-30 ) ) ;
#85858 = CIRCLE ( 'NONE', #48467, 0.09999999999998898659 ) ;
#85859 = AXIS2_PLACEMENT_3D ( 'NONE', #33164, #112665, #113933 ) ;
#85860 = CARTESIAN_POINT ( 'NONE',  ( 11.60000000000006004, 67.65000000001118963, -21.02310748452479316 ) ) ;
#85861 = CARTESIAN_POINT ( 'NONE',  ( -20.54999999999999716, 19.96675702282871256, -237.7735354486364088 ) ) ;
#85862 = EDGE_CURVE ( 'NONE', #121241, #170796, #46319, .T. ) ;
#85863 = CARTESIAN_POINT ( 'NONE',  ( -21.07946286933445279, 69.67096268100465295, -170.0997913277808209 ) ) ;
#85864 = CARTESIAN_POINT ( 'NONE',  ( 22.44352723754029810, 75.99072290496917503, -181.6728288298730547 ) ) ;
#85865 = VECTOR ( 'NONE', #235824, 1000.000000000000000 ) ;
#85866 = ORIENTED_EDGE ( 'NONE', *, *, #142470, .F. ) ;
#85867 = ORIENTED_EDGE ( 'NONE', *, *, #62958, .T. ) ;
#85868 = CARTESIAN_POINT ( 'NONE',  ( 18.49999999999999645, 1.835341550235567887, -145.5551512925629822 ) ) ;
#85870 = ORIENTED_EDGE ( 'NONE', *, *, #29459, .F. ) ;
#85869 = DIRECTION ( 'NONE',  ( 0.000000000000000000, 0.2617529984165039569, 0.9651348961777154178 ) ) ;
#85871 = CYLINDRICAL_SURFACE ( 'NONE', #217335, 0.09999999999999939493 ) ;
#85872 =( BOUNDED_CURVE ( )  B_SPLINE_CURVE ( 3, ( #110002, #14795, #10924, #232556 ),
 .UNSPECIFIED., .F., .F. ) 
 B_SPLINE_CURVE_WITH_KNOTS ( ( 4, 4 ),
 ( 4.712388980384689674, 6.231880751915386263 ),
 .UNSPECIFIED. ) 
 CURVE ( )  GEOMETRIC_REPRESENTATION_ITEM ( )  RATIONAL_B_SPLINE_CURVE ( ( 1.000000000000000000, 0.8166740347213228279, 0.8166740347213228279, 1.000000000000000000 ) ) 
 REPRESENTATION_ITEM ( '' )  );
#85873 = CARTESIAN_POINT ( 'NONE',  ( -20.94999999999999929, 44.52640028187936849, -247.3006740988509193 ) ) ;
#85874 = CIRCLE ( 'NONE', #194269, 0.09999999999998898659 ) ;
#85875 = VERTEX_POINT ( 'NONE', #104979 ) ;
#85876 = CARTESIAN_POINT ( 'NONE',  ( -15.55912972643740488, 8.490870273573721150, -188.3499999999999659 ) ) ;
#85877 = AXIS2_PLACEMENT_3D ( 'NONE', #124408, #27901, #150402 ) ;
#85878 = EDGE_CURVE ( 'NONE', #108455, #73797, #224951, .T. ) ;
#85879 = DIRECTION ( 'NONE',  ( 2.694716079187272946E-16, -1.000000000000000000, 0.000000000000000000 ) ) ;
#85880 = VECTOR ( 'NONE', #114784, 1000.000000000000000 ) ;
#85881 = ORIENTED_EDGE ( 'NONE', *, *, #46501, .F. ) ;
#85882 = DIRECTION ( 'NONE',  ( 1.000000000000000000, 0.000000000000000000, 0.000000000000000000 ) ) ;
#85883 = DIRECTION ( 'NONE',  ( -1.000000000000000000, 0.000000000000000000, 0.000000000000000000 ) ) ;
#85884 = EDGE_LOOP ( 'NONE', ( #169190, #254432, #170764, #35045 ) ) ;
#85885 = CIRCLE ( 'NONE', #40162, 12.97499999999998721 ) ;
#85886 = ORIENTED_EDGE ( 'NONE', *, *, #201299, .F. ) ;
#85887 = FACE_OUTER_BOUND ( 'NONE', #81775, .T. ) ;
#85888 = DIRECTION ( 'NONE',  ( 1.000000000000000000, 0.000000000000000000, 0.000000000000000000 ) ) ;
#85889 = CYLINDRICAL_SURFACE ( 'NONE', #124149, 0.09999999999999939493 ) ;
#85890 = DIRECTION ( 'NONE',  ( -0.000000000000000000, 0.8496786552930076786, 0.5273008465188218086 ) ) ;
#85891 = CARTESIAN_POINT ( 'NONE',  ( -16.87331047859649757, 14.15900158805613884, -219.2550725561364118 ) ) ;
#85892 = ADVANCED_FACE ( 'NONE', ( #125855 ), #148007, .T. ) ;
#85893 = CARTESIAN_POINT ( 'NONE',  ( 21.05000000000000071, -11.64999999999999147, 3.469446951953614189E-15 ) ) ;
#85894 = CARTESIAN_POINT ( 'NONE',  ( -16.93906926870270624, 10.01214687094654998, -12.55345230722682359 ) ) ;
#85895 = CARTESIAN_POINT ( 'NONE',  ( 21.05000000000000071, -1.290380839962420589, -194.8331666543516292 ) ) ;
#85896 = ADVANCED_FACE ( 'NONE', ( #171460 ), #34504, .T. ) ;
#85897 = FACE_OUTER_BOUND ( 'NONE', #237099, .T. ) ;
#85898 = CARTESIAN_POINT ( 'NONE',  ( 22.40736611211992368, 1.115600667400684642E-11, -155.8504291924551808 ) ) ;
#85899 = CARTESIAN_POINT ( 'NONE',  ( -23.15000000000000213, 1.115600667400684642E-11, -100.5000000000000426 ) ) ;
#85900 = CIRCLE ( 'NONE', #160959, 0.09999999999999939493 ) ;
#85901 = ORIENTED_EDGE ( 'NONE', *, *, #121818, .F. ) ;
#85902 = AXIS2_PLACEMENT_3D ( 'NONE', #90633, #171503, #249727 ) ;
#85903 = ORIENTED_EDGE ( 'NONE', *, *, #60070, .F. ) ;
#85904 = AXIS2_PLACEMENT_3D ( 'NONE', #208526, #31199, #186391 ) ;
#85905 = CARTESIAN_POINT ( 'NONE',  ( 20.94999999999999574, 14.72981487416292623, -236.4853282537515895 ) ) ;
#85906 = AXIS2_PLACEMENT_3D ( 'NONE', #182380, #106651, #166685 ) ;
#85908 = LINE ( 'NONE', #188896, #216005 ) ;
#85907 = CARTESIAN_POINT ( 'NONE',  ( 20.94999999999999574, 1.162701749949165642, -175.4999999999999716 ) ) ;
#85909 = EDGE_CURVE ( 'NONE', #227159, #53948, #9360, .T. ) ;
#85910 = EDGE_CURVE ( 'NONE', #143912, #48194, #225994, .T. ) ;
#85911 = CARTESIAN_POINT ( 'NONE',  ( 20.95520789717937404, 39.25246210041684947, -236.7994979020228357 ) ) ;
#85912 = CARTESIAN_POINT ( 'NONE',  ( -20.94999999999999929, 1.835341550235569663, -179.0551512925629538 ) ) ;
#85913 = LINE ( 'NONE', #67664, #160153 ) ;
#85914 = ORIENTED_EDGE ( 'NONE', *, *, #81576, .F. ) ;
#85915 = EDGE_LOOP ( 'NONE', ( #197825, #22624, #215241, #115993, #101556 ) ) ;
#85916 = CARTESIAN_POINT ( 'NONE',  ( -21.05000000000000071, -10.56629024491939894, -206.4738935375009703 ) ) ;
#85917 = VECTOR ( 'NONE', #97054, 1000.000000000000000 ) ;
#85918 = ORIENTED_EDGE ( 'NONE', *, *, #3430, .T. ) ;
#85919 = FACE_OUTER_BOUND ( 'NONE', #239260, .T. ) ;
#85920 = AXIS2_PLACEMENT_3D ( 'NONE', #245258, #169612, #150023 ) ;
#85921 = CIRCLE ( 'NONE', #206752, 0.2000000000000057288 ) ;
#85922 = ADVANCED_FACE ( 'NONE', ( #154461 ), #196393, .T. ) ;
#85923 = EDGE_CURVE ( 'NONE', #256898, #51707, #91878, .T. ) ;
#85924 = LINE ( 'NONE', #66399, #33925 ) ;
#85925 = TOROIDAL_SURFACE ( 'NONE', #127660, 11.70000000000000107, 0.1000000000000000056 ) ;
#85926 = VERTEX_POINT ( 'NONE', #11062 ) ;
#85927 = CARTESIAN_POINT ( 'NONE',  ( 18.59999999999999076, 76.00000000001244871, -170.0231074845243597 ) ) ;
#85928 = ORIENTED_EDGE ( 'NONE', *, *, #167821, .F. ) ;
#85929 = DIRECTION ( 'NONE',  ( -2.952720810173289605E-16, -1.000000000000000000, -7.086529944415894657E-15 ) ) ;
#85930 = DIRECTION ( 'NONE',  ( 1.000000000000000000, 0.000000000000000000, 0.000000000000000000 ) ) ;
#85931 = CARTESIAN_POINT ( 'NONE',  ( 18.49999999999999645, 43.63140573099096287, -239.9077968784524444 ) ) ;
#85932 = CARTESIAN_POINT ( 'NONE',  ( 18.51997666896852479, -9.392332131507911797, -141.1434061874842030 ) ) ;
#85933 = FACE_OUTER_BOUND ( 'NONE', #145220, .T. ) ;
#85934 = ADVANCED_FACE ( 'NONE', ( #90584 ), #55284, .T. ) ;
#85935 = DIRECTION ( 'NONE',  ( 0.000000000000000000, 6.982962677686266711E-15, -1.000000000000000000 ) ) ;
#85936 = DIRECTION ( 'NONE',  ( -1.000000000000000000, 0.000000000000000000, -0.000000000000000000 ) ) ;
#85937 = DIRECTION ( 'NONE',  ( 0.5932847527679310229, -0.8049926720990042694, 0.000000000000000000 ) ) ;
#85940 = ORIENTED_EDGE ( 'NONE', *, *, #99537, .T. ) ;
#85939 = EDGE_CURVE ( 'NONE', #224224, #163243, #13643, .T. ) ;
#85938 = CARTESIAN_POINT ( 'NONE',  ( 18.58725287972316664, -0.7668395408905932520, -242.4347282044658698 ) ) ;
#85942 = DIRECTION ( 'NONE',  ( -0.000000000000000000, -0.9126074666063771490, -0.4088369013363281623 ) ) ;
#85941 = CARTESIAN_POINT ( 'NONE',  ( -16.80117486205003630, 66.05034273169968628, -115.6742526115988881 ) ) ;
#85943 = ORIENTED_EDGE ( 'NONE', *, *, #130853, .T. ) ;
#85945 = ORIENTED_EDGE ( 'NONE', *, *, #234865, .T. ) ;
#85944 = CARTESIAN_POINT ( 'NONE',  ( 21.05000000000000071, 67.22371710472015138, -195.0351067629400461 ) ) ;
#85946 = AXIS2_PLACEMENT_3D ( 'NONE', #112114, #191664, #9146 ) ;
#85947 = ORIENTED_EDGE ( 'NONE', *, *, #77895, .T. ) ;
#85948 = CARTESIAN_POINT ( 'NONE',  ( 23.14999999999999858, 68.28935379556426710, -213.7087130192904567 ) ) ;
#85949 = DIRECTION ( 'NONE',  ( 0.000000000000000000, -0.9908441862701596881, -0.1350103645451904977 ) ) ;
#85950 = DIRECTION ( 'NONE',  ( -0.4999999999999799050, 0.000000000000000000, -0.8660254037844502539 ) ) ;
#85951 = DIRECTION ( 'NONE',  ( 0.000000000000000000, 0.000000000000000000, -1.000000000000000000 ) ) ;
#85952 = DIRECTION ( 'NONE',  ( 0.000000000000000000, 0.000000000000000000, -1.000000000000000000 ) ) ;
#85953 = EDGE_CURVE ( 'NONE', #164268, #183531, #1159, .T. ) ;
#85955 = ORIENTED_EDGE ( 'NONE', *, *, #184169, .T. ) ;
#85954 = CIRCLE ( 'NONE', #194347, 11.90000000000000213 ) ;
#85956 = LINE ( 'NONE', #205935, #206919 ) ;
#85958 = AXIS2_PLACEMENT_3D ( 'NONE', #18257, #97760, #177365 ) ;
#85957 = FACE_OUTER_BOUND ( 'NONE', #62933, .T. ) ;
#85959 = EDGE_CURVE ( 'NONE', #70460, #239230, #46942, .T. ) ;
#85960 = ORIENTED_EDGE ( 'NONE', *, *, #192513, .F. ) ;
#85961 = ORIENTED_EDGE ( 'NONE', *, *, #194450, .T. ) ;
#85962 = CARTESIAN_POINT ( 'NONE',  ( 20.94999999999999574, -10.74476030654553504, -206.4104182790846096 ) ) ;
#85963 = CIRCLE ( 'NONE', #123415, 1.500000000000001332 ) ;
#85964 = VERTEX_POINT ( 'NONE', #69770 ) ;
#85965 = B_SPLINE_CURVE_WITH_KNOTS ( 'NONE', 3,
 ( #104410, #163145, #242654, #183974, #45745, #165719, #66603, #125294, #226955, #246510 ),
 .UNSPECIFIED., .F., .F.,
 ( 4, 2, 2, 2, 4 ),
 ( 0.000000000000000000, 0.0003916577441626822214, 0.0005874866162440240368, 0.0006854010522846949987, 0.0007833154883253658522 ),
 .UNSPECIFIED. ) ;
#85966 = VERTEX_POINT ( 'NONE', #149312 ) ;
#85967 = DIRECTION ( 'NONE',  ( -0.000000000000000000, -6.982962677686266711E-15, 1.000000000000000000 ) ) ;
#85968 =( BOUNDED_SURFACE ( )  B_SPLINE_SURFACE ( 3, 2, ( 
 ( #181515, #22445, #45833 ),
 ( #142359, #5392, #25015 ),
 ( #221876, #125381, #163228 ),
 ( #21171, #84923, #160681 ),
 ( #164515, #244024, #242737 ),
 ( #121557, #204892, #23739 ) ),
 .UNSPECIFIED., .F., .F., .F. ) 
 B_SPLINE_SURFACE_WITH_KNOTS ( ( 4, 2, 4 ),
 ( 3, 3 ),
 ( 1.570796326794895448, 2.356194490192343505, 3.141592653589791784 ),
 ( 0.000000000000000000, 1.000000000000000000 ),
 .UNSPECIFIED. ) 
 GEOMETRIC_REPRESENTATION_ITEM ( )  RATIONAL_B_SPLINE_SURFACE ( (
 ( 1.000000000000000000, 0.7071067811865475727, 1.000000000000000000),
 ( 1.000000000000000000, 0.6611148371778297061, 1.000000000000000000),
 ( 1.000000000000000000, 0.6092287576697440477, 1.000000000000000000),
 ( 1.000000000000000000, 0.5278258667056308084, 1.000000000000000000),
 ( 1.000000000000000000, 0.4993418825335151356, 1.000000000000000000),
 ( 1.000000000000000000, 0.5000000000000456302, 1.000000000000000000) ) ) 
 REPRESENTATION_ITEM ( '' )  SURFACE ( )  );
#85969 =( GEOMETRIC_REPRESENTATION_CONTEXT ( 3 ) GLOBAL_UNCERTAINTY_ASSIGNED_CONTEXT ( ( #141761 ) ) GLOBAL_UNIT_ASSIGNED_CONTEXT ( ( #133337, #251988, #173800 ) ) REPRESENTATION_CONTEXT ( 'NONE', 'WORKASPACE' ) );
#85970 = DIRECTION ( 'NONE',  ( 0.000000000000000000, 0.000000000000000000, 1.000000000000000000 ) ) ;
#85971 = FACE_OUTER_BOUND ( 'NONE', #217343, .T. ) ;
#85972 = EDGE_CURVE ( 'NONE', #142241, #61955, #228837, .T. ) ;
#85973 = DIRECTION ( 'NONE',  ( 0.000000000000000000, -7.026728003956683390E-15, 1.000000000000000000 ) ) ;
#85974 = CARTESIAN_POINT ( 'NONE',  ( -23.15000000000000213, 46.19206980365409265, -240.6234452366647076 ) ) ;
#85975 = ORIENTED_EDGE ( 'NONE', *, *, #229152, .F. ) ;
#85976 = CYLINDRICAL_SURFACE ( 'NONE', #232676, 0.09999999999999939493 ) ;
#85977 = CARTESIAN_POINT ( 'NONE',  ( -20.54999999999999716, 1.115624548013267999E-11, -132.1000000000000227 ) ) ;
#85978 = DIRECTION ( 'NONE',  ( 0.000000000000000000, 0.7745938767306564943, 0.6324589521315772123 ) ) ;
#85979 = DIRECTION ( 'NONE',  ( 0.000000000000000000, -1.000000000000000000, 0.000000000000000000 ) ) ;
#85980 = ORIENTED_EDGE ( 'NONE', *, *, #73458, .T. ) ;
#85982 = DIRECTION ( 'NONE',  ( 2.952720810173289112E-16, -1.000000000000000000, 0.000000000000000000 ) ) ;
#85981 = CARTESIAN_POINT ( 'NONE',  ( -22.00356870140485555, 7.254242362510171738, -134.0000000000000000 ) ) ;
#85983 = VECTOR ( 'NONE', #210347, 1000.000000000000000 ) ;
#85984 = ORIENTED_EDGE ( 'NONE', *, *, #257844, .T. ) ;
#85987 = EDGE_LOOP ( 'NONE', ( #170905, #125914, #1413, #15444 ) ) ;
#85986 = PRESENTATION_STYLE_ASSIGNMENT (( #120044 ) ) ;
#85985 = CARTESIAN_POINT ( 'NONE',  ( -20.94999999999999929, 76.00000000001142553, -36.02310748452432421 ) ) ;
#85988 = ORIENTED_EDGE ( 'NONE', *, *, #143454, .T. ) ;
#85989 = CARTESIAN_POINT ( 'NONE',  ( -17.11825945287482753, 9.950000000011138823, -113.2500000000000426 ) ) ;
#85990 = VECTOR ( 'NONE', #257540, 1000.000000000000000 ) ;
#85991 = CARTESIAN_POINT ( 'NONE',  ( -21.05000000000000071, 33.98486250090727623, -243.5821103306120108 ) ) ;
#85992 = DIRECTION ( 'NONE',  ( -1.000000000000000000, 0.000000000000000000, 0.000000000000000000 ) ) ;
#85993 = ORIENTED_EDGE ( 'NONE', *, *, #190725, .F. ) ;
#85994 = DIRECTION ( 'NONE',  ( -1.000000000000000000, 0.000000000000000000, 0.000000000000000000 ) ) ;
#85995 = CIRCLE ( 'NONE', #119341, 0.3999999999999975797 ) ;
#85996 = DIRECTION ( 'NONE',  ( 9.044546369203337730E-15, 0.7397360091702647189, 0.6728971962616949742 ) ) ;
#85997 = AXIS2_PLACEMENT_3D ( 'NONE', #244729, #66109, #145631 ) ;
#85999 = CYLINDRICAL_SURFACE ( 'NONE', #84198, 0.1000000000000028644 ) ;
#85998 = DIRECTION ( 'NONE',  ( 0.000000000000000000, -0.9908441862701596881, 0.1350103645451904977 ) ) ;
#86001 = ORIENTED_EDGE ( 'NONE', *, *, #97566, .F. ) ;
#86000 = CARTESIAN_POINT ( 'NONE',  ( -20.54999999999999716, -11.75000000000000000, -16.75000000000000000 ) ) ;
#86002 = ORIENTED_EDGE ( 'NONE', *, *, #13429, .T. ) ;
#86003 = CARTESIAN_POINT ( 'NONE',  ( 19.97071067811865674, 64.27928932189311695, -78.37310748452439668 ) ) ;
#86004 = CARTESIAN_POINT ( 'NONE',  ( 23.14999999999999858, 11.65000000001116298, -59.98519422934606382 ) ) ;
#86005 = AXIS2_PLACEMENT_3D ( 'NONE', #181690, #3022, #241653 ) ;
#86006 = DIRECTION ( 'NONE',  ( 1.000000000000000000, -0.000000000000000000, -0.000000000000000000 ) ) ;
#86007 = EDGE_LOOP ( 'NONE', ( #37425, #124456, #238018, #228084 ) ) ;
#86008 = CYLINDRICAL_SURFACE ( 'NONE', #89545, 0.09999999999999939493 ) ;
#86009 = ORIENTED_EDGE ( 'NONE', *, *, #43936, .F. ) ;
#86010 = AXIS2_PLACEMENT_3D ( 'NONE', #192416, #76296, #18901 ) ;
#86011 = CARTESIAN_POINT ( 'NONE',  ( -20.64999999999999858, 76.00000000001169553, -67.62310748452431142 ) ) ;
#86012 = FACE_OUTER_BOUND ( 'NONE', #249629, .T. ) ;
#86013 = CARTESIAN_POINT ( 'NONE',  ( -18.59999999999999787, -1.162701749926853712, -41.60000000000000142 ) ) ;
#86014 = ORIENTED_EDGE ( 'NONE', *, *, #228046, .T. ) ;
#86015 = CARTESIAN_POINT ( 'NONE',  ( 23.14999999999998437, 1.115600667400684642E-11, -167.4999999999999716 ) ) ;
#86016 = EDGE_CURVE ( 'NONE', #176897, #243045, #171906, .T. ) ;
#86017 = EDGE_LOOP ( 'NONE', ( #47255, #53343, #158812, #143307 ) ) ;
#86018 = FACE_OUTER_BOUND ( 'NONE', #141055, .T. ) ;
#86019 = DIRECTION ( 'NONE',  ( 0.000000000000000000, -6.982962677686266711E-15, 1.000000000000000000 ) ) ;
#86020 = EDGE_LOOP ( 'NONE', ( #142968, #144915, #239728, #185844 ) ) ;
#86021 = VERTEX_POINT ( 'NONE', #230104 ) ;
#86022 = EDGE_LOOP ( 'NONE', ( #107522, #203411, #139025, #181216 ) ) ;
#86023 = FACE_OUTER_BOUND ( 'NONE', #29776, .T. ) ;
#86024 = ORIENTED_EDGE ( 'NONE', *, *, #164400, .T. ) ;
#86026 = VERTEX_POINT ( 'NONE', #51439 ) ;
#86025 = DIRECTION ( 'NONE',  ( 0.000000000000000000, -1.000000000000000000, 0.000000000000000000 ) ) ;
#86027 = ORIENTED_EDGE ( 'NONE', *, *, #78510, .T. ) ;
#86028 = CIRCLE ( 'NONE', #56803, 0.1000000000000002554 ) ;
#86029 = ADVANCED_FACE ( 'NONE', ( #131005 ), #175995, .T. ) ;
#86030 = CIRCLE ( 'NONE', #48643, 0.09999999999999739653 ) ;
#86032 = ORIENTED_EDGE ( 'NONE', *, *, #95944, .T. ) ;
#86031 = VERTEX_POINT ( 'NONE', #111444 ) ;
#86033 = CONICAL_SURFACE ( 'NONE', #102601, 4.049999999999998046, 0.7853981633974604915 ) ;
#86034 = AXIS2_PLACEMENT_3D ( 'NONE', #203754, #246718, #86337 ) ;
#86035 = FACE_OUTER_BOUND ( 'NONE', #179414, .T. ) ;
#86036 = ORIENTED_EDGE ( 'NONE', *, *, #97223, .F. ) ;
#86037 = CARTESIAN_POINT ( 'NONE',  ( -18.59999999999999787, 74.73821383144687047, -94.93660852097883662 ) ) ;
#86038 = DIRECTION ( 'NONE',  ( 0.000000000000000000, 0.000000000000000000, 1.000000000000000000 ) ) ;
#86039 = AXIS2_PLACEMENT_3D ( 'NONE', #174321, #153473, #78984 ) ;
#86040 = FACE_OUTER_BOUND ( 'NONE', #189872, .T. ) ;
#86041 = ORIENTED_EDGE ( 'NONE', *, *, #199622, .F. ) ;
#86042 = VERTEX_POINT ( 'NONE', #220811 ) ;
#86043 = ADVANCED_FACE ( 'NONE', ( #136110 ), #40928, .T. ) ;
#86044 = DIRECTION ( 'NONE',  ( 0.000000000000000000, 0.2617529984165083423, 0.9651348961777143076 ) ) ;
#86047 = VERTEX_POINT ( 'NONE', #60442 ) ;
#86046 = ADVANCED_FACE ( 'NONE', ( #117853 ), #55125, .T. ) ;
#86045 = DIRECTION ( 'NONE',  ( 0.000000000000000000, 0.000000000000000000, -1.000000000000000000 ) ) ;
#86048 = CARTESIAN_POINT ( 'NONE',  ( 23.25000000000000000, -9.599999999988842347, -57.10603087734755690 ) ) ;
#86050 = VERTEX_POINT ( 'NONE', #121737 ) ;
#86049 = CARTESIAN_POINT ( 'NONE',  ( 20.94999999999999929, -8.663551401857999323, -191.4758988819326646 ) ) ;
#86051 = VECTOR ( 'NONE', #172489, 1000.000000000000000 ) ;
#86052 = ORIENTED_EDGE ( 'NONE', *, *, #3449, .T. ) ;
#86053 = CYLINDRICAL_SURFACE ( 'NONE', #100122, 11.74999999999999645 ) ;
#86054 = EDGE_CURVE ( 'NONE', #192047, #112332, #57868, .T. ) ;
#86055 = VECTOR ( 'NONE', #250760, 1000.000000000000000 ) ;
#86056 = AXIS2_PLACEMENT_3D ( 'NONE', #138174, #61227, #255521 ) ;
#86057 = VERTEX_POINT ( 'NONE', #21359 ) ;
#86058 = VERTEX_POINT ( 'NONE', #254756 ) ;
#86059 = CARTESIAN_POINT ( 'NONE',  ( 23.24999999999999289, 9.088433780795693195, -230.0744959993385805 ) ) ;
#86060 = CARTESIAN_POINT ( 'NONE',  ( 21.05000000000000071, 1.115623935689868526E-11, -65.10000000000000853 ) ) ;
#86062 = ORIENTED_EDGE ( 'NONE', *, *, #134759, .T. ) ;
#86061 = ORIENTED_EDGE ( 'NONE', *, *, #89306, .F. ) ;
#86063 = EDGE_LOOP ( 'NONE', ( #111822, #9484, #56275, #181991, #208982, #32719, #83884, #159444, #145259, #135704 ) ) ;
#86064 = FACE_OUTER_BOUND ( 'NONE', #178210, .T. ) ;
#86066 = ORIENTED_EDGE ( 'NONE', *, *, #36326, .F. ) ;
#86065 = EDGE_CURVE ( 'NONE', #46992, #220791, #18758, .T. ) ;
#86067 = ORIENTED_EDGE ( 'NONE', *, *, #81038, .F. ) ;
#86068 = CYLINDRICAL_SURFACE ( 'NONE', #163556, 0.1000000000000028644 ) ;
#86069 = AXIS2_PLACEMENT_3D ( 'NONE', #71051, #150571, #51429 ) ;
#86071 = ORIENTED_EDGE ( 'NONE', *, *, #246966, .T. ) ;
#86070 = CARTESIAN_POINT ( 'NONE',  ( 23.14999999999999858, 4.813084112160684214, -189.0584822434761634 ) ) ;
#86072 = DIRECTION ( 'NONE',  ( 0.000000000000000000, 0.000000000000000000, 1.000000000000000000 ) ) ;
#86074 = DIRECTION ( 'NONE',  ( 0.000000000000000000, 1.000000000000000000, 0.000000000000000000 ) ) ;
#86073 = DIRECTION ( 'NONE',  ( 1.000000000000000000, -0.000000000000000000, -0.000000000000000000 ) ) ;
#86075 = FACE_OUTER_BOUND ( 'NONE', #51191, .T. ) ;
#86076 = DIRECTION ( 'NONE',  ( 0.000000000000000000, 0.000000000000000000, -1.000000000000000000 ) ) ;
#86077 = ORIENTED_EDGE ( 'NONE', *, *, #231910, .F. ) ;
#86079 = ADVANCED_FACE ( 'NONE', ( #116584 ), #76158, .T. ) ;
#86078 = ORIENTED_EDGE ( 'NONE', *, *, #96319, .T. ) ;
#86080 = FACE_OUTER_BOUND ( 'NONE', #166163, .T. ) ;
#86081 = DIRECTION ( 'NONE',  ( -1.000000000000000000, -0.000000000000000000, -0.000000000000000000 ) ) ;
#86082 = ORIENTED_EDGE ( 'NONE', *, *, #235597, .T. ) ;
#86083 = CIRCLE ( 'NONE', #123729, 0.09999999999999609201 ) ;
#86084 = AXIS2_PLACEMENT_3D ( 'NONE', #75924, #35544, #32990 ) ;
#86085 = AXIS2_PLACEMENT_3D ( 'NONE', #142745, #183190, #185748 ) ;
#86086 = CARTESIAN_POINT ( 'NONE',  ( -20.94999999999999929, 77.16270174995064224, -195.5231074845243313 ) ) ;
#86087 = ORIENTED_EDGE ( 'NONE', *, *, #117039, .F. ) ;
#86088 = ORIENTED_EDGE ( 'NONE', *, *, #77257, .T. ) ;
#86089 = LINE ( 'NONE', #126540, #55201 ) ;
#86090 = CARTESIAN_POINT ( 'NONE',  ( -18.35663730107557257, 64.52609257350087546, -127.2731074845243882 ) ) ;
#86091 = ORIENTED_EDGE ( 'NONE', *, *, #238701, .T. ) ;
#86092 = CARTESIAN_POINT ( 'NONE',  ( -21.00219873199057119, 11.60538868788778899, -107.4126474282948180 ) ) ;
#86093 = CARTESIAN_POINT ( 'NONE',  ( -20.85000000000000142, -1.164121893230052995, -175.4148480855716059 ) ) ;
#86094 = ORIENTED_EDGE ( 'NONE', *, *, #40615, .F. ) ;
#86095 = CARTESIAN_POINT ( 'NONE',  ( -21.05000000000000071, -1.360870587180885716, -175.5729979270909382 ) ) ;
#86096 = DIRECTION ( 'NONE',  ( 1.000000000000000000, 0.000000000000000000, 0.000000000000000000 ) ) ;
#86098 = FACE_OUTER_BOUND ( 'NONE', #102239, .T. ) ;
#86097 = CARTESIAN_POINT ( 'NONE',  ( -22.50000000000000000, 1.115600667400684642E-11, -55.35042919245524473 ) ) ;
#86099 = FACE_OUTER_BOUND ( 'NONE', #148590, .T. ) ;
#86100 = DIRECTION ( 'NONE',  ( 0.000000000000000000, -0.2617529984165152257, -0.9651348961777124202 ) ) ;
#86101 = FACE_OUTER_BOUND ( 'NONE', #107098, .T. ) ;
#86102 = DIRECTION ( 'NONE',  ( 0.000000000000000000, -0.2128009952263485993, 0.9770955615653341697 ) ) ;
#86103 = AXIS2_PLACEMENT_3D ( 'NONE', #69549, #149087, #30420 ) ;
#86104 = AXIS2_PLACEMENT_3D ( 'NONE', #195567, #252936, #16920 ) ;
#86105 = VECTOR ( 'NONE', #245101, 1000.000000000000000 ) ;
#86106 = ORIENTED_EDGE ( 'NONE', *, *, #250264, .T. ) ;
#86107 = EDGE_CURVE ( 'NONE', #57574, #31606, #109307, .T. ) ;
#86109 = EDGE_LOOP ( 'NONE', ( #139247, #221133, #241716, #18444 ) ) ;
#86108 = EDGE_LOOP ( 'NONE', ( #228594, #66003, #142309, #126425 ) ) ;
#86110 = CIRCLE ( 'NONE', #223673, 0.09999999999999990841 ) ;
#86111 = ORIENTED_EDGE ( 'NONE', *, *, #174891, .T. ) ;
#86112 = EDGE_CURVE ( 'NONE', #133329, #23498, #80235, .T. ) ;
#86113 = DIRECTION ( 'NONE',  ( 1.000000000000000000, 0.000000000000000000, 0.000000000000000000 ) ) ;
#86114 = DIRECTION ( 'NONE',  ( -1.000000000000000000, 0.000000000000000000, 0.000000000000000000 ) ) ;
#86115 = EDGE_CURVE ( 'NONE', #45034, #210604, #98255, .T. ) ;
#86116 = EDGE_CURVE ( 'NONE', #246341, #13368, #196125, .T. ) ;
#86118 = DIRECTION ( 'NONE',  ( 2.952720810173289112E-16, 0.4088369013363281623, -0.9126074666063770380 ) ) ;
#86117 = CARTESIAN_POINT ( 'NONE',  ( 20.27550659511089037, 9.216043722520002035, -188.3499999999999659 ) ) ;
#86119 = CARTESIAN_POINT ( 'NONE',  ( -21.05000000000000071, 76.00000000001234923, -165.7231074845244052 ) ) ;
#86120 = VERTEX_POINT ( 'NONE', #177861 ) ;
#86121 = CARTESIAN_POINT ( 'NONE',  ( 18.39999999999999858, -9.399999999999998579, 11.75000000000000000 ) ) ;
#86122 = CARTESIAN_POINT ( 'NONE',  ( -18.50000000000000000, 3.132039894996826224, -190.2813437854022993 ) ) ;
#86123 = FACE_OUTER_BOUND ( 'NONE', #118952, .T. ) ;
#86124 = EDGE_CURVE ( 'NONE', #29396, #185772, #175305, .T. ) ;
#86125 = CYLINDRICAL_SURFACE ( 'NONE', #99707, 0.1000000000000028644 ) ;
#86126 = ORIENTED_EDGE ( 'NONE', *, *, #46805, .F. ) ;
#86127 = ADVANCED_FACE ( 'NONE', ( #119157 ), #180413, .T. ) ;
#86129 = EDGE_CURVE ( 'NONE', #230182, #12655, #6278, .T. ) ;
#86128 = EDGE_CURVE ( 'NONE', #125226, #973, #216946, .T. ) ;
#86130 = CARTESIAN_POINT ( 'NONE',  ( 18.45068634130096896, -9.486506073342757972, -7.068778431168105669 ) ) ;
#86131 = CARTESIAN_POINT ( 'NONE',  ( 20.94999999999999929, 85.00000000001251976, -179.9170766071767389 ) ) ;
#86132 = VERTEX_POINT ( 'NONE', #71713 ) ;
#86133 = ORIENTED_EDGE ( 'NONE', *, *, #123858, .T. ) ;
#86134 = DIRECTION ( 'NONE',  ( -0.000000000000000000, 0.000000000000000000, -1.000000000000000000 ) ) ;
#86135 = LINE ( 'NONE', #242665, #68907 ) ;
#86136 = DIRECTION ( 'NONE',  ( 0.000000000000000000, 0.000000000000000000, -1.000000000000000000 ) ) ;
#86137 = CARTESIAN_POINT ( 'NONE',  ( 20.95443524775735256, 67.12144573613879572, -60.98938520892424009 ) ) ;
#86138 = DIRECTION ( 'NONE',  ( -0.000000000000000000, 0.000000000000000000, 1.000000000000000000 ) ) ;
#86139 = AXIS2_PLACEMENT_3D ( 'NONE', #156161, #37484, #212273 ) ;
#86140 = CARTESIAN_POINT ( 'NONE',  ( -21.07928932188134041, 6.328516656398702978, 0.09889514565463444762 ) ) ;
#86141 = ORIENTED_EDGE ( 'NONE', *, *, #214239, .T. ) ;
#86142 = CARTESIAN_POINT ( 'NONE',  ( 20.04999999999999716, 67.25000000001257661, -190.8731074845244109 ) ) ;
#86143 = CARTESIAN_POINT ( 'NONE',  ( -18.59999999999999787, 9.350000000011156942, -112.8500000000000369 ) ) ;
#86144 = ADVANCED_FACE ( 'NONE', ( #209938 ), #241661, .T. ) ;
#86146 = DIRECTION ( 'NONE',  ( 1.000000000000000000, 0.000000000000000000, 0.000000000000000000 ) ) ;
#86145 = DIRECTION ( 'NONE',  ( -1.000000000000000000, 0.000000000000000000, 0.000000000000000000 ) ) ;
#86147 = DIRECTION ( 'NONE',  ( 0.000000000000000000, 0.000000000000000000, 1.000000000000000000 ) ) ;
#86148 = AXIS2_PLACEMENT_3D ( 'NONE', #63804, #243723, #248525 ) ;
#86149 = CARTESIAN_POINT ( 'NONE',  ( -20.64999999999999858, -8.999999999988844479, -158.0060308773475981 ) ) ;
#86150 = LINE ( 'NONE', #189137, #166198 ) ;
#86151 = FACE_OUTER_BOUND ( 'NONE', #108397, .T. ) ;
#86152 = ADVANCED_FACE ( 'NONE', ( #5591 ), #71928, .T. ) ;
#86153 = ADVANCED_FACE ( 'NONE', ( #105979 ), #230790, .F. ) ;
#86154 = AXIS2_PLACEMENT_3D ( 'NONE', #15456, #36303, #97504 ) ;
#86156 = ORIENTED_EDGE ( 'NONE', *, *, #206744, .T. ) ;
#86155 = CYLINDRICAL_SURFACE ( 'NONE', #65269, 11.79999999999999538 ) ;
#86157 = AXIS2_PLACEMENT_3D ( 'NONE', #238465, #256695, #140642 ) ;
#86158 = EDGE_CURVE ( 'NONE', #41292, #103483, #185545, .T. ) ;
#86159 = AXIS2_PLACEMENT_3D ( 'NONE', #236183, #211496, #135787 ) ;
#86160 = AXIS2_PLACEMENT_3D ( 'NONE', #64706, #223765, #142935 ) ;
#86161 = ADVANCED_FACE ( 'NONE', ( #223368 ), #123013, .T. ) ;
#86162 = EDGE_CURVE ( 'NONE', #232478, #29232, #131665, .T. ) ;
#86163 = DIRECTION ( 'NONE',  ( 2.952720810173289605E-16, 1.000000000000000000, 7.086529944415894657E-15 ) ) ;
#86164 = DIRECTION ( 'NONE',  ( -3.265361837132813093E-16, -0.9651348961777157509, 0.2617529984165031243 ) ) ;
#86165 = B_SPLINE_CURVE_WITH_KNOTS ( 'NONE', 3,
 ( #252884, #95102, #114666, #212498, #215049, #76815 ),
 .UNSPECIFIED., .F., .F.,
 ( 4, 2, 4 ),
 ( 0.000000000000000000, 0.0001891491689349454879, 0.0003782983378698909758 ),
 .UNSPECIFIED. ) ;
#86166 = DIRECTION ( 'NONE',  ( 1.734723475976817507E-14, -6.982962677686266711E-15, 1.000000000000000000 ) ) ;
#86167 = CIRCLE ( 'NONE', #52865, 11.80000000000000604 ) ;
#86168 = VERTEX_POINT ( 'NONE', #244209 ) ;
#86169 = LINE ( 'NONE', #186604, #13913 ) ;
#86170 = AXIS2_PLACEMENT_3D ( 'NONE', #81203, #2962, #218146 ) ;
#86171 = CARTESIAN_POINT ( 'NONE',  ( 18.54999999999999716, 8.750000000011182166, -188.3499999999999659 ) ) ;
#86172 = DIRECTION ( 'NONE',  ( 0.000000000000000000, -0.9579639084728132081, -0.2868887416116073785 ) ) ;
#86173 = CIRCLE ( 'NONE', #115417, 0.09999999999999939493 ) ;
#86174 = EDGE_LOOP ( 'NONE', ( #2010, #98315, #181234, #148435 ) ) ;
#86175 = DIRECTION ( 'NONE',  ( 1.000000000000000000, 0.000000000000000000, 0.000000000000000000 ) ) ;
#86177 = ORIENTED_EDGE ( 'NONE', *, *, #210467, .F. ) ;
#86176 = FACE_OUTER_BOUND ( 'NONE', #122969, .T. ) ;
#86179 = DIRECTION ( 'NONE',  ( 0.000000000000000000, 0.000000000000000000, 1.000000000000000000 ) ) ;
#86178 = CARTESIAN_POINT ( 'NONE',  ( -20.64999999999999858, 71.65000000001155911, -57.17310748452435121 ) ) ;
#86180 = AXIS2_PLACEMENT_3D ( 'NONE', #123886, #243816, #219106 ) ;
#86181 = CARTESIAN_POINT ( 'NONE',  ( 23.24999999999999645, 1.115600667400684642E-11, -167.5000000000000284 ) ) ;
#86183 = VERTEX_POINT ( 'NONE', #23930 ) ;
#86182 = CIRCLE ( 'NONE', #69665, 0.09999999999999939493 ) ;
#86184 = LINE ( 'NONE', #105745, #92799 ) ;
#86185 = CARTESIAN_POINT ( 'NONE',  ( 0.000000000000000000, 0.000000000000000000, 0.000000000000000000 ) ) ;
#86186 = DIRECTION ( 'NONE',  ( 0.000000000000000000, -7.147358527629766941E-15, 1.000000000000000000 ) ) ;
#86187 = CARTESIAN_POINT ( 'NONE',  ( -22.84999999999999787, 4.898587196589412829E-16, 4.000000000000000000 ) ) ;
#86188 = CARTESIAN_POINT ( 'NONE',  ( -18.59999999999999787, 43.08613539620618837, -254.3146655184800409 ) ) ;
#86189 = ORIENTED_EDGE ( 'NONE', *, *, #246957, .T. ) ;
#86190 = PLANE ( 'NONE',  #21186 ) ;
#86191 = CARTESIAN_POINT ( 'NONE',  ( -20.94999999999999929, 77.16270174994961906, -61.52310748452431710 ) ) ;
#86192 = AXIS2_PLACEMENT_3D ( 'NONE', #230803, #130385, #106967 ) ;
#86193 = DIRECTION ( 'NONE',  ( 1.000000000000000000, 0.000000000000000000, 0.000000000000000000 ) ) ;
#86194 = AXIS2_PLACEMENT_3D ( 'NONE', #122126, #216071, #136525 ) ;
#86195 = CARTESIAN_POINT ( 'NONE',  ( -22.45372860728439690, 0.01492061955964466002, -122.3502028652961400 ) ) ;
#86196 = ORIENTED_EDGE ( 'NONE', *, *, #220936, .T. ) ;
#86197 = ORIENTED_EDGE ( 'NONE', *, *, #239164, .F. ) ;
#86198 = DIRECTION ( 'NONE',  ( 0.000000000000000000, 0.000000000000000000, 1.000000000000000000 ) ) ;
#86199 = DIRECTION ( 'NONE',  ( 1.000000000000000000, 0.000000000000000000, 0.000000000000000000 ) ) ;
#86200 = DIRECTION ( 'NONE',  ( 0.000000000000000000, 6.982962677686266711E-15, -1.000000000000000000 ) ) ;
#86201 = EDGE_CURVE ( 'NONE', #123298, #39898, #6899, .T. ) ;
#86202 = CARTESIAN_POINT ( 'NONE',  ( 18.54999999999999716, 23.65833333334447985, -117.2500000000000284 ) ) ;
#86203 = CARTESIAN_POINT ( 'NONE',  ( 18.49999999999999645, 18.18127959618848166, -237.5711165786817389 ) ) ;
#86204 = TOROIDAL_SURFACE ( 'NONE', #219496, 4.149999999999999467, 0.1000000000000000056 ) ;
#86206 = CARTESIAN_POINT ( 'NONE',  ( -22.57320508075687115, 31.85509083104287598, -238.8280249686205536 ) ) ;
#86205 = CARTESIAN_POINT ( 'NONE',  ( 18.59999999999999787, -1.362429037182151470, -141.8888812479212334 ) ) ;
#86207 = DIRECTION ( 'NONE',  ( 1.000000000000000000, -0.000000000000000000, -0.000000000000000000 ) ) ;
#86208 = ADVANCED_FACE ( 'NONE', ( #63016 ), #203815, .T. ) ;
#86209 = CARTESIAN_POINT ( 'NONE',  ( 20.94999999999999929, -4.254329952141543636, -236.2118329068271976 ) ) ;
#86210 = CARTESIAN_POINT ( 'NONE',  ( 21.00000000000000000, 0.000000000000000000, -4.100000000000000533 ) ) ;
#86211 = DIRECTION ( 'NONE',  ( 1.000000000000000000, 0.000000000000000000, -0.000000000000000000 ) ) ;
#86213 = ORIENTED_EDGE ( 'NONE', *, *, #233406, .T. ) ;
#86212 = LINE ( 'NONE', #122821, #186382 ) ;
#86214 = DIRECTION ( 'NONE',  ( -1.000000000000000000, 0.000000000000000000, 0.000000000000000000 ) ) ;
#86215 = DIRECTION ( 'NONE',  ( 0.000000000000000000, 1.000000000000000000, 0.000000000000000000 ) ) ;
#86217 = DIRECTION ( 'NONE',  ( -1.000000000000000000, -3.427148797533456523E-14, -5.467925025959484217E-15 ) ) ;
#86216 = LINE ( 'NONE', #66691, #105124 ) ;
#86218 = CIRCLE ( 'NONE', #40499, 0.1000000000000016431 ) ;
#86219 = EDGE_CURVE ( 'NONE', #17520, #207643, #201086, .T. ) ;
#86220 = EDGE_CURVE ( 'NONE', #21212, #92552, #47121, .T. ) ;
#86221 = ORIENTED_EDGE ( 'NONE', *, *, #27547, .F. ) ;
#86222 = CARTESIAN_POINT ( 'NONE',  ( -16.88853107394619357, 66.04912151666502496, -115.6701711376321384 ) ) ;
#86223 = DIRECTION ( 'NONE',  ( -0.000000000000000000, 0.8814952561688430555, -0.4721928772777346239 ) ) ;
#86224 = DIRECTION ( 'NONE',  ( 0.000000000000000000, 0.000000000000000000, -1.000000000000000000 ) ) ;
#86225 = CARTESIAN_POINT ( 'NONE',  ( -23.15000000000000213, 76.00000000001142553, -36.02310748452432421 ) ) ;
#86226 = DIRECTION ( 'NONE',  ( 1.000000000000000000, 0.000000000000000000, 0.000000000000000000 ) ) ;
#86227 = ORIENTED_EDGE ( 'NONE', *, *, #68165, .F. ) ;
#86228 = AXIS2_PLACEMENT_3D ( 'NONE', #236460, #237747, #14873 ) ;
#86229 = ORIENTED_EDGE ( 'NONE', *, *, #23788, .T. ) ;
#86230 = AXIS2_PLACEMENT_3D ( 'NONE', #4277, #64271, #83783 ) ;
#86231 = AXIS2_PLACEMENT_3D ( 'NONE', #236252, #17227, #116325 ) ;
#86232 = CIRCLE ( 'NONE', #148629, 0.09999999999999817368 ) ;
#86233 = CARTESIAN_POINT ( 'NONE',  ( -23.25000000000000000, -11.74999999998884448, -97.40000000000004832 ) ) ;
#86234 = ORIENTED_EDGE ( 'NONE', *, *, #189237, .F. ) ;
#86235 = DIRECTION ( 'NONE',  ( 1.000000000000000000, -0.000000000000000000, -0.000000000000000000 ) ) ;
#86236 = VERTEX_POINT ( 'NONE', #82552 ) ;
#86237 = AXIS2_PLACEMENT_3D ( 'NONE', #7859, #125229, #166957 ) ;
#86238 = EDGE_CURVE ( 'NONE', #221522, #222996, #80423, .T. ) ;
#86239 = DIRECTION ( 'NONE',  ( -0.000000000000000000, -0.9126074666063770380, -0.4088369013363281068 ) ) ;
#86240 = ADVANCED_FACE ( 'NONE', ( #43466 ), #46021, .F. ) ;
#86241 = CARTESIAN_POINT ( 'NONE',  ( 22.39999999999999503, 68.20922040163875977, -136.5231074845243313 ) ) ;
#86242 = CARTESIAN_POINT ( 'NONE',  ( -18.39999999999999858, 85.60000000001211617, -129.9229180933022576 ) ) ;
#86243 = VERTEX_POINT ( 'NONE', #85118 ) ;
#86245 = CIRCLE ( 'NONE', #198693, 7.800000000000001599 ) ;
#86244 = CARTESIAN_POINT ( 'NONE',  ( -23.15000000000000213, 1.115600667400684642E-11, -167.5000000000000284 ) ) ;
#86246 = CARTESIAN_POINT ( 'NONE',  ( -20.85000000000000142, 64.35000000001141984, -36.02310748452440237 ) ) ;
#86247 = AXIS2_PLACEMENT_3D ( 'NONE', #122185, #222536, #161319 ) ;
#86248 = CARTESIAN_POINT ( 'NONE',  ( -23.25000000000000000, 1.115600667400684642E-11, -134.0000000000000284 ) ) ;
#86249 = CARTESIAN_POINT ( 'NONE',  ( -18.50000000000000000, 64.35000000001203091, -114.7731074845243882 ) ) ;
#86250 = ADVANCED_FACE ( 'NONE', ( #163420 ), #143830, .F. ) ;
#86251 = DIRECTION ( 'NONE',  ( 0.000000000000000000, 6.982962677686266711E-15, -1.000000000000000000 ) ) ;
#86252 = CARTESIAN_POINT ( 'NONE',  ( 21.05543885634738643, 11.16761608078845924, -211.0378151740945611 ) ) ;
#86254 = ORIENTED_EDGE ( 'NONE', *, *, #83445, .F. ) ;
#86253 = ADVANCED_FACE ( 'NONE', ( #134218 ), #115969, .T. ) ;
#86256 = CARTESIAN_POINT ( 'NONE',  ( -22.49756042579671700, 75.92195366299559112, -215.1729724456266979 ) ) ;
#86255 = DIRECTION ( 'NONE',  ( 4.408576920032446123E-17, 0.8096735173027155286, -0.5868805631290315850 ) ) ;
#86257 = ORIENTED_EDGE ( 'NONE', *, *, #222976, .T. ) ;
#86259 = EDGE_LOOP ( 'NONE', ( #219171, #230186, #228156, #214305 ) ) ;
#86258 = DIRECTION ( 'NONE',  ( -0.1538461538461484146, -0.9880948137434723000, 0.000000000000000000 ) ) ;
#86260 = AXIS2_PLACEMENT_3D ( 'NONE', #185698, #170033, #229955 ) ;
#86261 = ORIENTED_EDGE ( 'NONE', *, *, #99185, .T. ) ;
#86262 = DIRECTION ( 'NONE',  ( 0.000000000000000000, -6.982962677686266711E-15, 1.000000000000000000 ) ) ;
#86263 = CARTESIAN_POINT ( 'NONE',  ( -22.39999999999999858, 68.20922040163897293, -170.1231074845244109 ) ) ;
#86264 = FACE_OUTER_BOUND ( 'NONE', #234045, .T. ) ;
#86265 = DIRECTION ( 'NONE',  ( 1.000000000000000000, 0.000000000000000000, 0.000000000000000000 ) ) ;
#86266 = ORIENTED_EDGE ( 'NONE', *, *, #2358, .T. ) ;
#86267 = CARTESIAN_POINT ( 'NONE',  ( -18.59999999999999787, 66.75000000001185185, -90.77310748452437394 ) ) ;
#86268 = CARTESIAN_POINT ( 'NONE',  ( -19.89999999999999858, 1.350000000000000089, 0.000000000000000000 ) ) ;
#86269 = EDGE_CURVE ( 'NONE', #181190, #77088, #36450, .T. ) ;
#86270 = EDGE_LOOP ( 'NONE', ( #57276, #161262, #240633, #213475 ) ) ;
#86271 = EDGE_CURVE ( 'NONE', #114442, #41849, #101256, .T. ) ;
#86272 = CARTESIAN_POINT ( 'NONE',  ( 18.40000000000000213, -9.499999999988844479, -174.4993620971800965 ) ) ;
#86273 = DIRECTION ( 'NONE',  ( 0.5932847527679298016, -0.3801118060259217613, -0.7095972217059537401 ) ) ;
#86274 = ADVANCED_FACE ( 'NONE', ( #153854 ), #221906, .F. ) ;
#86275 = AXIS2_PLACEMENT_3D ( 'NONE', #101574, #216417, #181164 ) ;
#86276 = ORIENTED_EDGE ( 'NONE', *, *, #177993, .T. ) ;
#86277 = CARTESIAN_POINT ( 'NONE',  ( -16.89935556175703368, 9.950000000011137047, -147.1396763628858082 ) ) ;
#86278 = AXIS2_PLACEMENT_3D ( 'NONE', #59034, #214304, #255937 ) ;
#86279 = ORIENTED_EDGE ( 'NONE', *, *, #44048, .F. ) ;
#86280 = LINE ( 'NONE', #128013, #96479 ) ;
#86281 = EDGE_LOOP ( 'NONE', ( #106151, #13261 ) ) ;
#86282 = DIRECTION ( 'NONE',  ( -0.7071067811865456854, 0.7071067811865493491, 0.000000000000000000 ) ) ;
#86283 = CARTESIAN_POINT ( 'NONE',  ( -23.25000000000000000, 71.85000000001151932, -48.37310748452435405 ) ) ;
#86284 = CARTESIAN_POINT ( 'NONE',  ( -22.47071067811865319, 76.00000000001267608, -203.5231074845243597 ) ) ;
#86285 = EDGE_CURVE ( 'NONE', #155942, #205417, #5423, .T. ) ;
#86286 = DIRECTION ( 'NONE',  ( -1.000000000000000000, -0.000000000000000000, -0.000000000000000000 ) ) ;
#86287 = EDGE_CURVE ( 'NONE', #182258, #69777, #155120, .T. ) ;
#86288 = AXIS2_PLACEMENT_3D ( 'NONE', #94995, #50706, #250222 ) ;
#86289 = CIRCLE ( 'NONE', #123748, 0.1000000000000008937 ) ;
#86290 = CARTESIAN_POINT ( 'NONE',  ( 23.40000000000005187, 76.00000000001119815, -36.02310748452479316 ) ) ;
#86291 = CARTESIAN_POINT ( 'NONE',  ( -19.89999999999999858, 4.513204987021262937, 22.00000000000000355 ) ) ;
#86292 = CARTESIAN_POINT ( 'NONE',  ( 20.94983749550516450, 10.29766095125292402, -72.47436639332755703 ) ) ;
#86293 = VERTEX_POINT ( 'NONE', #251616 ) ;
#86295 = CYLINDRICAL_SURFACE ( 'NONE', #196014, 0.09999999999999939493 ) ;
#86294 = FACE_OUTER_BOUND ( 'NONE', #166438, .T. ) ;
#86296 = CIRCLE ( 'NONE', #165633, 0.1000000000000028644 ) ;
#86297 = LINE ( 'NONE', #246674, #238856 ) ;
#86298 = CARTESIAN_POINT ( 'NONE',  ( -21.52071067811865746, 7.779289321892505882, -188.7499999999999716 ) ) ;
#86299 = CARTESIAN_POINT ( 'NONE',  ( -23.15000000000000213, 1.115600667400684642E-11, -46.27499999999999858 ) ) ;
#86301 = EDGE_LOOP ( 'NONE', ( #85442, #249332, #22361, #202841 ) ) ;
#86300 = DIRECTION ( 'NONE',  ( 0.000000000000000000, -1.000000000000000000, -6.982962677686265922E-15 ) ) ;
#86303 = ORIENTED_EDGE ( 'NONE', *, *, #22087, .F. ) ;
#86302 = FACE_OUTER_BOUND ( 'NONE', #36187, .T. ) ;
#86304 = DIRECTION ( 'NONE',  ( 1.000000000000000000, 0.000000000000000000, 0.000000000000000000 ) ) ;
#86305 = SPHERICAL_SURFACE ( 'NONE', #192269, 0.1000000000000000056 ) ;
#86306 = CARTESIAN_POINT ( 'NONE',  ( 18.59999999999999787, 5.900000000011102586, -110.7190997646564483 ) ) ;
#86308 = ORIENTED_EDGE ( 'NONE', *, *, #163616, .T. ) ;
#86307 = CARTESIAN_POINT ( 'NONE',  ( 18.54999999999999716, 52.34166666667870516, -119.7731074845244592 ) ) ;
#86309 =( GEOMETRIC_REPRESENTATION_CONTEXT ( 3 ) GLOBAL_UNCERTAINTY_ASSIGNED_CONTEXT ( ( #140545 ) ) GLOBAL_UNIT_ASSIGNED_CONTEXT ( ( #164712, #47299, #6912 ) ) REPRESENTATION_CONTEXT ( 'NONE', 'WORKASPACE' ) );
#86310 = CARTESIAN_POINT ( 'NONE',  ( 22.49999999999999645, 11.74956712350054744, -167.3991416309012550 ) ) ;
#86311 = CARTESIAN_POINT ( 'NONE',  ( -20.94999999999999929, 1.360870587203197646, -41.57299792709095954 ) ) ;
#86312 = ORIENTED_EDGE ( 'NONE', *, *, #89291, .T. ) ;
#86313 = DIRECTION ( 'NONE',  ( 0.000000000000000000, 1.000000000000000000, 0.000000000000000000 ) ) ;
#86314 = ORIENTED_EDGE ( 'NONE', *, *, #211559, .T. ) ;
#86315 = LINE ( 'NONE', #25116, #253309 ) ;
#86316 = AXIS2_PLACEMENT_3D ( 'NONE', #255169, #12798, #16637 ) ;
#86317 = ORIENTED_EDGE ( 'NONE', *, *, #83007, .F. ) ;
#86318 = DIRECTION ( 'NONE',  ( 1.000000000000000000, -0.000000000000000000, 0.000000000000000000 ) ) ;
#86319 = FACE_OUTER_BOUND ( 'NONE', #160676, .T. ) ;
#86320 = CIRCLE ( 'NONE', #169620, 0.5000000000000076605 ) ;
#86321 = ORIENTED_EDGE ( 'NONE', *, *, #132678, .T. ) ;
#86322 = CIRCLE ( 'NONE', #173902, 0.1000000000000028644 ) ;
#86323 = AXIS2_PLACEMENT_3D ( 'NONE', #131349, #90937, #210890 ) ;
#86324 = CYLINDRICAL_SURFACE ( 'NONE', #60389, 0.1000000000000028644 ) ;
#86325 = EDGE_CURVE ( 'NONE', #46041, #189963, #98145, .T. ) ;
#86326 = ORIENTED_EDGE ( 'NONE', *, *, #202030, .F. ) ;
#86327 = ORIENTED_EDGE ( 'NONE', *, *, #134985, .F. ) ;
#86329 = CARTESIAN_POINT ( 'NONE',  ( -21.05000000000000071, 61.12590067186530973, -234.3012893943865720 ) ) ;
#86328 = AXIS2_PLACEMENT_3D ( 'NONE', #222715, #24557, #109186 ) ;
#86330 = ORIENTED_EDGE ( 'NONE', *, *, #47896, .F. ) ;
#86331 = CARTESIAN_POINT ( 'NONE',  ( -16.89020380669786547, 9.950000000011135270, -46.25741114811057741 ) ) ;
#86332 = VECTOR ( 'NONE', #239489, 1000.000000000000000 ) ;
#86334 = EDGE_CURVE ( 'NONE', #233410, #231082, #196982, .T. ) ;
#86333 = ORIENTED_EDGE ( 'NONE', *, *, #209548, .F. ) ;
#86336 = ORIENTED_EDGE ( 'NONE', *, *, #218430, .F. ) ;
#86335 = FACE_OUTER_BOUND ( 'NONE', #104571, .T. ) ;
#86337 = DIRECTION ( 'NONE',  ( 0.000000000000000000, -6.454785026890489601E-15, 1.000000000000000000 ) ) ;
#86338 = VERTEX_POINT ( 'NONE', #255411 ) ;
#86339 = ADVANCED_FACE ( 'NONE', ( #136790 ), #97647, .T. ) ;
#86340 = CARTESIAN_POINT ( 'NONE',  ( -22.20000000000000284, 6.223900101154157483, 12.09999999999999787 ) ) ;
#86341 = EDGE_CURVE ( 'NONE', #88995, #70665, #242769, .T. ) ;
#86342 = ORIENTED_EDGE ( 'NONE', *, *, #144421, .F. ) ;
#86344 = ORIENTED_EDGE ( 'NONE', *, *, #49262, .F. ) ;
#86343 = ORIENTED_EDGE ( 'NONE', *, *, #184384, .F. ) ;
#86345 = CARTESIAN_POINT ( 'NONE',  ( 20.95000000000005613, 65.19115966511134275, -30.12310748452479103 ) ) ;
#86346 = CARTESIAN_POINT ( 'NONE',  ( -16.93301857435213975, 14.19232141894375410, -219.2844300510592177 ) ) ;
#86347 = VERTEX_POINT ( 'NONE', #216330 ) ;
#86348 = VECTOR ( 'NONE', #45019, 1000.000000000000227 ) ;
#86349 = VERTEX_POINT ( 'NONE', #232074 ) ;
#86350 = TOROIDAL_SURFACE ( 'NONE', #19774, 11.65000000000000036, 0.1000000000000000056 ) ;
#86351 = EDGE_CURVE ( 'NONE', #251476, #212682, #37748, .T. ) ;
#86352 = CARTESIAN_POINT ( 'NONE',  ( -18.39999999999999858, -9.500000000000005329, -7.032069396699667685 ) ) ;
#86353 = CARTESIAN_POINT ( 'NONE',  ( -18.59999999999999787, 64.25000000001161027, -62.50830171387040934 ) ) ;
#86355 = VERTEX_POINT ( 'NONE', #95108 ) ;
#86354 = CARTESIAN_POINT ( 'NONE',  ( -20.94999999999999929, 7.021664781900089913, -37.13356540189729316 ) ) ;
#86356 = CARTESIAN_POINT ( 'NONE',  ( 21.05000000000000071, 28.34113089492129589, -239.5930034413672161 ) ) ;
#86357 = ORIENTED_EDGE ( 'NONE', *, *, #123735, .T. ) ;
#86358 = AXIS2_PLACEMENT_3D ( 'NONE', #61010, #223924, #63576 ) ;
#86359 = LINE ( 'NONE', #146350, #199300 ) ;
#86360 = DIRECTION ( 'NONE',  ( 1.000000000000000000, 0.000000000000000000, 0.000000000000000000 ) ) ;
#86361 = ORIENTED_EDGE ( 'NONE', *, *, #244142, .T. ) ;
#86362 = CARTESIAN_POINT ( 'NONE',  ( 18.59999999999999076, 64.35000000001197407, -111.6731074845243796 ) ) ;
#86363 = CARTESIAN_POINT ( 'NONE',  ( -23.15000000000000213, 11.75000000001115552, -160.4851942293460638 ) ) ;
#86364 = ORIENTED_EDGE ( 'NONE', *, *, #105877, .F. ) ;
#86365 = CARTESIAN_POINT ( 'NONE',  ( 0.8999999999999993561, -11.65000000000000036, 26.00000000000000355 ) ) ;
#86366 = EDGE_LOOP ( 'NONE', ( #175514, #205724, #169865, #253237 ) ) ;
#86367 = VECTOR ( 'NONE', #58540, 999.9999999999998863 ) ;
#86368 = AXIS2_PLACEMENT_3D ( 'NONE', #36887, #139778, #155547 ) ;
#86369 = TOROIDAL_SURFACE ( 'NONE', #128106, 2.100000000000002309, 0.1000000000000000056 ) ;
#86371 = ORIENTED_EDGE ( 'NONE', *, *, #43147, .T. ) ;
#86370 = VERTEX_POINT ( 'NONE', #215054 ) ;
#86372 = VERTEX_POINT ( 'NONE', #191679 ) ;
#86373 = EDGE_CURVE ( 'NONE', #172709, #208877, #88630, .T. ) ;
#86374 = VERTEX_POINT ( 'NONE', #33904 ) ;
#86375 = EDGE_CURVE ( 'NONE', #180038, #18766, #117866, .T. ) ;
#86376 = CARTESIAN_POINT ( 'NONE',  ( -18.59999999999999787, 74.65925378207832352, -113.2959699899454904 ) ) ;
#86377 = ORIENTED_EDGE ( 'NONE', *, *, #223023, .F. ) ;
#86378 = CARTESIAN_POINT ( 'NONE',  ( -16.90202395485795250, 66.03405545546092981, -48.62009376326439991 ) ) ;
#86379 = CARTESIAN_POINT ( 'NONE',  ( 20.95512820512820440, 43.40368376489742275, -234.8883907171572787 ) ) ;
#86380 = ORIENTED_EDGE ( 'NONE', *, *, #30136, .T. ) ;
#86381 = CIRCLE ( 'NONE', #124033, 0.09999999999999108213 ) ;
#86382 = AXIS2_PLACEMENT_3D ( 'NONE', #60137, #140992, #164401 ) ;
#86384 = ADVANCED_FACE ( 'NONE', ( #179795 ), #239760, .T. ) ;
#86383 = ORIENTED_EDGE ( 'NONE', *, *, #102467, .T. ) ;
#86385 = CIRCLE ( 'NONE', #149369, 4.000000000000003553 ) ;
#86386 = EDGE_LOOP ( 'NONE', ( #184650, #84731, #223155, #241095 ) ) ;
#86387 = B_SPLINE_CURVE_WITH_KNOTS ( 'NONE', 3,
 ( #246621, #127977, #227059, #167130, #190537, #67993 ),
 .UNSPECIFIED., .F., .F.,
 ( 4, 2, 4 ),
 ( 0.000000000000000000, 0.0001891491689349436448, 0.0003782983378698872895 ),
 .UNSPECIFIED. ) ;
#86388 = AXIS2_PLACEMENT_3D ( 'NONE', #34498, #93151, #71054 ) ;
#86389 = CARTESIAN_POINT ( 'NONE',  ( -23.15000000000000213, 64.25000000001217870, -139.6231074845244393 ) ) ;
#86390 = VERTEX_POINT ( 'NONE', #238467 ) ;
#86391 = DIRECTION ( 'NONE',  ( 0.000000000000000000, 1.000000000000000000, 0.000000000000000000 ) ) ;
#86393 = VERTEX_POINT ( 'NONE', #162802 ) ;
#86392 = CARTESIAN_POINT ( 'NONE',  ( -23.25000000000000000, 64.27847795353595473, -247.1247091181747066 ) ) ;
#86394 = DIRECTION ( 'NONE',  ( -1.000000000000000000, -0.000000000000000000, 0.000000000000000000 ) ) ;
#86395 = CARTESIAN_POINT ( 'NONE',  ( -18.59999999999999787, 14.05000000001115623, -139.5136950707610026 ) ) ;
#86396 = CARTESIAN_POINT ( 'NONE',  ( -16.92209698673947571, 12.42693673621513994, -211.3021356947419349 ) ) ;
#86397 = LINE ( 'NONE', #166003, #252619 ) ;
#86398 = AXIS2_PLACEMENT_3D ( 'NONE', #88299, #225249, #160523 ) ;
#86400 = EDGE_CURVE ( 'NONE', #108241, #11008, #238690, .T. ) ;
#86399 = CARTESIAN_POINT ( 'NONE',  ( -23.15000000000000213, 76.00000000001242029, -166.1231074845243825 ) ) ;
#86402 = CYLINDRICAL_SURFACE ( 'NONE', #253518, 4.000000000000003553 ) ;
#86401 = DIRECTION ( 'NONE',  ( 0.000000000000000000, 0.000000000000000000, -1.000000000000000000 ) ) ;
#86403 = FACE_OUTER_BOUND ( 'NONE', #163746, .T. ) ;
#86404 = AXIS2_PLACEMENT_3D ( 'NONE', #72406, #151949, #11133 ) ;
#86405 = DIRECTION ( 'NONE',  ( -3.265361837132813093E-16, 1.000000000000000000, 0.000000000000000000 ) ) ;
#86407 = DIRECTION ( 'NONE',  ( -7.304098846218134667E-16, 1.000000000000000000, -0.000000000000000000 ) ) ;
#86406 = AXIS2_PLACEMENT_3D ( 'NONE', #43957, #230291, #112923 ) ;
#86408 = DIRECTION ( 'NONE',  ( 1.000000000000000000, 0.000000000000000000, 0.000000000000000000 ) ) ;
#86410 = ORIENTED_EDGE ( 'NONE', *, *, #174597, .T. ) ;
#86409 = AXIS2_PLACEMENT_3D ( 'NONE', #247415, #131325, #133890 ) ;
#86411 = EDGE_CURVE ( 'NONE', #212886, #196267, #130338, .T. ) ;
#86414 = VERTEX_POINT ( 'NONE', #2404 ) ;
#86413 = EDGE_CURVE ( 'NONE', #196849, #16167, #62405, .T. ) ;
#86412 = DIRECTION ( 'NONE',  ( -1.000000000000000000, 0.000000000000000000, 0.000000000000000000 ) ) ;
#86415 = EDGE_LOOP ( 'NONE', ( #189637, #46035, #109512, #217308 ) ) ;
#86416 = DIRECTION ( 'NONE',  ( -1.000000000000000000, 0.000000000000000000, 0.000000000000000000 ) ) ;
#86417 = LINE ( 'NONE', #87715, #207017 ) ;
#86418 = EDGE_CURVE ( 'NONE', #41254, #132235, #246867, .T. ) ;
#86419 = EDGE_CURVE ( 'NONE', #46846, #43496, #13827, .T. ) ;
#86420 = DIRECTION ( 'NONE',  ( 1.000000000000000000, 0.000000000000000000, 0.000000000000000000 ) ) ;
#86421 = ORIENTED_EDGE ( 'NONE', *, *, #76329, .F. ) ;
#86422 = CARTESIAN_POINT ( 'NONE',  ( 23.14999999999998437, 36.65892442174472876, -249.5511627012454596 ) ) ;
#86423 = CARTESIAN_POINT ( 'NONE',  ( -16.89268316805465986, 9.951721813242182080, -20.85575247854553993 ) ) ;
#86424 = ORIENTED_EDGE ( 'NONE', *, *, #166041, .T. ) ;
#86425 = EDGE_CURVE ( 'NONE', #242287, #183962, #139345, .T. ) ;
#86426 = CARTESIAN_POINT ( 'NONE',  ( 21.05000000000000071, 76.00000000001213607, -136.5231074845243313 ) ) ;
#86427 = DIRECTION ( 'NONE',  ( 1.000000000000000000, 0.000000000000000000, 0.000000000000000000 ) ) ;
#86428 = ADVANCED_FACE ( 'NONE', ( #83212 ), #126253, .F. ) ;
#86429 = FACE_OUTER_BOUND ( 'NONE', #147043, .T. ) ;
#86430 = DIRECTION ( 'NONE',  ( 0.000000000000000000, -6.467318590049456648E-15, 1.000000000000000000 ) ) ;
#86432 = VERTEX_POINT ( 'NONE', #24581 ) ;
#86431 = DIRECTION ( 'NONE',  ( -0.000000000000000000, -6.982962677686266711E-15, 1.000000000000000000 ) ) ;
#86433 = EDGE_CURVE ( 'NONE', #42744, #212838, #34692, .T. ) ;
#86434 = DIRECTION ( 'NONE',  ( -1.000000000000000000, -2.952720810173289112E-16, 0.000000000000000000 ) ) ;
#86435 = DIRECTION ( 'NONE',  ( 0.000000000000000000, 0.000000000000000000, -1.000000000000000000 ) ) ;
#86436 = DIRECTION ( 'NONE',  ( -1.000000000000000000, 0.000000000000000000, 0.000000000000000000 ) ) ;
#86437 = FACE_OUTER_BOUND ( 'NONE', #143195, .T. ) ;
#86438 = VERTEX_POINT ( 'NONE', #100210 ) ;
#86439 = DIRECTION ( 'NONE',  ( 0.000000000000000000, 0.5000000000000209832, 0.8660254037844264952 ) ) ;
#86440 = DIRECTION ( 'NONE',  ( 1.000000000000000000, 0.000000000000000000, 0.000000000000000000 ) ) ;
#86441 = EDGE_CURVE ( 'NONE', #141218, #160294, #102777, .T. ) ;
#86442 = FACE_OUTER_BOUND ( 'NONE', #257255, .T. ) ;
#86443 = DIRECTION ( 'NONE',  ( 0.000000000000000000, 1.000000000000000000, 1.734723475976807292E-15 ) ) ;
#86444 = CARTESIAN_POINT ( 'NONE',  ( 18.49999999999999289, 65.79142135624904597, -81.27310748452438816 ) ) ;
#86445 = CARTESIAN_POINT ( 'NONE',  ( -18.39999999999999858, 11.47316190337362762, -143.2998292484660112 ) ) ;
#86446 = DIRECTION ( 'NONE',  ( 0.000000000000000000, 0.9126074666063772600, 0.4088369013363276627 ) ) ;
#86447 = AXIS2_PLACEMENT_3D ( 'NONE', #64736, #85546, #46447 ) ;
#86448 = TOROIDAL_SURFACE ( 'NONE', #61544, 11.70000000000000107, 0.1000000000000000056 ) ;
#86449 = DIRECTION ( 'NONE',  ( -0.000000000000000000, 0.2617529984165031243, 0.9651348961777157509 ) ) ;
#86450 = DIRECTION ( 'NONE',  ( 0.000000000000000000, 0.000000000000000000, -1.000000000000000000 ) ) ;
#86451 = EDGE_CURVE ( 'NONE', #79411, #222495, #9543, .T. ) ;
#86452 = AXIS2_PLACEMENT_3D ( 'NONE', #213515, #131414, #54445 ) ;
#86453 = EDGE_CURVE ( 'NONE', #193203, #140485, #255193, .T. ) ;
#86454 = EDGE_LOOP ( 'NONE', ( #168756, #67655, #162965, #211668 ) ) ;
#86455 = DIRECTION ( 'NONE',  ( 0.000000000000000000, 0.000000000000000000, -1.000000000000000000 ) ) ;
#86456 = VERTEX_POINT ( 'NONE', #143205 ) ;
#86457 = EDGE_LOOP ( 'NONE', ( #23241, #62267, #12154, #58743, #235992 ) ) ;
#86458 = ADVANCED_FACE ( 'NONE', ( #23302 ), #142789, .F. ) ;
#86459 = CARTESIAN_POINT ( 'NONE',  ( 20.87631937322882436, 65.52850496324731466, -95.44336160994302531 ) ) ;
#86460 = CARTESIAN_POINT ( 'NONE',  ( -21.05000000000000071, 4.436385504674529301, -245.3241086753762659 ) ) ;
#86461 = ORIENTED_EDGE ( 'NONE', *, *, #14819, .F. ) ;
#86462 = EDGE_CURVE ( 'NONE', #256904, #232714, #220198, .T. ) ;
#86463 = EDGE_CURVE ( 'NONE', #997, #244808, #176175, .T. ) ;
#86464 = ORIENTED_EDGE ( 'NONE', *, *, #164334, .F. ) ;
#86465 = AXIS2_PLACEMENT_3D ( 'NONE', #173308, #254059, #93713 ) ;
#86466 = EDGE_CURVE ( 'NONE', #142512, #132861, #39003, .T. ) ;
#86467 = VECTOR ( 'NONE', #247576, 1000.000000000000000 ) ;
#86468 = ORIENTED_EDGE ( 'NONE', *, *, #234238, .F. ) ;
#86469 = DIRECTION ( 'NONE',  ( 0.000000000000000000, -0.4930308989875248349, -0.8700118002898312719 ) ) ;
#86470 = ORIENTED_EDGE ( 'NONE', *, *, #120594, .F. ) ;
#86471 = DIRECTION ( 'NONE',  ( 0.000000000000000000, 0.4599910535713788717, -0.8879235499941945386 ) ) ;
#86472 = DIRECTION ( 'NONE',  ( 0.000000000000000000, -0.1350103645451876666, 0.9908441862701600211 ) ) ;
#86473 = CIRCLE ( 'NONE', #240622, 0.09999999999998898659 ) ;
#86474 = DIRECTION ( 'NONE',  ( 1.000000000000000000, -0.000000000000000000, -0.000000000000000000 ) ) ;
#86475 = DIRECTION ( 'NONE',  ( 1.734723475976814920E-13, -0.4608403197577645716, -0.8874830700839093645 ) ) ;
#86476 = CARTESIAN_POINT ( 'NONE',  ( -21.08376601933334271, 1.568551483692875781, -230.6818607317798637 ) ) ;
#86477 = DIRECTION ( 'NONE',  ( -1.000000000000000000, -8.623019343401632876E-17, -8.389849937938899189E-16 ) ) ;
#86478 = CARTESIAN_POINT ( 'NONE',  ( -22.39999999999999858, 11.65000000001115588, -33.50000000000000000 ) ) ;
#86480 = ORIENTED_EDGE ( 'NONE', *, *, #151385, .T. ) ;
#86479 = DIRECTION ( 'NONE',  ( 2.952720810173289112E-16, 1.000000000000000000, 6.938893903907222067E-15 ) ) ;
#86481 = CARTESIAN_POINT ( 'NONE',  ( 20.95539060131842746, 65.37613784235595915, -61.86937367086819961 ) ) ;
#86482 = ADVANCED_FACE ( 'NONE', ( #198053 ), #98925, .F. ) ;
#86483 = CARTESIAN_POINT ( 'NONE',  ( -21.93340585899449380, 76.00000000001170974, -76.84725450664456048 ) ) ;
#86484 = ORIENTED_EDGE ( 'NONE', *, *, #135583, .F. ) ;
#86485 = CARTESIAN_POINT ( 'NONE',  ( -16.87036670365548474, 65.91505003675696628, -149.0731074845244279 ) ) ;
#86486 = SPHERICAL_SURFACE ( 'NONE', #154150, 0.1000000000000000056 ) ;
#86487 = EDGE_LOOP ( 'NONE', ( #55225, #111368, #216579, #138036 ) ) ;
#86488 = CARTESIAN_POINT ( 'NONE',  ( 22.00356870069427018, 76.00000000002543743, -76.77734984627505810 ) ) ;
#86489 = CIRCLE ( 'NONE', #153193, 4.300000000000025580 ) ;
#86490 = DIRECTION ( 'NONE',  ( 1.000000000000000000, 0.000000000000000000, 0.000000000000000000 ) ) ;
#86491 = VERTEX_POINT ( 'NONE', #105334 ) ;
#86492 = CIRCLE ( 'NONE', #37052, 0.1999999999999996503 ) ;
#86493 = DIRECTION ( 'NONE',  ( -0.000000000000000000, -0.000000000000000000, -1.000000000000000000 ) ) ;
#86494 = CYLINDRICAL_SURFACE ( 'NONE', #170425, 0.5000000000000004441 ) ;
#86495 = DIRECTION ( 'NONE',  ( 0.000000000000000000, -0.9915357197604882655, 0.1298341882519791490 ) ) ;
#86496 = DIRECTION ( 'NONE',  ( 0.000000000000000000, 1.000000000000000000, 0.000000000000000000 ) ) ;
#86497 = VERTEX_POINT ( 'NONE', #225297 ) ;
#86498 = CIRCLE ( 'NONE', #19924, 0.09999999999999875655 ) ;
#86499 = ORIENTED_EDGE ( 'NONE', *, *, #164318, .T. ) ;
#86500 = CARTESIAN_POINT ( 'NONE',  ( 21.08804582317324261, 67.12183383291996108, -90.67310765511901138 ) ) ;
#86501 = DIRECTION ( 'NONE',  ( 0.000000000000000000, 1.084202172485623868E-14, 1.000000000000000000 ) ) ;
#86502 = EDGE_CURVE ( 'NONE', #217324, #146896, #46668, .T. ) ;
#86503 = DIRECTION ( 'NONE',  ( 0.000000000000000000, 0.000000000000000000, -1.000000000000000000 ) ) ;
#86504 = DIRECTION ( 'NONE',  ( 0.000000000000000000, 0.000000000000000000, -1.000000000000000000 ) ) ;
#86505 = AXIS2_PLACEMENT_3D ( 'NONE', #150491, #51341, #69679 ) ;
#86507 = CARTESIAN_POINT ( 'NONE',  ( -22.39999999999999858, -3.187427350888460076, -228.3200064793908837 ) ) ;
#86506 = AXIS2_PLACEMENT_3D ( 'NONE', #163763, #69807, #88034 ) ;
#86508 = EDGE_CURVE ( 'NONE', #52291, #23148, #22232, .T. ) ;
#86509 = CARTESIAN_POINT ( 'NONE',  ( -33.72168855820451938, 9.950000000011156587, -46.14999999999994884 ) ) ;
#86510 = AXIS2_PLACEMENT_3D ( 'NONE', #84305, #45241, #242151 ) ;
#86511 = VERTEX_POINT ( 'NONE', #126213 ) ;
#86512 = CARTESIAN_POINT ( 'NONE',  ( -18.50000000000000000, 36.65892442174935439, -249.5511627012433848 ) ) ;
#86514 = ORIENTED_EDGE ( 'NONE', *, *, #72089, .T. ) ;
#86513 = LINE ( 'NONE', #85225, #37948 ) ;
#86515 = CARTESIAN_POINT ( 'NONE',  ( -20.94999999999999929, 87.65000000001266756, -200.6231074845242688 ) ) ;
#86516 = AXIS2_PLACEMENT_3D ( 'NONE', #174038, #214396, #96976 ) ;
#86517 = CARTESIAN_POINT ( 'NONE',  ( -23.39999999999994529, 76.00000000001119815, -40.17310748452479174 ) ) ;
#86518 = CARTESIAN_POINT ( 'NONE',  ( -21.08078803292166725, 75.92081401285399522, -75.85612044896146244 ) ) ;
#86519 = DIRECTION ( 'NONE',  ( 0.000000000000000000, 0.000000000000000000, 1.000000000000000000 ) ) ;
#86520 = ADVANCED_FACE ( 'NONE', ( #7559 ), #166668, .F. ) ;
#86521 = CIRCLE ( 'NONE', #127692, 0.09999999999999939493 ) ;
#86522 = ADVANCED_FACE ( 'NONE', ( #67529 ), #248746, .T. ) ;
#86524 = ORIENTED_EDGE ( 'NONE', *, *, #135504, .T. ) ;
#86523 = DIRECTION ( 'NONE',  ( 0.000000000000000000, 0.9651348961777157509, -0.2617529984165031243 ) ) ;
#86525 = DIRECTION ( 'NONE',  ( 0.000000000000000000, -0.9651348961777161950, 0.2617529984165014589 ) ) ;
#86526 = DIRECTION ( 'NONE',  ( 0.000000000000000000, 0.8814952561688476074, -0.4721928772777262417 ) ) ;
#86527 = DIRECTION ( 'NONE',  ( 0.000000000000000000, -0.8164390028469705740, 0.5774316882803059992 ) ) ;
#86528 = LINE ( 'NONE', #186975, #174057 ) ;
#86529 = ORIENTED_EDGE ( 'NONE', *, *, #104637, .F. ) ;
#86530 = LINE ( 'NONE', #87819, #26480 ) ;
#86531 = CARTESIAN_POINT ( 'NONE',  ( -16.88705144915408951, 66.05000000001200533, -115.9540860792368733 ) ) ;
#86532 = CARTESIAN_POINT ( 'NONE',  ( -18.58735405345341718, 87.01880836603646685, -199.4423219559112681 ) ) ;
#86533 = LINE ( 'NONE', #81391, #154977 ) ;
#86534 = CIRCLE ( 'NONE', #194913, 7.791421356237338003 ) ;
#86535 = EDGE_LOOP ( 'NONE', ( #235490, #232342, #73854, #153059, #47439, #235187, #162390, #189748, #212237, #187725, #207508, #172841, #254869, #112469, #183044, #23200, #251541, #210494, #15332, #192049, #203669, #53660, #114485, #125490, #113147 ) ) ;
#86536 = DIRECTION ( 'NONE',  ( -0.000000000000000000, 0.2617529984165031243, 0.9651348961777157509 ) ) ;
#86537 = AXIS2_PLACEMENT_3D ( 'NONE', #17445, #55255, #134802 ) ;
#86538 = ORIENTED_EDGE ( 'NONE', *, *, #211549, .T. ) ;
#86539 = CIRCLE ( 'NONE', #249090, 0.09999999999999939493 ) ;
#86540 = CARTESIAN_POINT ( 'NONE',  ( 21.00023020733502577, -1.359983335743155886, -194.7555100259054086 ) ) ;
#86542 = DIRECTION ( 'NONE',  ( 1.000000000000000000, 0.000000000000000000, 0.000000000000000000 ) ) ;
#86541 = TOROIDAL_SURFACE ( 'NONE', #103122, 0.2000000000000000111, 0.1000000000000000056 ) ;
#86543 = TOROIDAL_SURFACE ( 'NONE', #28350, 0.2000000000000000111, 0.1000000000000000056 ) ;
#86544 = FACE_OUTER_BOUND ( 'NONE', #73561, .T. ) ;
#86545 = DIRECTION ( 'NONE',  ( -1.000000000000000000, 0.000000000000000000, 0.000000000000000000 ) ) ;
#86546 = ORIENTED_EDGE ( 'NONE', *, *, #163805, .F. ) ;
#86547 = VECTOR ( 'NONE', #109113, 999.9999999999998863 ) ;
#86548 = CARTESIAN_POINT ( 'NONE',  ( 18.59999999999999432, 45.93315328338058379, -256.6017782078560003 ) ) ;
#86549 = CARTESIAN_POINT ( 'NONE',  ( -21.05000000000000071, 74.83729825007462466, -195.4231074845243654 ) ) ;
#86550 = DIRECTION ( 'NONE',  ( 1.000000000000000000, 0.000000000000000000, 0.000000000000000000 ) ) ;
#86551 = CARTESIAN_POINT ( 'NONE',  ( 20.94999999999999929, 47.95459712139159336, -246.5019368548292675 ) ) ;
#86552 = AXIS2_PLACEMENT_3D ( 'NONE', #97007, #60472, #159600 ) ;
#86553 = ADVANCED_FACE ( 'NONE', ( #29727 ), #227892, .F. ) ;
#86555 = PRESENTATION_LAYER_ASSIGNMENT (  '', '', ( #94955 ) ) ;
#86554 = PLANE ( 'NONE',  #61569 ) ;
#86556 = VECTOR ( 'NONE', #124694, 1000.000000000000000 ) ;
#86557 = ORIENTED_EDGE ( 'NONE', *, *, #126501, .F. ) ;
#86559 = EDGE_LOOP ( 'NONE', ( #108221, #4693, #143970, #1049 ) ) ;
#86558 = CARTESIAN_POINT ( 'NONE',  ( -21.93340585971692391, 7.324147022868191748, -167.4999999999999432 ) ) ;
#86560 = ORIENTED_EDGE ( 'NONE', *, *, #2498, .T. ) ;
#86561 = CARTESIAN_POINT ( 'NONE',  ( -18.40000000000000213, 11.47316190337362762, -180.0499999999999545 ) ) ;
#86562 = ORIENTED_EDGE ( 'NONE', *, *, #13932, .T. ) ;
#86563 = CARTESIAN_POINT ( 'NONE',  ( 21.07189867249812210, 65.27501972991890966, -124.3106560422476434 ) ) ;
#86564 = CARTESIAN_POINT ( 'NONE',  ( 23.14999999999999503, 69.35000000001156195, -57.37310748452436826 ) ) ;
#86565 = CARTESIAN_POINT ( 'NONE',  ( -22.47071067811865319, 59.75442326890419764, -233.9300113800878762 ) ) ;
#86566 = ORIENTED_EDGE ( 'NONE', *, *, #253778, .F. ) ;
#86567 = CARTESIAN_POINT ( 'NONE',  ( -23.25000000000000000, 77.83585931145570669, -125.0186683157258329 ) ) ;
#86568 = CARTESIAN_POINT ( 'NONE',  ( 19.97071067811864609, 11.72071067812981404, -91.65000000000004832 ) ) ;
#86569 = CARTESIAN_POINT ( 'NONE',  ( 20.72390388899108515, 10.58996311843486993, -41.01134829574520779 ) ) ;
#86570 = ADVANCED_FACE ( 'NONE', ( #8849 ), #109215, .T. ) ;
#86571 = ORIENTED_EDGE ( 'NONE', *, *, #116960, .T. ) ;
#86572 = CARTESIAN_POINT ( 'NONE',  ( 18.59999999999999432, 74.83729825007431202, -162.0231074845243597 ) ) ;
#86574 = ORIENTED_EDGE ( 'NONE', *, *, #201003, .T. ) ;
#86573 = DIRECTION ( 'NONE',  ( 1.000000000000000000, -1.186688945009009831E-16, -8.286604613020806758E-31 ) ) ;
#86576 = EDGE_CURVE ( 'NONE', #68945, #115014, #122170, .T. ) ;
#86575 = CARTESIAN_POINT ( 'NONE',  ( -18.59999999999999787, 1.162701749949165642, -108.6000000000000227 ) ) ;
#86577 = VECTOR ( 'NONE', #182374, 1000.000000000000000 ) ;
#86578 = DIRECTION ( 'NONE',  ( 0.000000000000000000, -0.1350103645451904977, 0.9908441862701596881 ) ) ;
#86579 = ORIENTED_EDGE ( 'NONE', *, *, #217372, .F. ) ;
#86580 = CIRCLE ( 'NONE', #128321, 0.2000000000000057288 ) ;
#86581 = LINE ( 'NONE', #181866, #206071 ) ;
#86583 = EDGE_CURVE ( 'NONE', #118009, #221355, #209615, .T. ) ;
#86582 = CARTESIAN_POINT ( 'NONE',  ( -21.05000000000000071, 0.000000000000000000, 0.000000000000000000 ) ) ;
#86584 = DIRECTION ( 'NONE',  ( 1.000000000000000000, -2.952720810173289112E-16, -2.061873921506763405E-30 ) ) ;
#86585 = VERTEX_POINT ( 'NONE', #88351 ) ;
#86586 = CARTESIAN_POINT ( 'NONE',  ( 23.14999999999999503, 69.45000000001149942, -48.37310748452436826 ) ) ;
#86587 = ADVANCED_FACE ( 'NONE', ( #106634 ), #188759, .T. ) ;
#86588 = FACE_OUTER_BOUND ( 'NONE', #149269, .T. ) ;
#86589 = AXIS2_PLACEMENT_3D ( 'NONE', #244506, #46297, #63298 ) ;
#86590 = EDGE_CURVE ( 'NONE', #132438, #59112, #238872, .T. ) ;
#86591 = ORIENTED_EDGE ( 'NONE', *, *, #62780, .T. ) ;
#86592 = AXIS2_PLACEMENT_3D ( 'NONE', #40041, #223763, #182095 ) ;
#86593 = AXIS2_PLACEMENT_3D ( 'NONE', #225978, #143903, #86475 ) ;
#86594 = EDGE_CURVE ( 'NONE', #162687, #141245, #10133, .T. ) ;
#86595 = AXIS2_PLACEMENT_3D ( 'NONE', #35685, #76057, #257213 ) ;
#86596 = CIRCLE ( 'NONE', #65776, 0.09999999999999939493 ) ;
#86597 = B_SPLINE_CURVE_WITH_KNOTS ( 'NONE', 3,
 ( #23183, #240927, #63555, #183521, #121008, #200512, #257865, #162678, #102662, #123543, #203070, #21880, #143085, #222614, #24469, #103949 ),
 .UNSPECIFIED., .F., .F.,
 ( 4, 3, 3, 3, 3, 4 ),
 ( 0.000000000000000000, 2.209833635978077814E-05, 5.595056164119279336E-05, 8.979992002655381403E-05, 0.0001236482757198913553, 0.0001574984039362988268 ),
 .UNSPECIFIED. ) ;
#86598 = ORIENTED_EDGE ( 'NONE', *, *, #178282, .F. ) ;
#86599 = CARTESIAN_POINT ( 'NONE',  ( 23.14999999999999858, 76.00000000001190870, -103.0231074845243029 ) ) ;
#86600 = ORIENTED_EDGE ( 'NONE', *, *, #109601, .F. ) ;
#86601 = CARTESIAN_POINT ( 'NONE',  ( 21.05000000000000071, 7.128833340093095217, -233.7327013124392749 ) ) ;
#86603 = ADVANCED_FACE ( 'NONE', ( #226589 ), #167996, .F. ) ;
#86602 = DIRECTION ( 'NONE',  ( -0.000000000000000000, -6.982962677686266711E-15, 1.000000000000000000 ) ) ;
#86605 = VERTEX_POINT ( 'NONE', #89648 ) ;
#86604 = CARTESIAN_POINT ( 'NONE',  ( -16.85312841634287295, 9.913606177331358182, -146.8971731332925685 ) ) ;
#86606 = CARTESIAN_POINT ( 'NONE',  ( 20.85000000106584750, 11.75000000001115907, -127.1555046564734113 ) ) ;
#86607 = CARTESIAN_POINT ( 'NONE',  ( 20.95512820512820440, 10.62384868372303615, -112.6500000000000341 ) ) ;
#86608 =( NAMED_UNIT ( * ) PLANE_ANGLE_UNIT ( ) SI_UNIT ( $, .RADIAN. ) );
#86609 = DIRECTION ( 'NONE',  ( 0.000000000000000000, 0.000000000000000000, 1.000000000000000000 ) ) ;
#86610 = CARTESIAN_POINT ( 'NONE',  ( -23.25000000000000000, 11.65000000001115588, -146.1500000000000341 ) ) ;
#86611 = CARTESIAN_POINT ( 'NONE',  ( -20.64999999999999858, 46.15118611352045974, -240.5321844900040844 ) ) ;
#86612 = VECTOR ( 'NONE', #106799, 1000.000000000000000 ) ;
#86613 = DIRECTION ( 'NONE',  ( -1.000000000000000000, -0.000000000000000000, -0.000000000000000000 ) ) ;
#86614 = CARTESIAN_POINT ( 'NONE',  ( -21.05000000000000071, 6.257814610487270279, -100.4022097086912311 ) ) ;
#86616 = ORIENTED_EDGE ( 'NONE', *, *, #172148, .T. ) ;
#86615 = CARTESIAN_POINT ( 'NONE',  ( -21.05000000000000071, 1.115600667400684642E-11, -100.5000000000000426 ) ) ;
#86617 = CARTESIAN_POINT ( 'NONE',  ( -20.54999999999999716, 73.60000000001184617, -89.79848556176223440 ) ) ;
#86618 = VERTEX_POINT ( 'NONE', #31012 ) ;
#86619 = AXIS2_PLACEMENT_3D ( 'NONE', #248919, #111980, #170707 ) ;
#86620 = DIRECTION ( 'NONE',  ( 0.000000000000000000, 0.000000000000000000, -1.000000000000000000 ) ) ;
#86621 = CARTESIAN_POINT ( 'NONE',  ( -20.54999999999999716, -9.399999999988846611, -157.6060308773475924 ) ) ;
#86622 = CARTESIAN_POINT ( 'NONE',  ( 20.97250901189795513, 65.37543196631075659, -195.8585617675574611 ) ) ;
#86623 = CARTESIAN_POINT ( 'NONE',  ( 23.24999999999997513, 64.25000000001195133, -110.0379132551783243 ) ) ;
#86624 = ORIENTED_EDGE ( 'NONE', *, *, #146413, .T. ) ;
#86625 = CARTESIAN_POINT ( 'NONE',  ( 21.05000000000000426, 10.23297665902167886, -228.1194301247179510 ) ) ;
#86626 = CARTESIAN_POINT ( 'NONE',  ( -21.09610168723073542, 6.378955715235941071, -100.4664104931085262 ) ) ;
#86627 = CIRCLE ( 'NONE', #32537, 4.100000000000006750 ) ;
#86628 = AXIS2_PLACEMENT_3D ( 'NONE', #84107, #25491, #63306 ) ;
#86629 = VERTEX_POINT ( 'NONE', #169243 ) ;
#86631 = EDGE_CURVE ( 'NONE', #96897, #254455, #68178, .T. ) ;
#86630 = CARTESIAN_POINT ( 'NONE',  ( 21.04999999999999361, 75.90156250001241744, -209.8223383946166507 ) ) ;
#86632 = CARTESIAN_POINT ( 'NONE',  ( 23.50000000000004263, 83.98667523412385094, -37.28476067066772970 ) ) ;
#86633 = ORIENTED_EDGE ( 'NONE', *, *, #153604, .T. ) ;
#86634 = DIRECTION ( 'NONE',  ( 0.000000000000000000, 0.000000000000000000, 1.000000000000000000 ) ) ;
#86635 = ORIENTED_EDGE ( 'NONE', *, *, #240182, .F. ) ;
#86637 = ADVANCED_FACE ( 'NONE', ( #110504 ), #138864, .F. ) ;
#86636 = CARTESIAN_POINT ( 'NONE',  ( -13.43673303185029688, 9.446648990640015953, -48.58916329592318561 ) ) ;
#86638 = ORIENTED_EDGE ( 'NONE', *, *, #245943, .F. ) ;
#86639 = CYLINDRICAL_SURFACE ( 'NONE', #31767, 0.1000000000000028644 ) ;
#86640 = ADVANCED_FACE ( 'NONE', ( #148358 ), #131353, .T. ) ;
#86641 = LINE ( 'NONE', #68401, #238974 ) ;
#86642 = TOROIDAL_SURFACE ( 'NONE', #70147, 7.800000000000000711, 0.1000000000000000056 ) ;
#86643 = EDGE_CURVE ( 'NONE', #108899, #175784, #32287, .T. ) ;
#86644 = ORIENTED_EDGE ( 'NONE', *, *, #54155, .F. ) ;
#86645 = ORIENTED_EDGE ( 'NONE', *, *, #196107, .T. ) ;
#86647 = DIRECTION ( 'NONE',  ( -0.000000000000000000, 0.000000000000000000, -1.000000000000000000 ) ) ;
#86646 = CIRCLE ( 'NONE', #165824, 0.1000000000000028644 ) ;
#86649 = ORIENTED_EDGE ( 'NONE', *, *, #100628, .T. ) ;
